#126376=CARTESIAN_POINT('Ctrl Pts',(-6.43768917687825,-78.1193716314746,
57.2055448111296));
#126377=CARTESIAN_POINT('Ctrl Pts',(-6.46127749702327,-78.5607009250776,
57.2372938612818));
#126378=CARTESIAN_POINT('Ctrl Pts',(-6.50284708023062,-79.220321178602,
57.2950452555082));
#126379=CARTESIAN_POINT('Ctrl Pts',(-6.52517453823015,-79.5495378836441,
57.3264553750152));
#126380=CARTESIAN_POINT('Ctrl Pts',(-6.55374130281479,-79.9325855515165,
57.3676563681427));
#126381=CARTESIAN_POINT('Ctrl Pts',(-6.56650133766688,-80.0965263046025,
57.3863044363751));
#126382=CARTESIAN_POINT('Ctrl Pts',(-6.5751203655941,-80.2057706881831,
57.3989582017931));
#126383=CARTESIAN_POINT('Ctrl Pts',(-6.57964866975663,-80.2623756631579,
57.4056368678187));
#126384=CARTESIAN_POINT('Ctrl Pts',(-6.72015992204332,-81.9970282825598,
57.6138171149191));
#126385=CARTESIAN_POINT('Ctrl Pts',(-6.90771485277002,-83.6167188709601,
57.9152192285855));
#126386=CARTESIAN_POINT('Ctrl Pts',(-7.08824189517591,-85.17401265925,58.3404161122));
#126387=CARTESIAN_POINT('',(-7.08815755158619,25.,58.3404518909995));
#126388=CARTESIAN_POINT('Origin',(27.4324635166691,25.,72.98888938658));
#126389=CARTESIAN_POINT('',(-8.15021171484832,-89.0000000007984,61.1515796381337));
#126390=CARTESIAN_POINT('Ctrl Pts',(-7.08815755570517,-85.17401265925,58.3404519007063));
#126391=CARTESIAN_POINT('Ctrl Pts',(-7.17009088674586,-85.5332934006639,
58.5335366223212));
#126392=CARTESIAN_POINT('Ctrl Pts',(-7.25466994278313,-85.8832477134225,
58.7373493420429));
#126393=CARTESIAN_POINT('Ctrl Pts',(-7.34134732186451,-86.2238755975257,
58.9520777911399));
#126394=CARTESIAN_POINT('Ctrl Pts',(-7.38468601140521,-86.3941895395773,
59.0594420156884));
#126395=CARTESIAN_POINT('Ctrl Pts',(-7.42854839638355,-86.5621718744651,
59.1695353419165));
#126396=CARTESIAN_POINT('Ctrl Pts',(-7.47286045458535,-86.727822602189,
59.2823814993839));
#126397=CARTESIAN_POINT('Ctrl Pts',(-7.49501648368625,-86.8106479660509,
59.3388045781176));
#126398=CARTESIAN_POINT('Ctrl Pts',(-7.51728487970092,-86.8928904281219,
59.395915884714));
#126399=CARTESIAN_POINT('Ctrl Pts',(-7.53965601887953,-86.974549988402,
59.4537183425445));
#126400=CARTESIAN_POINT('Ctrl Pts',(-7.56202715805814,-87.056209548682,
59.5115208003749));
#126401=CARTESIAN_POINT('Ctrl Pts',(-7.58475892257956,-87.1382060307662,
59.5706907776505));
#126402=CARTESIAN_POINT('Ctrl Pts',(-7.6070678306237,-87.2177799638692,
59.6292021536361));
#126403=CARTESIAN_POINT('Ctrl Pts',(-7.69754835975279,-87.5405161353482,
59.8665127494201));
#126404=CARTESIAN_POINT('Ctrl Pts',(-7.78908991439444,-87.8523241301438,
60.1138381553492));
#126405=CARTESIAN_POINT('Ctrl Pts',(-7.88109427946115,-88.1532039481646,
60.371336700763));
#126406=CARTESIAN_POINT('Ctrl Pts',(-7.97056691853573,-88.4458043192783,
60.6217495414943));
#126407=CARTESIAN_POINT('Ctrl Pts',(-8.06047707269029,-88.7280696699181,
60.8817836000023));
#126408=CARTESIAN_POINT('Ctrl Pts',(-8.15022843089587,-89.,61.15157407589));
#126409=CARTESIAN_POINT('Origin',(27.4324635166691,-89.,72.98888938658));
#126410=CARTESIAN_POINT('Origin',(27.4324635166691,-89.,72.98888938658));
#126411=CARTESIAN_POINT('',(-9.69875398068591,-89.98547710816,72.9888884257558));
#126412=CARTESIAN_POINT('Ctrl Pts',(-8.15021171484831,-89.0000000007984,
61.1515796381337));
#126413=CARTESIAN_POINT('Ctrl Pts',(-8.18209401555367,-89.016084121901,
61.247394756252));
#126414=CARTESIAN_POINT('Ctrl Pts',(-8.21351914995864,-89.0320746553665,
61.3439406457586));
#126415=CARTESIAN_POINT('Ctrl Pts',(-8.24446559888565,-89.0479569881628,
61.441196198803));
#126416=CARTESIAN_POINT('Ctrl Pts',(-8.29197525924787,-89.0723398903396,
61.5905050356386));
#126417=CARTESIAN_POINT('Ctrl Pts',(-8.33835843912484,-89.0964700937086,
61.7414879393347));
#126418=CARTESIAN_POINT('Ctrl Pts',(-8.38362243092968,-89.1203436093358,
61.8941276178605));
#126419=CARTESIAN_POINT('Ctrl Pts',(-8.42888642273451,-89.1442171249629,
62.0467672963862));
#126420=CARTESIAN_POINT('Ctrl Pts',(-8.47303075616557,-89.1678336747818,
62.2010637343623));
#126421=CARTESIAN_POINT('Ctrl Pts',(-8.51603088739236,-89.1911430500894,
62.3569811977979));
#126422=CARTESIAN_POINT('Ctrl Pts',(-8.54388046912763,-89.2062396633859,
62.4579631254809));
#126423=CARTESIAN_POINT('Ctrl Pts',(-8.57124991958204,-89.2212197737176,
62.55963207447));
#126424=CARTESIAN_POINT('Ctrl Pts',(-8.59812340744795,-89.2360643190087,
62.6619701173454));
#126425=CARTESIAN_POINT('Ctrl Pts',(-8.62625664141202,-89.2516047307279,
62.7691054515457));
#126426=CARTESIAN_POINT('Ctrl Pts',(-8.65384642235063,-89.2669966465503,
62.8769743529093));
#126427=CARTESIAN_POINT('Ctrl Pts',(-8.68089332036743,-89.282247619279,
62.9855784771597));
#126428=CARTESIAN_POINT('Ctrl Pts',(-8.70733466723629,-89.2971571390234,
63.0917510711077));
#126429=CARTESIAN_POINT('Ctrl Pts',(-8.73325657894745,-89.3119259141199,
63.1986202964528));
#126430=CARTESIAN_POINT('Ctrl Pts',(-8.7586549986539,-89.3265499257272,
63.3061769093053));
#126431=CARTESIAN_POINT('Ctrl Pts',(-8.77135420850712,-89.3338619315309,
63.3599552157315));
#126432=CARTESIAN_POINT('Ctrl Pts',(-8.7839224900317,-89.3411377408504,
63.4139053859424));
#126433=CARTESIAN_POINT('Ctrl Pts',(-8.79635897506002,-89.3483768140945,
63.4680263665213));
#126434=CARTESIAN_POINT('Ctrl Pts',(-8.80504617371202,-89.353433489448,
63.5058312373075));
#126435=CARTESIAN_POINT('Ctrl Pts',(-8.8135248704471,-89.3583844131764,
63.5430801157702));
#126436=CARTESIAN_POINT('Ctrl Pts',(-8.82209708340818,-89.3634146593055,
63.5811113108075));
#126437=CARTESIAN_POINT('Ctrl Pts',(-8.82579674339726,-89.365585650673,
63.5975250993187));
#126438=CARTESIAN_POINT('Ctrl Pts',(-8.82951373013669,-89.3677709458225,
63.6140850461936));
#126439=CARTESIAN_POINT('Ctrl Pts',(-8.83327191475055,-89.369983233208,
63.6309007518484));
#126440=CARTESIAN_POINT('Ctrl Pts',(-8.8572936644153,-89.3841238407679,
63.7383842081388));
#126441=CARTESIAN_POINT('Ctrl Pts',(-8.88059574867455,-89.3979965883317,
63.8456211319469));
#126442=CARTESIAN_POINT('Ctrl Pts',(-8.9031979127015,-89.41159584742,63.9525808563939));
#126443=CARTESIAN_POINT('Ctrl Pts',(-8.93881407811077,-89.4330253645474,
64.1211264537753));
#126444=CARTESIAN_POINT('Ctrl Pts',(-8.97269344987008,-89.4537784137391,
64.2889863577911));
#126445=CARTESIAN_POINT('Ctrl Pts',(-9.00495691259786,-89.4738783490184,
64.456129214163));
#126446=CARTESIAN_POINT('Ctrl Pts',(-9.03722037532564,-89.4939782842977,
64.623272070535));
#126447=CARTESIAN_POINT('Ctrl Pts',(-9.067867221227,-89.5134242699625,64.7896971699235));
#126448=CARTESIAN_POINT('Ctrl Pts',(-9.09700654351357,-89.5321971028266,
64.9553440727831));
#126449=CARTESIAN_POINT('Ctrl Pts',(-9.11569946399035,-89.544239904248,
65.0616068180841));
#126450=CARTESIAN_POINT('Ctrl Pts',(-9.1337712008358,-89.5560112179457,
65.1675566042376));
#126451=CARTESIAN_POINT('Ctrl Pts',(-9.15124299591421,-89.5675125901354,
65.2731732755662));
#126452=CARTESIAN_POINT('Ctrl Pts',(-9.16964894930865,-89.5796289021427,
65.3844369162756));
#126453=CARTESIAN_POINT('Ctrl Pts',(-9.18738923923466,-89.5914456250726,
65.4953311385514));
#126454=CARTESIAN_POINT('Ctrl Pts',(-9.20449991765006,-89.6029672745584,
65.6058534556344));
#126455=CARTESIAN_POINT('Ctrl Pts',(-9.22117638648685,-89.6141965446045,
65.7135711002455));
#126456=CARTESIAN_POINT('Ctrl Pts',(-9.23725367603251,-89.6251457653554,
65.8209307443482));
#126457=CARTESIAN_POINT('Ctrl Pts',(-9.25276003570989,-89.6358193485331,
65.9279223147034));
#126458=CARTESIAN_POINT('Ctrl Pts',(-9.26051321554857,-89.6411561401219,
65.981418099881));
#126459=CARTESIAN_POINT('Ctrl Pts',(-9.26812362181095,-89.6464240048523,
66.0348218752061));
#126460=CARTESIAN_POINT('Ctrl Pts',(-9.27559453031638,-89.6516234702577,
66.0881325230372));
#126461=CARTESIAN_POINT('Ctrl Pts',(-9.27932998456911,-89.6542232029604,
66.1147878469527));
#126462=CARTESIAN_POINT('Ctrl Pts',(-9.28303056205811,-89.6568058346514,
66.1414198894198));
#126463=CARTESIAN_POINT('Ctrl Pts',(-9.28669665832162,-89.6593714261074,
66.1680285154141));
#126464=CARTESIAN_POINT('Ctrl Pts',(-9.28852970645337,-89.6606542218354,
66.1813328284112));
#126465=CARTESIAN_POINT('Ctrl Pts',(-9.29035413414395,-89.6619327574292,
66.1946312873125));
#126466=CARTESIAN_POINT('Ctrl Pts',(-9.2921699899623,-89.6632070403074,
66.2079238756842));
#126467=CARTESIAN_POINT('Ctrl Pts',(-9.29307791787148,-89.6638441817465,
66.2145701698701));
#126468=CARTESIAN_POINT('Ctrl Pts',(-9.29398370280446,-89.6644802600019,
66.2212149964247));
#126469=CARTESIAN_POINT('Ctrl Pts',(-9.29488735077875,-89.66511527599,66.2278583533219));
#126470=CARTESIAN_POINT('Ctrl Pts',(-9.29579099875305,-89.6657502919782,
66.2345017102192));
#126471=CARTESIAN_POINT('Ctrl Pts',(-9.29651740248539,-89.6662610229698,
66.239850723387));
#126472=CARTESIAN_POINT('Ctrl Pts',(-9.29759188980969,-89.6670171380553,
66.2477840130256));
#126473=CARTESIAN_POINT('Ctrl Pts',(-9.31182399920604,-89.6770322516533,
66.3528643089539));
#126474=CARTESIAN_POINT('Ctrl Pts',(-9.32551671844582,-89.6867588740448,
66.457480530125));
#126475=CARTESIAN_POINT('Ctrl Pts',(-9.33868951779708,-89.6962118077819,
66.5616189265927));
#126476=CARTESIAN_POINT('Ctrl Pts',(-9.36621604052355,-89.7159651182519,
66.7792315889151));
#126477=CARTESIAN_POINT('Ctrl Pts',(-9.3914768363582,-89.7345241980598,
66.994757794308));
#126478=CARTESIAN_POINT('Ctrl Pts',(-9.41474181762129,-89.7519385865142,
67.2081436914698));
#126479=CARTESIAN_POINT('Ctrl Pts',(-9.434138334951,-89.7664573382649,67.3860481224001));
#126480=CARTESIAN_POINT('Ctrl Pts',(-9.45214578494019,-89.7801797718888,
67.5624644758447));
#126481=CARTESIAN_POINT('Ctrl Pts',(-9.46889638665283,-89.7931234924939,
67.7373665660249));
#126482=CARTESIAN_POINT('Ctrl Pts',(-9.47600631428016,-89.7986175588151,
67.8116051649949));
#126483=CARTESIAN_POINT('Ctrl Pts',(-9.48289068462014,-89.8039692324113,
67.8855695517355));
#126484=CARTESIAN_POINT('Ctrl Pts',(-9.48955517202189,-89.8091856646797,
67.9592604516609));
#126485=CARTESIAN_POINT('Ctrl Pts',(-9.50466375404086,-89.8210114646285,
68.1263198124878));
#126486=CARTESIAN_POINT('Ctrl Pts',(-9.5186447410226,-89.8321414282993,
68.2919706567794));
#126487=CARTESIAN_POINT('Ctrl Pts',(-9.53162797150561,-89.8425937213016,
68.4561895503427));
#126488=CARTESIAN_POINT('Ctrl Pts',(-9.54098307770475,-89.8501251528039,
68.5745179733959));
#126489=CARTESIAN_POINT('Ctrl Pts',(-9.54981726512395,-89.8573080437861,
68.6921043252551));
#126490=CARTESIAN_POINT('Ctrl Pts',(-9.55816846897785,-89.8641521140158,
68.8089439460119));
#126491=CARTESIAN_POINT('Ctrl Pts',(-9.5623440709048,-89.8675741491307,
68.8673637563902));
#126492=CARTESIAN_POINT('Ctrl Pts',(-9.56639886080588,-89.870911431891,
68.9255968914723));
#126493=CARTESIAN_POINT('Ctrl Pts',(-9.57033720511539,-89.8741650071343,
68.9836429109746));
#126494=CARTESIAN_POINT('Ctrl Pts',(-9.57230637727014,-89.8757917947559,
69.0126659207258));
#126495=CARTESIAN_POINT('Ctrl Pts',(-9.57424643505923,-89.8773976532099,
69.0416421518496));
#126496=CARTESIAN_POINT('Ctrl Pts',(-9.57615790736035,-89.8789827019431,
69.0705715529551));
#126497=CARTESIAN_POINT('Ctrl Pts',(-9.57711364351091,-89.8797752263098,
69.0850362535078));
#126498=CARTESIAN_POINT('Ctrl Pts',(-9.5780622331368,-89.8805625481215,
69.0994892465667));
#126499=CARTESIAN_POINT('Ctrl Pts',(-9.57900374133827,-89.8813446818348,
69.1139305261119));
#126500=CARTESIAN_POINT('Ctrl Pts',(-9.57970987248937,-89.8819312821198,
69.1247614857708));
#126501=CARTESIAN_POINT('Ctrl Pts',(-9.58041202032738,-89.8825149640896,
69.1355858565792));
#126502=CARTESIAN_POINT('Ctrl Pts',(-9.5811102120887,-89.8830957337268,
69.1464036360814));
#126503=CARTESIAN_POINT('Ctrl Pts',(-9.58134294267581,-89.8832893236059,
69.1500095625822));
#126504=CARTESIAN_POINT('Ctrl Pts',(-9.5814788872496,-89.8834024123336,
69.1521169202122));
#126505=CARTESIAN_POINT('Ctrl Pts',(-9.58180708615587,-89.8836755328058,
69.1572192183974));
#126506=CARTESIAN_POINT('Ctrl Pts',(-9.59057123577426,-89.890968880334,
69.2934698390995));
#126507=CARTESIAN_POINT('Ctrl Pts',(-9.59875323496047,-89.8978406637106,
69.429383537476));
#126508=CARTESIAN_POINT('Ctrl Pts',(-9.60637084586831,-89.9043168788772,
69.5650066938047));
#126509=CARTESIAN_POINT('Ctrl Pts',(-9.6151037548574,-89.9117412798249,
69.7204865017603));
#126510=CARTESIAN_POINT('Ctrl Pts',(-9.62309536810506,-89.9186454307002,
69.8755816217704));
#126511=CARTESIAN_POINT('Ctrl Pts',(-9.63040876584963,-89.925030666439,
70.0302322420457));
#126512=CARTESIAN_POINT('Ctrl Pts',(-9.63791116337966,-89.9315809155174,
70.1888794908479));
#126513=CARTESIAN_POINT('Ctrl Pts',(-9.64469942220319,-89.9375852668526,
70.3470593513853));
#126514=CARTESIAN_POINT('Ctrl Pts',(-9.65083230009781,-89.9430469783969,
70.5047651994685));
#126515=CARTESIAN_POINT('Ctrl Pts',(-9.65730123938662,-89.9488079736425,
70.6711128056447));
#126516=CARTESIAN_POINT('Ctrl Pts',(-9.66304052990155,-89.9539654654836,
70.836933200003));
#126517=CARTESIAN_POINT('Ctrl Pts',(-9.66811581934112,-89.9585219861143,
71.0022782405352));
#126518=CARTESIAN_POINT('Ctrl Pts',(-9.67230014378107,-89.962278611399,
71.1385970263627));
#126519=CARTESIAN_POINT('Ctrl Pts',(-9.67603295014039,-89.9656267811013,
71.2745939771198));
#126520=CARTESIAN_POINT('Ctrl Pts',(-9.67935298844021,-89.9685655423977,
71.4103244434226));
#126521=CARTESIAN_POINT('Ctrl Pts',(-9.6832714542365,-89.9720340070909,
71.5705199416948));
#126522=CARTESIAN_POINT('Ctrl Pts',(-9.68661369895617,-89.9749328318067,
71.7303422457988));
#126523=CARTESIAN_POINT('Ctrl Pts',(-9.68935269073222,-89.9772973600029,
71.8897156366769));
#126524=CARTESIAN_POINT('Ctrl Pts',(-9.69223792563923,-89.9797881375766,
72.0575984593386));
#126525=CARTESIAN_POINT('Ctrl Pts',(-9.69445346644508,-89.981686222432,
72.2249840222755));
#126526=CARTESIAN_POINT('Ctrl Pts',(-9.69599245988841,-89.9830179188359,
72.3918357271171));
#126527=CARTESIAN_POINT('Ctrl Pts',(-9.69764057859723,-89.9844440417134,
72.5705183703347));
#126528=CARTESIAN_POINT('Ctrl Pts',(-9.69851227080421,-89.9852209484255,
72.7485899466107));
#126529=CARTESIAN_POINT('Ctrl Pts',(-9.69863352861823,-89.9853599569616,
72.926047324153));
#126530=CARTESIAN_POINT('Ctrl Pts',(-9.69864784763287,-89.9853763721121,
72.9470027966594));
#126531=CARTESIAN_POINT('Ctrl Pts',(-9.69865174465511,-89.9853838658523,
72.9679497363086));
#126532=CARTESIAN_POINT('Ctrl Pts',(-9.69864529703997,-89.9853824355062,
72.9888881602058));
#126533=CARTESIAN_POINT('',(-8.1502284310481,-88.9999999997697,84.8262046968124));
#126534=CARTESIAN_POINT('Ctrl Pts',(-9.69875398068591,-89.98547710816,72.9888884257558));
#126535=CARTESIAN_POINT('Ctrl Pts',(-9.69890573883026,-89.9848877911751,
73.9716069035248));
#126536=CARTESIAN_POINT('Ctrl Pts',(-9.67912136001599,-89.9640632821437,
74.9856759988131));
#126537=CARTESIAN_POINT('Ctrl Pts',(-9.60195490217224,-89.8977852775027,
76.5544514555789));
#126538=CARTESIAN_POINT('Ctrl Pts',(-9.56819216649599,-89.8697589747,77.0852934680504));
#126539=CARTESIAN_POINT('Ctrl Pts',(-9.50208752038253,-89.8176498462862,
77.8929954127754));
#126540=CARTESIAN_POINT('Ctrl Pts',(-9.47746662247536,-89.7985988344223,
78.1641308573158));
#126541=CARTESIAN_POINT('Ctrl Pts',(-9.43614470342231,-89.7673400574451,
78.5735759435839));
#126542=CARTESIAN_POINT('Ctrl Pts',(-9.41438517235184,-89.7510400643076,
78.7789833001031));
#126543=CARTESIAN_POINT('Ctrl Pts',(-9.38695474897263,-89.730815278714,
79.0197918353817));
#126544=CARTESIAN_POINT('Ctrl Pts',(-9.37271249123869,-89.7203966553879,
79.1404831516953));
#126545=CARTESIAN_POINT('Ctrl Pts',(-9.36545758383888,-89.715110269035,
79.2008999758989));
#126546=CARTESIAN_POINT('Ctrl Pts',(-9.36231945271429,-89.71282810399,79.2268080846274));
#126547=CARTESIAN_POINT('Ctrl Pts',(-9.36022092200985,-89.7113029721415,
79.2440835239248));
#126548=CARTESIAN_POINT('Ctrl Pts',(-9.35901417344777,-89.710426596697,
79.2539855590541));
#126549=CARTESIAN_POINT('Ctrl Pts',(-9.24272592603309,-89.6260229082353,
80.2058056935545));
#126550=CARTESIAN_POINT('Ctrl Pts',(-9.09014305109249,-89.5253628372099,
81.1460397672208));
#126551=CARTESIAN_POINT('Ctrl Pts',(-8.69368888297694,-89.2881476313874,
83.006160518697));
#126552=CARTESIAN_POINT('Ctrl Pts',(-8.4496752067201,-89.1513839217613,
83.9260746582551));
#126553=CARTESIAN_POINT('Ctrl Pts',(-8.15022843089591,-89.,84.82620469727));
#126554=CARTESIAN_POINT('Origin',(27.4324635166691,-89.,72.98888938658));
#126555=CARTESIAN_POINT('Origin',(27.4324635166691,25.,72.98888938658));
#126556=CARTESIAN_POINT('Ctrl Pts',(-8.15022843089586,-89.,84.82620469727));
#126557=CARTESIAN_POINT('Ctrl Pts',(-8.0592727893093,-88.7244220625868,
85.0996152207309));
#126558=CARTESIAN_POINT('Ctrl Pts',(-7.96815107952594,-88.4382163304836,
85.3630149775318));
#126559=CARTESIAN_POINT('Ctrl Pts',(-7.87748303577277,-88.1413827738554,
85.6165445316851));
#126560=CARTESIAN_POINT('Ctrl Pts',(-7.83214901389618,-87.9929659955412,
85.7433093087617));
#126561=CARTESIAN_POINT('Ctrl Pts',(-7.7869276544551,-87.8418922610958,
85.8676067479479));
#126562=CARTESIAN_POINT('Ctrl Pts',(-7.7418919204437,-87.6881615705191,
85.989455512086));
#126563=CARTESIAN_POINT('Ctrl Pts',(-7.719374053438,-87.6112962252308,86.050379894155));
#126564=CARTESIAN_POINT('Ctrl Pts',(-7.69690255497006,-87.5337666409097,
86.1106920933842));
#126565=CARTESIAN_POINT('Ctrl Pts',(-7.67448625331229,-87.4555728175557,
86.1703945300757));
#126566=CARTESIAN_POINT('Ctrl Pts',(-7.65206995165452,-87.3773789942017,
86.2300969667672));
#126567=CARTESIAN_POINT('Ctrl Pts',(-7.62999301043884,-87.2995343704679,
86.2884442841026));
#126568=CARTESIAN_POINT('Ctrl Pts',(-7.60741161314129,-87.2189986303954,
86.3476749184798));
#126569=CARTESIAN_POINT('Ctrl Pts',(-7.51708602403756,-86.8968556704137,
86.5845974557616));
#126570=CARTESIAN_POINT('Ctrl Pts',(-7.42825142502899,-86.5653686931437,
86.8104033987204));
#126571=CARTESIAN_POINT('Ctrl Pts',(-7.34151639358491,-86.2245376985853,
87.0252821283513));
#126572=CARTESIAN_POINT('Ctrl Pts',(-7.25478136214084,-85.8837067040269,
87.2401608579821));
#126573=CARTESIAN_POINT('Ctrl Pts',(-7.17014580984083,-85.5335316921802,
87.4441127186809));
#126574=CARTESIAN_POINT('Ctrl Pts',(-7.08815755482003,-85.1740126630452,
87.6373268745396));
#126575=CARTESIAN_POINT('Ctrl Pts',(-7.03188518854192,-85.51135559513,87.78728732497));
#126576=CARTESIAN_POINT('Ctrl Pts',(-6.88609751019091,-84.8164336540901,
88.13174534986));
#126577=CARTESIAN_POINT('Ctrl Pts',(-6.48107502706592,-82.93977280408,88.90591654473));
#126578=CARTESIAN_POINT('Ctrl Pts',(-5.85681573002491,-79.41119109238,89.73590455514));
#126579=CARTESIAN_POINT('Ctrl Pts',(-5.56514360048591,-74.999772686,90.0489960419));
#126580=CARTESIAN_POINT('Ctrl Pts',(-5.85684197555091,-70.58850343071,89.73588726852));
#126581=CARTESIAN_POINT('Ctrl Pts',(-6.48119721132191,-67.05962993044,88.90572058463));
#126582=CARTESIAN_POINT('Ctrl Pts',(-6.88619857614591,-65.18309553123,88.13154378191));
#126583=CARTESIAN_POINT('Ctrl Pts',(-7.03199309806391,-64.48813202086,87.78703389719));
#126584=CARTESIAN_POINT('Ctrl Pts',(-7.61748505797291,-84.28363064449,86.1725311745699));
#126585=CARTESIAN_POINT('Ctrl Pts',(-7.51829975074291,-83.66265636758,86.47777956431));
#126586=CARTESIAN_POINT('Ctrl Pts',(-7.23957840814891,-81.99276209823,87.16157935315));
#126587=CARTESIAN_POINT('Ctrl Pts',(-6.79943451186591,-78.87943948555,87.89696709168));
#126588=CARTESIAN_POINT('Ctrl Pts',(-6.59060359545691,-74.99979991999,88.17713587471));
#126589=CARTESIAN_POINT('Ctrl Pts',(-6.79945368327691,-71.12029257632,87.8969512836301));
#126590=CARTESIAN_POINT('Ctrl Pts',(-7.23966353825691,-68.0067086013501,
87.16140622182));
#126591=CARTESIAN_POINT('Ctrl Pts',(-7.51836905611891,-66.33692462081,86.47760140457));
#126592=CARTESIAN_POINT('Ctrl Pts',(-7.61755845601991,-65.7159117191401,
86.1723066272));
#126593=CARTESIAN_POINT('Ctrl Pts',(-8.94180725924391,-83.1405774216701,
84.9904520841));
#126594=CARTESIAN_POINT('Ctrl Pts',(-8.87784551922691,-82.57791839499,85.27891283488));
#126595=CARTESIAN_POINT('Ctrl Pts',(-8.69724304976191,-81.08162805277,85.91955509897));
#126596=CARTESIAN_POINT('Ctrl Pts',(-8.40920175141591,-78.35538419096,86.60152333573));
#126597=CARTESIAN_POINT('Ctrl Pts',(-8.27170075666791,-74.99982653108,86.86227405379));
#126598=CARTESIAN_POINT('Ctrl Pts',(-8.40921447291491,-71.64438573464,86.60150867591));
#126599=CARTESIAN_POINT('Ctrl Pts',(-8.69729849347391,-68.91790285567,85.9193939094799));
#126600=CARTESIAN_POINT('Ctrl Pts',(-8.87789036104291,-67.42170567277,85.27874554859));
#126601=CARTESIAN_POINT('Ctrl Pts',(-8.94185458683591,-66.85900818197,84.99023987675));
#126602=CARTESIAN_POINT('Ctrl Pts',(-10.7849815469809,-82.27197103756,84.43730442383));
#126603=CARTESIAN_POINT('Ctrl Pts',(-10.7390165867829,-81.74231307311,84.73418669521));
#126604=CARTESIAN_POINT('Ctrl Pts',(-10.6120605629239,-80.3576414581,85.38605053251));
#126605=CARTESIAN_POINT('Ctrl Pts',(-10.4188562658489,-77.92603135117,86.06464899639));
#126606=CARTESIAN_POINT('Ctrl Pts',(-10.3293313697989,-74.99984810118,86.32271016737));
#126607=CARTESIAN_POINT('Ctrl Pts',(-10.4188642324849,-72.07377047682,86.06463496379));
#126608=CARTESIAN_POINT('Ctrl Pts',(-10.6120986166669,-69.64193190681,85.38588841531));
#126609=CARTESIAN_POINT('Ctrl Pts',(-10.7390483236119,-68.25733819811,84.73401594236));
#126610=CARTESIAN_POINT('Ctrl Pts',(-10.7850155734819,-67.72763911956,84.43708596738));
#126611=CARTESIAN_POINT('',(-10.5124641215422,-67.7275765921281,84.5902475699691));
#126612=CARTESIAN_POINT('Origin',(-13.9923868665804,-64.8259016968275,90.5664476682519));
#126613=CARTESIAN_POINT('',(-10.5124533883332,-82.2723820629486,84.5902806024135));
#126614=CARTESIAN_POINT('Ctrl Pts',(-7.08822305920791,-85.17401266098,87.6373546719));
#126615=CARTESIAN_POINT('Ctrl Pts',(-7.69414323235493,-84.0874541957658,
86.2096035275483));
#126616=CARTESIAN_POINT('Ctrl Pts',(-8.88948386358317,-83.0746694882491,
85.1457926978883));
#126617=CARTESIAN_POINT('Ctrl Pts',(-10.5124533883332,-82.2723820629485,
84.5902806024135));
#126618=CARTESIAN_POINT('',(-9.07682641225685,-75.0000006726261,86.7031084130407));
#126619=CARTESIAN_POINT('Ctrl Pts',(-9.07682655323991,-75.00000067265,86.70310871249));
#126620=CARTESIAN_POINT('Ctrl Pts',(-9.07712527162583,-75.7710653833458,
86.703079548411));
#126621=CARTESIAN_POINT('Ctrl Pts',(-9.14270874172081,-76.5105174064079,
86.6375317298765));
#126622=CARTESIAN_POINT('Ctrl Pts',(-9.35334858385702,-77.8974408785069,
86.4100699179464));
#126623=CARTESIAN_POINT('Ctrl Pts',(-9.49860676910191,-78.5448431892613,
86.2490985948516));
#126624=CARTESIAN_POINT('Ctrl Pts',(-9.80522934488242,-79.7518959795621,
85.8621453182158));
#126625=CARTESIAN_POINT('Ctrl Pts',(-9.96585902065113,-80.3121962983374,
85.6360301024058));
#126626=CARTESIAN_POINT('Ctrl Pts',(-10.2616504213497,-81.3517147132588,
85.1408733798662));
#126627=CARTESIAN_POINT('Ctrl Pts',(-10.3972012330611,-81.831526988694,
84.8713589226467));
#126628=CARTESIAN_POINT('Ctrl Pts',(-10.5124534169749,-82.27238204879,84.59028059261));
#126629=CARTESIAN_POINT('Ctrl Pts',(-10.5124650377649,-67.72757582813,84.59024914348));
#126630=CARTESIAN_POINT('Ctrl Pts',(-10.4327423171429,-68.0325174777516,
84.7846763698828));
#126631=CARTESIAN_POINT('Ctrl Pts',(-10.3563334338288,-68.3071255764948,
84.9428892616601));
#126632=CARTESIAN_POINT('Ctrl Pts',(-10.2548365651166,-68.6670586204727,
85.1382149877773));
#126633=CARTESIAN_POINT('Ctrl Pts',(-10.223125993645,-68.7784239097236,
85.1962985864462));
#126634=CARTESIAN_POINT('Ctrl Pts',(-10.1646839277008,-68.9833111354606,
85.3001142621517));
#126635=CARTESIAN_POINT('Ctrl Pts',(-10.137524099967,-69.0783222991939,
85.3465564639887));
#126636=CARTESIAN_POINT('Ctrl Pts',(-10.0666768665712,-69.3268944073992,
85.4651755558802));
#126637=CARTESIAN_POINT('Ctrl Pts',(-10.0065160646104,-69.5382359356507,
85.5619916181195));
#126638=CARTESIAN_POINT('Ctrl Pts',(-9.8977910040944,-69.927385302646,85.7233076444201));
#126639=CARTESIAN_POINT('Ctrl Pts',(-9.85850403230828,-70.0691379356638,
85.7797140223083));
#126640=CARTESIAN_POINT('Ctrl Pts',(-9.79563566630381,-70.3003928382042,
85.8665387091036));
#126641=CARTESIAN_POINT('Ctrl Pts',(-9.77402788007526,-70.3805828396457,
85.8958465728976));
#126642=CARTESIAN_POINT('Ctrl Pts',(-9.74076713746608,-70.5056027949893,
85.940114802761));
#126643=CARTESIAN_POINT('Ctrl Pts',(-9.7239250814145,-70.5692965693181,
85.962325255793));
#126644=CARTESIAN_POINT('Ctrl Pts',(-9.70394026882669,-70.645695140865,
85.9883150254738));
#126645=CARTESIAN_POINT('Ctrl Pts',(-9.69386879831417,-70.6844189512115,
86.0013220886582));
#126646=CARTESIAN_POINT('Ctrl Pts',(-9.68953604802536,-70.7011275081655,
86.0068983758215));
#126647=CARTESIAN_POINT('Ctrl Pts',(-9.68664396323484,-70.7122916036429,
86.0106162205642));
#126648=CARTESIAN_POINT('Ctrl Pts',(-9.68488025991898,-70.7191079772815,
86.0128804243338));
#126649=CARTESIAN_POINT('Ctrl Pts',(-9.53862940322314,-71.2848144523634,
86.2004563984907));
#126650=CARTESIAN_POINT('Ctrl Pts',(-9.38875606960968,-71.9186428381076,
86.3702386471311));
#126651=CARTESIAN_POINT('Ctrl Pts',(-9.1579878314319,-73.3455803154869,
86.621969533406));
#126652=CARTESIAN_POINT('Ctrl Pts',(-9.07716137299026,-74.1401369689079,
86.7030186524931));
#126653=CARTESIAN_POINT('Ctrl Pts',(-9.07682655323991,-75.00000067265,86.70310871249));
#126654=CARTESIAN_POINT('Ctrl Pts',(-6.92065457530891,-65.0085199552,88.04213796552));
#126655=CARTESIAN_POINT('Ctrl Pts',(-7.12075460565991,-64.0617034611701,
87.58903703014));
#126656=CARTESIAN_POINT('Ctrl Pts',(-7.57373925880491,-62.21199765049,86.51254138381));
#126657=CARTESIAN_POINT('Ctrl Pts',(-8.29170030411691,-59.88527159252,84.5296397505));
#126658=CARTESIAN_POINT('Ctrl Pts',(-8.94052593337591,-58.09298635035,82.330744365395));
#126659=CARTESIAN_POINT('Ctrl Pts',(-9.43809466145892,-56.85575438086,80.175556126363));
#126660=CARTESIAN_POINT('Ctrl Pts',(-9.78504368857292,-56.04942203172,78.151265483228));
#126661=CARTESIAN_POINT('Ctrl Pts',(-10.0084080082939,-55.55161389672,76.24295421649));
#126662=CARTESIAN_POINT('Ctrl Pts',(-10.1306719411089,-55.28587008401,74.370377310615));
#126663=CARTESIAN_POINT('Ctrl Pts',(-10.1545766833119,-55.23449747153,72.4633569248084));
#126664=CARTESIAN_POINT('Ctrl Pts',(-10.0742919226589,-55.40774496076,70.54498904177));
#126665=CARTESIAN_POINT('Ctrl Pts',(-9.89754394190891,-55.79679141717,68.694837416293));
#126666=CARTESIAN_POINT('Ctrl Pts',(-9.63436051758492,-56.39594592554,66.889026863432));
#126667=CARTESIAN_POINT('Ctrl Pts',(-9.27716813710291,-57.24836476724,65.062303256644));
#126668=CARTESIAN_POINT('Ctrl Pts',(-8.80090929958791,-58.46683609555,63.14889932481));
#126669=CARTESIAN_POINT('Ctrl Pts',(-8.20270682605691,-60.16216466129,61.19431102613));
#126670=CARTESIAN_POINT('Ctrl Pts',(-7.53829930230291,-62.35228602585,59.3803617293));
#126671=CARTESIAN_POINT('Ctrl Pts',(-7.11363397064091,-64.09507808025,58.37279234099));
#126672=CARTESIAN_POINT('Ctrl Pts',(-6.92079475816891,-65.00772646722,57.93600906651));
#126673=CARTESIAN_POINT('Ctrl Pts',(-7.63686846205491,-66.3621040647101,
86.13865710204));
#126674=CARTESIAN_POINT('Ctrl Pts',(-7.76950703063191,-65.54018993106,85.74905955785));
#126675=CARTESIAN_POINT('Ctrl Pts',(-8.07016186809891,-63.92982350139,84.82480089674));
#126676=CARTESIAN_POINT('Ctrl Pts',(-8.54916445708991,-61.88218169553,83.12176196493));
#126677=CARTESIAN_POINT('Ctrl Pts',(-8.98476748958292,-60.28053161396,81.222506221777));
#126678=CARTESIAN_POINT('Ctrl Pts',(-9.32101949477791,-59.15720375094,79.345376616387));
#126679=CARTESIAN_POINT('Ctrl Pts',(-9.5568109059989,-58.41509188199,77.567583873189));
#126680=CARTESIAN_POINT('Ctrl Pts',(-9.70924409102191,-57.95233484547,75.880638307014));
#126681=CARTESIAN_POINT('Ctrl Pts',(-9.79291036296791,-57.70366775115,74.217967928337));
#126682=CARTESIAN_POINT('Ctrl Pts',(-9.80928988049891,-57.65544493246,72.5212298562295));
#126683=CARTESIAN_POINT('Ctrl Pts',(-9.75430501765591,-57.81788267456,70.815731431435));
#126684=CARTESIAN_POINT('Ctrl Pts',(-9.63352487119791,-58.18069632678,69.176762924934));
#126685=CARTESIAN_POINT('Ctrl Pts',(-9.45430378327291,-58.73477501893,67.585691843247));
#126686=CARTESIAN_POINT('Ctrl Pts',(-9.21211183497991,-59.51491229764,65.986727637278));
#126687=CARTESIAN_POINT('Ctrl Pts',(-8.89088286577791,-60.61594879951,64.324292302119));
#126688=CARTESIAN_POINT('Ctrl Pts',(-8.48972710545391,-62.12654662001,62.63793056294));
#126689=CARTESIAN_POINT('Ctrl Pts',(-8.04663367869591,-64.05203475839,61.08013396196));
#126690=CARTESIAN_POINT('Ctrl Pts',(-7.76477879250591,-65.56916470704,60.21501006199));
#126691=CARTESIAN_POINT('Ctrl Pts',(-7.63695856837891,-66.36141690504,59.8394398311601));
#126692=CARTESIAN_POINT('Ctrl Pts',(-9.30568646040191,-67.5925100747501,
84.84655826695));
#126693=CARTESIAN_POINT('Ctrl Pts',(-9.38430344193091,-66.8864512848699,
84.49764454981));
#126694=CARTESIAN_POINT('Ctrl Pts',(-9.56256965368191,-65.50055373805,83.67212409033));
#126695=CARTESIAN_POINT('Ctrl Pts',(-9.84698595988291,-63.72418521299,82.154388156787));
#126696=CARTESIAN_POINT('Ctrl Pts',(-10.1060740212189,-62.31869562594,80.456822147596));
#126697=CARTESIAN_POINT('Ctrl Pts',(-10.3064235701329,-61.32140256381,78.769328788008));
#126698=CARTESIAN_POINT('Ctrl Pts',(-10.4471274598089,-60.65609648668,77.161368332835));
#126699=CARTESIAN_POINT('Ctrl Pts',(-10.5381893031789,-60.23829278713,75.6280051070961));
#126700=CARTESIAN_POINT('Ctrl Pts',(-10.5882066814419,-60.01274187767,74.111586341137));
#126701=CARTESIAN_POINT('Ctrl Pts',(-10.5980020454079,-59.96890586323,72.561632978805));
#126702=CARTESIAN_POINT('Ctrl Pts',(-10.5651238429639,-60.11644815221,71.0046224172161));
#126703=CARTESIAN_POINT('Ctrl Pts',(-10.4929458682419,-60.44475452627,69.512475580624));
#126704=CARTESIAN_POINT('Ctrl Pts',(-10.3859423486419,-60.94317745813,68.069876677003));
#126705=CARTESIAN_POINT('Ctrl Pts',(-10.2415081737819,-61.6397769585701,
66.627215680196));
#126706=CARTESIAN_POINT('Ctrl Pts',(-10.0502091869879,-62.61390026386,65.135327797585));
#126707=CARTESIAN_POINT('Ctrl Pts',(-9.81168369918191,-63.93662258829,63.629051184382));
#126708=CARTESIAN_POINT('Ctrl Pts',(-9.54861819276191,-65.60577043727,62.24063178495));
#126709=CARTESIAN_POINT('Ctrl Pts',(-9.38149959755591,-66.91134741848,61.4678544918301));
#126710=CARTESIAN_POINT('Ctrl Pts',(-9.30573940932591,-67.59192210557,61.1315047603));
#126711=CARTESIAN_POINT('Ctrl Pts',(-11.5646178953289,-68.43247654302,84.4465034494));
#126712=CARTESIAN_POINT('Ctrl Pts',(-11.6143874109131,-67.80806067473,84.10661689733));
#126713=CARTESIAN_POINT('Ctrl Pts',(-11.7267907129605,-66.583003723,83.30488853365));
#126714=CARTESIAN_POINT('Ctrl Pts',(-11.9032597796691,-65.01117314613,81.837645484982));
#126715=CARTESIAN_POINT('Ctrl Pts',(-12.0608820228823,-63.7647605769001,
80.200009462762));
#126716=CARTESIAN_POINT('Ctrl Pts',(-12.1802633017076,-62.87825648365,78.57253830883));
#126717=CARTESIAN_POINT('Ctrl Pts',(-12.2626041075034,-62.2856582147501,
77.02085457485));
#126718=CARTESIAN_POINT('Ctrl Pts',(-12.3151851184271,-61.91294559539,75.539930091032));
#126719=CARTESIAN_POINT('Ctrl Pts',(-12.3438113818399,-61.71152917766,74.074340121796));
#126720=CARTESIAN_POINT('Ctrl Pts',(-12.3493938338451,-61.67236410253,72.5757901676427));
#126721=CARTESIAN_POINT('Ctrl Pts',(-12.3306271776957,-61.80416073374,71.070632227735));
#126722=CARTESIAN_POINT('Ctrl Pts',(-12.2891286387917,-62.09718082047,69.629053886055));
#126723=CARTESIAN_POINT('Ctrl Pts',(-12.2269112507223,-62.54145725969,68.23640962794));
#126724=CARTESIAN_POINT('Ctrl Pts',(-12.1417578310604,-63.16140834367,66.844644399399));
#126725=CARTESIAN_POINT('Ctrl Pts',(-12.0270663262746,-64.02670740855,65.4058375265251));
#126726=CARTESIAN_POINT('Ctrl Pts',(-11.8814290941622,-65.19921867886,63.9523875906491));
#126727=CARTESIAN_POINT('Ctrl Pts',(-11.7180007421678,-66.67599988134,62.60977879472));
#126728=CARTESIAN_POINT('Ctrl Pts',(-11.6126219518349,-67.83008530504,61.85919024876));
#126729=CARTESIAN_POINT('Ctrl Pts',(-11.5646546770989,-68.43195908097,61.53154922964));
#126730=CARTESIAN_POINT('',(-10.5124610812362,-67.7276344807769,61.3874942276418));
#126731=CARTESIAN_POINT('Ctrl Pts',(-7.08825603872491,-64.825987319,58.34041012264));
#126732=CARTESIAN_POINT('Ctrl Pts',(-7.69416695291821,-65.9125766751487,
59.7681366846271));
#126733=CARTESIAN_POINT('Ctrl Pts',(-8.88950139818992,-66.9253426838604,
60.8319665772906));
#126734=CARTESIAN_POINT('Ctrl Pts',(-10.5124619777589,-67.72763373312,61.38749268805));
#126735=CARTESIAN_POINT('Ctrl Pts',(-10.5124561093177,-67.7276386264893,
61.3875027668017));
#126736=CARTESIAN_POINT('Ctrl Pts',(-10.5438023417544,-67.6076229168416,
61.4640236233382));
#126737=CARTESIAN_POINT('Ctrl Pts',(-10.576340043582,-67.4844449032088,
61.5453107016493));
#126738=CARTESIAN_POINT('Ctrl Pts',(-10.6098920208526,-67.3584444482681,
61.6317332225431));
#126739=CARTESIAN_POINT('Ctrl Pts',(-10.6430841483886,-67.2337953661514,
61.7172288495922));
#126740=CARTESIAN_POINT('Ctrl Pts',(-10.6772689260462,-67.1063838842474,
61.8077504324841));
#126741=CARTESIAN_POINT('Ctrl Pts',(-10.7122657704729,-66.9765786831478,
61.9036851495562));
#126742=CARTESIAN_POINT('Ctrl Pts',(-10.7465708814531,-66.849339159057,
61.9977236598827));
#126743=CARTESIAN_POINT('Ctrl Pts',(-10.7816562679877,-66.7197994639639,
62.0969635646312));
#126744=CARTESIAN_POINT('Ctrl Pts',(-10.8173430910532,-66.5883473939177,
62.2017966028244));
#126745=CARTESIAN_POINT('Ctrl Pts',(-10.8465046193832,-66.4809311843642,
62.2874610400198));
#126746=CARTESIAN_POINT('Ctrl Pts',(-10.8760675936279,-66.3722386719903,
62.3768607253668));
#126747=CARTESIAN_POINT('Ctrl Pts',(-10.905929980847,-66.2625034493625,
62.4702223439506));
#126748=CARTESIAN_POINT('Ctrl Pts',(-10.9314965512758,-66.1685540515048,
62.5501535423291));
#126749=CARTESIAN_POINT('Ctrl Pts',(-10.9572825668611,-66.0738408708389,
62.6329889654811));
#126750=CARTESIAN_POINT('Ctrl Pts',(-10.9832185102277,-65.9785092162543,
62.7188774816556));
#126751=CARTESIAN_POINT('Ctrl Pts',(-11.026670215868,-65.8187956120613,
62.8627705519772));
#126752=CARTESIAN_POINT('Ctrl Pts',(-11.0705064137141,-65.6573614979089,
63.0151950488345));
#126753=CARTESIAN_POINT('Ctrl Pts',(-11.1143817956528,-65.4951382027885,
63.1767142242415));
#126754=CARTESIAN_POINT('Ctrl Pts',(-11.1560082078672,-65.3412301692834,
63.3299542298881));
#126755=CARTESIAN_POINT('Ctrl Pts',(-11.1976696927773,-65.1866119558448,
63.4913808424263));
#126756=CARTESIAN_POINT('Ctrl Pts',(-11.2390529797762,-65.032118176574,
63.6614748088734));
#126757=CARTESIAN_POINT('Ctrl Pts',(-11.2609077837574,-64.9505289286642,
63.751302624996));
#126758=CARTESIAN_POINT('Ctrl Pts',(-11.282686080715,-64.868981940792,63.8435429374389));
#126759=CARTESIAN_POINT('Ctrl Pts',(-11.3043495221077,-64.7876164372335,
63.9382629119894));
#126760=CARTESIAN_POINT('Ctrl Pts',(-11.3248151405692,-64.7107498248809,
64.0277455950355));
#126761=CARTESIAN_POINT('Ctrl Pts',(-11.3451782345556,-64.6340451386831,
64.1194414174417));
#126762=CARTESIAN_POINT('Ctrl Pts',(-11.3654052810579,-64.5576276447232,
64.2133953716165));
#126763=CARTESIAN_POINT('Ctrl Pts',(-11.3862242573906,-64.478973848284,
64.3100988200467));
#126764=CARTESIAN_POINT('Ctrl Pts',(-11.406899835192,-64.4006233060692,
64.4091961323424));
#126765=CARTESIAN_POINT('Ctrl Pts',(-11.4273972521796,-64.3227181963433,
64.5107349606021));
#126766=CARTESIAN_POINT('Ctrl Pts',(-11.4376459606734,-64.2837656414803,
64.5615043747319));
#126767=CARTESIAN_POINT('Ctrl Pts',(-11.4478501704006,-64.2449246102199,
64.612884080549));
#126768=CARTESIAN_POINT('Ctrl Pts',(-11.4580056783908,-64.2062137707468,
64.6648794653407));
#126769=CARTESIAN_POINT('Ctrl Pts',(-11.4630834323859,-64.1868583510102,
64.6908771577365));
#126770=CARTESIAN_POINT('Ctrl Pts',(-11.468149010096,-64.1675354801149,
64.7170287702674));
#126771=CARTESIAN_POINT('Ctrl Pts',(-11.4732018890547,-64.1482475470137,
64.7433349320655));
#126772=CARTESIAN_POINT('Ctrl Pts',(-11.4757283285341,-64.1386035804631,
64.7564880129645));
#126773=CARTESIAN_POINT('Ctrl Pts',(-11.4782515932834,-64.1289683484049,
64.7696797312012));
#126774=CARTESIAN_POINT('Ctrl Pts',(-11.4807716179499,-64.1193421511978,
64.7829101641624));
#126775=CARTESIAN_POINT('Ctrl Pts',(-11.482976639533,-64.1109192286416,
64.7944867930035));
#126776=CARTESIAN_POINT('Ctrl Pts',(-11.4851791804248,-64.1025032233963,
64.8060930628069));
#126777=CARTESIAN_POINT('Ctrl Pts',(-11.487379196887,-64.094094337761,64.8177290245631));
#126778=CARTESIAN_POINT('Ctrl Pts',(-11.487693484953,-64.0928930683846,
64.819391304814));
#126779=CARTESIAN_POINT('Ctrl Pts',(-11.4877849049776,-64.0925436650061,
64.8198744603236));
#126780=CARTESIAN_POINT('Ctrl Pts',(-11.4883219064042,-64.0904909661437,
64.822717683314));
#126781=CARTESIAN_POINT('Ctrl Pts',(-11.5258190563035,-63.9471573488824,
65.0212511571591));
#126782=CARTESIAN_POINT('Ctrl Pts',(-11.5609964063703,-63.8111425419701,
65.2209281352053));
#126783=CARTESIAN_POINT('Ctrl Pts',(-11.594015105858,-63.6821643659619,
65.4211892538843));
#126784=CARTESIAN_POINT('Ctrl Pts',(-11.6274131721106,-63.5517043013831,
65.6237512630868));
#126785=CARTESIAN_POINT('Ctrl Pts',(-11.6586031518168,-63.4284436783251,
65.8269094954421));
#126786=CARTESIAN_POINT('Ctrl Pts',(-11.6877753102132,-63.312096759407,
66.0300444814576));
#126787=CARTESIAN_POINT('Ctrl Pts',(-11.7174950675559,-63.1935658591276,
66.2369925725164));
#126788=CARTESIAN_POINT('Ctrl Pts',(-11.7451206692197,-63.0822108218853,
66.4439166065601));
#126789=CARTESIAN_POINT('Ctrl Pts',(-11.7708581256066,-62.9777293233036,
66.6502154332417));
#126790=CARTESIAN_POINT('Ctrl Pts',(-11.7801202228301,-62.9401297336867,
66.7244558617095));
#126791=CARTESIAN_POINT('Ctrl Pts',(-11.7891378310711,-62.9034202902373,
66.7986158159301));
#126792=CARTESIAN_POINT('Ctrl Pts',(-11.7979206601765,-62.8675868429193,
66.8726689124244));
#126793=CARTESIAN_POINT('Ctrl Pts',(-11.8039223096278,-62.8431004517058,
66.9232722795869));
#126794=CARTESIAN_POINT('Ctrl Pts',(-11.8098143307674,-62.8190231075782,
66.973825761044));
#126795=CARTESIAN_POINT('Ctrl Pts',(-11.8156000723212,-62.7953502204353,
67.0243199683128));
#126796=CARTESIAN_POINT('Ctrl Pts',(-11.8366325561611,-62.7092939022176,
67.2078778732972));
#126797=CARTESIAN_POINT('Ctrl Pts',(-11.856262485958,-62.6285637495704,
67.3906826664573));
#126798=CARTESIAN_POINT('Ctrl Pts',(-11.8745953081227,-62.5528590078558,
67.5723776005199));
#126799=CARTESIAN_POINT('Ctrl Pts',(-11.8934193020411,-62.4751259897296,
67.7589404931876));
#126800=CARTESIAN_POINT('Ctrl Pts',(-11.9108757973575,-62.4026912023522,
67.9443333953572));
#126801=CARTESIAN_POINT('Ctrl Pts',(-11.9270787481793,-62.3352376974856,
68.128224202014));
#126802=CARTESIAN_POINT('Ctrl Pts',(-11.9310492584917,-62.3187083109794,
68.1732863855755));
#126803=CARTESIAN_POINT('Ctrl Pts',(-11.9349444923878,-62.3024780870216,
68.2182586128735));
#126804=CARTESIAN_POINT('Ctrl Pts',(-11.9387661208648,-62.2865424453986,
68.2631364596983));
#126805=CARTESIAN_POINT('Ctrl Pts',(-11.9542469369982,-62.2219896665453,
68.4449295616027));
#126806=CARTESIAN_POINT('Ctrl Pts',(-11.9685202013225,-62.1622697499585,
68.6251697788815));
#126807=CARTESIAN_POINT('Ctrl Pts',(-11.9817054877579,-62.1070691003341,
68.8035570717619));
#126808=CARTESIAN_POINT('Ctrl Pts',(-11.9905306773405,-62.070122144316,
68.9229554395179));
#126809=CARTESIAN_POINT('Ctrl Pts',(-11.9988683951492,-62.0352000449545,
69.0415248418523));
#126810=CARTESIAN_POINT('Ctrl Pts',(-12.0067537158868,-62.0022120194877,
69.1591878279127));
#126811=CARTESIAN_POINT('Ctrl Pts',(-12.0165282381559,-61.9613205706461,
69.3050410551654));
#126812=CARTESIAN_POINT('Ctrl Pts',(-12.0256045901432,-61.9233962069462,
69.4495053598849));
#126813=CARTESIAN_POINT('Ctrl Pts',(-12.0340260667932,-61.8882498965005,
69.5924495455297));
#126814=CARTESIAN_POINT('Ctrl Pts',(-12.0443085686483,-61.845336756991,
69.7669823400919));
#126815=CARTESIAN_POINT('Ctrl Pts',(-12.053615002802,-61.8065643760454,
69.9392473392475));
#126816=CARTESIAN_POINT('Ctrl Pts',(-12.0620297563089,-61.7715807855154,
70.1090179180091));
#126817=CARTESIAN_POINT('Ctrl Pts',(-12.0707293734922,-61.7354128995448,
70.2845357205214));
#126818=CARTESIAN_POINT('Ctrl Pts',(-12.0784759221661,-61.7032945687419,
70.457387502534));
#126819=CARTESIAN_POINT('Ctrl Pts',(-12.0853584309557,-61.6748564071382,
70.6273760230889));
#126820=CARTESIAN_POINT('Ctrl Pts',(-12.0912109139692,-61.650674257459,
70.7719243207282));
#126821=CARTESIAN_POINT('Ctrl Pts',(-12.096438548449,-61.6291535020079,
70.9144032875922));
#126822=CARTESIAN_POINT('Ctrl Pts',(-12.1010937813383,-61.6100782623838,
71.0547188720989));
#126823=CARTESIAN_POINT('Ctrl Pts',(-12.101742421823,-61.607420399078,71.07426985288));
#126824=CARTESIAN_POINT('Ctrl Pts',(-12.1023799462569,-61.604810030352,
71.0937788696004));
#126825=CARTESIAN_POINT('Ctrl Pts',(-12.1030065055343,-61.6022465427781,
71.1132456782365));
#126826=CARTESIAN_POINT('Ctrl Pts',(-12.1084457844721,-61.5799924249766,
71.2822407055606));
#126827=CARTESIAN_POINT('Ctrl Pts',(-12.1130528169592,-61.5612642377236,
71.4480414148776));
#126828=CARTESIAN_POINT('Ctrl Pts',(-12.116911318386,-61.5456656243764,
71.6104912946339));
#126829=CARTESIAN_POINT('Ctrl Pts',(-12.1200457784369,-61.5329940648827,
71.7424577246135));
#126830=CARTESIAN_POINT('Ctrl Pts',(-12.1226861568724,-61.5223882620892,
71.87221393459));
#126831=CARTESIAN_POINT('Ctrl Pts',(-12.1248747923724,-61.513648042856,
71.9996978758656));
#126832=CARTESIAN_POINT('Ctrl Pts',(-12.1273162086756,-61.5038983546462,
72.1419058280955));
#126833=CARTESIAN_POINT('Ctrl Pts',(-12.1291916676191,-61.4964661468903,
72.2812835408876));
#126834=CARTESIAN_POINT('Ctrl Pts',(-12.1305459358192,-61.4910776631597,
72.4177568917541));
#126835=CARTESIAN_POINT('Ctrl Pts',(-12.1311089653444,-61.488837430807,
72.474494933694));
#126836=CARTESIAN_POINT('Ctrl Pts',(-12.1315818513851,-61.4869505975996,
72.5307311892445));
#126837=CARTESIAN_POINT('Ctrl Pts',(-12.1319676597541,-61.4853982272355,
72.5864611708658));
#126838=CARTESIAN_POINT('Ctrl Pts',(-12.1320458483712,-61.4850836210691,
72.5977555090442));
#126839=CARTESIAN_POINT('Ctrl Pts',(-12.1321204603002,-61.4847827532277,
72.6090290559099));
#126840=CARTESIAN_POINT('Ctrl Pts',(-12.1321915229297,-61.484495458529,
72.6202817765625));
#126841=CARTESIAN_POINT('Ctrl Pts',(-12.1324023774452,-61.4836430078827,
72.6536704504152));
#126842=CARTESIAN_POINT('Ctrl Pts',(-12.1325820021325,-61.482910069771,
72.6868757439766));
#126843=CARTESIAN_POINT('Ctrl Pts',(-12.1327311936757,-61.4822924708232,
72.7198968084425));
#126844=CARTESIAN_POINT('Ctrl Pts',(-12.1328457263696,-61.481818346957,
72.7452467135941));
#126845=CARTESIAN_POINT('Ctrl Pts',(-12.1329392063142,-61.4814268389799,
72.7695145227435));
#126846=CARTESIAN_POINT('Ctrl Pts',(-12.1330192927011,-61.4810814594443,
72.7949419211735));
#126847=CARTESIAN_POINT('Ctrl Pts',(-12.1330435277201,-61.480976943809,
72.8026365308037));
#126848=CARTESIAN_POINT('Ctrl Pts',(-12.1330664824746,-61.4808770019494,
72.8104373358324));
#126849=CARTESIAN_POINT('Ctrl Pts',(-12.1330882249236,-61.4807815611221,
72.8184064724661));
#126850=CARTESIAN_POINT('Ctrl Pts',(-12.1335198815254,-61.4788867578659,
72.9766191208087));
#126851=CARTESIAN_POINT('Ctrl Pts',(-12.1332896604181,-61.4795152831409,
73.1386795008977));
#126852=CARTESIAN_POINT('Ctrl Pts',(-12.1323239957528,-61.4830694277461,
73.3045108131254));
#126853=CARTESIAN_POINT('Ctrl Pts',(-12.1313891342929,-61.4865102006496,
73.4650523636382));
#126854=CARTESIAN_POINT('Ctrl Pts',(-12.1297650083798,-61.4926929857708,
73.6291282763541));
#126855=CARTESIAN_POINT('Ctrl Pts',(-12.1273794940025,-61.5020097389348,
73.7966288939179));
#126856=CARTESIAN_POINT('Ctrl Pts',(-12.1259968230349,-61.5074098338727,
73.8937141360713));
#126857=CARTESIAN_POINT('Ctrl Pts',(-12.1243582631598,-61.5138632821912,
73.9919491456346));
#126858=CARTESIAN_POINT('Ctrl Pts',(-12.1224488799031,-61.5214506542386,
74.0913057436497));
#126859=CARTESIAN_POINT('Ctrl Pts',(-12.1192505880294,-61.5341598001248,
74.2577319437944));
#126860=CARTESIAN_POINT('Ctrl Pts',(-12.1152925857901,-61.5500496941281,
74.4273073862083));
#126861=CARTESIAN_POINT('Ctrl Pts',(-12.1105082832172,-61.5694865436168,
74.5998752133286));
#126862=CARTESIAN_POINT('Ctrl Pts',(-12.1058412023223,-61.5884471648407,
74.7682149027085));
#126863=CARTESIAN_POINT('Ctrl Pts',(-12.1003894003114,-61.6107843636321,
74.9394029220836));
#126864=CARTESIAN_POINT('Ctrl Pts',(-12.094069497973,-61.6368433161217,
75.1132814589855));
#126865=CARTESIAN_POINT('Ctrl Pts',(-12.0890393747711,-61.6575841020577,
75.2516744935554));
#126866=CARTESIAN_POINT('Ctrl Pts',(-12.0834592429624,-61.680682966408,
75.3917711999041));
#126867=CARTESIAN_POINT('Ctrl Pts',(-12.0772848465946,-61.7063238630825,
75.5334705951441));
#126868=CARTESIAN_POINT('Ctrl Pts',(-12.0695748590907,-61.7383417286644,
75.7104110605041));
#126869=CARTESIAN_POINT('Ctrl Pts',(-12.0609382481766,-61.7743231686574,
75.8898518990448));
#126870=CARTESIAN_POINT('Ctrl Pts',(-12.0512938757378,-61.8146144057835,
76.0715772112131));
#126871=CARTESIAN_POINT('Ctrl Pts',(-12.0416495032989,-61.8549056429096,
76.2533025233813));
#126872=CARTESIAN_POINT('Ctrl Pts',(-12.0309973732903,-61.8995066938939,
76.4373127173123));
#126873=CARTESIAN_POINT('Ctrl Pts',(-12.0192532062723,-61.9487789363498,
76.6233402471264));
#126874=CARTESIAN_POINT('Ctrl Pts',(-12.0119610900703,-61.9793727551339,
76.7388473207304));
#126875=CARTESIAN_POINT('Ctrl Pts',(-12.0042493416637,-62.0117709110583,
76.8551362886535));
#126876=CARTESIAN_POINT('Ctrl Pts',(-11.9960865951416,-62.04605383537,76.9721351064428));
#126877=CARTESIAN_POINT('Ctrl Pts',(-11.983203031392,-62.1001638386265,
77.1567986536362));
#126878=CARTESIAN_POINT('Ctrl Pts',(-11.9691959878891,-62.158968700625,
77.3432328300292));
#126879=CARTESIAN_POINT('Ctrl Pts',(-11.953950818084,-62.2227705709226,
77.5311535277543));
#126880=CARTESIAN_POINT('Ctrl Pts',(-11.9391675825026,-62.2846392212027,
77.7133801595713));
#126881=CARTESIAN_POINT('Ctrl Pts',(-11.9232200992943,-62.3512067118891,
77.8970046933264));
#126882=CARTESIAN_POINT('Ctrl Pts',(-11.9060019391879,-62.4227585422542,
78.0817208074706));
#126883=CARTESIAN_POINT('Ctrl Pts',(-11.8924848796091,-62.47893006976,78.2267315812477));
#126884=CARTESIAN_POINT('Ctrl Pts',(-11.8781846626541,-62.5381736325303,
78.3724142381549));
#126885=CARTESIAN_POINT('Ctrl Pts',(-11.8630490617186,-62.6006315321448,
78.518598370791));
#126886=CARTESIAN_POINT('Ctrl Pts',(-11.8527079585239,-62.6433046699995,
78.6184758191628));
#126887=CARTESIAN_POINT('Ctrl Pts',(-11.8419768601538,-62.6874783657934,
78.7185868613273));
#126888=CARTESIAN_POINT('Ctrl Pts',(-11.8308411848522,-62.7331971715572,
78.8188816475872));
#126889=CARTESIAN_POINT('Ctrl Pts',(-11.8088680429328,-62.8234104527664,
79.0167853680701));
#126890=CARTESIAN_POINT('Ctrl Pts',(-11.7853100432508,-62.9196242385598,
79.2153970823566));
#126891=CARTESIAN_POINT('Ctrl Pts',(-11.7600015537594,-63.0221098479846,
79.4142611496952));
#126892=CARTESIAN_POINT('Ctrl Pts',(-11.7374125321294,-63.1135830925194,
79.5917567177362));
#126893=CARTESIAN_POINT('Ctrl Pts',(-11.7134289650972,-63.2100527378074,
79.7694528166375));
#126894=CARTESIAN_POINT('Ctrl Pts',(-11.6879340427069,-63.3117149837188,
79.946990504635));
#126895=CARTESIAN_POINT('Ctrl Pts',(-11.6776109810424,-63.3528786953563,
80.0188766815338));
#126896=CARTESIAN_POINT('Ctrl Pts',(-11.6670390543325,-63.3948936216669,
80.0907377515338));
#126897=CARTESIAN_POINT('Ctrl Pts',(-11.6562097610406,-63.4377703728835,
80.162545776049));
#126898=CARTESIAN_POINT('Ctrl Pts',(-11.6386839781394,-63.507160739649,
80.2787575928594));
#126899=CARTESIAN_POINT('Ctrl Pts',(-11.6204840638948,-63.5788083395828,
80.3948305815524));
#126900=CARTESIAN_POINT('Ctrl Pts',(-11.6015778893442,-63.6527581555802,
80.510661085996));
#126901=CARTESIAN_POINT('Ctrl Pts',(-11.5862836790107,-63.712580095601,
80.6043625428008));
#126902=CARTESIAN_POINT('Ctrl Pts',(-11.5705275262936,-63.7739076751408,
80.6979037327157));
#126903=CARTESIAN_POINT('Ctrl Pts',(-11.5542930734213,-63.8367611427316,
80.7912243017232));
#126904=CARTESIAN_POINT('Ctrl Pts',(-11.5461758469852,-63.868187876527,
80.837884586227));
#126905=CARTESIAN_POINT('Ctrl Pts',(-11.5379390457412,-63.8999960821772,
80.8844897138579));
#126906=CARTESIAN_POINT('Ctrl Pts',(-11.5295806409392,-63.9321880788289,
80.9310318791045));
#126907=CARTESIAN_POINT('Ctrl Pts',(-11.5254014385383,-63.9482840771547,
80.9543029617278));
#126908=CARTESIAN_POINT('Ctrl Pts',(-11.5211918353313,-63.9644760231451,
80.9775583038081));
#126909=CARTESIAN_POINT('Ctrl Pts',(-11.5169515785101,-63.9807642000307,
81.0007969225799));
#126910=CARTESIAN_POINT('Ctrl Pts',(-11.5148314500995,-63.9889082884735,
81.0124162319659));
#126911=CARTESIAN_POINT('Ctrl Pts',(-11.5127036582898,-63.9970764346354,
81.0240313605289));
#126912=CARTESIAN_POINT('Ctrl Pts',(-11.5105681715546,-64.0052686731633,
81.0356421845783));
#126913=CARTESIAN_POINT('Ctrl Pts',(-11.5089665565033,-64.0114128520592,
81.0443503026154));
#126914=CARTESIAN_POINT('Ctrl Pts',(-11.5073606130567,-64.0175705829106,
81.053055999364));
#126915=CARTESIAN_POINT('Ctrl Pts',(-11.5057503279326,-64.0237418801664,
81.0617592224612));
#126916=CARTESIAN_POINT('Ctrl Pts',(-11.5052135662245,-64.0257989792517,
81.0646602968269));
#126917=CARTESIAN_POINT('Ctrl Pts',(-11.5044589032026,-64.0286905507612,
81.0687338632904));
#126918=CARTESIAN_POINT('Ctrl Pts',(-11.5041385950919,-64.0299177000775,
81.0704616190519));
#126919=CARTESIAN_POINT('Ctrl Pts',(-11.4693282359868,-64.1632815049607,
81.2582301971615));
#126920=CARTESIAN_POINT('Ctrl Pts',(-11.4338224094827,-64.2984486344061,
81.4383197181533));
#126921=CARTESIAN_POINT('Ctrl Pts',(-11.3978475310335,-64.4346583969914,
81.6109610394162));
#126922=CARTESIAN_POINT('Ctrl Pts',(-11.3818221835758,-64.4953343149279,
81.687865737307));
#126923=CARTESIAN_POINT('Ctrl Pts',(-11.365703592804,-64.5562176505651,
81.7632928978732));
#126924=CARTESIAN_POINT('Ctrl Pts',(-11.3495109701921,-64.6172436488808,
81.8372649522619));
#126925=CARTESIAN_POINT('Ctrl Pts',(-11.3088630152425,-64.7704357592468,
82.0229552389044));
#126926=CARTESIAN_POINT('Ctrl Pts',(-11.2677500849922,-64.9245238729807,
82.1994752984627));
#126927=CARTESIAN_POINT('Ctrl Pts',(-11.2264661430999,-65.0785573569255,
82.3672898262114));
#126928=CARTESIAN_POINT('Ctrl Pts',(-11.1844002383752,-65.2355084028539,
82.5382829439258));
#126929=CARTESIAN_POINT('Ctrl Pts',(-11.1421568545417,-65.3924027172242,
82.7002380132411));
#126930=CARTESIAN_POINT('Ctrl Pts',(-11.1000240148836,-65.548281736956,
82.8536621198914));
#126931=CARTESIAN_POINT('Ctrl Pts',(-11.0627471787476,-65.6861949828407,
82.9894033927163));
#126932=CARTESIAN_POINT('Ctrl Pts',(-11.0255565497497,-65.8233142083913,
83.1184672839319));
#126933=CARTESIAN_POINT('Ctrl Pts',(-10.9886364195613,-65.9590053830707,
83.2412108269353));
#126934=CARTESIAN_POINT('Ctrl Pts',(-10.966306089561,-66.0410752103776,
83.3154495635453));
#126935=CARTESIAN_POINT('Ctrl Pts',(-10.9440995863303,-66.1226383441794,
83.3873692256676));
#126936=CARTESIAN_POINT('Ctrl Pts',(-10.9220620077695,-66.2035972621863,
83.4570689492617));
#126937=CARTESIAN_POINT('Ctrl Pts',(-10.8850013345343,-66.3397461588291,
83.5742832191318));
#126938=CARTESIAN_POINT('Ctrl Pts',(-10.8484188681295,-66.4741832051189,
83.6852208513242));
#126939=CARTESIAN_POINT('Ctrl Pts',(-10.8125103570658,-66.6064494670023,
83.790334502538));
#126940=CARTESIAN_POINT('Ctrl Pts',(-10.7771834166723,-66.7365735576764,
83.8937457435215));
#126941=CARTESIAN_POINT('Ctrl Pts',(-10.7425087210743,-66.8645970764474,
83.9915201052581));
#126942=CARTESIAN_POINT('Ctrl Pts',(-10.7086632572777,-66.9901294897027,
84.0840601625485));
#126943=CARTESIAN_POINT('Ctrl Pts',(-10.6739820207459,-67.1187617738597,
84.1788853844699));
#126944=CARTESIAN_POINT('Ctrl Pts',(-10.6401714806484,-67.2447785203136,
84.2682147686759));
#126945=CARTESIAN_POINT('Ctrl Pts',(-10.6074124011771,-67.3678047457111,
84.3524499440023));
#126946=CARTESIAN_POINT('Ctrl Pts',(-10.5746533217058,-67.4908309711085,
84.4366851193286));
#126947=CARTESIAN_POINT('Ctrl Pts',(-10.5429456614745,-67.6108669255703,
84.5158261086302));
#126948=CARTESIAN_POINT('Ctrl Pts',(-10.5124609685256,-67.727579221203,
84.5902421548952));
#126949=CARTESIAN_POINT('Ctrl Pts',(-7.03190132271491,-64.48874263761,58.19041163036));
#126950=CARTESIAN_POINT('Ctrl Pts',(-6.87538499698691,-65.23521415548,57.82043934767));
#126951=CARTESIAN_POINT('Ctrl Pts',(-6.44219525657191,-67.23717591574,57.00605633762));
#126952=CARTESIAN_POINT('Ctrl Pts',(-5.81802729745091,-70.88052909333,56.2001657272));
#126953=CARTESIAN_POINT('Ctrl Pts',(-5.65466277349091,-73.83365375479,56.02303478332));
#126954=CARTESIAN_POINT('Ctrl Pts',(-5.66377280622291,-75.2425631386,56.03448007742));
#126955=CARTESIAN_POINT('Ctrl Pts',(-7.61748996822491,-65.7164492576301,
59.80517843096));
#126956=CARTESIAN_POINT('Ctrl Pts',(-7.51101325256191,-66.3834691039,59.4773126071101));
#126957=CARTESIAN_POINT('Ctrl Pts',(-7.21262838267092,-68.16429015863,58.75816291855));
#126958=CARTESIAN_POINT('Ctrl Pts',(-6.77170455789591,-71.37723474796,58.04355709918));
#126959=CARTESIAN_POINT('Ctrl Pts',(-6.65471882509291,-73.97423010814,57.88507987323));
#126960=CARTESIAN_POINT('Ctrl Pts',(-6.66121085611991,-75.21333331973,57.8952394617801));
#126961=CARTESIAN_POINT('Ctrl Pts',(-8.94180688412191,-66.85948039078,60.9872761331401));
#126962=CARTESIAN_POINT('Ctrl Pts',(-8.87314531440391,-67.46383081509,60.6774497334101));
#126963=CARTESIAN_POINT('Ctrl Pts',(-8.67972634156291,-69.0582366384701,
60.0041732311799));
#126964=CARTESIAN_POINT('Ctrl Pts',(-8.39095292952791,-71.86723579451,59.34163138087));
#126965=CARTESIAN_POINT('Ctrl Pts',(-8.31392057053391,-74.11277277759,59.19423894577));
#126966=CARTESIAN_POINT('Ctrl Pts',(-8.31818721880991,-75.18451754242,59.20357135831));
#126967=CARTESIAN_POINT('Ctrl Pts',(-10.7849809204589,-67.72806305548,61.54044568591));
#126968=CARTESIAN_POINT('Ctrl Pts',(-10.7356317320139,-68.29693106613,61.22159666065));
#126969=CARTESIAN_POINT('Ctrl Pts',(-10.5999126060329,-69.77059692297,60.53721706415));
#126970=CARTESIAN_POINT('Ctrl Pts',(-10.4069349481069,-72.2691792786301,
59.87887438407));
#126971=CARTESIAN_POINT('Ctrl Pts',(-10.3567972434249,-74.22628006642,59.73315744833));
#126972=CARTESIAN_POINT('Ctrl Pts',(-10.3596005994849,-75.1608999773,59.74225854723));
#126973=CARTESIAN_POINT('',(-9.07718749353492,-75.0000704107034,59.2746757745282));
#126974=CARTESIAN_POINT('Origin',(-12.2732112378679,-75.0025912594184,52.4899004903005));
#126975=CARTESIAN_POINT('Ctrl Pts',(-9.07715892555361,-75.0000703914058,
59.2747363757385));
#126976=CARTESIAN_POINT('Ctrl Pts',(-9.0773127009558,-74.832857148716,59.2747599930608));
#126977=CARTESIAN_POINT('Ctrl Pts',(-9.08051151357833,-74.6670415245432,
59.2778801351493));
#126978=CARTESIAN_POINT('Ctrl Pts',(-9.08649648450185,-74.50288770246,59.2839023726706));
#126979=CARTESIAN_POINT('Ctrl Pts',(-9.0925301261762,-74.3373989549659,
59.2899735840006));
#126980=CARTESIAN_POINT('Ctrl Pts',(-9.10139524577937,-74.1735991368877,
59.2989940519194));
#126981=CARTESIAN_POINT('Ctrl Pts',(-9.11282574947299,-74.011705812419,
59.3107672755481));
#126982=CARTESIAN_POINT('Ctrl Pts',(-9.12433239231336,-73.8487341085611,
59.3226189211978));
#126983=CARTESIAN_POINT('Ctrl Pts',(-9.13843855877331,-73.6876942906821,
59.3372598927645));
#126984=CARTESIAN_POINT('Ctrl Pts',(-9.15487444279722,-73.5287554860593,
59.3544959235967));
#126985=CARTESIAN_POINT('Ctrl Pts',(-9.17153044121632,-73.3676881242626,
59.3719627846353));
#126986=CARTESIAN_POINT('Ctrl Pts',(-9.19057884342498,-73.2087783349392,
59.3920944476079));
#126987=CARTESIAN_POINT('Ctrl Pts',(-9.21174268813516,-73.052149383601,
59.4146985404614));
#126988=CARTESIAN_POINT('Ctrl Pts',(-9.22410816607753,-72.9606352060292,
59.4279055175213));
#126989=CARTESIAN_POINT('Ctrl Pts',(-9.23719588777561,-72.8698986706841,
59.4419567242433));
#126990=CARTESIAN_POINT('Ctrl Pts',(-9.25095145667989,-72.7799564487297,
59.4568157702803));
#126991=CARTESIAN_POINT('Ctrl Pts',(-9.2740752764921,-72.6287589411269,
59.4817945919875));
#126992=CARTESIAN_POINT('Ctrl Pts',(-9.29905722820936,-72.4796871923342,
59.5090536971147));
#126993=CARTESIAN_POINT('Ctrl Pts',(-9.32558888018677,-72.3328475236606,
59.5384048910294));
#126994=CARTESIAN_POINT('Ctrl Pts',(-9.3361553352476,-72.2743673822239,
59.5500942525417));
#126995=CARTESIAN_POINT('Ctrl Pts',(-9.34696763875273,-72.2162406966429,
59.5621155468557));
#126996=CARTESIAN_POINT('Ctrl Pts',(-9.35800653552035,-72.1584719535309,
59.574457351823));
#126997=CARTESIAN_POINT('Ctrl Pts',(-9.38679592664713,-72.0078113417539,
59.6066447214392));
#126998=CARTESIAN_POINT('Ctrl Pts',(-9.41712538814356,-71.8595886590536,
59.6410108307925));
#126999=CARTESIAN_POINT('Ctrl Pts',(-9.44860522972388,-71.7137833374362,
59.6773583586395));
#127000=CARTESIAN_POINT('Ctrl Pts',(-9.48147079396201,-71.5615597580496,
59.715305881606));
#127001=CARTESIAN_POINT('Ctrl Pts',(-9.51559001782784,-71.4119710067821,
59.7554127840311));
#127002=CARTESIAN_POINT('Ctrl Pts',(-9.55053752099497,-71.2649410788004,
59.7974761241889));
#127003=CARTESIAN_POINT('Ctrl Pts',(-9.58548502416211,-71.1179111508188,
59.8395394643468));
#127004=CARTESIAN_POINT('Ctrl Pts',(-9.62126076092705,-70.9734395747625,
59.8835591509684));
#127005=CARTESIAN_POINT('Ctrl Pts',(-9.65745893337754,-70.8314033385646,
59.9293563090885));
#127006=CARTESIAN_POINT('Ctrl Pts',(-9.69745063613198,-70.6744818545821,
59.9799529610892));
#127007=CARTESIAN_POINT('Ctrl Pts',(-9.73787512708575,-70.5205510584211,
60.0326779352948));
#127008=CARTESIAN_POINT('Ctrl Pts',(-9.77836794971244,-70.3696212117005,
60.0873359005608));
#127009=CARTESIAN_POINT('Ctrl Pts',(-9.81980468036516,-70.2151731144741,
60.1432679704398));
#127010=CARTESIAN_POINT('Ctrl Pts',(-9.86131281739014,-70.0638671796215,
60.201224220966));
#127011=CARTESIAN_POINT('Ctrl Pts',(-9.90252777852388,-69.9156655216722,
60.2610014311872));
#127012=CARTESIAN_POINT('Ctrl Pts',(-9.94565783802503,-69.7605775111613,
60.3235562550359));
#127013=CARTESIAN_POINT('Ctrl Pts',(-9.9884666611632,-69.6088886519274,
60.3881052946684));
#127014=CARTESIAN_POINT('Ctrl Pts',(-10.0305673179908,-69.4605073347355,
60.4544214019772));
#127015=CARTESIAN_POINT('Ctrl Pts',(-10.0464816427542,-69.4044182223903,
60.4794893260496));
#127016=CARTESIAN_POINT('Ctrl Pts',(-10.0622950959451,-69.348801273108,
60.5048097923068));
#127017=CARTESIAN_POINT('Ctrl Pts',(-10.0779879145727,-69.2936500306986,
60.5303706686463));
#127018=CARTESIAN_POINT('Ctrl Pts',(-10.0913798922194,-69.2465849225712,
60.5521838745904));
#127019=CARTESIAN_POINT('Ctrl Pts',(-10.1046840277155,-69.1998589447846,
60.5741721611837));
#127020=CARTESIAN_POINT('Ctrl Pts',(-10.1178881125732,-69.1534664352015,
60.5963277239018));
#127021=CARTESIAN_POINT('Ctrl Pts',(-10.1645098311032,-68.9896611774352,
60.6745558192263));
#127022=CARTESIAN_POINT('Ctrl Pts',(-10.20985514067,-68.830019727719,60.7548568087025));
#127023=CARTESIAN_POINT('Ctrl Pts',(-10.2536478639727,-68.674514504205,
60.8369131460621));
#127024=CARTESIAN_POINT('Ctrl Pts',(-10.2976229428249,-68.5183617475314,
60.9193111709755));
#127025=CARTESIAN_POINT('Ctrl Pts',(-10.3400326286217,-68.3663793370692,
61.0034794657588));
#127026=CARTESIAN_POINT('Ctrl Pts',(-10.3806348632554,-68.2185240971467,
61.0890630067659));
#127027=CARTESIAN_POINT('Ctrl Pts',(-10.421394210819,-68.0700967219673,
61.1749777187295));
#127028=CARTESIAN_POINT('Ctrl Pts',(-10.4603322871068,-67.9258281880866,
61.2623188942037));
#127029=CARTESIAN_POINT('Ctrl Pts',(-10.4972393820192,-67.7856650022798,
61.3506897699846));
#127030=CARTESIAN_POINT('Ctrl Pts',(-10.5023538913183,-67.7662414762911,
61.3629360241811));
#127031=CARTESIAN_POINT('Ctrl Pts',(-10.507429450164,-67.7468967778124,
61.37520199055));
#127032=CARTESIAN_POINT('Ctrl Pts',(-10.5124655500624,-67.7276307548579,
61.387486552728));
#127033=CARTESIAN_POINT('Ctrl Pts',(-5.66390799836291,-74.75737804457,56.03434061462));
#127034=CARTESIAN_POINT('Ctrl Pts',(-5.65535142628591,-76.10467861883,56.0232167771601));
#127035=CARTESIAN_POINT('Ctrl Pts',(-5.80770735786591,-79.026938051,56.19025778671));
#127036=CARTESIAN_POINT('Ctrl Pts',(-6.42570231203591,-82.68817021729,56.97863787517));
#127037=CARTESIAN_POINT('Ctrl Pts',(-6.87092180434491,-84.74323712603,57.80972126602));
#127038=CARTESIAN_POINT('Ctrl Pts',(-7.03202708148491,-85.51176293719,58.190648673));
#127039=CARTESIAN_POINT('Ctrl Pts',(-6.66130762481391,-74.78661230242,57.89514017999));
#127040=CARTESIAN_POINT('Ctrl Pts',(-6.65520895153991,-75.97153049077,57.88529641475));
#127041=CARTESIAN_POINT('Ctrl Pts',(-6.76428650217192,-78.54142323843,58.0346527913201));
#127042=CARTESIAN_POINT('Ctrl Pts',(-7.20118434740491,-81.76946793919,58.7339909933601));
#127043=CARTESIAN_POINT('Ctrl Pts',(-7.50797960521091,-83.59728170036,59.46781607306));
#127044=CARTESIAN_POINT('Ctrl Pts',(-7.61757460804891,-84.28400193635,59.8053942113101));
#127045=CARTESIAN_POINT('Ctrl Pts',(-8.31825718332691,-74.8154343473,59.20351517363));
#127046=CARTESIAN_POINT('Ctrl Pts',(-8.31424878828192,-75.84030625732,59.19451804723));
#127047=CARTESIAN_POINT('Ctrl Pts',(-8.38606722527991,-78.06244770262,59.33332269739));
#127048=CARTESIAN_POINT('Ctrl Pts',(-8.67229125102691,-80.88281314368,59.98168293644));
#127049=CARTESIAN_POINT('Ctrl Pts',(-8.87119507621291,-82.5187403495901,
60.66848706106));
#127050=CARTESIAN_POINT('Ctrl Pts',(-8.94186638725491,-83.14093103373,60.98748931569));
#127051=CARTESIAN_POINT('Ctrl Pts',(-10.3596572459539,-74.8390589230501,
59.74223918064));
#127052=CARTESIAN_POINT('Ctrl Pts',(-10.3570244645989,-75.73279276851,59.73351469424));
#127053=CARTESIAN_POINT('Ctrl Pts',(-10.4037890980549,-77.6695346223,59.8706524028));
#127054=CARTESIAN_POINT('Ctrl Pts',(-10.5947786127089,-80.17541503562,60.51456235328));
#127055=CARTESIAN_POINT('Ctrl Pts',(-10.7342367672979,-81.68668075087,61.21238965717));
#127056=CARTESIAN_POINT('Ctrl Pts',(-10.7850333778129,-82.27233159581,61.54067352347));
#127057=CARTESIAN_POINT('',(-10.5124842662009,-82.2724282582398,61.3875276985405));
#127058=CARTESIAN_POINT('Origin',(-13.992064676801,-85.1738977789521,55.4111095407736));
#127059=CARTESIAN_POINT('Ctrl Pts',(-10.5124867527329,-82.2724303312993,
61.3875234280722));
#127060=CARTESIAN_POINT('Ctrl Pts',(-10.4762711011264,-82.1338625944223,
61.2991699968375));
#127061=CARTESIAN_POINT('Ctrl Pts',(-10.438002373032,-81.9912324976581,
61.2117810269455));
#127062=CARTESIAN_POINT('Ctrl Pts',(-10.3978910917222,-81.8444856272407,
61.1257577565632));
#127063=CARTESIAN_POINT('Ctrl Pts',(-10.3579096744694,-81.698213863659,
61.0400129946334));
#127064=CARTESIAN_POINT('Ctrl Pts',(-10.3160974143833,-81.5478516042782,
60.9556248663313));
#127065=CARTESIAN_POINT('Ctrl Pts',(-10.2726971972061,-81.3933546676573,
60.8729533678949));
#127066=CARTESIAN_POINT('Ctrl Pts',(-10.2295936236166,-81.2399137286455,
60.7908469350617));
#127067=CARTESIAN_POINT('Ctrl Pts',(-10.1849235906381,-81.0823940478829,
60.7104334616942));
#127068=CARTESIAN_POINT('Ctrl Pts',(-10.1389615230731,-80.9207673678253,
60.6320326508068));
#127069=CARTESIAN_POINT('Ctrl Pts',(-10.1319059530302,-80.8959562915974,
60.6199974565272));
#127070=CARTESIAN_POINT('Ctrl Pts',(-10.1248200088764,-80.8710484703209,
60.6080096315989));
#127071=CARTESIAN_POINT('Ctrl Pts',(-10.1177047628883,-80.8460438430459,
60.5960702697948));
#127072=CARTESIAN_POINT('Ctrl Pts',(-10.0996785737433,-80.7826956269042,
60.5658223775208));
#127073=CARTESIAN_POINT('Ctrl Pts',(-10.0814646789748,-80.7187301616859,
60.5358871188695));
#127074=CARTESIAN_POINT('Ctrl Pts',(-10.0630950294152,-80.654132126471,
60.5062841964149));
#127075=CARTESIAN_POINT('Ctrl Pts',(-10.0218969588841,-80.5092565041948,
60.4398929850177));
#127076=CARTESIAN_POINT('Ctrl Pts',(-9.97991351415051,-80.3611963072566,
60.3751730647508));
#127077=CARTESIAN_POINT('Ctrl Pts',(-9.93751558889771,-80.2098428202604,
60.3123409636049));
#127078=CARTESIAN_POINT('Ctrl Pts',(-9.89646762773618,-80.0633084788077,
60.2515094575311));
#127079=CARTESIAN_POINT('Ctrl Pts',(-9.85503123342581,-79.9136868150178,
60.1924473470377));
#127080=CARTESIAN_POINT('Ctrl Pts',(-9.81356958142742,-79.7609190158336,
60.1353567984347));
#127081=CARTESIAN_POINT('Ctrl Pts',(-9.77350619410377,-79.613303201839,
60.0801915879097));
#127082=CARTESIAN_POINT('Ctrl Pts',(-9.73341937574205,-79.4627496238593,
60.0268671777777));
#127083=CARTESIAN_POINT('Ctrl Pts',(-9.69366035730599,-79.3092477597733,
59.975572340852));
#127084=CARTESIAN_POINT('Ctrl Pts',(-9.68152659738807,-79.2624016644964,
59.9599180500579));
#127085=CARTESIAN_POINT('Ctrl Pts',(-9.66942352908825,-79.2152812982283,
59.944452833371));
#127086=CARTESIAN_POINT('Ctrl Pts',(-9.65736155610982,-79.1678872397631,
59.9291821806378));
#127087=CARTESIAN_POINT('Ctrl Pts',(-9.62201461612017,-79.0290015911687,
59.8844323833426));
#127088=CARTESIAN_POINT('Ctrl Pts',(-9.58703968796021,-78.8878078118406,
59.8413703728143));
#127089=CARTESIAN_POINT('Ctrl Pts',(-9.55282750996213,-78.7441854699933,
59.800166502298));
#127090=CARTESIAN_POINT('Ctrl Pts',(-9.5191756918907,-78.6029155128712,
59.7596375083668));
#127091=CARTESIAN_POINT('Ctrl Pts',(-9.48626192830372,-78.4592955945563,
59.7209064168299));
#127092=CARTESIAN_POINT('Ctrl Pts',(-9.45447515147843,-78.3132529060324,
59.6841568027735));
#127093=CARTESIAN_POINT('Ctrl Pts',(-9.42327095192074,-78.1698868383845,
59.6480807231828));
#127094=CARTESIAN_POINT('Ctrl Pts',(-9.39315293618557,-78.0241857785365,
59.6139143499317));
#127095=CARTESIAN_POINT('Ctrl Pts',(-9.36450404991878,-77.8761252320951,
59.5818497633476));
#127096=CARTESIAN_POINT('Ctrl Pts',(-9.35417346630618,-77.8227356573488,
59.5702875026152));
#127097=CARTESIAN_POINT('Ctrl Pts',(-9.34403404331903,-77.7690397248902,
59.558998692747));
#127098=CARTESIAN_POINT('Ctrl Pts',(-9.33410417244265,-77.7150378179831,
59.547992859992));
#127099=CARTESIAN_POINT('Ctrl Pts',(-9.30747413422574,-77.5702149031008,
59.5184772952358));
#127100=CARTESIAN_POINT('Ctrl Pts',(-9.28235096974286,-77.4231876848988,
59.4909962251838));
#127101=CARTESIAN_POINT('Ctrl Pts',(-9.25904243547962,-77.2740527153528,
59.4657370725323));
#127102=CARTESIAN_POINT('Ctrl Pts',(-9.25620601913232,-77.2559044757081,
59.4626632853653));
#127103=CARTESIAN_POINT('Ctrl Pts',(-9.25339647976746,-77.2377250856647,
59.459622413244));
#127104=CARTESIAN_POINT('Ctrl Pts',(-9.25061437593473,-77.2195147713465,
59.4566148033186));
#127105=CARTESIAN_POINT('Ctrl Pts',(-9.22695626991347,-77.0646601818987,
59.4310390668385));
#127106=CARTESIAN_POINT('Ctrl Pts',(-9.20528666567254,-76.9074701121915,
59.407860857459));
#127107=CARTESIAN_POINT('Ctrl Pts',(-9.18587873902337,-76.7480308556771,
59.3872658982294));
#127108=CARTESIAN_POINT('Ctrl Pts',(-9.16679394018577,-76.5912461463984,
59.3670138300373));
#127109=CARTESIAN_POINT('Ctrl Pts',(-9.14989624892856,-76.4322864143346,
59.3492599343375));
#127110=CARTESIAN_POINT('Ctrl Pts',(-9.13545003206928,-76.2712822983254,
59.334193112631));
#127111=CARTESIAN_POINT('Ctrl Pts',(-9.12111676305156,-76.1115369940565,
59.3192440909692));
#127112=CARTESIAN_POINT('Ctrl Pts',(-9.10919691016474,-75.9497790199847,
59.3069405025098));
#127113=CARTESIAN_POINT('Ctrl Pts',(-9.09995150671631,-75.7861860647748,
59.2974758526382));
#127114=CARTESIAN_POINT('Ctrl Pts',(-9.09078434628428,-75.6239775820057,
59.2880913012457));
#127115=CARTESIAN_POINT('Ctrl Pts',(-9.08424670897293,-75.4599649789326,
59.2814980596483));
#127116=CARTESIAN_POINT('Ctrl Pts',(-9.0805937999134,-75.2943723586259,
59.2778904338773));
#127117=CARTESIAN_POINT('Ctrl Pts',(-9.07844141775526,-75.1968011911922,
59.2757647337254));
#127118=CARTESIAN_POINT('Ctrl Pts',(-9.07729057504939,-75.0986824358921,
59.2746756866574));
#127119=CARTESIAN_POINT('Ctrl Pts',(-9.07719325348405,-75.0000704146066,
59.2746634980018));
#127120=CARTESIAN_POINT('Ctrl Pts',(-6.95501045707591,-85.1529137311,58.01387408059));
#127121=CARTESIAN_POINT('Ctrl Pts',(-7.05774004267591,-85.63125128373,58.24814136492));
#127122=CARTESIAN_POINT('Ctrl Pts',(-7.30909908298691,-86.71753851572,58.83656145538));
#127123=CARTESIAN_POINT('Ctrl Pts',(-7.70408428485791,-88.18560403961,59.83257430806));
#127124=CARTESIAN_POINT('Ctrl Pts',(-7.99155039204292,-89.1287412301401,
60.6313043667));
#127125=CARTESIAN_POINT('Ctrl Pts',(-8.11817253279791,-89.52581262105,61.00177960564));
#127126=CARTESIAN_POINT('Ctrl Pts',(-7.61082803413691,-83.8733505902,59.77519556645));
#127127=CARTESIAN_POINT('Ctrl Pts',(-7.68132640632891,-84.29308008815,59.97887993217));
#127128=CARTESIAN_POINT('Ctrl Pts',(-7.85394933178791,-85.24759038451,60.490155777));
#127129=CARTESIAN_POINT('Ctrl Pts',(-8.12583286142491,-86.5433442491299,
61.3549613678501));
#127130=CARTESIAN_POINT('Ctrl Pts',(-8.32426658251891,-87.38107274318,62.04914416167));
#127131=CARTESIAN_POINT('Ctrl Pts',(-8.41178668367091,-87.73491510949,62.37149197426));
#127132=CARTESIAN_POINT('Ctrl Pts',(-9.10619475060691,-82.69410558745,61.0173249886));
#127133=CARTESIAN_POINT('Ctrl Pts',(-9.15027307656091,-83.0587530577401,
61.20050989027));
#127134=CARTESIAN_POINT('Ctrl Pts',(-9.25823067031591,-83.88877557576,61.65978326684));
#127135=CARTESIAN_POINT('Ctrl Pts',(-9.42839777627291,-85.01925517755,62.43508999421));
#127136=CARTESIAN_POINT('Ctrl Pts',(-9.55271238964991,-85.7537033340401,
63.057206833302));
#127137=CARTESIAN_POINT('Ctrl Pts',(-9.60756611401691,-86.06469941247,63.346234090372));
#127138=CARTESIAN_POINT('Ctrl Pts',(-11.1563436524369,-81.83974571622,61.5037200941));
#127139=CARTESIAN_POINT('Ctrl Pts',(-11.1848443441729,-82.16332661371,61.68039275776));
#127140=CARTESIAN_POINT('Ctrl Pts',(-11.2545217931519,-82.89985707379,62.12270842198));
#127141=CARTESIAN_POINT('Ctrl Pts',(-11.3637278730099,-83.90357345901,62.86726820837));
#127142=CARTESIAN_POINT('Ctrl Pts',(-11.4429513703819,-84.55653760648,63.463524128386));
#127143=CARTESIAN_POINT('Ctrl Pts',(-11.4777951321979,-84.83322947472,63.740383029282));
#127144=CARTESIAN_POINT('',(-11.2183622024927,-84.8936594351933,63.5797742587981));
#127145=CARTESIAN_POINT('Origin',(-15.266749813004,-89.0000231752399,58.784173264979));
#127146=CARTESIAN_POINT('Ctrl Pts',(-11.2183618829509,-84.89365911108,63.579774637322));
#127147=CARTESIAN_POINT('Ctrl Pts',(-11.1916862812499,-84.79459105882,63.472429641703));
#127148=CARTESIAN_POINT('Ctrl Pts',(-11.1374145693669,-84.59364149351,63.261778406171));
#127149=CARTESIAN_POINT('Ctrl Pts',(-11.0534807578479,-84.28415018161,62.95789841798));
#127150=CARTESIAN_POINT('Ctrl Pts',(-10.9672526777759,-83.96690341805,62.66606616824));
#127151=CARTESIAN_POINT('Ctrl Pts',(-10.8789867581169,-83.64220144843,62.38623331845));
#127152=CARTESIAN_POINT('Ctrl Pts',(-10.7889753777679,-83.31030668945,62.11833551683));
#127153=CARTESIAN_POINT('Ctrl Pts',(-10.6976076698479,-82.97144101564,61.86230947727));
#127154=CARTESIAN_POINT('Ctrl Pts',(-10.6052835128899,-82.62579823329,61.61807691418));
#127155=CARTESIAN_POINT('Ctrl Pts',(-10.5434296705349,-82.39092106547,61.46307272833));
#127156=CARTESIAN_POINT('Ctrl Pts',(-10.5124834373569,-82.27242756722,61.38752912203));
#127157=CARTESIAN_POINT('Ctrl Pts',(-8.06612779774991,-89.12550208689,60.88625533387));
#127158=CARTESIAN_POINT('Ctrl Pts',(-8.09637982822591,-89.23409807329,60.9678095002));
#127159=CARTESIAN_POINT('Ctrl Pts',(-8.20385936829092,-89.63416343301,61.28679075656));
#127160=CARTESIAN_POINT('Ctrl Pts',(-8.35457669863391,-90.30389549261,61.94147242306));
#127161=CARTESIAN_POINT('Ctrl Pts',(-8.4646874159229,-91.0756228145,62.9334803921));
#127162=CARTESIAN_POINT('Ctrl Pts',(-8.49068670939391,-91.7484865399,64.060395809805));
#127163=CARTESIAN_POINT('Ctrl Pts',(-8.4424810519869,-92.33192150942,65.328224889624));
#127164=CARTESIAN_POINT('Ctrl Pts',(-8.32876960322491,-92.84821811054,66.807276461651));
#127165=CARTESIAN_POINT('Ctrl Pts',(-8.15823859365691,-93.3022201360699,
68.644737618775));
#127166=CARTESIAN_POINT('Ctrl Pts',(-7.99043840954591,-93.61899006591,70.8474005016));
#127167=CARTESIAN_POINT('Ctrl Pts',(-7.95242679364891,-93.68276184645,72.4799516511365));
#127168=CARTESIAN_POINT('Ctrl Pts',(-7.95741734812491,-93.6732941703,73.2720763218484));
#127169=CARTESIAN_POINT('Ctrl Pts',(-8.43949877683291,-87.3537747401099,
62.27006488597));
#127170=CARTESIAN_POINT('Ctrl Pts',(-8.45731359140492,-87.4535563417601,
62.34368555564));
#127171=CARTESIAN_POINT('Ctrl Pts',(-8.52131292219791,-87.82106654726,62.63149311457));
#127172=CARTESIAN_POINT('Ctrl Pts',(-8.61411039860292,-88.43540728025,63.222074263414));
#127173=CARTESIAN_POINT('Ctrl Pts',(-8.68403744008991,-89.13943833049,64.117405994067));
#127174=CARTESIAN_POINT('Ctrl Pts',(-8.70113772340991,-89.7471218280801,
65.132620071883));
#127175=CARTESIAN_POINT('Ctrl Pts',(-8.66952211163591,-90.26679126728,66.269050071176));
#127176=CARTESIAN_POINT('Ctrl Pts',(-8.59296528164791,-90.71932698016,67.5848917653981));
#127177=CARTESIAN_POINT('Ctrl Pts',(-8.47524822121891,-91.1106638471899,
69.204437583702));
#127178=CARTESIAN_POINT('Ctrl Pts',(-8.35657014317891,-91.37998713432,71.128070825606));
#127179=CARTESIAN_POINT('Ctrl Pts',(-8.32937461695891,-91.43389890748,72.5465372663564));
#127180=CARTESIAN_POINT('Ctrl Pts',(-8.33290939283891,-91.42587213809,73.2350085774806));
#127181=CARTESIAN_POINT('Ctrl Pts',(-9.70290977013891,-85.71563863313,63.225929504496));
#127182=CARTESIAN_POINT('Ctrl Pts',(-9.71347226780991,-85.81258521909,63.3042697667619));
#127183=CARTESIAN_POINT('Ctrl Pts',(-9.75155217659191,-86.16920472985,63.607119168682));
#127184=CARTESIAN_POINT('Ctrl Pts',(-9.80734092195292,-86.76321296501,64.208958863088));
#127185=CARTESIAN_POINT('Ctrl Pts',(-9.84976775888791,-87.44130407606,65.092689108936));
#127186=CARTESIAN_POINT('Ctrl Pts',(-9.86024687222591,-88.02252314883,66.068935008635));
#127187=CARTESIAN_POINT('Ctrl Pts',(-9.84088807922991,-88.51301036784,67.134160433264));
#127188=CARTESIAN_POINT('Ctrl Pts',(-9.79367311983191,-88.93113286615,68.3343103616489));
#127189=CARTESIAN_POINT('Ctrl Pts',(-9.72059012292691,-89.2817921413201,
69.767187011365));
#127190=CARTESIAN_POINT('Ctrl Pts',(-9.64644890999391,-89.51483550078,71.418566814176));
#127191=CARTESIAN_POINT('Ctrl Pts',(-9.62940986650091,-89.56052949701,72.6152524275675));
#127192=CARTESIAN_POINT('Ctrl Pts',(-9.63161894838992,-89.55368004058,73.1967232445338));
#127193=CARTESIAN_POINT('Ctrl Pts',(-11.6147520896694,-84.5243630961,63.571054202212));
#127194=CARTESIAN_POINT('Ctrl Pts',(-11.6246340679083,-84.6249961903,63.66586459399));
#127195=CARTESIAN_POINT('Ctrl Pts',(-11.6593120484911,-84.99447215027,64.027094849045));
#127196=CARTESIAN_POINT('Ctrl Pts',(-11.7060805587835,-85.60709500622,64.713399121719));
#127197=CARTESIAN_POINT('Ctrl Pts',(-11.7389496702744,-86.30596314069,65.6728212489209));
#127198=CARTESIAN_POINT('Ctrl Pts',(-11.7463516547408,-86.90449452193,66.690284220663));
#127199=CARTESIAN_POINT('Ctrl Pts',(-11.7325725181496,-87.40596349938,67.7581163994829));
#127200=CARTESIAN_POINT('Ctrl Pts',(-11.7012754818754,-87.82560147568,68.912217015091));
#127201=CARTESIAN_POINT('Ctrl Pts',(-11.6561110576122,-88.16534971416,70.225368387264));
#127202=CARTESIAN_POINT('Ctrl Pts',(-11.6134044513163,-88.3802178611799,
71.663335401016));
#127203=CARTESIAN_POINT('Ctrl Pts',(-11.6039200063252,-88.42090783937,72.6729563753231));
#127204=CARTESIAN_POINT('Ctrl Pts',(-11.6051869982177,-88.4147469583799,
73.1645418273416));
#127205=CARTESIAN_POINT('',(-11.2241290292204,-88.6512992632751,72.9889531634726));
#127206=CARTESIAN_POINT('Origin',(-15.3537166934403,-94.9097718533471,73.0060860461187));
#127207=CARTESIAN_POINT('Ctrl Pts',(-11.2240197558157,-88.6511336051499,
72.9889531154357));
#127208=CARTESIAN_POINT('Ctrl Pts',(-11.2242745255353,-88.6509671919425,
72.9761856442956));
#127209=CARTESIAN_POINT('Ctrl Pts',(-11.2245118171374,-88.6508027974082,
72.9569880187906));
#127210=CARTESIAN_POINT('Ctrl Pts',(-11.2247672217957,-88.6505537102174,
72.9313531986707));
#127211=CARTESIAN_POINT('Ctrl Pts',(-11.2250224784259,-88.6503047673933,
72.905733236053));
#127212=CARTESIAN_POINT('Ctrl Pts',(-11.2252958726478,-88.6499712088215,
72.8736832010589));
#127213=CARTESIAN_POINT('Ctrl Pts',(-11.2256349948435,-88.6494160359053,
72.8352002030464));
#127214=CARTESIAN_POINT('Ctrl Pts',(-11.2259720748059,-88.6488642063049,
72.7969489541183));
#127215=CARTESIAN_POINT('Ctrl Pts',(-11.2263741723918,-88.6480933420174,
72.7523415227726));
#127216=CARTESIAN_POINT('Ctrl Pts',(-11.2268989971422,-88.6469198945246,
72.7013851606149));
#127217=CARTESIAN_POINT('Ctrl Pts',(-11.2272369925059,-88.6461641759504,
72.6685684648564));
#127218=CARTESIAN_POINT('Ctrl Pts',(-11.2276261104829,-88.6452404949846,
72.6331187210802));
#127219=CARTESIAN_POINT('Ctrl Pts',(-11.2280839387327,-88.6440892094085,
72.5950416458244));
#127220=CARTESIAN_POINT('Ctrl Pts',(-11.2287632555083,-88.6423809539531,
72.5385436119001));
#127221=CARTESIAN_POINT('Ctrl Pts',(-11.2295979323301,-88.640170573144,
72.4762570353377));
#127222=CARTESIAN_POINT('Ctrl Pts',(-11.2306657390954,-88.637218963774,
72.4081865053001));
#127223=CARTESIAN_POINT('Ctrl Pts',(-11.2316410246325,-88.634523099669,
72.3460140171672));
#127224=CARTESIAN_POINT('Ctrl Pts',(-11.2328109383719,-88.6312084061529,
72.2790163014364));
#127225=CARTESIAN_POINT('Ctrl Pts',(-11.2342393575461,-88.6270626171519,
72.2072196998836));
#127226=CARTESIAN_POINT('Ctrl Pts',(-11.2357355307736,-88.6227201813865,
72.1320175778403));
#127227=CARTESIAN_POINT('Ctrl Pts',(-11.2375167516463,-88.6174653044088,
72.051546660498));
#127228=CARTESIAN_POINT('Ctrl Pts',(-11.2396643553321,-88.6110151748712,
71.9658383006492));
#127229=CARTESIAN_POINT('Ctrl Pts',(-11.240738157175,-88.6077901101024,
71.9229841207248));
#127230=CARTESIAN_POINT('Ctrl Pts',(-11.2419034100726,-88.6042657527526,
71.8788202239335));
#127231=CARTESIAN_POINT('Ctrl Pts',(-11.2431696669609,-88.6004035007701,
71.8333495265937));
#127232=CARTESIAN_POINT('Ctrl Pts',(-11.243802795405,-88.5984723747788,
71.8106141779239));
#127233=CARTESIAN_POINT('Ctrl Pts',(-11.244461156607,-88.5964567476816,
71.7875521308478));
#127234=CARTESIAN_POINT('Ctrl Pts',(-11.2451459415228,-88.5943515507392,
71.7641637757324));
#127235=CARTESIAN_POINT('Ctrl Pts',(-11.2454883339806,-88.593298952268,
71.7524695981747));
#127236=CARTESIAN_POINT('Ctrl Pts',(-11.2458373311496,-88.5922239595018,
71.7406938437182));
#127237=CARTESIAN_POINT('Ctrl Pts',(-11.2461930770222,-88.5911259259485,
71.7288365623583));
#127238=CARTESIAN_POINT('Ctrl Pts',(-11.2463709499585,-88.5905769091719,
71.7229079216783));
#127239=CARTESIAN_POINT('Ctrl Pts',(-11.2465505099919,-88.5900221320799,
71.7169588992809));
#127240=CARTESIAN_POINT('Ctrl Pts',(-11.2467317749972,-88.5894615129103,
71.7109895015165));
#127241=CARTESIAN_POINT('Ctrl Pts',(-11.2468224074999,-88.5891812033255,
71.7080048026343));
#127242=CARTESIAN_POINT('Ctrl Pts',(-11.2469134662406,-88.5888994332138,
71.7050150099109));
#127243=CARTESIAN_POINT('Ctrl Pts',(-11.2470049534458,-88.5886161922945,
71.7020201241467));
#127244=CARTESIAN_POINT('Ctrl Pts',(-11.2470964406511,-88.5883329513752,
71.6990252383824));
#127245=CARTESIAN_POINT('Ctrl Pts',(-11.2472508047561,-88.5878547041565,
71.6939931057192));
#127246=CARTESIAN_POINT('Ctrl Pts',(-11.2472807026685,-88.5877620467987,
71.6930201885352));
#127247=CARTESIAN_POINT('Ctrl Pts',(-11.2477188332067,-88.5864042256359,
71.6787628475912));
#127248=CARTESIAN_POINT('Ctrl Pts',(-11.2481906728962,-88.5849616586075,
71.6639168877229));
#127249=CARTESIAN_POINT('Ctrl Pts',(-11.2486979846655,-88.5834283333534,
71.6484822011923));
#127250=CARTESIAN_POINT('Ctrl Pts',(-11.2503106722699,-88.5785540631702,
71.5994170520069));
#127251=CARTESIAN_POINT('Ctrl Pts',(-11.2522817326128,-88.5727659906201,
71.5444007021859));
#127252=CARTESIAN_POINT('Ctrl Pts',(-11.2546673042124,-88.5658423347889,
71.4834425465419));
#127253=CARTESIAN_POINT('Ctrl Pts',(-11.2570204709904,-88.5590127276259,
71.4233124264758));
#127254=CARTESIAN_POINT('Ctrl Pts',(-11.2597772685108,-88.5510780541774,
71.3574005696904));
#127255=CARTESIAN_POINT('Ctrl Pts',(-11.2629906638128,-88.5417831055776,
71.2857435995938));
#127256=CARTESIAN_POINT('Ctrl Pts',(-11.2644459367637,-88.5375736367738,
71.2532918031204));
#127257=CARTESIAN_POINT('Ctrl Pts',(-11.2659948166465,-88.5330846099312,
71.2196620993046));
#127258=CARTESIAN_POINT('Ctrl Pts',(-11.2676418836711,-88.5282895140319,
71.1848600200692));
#127259=CARTESIAN_POINT('Ctrl Pts',(-11.2711519048001,-88.5180708115325,
71.1106942261965));
#127260=CARTESIAN_POINT('Ctrl Pts',(-11.2751087946652,-88.5064636760206,
71.0311953045052));
#127261=CARTESIAN_POINT('Ctrl Pts',(-11.2795473902357,-88.4931829448063,
70.9464067805103));
#127262=CARTESIAN_POINT('Ctrl Pts',(-11.2815142287214,-88.4872979632045,
70.9088351366222));
#127263=CARTESIAN_POINT('Ctrl Pts',(-11.2835755289603,-88.4810838644701,
70.8702252769905));
#127264=CARTESIAN_POINT('Ctrl Pts',(-11.2857335898617,-88.4745134816927,
70.8305831879646));
#127265=CARTESIAN_POINT('Ctrl Pts',(-11.2892476854252,-88.4638145468512,
70.7660316782822));
#127266=CARTESIAN_POINT('Ctrl Pts',(-11.293018420646,-88.4521714371299,
70.6987413507889));
#127267=CARTESIAN_POINT('Ctrl Pts',(-11.2970505565863,-88.4394586051646,
70.628738799706));
#127268=CARTESIAN_POINT('Ctrl Pts',(-11.2990666245565,-88.4331021891819,
70.5937375241646));
#127269=CARTESIAN_POINT('Ctrl Pts',(-11.3011479344878,-88.4264781837837,
70.5580582142501));
#127270=CARTESIAN_POINT('Ctrl Pts',(-11.3032946151084,-88.4195697734577,
70.5217045156815));
#127271=CARTESIAN_POINT('Ctrl Pts',(-11.3043679554187,-88.4161155682947,
70.5035276663972));
#127272=CARTESIAN_POINT('Ctrl Pts',(-11.3054576310313,-88.4125902510797,
70.4851822214201));
#127273=CARTESIAN_POINT('Ctrl Pts',(-11.3065636138707,-88.4089916532588,
70.466668651342));
#127274=CARTESIAN_POINT('Ctrl Pts',(-11.3071166052905,-88.4071923543484,
70.4574118663029));
#127275=CARTESIAN_POINT('Ctrl Pts',(-11.3076736730322,-88.405374734581,
70.4481130500982));
#127276=CARTESIAN_POINT('Ctrl Pts',(-11.3082348106141,-88.4035385188914,
70.4387722639503));
#127277=CARTESIAN_POINT('Ctrl Pts',(-11.3087959481959,-88.4017023032017,
70.4294314778024));
#127278=CARTESIAN_POINT('Ctrl Pts',(-11.309459193718,-88.3995248099728,
70.4184256286073));
#127279=CARTESIAN_POINT('Ctrl Pts',(-11.3099304244086,-88.3979738061611,
70.4106240577841));
#127280=CARTESIAN_POINT('Ctrl Pts',(-11.3161893151632,-88.3773733579903,
70.3070035159241));
#127281=CARTESIAN_POINT('Ctrl Pts',(-11.3224767080662,-88.3558955118018,
70.2052254946104));
#127282=CARTESIAN_POINT('Ctrl Pts',(-11.3287287672198,-88.3336575856445,
70.1053181242262));
#127283=CARTESIAN_POINT('Ctrl Pts',(-11.3396427516581,-88.2948376746266,
69.9309135866394));
#127284=CARTESIAN_POINT('Ctrl Pts',(-11.3504467258724,-88.253701523487,
69.7622090979111));
#127285=CARTESIAN_POINT('Ctrl Pts',(-11.3608858503052,-88.2108286042613,
69.5991748821252));
#127286=CARTESIAN_POINT('Ctrl Pts',(-11.3716123989377,-88.166775249399,
69.431651786138));
#127287=CARTESIAN_POINT('Ctrl Pts',(-11.3819537487847,-88.1208883263476,
69.2701150314172));
#127288=CARTESIAN_POINT('Ctrl Pts',(-11.3916854425355,-88.0737898026253,
69.1145168693028));
#127289=CARTESIAN_POINT('Ctrl Pts',(-11.3931999939023,-88.0664598212977,
69.0903010015266));
#127290=CARTESIAN_POINT('Ctrl Pts',(-11.3946998778907,-88.0591004783046,
69.0662289505687));
#127291=CARTESIAN_POINT('Ctrl Pts',(-11.3961843563362,-88.0517141003437,
69.0423005151616));
#127292=CARTESIAN_POINT('Ctrl Pts',(-11.4015341233223,-88.0250950537155,
68.956067162196));
#127293=CARTESIAN_POINT('Ctrl Pts',(-11.4066887884465,-87.9981222265563,
68.8717032079022));
#127294=CARTESIAN_POINT('Ctrl Pts',(-11.4116279620168,-87.9708955175075,
68.7891981885541));
#127295=CARTESIAN_POINT('Ctrl Pts',(-11.4185172356412,-87.9329190735016,
68.6741182777992));
#127296=CARTESIAN_POINT('Ctrl Pts',(-11.4249872025774,-87.8944486596017,
68.562654875211));
#127297=CARTESIAN_POINT('Ctrl Pts',(-11.4310142678285,-87.855743445013,
68.4547791264471));
#127298=CARTESIAN_POINT('Ctrl Pts',(-11.4361883127967,-87.822516241981,
68.3621712067002));
#127299=CARTESIAN_POINT('Ctrl Pts',(-11.4410356293391,-87.7891159936686,
68.2722057637127));
#127300=CARTESIAN_POINT('Ctrl Pts',(-11.4455514956465,-87.7556979118045,
68.1848566034732));
#127301=CARTESIAN_POINT('Ctrl Pts',(-11.4478094288002,-87.7389888708724,
68.1411820233534));
#127302=CARTESIAN_POINT('Ctrl Pts',(-11.4499845038457,-87.7222753760469,
68.0981615098983));
#127303=CARTESIAN_POINT('Ctrl Pts',(-11.4520774016122,-87.7055757548429,
68.0557915330754));
#127304=CARTESIAN_POINT('Ctrl Pts',(-11.4534623527881,-87.6945249713823,
68.0277536851878));
#127305=CARTESIAN_POINT('Ctrl Pts',(-11.4547703837296,-87.683821685813,
68.0008571179604));
#127306=CARTESIAN_POINT('Ctrl Pts',(-11.4560833007314,-87.6727952916227,
67.9733995645209));
#127307=CARTESIAN_POINT('Ctrl Pts',(-11.4567544255561,-87.667158920962,
67.9593640651589));
#127308=CARTESIAN_POINT('Ctrl Pts',(-11.4574267125168,-87.6614374289534,
67.9451823919486));
#127309=CARTESIAN_POINT('Ctrl Pts',(-11.4581103184323,-87.6555367675149,
67.9306298265414));
#127310=CARTESIAN_POINT('Ctrl Pts',(-11.4623071180713,-87.619311373272,
67.8412885849503));
#127311=CARTESIAN_POINT('Ctrl Pts',(-11.4662235340514,-87.5818180497456,
67.7513816670787));
#127312=CARTESIAN_POINT('Ctrl Pts',(-11.4698027840946,-87.5430029926291,
67.6609294029669));
#127313=CARTESIAN_POINT('Ctrl Pts',(-11.475785945847,-87.4781187955625,
67.5097271900694));
#127314=CARTESIAN_POINT('Ctrl Pts',(-11.4808278170763,-87.4095416663116,
67.3569981853293));
#127315=CARTESIAN_POINT('Ctrl Pts',(-11.4846831264988,-87.337022253606,
67.2029120936388));
#127316=CARTESIAN_POINT('Ctrl Pts',(-11.4883729157958,-87.2676163192169,
67.0554413851604));
#127317=CARTESIAN_POINT('Ctrl Pts',(-11.4909758971826,-87.1945991804734,
66.9067274080467));
#127318=CARTESIAN_POINT('Ctrl Pts',(-11.4922587536103,-87.1177441567912,
66.7569628191743));
#127319=CARTESIAN_POINT('Ctrl Pts',(-11.4926072969111,-87.096863173498,
66.7162728066242));
#127320=CARTESIAN_POINT('Ctrl Pts',(-11.4928582814169,-87.0756988479199,
66.6755055098484));
#127321=CARTESIAN_POINT('Ctrl Pts',(-11.4930067714473,-87.0542465467405,
66.6346654152655));
#127322=CARTESIAN_POINT('Ctrl Pts',(-11.493518944891,-86.9802530339186,
66.4937993125153));
#127323=CARTESIAN_POINT('Ctrl Pts',(-11.4928126466536,-86.9028330702812,
66.3520630396957));
#127324=CARTESIAN_POINT('Ctrl Pts',(-11.4907005478281,-86.8218389933892,
66.2097182555379));
#127325=CARTESIAN_POINT('Ctrl Pts',(-11.4885884490026,-86.7408449164971,
66.0673734713802));
#127326=CARTESIAN_POINT('Ctrl Pts',(-11.4850706336615,-86.6562766227845,
65.9244197258589));
#127327=CARTESIAN_POINT('Ctrl Pts',(-11.4799467033179,-86.5679916716801,
65.781175173196));
#127328=CARTESIAN_POINT('Ctrl Pts',(-11.4778444076629,-86.5317692688256,
65.7224034139284));
#127329=CARTESIAN_POINT('Ctrl Pts',(-11.4754702275825,-86.4949212922084,
65.663581338532));
#127330=CARTESIAN_POINT('Ctrl Pts',(-11.4727992458932,-86.457434097807,
65.604715206676));
#127331=CARTESIAN_POINT('Ctrl Pts',(-11.4676289803903,-86.3848694865291,
65.4907670160001));
#127332=CARTESIAN_POINT('Ctrl Pts',(-11.4613470631302,-86.3099097321324,
65.3766505663401));
#127333=CARTESIAN_POINT('Ctrl Pts',(-11.4537794840977,-86.2324876677326,
65.262464666662));
#127334=CARTESIAN_POINT('Ctrl Pts',(-11.4465361633332,-86.1583830109739,
65.1531714442723));
#127335=CARTESIAN_POINT('Ctrl Pts',(-11.4381149629705,-86.0820223655018,
65.0438144674924));
#127336=CARTESIAN_POINT('Ctrl Pts',(-11.4283559618822,-86.0033458151717,
64.9345266511644));
#127337=CARTESIAN_POINT('Ctrl Pts',(-11.4205914636241,-85.9407488411113,
64.8475746104977));
#127338=CARTESIAN_POINT('Ctrl Pts',(-11.411979975111,-85.876685805877,64.7606671320666));
#127339=CARTESIAN_POINT('Ctrl Pts',(-11.4024376136905,-85.811127109965,
64.6738946118772));
#127340=CARTESIAN_POINT('Ctrl Pts',(-11.4010476440789,-85.8015776293827,
64.6612550606308));
#127341=CARTESIAN_POINT('Ctrl Pts',(-11.399638690759,-85.7919965920506,
64.6486194534414));
#127342=CARTESIAN_POINT('Ctrl Pts',(-11.3982101770104,-85.7823838748884,
64.635987712293));
#127343=CARTESIAN_POINT('Ctrl Pts',(-11.3880774781259,-85.7141991839361,
64.5463885540258));
#127344=CARTESIAN_POINT('Ctrl Pts',(-11.3769610614966,-85.6444206348788,
64.4569799346877));
#127345=CARTESIAN_POINT('Ctrl Pts',(-11.3646619607724,-85.5730292249959,
64.3677650832233));
#127346=CARTESIAN_POINT('Ctrl Pts',(-11.352722443728,-85.5037250559967,
64.2811585691726));
#127347=CARTESIAN_POINT('Ctrl Pts',(-11.3396683115244,-85.4329006832326,
64.1947343917873));
#127348=CARTESIAN_POINT('Ctrl Pts',(-11.3253131918183,-85.3605404164633,
64.1085436510511));
#127349=CARTESIAN_POINT('Ctrl Pts',(-11.3115545684955,-85.2911869262528,
64.0259343827223));
#127350=CARTESIAN_POINT('Ctrl Pts',(-11.2966007409571,-85.2204222912503,
63.9435394171877));
#127351=CARTESIAN_POINT('Ctrl Pts',(-11.2802847637017,-85.1482379428458,
63.8614513511311));
#127352=CARTESIAN_POINT('Ctrl Pts',(-11.2744827839982,-85.1225691080715,
63.8322607433176));
#127353=CARTESIAN_POINT('Ctrl Pts',(-11.2685085368507,-85.0967208144483,
63.8031094064044));
#127354=CARTESIAN_POINT('Ctrl Pts',(-11.262354457998,-85.0706929373549,
63.7740031019365));
#127355=CARTESIAN_POINT('Ctrl Pts',(-11.2486127761017,-85.0125742788164,
63.7090105032463));
#127356=CARTESIAN_POINT('Ctrl Pts',(-11.2339742973963,-84.9535597088113,
63.6442408305321));
#127357=CARTESIAN_POINT('Ctrl Pts',(-11.2183631611147,-84.8936604075354,
63.579773123225));
#127358=CARTESIAN_POINT('Ctrl Pts',(-7.95814792783791,-93.67295473434,72.7059852969892));
#127359=CARTESIAN_POINT('Ctrl Pts',(-7.95271346435991,-93.6874724926401,
73.9073476595992));
#127360=CARTESIAN_POINT('Ctrl Pts',(-8.06439460568691,-93.50423865288,76.59995736407));
#127361=CARTESIAN_POINT('Ctrl Pts',(-8.42970521090091,-92.66068586414,80.031694782438));
#127362=CARTESIAN_POINT('Ctrl Pts',(-8.53434685477391,-91.35085311195,82.802279089842));
#127363=CARTESIAN_POINT('Ctrl Pts',(-8.31596425941191,-90.05403658787,84.34463821187));
#127364=CARTESIAN_POINT('Ctrl Pts',(-8.1057478610679,-89.26927616764,84.98339808023));
#127365=CARTESIAN_POINT('Ctrl Pts',(-8.06516310420291,-89.12509080528,85.09190979212));
#127366=CARTESIAN_POINT('Ctrl Pts',(-8.33354804813591,-91.42591365382,72.7430411923306));
#127367=CARTESIAN_POINT('Ctrl Pts',(-8.32981191803891,-91.43826407759,73.7872734245095));
#127368=CARTESIAN_POINT('Ctrl Pts',(-8.40995296574992,-91.28362370523,76.126620078171));
#127369=CARTESIAN_POINT('Ctrl Pts',(-8.66300469726491,-90.56112912654,79.150030229971));
#127370=CARTESIAN_POINT('Ctrl Pts',(-8.72873058528991,-89.39410231427,81.640904005726));
#127371=CARTESIAN_POINT('Ctrl Pts',(-8.58890642680991,-88.20699181858,83.0342999759601));
#127372=CARTESIAN_POINT('Ctrl Pts',(-8.46279625181091,-87.48612778525,83.61026163649));
#127373=CARTESIAN_POINT('Ctrl Pts',(-8.43880080502891,-87.3536321469,83.70816700881));
#127374=CARTESIAN_POINT('Ctrl Pts',(-9.63185731428291,-89.5539832136501,
72.781364998818));
#127375=CARTESIAN_POINT('Ctrl Pts',(-9.62954009343191,-89.56450050364,73.6635123434199));
#127376=CARTESIAN_POINT('Ctrl Pts',(-9.67979255886791,-89.43456846233,75.636780916767));
#127377=CARTESIAN_POINT('Ctrl Pts',(-9.83705040271291,-88.79415684226,78.3069686379569));
#127378=CARTESIAN_POINT('Ctrl Pts',(-9.87680294572491,-87.68882950106,80.657534553207));
#127379=CARTESIAN_POINT('Ctrl Pts',(-9.79176044324591,-86.54376161791,82.044574788622));
#127380=CARTESIAN_POINT('Ctrl Pts',(-9.71654265497591,-85.8444122705301,
82.648215408587));
#127381=CARTESIAN_POINT('Ctrl Pts',(-9.70229630805891,-85.7156408435,82.752331765737));
#127382=CARTESIAN_POINT('Ctrl Pts',(-11.6048653665117,-88.41503849039,72.8136299831037));
#127383=CARTESIAN_POINT('Ctrl Pts',(-11.603416364145,-88.42440730528,73.5597250211369));
#127384=CARTESIAN_POINT('Ctrl Pts',(-11.6311458484653,-88.31057472766,75.224087177656));
#127385=CARTESIAN_POINT('Ctrl Pts',(-11.7273886361771,-87.6975782204,77.663686258094));
#127386=CARTESIAN_POINT('Ctrl Pts',(-11.7590758209942,-86.56104819585,80.0401709969071));
#127387=CARTESIAN_POINT('Ctrl Pts',(-11.6945650537626,-85.38232181583,81.564678001863));
#127388=CARTESIAN_POINT('Ctrl Pts',(-11.6272962250143,-84.6579922825401,
82.281183093728));
#127389=CARTESIAN_POINT('Ctrl Pts',(-11.6140949378786,-84.52426756057,82.407140345955));
#127390=CARTESIAN_POINT('',(-11.2182878249493,-84.8936697055269,82.3980269273797));
#127391=CARTESIAN_POINT('Origin',(-15.2669619786145,-88.9999686914874,87.1938529810033));
#127392=CARTESIAN_POINT('Ctrl Pts',(-11.2182787039429,-84.89366045326,82.398016121838));
#127393=CARTESIAN_POINT('Ctrl Pts',(-11.3430626531798,-85.3496693368457,
81.9024669884646));
#127394=CARTESIAN_POINT('Ctrl Pts',(-11.4164398924616,-85.7961369782742,
81.3484093064796));
#127395=CARTESIAN_POINT('Ctrl Pts',(-11.4782992679321,-86.4220082696662,
80.4300644193753));
#127396=CARTESIAN_POINT('Ctrl Pts',(-11.4902933546158,-86.6235627591728,
80.1091043375985));
#127397=CARTESIAN_POINT('Ctrl Pts',(-11.4960118930784,-86.9113210240422,
79.6062440989535));
#127398=CARTESIAN_POINT('Ctrl Pts',(-11.4959454832308,-87.0047852362595,
79.4351079792639));
#127399=CARTESIAN_POINT('Ctrl Pts',(-11.4931937770432,-87.1408527017736,
79.1732045109814));
#127400=CARTESIAN_POINT('Ctrl Pts',(-11.4911535852368,-87.207857804048,
79.0409473814055));
#127401=CARTESIAN_POINT('Ctrl Pts',(-11.4876778074931,-87.2841422644907,
78.8843632165692));
#127402=CARTESIAN_POINT('Ctrl Pts',(-11.4856711248064,-87.3218005338773,
78.8055014690377));
#127403=CARTESIAN_POINT('Ctrl Pts',(-11.4845249525581,-87.3418433962271,
78.7631016647935));
#127404=CARTESIAN_POINT('Ctrl Pts',(-11.4839708080131,-87.351160796497,
78.7432736154725));
#127405=CARTESIAN_POINT('Ctrl Pts',(-11.4836494562678,-87.3564761847352,
78.7319331490591));
#127406=CARTESIAN_POINT('Ctrl Pts',(-11.4835239494247,-87.3585369885875,
78.7275313025709));
#127407=CARTESIAN_POINT('Ctrl Pts',(-11.4788357164147,-87.4352505833193,
78.5635820136977));
#127408=CARTESIAN_POINT('Ctrl Pts',(-11.4691050177157,-87.5706949678135,
78.2721609350838));
#127409=CARTESIAN_POINT('Ctrl Pts',(-11.436532125925,-87.8206224854711,
77.6267037058662));
#127410=CARTESIAN_POINT('Ctrl Pts',(-11.422499106422,-87.9113251064847,
77.3766987634165));
#127411=CARTESIAN_POINT('Ctrl Pts',(-11.3963228623726,-88.0493517436767,
76.9476848439182));
#127412=CARTESIAN_POINT('Ctrl Pts',(-11.3867564782335,-88.0956584606176,
76.7956922087132));
#127413=CARTESIAN_POINT('Ctrl Pts',(-11.3713368768106,-88.1642089966755,
76.5540216285056));
#127414=CARTESIAN_POINT('Ctrl Pts',(-11.3633625248204,-88.1982545023846,
76.4297665144432));
#127415=CARTESIAN_POINT('Ctrl Pts',(-11.3536733662997,-88.2372497858451,
76.2787824303504));
#127416=CARTESIAN_POINT('Ctrl Pts',(-11.3487450162542,-88.2565240599301,
76.2017818743169));
#127417=CARTESIAN_POINT('Ctrl Pts',(-11.3466164315199,-88.2647320395063,
76.1684580009983));
#127418=CARTESIAN_POINT('Ctrl Pts',(-11.3451939196021,-88.2701918684418,
76.1461701194819));
#127419=CARTESIAN_POINT('Ctrl Pts',(-11.3443530684592,-88.273401943246,
76.1329833439319));
#127420=CARTESIAN_POINT('Ctrl Pts',(-11.3062141912186,-88.4184339482895,
75.5343934562496));
#127421=CARTESIAN_POINT('Ctrl Pts',(-11.2748698034577,-88.5118391686237,
74.9752281112511));
#127422=CARTESIAN_POINT('Ctrl Pts',(-11.2346789802457,-88.6282672494248,
73.9272753026554));
#127423=CARTESIAN_POINT('Ctrl Pts',(-11.2248258049113,-88.6512540350557,
73.4383979205486));
#127424=CARTESIAN_POINT('Ctrl Pts',(-11.2240831851649,-88.65122976349,72.9889532029839));
#127425=CARTESIAN_POINT('Ctrl Pts',(-8.11808175007291,-89.52553005688,84.97626614071));
#127426=CARTESIAN_POINT('Ctrl Pts',(-7.99010363327091,-89.1241947504099,
85.35070169572));
#127427=CARTESIAN_POINT('Ctrl Pts',(-7.69938772208291,-88.16991851438,86.15798661873));
#127428=CARTESIAN_POINT('Ctrl Pts',(-7.30474282753991,-86.6999882338099,
87.1516158381));
#127429=CARTESIAN_POINT('Ctrl Pts',(-7.05497526331491,-85.61835734781,87.73595158981));
#127430=CARTESIAN_POINT('Ctrl Pts',(-6.95502900065691,-85.15297983312,87.96387367036));
#127431=CARTESIAN_POINT('Ctrl Pts',(-8.41172030319291,-87.7346806391301,
83.6065321030901));
#127432=CARTESIAN_POINT('Ctrl Pts',(-8.32326273657991,-87.3770388479801,
83.93232607158));
#127433=CARTESIAN_POINT('Ctrl Pts',(-8.12258789573591,-86.52944513715,84.63393589531));
#127434=CARTESIAN_POINT('Ctrl Pts',(-7.85094891605191,-85.2321620574,85.49666769891));
#127435=CARTESIAN_POINT('Ctrl Pts',(-7.67942255015891,-84.28177895711,86.00440541648));
#127436=CARTESIAN_POINT('Ctrl Pts',(-7.61083400787491,-83.8734210634099,
86.202573254));
#127437=CARTESIAN_POINT('Ctrl Pts',(-9.60750379728591,-86.06450877549,82.631770479613));
#127438=CARTESIAN_POINT('Ctrl Pts',(-9.55206217138891,-85.75017345838,82.9238877548731));
#127439=CARTESIAN_POINT('Ctrl Pts',(-9.42634334149491,-85.00709560531,83.5526574662701));
#127440=CARTESIAN_POINT('Ctrl Pts',(-9.25633058814091,-83.87535919677,84.32611853891));
#127441=CARTESIAN_POINT('Ctrl Pts',(-9.14905898422491,-83.04894649912,84.7822283658801));
#127442=CARTESIAN_POINT('Ctrl Pts',(-9.10617448690291,-82.6941779,84.96045202937));
#127443=CARTESIAN_POINT('Ctrl Pts',(-11.4777197527979,-84.8330644961,82.237604660585));
#127444=CARTESIAN_POINT('Ctrl Pts',(-11.4425022483259,-84.5534017806,82.517423172522));
#127445=CARTESIAN_POINT('Ctrl Pts',(-11.3623805326309,-83.89277021298,83.12005866634));
#127446=CARTESIAN_POINT('Ctrl Pts',(-11.2532616833429,-82.88795497252,83.86287547546));
#127447=CARTESIAN_POINT('Ctrl Pts',(-11.1840224014209,-82.15462766988,84.30215902993));
#127448=CARTESIAN_POINT('Ctrl Pts',(-11.1562934646479,-81.83981305517,84.47404654791));
#127449=CARTESIAN_POINT('Ctrl Pts',(-10.5124540782072,-82.2723839409002,
84.5902798667472));
#127450=CARTESIAN_POINT('Ctrl Pts',(-10.5589860307587,-82.4505577062519,
84.4766884517136));
#127451=CARTESIAN_POINT('Ctrl Pts',(-10.6048707416816,-82.6240058202091,
84.3601665283034));
#127452=CARTESIAN_POINT('Ctrl Pts',(-10.6498634719091,-82.7927321454252,
84.241090889674));
#127453=CARTESIAN_POINT('Ctrl Pts',(-10.6647639335523,-82.8486100644659,
84.2016560303743));
#127454=CARTESIAN_POINT('Ctrl Pts',(-10.6795667719249,-82.9039704873559,
84.1619410628824));
#127455=CARTESIAN_POINT('Ctrl Pts',(-10.6942637014701,-82.9588146439936,
84.1219596015313));
#127456=CARTESIAN_POINT('Ctrl Pts',(-10.7011862115472,-82.9846471980538,
84.1031276361028));
#127457=CARTESIAN_POINT('Ctrl Pts',(-10.7080853830463,-83.0103652957587,
84.0842364087212));
#127458=CARTESIAN_POINT('Ctrl Pts',(-10.7149605779035,-83.0359688607419,
84.0652873462258));
#127459=CARTESIAN_POINT('Ctrl Pts',(-10.7374211071262,-83.1196129801387,
84.0033827775899));
#127460=CARTESIAN_POINT('Ctrl Pts',(-10.7596256252642,-83.2020345828744,
83.9408609130829));
#127461=CARTESIAN_POINT('Ctrl Pts',(-10.7815513942294,-83.2832401218694,
83.8777695031336));
#127462=CARTESIAN_POINT('Ctrl Pts',(-10.7958700307634,-83.3362714476698,
83.8365676201386));
#127463=CARTESIAN_POINT('Ctrl Pts',(-10.8100698415077,-83.3887839747292,
83.7951229639608));
#127464=CARTESIAN_POINT('Ctrl Pts',(-10.8241461578732,-83.4407780456636,
83.7534493364609));
#127465=CARTESIAN_POINT('Ctrl Pts',(-10.8311843160559,-83.4667750811308,
83.732612522711));
#127466=CARTESIAN_POINT('Ctrl Pts',(-10.8381916040485,-83.4926425056323,
83.7117184715802));
#127467=CARTESIAN_POINT('Ctrl Pts',(-10.8451674543059,-83.5183804254234,
83.6907689146438));
#127468=CARTESIAN_POINT('Ctrl Pts',(-10.8507162070296,-83.5388529624296,
83.6741051522605));
#127469=CARTESIAN_POINT('Ctrl Pts',(-10.8564229129647,-83.5599006965701,
83.6568664032067));
#127470=CARTESIAN_POINT('Ctrl Pts',(-10.8618629080467,-83.5799551092879,
83.640341318734));
#127471=CARTESIAN_POINT('Ctrl Pts',(-10.8632620339316,-83.5851129536458,
83.6360911910982));
#127472=CARTESIAN_POINT('Ctrl Pts',(-10.8646435212819,-83.5902052797057,
83.6318884682935));
#127473=CARTESIAN_POINT('Ctrl Pts',(-10.8660001538151,-83.5952057823778,
83.6277554717686));
#127474=CARTESIAN_POINT('Ctrl Pts',(-10.8932821168994,-83.6957661964699,
83.5446406592721));
#127475=CARTESIAN_POINT('Ctrl Pts',(-10.9215231939352,-83.7996244495179,
83.4562915788775));
#127476=CARTESIAN_POINT('Ctrl Pts',(-10.9505677005548,-83.9063897436635,
83.3623391081002));
#127477=CARTESIAN_POINT('Ctrl Pts',(-10.9741423207597,-83.9930481707976,
83.2860804942117));
#127478=CARTESIAN_POINT('Ctrl Pts',(-10.9982461043705,-84.0816211316533,
83.2061296345882));
#127479=CARTESIAN_POINT('Ctrl Pts',(-11.0227911613409,-84.1718808298857,
83.1222729447451));
#127480=CARTESIAN_POINT('Ctrl Pts',(-11.0523588430011,-84.2806102586782,
83.0212567640396));
#127481=CARTESIAN_POINT('Ctrl Pts',(-11.0825673448688,-84.391789165629,
82.9145725157852));
#127482=CARTESIAN_POINT('Ctrl Pts',(-11.1132477111449,-84.5049638728565,
82.8018482205845));
#127483=CARTESIAN_POINT('Ctrl Pts',(-11.1434088030221,-84.6162230642284,
82.6910318178809));
#127484=CARTESIAN_POINT('Ctrl Pts',(-11.1740259596734,-84.729411220195,
82.5743778595687));
#127485=CARTESIAN_POINT('Ctrl Pts',(-11.2049266350637,-84.8440507040571,
82.4515174287385));
#127486=CARTESIAN_POINT('Ctrl Pts',(-11.2093777150624,-84.8605639196173,
82.4338200289442));
#127487=CARTESIAN_POINT('Ctrl Pts',(-11.2138346564853,-84.8771071660355,
82.4159938285928));
#127488=CARTESIAN_POINT('Ctrl Pts',(-11.2182969218548,-84.8936789311703,
82.398037702481));
#127489=CARTESIAN_POINT('Ctrl Pts',(-8.78823419897191,-74.82614074722,86.78284890078));
#127490=CARTESIAN_POINT('Ctrl Pts',(-8.7830641547019,-75.27337593527,86.78841383868));
#127491=CARTESIAN_POINT('Ctrl Pts',(-8.81909035363991,-76.30222111183,86.7513931298999));
#127492=CARTESIAN_POINT('Ctrl Pts',(-9.02657683691191,-77.8128025443,86.5260662143401));
#127493=CARTESIAN_POINT('Ctrl Pts',(-9.35664843786591,-79.26654580558,86.1326423177499));
#127494=CARTESIAN_POINT('Ctrl Pts',(-9.6889294635519,-80.5040342907,85.6588740936));
#127495=CARTESIAN_POINT('Ctrl Pts',(-9.98045484240391,-81.56707970974,85.1378870544099));
#127496=CARTESIAN_POINT('Ctrl Pts',(-10.1467265870689,-82.21888736454,84.7499607329399));
#127497=CARTESIAN_POINT('Ctrl Pts',(-10.2190780893279,-82.52447496234,84.5512375554));
#127498=CARTESIAN_POINT('Ctrl Pts',(-10.2208467462859,-82.53195984062,84.54635981205));
#127499=CARTESIAN_POINT('Ctrl Pts',(-9.36200580719791,-74.83444576085,86.7229059112));
#127500=CARTESIAN_POINT('Ctrl Pts',(-9.35704322394791,-75.26072541529,86.72795887141));
#127501=CARTESIAN_POINT('Ctrl Pts',(-9.39143229143391,-76.2407078089901,
86.69443228383));
#127502=CARTESIAN_POINT('Ctrl Pts',(-9.59050034074491,-77.69241237804,86.4878381930401));
#127503=CARTESIAN_POINT('Ctrl Pts',(-9.91209801158591,-79.1100671474,86.11982387127));
#127504=CARTESIAN_POINT('Ctrl Pts',(-10.2428814792609,-80.34262221862,85.66384781911));
#127505=CARTESIAN_POINT('Ctrl Pts',(-10.5367862747679,-81.4145391991,85.1527501983101));
#127506=CARTESIAN_POINT('Ctrl Pts',(-10.7064485902869,-82.07950817142,84.76549076934));
#127507=CARTESIAN_POINT('Ctrl Pts',(-10.7804334814949,-82.39193104589,84.56605530898));
#127508=CARTESIAN_POINT('Ctrl Pts',(-10.7822421679279,-82.39958375107,84.56115953279));
#127509=CARTESIAN_POINT('Ctrl Pts',(-9.69871563901291,-74.8448186684699,
86.25448988185));
#127510=CARTESIAN_POINT('Ctrl Pts',(-9.69387480135591,-75.24465675332,86.25906511337));
#127511=CARTESIAN_POINT('Ctrl Pts',(-9.72730314117991,-76.16342344133,86.22876881924));
#127512=CARTESIAN_POINT('Ctrl Pts',(-9.92143095043291,-77.53286478316,86.04033581316));
#127513=CARTESIAN_POINT('Ctrl Pts',(-10.2380558140759,-78.88352999808,85.69971076668));
#127514=CARTESIAN_POINT('Ctrl Pts',(-10.5679604608069,-80.07432532315,85.2691364616501));
#127515=CARTESIAN_POINT('Ctrl Pts',(-10.8632615836509,-81.11812953757,84.78024447856));
#127516=CARTESIAN_POINT('Ctrl Pts',(-11.0349136081859,-81.77043206243,84.4055551387));
#127517=CARTESIAN_POINT('Ctrl Pts',(-11.1098570308209,-82.07731007429,84.21193509085));
#127518=CARTESIAN_POINT('Ctrl Pts',(-11.1116892079909,-82.0848272083201,
84.20718173107));
#127519=CARTESIAN_POINT('Ctrl Pts',(-9.5727563378399,-74.8503092594,85.69145592527));
#127520=CARTESIAN_POINT('Ctrl Pts',(-9.56786995654791,-75.23593651453,85.69590777201));
#127521=CARTESIAN_POINT('Ctrl Pts',(-9.6016576936139,-76.12215123656,85.6664135340699));
#127522=CARTESIAN_POINT('Ctrl Pts',(-9.79763359022991,-77.44106222501,85.48340131111));
#127523=CARTESIAN_POINT('Ctrl Pts',(-10.1161187242309,-78.73872216599,85.1537934685601));
#127524=CARTESIAN_POINT('Ctrl Pts',(-10.4463521278369,-79.87891190224,84.73921042734));
#127525=CARTESIAN_POINT('Ctrl Pts',(-10.7411309005779,-80.876455559,84.26996174785));
#127526=CARTESIAN_POINT('Ctrl Pts',(-10.9120385977019,-81.49875083394,83.9113232946299));
#127527=CARTESIAN_POINT('Ctrl Pts',(-10.9866234446819,-81.79141909568,83.7261498249799));
#127528=CARTESIAN_POINT('Ctrl Pts',(-10.9884468342349,-81.79858809794,83.72160390688));
#127529=CARTESIAN_POINT('Ctrl Pts',(-9.44679703666692,-74.85579985033,85.12842196869));
#127530=CARTESIAN_POINT('Ctrl Pts',(-9.44186511173891,-75.2272162757499,
85.13275043066));
#127531=CARTESIAN_POINT('Ctrl Pts',(-9.47601224604791,-76.0808790318,85.10405824889));
#127532=CARTESIAN_POINT('Ctrl Pts',(-9.67383623002691,-77.34925966686,84.92646680905));
#127533=CARTESIAN_POINT('Ctrl Pts',(-9.99418163438691,-78.5939143339,84.60787617043));
#127534=CARTESIAN_POINT('Ctrl Pts',(-10.3247437948669,-79.68349848133,84.20928439302));
#127535=CARTESIAN_POINT('Ctrl Pts',(-10.6190002175039,-80.63478158042,83.75967901714));
#127536=CARTESIAN_POINT('Ctrl Pts',(-10.7891635872179,-81.22706960545,83.41709145055));
#127537=CARTESIAN_POINT('Ctrl Pts',(-10.8633898585419,-81.50552811708,83.2403645591));
#127538=CARTESIAN_POINT('Ctrl Pts',(-10.8652044604789,-81.51234898755,83.23602608269));
#127539=CARTESIAN_POINT('Ctrl Pts',(-8.94256573703792,-74.85272923674,84.84802251592));
#127540=CARTESIAN_POINT('Ctrl Pts',(-8.93745149507291,-75.23168732494,84.85266460914));
#127541=CARTESIAN_POINT('Ctrl Pts',(-8.97303734281391,-76.1032728097299,
84.82180884061));
#127542=CARTESIAN_POINT('Ctrl Pts',(-9.17825945844692,-77.38671306824,84.63326576812));
#127543=CARTESIAN_POINT('Ctrl Pts',(-9.50605176455791,-78.6278621281099,
84.30193835036));
#127544=CARTESIAN_POINT('Ctrl Pts',(-9.83792998113391,-79.6919023574,83.89921264773));
#127545=CARTESIAN_POINT('Ctrl Pts',(-10.1300953690529,-80.60977329784,83.45352654133));
#127546=CARTESIAN_POINT('Ctrl Pts',(-10.2972791003129,-81.17481917682,83.1197160038201));
#127547=CARTESIAN_POINT('Ctrl Pts',(-10.3700699471209,-81.4399240801001,
82.9484073536091));
#127548=CARTESIAN_POINT('Ctrl Pts',(-10.3718493710999,-81.44641751861,82.94420235099));
#127549=CARTESIAN_POINT('Ctrl Pts',(-8.3979150344609,-74.84315483705,85.03813500131));
#127550=CARTESIAN_POINT('Ctrl Pts',(-8.3926038608449,-75.24635390287,85.0433175979099));
#127551=CARTESIAN_POINT('Ctrl Pts',(-8.42974374991891,-76.17432795641,85.0087822784299));
#127552=CARTESIAN_POINT('Ctrl Pts',(-8.6429570346969,-77.52832734109,84.8002531342));
#127553=CARTESIAN_POINT('Ctrl Pts',(-8.9787931894819,-78.8178193399,84.4409690414599));
#127554=CARTESIAN_POINT('Ctrl Pts',(-9.31209295778892,-79.89849263975,84.01675409896));
#127555=CARTESIAN_POINT('Ctrl Pts',(-9.6019996927279,-80.81818713473,83.5566371803699));
#127556=CARTESIAN_POINT('Ctrl Pts',(-9.76596493640291,-81.37700916158,83.21844889811));
#127557=CARTESIAN_POINT('Ctrl Pts',(-9.83720529443491,-81.63856398261,83.04589974118));
#127558=CARTESIAN_POINT('Ctrl Pts',(-9.83894672057291,-81.64497007984,83.04166481234));
#127559=CARTESIAN_POINT('Origin',(-10.0948648922209,-81.92420577264,83.87306935796));
#127560=CARTESIAN_POINT('Ctrl Pts',(-9.07682613029074,-75.0000006725783,
86.7031078141421));
#127561=CARTESIAN_POINT('Ctrl Pts',(-9.10399999504518,-74.9999907514271,
86.6903141483888));
#127562=CARTESIAN_POINT('Ctrl Pts',(-9.13088724151304,-74.9999811036892,
86.6759898162106));
#127563=CARTESIAN_POINT('Ctrl Pts',(-9.1572412637087,-74.999971777649,86.6601431358597));
#127564=CARTESIAN_POINT('Ctrl Pts',(-9.18329122530418,-74.9999625592083,
86.6444792872262));
#127565=CARTESIAN_POINT('Ctrl Pts',(-9.20881934010855,-74.9999536552907,
86.6273278788702));
#127566=CARTESIAN_POINT('Ctrl Pts',(-9.23358406665683,-74.9999451130034,
86.6087473498612));
#127567=CARTESIAN_POINT('Ctrl Pts',(-9.25813552876659,-74.9999366442791,
86.5903268293255));
#127568=CARTESIAN_POINT('Ctrl Pts',(-9.28193582084024,-74.9999285311918,
86.5705018011061));
#127569=CARTESIAN_POINT('Ctrl Pts',(-9.30475915361208,-74.9999208170244,
86.5493793145265));
#127570=CARTESIAN_POINT('Ctrl Pts',(-9.32745319920907,-74.9999131465553,
86.5283764803502));
#127571=CARTESIAN_POINT('Ctrl Pts',(-9.34918050304556,-74.9999058706931,
86.506091191989));
#127572=CARTESIAN_POINT('Ctrl Pts',(-9.3697412764515,-74.9998990263766,
86.4826751026726));
#127573=CARTESIAN_POINT('Ctrl Pts',(-9.39024645363464,-74.9998922005671,
86.4593223303381));
#127574=CARTESIAN_POINT('Ctrl Pts',(-9.40959070386907,-74.9998858041356,
86.434845429367));
#127575=CARTESIAN_POINT('Ctrl Pts',(-9.4276093994838,-74.9998798654377,
86.4094343007998));
#127576=CARTESIAN_POINT('Ctrl Pts',(-9.44563283269752,-74.9998739251784,
86.3840164909646));
#127577=CARTESIAN_POINT('Ctrl Pts',(-9.46232950020998,-74.9998684430116,
86.3576647027707));
#127578=CARTESIAN_POINT('Ctrl Pts',(-9.47757741530284,-74.9998634368882,
86.330598712092));
#127579=CARTESIAN_POINT('Ctrl Pts',(-9.49293759605705,-74.9998583939063,
86.3033334429334));
#127580=CARTESIAN_POINT('Ctrl Pts',(-9.50682728712112,-74.9998538340757,
86.2753442715325));
#127581=CARTESIAN_POINT('Ctrl Pts',(-9.51917165228492,-74.9998497636995,
86.2468739512399));
#127582=CARTESIAN_POINT('Ctrl Pts',(-9.53159872212772,-74.9998456660525,
86.218212885723));
#127583=CARTESIAN_POINT('Ctrl Pts',(-9.54245964807191,-74.9998420644443,
86.189065122376));
#127584=CARTESIAN_POINT('Ctrl Pts',(-9.55173123092076,-74.9998389525596,
86.1596830567581));
#127585=CARTESIAN_POINT('Ctrl Pts',(-9.56108916788417,-74.9998358116912,
86.1300273310433));
#127586=CARTESIAN_POINT('Ctrl Pts',(-9.56882823591605,-74.9998331696532,
86.1001338087774));
#127587=CARTESIAN_POINT('Ctrl Pts',(-9.57497724561255,-74.9998310074135,
86.0702529880118));
#127588=CARTESIAN_POINT('Ctrl Pts',(-9.58119948158175,-74.9998288194246,
86.0400163276497));
#127589=CARTESIAN_POINT('Ctrl Pts',(-9.58579401693701,-74.9998271226158,
86.0097934597263));
#127590=CARTESIAN_POINT('Ctrl Pts',(-9.58883927510594,-74.9998258857931,
85.9798218969432));
#127591=CARTESIAN_POINT('Ctrl Pts',(-9.59195555286494,-74.9998246201261,
85.9491513562788));
#127592=CARTESIAN_POINT('Ctrl Pts',(-9.59345005338149,-74.9998238360011,
85.9187446672511));
#127593=CARTESIAN_POINT('Ctrl Pts',(-9.5934493444679,-74.9998234900437,
85.8888219184142));
#127594=CARTESIAN_POINT('Ctrl Pts',(-9.59344862496583,-74.999823138919,
85.8584522370923));
#127595=CARTESIAN_POINT('Ctrl Pts',(-9.59190851333374,-74.9998232389509,
85.8285814699716));
#127596=CARTESIAN_POINT('Ctrl Pts',(-9.58899358054596,-74.9998237373645,
85.7993962358241));
#127597=CARTESIAN_POINT('Ctrl Pts',(-9.58600511871662,-74.9998242483505,
85.7694748055271));
#127598=CARTESIAN_POINT('Ctrl Pts',(-9.58157246621915,-74.9998251778617,
85.7402741621824));
#127599=CARTESIAN_POINT('Ctrl Pts',(-9.5758936539825,-74.9998264644108,
85.7119449365536));
#127600=CARTESIAN_POINT('Ctrl Pts',(-9.57457467685541,-74.9998267632284,
85.705365109809));
#127601=CARTESIAN_POINT('Ctrl Pts',(-9.57318852871841,-74.9998270812952,
85.6988320763153));
#127602=CARTESIAN_POINT('Ctrl Pts',(-9.57173776914569,-74.9998274178246,
85.6923473348233));
#127603=CARTESIAN_POINT('Ctrl Pts',(-9.56551370279836,-74.9998288616072,
85.6645264180766));
#127604=CARTESIAN_POINT('Ctrl Pts',(-9.55783270403854,-74.9998306249665,
85.6364049762161));
#127605=CARTESIAN_POINT('Ctrl Pts',(-9.54857347396069,-74.9998327271977,
85.6081918997131));
#127606=CARTESIAN_POINT('Ctrl Pts',(-9.53951690601265,-74.9998347834162,
85.5805963391509));
#127607=CARTESIAN_POINT('Ctrl Pts',(-9.52894976120909,-74.9998371640152,
85.5529135806603));
#127608=CARTESIAN_POINT('Ctrl Pts',(-9.51679285414336,-74.9998398786314,
85.525374443191));
#127609=CARTESIAN_POINT('Ctrl Pts',(-9.50486790627308,-74.9998425414514,
85.4983607647169));
#127610=CARTESIAN_POINT('Ctrl Pts',(-9.49141274535437,-74.9998455258108,
85.4714859248127));
#127611=CARTESIAN_POINT('Ctrl Pts',(-9.47639499415803,-74.9998488301971,
85.444993978127));
#127612=CARTESIAN_POINT('Ctrl Pts',(-9.46162100402897,-74.9998520809482,
85.4189320362478));
#127613=CARTESIAN_POINT('Ctrl Pts',(-9.44533438718281,-74.9998556415217,
85.3932414401984));
#127614=CARTESIAN_POINT('Ctrl Pts',(-9.42755231432449,-74.9998594982772,
85.3681696172929));
#127615=CARTESIAN_POINT('Ctrl Pts',(-9.41000756113224,-74.9998633035605,
85.3434324031075));
#127616=CARTESIAN_POINT('Ctrl Pts',(-9.39100687524507,-74.9998673972163,
85.3192984171782));
#127617=CARTESIAN_POINT('Ctrl Pts',(-9.37061743520078,-74.999871753094,
85.2960079213209));
#127618=CARTESIAN_POINT('Ctrl Pts',(-9.34984201493274,-74.9998761914302,
85.2722765270973));
#127619=CARTESIAN_POINT('Ctrl Pts',(-9.32762462572471,-74.9998809020583,
85.2494218850682));
#127620=CARTESIAN_POINT('Ctrl Pts',(-9.30409180453394,-74.9998858428542,
85.2276865690306));
#127621=CARTESIAN_POINT('Ctrl Pts',(-9.28144013241718,-74.9998905986497,
85.2067650973445));
#127622=CARTESIAN_POINT('Ctrl Pts',(-9.25757030985327,-74.9998955675488,
85.186881423829));
#127623=CARTESIAN_POINT('Ctrl Pts',(-9.23264164306874,-74.9999006997037,
85.1682285148043));
#127624=CARTESIAN_POINT('Ctrl Pts',(-9.20779321329438,-74.9999058153399,
85.1496356432322));
#127625=CARTESIAN_POINT('Ctrl Pts',(-9.18189331394207,-74.9999110930441,
85.1322663161802));
#127626=CARTESIAN_POINT('Ctrl Pts',(-9.15513836009451,-74.9999164730492,
85.1162773047068));
#127627=CARTESIAN_POINT('Ctrl Pts',(-9.12839924598703,-74.9999218498692,
85.1002977592108));
#127628=CARTESIAN_POINT('Ctrl Pts',(-9.10080683593486,-74.9999273286825,
85.0856974009578));
#127629=CARTESIAN_POINT('Ctrl Pts',(-9.07258596059659,-74.9999328418655,
85.0725893291592));
#127630=CARTESIAN_POINT('Ctrl Pts',(-9.04430746240289,-74.9999383663057,
85.0594544926158));
#127631=CARTESIAN_POINT('Ctrl Pts',(-9.01539879073536,-74.9999439250373,
85.0478183180839));
#127632=CARTESIAN_POINT('Ctrl Pts',(-8.9861029073353,-74.9999494450838,
85.0377450762627));
#127633=CARTESIAN_POINT('Ctrl Pts',(-8.95654791083695,-74.9999550139534,
85.0275827397088));
#127634=CARTESIAN_POINT('Ctrl Pts',(-8.92659973489103,-74.9999605432158,
85.0190111633963));
#127635=CARTESIAN_POINT('Ctrl Pts',(-8.89651140595007,-74.999965956364,
85.0120433514983));
#127636=CARTESIAN_POINT('Ctrl Pts',(-8.86622517470663,-74.9999714051166,
85.0050297096699));
#127637=CARTESIAN_POINT('Ctrl Pts',(-8.83579781987997,-74.9999767359927,
84.9996407568067));
#127638=CARTESIAN_POINT('Ctrl Pts',(-8.80547732474302,-74.9999818729188,
84.995837732317));
#127639=CARTESIAN_POINT('Ctrl Pts',(-8.77474583349687,-74.9999870794761,
84.9919831576049));
#127640=CARTESIAN_POINT('Ctrl Pts',(-8.74412491066357,-74.9999920865798,
84.9897573534694));
#127641=CARTESIAN_POINT('Ctrl Pts',(-8.71384962962935,-74.9999968203932,
84.9890718459364));
#127642=CARTESIAN_POINT('Ctrl Pts',(-8.70698518555899,-74.999997893711,
84.988916417879));
#127643=CARTESIAN_POINT('Ctrl Pts',(-8.70013839104334,-74.9999989530079,
84.9888399980106));
#127644=CARTESIAN_POINT('Ctrl Pts',(-8.69331176399212,-74.9999999974771,
84.9888412596817));
#127645=CARTESIAN_POINT('Ctrl Pts',(-10.2209979427679,-67.46798896641,84.5463096825499));
#127646=CARTESIAN_POINT('Ctrl Pts',(-10.2196132646019,-67.4738480541,84.5501279961));
#127647=CARTESIAN_POINT('Ctrl Pts',(-10.1480245164719,-67.77630330004,84.7469081971199));
#127648=CARTESIAN_POINT('Ctrl Pts',(-9.98388527989691,-68.42046765222,85.1308217788001));
#127649=CARTESIAN_POINT('Ctrl Pts',(-9.69703741833592,-69.46700133775,85.64545920484));
#127650=CARTESIAN_POINT('Ctrl Pts',(-9.37340189687591,-70.6706622866,86.1104956752401));
#127651=CARTESIAN_POINT('Ctrl Pts',(-9.05098927287391,-72.06834247106,86.4981844835201));
#127652=CARTESIAN_POINT('Ctrl Pts',(-8.82755044173492,-73.59330681594,86.7431130017399));
#127653=CARTESIAN_POINT('Ctrl Pts',(-8.7822484149829,-74.66230448112,86.7892411673399));
#127654=CARTESIAN_POINT('Ctrl Pts',(-8.78824703444391,-75.1740212775,86.7828639942899));
#127655=CARTESIAN_POINT('Ctrl Pts',(-10.7823181781539,-67.6003915011101,
84.56103425336));
#127656=CARTESIAN_POINT('Ctrl Pts',(-10.7809021555679,-67.60638197925,84.56486670678));
#127657=CARTESIAN_POINT('Ctrl Pts',(-10.7076960644999,-67.91560684941,84.76235822432));
#127658=CARTESIAN_POINT('Ctrl Pts',(-10.5401996588409,-68.57280682492,85.14564918501));
#127659=CARTESIAN_POINT('Ctrl Pts',(-10.2509568505849,-69.62827488174,85.65066970524));
#127660=CARTESIAN_POINT('Ctrl Pts',(-9.92861982731791,-70.82766304517,86.09858814927));
#127661=CARTESIAN_POINT('Ctrl Pts',(-9.61403567119891,-72.1924890331,86.46193063502));
#127662=CARTESIAN_POINT('Ctrl Pts',(-9.39940208312791,-73.65946242481,86.68685818601));
#127663=CARTESIAN_POINT('Ctrl Pts',(-9.35621111589692,-74.67798882017,86.72863385846));
#127664=CARTESIAN_POINT('Ctrl Pts',(-9.36195895040191,-75.16571991393,86.72284269434));
#127665=CARTESIAN_POINT('Ctrl Pts',(-11.1116938129149,-67.91511854175,84.2070762476901));
#127666=CARTESIAN_POINT('Ctrl Pts',(-11.1102593978189,-67.921002933,84.21079725143));
#127667=CARTESIAN_POINT('Ctrl Pts',(-11.0361042703119,-68.22474376388,84.40253481458));
#127668=CARTESIAN_POINT('Ctrl Pts',(-10.8666379201759,-68.8694457640601,
84.77340996466));
#127669=CARTESIAN_POINT('Ctrl Pts',(-10.5759897874039,-69.89736182966,85.25658866886));
#127670=CARTESIAN_POINT('Ctrl Pts',(-10.2544147065009,-71.05644978244,85.67978174226));
#127671=CARTESIAN_POINT('Ctrl Pts',(-9.94442419660191,-72.3579693818601,
86.01654748832));
#127672=CARTESIAN_POINT('Ctrl Pts',(-9.73495741411192,-73.74276331425,86.22195023037));
#127673=CARTESIAN_POINT('Ctrl Pts',(-9.69300518998291,-74.69786958715,86.25970207886));
#127674=CARTESIAN_POINT('Ctrl Pts',(-9.69860586703891,-75.15534537984,86.25445790011));
#127675=CARTESIAN_POINT('Ctrl Pts',(-10.9884700791849,-68.20132868183,83.72155861371));
#127676=CARTESIAN_POINT('Ctrl Pts',(-10.9870425449669,-68.20694057842,83.7251172404199));
#127677=CARTESIAN_POINT('Ctrl Pts',(-10.9132424644069,-68.49661756483,83.9084902576501));
#127678=CARTESIAN_POINT('Ctrl Pts',(-10.7445130962709,-69.1116606135,84.26347398636));
#127679=CARTESIAN_POINT('Ctrl Pts',(-10.4543907137839,-70.09399590872,84.7272181967299));
#127680=CARTESIAN_POINT('Ctrl Pts',(-10.1325305802749,-71.20375407453,85.13464253368));
#127681=CARTESIAN_POINT('Ctrl Pts',(-9.82082152723193,-72.45392520214,85.4604053674));
#127682=CARTESIAN_POINT('Ctrl Pts',(-9.60942177518391,-73.78740469336,85.6598394857501));
#127683=CARTESIAN_POINT('Ctrl Pts',(-9.56700612105591,-74.7086282923,85.69659181281));
#127684=CARTESIAN_POINT('Ctrl Pts',(-9.5726618516389,-75.14984776556,85.6914891603501));
#127685=CARTESIAN_POINT('Ctrl Pts',(-10.8652463454549,-68.48753882192,83.23604097973));
#127686=CARTESIAN_POINT('Ctrl Pts',(-10.8638256921159,-68.49287822383,83.2394372294));
#127687=CARTESIAN_POINT('Ctrl Pts',(-10.7903806585019,-68.7684913657901,
83.41444570072));
#127688=CARTESIAN_POINT('Ctrl Pts',(-10.6223882723649,-69.35387546295,83.7535380080601));
#127689=CARTESIAN_POINT('Ctrl Pts',(-10.3327916401629,-70.29062998778,84.1978477246001));
#127690=CARTESIAN_POINT('Ctrl Pts',(-10.0106464540489,-71.3510583666101,
84.5895033251));
#127691=CARTESIAN_POINT('Ctrl Pts',(-9.69721885786292,-72.54988102242,84.90426324647));
#127692=CARTESIAN_POINT('Ctrl Pts',(-9.48388613625691,-73.83204607248,85.09772874113));
#127693=CARTESIAN_POINT('Ctrl Pts',(-9.44100705212892,-74.71938699745,85.13348154676));
#127694=CARTESIAN_POINT('Ctrl Pts',(-9.44671783623892,-75.14435015128,85.12852042059));
#127695=CARTESIAN_POINT('Ctrl Pts',(-10.3719730784129,-68.55349464875,82.94422086921));
#127696=CARTESIAN_POINT('Ctrl Pts',(-10.3705799697159,-68.55857769736,82.947512593833));
#127697=CARTESIAN_POINT('Ctrl Pts',(-10.2985562139839,-68.82096881656,83.11714949015));
#127698=CARTESIAN_POINT('Ctrl Pts',(-10.1335140185879,-69.37940206064,83.44752071946));
#127699=CARTESIAN_POINT('Ctrl Pts',(-9.84602200173092,-70.28308242848,83.8878227876));
#127700=CARTESIAN_POINT('Ctrl Pts',(-9.52273573000191,-71.31819837143,84.2832300510801));
#127701=CARTESIAN_POINT('Ctrl Pts',(-9.20242868482291,-72.51202975347,84.60993193985));
#127702=CARTESIAN_POINT('Ctrl Pts',(-8.98135815021491,-73.80812186411,84.81498348635));
#127703=CARTESIAN_POINT('Ctrl Pts',(-8.93662392322791,-74.71381618721,84.8534306707901));
#127704=CARTESIAN_POINT('Ctrl Pts',(-8.9425550904749,-75.14741240926,84.84811080078));
#127705=CARTESIAN_POINT('Ctrl Pts',(-9.83910307039591,-68.35501114641,83.04159391677));
#127706=CARTESIAN_POINT('Ctrl Pts',(-9.83773971744291,-68.36002571887,83.04490899157));
#127707=CARTESIAN_POINT('Ctrl Pts',(-9.76725133045291,-68.61889431212,83.21576580024));
#127708=CARTESIAN_POINT('Ctrl Pts',(-9.60539614775291,-69.17113967145,83.5504287047001));
#127709=CARTESIAN_POINT('Ctrl Pts',(-9.3201776909509,-70.07640947898,84.0048347668901));
#127710=CARTESIAN_POINT('Ctrl Pts',(-8.99565873474091,-71.1271876013501,
84.4210007850601));
#127711=CARTESIAN_POINT('Ctrl Pts',(-8.66792000354691,-72.36572865333,84.77458937839));
#127712=CARTESIAN_POINT('Ctrl Pts',(-8.43849051508591,-73.73165933346,85.0010199440401));
#127713=CARTESIAN_POINT('Ctrl Pts',(-8.39175222654391,-74.69564784935,85.0440503938199));
#127714=CARTESIAN_POINT('Ctrl Pts',(-8.39792146783991,-75.15698307681,85.0381118389));
#127715=CARTESIAN_POINT('Origin',(-10.0948615431041,-68.0757444516113,83.873039637936));
#127716=CARTESIAN_POINT('Ctrl Pts',(-10.1785854175429,-67.85588330056,61.19532449647));
#127717=CARTESIAN_POINT('Ctrl Pts',(-10.1850298753019,-67.82902615816,61.21159366354));
#127718=CARTESIAN_POINT('Ctrl Pts',(-10.2405662560859,-67.59793547837,61.35266188607));
#127719=CARTESIAN_POINT('Ctrl Pts',(-10.3533091174039,-67.13450494732,61.65463623851));
#127720=CARTESIAN_POINT('Ctrl Pts',(-10.5195786451669,-66.45531759647,62.15428395171));
#127721=CARTESIAN_POINT('Ctrl Pts',(-10.6976369657359,-65.72051916043,62.77307815338));
#127722=CARTESIAN_POINT('Ctrl Pts',(-10.8773515530769,-64.95635886287,63.519467755676));
#127723=CARTESIAN_POINT('Ctrl Pts',(-11.0500634386659,-64.18718474885,64.403598938773));
#127724=CARTESIAN_POINT('Ctrl Pts',(-11.2102175450769,-63.4329994378,65.4436382220611));
#127725=CARTESIAN_POINT('Ctrl Pts',(-11.3532874167409,-62.71533896826,66.6679533293209));
#127726=CARTESIAN_POINT('Ctrl Pts',(-11.4749421508609,-62.0659368475,68.113631709785));
#127727=CARTESIAN_POINT('Ctrl Pts',(-11.5688811502722,-61.5357441304,69.820891505791));
#127728=CARTESIAN_POINT('Ctrl Pts',(-11.6237522292211,-61.21258620971,71.773832111478));
#127729=CARTESIAN_POINT('Ctrl Pts',(-11.6284201506308,-61.1848010717,73.857068402466));
#127730=CARTESIAN_POINT('Ctrl Pts',(-11.5808138773938,-61.46645898683,75.861242610505));
#127731=CARTESIAN_POINT('Ctrl Pts',(-11.4904794662569,-61.98015285862,77.637523541923));
#127732=CARTESIAN_POINT('Ctrl Pts',(-11.3699894781989,-62.62857578264,79.142058916883));
#127733=CARTESIAN_POINT('Ctrl Pts',(-11.2268663935649,-63.35208396897,80.410836525289));
#127734=CARTESIAN_POINT('Ctrl Pts',(-11.0656654745509,-64.11575643041,81.484871784862));
#127735=CARTESIAN_POINT('Ctrl Pts',(-10.8912137555179,-64.89642330348,82.395342195428));
#127736=CARTESIAN_POINT('Ctrl Pts',(-10.7089402192919,-65.67337171062,83.1624171289));
#127737=CARTESIAN_POINT('Ctrl Pts',(-10.5277886673999,-66.42174040101,83.7974836243801));
#127738=CARTESIAN_POINT('Ctrl Pts',(-10.3581235993269,-67.1148137986,84.3098671031399));
#127739=CARTESIAN_POINT('Ctrl Pts',(-10.2425760647809,-67.5895814439499,
84.6199517927501));
#127740=CARTESIAN_POINT('Ctrl Pts',(-10.1854502907699,-67.82725682396,84.7651133990399));
#127741=CARTESIAN_POINT('Ctrl Pts',(-10.1785764846769,-67.85590275553,84.7824661081499));
#127742=CARTESIAN_POINT('Ctrl Pts',(-10.7233079330559,-68.00453699972,61.20971563528));
#127743=CARTESIAN_POINT('Ctrl Pts',(-10.7297606902689,-67.9776801853,61.22566612772));
#127744=CARTESIAN_POINT('Ctrl Pts',(-10.7853820779999,-67.74653156878,61.36401929391));
#127745=CARTESIAN_POINT('Ctrl Pts',(-10.8985266262999,-67.28195020988,61.66103214993));
#127746=CARTESIAN_POINT('Ctrl Pts',(-11.0658987462389,-66.59877623104,62.15484889246));
#127747=CARTESIAN_POINT('Ctrl Pts',(-11.2455867209609,-65.85758537412,62.76912806206));
#127748=CARTESIAN_POINT('Ctrl Pts',(-11.4272960177459,-65.08510007019,63.512959516944));
#127749=CARTESIAN_POINT('Ctrl Pts',(-11.6019946953778,-64.30706109192,64.396071768386));
#127750=CARTESIAN_POINT('Ctrl Pts',(-11.7639748214603,-63.54414794216,65.436512178071));
#127751=CARTESIAN_POINT('Ctrl Pts',(-11.9085537069501,-62.81872865971,66.6619954797));
#127752=CARTESIAN_POINT('Ctrl Pts',(-12.0313720955718,-62.1629201997,68.10924847471));
#127753=CARTESIAN_POINT('Ctrl Pts',(-12.1261231817684,-61.6279818110999,
69.8182781818619));
#127754=CARTESIAN_POINT('Ctrl Pts',(-12.1814253595411,-61.30218855351,71.772869650253));
#127755=CARTESIAN_POINT('Ctrl Pts',(-12.1861300800116,-61.27417565406,73.8577126819013));
#127756=CARTESIAN_POINT('Ctrl Pts',(-12.1381497767974,-61.55812922566,75.863657594818));
#127757=CARTESIAN_POINT('Ctrl Pts',(-12.0470505708238,-62.07633100854,77.64164293623));
#127758=CARTESIAN_POINT('Ctrl Pts',(-11.9254239898882,-62.73106818597,79.147840288293));
#127759=CARTESIAN_POINT('Ctrl Pts',(-11.7808009392146,-63.46234925653,80.417907163538));
#127760=CARTESIAN_POINT('Ctrl Pts',(-11.6177839675048,-64.2347707502,81.4923857304049));
#127761=CARTESIAN_POINT('Ctrl Pts',(-11.4413148751619,-65.0244906302599,
82.401998788017));
#127762=CARTESIAN_POINT('Ctrl Pts',(-11.2570027672979,-65.80998285409,83.16660599563));
#127763=CARTESIAN_POINT('Ctrl Pts',(-11.0741741737809,-66.56495328861,83.79717032534));
#127764=CARTESIAN_POINT('Ctrl Pts',(-10.9033624485049,-67.2621908432,84.30367256423));
#127765=CARTESIAN_POINT('Ctrl Pts',(-10.7873948695429,-67.73817520654,84.6086930769));
#127766=CARTESIAN_POINT('Ctrl Pts',(-10.7301812558329,-67.97591244501,84.75106289439));
#127767=CARTESIAN_POINT('Ctrl Pts',(-10.7232986708699,-68.00455776379,84.76807553907));
#127768=CARTESIAN_POINT('Ctrl Pts',(-11.0265915836499,-68.30671850109,61.57813520514));
#127769=CARTESIAN_POINT('Ctrl Pts',(-11.0330489617269,-68.28068236006,61.59340875318));
#127770=CARTESIAN_POINT('Ctrl Pts',(-11.0887176785409,-68.05656087501,61.72591938424));
#127771=CARTESIAN_POINT('Ctrl Pts',(-11.2020858729929,-67.60548761868,62.01090569511));
#127772=CARTESIAN_POINT('Ctrl Pts',(-11.3700718801319,-66.94081207514,62.48616605829));
#127773=CARTESIAN_POINT('Ctrl Pts',(-11.5506671928959,-66.2184602959799,
63.078991875129));
#127774=CARTESIAN_POINT('Ctrl Pts',(-11.7334870785492,-65.46461996317,63.798576759107));
#127775=CARTESIAN_POINT('Ctrl Pts',(-11.9092919369002,-64.70507433139,64.6541034439819));
#127776=CARTESIAN_POINT('Ctrl Pts',(-12.0722887309123,-63.9602739817501,
65.6629970275841));
#127777=CARTESIAN_POINT('Ctrl Pts',(-12.2177077858624,-63.25239876227,66.851736936753));
#127778=CARTESIAN_POINT('Ctrl Pts',(-12.3411740591877,-62.61281265647,68.255713330532));
#127779=CARTESIAN_POINT('Ctrl Pts',(-12.4363772887007,-62.09139235649,69.913585361883));
#127780=CARTESIAN_POINT('Ctrl Pts',(-12.4919194881749,-61.77398372438,71.809446369507));
#127781=CARTESIAN_POINT('Ctrl Pts',(-12.4966446971569,-61.74669107217,73.8315534842725));
#127782=CARTESIAN_POINT('Ctrl Pts',(-12.4484561463053,-62.02333606787,75.777270406522));
#127783=CARTESIAN_POINT('Ctrl Pts',(-12.3569311276225,-62.5283895667699,
77.501952488849));
#127784=CARTESIAN_POINT('Ctrl Pts',(-12.2346717290096,-63.166882314,78.963124476845));
#127785=CARTESIAN_POINT('Ctrl Pts',(-12.0892135463862,-63.88044861778,80.195157982113));
#127786=CARTESIAN_POINT('Ctrl Pts',(-11.9251854560324,-64.63447944362,81.23707495747));
#127787=CARTESIAN_POINT('Ctrl Pts',(-11.7475931563231,-65.4054610954199,
82.118389008027));
#127788=CARTESIAN_POINT('Ctrl Pts',(-11.5621460385589,-66.17204120784,82.858168756855));
#127789=CARTESIAN_POINT('Ctrl Pts',(-11.3783837232079,-66.90787617342,83.46678987785));
#127790=CARTESIAN_POINT('Ctrl Pts',(-11.2069335767679,-67.5862913034,83.95431827718));
#127791=CARTESIAN_POINT('Ctrl Pts',(-11.0907321308349,-68.04845841504,84.24700650097));
#127792=CARTESIAN_POINT('Ctrl Pts',(-11.0334696108579,-68.27896957299,84.38336540787));
#127793=CARTESIAN_POINT('Ctrl Pts',(-11.0265821381089,-68.30673940993,84.39965592943));
#127794=CARTESIAN_POINT('Ctrl Pts',(-10.8914619965499,-68.56616924746,62.0613048488));
#127795=CARTESIAN_POINT('Ctrl Pts',(-10.8979173157779,-68.54124112046,62.07598283942));
#127796=CARTESIAN_POINT('Ctrl Pts',(-10.9535649448759,-68.32666790684,62.20331802211));
#127797=CARTESIAN_POINT('Ctrl Pts',(-11.0668334926369,-67.89498854316,62.47702364874));
#127798=CARTESIAN_POINT('Ctrl Pts',(-11.2345459791829,-67.2592822743,62.93305408088));
#127799=CARTESIAN_POINT('Ctrl Pts',(-11.4147370228249,-66.56876560972,63.5014215856259));
#127800=CARTESIAN_POINT('Ctrl Pts',(-11.5970620799083,-65.84843083062,64.190818954792));
#127801=CARTESIAN_POINT('Ctrl Pts',(-11.7723740737627,-65.1227258372001,
65.010109503435));
#127802=CARTESIAN_POINT('Ctrl Pts',(-11.9349178861608,-64.411115162,65.975997102607));
#127803=CARTESIAN_POINT('Ctrl Pts',(-12.0799625992957,-63.73469249597,67.113945853266));
#127804=CARTESIAN_POINT('Ctrl Pts',(-12.2031402042661,-63.12342146587,68.457901389867));
#127805=CARTESIAN_POINT('Ctrl Pts',(-12.2981419790039,-62.6250033886,70.04491365903));
#127806=CARTESIAN_POINT('Ctrl Pts',(-12.3535772355771,-62.3215537612,71.859806698113));
#127807=CARTESIAN_POINT('Ctrl Pts',(-12.3582933157977,-62.29546158414,73.7955804875104));
#127808=CARTESIAN_POINT('Ctrl Pts',(-12.3101975507498,-62.55994049022,75.658187143643));
#127809=CARTESIAN_POINT('Ctrl Pts',(-12.2188622551049,-63.0427289581601,
77.309177295583));
#127810=CARTESIAN_POINT('Ctrl Pts',(-12.0968848116561,-63.6529689013,78.707879311435));
#127811=CARTESIAN_POINT('Ctrl Pts',(-11.9517987263592,-64.33483804012,79.887258435538));
#127812=CARTESIAN_POINT('Ctrl Pts',(-11.7882211451067,-65.05528272997,80.884756776892));
#127813=CARTESIAN_POINT('Ctrl Pts',(-11.6111292962042,-65.79190488112,81.728709591473));
#127814=CARTESIAN_POINT('Ctrl Pts',(-11.4261878879259,-66.52439984917,82.437426898831));
#127815=CARTESIAN_POINT('Ctrl Pts',(-11.2428415971309,-67.22779009247,83.02091527749));
#127816=CARTESIAN_POINT('Ctrl Pts',(-11.0716759025169,-67.87662086228,83.48870022348));
#127817=CARTESIAN_POINT('Ctrl Pts',(-10.9555786572129,-68.3189106767101,
83.76979752821));
#127818=CARTESIAN_POINT('Ctrl Pts',(-10.8983379276749,-68.53960095533,83.9008303234899));
#127819=CARTESIAN_POINT('Ctrl Pts',(-10.8914526327039,-68.56618904268,83.9164856622999));
#127820=CARTESIAN_POINT('Ctrl Pts',(-10.7563324094499,-68.82561999382,62.54447449247));
#127821=CARTESIAN_POINT('Ctrl Pts',(-10.7627856698279,-68.80179988086,62.5585569256599));
#127822=CARTESIAN_POINT('Ctrl Pts',(-10.8184122112099,-68.59677493867,62.68071665998));
#127823=CARTESIAN_POINT('Ctrl Pts',(-10.9315811122809,-68.1844894676501,
62.94314160236));
#127824=CARTESIAN_POINT('Ctrl Pts',(-11.0990200782339,-67.57775247346,63.379942103459));
#127825=CARTESIAN_POINT('Ctrl Pts',(-11.2788068527549,-66.91907092346,63.923851296123));
#127826=CARTESIAN_POINT('Ctrl Pts',(-11.4606370812679,-66.23224169808,64.583061150478));
#127827=CARTESIAN_POINT('Ctrl Pts',(-11.6354562106252,-65.540377343,65.366115562889));
#127828=CARTESIAN_POINT('Ctrl Pts',(-11.7975470414093,-64.86195634224,66.288997177629));
#127829=CARTESIAN_POINT('Ctrl Pts',(-11.942217412729,-64.21698622967,67.37615476978));
#127830=CARTESIAN_POINT('Ctrl Pts',(-12.0651063493446,-63.63403027526,68.660089449201));
#127831=CARTESIAN_POINT('Ctrl Pts',(-12.1599066693072,-63.15861442072,70.176241956177));
#127832=CARTESIAN_POINT('Ctrl Pts',(-12.2152349829793,-62.86912379802,71.910167026718));
#127833=CARTESIAN_POINT('Ctrl Pts',(-12.2199419344384,-62.84423209612,73.7596074907483));
#127834=CARTESIAN_POINT('Ctrl Pts',(-12.1719389551942,-63.09654491258,75.539103880765));
#127835=CARTESIAN_POINT('Ctrl Pts',(-12.0807933825874,-63.5570683495501,
77.116402102318));
#127836=CARTESIAN_POINT('Ctrl Pts',(-11.9590978943026,-64.13905548859,78.452634146025));
#127837=CARTESIAN_POINT('Ctrl Pts',(-11.8143839063321,-64.78922746246,79.579358888962));
#127838=CARTESIAN_POINT('Ctrl Pts',(-11.6512568341809,-65.47608601633,80.532438596313));
#127839=CARTESIAN_POINT('Ctrl Pts',(-11.4746654360849,-66.17834866682,81.339030174918));
#127840=CARTESIAN_POINT('Ctrl Pts',(-11.2902297372939,-66.87675849051,82.0166850408071));
#127841=CARTESIAN_POINT('Ctrl Pts',(-11.1072994710539,-67.54770401151,82.57504067714));
#127842=CARTESIAN_POINT('Ctrl Pts',(-10.9364182282669,-68.16695042115,83.02308216978));
#127843=CARTESIAN_POINT('Ctrl Pts',(-10.8204251835919,-68.58936293838,83.2925885554499));
#127844=CARTESIAN_POINT('Ctrl Pts',(-10.7632062444909,-68.80023233767,83.4182952391));
#127845=CARTESIAN_POINT('Ctrl Pts',(-10.7563231272989,-68.82563867543,83.43331539516));
#127846=CARTESIAN_POINT('Ctrl Pts',(-10.2705525273999,-68.8738338756999,
62.8285888422));
#127847=CARTESIAN_POINT('Ctrl Pts',(-10.2769983863809,-68.85068949284,62.84254390307));
#127848=CARTESIAN_POINT('Ctrl Pts',(-10.3325491191389,-68.6515326229,62.96355658686));
#127849=CARTESIAN_POINT('Ctrl Pts',(-10.4453597984549,-68.2519310358,63.222773199426));
#127850=CARTESIAN_POINT('Ctrl Pts',(-10.6118154801089,-67.66581941013,63.652159528043));
#127851=CARTESIAN_POINT('Ctrl Pts',(-10.7901489399979,-67.03129298199,64.184490448952));
#127852=CARTESIAN_POINT('Ctrl Pts',(-10.9702003000219,-66.37106895915,64.82717780351));
#127853=CARTESIAN_POINT('Ctrl Pts',(-11.1432476215749,-65.7064139723,65.5888798818629));
#127854=CARTESIAN_POINT('Ctrl Pts',(-11.3037100202759,-65.05470374144,66.4852275554991));
#127855=CARTESIAN_POINT('Ctrl Pts',(-11.4470346631969,-64.43466710615,67.540533680774));
#127856=CARTESIAN_POINT('Ctrl Pts',(-11.5688858605402,-63.87372908761,68.786685139671));
#127857=CARTESIAN_POINT('Ctrl Pts',(-11.6629619669604,-63.41586028015,70.25829726077));
#127858=CARTESIAN_POINT('Ctrl Pts',(-11.7179058295959,-63.13683705251,71.941603319142));
#127859=CARTESIAN_POINT('Ctrl Pts',(-11.7225799638996,-63.1128463781799,
73.737184164859));
#127860=CARTESIAN_POINT('Ctrl Pts',(-11.6749105420778,-63.3560371312,75.464665840692));
#127861=CARTESIAN_POINT('Ctrl Pts',(-11.5844470083718,-63.79963931423,76.995744338442));
#127862=CARTESIAN_POINT('Ctrl Pts',(-11.4637651259839,-64.35971469293,78.2926343272081));
#127863=CARTESIAN_POINT('Ctrl Pts',(-11.3203887976569,-64.98479353874,79.386281247239));
#127864=CARTESIAN_POINT('Ctrl Pts',(-11.1588812691069,-65.64468375819,80.311933956733));
#127865=CARTESIAN_POINT('Ctrl Pts',(-10.9840889509839,-66.31928118437,81.096367163558));
#127866=CARTESIAN_POINT('Ctrl Pts',(-10.8014712366919,-66.99057019265,81.756898804972));
#127867=CARTESIAN_POINT('Ctrl Pts',(-10.6200365449139,-67.63683369098,82.303255188861));
#127868=CARTESIAN_POINT('Ctrl Pts',(-10.4501778833209,-68.2349480315001,
82.743606443185));
#127869=CARTESIAN_POINT('Ctrl Pts',(-10.3345594314369,-68.64433296274,83.00979126212));
#127870=CARTESIAN_POINT('Ctrl Pts',(-10.2774188271899,-68.84916507436,83.13431579583));
#127871=CARTESIAN_POINT('Ctrl Pts',(-10.2705435389349,-68.87385090858,83.14920024321));
#127872=CARTESIAN_POINT('Ctrl Pts',(-9.74962299603692,-68.67949730555,62.72912345785));
#127873=CARTESIAN_POINT('Ctrl Pts',(-9.75606091807592,-68.65615750078,62.74350205631));
#127874=CARTESIAN_POINT('Ctrl Pts',(-9.8115303569129,-68.4553773527,62.86814106512));
#127875=CARTESIAN_POINT('Ctrl Pts',(-9.92395689456892,-68.05351180776,63.134305424098));
#127876=CARTESIAN_POINT('Ctrl Pts',(-10.0893581442709,-67.46628603603,63.572908639484));
#127877=CARTESIAN_POINT('Ctrl Pts',(-10.2661331318189,-66.83254665104,64.114061097385));
#127878=CARTESIAN_POINT('Ctrl Pts',(-10.4442769094929,-66.17474813376,64.76462187543));
#127879=CARTESIAN_POINT('Ctrl Pts',(-10.6154242202729,-65.51299951022,65.533723174415));
#127880=CARTESIAN_POINT('Ctrl Pts',(-10.7741403581809,-64.8641732358,66.437242013761));
#127881=CARTESIAN_POINT('Ctrl Pts',(-10.9160218996279,-64.24635739527,67.500323013726));
#127882=CARTESIAN_POINT('Ctrl Pts',(-11.0367602698399,-63.68684013021,68.755468049206));
#127883=CARTESIAN_POINT('Ctrl Pts',(-11.1300597606879,-63.22966687071,70.237786913862));
#127884=CARTESIAN_POINT('Ctrl Pts',(-11.1845913545039,-62.95082114388,71.933698569817));
#127885=CARTESIAN_POINT('Ctrl Pts',(-11.1892302970969,-62.92684685694,73.7428738420364));
#127886=CARTESIAN_POINT('Ctrl Pts',(-11.1419185679629,-63.16988410153,75.483218478992));
#127887=CARTESIAN_POINT('Ctrl Pts',(-11.0521864235499,-63.61289869572,77.02556789635));
#127888=CARTESIAN_POINT('Ctrl Pts',(-10.9325914886959,-64.17163444229,78.331795327822));
#127889=CARTESIAN_POINT('Ctrl Pts',(-10.7906496092569,-64.79452149207,79.433424117582));
#127890=CARTESIAN_POINT('Ctrl Pts',(-10.6308788098719,-65.4515763686501,
80.366454544603));
#127891=CARTESIAN_POINT('Ctrl Pts',(-10.4580157480269,-66.12317064763,81.158323495647));
#127892=CARTESIAN_POINT('Ctrl Pts',(-10.2773475624179,-66.79191739163,81.826792191972));
#127893=CARTESIAN_POINT('Ctrl Pts',(-10.0975166606109,-67.43729186041,82.382075997074));
#127894=CARTESIAN_POINT('Ctrl Pts',(-9.9287545712769,-68.03645111936,82.83178482597));
#127895=CARTESIAN_POINT('Ctrl Pts',(-9.8135378166519,-68.44811923391,83.10507469653));
#127896=CARTESIAN_POINT('Ctrl Pts',(-9.75648121534591,-68.65461870147,83.23332881579));
#127897=CARTESIAN_POINT('Ctrl Pts',(-9.74961432250691,-68.6795132254,83.24866516762));
#127898=CARTESIAN_POINT('Origin',(-10.0948830014566,-68.0758056986579,62.1047072263252));
#127899=CARTESIAN_POINT('Ctrl Pts',(-8.78850469721091,-75.17359603956,59.19490760027));
#127900=CARTESIAN_POINT('Ctrl Pts',(-8.78188852477292,-74.58082390223,59.18747495126));
#127901=CARTESIAN_POINT('Ctrl Pts',(-8.83939730088191,-73.4519410195699,
59.24647973494));
#127902=CARTESIAN_POINT('Ctrl Pts',(-9.0876090788949,-71.8919076279,59.52130962477));
#127903=CARTESIAN_POINT('Ctrl Pts',(-9.40574366428991,-70.55021010581,59.90923180519));
#127904=CARTESIAN_POINT('Ctrl Pts',(-9.7179242559119,-69.39113414181,60.36713913229));
#127905=CARTESIAN_POINT('Ctrl Pts',(-9.99356323184191,-68.38469862843,60.8676797454));
#127906=CARTESIAN_POINT('Ctrl Pts',(-10.1509562713109,-67.76495549583,61.2382841953));
#127907=CARTESIAN_POINT('Ctrl Pts',(-10.2198399627489,-67.47399185811,61.42758621355));
#127908=CARTESIAN_POINT('Ctrl Pts',(-10.2212119301449,-67.46818801423,61.43136843613));
#127909=CARTESIAN_POINT('Ctrl Pts',(-9.36212373097791,-75.16592254393,59.25507590282));
#127910=CARTESIAN_POINT('Ctrl Pts',(-9.35580368697291,-74.60107228412,59.24829590499));
#127911=CARTESIAN_POINT('Ctrl Pts',(-9.41070341504091,-73.52317121109,59.30190722471));
#127912=CARTESIAN_POINT('Ctrl Pts',(-9.64914079436791,-72.0227183761,59.5544042459601));
#127913=CARTESIAN_POINT('Ctrl Pts',(-9.9606708405339,-70.70775665002,59.91952962685));
#127914=CARTESIAN_POINT('Ctrl Pts',(-10.2718202607639,-69.55215247787,60.36120446053));
#127915=CARTESIAN_POINT('Ctrl Pts',(-10.5499421585049,-68.53642237687,60.85287618635));
#127916=CARTESIAN_POINT('Ctrl Pts',(-10.7105856685029,-67.90404690096,61.22299765997));
#127917=CARTESIAN_POINT('Ctrl Pts',(-10.7810225640879,-67.6065779882001,
61.4129801104));
#127918=CARTESIAN_POINT('Ctrl Pts',(-10.7824255217669,-67.60064414927,61.41677625211));
#127919=CARTESIAN_POINT('Ctrl Pts',(-9.69865424996091,-75.15593500828,59.72344078075));
#127920=CARTESIAN_POINT('Ctrl Pts',(-9.69250793843191,-74.62620644493,59.71728021902));
#127921=CARTESIAN_POINT('Ctrl Pts',(-9.74587699154091,-73.61389373368,59.76584842473));
#127922=CARTESIAN_POINT('Ctrl Pts',(-9.97857993168691,-72.1976445875,59.9965061873401));
#127923=CARTESIAN_POINT('Ctrl Pts',(-10.2862352301819,-70.9405985037,60.33596972223));
#127924=CARTESIAN_POINT('Ctrl Pts',(-10.5967796833119,-69.82341248365,60.75367197684));
#127925=CARTESIAN_POINT('Ctrl Pts',(-10.8763582603419,-68.83375635653,61.22439153824));
#127926=CARTESIAN_POINT('Ctrl Pts',(-11.0389087547129,-68.21334787189,61.5826002728));
#127927=CARTESIAN_POINT('Ctrl Pts',(-11.1102568833069,-67.92115734446,61.76704648123));
#127928=CARTESIAN_POINT('Ctrl Pts',(-11.1116780223479,-67.91532865455,61.77073220163));
#127929=CARTESIAN_POINT('Ctrl Pts',(-9.57270218655892,-75.15032266631,60.28631102627));
#127930=CARTESIAN_POINT('Ctrl Pts',(-9.56649085280391,-74.63939257487,60.28032181318));
#127931=CARTESIAN_POINT('Ctrl Pts',(-9.62043278610791,-73.6633464358201,
60.32757492167));
#127932=CARTESIAN_POINT('Ctrl Pts',(-9.8552819341209,-72.29952800127,60.55151405768));
#127933=CARTESIAN_POINT('Ctrl Pts',(-10.1643874204499,-71.09278793092,60.87963793134));
#127934=CARTESIAN_POINT('Ctrl Pts',(-10.4751582924339,-70.02323555163,61.28168335214));
#127935=CARTESIAN_POINT('Ctrl Pts',(-10.7541916833609,-69.07755870261,61.73340035548));
#127936=CARTESIAN_POINT('Ctrl Pts',(-10.9160284575699,-68.48570155355,62.07624524263));
#127937=CARTESIAN_POINT('Ctrl Pts',(-10.9870355422719,-68.20703783005,62.25264647826));
#127938=CARTESIAN_POINT('Ctrl Pts',(-10.9884498766409,-68.20147900883,62.25617139248));
#127939=CARTESIAN_POINT('Ctrl Pts',(-9.44675012315791,-75.14471032433,60.84918127178));
#127940=CARTESIAN_POINT('Ctrl Pts',(-9.4404737671749,-74.65257870482,60.84336340734));
#127941=CARTESIAN_POINT('Ctrl Pts',(-9.49498858067491,-73.71279913797,60.88930141861));
#127942=CARTESIAN_POINT('Ctrl Pts',(-9.73198393655491,-72.4014114150499,
61.10652192802));
#127943=CARTESIAN_POINT('Ctrl Pts',(-10.0425396107169,-71.24497735813,61.42330614046));
#127944=CARTESIAN_POINT('Ctrl Pts',(-10.3535369015559,-70.22305861962,61.80969472745));
#127945=CARTESIAN_POINT('Ctrl Pts',(-10.6320251063809,-69.3213610486901,
62.24240917272));
#127946=CARTESIAN_POINT('Ctrl Pts',(-10.7931481604269,-68.7580552352099,
62.56989021246));
#127947=CARTESIAN_POINT('Ctrl Pts',(-10.8638142012379,-68.49291831565,62.7382464752801));
#127948=CARTESIAN_POINT('Ctrl Pts',(-10.8652217309329,-68.48762936311,62.74161058333));
#127949=CARTESIAN_POINT('Ctrl Pts',(-8.94267290200891,-75.1472320879701,
61.12956993419));
#127950=CARTESIAN_POINT('Ctrl Pts',(-8.93613631826291,-74.64498528552,61.12336056877));
#127951=CARTESIAN_POINT('Ctrl Pts',(-8.99294387591691,-73.68786066791,61.17259229674));
#127952=CARTESIAN_POINT('Ctrl Pts',(-9.23852864643891,-72.3620147815,61.4027146666999));
#127953=CARTESIAN_POINT('Ctrl Pts',(-9.55488816877592,-71.21458424523,61.73007623356));
#127954=CARTESIAN_POINT('Ctrl Pts',(-9.86679161854391,-70.2176116156401,
62.11961002449));
#127955=CARTESIAN_POINT('Ctrl Pts',(-10.1430979147259,-69.34834314582,62.54799863675));
#127956=CARTESIAN_POINT('Ctrl Pts',(-10.3013645639899,-68.8110505217,62.8669547831799));
#127957=CARTESIAN_POINT('Ctrl Pts',(-10.3706657009459,-68.55862913711,63.030145528726));
#127958=CARTESIAN_POINT('Ctrl Pts',(-10.3720459974179,-68.55359402616,63.033406146974));
#127959=CARTESIAN_POINT('Ctrl Pts',(-8.39808036486592,-75.1561989854,60.93968441351));
#127960=CARTESIAN_POINT('Ctrl Pts',(-8.39126263749392,-74.62169807166,60.93278290848));
#127961=CARTESIAN_POINT('Ctrl Pts',(-8.45054721911191,-73.60523376996,60.98771117336));
#127962=CARTESIAN_POINT('Ctrl Pts',(-8.7054117803419,-72.20772431819,61.24171476441));
#127963=CARTESIAN_POINT('Ctrl Pts',(-9.02804163640791,-71.02196462817,61.59448643168));
#127964=CARTESIAN_POINT('Ctrl Pts',(-9.34092407782691,-70.01054271518,62.00386093826));
#127965=CARTESIAN_POINT('Ctrl Pts',(-9.6148730939859,-69.14043351377,62.44549770458));
#127966=CARTESIAN_POINT('Ctrl Pts',(-9.7700537543129,-68.60919338644,62.76847752884));
#127967=CARTESIAN_POINT('Ctrl Pts',(-9.83788028297091,-68.36015993432,62.93284186008));
#127968=CARTESIAN_POINT('Ctrl Pts',(-9.83923115734292,-68.35519262538,62.93612561805));
#127969=CARTESIAN_POINT('Ctrl Pts',(-9.07717754188891,-75.00007042599,59.27469685199));
#127970=CARTESIAN_POINT('Ctrl Pts',(-9.16720240148093,-75.0001184241262,
59.3170480141474));
#127971=CARTESIAN_POINT('Ctrl Pts',(-9.25404279049002,-75.0000081264142,
59.3767114129865));
#127972=CARTESIAN_POINT('Ctrl Pts',(-9.40351821239825,-74.9998108011234,
59.5255401835551));
#127973=CARTESIAN_POINT('Ctrl Pts',(-9.46580962876273,-74.9997241032735,
59.6145335066925));
#127974=CARTESIAN_POINT('Ctrl Pts',(-9.5544246386508,-74.9995852537322,
59.8054548367005));
#127975=CARTESIAN_POINT('Ctrl Pts',(-9.58072200049293,-74.9995331268317,
59.9070017703381));
#127976=CARTESIAN_POINT('Ctrl Pts',(-9.5990568491044,-74.999461759626,60.1039339215817));
#127977=CARTESIAN_POINT('Ctrl Pts',(-9.59135343873692,-74.9994422704594,
60.1991266817374));
#127978=CARTESIAN_POINT('Ctrl Pts',(-9.55275050059125,-74.9994255438882,
60.3716696675316));
#127979=CARTESIAN_POINT('Ctrl Pts',(-9.51915258821981,-74.9994305591295,
60.461075888367));
#127980=CARTESIAN_POINT('Ctrl Pts',(-9.41864283736518,-74.9994712546601,
60.6314235011437));
#127981=CARTESIAN_POINT('Ctrl Pts',(-9.35157790424355,-74.9995070680353,
60.7120836753056));
#127982=CARTESIAN_POINT('Ctrl Pts',(-9.19005028283362,-74.9996032866802,
60.8470403630072));
#127983=CARTESIAN_POINT('Ctrl Pts',(-9.09577378900014,-74.999663508245,
60.9010033430434));
#127984=CARTESIAN_POINT('Ctrl Pts',(-8.89712916494651,-74.9997921275302,
60.971943546326));
#127985=CARTESIAN_POINT('Ctrl Pts',(-8.79314519935482,-74.9998601681799,
60.9889116321022));
#127986=CARTESIAN_POINT('Ctrl Pts',(-8.69365830054091,-75.00000003516,60.98889557741));
#127987=CARTESIAN_POINT('Ctrl Pts',(-10.2211081281489,-82.53194766886,61.43143972309));
#127988=CARTESIAN_POINT('Ctrl Pts',(-10.2201357177169,-82.52783508187,61.42875952001));
#127989=CARTESIAN_POINT('Ctrl Pts',(-10.1636466673389,-82.28917485816,61.27340440246));
#127990=CARTESIAN_POINT('Ctrl Pts',(-10.0368070869879,-81.78301134763,60.9658648185301));
#127991=CARTESIAN_POINT('Ctrl Pts',(-9.81630097459091,-80.9666590177,60.53842194595));
#127992=CARTESIAN_POINT('Ctrl Pts',(-9.56244033240291,-80.03767866059,60.13185887577));
#127993=CARTESIAN_POINT('Ctrl Pts',(-9.28898299286992,-78.9779691788,59.7621739654));
#127994=CARTESIAN_POINT('Ctrl Pts',(-9.02433492858491,-77.76063725352,59.45104885705));
#127995=CARTESIAN_POINT('Ctrl Pts',(-8.82681152382191,-76.3599906814101,
59.23360212967));
#127996=CARTESIAN_POINT('Ctrl Pts',(-8.7826942367269,-75.35421730322,59.18826906547));
#127997=CARTESIAN_POINT('Ctrl Pts',(-8.78852660746291,-74.82645883891,59.19489180675));
#127998=CARTESIAN_POINT('Ctrl Pts',(-10.7823639233799,-82.39954255881,61.4167769709));
#127999=CARTESIAN_POINT('Ctrl Pts',(-10.7813694075629,-82.39533735498,61.41408657358));
#128000=CARTESIAN_POINT('Ctrl Pts',(-10.7235982190879,-82.15131047794,61.25815097326));
#128001=CARTESIAN_POINT('Ctrl Pts',(-10.5941274800899,-81.6347455455,60.95074942728));
#128002=CARTESIAN_POINT('Ctrl Pts',(-10.3707861071929,-80.80778684534,60.52861636853));
#128003=CARTESIAN_POINT('Ctrl Pts',(-10.1166516515639,-79.87750579632,60.13360638867));
#128004=CARTESIAN_POINT('Ctrl Pts',(-9.8458315642529,-78.82770723874,59.78020710747));
#128005=CARTESIAN_POINT('Ctrl Pts',(-9.58828415333991,-77.64224093098,59.48963830546));
#128006=CARTESIAN_POINT('Ctrl Pts',(-9.39873529568491,-76.29731610985,59.29012441741));
#128007=CARTESIAN_POINT('Ctrl Pts',(-9.35661561995691,-75.3371255297,59.24892709446));
#128008=CARTESIAN_POINT('Ctrl Pts',(-9.3621874047499,-74.83402387572,59.25497557751));
#128009=CARTESIAN_POINT('Ctrl Pts',(-11.1116909558609,-82.08485676008,61.77071305075));
#128010=CARTESIAN_POINT('Ctrl Pts',(-11.1106834693079,-82.08072576851,61.76810071081));
#128011=CARTESIAN_POINT('Ctrl Pts',(-11.0521599630159,-81.84101032029,61.6166957882701));
#128012=CARTESIAN_POINT('Ctrl Pts',(-10.9211453438879,-81.33416964011,61.31902500224));
#128013=CARTESIAN_POINT('Ctrl Pts',(-10.6961403303939,-80.5265460574199,
60.91344585688));
#128014=CARTESIAN_POINT('Ctrl Pts',(-10.4418452097559,-79.62464188561,60.5380300981801));
#128015=CARTESIAN_POINT('Ctrl Pts',(-10.1725725780889,-78.61395801647,60.20586918788));
#128016=CARTESIAN_POINT('Ctrl Pts',(-9.91919160451791,-77.48554684164,59.93722926782));
#128017=CARTESIAN_POINT('Ctrl Pts',(-9.73432195722691,-76.2175491581999,
59.75515226542));
#128018=CARTESIAN_POINT('Ctrl Pts',(-9.69337441625392,-75.31589529607,59.71782522343));
#128019=CARTESIAN_POINT('Ctrl Pts',(-9.69879329751091,-74.84394649489,59.72332601301));
#128020=CARTESIAN_POINT('Ctrl Pts',(-10.9885024775799,-81.7986701666301,
62.25617781303));
#128021=CARTESIAN_POINT('Ctrl Pts',(-10.9874998428759,-81.7947305082801,
62.25367949842));
#128022=CARTESIAN_POINT('Ctrl Pts',(-10.9292577495199,-81.56611673017,62.10888171807));
#128023=CARTESIAN_POINT('Ctrl Pts',(-10.7988206361079,-81.08261256883,61.8240166475));
#128024=CARTESIAN_POINT('Ctrl Pts',(-10.5744379260799,-80.31131472407,61.43514752791));
#128025=CARTESIAN_POINT('Ctrl Pts',(-10.3202029039939,-79.4484578645,61.07424270354));
#128026=CARTESIAN_POINT('Ctrl Pts',(-10.0503514291499,-78.47989301382,60.7540472192201));
#128027=CARTESIAN_POINT('Ctrl Pts',(-9.79541195285791,-77.39551035263,60.49402055841));
#128028=CARTESIAN_POINT('Ctrl Pts',(-9.60879199433392,-76.17411857882,60.31720507657));
#128029=CARTESIAN_POINT('Ctrl Pts',(-9.56740600318091,-75.30474683854,60.28089049991));
#128030=CARTESIAN_POINT('Ctrl Pts',(-9.57288207972391,-74.84958042058,60.28623701171));
#128031=CARTESIAN_POINT('Ctrl Pts',(-10.8653139992979,-81.51248357318,62.7416425753));
#128032=CARTESIAN_POINT('Ctrl Pts',(-10.8643162164439,-81.50873524805,62.73925828603));
#128033=CARTESIAN_POINT('Ctrl Pts',(-10.8063555360239,-81.2912231400401,
62.60106764788));
#128034=CARTESIAN_POINT('Ctrl Pts',(-10.6764959283279,-80.83105549755,62.32900829277));
#128035=CARTESIAN_POINT('Ctrl Pts',(-10.4527355217649,-80.09608339071,61.95684919894));
#128036=CARTESIAN_POINT('Ctrl Pts',(-10.1985605982329,-79.2722738434,61.6104553089));
#128037=CARTESIAN_POINT('Ctrl Pts',(-9.9281302802099,-78.34582801118,61.30222525055));
#128038=CARTESIAN_POINT('Ctrl Pts',(-9.67163230119791,-77.30547386363,61.050811849));
#128039=CARTESIAN_POINT('Ctrl Pts',(-9.48326203144091,-76.13068799945,60.8792578877099));
#128040=CARTESIAN_POINT('Ctrl Pts',(-9.44143759010691,-75.29359838101,60.8439557764));
#128041=CARTESIAN_POINT('Ctrl Pts',(-9.44697086193691,-74.85521434627,60.84914801041));
#128042=CARTESIAN_POINT('Ctrl Pts',(-10.3721229628409,-81.44648700826,63.033466560404));
#128043=CARTESIAN_POINT('Ctrl Pts',(-10.3711446046019,-81.44291898027,63.031155889041));
#128044=CARTESIAN_POINT('Ctrl Pts',(-10.3143105744929,-81.23586276699,62.8972233234));
#128045=CARTESIAN_POINT('Ctrl Pts',(-10.1867630388899,-80.79701286147,62.63246723488));
#128046=CARTESIAN_POINT('Ctrl Pts',(-9.9654940543779,-80.0910257475,62.26598172626));
#128047=CARTESIAN_POINT('Ctrl Pts',(-9.71155973831091,-79.29077964255,61.9192959056199));
#128048=CARTESIAN_POINT('Ctrl Pts',(-9.4388119936039,-78.3812453924001,
61.60574375877));
#128049=CARTESIAN_POINT('Ctrl Pts',(-9.17607447350191,-77.34240237262,61.34385874115));
#128050=CARTESIAN_POINT('Ctrl Pts',(-8.98069674798891,-76.1526840562,61.16186671292));
#128051=CARTESIAN_POINT('Ctrl Pts',(-8.93711695013291,-75.29999905499,61.12404109126));
#128052=CARTESIAN_POINT('Ctrl Pts',(-8.9428792060599,-74.85278591516,61.12957580007));
#128053=CARTESIAN_POINT('Ctrl Pts',(-9.83927396841091,-81.64488567277,62.93618296021));
#128054=CARTESIAN_POINT('Ctrl Pts',(-9.8383165967389,-81.64136614092,62.93385618928));
#128055=CARTESIAN_POINT('Ctrl Pts',(-9.78269981195991,-81.4371165775,62.79898052422));
#128056=CARTESIAN_POINT('Ctrl Pts',(-9.65765026435391,-81.00328678021,62.53113344782));
#128057=CARTESIAN_POINT('Ctrl Pts',(-9.43907303949791,-80.29952945763,62.15548485613));
#128058=CARTESIAN_POINT('Ctrl Pts',(-9.18539867836992,-79.49157988093,61.79389977818));
#128059=CARTESIAN_POINT('Ctrl Pts',(-8.91014716050591,-78.56242221897,61.4613028198301));
#128060=CARTESIAN_POINT('Ctrl Pts',(-8.64066837191091,-77.48156077165,61.1768753106));
#128061=CARTESIAN_POINT('Ctrl Pts',(-8.4377197144919,-76.22537355638,60.97573715615));
#128062=CARTESIAN_POINT('Ctrl Pts',(-8.39224341023391,-75.3196616209701,
60.93354232254));
#128063=CARTESIAN_POINT('Ctrl Pts',(-8.3982530630859,-74.84392171622,60.93968686546));
#128064=CARTESIAN_POINT('Origin',(-10.0948738970799,-81.9242545390876,62.1047355865488));
#128065=CARTESIAN_POINT('Ctrl Pts',(-10.9000979577359,-85.14899987206,63.654865562155));
#128066=CARTESIAN_POINT('Ctrl Pts',(-10.9000477186829,-85.1487800261801,
63.654626518916));
#128067=CARTESIAN_POINT('Ctrl Pts',(-10.8750123876449,-85.03922772795,63.535516356367));
#128068=CARTESIAN_POINT('Ctrl Pts',(-10.8237192351409,-84.81696300348,63.302245679743));
#128069=CARTESIAN_POINT('Ctrl Pts',(-10.7430009632029,-84.4733922665001,
62.9660343526));
#128070=CARTESIAN_POINT('Ctrl Pts',(-10.6588871180149,-84.1207589005599,
62.64415049315));
#128071=CARTESIAN_POINT('Ctrl Pts',(-10.5716358795289,-83.75942733737,62.33649495227));
#128072=CARTESIAN_POINT('Ctrl Pts',(-10.4815738635699,-83.38968061365,62.04294556664));
#128073=CARTESIAN_POINT('Ctrl Pts',(-10.3891615445639,-83.01173552994,61.76338234176));
#128074=CARTESIAN_POINT('Ctrl Pts',(-10.2950592384889,-82.62625937344,61.49804807824));
#128075=CARTESIAN_POINT('Ctrl Pts',(-10.2315020580689,-82.36404669929,61.33035293551));
#128076=CARTESIAN_POINT('Ctrl Pts',(-10.1997022332309,-82.23195048545,61.24897957104));
#128077=CARTESIAN_POINT('Ctrl Pts',(-11.4503057701359,-85.02149435186,63.648348588485));
#128078=CARTESIAN_POINT('Ctrl Pts',(-11.4502549602019,-85.02127201958,63.648109994586));
#128079=CARTESIAN_POINT('Ctrl Pts',(-11.4249351524119,-84.91048075584,63.529223852626));
#128080=CARTESIAN_POINT('Ctrl Pts',(-11.3730662784169,-84.68574220319,63.296515421712));
#128081=CARTESIAN_POINT('Ctrl Pts',(-11.2914781830179,-84.33853514106,62.96153745929));
#128082=CARTESIAN_POINT('Ctrl Pts',(-11.2065129108719,-83.9824407764401,
62.6413211441));
#128083=CARTESIAN_POINT('Ctrl Pts',(-11.1184473571699,-83.61789787307,62.33578331032));
#128084=CARTESIAN_POINT('Ctrl Pts',(-11.0276490263389,-83.24534740716,62.04487515227));
#128085=CARTESIAN_POINT('Ctrl Pts',(-10.9346294336719,-82.86520152909,61.76854759814));
#128086=CARTESIAN_POINT('Ctrl Pts',(-10.8400644177689,-82.4781916511,61.50699095751));
#128087=CARTESIAN_POINT('Ctrl Pts',(-10.7763175869489,-82.2154961895,61.34218060436));
#128088=CARTESIAN_POINT('Ctrl Pts',(-10.7444583451179,-82.0833195767701,
61.26233610244));
#128089=CARTESIAN_POINT('Ctrl Pts',(-11.7566449436726,-84.63945239913,63.929825092945));
#128090=CARTESIAN_POINT('Ctrl Pts',(-11.7565938158894,-84.63923537938,63.929594055548));
#128091=CARTESIAN_POINT('Ctrl Pts',(-11.7311156199935,-84.53109144801,63.814473228003));
#128092=CARTESIAN_POINT('Ctrl Pts',(-11.678926201576,-84.31174641896,63.589208692137));
#128093=CARTESIAN_POINT('Ctrl Pts',(-11.5968538146156,-83.97298246405,63.265198385424));
#128094=CARTESIAN_POINT('Ctrl Pts',(-11.5114144935289,-83.62570705904,62.95575715306));
#128095=CARTESIAN_POINT('Ctrl Pts',(-11.4228955535879,-83.27038980136,62.66081388226));
#128096=CARTESIAN_POINT('Ctrl Pts',(-11.3316872647659,-82.90755219152,62.3803649164701));
#128097=CARTESIAN_POINT('Ctrl Pts',(-11.2383295603769,-82.53771004922,62.11440489199));
#128098=CARTESIAN_POINT('Ctrl Pts',(-11.1435069215479,-82.16161060535,61.8630870648701));
#128099=CARTESIAN_POINT('Ctrl Pts',(-11.0796544990849,-81.90665320588,61.70502854942));
#128100=CARTESIAN_POINT('Ctrl Pts',(-11.0477621756589,-81.77846676124,61.6285331978));
#128101=CARTESIAN_POINT('Ctrl Pts',(-11.6201560889415,-84.2510004051699,
64.316483348219));
#128102=CARTESIAN_POINT('Ctrl Pts',(-11.6201051027755,-84.2507930465299,
64.316262066733));
#128103=CARTESIAN_POINT('Ctrl Pts',(-11.5946974764085,-84.1474633713399,
64.206002372866));
#128104=CARTESIAN_POINT('Ctrl Pts',(-11.5426508759679,-83.93787626324,63.990228763609));
#128105=CARTESIAN_POINT('Ctrl Pts',(-11.4607942642209,-83.61415126761,63.679797194182));
#128106=CARTESIAN_POINT('Ctrl Pts',(-11.3755661547679,-83.28224709377,63.383240444918));
#128107=CARTESIAN_POINT('Ctrl Pts',(-11.2872492202299,-82.94260064881,63.100487697675));
#128108=CARTESIAN_POINT('Ctrl Pts',(-11.1962235874359,-82.59568424389,62.83152291331));
#128109=CARTESIAN_POINT('Ctrl Pts',(-11.1030165281019,-82.24195835696,62.57632883436));
#128110=CARTESIAN_POINT('Ctrl Pts',(-11.0083086726939,-81.88212745736,62.33506116619));
#128111=CARTESIAN_POINT('Ctrl Pts',(-10.9445032963929,-81.6381032979,62.18323639217));
#128112=CARTESIAN_POINT('Ctrl Pts',(-10.9126257124109,-81.51538607709,62.10973529188));
#128113=CARTESIAN_POINT('Ctrl Pts',(-11.4836672342099,-83.8625484112,64.703141603492));
#128114=CARTESIAN_POINT('Ctrl Pts',(-11.4836163896619,-83.86235071367,64.702930077918));
#128115=CARTESIAN_POINT('Ctrl Pts',(-11.4582793328239,-83.76383529467,64.5975315177281));
#128116=CARTESIAN_POINT('Ctrl Pts',(-11.4063755503609,-83.56400610752,64.391248835081));
#128117=CARTESIAN_POINT('Ctrl Pts',(-11.3247347138269,-83.25532007118,64.09439600294));
#128118=CARTESIAN_POINT('Ctrl Pts',(-11.2397178160059,-82.9387871285,63.810723736779));
#128119=CARTESIAN_POINT('Ctrl Pts',(-11.1516028868719,-82.61481149627,63.540161513093));
#128120=CARTESIAN_POINT('Ctrl Pts',(-11.0607599101069,-82.28381629625,63.282680910147));
#128121=CARTESIAN_POINT('Ctrl Pts',(-10.9677034958279,-81.94620666469,63.038252776739));
#128122=CARTESIAN_POINT('Ctrl Pts',(-10.8731104238399,-81.60264430937,62.8070352675));
#128123=CARTESIAN_POINT('Ctrl Pts',(-10.8093520937009,-81.36955338991,62.66144423492));
#128124=CARTESIAN_POINT('Ctrl Pts',(-10.7774892491629,-81.2523053929401,
62.59093738595));
#128125=CARTESIAN_POINT('Ctrl Pts',(-10.9929963408319,-83.7199759237,64.943857048887));
#128126=CARTESIAN_POINT('Ctrl Pts',(-10.9929460053909,-83.71978596121,64.94365114242));
#128127=CARTESIAN_POINT('Ctrl Pts',(-10.9678626426279,-83.62512498703,64.841052354269));
#128128=CARTESIAN_POINT('Ctrl Pts',(-10.9164722839509,-83.43308060028,64.640143517834));
#128129=CARTESIAN_POINT('Ctrl Pts',(-10.8356071489709,-83.13626195926,64.350661465033));
#128130=CARTESIAN_POINT('Ctrl Pts',(-10.7513495468499,-82.83166930126,64.073614942909));
#128131=CARTESIAN_POINT('Ctrl Pts',(-10.6639608174649,-82.51963186023,63.80892177283));
#128132=CARTESIAN_POINT('Ctrl Pts',(-10.5737744803679,-82.20042580216,63.5564916609381));
#128133=CARTESIAN_POINT('Ctrl Pts',(-10.4812596278459,-81.87427785351,63.316235685092));
#128134=CARTESIAN_POINT('Ctrl Pts',(-10.3870791967539,-81.54177615285,63.088352361282));
#128135=CARTESIAN_POINT('Ctrl Pts',(-10.3234899953139,-81.31571279398,62.94442831965));
#128136=CARTESIAN_POINT('Ctrl Pts',(-10.2916801383709,-81.20186095682,62.87461613406));
#128137=CARTESIAN_POINT('Ctrl Pts',(-10.4668214943349,-83.9158800948,64.88229121328));
#128138=CARTESIAN_POINT('Ctrl Pts',(-10.4667717048379,-83.91569091757,64.882083139652));
#128139=CARTESIAN_POINT('Ctrl Pts',(-10.4419603929409,-83.82142121439,64.778404382196));
#128140=CARTESIAN_POINT('Ctrl Pts',(-10.3911206083559,-83.6301324804899,
64.575262137112));
#128141=CARTESIAN_POINT('Ctrl Pts',(-10.3110873031249,-83.33430210374,64.282155774695));
#128142=CARTESIAN_POINT('Ctrl Pts',(-10.2276439378039,-83.0304638771,64.00117300774));
#128143=CARTESIAN_POINT('Ctrl Pts',(-10.1410339545129,-82.7188784586,63.732215622428));
#128144=CARTESIAN_POINT('Ctrl Pts',(-10.0515517702039,-82.39967273597,63.475122147589));
#128145=CARTESIAN_POINT('Ctrl Pts',(-9.95961766575091,-82.0728878304499,
63.22973483264));
#128146=CARTESIAN_POINT('Ctrl Pts',(-9.86587973341591,-81.73905528501,62.996304253343));
#128147=CARTESIAN_POINT('Ctrl Pts',(-9.80247189848491,-81.51154958802,62.84839778456));
#128148=CARTESIAN_POINT('Ctrl Pts',(-9.7707188632119,-81.39681512848,62.77652950846));
#128149=CARTESIAN_POINT('Origin',(-10.7325612699948,-84.4008983433199,64.1552576107488));
#128150=CARTESIAN_POINT('Ctrl Pts',(-10.9457112853099,-88.7723095427,73.1633008345938));
#128151=CARTESIAN_POINT('Ctrl Pts',(-10.9450018737129,-88.7745370054799,
72.987400423028));
#128152=CARTESIAN_POINT('Ctrl Pts',(-10.9460260077449,-88.77205014386,72.6044578842011));
#128153=CARTESIAN_POINT('Ctrl Pts',(-10.9558737619719,-88.74262773799,71.9944222624584));
#128154=CARTESIAN_POINT('Ctrl Pts',(-10.9769412377749,-88.6771448963399,
71.310998753955));
#128155=CARTESIAN_POINT('Ctrl Pts',(-11.0102164392899,-88.56545006486,70.560459108714));
#128156=CARTESIAN_POINT('Ctrl Pts',(-11.0530137011699,-88.3969466046301,
69.752251524636));
#128157=CARTESIAN_POINT('Ctrl Pts',(-11.0991047356729,-88.1686714004199,
68.920979936926));
#128158=CARTESIAN_POINT('Ctrl Pts',(-11.1393227521459,-87.888632837,68.107252447975));
#128159=CARTESIAN_POINT('Ctrl Pts',(-11.1675251720229,-87.5709448254,67.341066879205));
#128160=CARTESIAN_POINT('Ctrl Pts',(-11.1808972887479,-87.22746712569,66.633570170775));
#128161=CARTESIAN_POINT('Ctrl Pts',(-11.1788763078239,-86.87105465404,65.992404193633));
#128162=CARTESIAN_POINT('Ctrl Pts',(-11.1627503627999,-86.51320748952,65.419759920927));
#128163=CARTESIAN_POINT('Ctrl Pts',(-11.1340216992209,-86.1624575053199,
64.91289537508));
#128164=CARTESIAN_POINT('Ctrl Pts',(-11.0945767098009,-85.8242611711499,
64.466136015972));
#128165=CARTESIAN_POINT('Ctrl Pts',(-11.0458305932859,-85.50274962242,64.073903342735));
#128166=CARTESIAN_POINT('Ctrl Pts',(-10.9894638587469,-85.2010373165,63.730974057673));
#128167=CARTESIAN_POINT('Ctrl Pts',(-10.9440465981759,-84.99834908578,63.514663353308));
#128168=CARTESIAN_POINT('Ctrl Pts',(-10.9192732707999,-84.89780249114,63.41068261844));
#128169=CARTESIAN_POINT('Ctrl Pts',(-10.9177140490529,-84.89150973702,63.404187754761));
#128170=CARTESIAN_POINT('Ctrl Pts',(-11.4761904670739,-88.6404673409601,
73.1593416733101));
#128171=CARTESIAN_POINT('Ctrl Pts',(-11.4754919605259,-88.64261186187,72.9876546744834));
#128172=CARTESIAN_POINT('Ctrl Pts',(-11.4764990546509,-88.64023131728,72.6137103493763));
#128173=CARTESIAN_POINT('Ctrl Pts',(-11.4862124533569,-88.6118783058,72.0173035258748));
#128174=CARTESIAN_POINT('Ctrl Pts',(-11.5069967010369,-88.54872844628,71.348776611085));
#128175=CARTESIAN_POINT('Ctrl Pts',(-11.5399844616029,-88.44039024958,70.61107031933));
#128176=CARTESIAN_POINT('Ctrl Pts',(-11.582615894791,-88.27588931312,69.813090462725));
#128177=CARTESIAN_POINT('Ctrl Pts',(-11.6287959324594,-88.05129587406,68.987787659599));
#128178=CARTESIAN_POINT('Ctrl Pts',(-11.669305562902,-87.77371776389,68.175949983838));
#128179=CARTESIAN_POINT('Ctrl Pts',(-11.6978313787621,-87.45685828132,67.408646414581));
#128180=CARTESIAN_POINT('Ctrl Pts',(-11.7114009845464,-87.11262810213,66.698289589759));
#128181=CARTESIAN_POINT('Ctrl Pts',(-11.7093587965017,-86.75393399862,66.053125508229));
#128182=CARTESIAN_POINT('Ctrl Pts',(-11.6929225816759,-86.39232720817,65.475670662799));
#128183=CARTESIAN_POINT('Ctrl Pts',(-11.6635630956701,-86.0365935910501,
64.963608459124));
#128184=CARTESIAN_POINT('Ctrl Pts',(-11.6230843718873,-85.69193147085,64.510908749976));
#128185=CARTESIAN_POINT('Ctrl Pts',(-11.5728539359695,-85.36268242413,64.112285611781));
#128186=CARTESIAN_POINT('Ctrl Pts',(-11.5144463383459,-85.05180029684,63.76229349374));
#128187=CARTESIAN_POINT('Ctrl Pts',(-11.4670572666889,-84.84139611019,63.540339695315));
#128188=CARTESIAN_POINT('Ctrl Pts',(-11.4410866627279,-84.73653930447,63.43329389282));
#128189=CARTESIAN_POINT('Ctrl Pts',(-11.4394516418749,-84.72997489958,63.426606166869));
#128190=CARTESIAN_POINT('Ctrl Pts',(-11.7472020744045,-88.1658022693401,
73.1521332719869));
#128191=CARTESIAN_POINT('Ctrl Pts',(-11.746509139036,-88.1678377977,72.9878314959629));
#128192=CARTESIAN_POINT('Ctrl Pts',(-11.7475075277997,-88.16558611108,72.6298738240873));
#128193=CARTESIAN_POINT('Ctrl Pts',(-11.7571522868552,-88.1386590847199,
72.058565121298));
#128194=CARTESIAN_POINT('Ctrl Pts',(-11.7777918387362,-88.07865829698,71.417961246875));
#128195=CARTESIAN_POINT('Ctrl Pts',(-11.8106327512531,-87.97536584284,70.709076227008));
#128196=CARTESIAN_POINT('Ctrl Pts',(-11.8531794657527,-87.8179219397101,
69.940253903915));
#128197=CARTESIAN_POINT('Ctrl Pts',(-11.8994049734258,-87.6019786177801,
69.1425609119151));
#128198=CARTESIAN_POINT('Ctrl Pts',(-11.9400635838349,-87.33393685455,68.355683161392));
#128199=CARTESIAN_POINT('Ctrl Pts',(-11.9687546164803,-87.02686944062,67.610366073095));
#128200=CARTESIAN_POINT('Ctrl Pts',(-11.9824251156254,-86.6923642999,66.919355788869));
#128201=CARTESIAN_POINT('Ctrl Pts',(-11.9803720932708,-86.3429766281501,
66.29098910701));
#128202=CARTESIAN_POINT('Ctrl Pts',(-11.9637773675727,-85.98994563365,65.7278882031509));
#128203=CARTESIAN_POINT('Ctrl Pts',(-11.9340956065262,-85.6419386551799,
65.228039708533));
#128204=CARTESIAN_POINT('Ctrl Pts',(-11.8930887677471,-85.3038582790601,
64.78539468191));
#128205=CARTESIAN_POINT('Ctrl Pts',(-11.8421000216054,-84.98003443023,64.394984537295));
#128206=CARTESIAN_POINT('Ctrl Pts',(-11.7826497862989,-84.67324521565,64.051401372673));
#128207=CARTESIAN_POINT('Ctrl Pts',(-11.7342533542964,-84.46477706569,63.832868896649));
#128208=CARTESIAN_POINT('Ctrl Pts',(-11.7076710847639,-84.3606282937899,
63.727283428551));
#128209=CARTESIAN_POINT('Ctrl Pts',(-11.705997339607,-84.35410721095,63.7206861801679));
#128210=CARTESIAN_POINT('Ctrl Pts',(-11.5910801936143,-87.6419739009899,
73.1461352299971));
#128211=CARTESIAN_POINT('Ctrl Pts',(-11.5903840488516,-87.6439418162,72.9878214938683));
#128212=CARTESIAN_POINT('Ctrl Pts',(-11.5913874525196,-87.6417618083599,
72.6429485013794));
#128213=CARTESIAN_POINT('Ctrl Pts',(-11.6010717528755,-87.6157351480201,
72.0926798649851));
#128214=CARTESIAN_POINT('Ctrl Pts',(-11.6217946597851,-87.5577512951999,
71.475750416479));
#128215=CARTESIAN_POINT('Ctrl Pts',(-11.6547201671793,-87.4580720574301,
70.793843819682));
#128216=CARTESIAN_POINT('Ctrl Pts',(-11.6973156856438,-87.30637374418,70.0550700349761));
#128217=CARTESIAN_POINT('Ctrl Pts',(-11.7435149993737,-87.0986973501601,
69.28954660411));
#128218=CARTESIAN_POINT('Ctrl Pts',(-11.7840877867703,-86.8413680052499,
68.535257011051));
#128219=CARTESIAN_POINT('Ctrl Pts',(-11.8126836428455,-86.5469981707199,
67.821428576924));
#128220=CARTESIAN_POINT('Ctrl Pts',(-11.8262960202688,-86.2266790269099,
67.160002425791));
#128221=CARTESIAN_POINT('Ctrl Pts',(-11.8242492392441,-85.89242826919,66.558836652314));
#128222=CARTESIAN_POINT('Ctrl Pts',(-11.8077458270353,-85.5550029313299,
66.02037389564));
#128223=CARTESIAN_POINT('Ctrl Pts',(-11.778249719238,-85.2226526474,65.542594259322));
#128224=CARTESIAN_POINT('Ctrl Pts',(-11.7375471121017,-84.9001296381899,
65.119778448422));
#128225=CARTESIAN_POINT('Ctrl Pts',(-11.6869952063578,-84.5915372927401,
64.747103648563));
#128226=CARTESIAN_POINT('Ctrl Pts',(-11.6281456042038,-84.29957157528,64.419436216352));
#128227=CARTESIAN_POINT('Ctrl Pts',(-11.5803294831087,-84.10149369279,64.21127282023));
#128228=CARTESIAN_POINT('Ctrl Pts',(-11.5540995762679,-84.00263316253,64.110769627984));
#128229=CARTESIAN_POINT('Ctrl Pts',(-11.5524481390529,-83.99644357262,64.104490221532));
#128230=CARTESIAN_POINT('Ctrl Pts',(-11.4349583128239,-87.11814553264,73.1401371880075));
#128231=CARTESIAN_POINT('Ctrl Pts',(-11.4342589586669,-87.1200458347101,
72.9878114917734));
#128232=CARTESIAN_POINT('Ctrl Pts',(-11.4352673772399,-87.11793750563,72.6560231786716));
#128233=CARTESIAN_POINT('Ctrl Pts',(-11.4449912188959,-87.09281121132,72.1267946086722));
#128234=CARTESIAN_POINT('Ctrl Pts',(-11.4657974808339,-87.03684429341,71.533539586084));
#128235=CARTESIAN_POINT('Ctrl Pts',(-11.4988075831059,-86.94077827202,70.878611412355));
#128236=CARTESIAN_POINT('Ctrl Pts',(-11.5414519055349,-86.79482554866,70.169886166037));
#128237=CARTESIAN_POINT('Ctrl Pts',(-11.5876250253216,-86.59541608253,69.436532296305));
#128238=CARTESIAN_POINT('Ctrl Pts',(-11.6281119897057,-86.34879915595,68.714830860709));
#128239=CARTESIAN_POINT('Ctrl Pts',(-11.6566126692108,-86.06712690083,68.032491080753));
#128240=CARTESIAN_POINT('Ctrl Pts',(-11.6701669249123,-85.76099375391,67.400649062714));
#128241=CARTESIAN_POINT('Ctrl Pts',(-11.6681263852174,-85.4418799102201,
66.826684197617));
#128242=CARTESIAN_POINT('Ctrl Pts',(-11.6517142864979,-85.120060229,66.31285958813));
#128243=CARTESIAN_POINT('Ctrl Pts',(-11.6224038319499,-84.8033666396201,
65.8571488101121));
#128244=CARTESIAN_POINT('Ctrl Pts',(-11.5820054564562,-84.49640099733,65.454162214934));
#128245=CARTESIAN_POINT('Ctrl Pts',(-11.5318903911099,-84.20304015525,65.099222759832));
#128246=CARTESIAN_POINT('Ctrl Pts',(-11.4736414221089,-83.9258979349,64.78747106003));
#128247=CARTESIAN_POINT('Ctrl Pts',(-11.4264056119209,-83.73821031989,64.589676743811));
#128248=CARTESIAN_POINT('Ctrl Pts',(-11.4005280677719,-83.6446380312701,
64.494255827417));
#128249=CARTESIAN_POINT('Ctrl Pts',(-11.3988989384989,-83.63877993428,64.488294262896));
#128250=CARTESIAN_POINT('Ctrl Pts',(-10.9482903854889,-86.86922914558,73.139060295455));
#128251=CARTESIAN_POINT('Ctrl Pts',(-10.9475810269089,-86.87114504394,72.9876208540694));
#128252=CARTESIAN_POINT('Ctrl Pts',(-10.9486050780959,-86.86900686913,72.657920188345));
#128253=CARTESIAN_POINT('Ctrl Pts',(-10.9584521791089,-86.84369829509,72.1326568375601));
#128254=CARTESIAN_POINT('Ctrl Pts',(-10.9795182779059,-86.78736836434,71.544181042512));
#128255=CARTESIAN_POINT('Ctrl Pts',(-11.0127920819299,-86.69124765573,70.897697785394));
#128256=CARTESIAN_POINT('Ctrl Pts',(-11.0555885375789,-86.54617447248,70.201322045947));
#128257=CARTESIAN_POINT('Ctrl Pts',(-11.1016800048009,-86.3495342702701,
69.484795244371));
#128258=CARTESIAN_POINT('Ctrl Pts',(-11.1418994390519,-86.10817841465,68.783148983785));
#128259=CARTESIAN_POINT('Ctrl Pts',(-11.1701034312259,-85.83425367749,68.1223190428309));
#128260=CARTESIAN_POINT('Ctrl Pts',(-11.1834765081089,-85.5379910790401,
67.511996026178));
#128261=CARTESIAN_POINT('Ctrl Pts',(-11.1814554240789,-85.23047992381,66.958807276233));
#128262=CARTESIAN_POINT('Ctrl Pts',(-11.1653279705759,-84.92164105655,66.4646622131589));
#128263=CARTESIAN_POINT('Ctrl Pts',(-11.1365962400459,-84.61884793878,66.0272221703121));
#128264=CARTESIAN_POINT('Ctrl Pts',(-11.0971462247829,-84.32679045813,65.641571644434));
#128265=CARTESIAN_POINT('Ctrl Pts',(-11.0483928917579,-84.04904419777,65.302917614327));
#128266=CARTESIAN_POINT('Ctrl Pts',(-10.9920162348879,-83.7882852518,65.006741888935));
#128267=CARTESIAN_POINT('Ctrl Pts',(-10.9465893877049,-83.61301402036,64.819849403497));
#128268=CARTESIAN_POINT('Ctrl Pts',(-10.9218102393719,-83.52603852108,64.729988468514));
#128269=CARTESIAN_POINT('Ctrl Pts',(-10.9202506491019,-83.5205950042099,
64.724375472001));
#128270=CARTESIAN_POINT('Ctrl Pts',(-10.4321617544179,-87.04922107186,73.1435707901278));
#128271=CARTESIAN_POINT('Ctrl Pts',(-10.4314417857939,-87.0512261270099,
72.9873675219955));
#128272=CARTESIAN_POINT('Ctrl Pts',(-10.4324824159229,-87.0489750465499,
72.6474659132869));
#128273=CARTESIAN_POINT('Ctrl Pts',(-10.4424602378649,-87.0225143174599,
72.1066397846169));
#128274=CARTESIAN_POINT('Ctrl Pts',(-10.4638019028829,-86.96366601015,71.501091268797));
#128275=CARTESIAN_POINT('Ctrl Pts',(-10.4973553719879,-86.8638565438999,
70.839294831367));
#128276=CARTESIAN_POINT('Ctrl Pts',(-10.5403131703229,-86.71425270862,70.1299293360159));
#128277=CARTESIAN_POINT('Ctrl Pts',(-10.5863180420969,-86.5131708543901,
69.40447675936));
#128278=CARTESIAN_POINT('Ctrl Pts',(-10.6262537511339,-86.2683698718599,
68.697945218175));
#128279=CARTESIAN_POINT('Ctrl Pts',(-10.6541430958509,-85.99244945822,68.035338875427));
#128280=CARTESIAN_POINT('Ctrl Pts',(-10.6673240261589,-85.69563537809,67.425156634356));
#128281=CARTESIAN_POINT('Ctrl Pts',(-10.6653235755539,-85.3890144863201,
66.873465711372));
#128282=CARTESIAN_POINT('Ctrl Pts',(-10.6494979984179,-85.0825007902901,
66.381866509769));
#128283=CARTESIAN_POINT('Ctrl Pts',(-10.6213800252729,-84.78325215938,65.947595579691));
#128284=CARTESIAN_POINT('Ctrl Pts',(-10.5829357797369,-84.49623044878,65.566062724265));
#128285=CARTESIAN_POINT('Ctrl Pts',(-10.5356266122269,-84.22482162347,65.232168945831));
#128286=CARTESIAN_POINT('Ctrl Pts',(-10.4812356089069,-83.97186993939,64.94159309689));
#128287=CARTESIAN_POINT('Ctrl Pts',(-10.4377272312729,-83.80335960198,64.759390591149));
#128288=CARTESIAN_POINT('Ctrl Pts',(-10.4141129707359,-83.72020822447,64.672127566615));
#128289=CARTESIAN_POINT('Ctrl Pts',(-10.4126271290499,-83.71500588789,64.666678216697));
#128290=CARTESIAN_POINT('Ctrl Pts',(-11.2240831851649,-88.65122976349,72.9889532029839));
#128291=CARTESIAN_POINT('Ctrl Pts',(-11.3032351536548,-88.5991560625599,
72.9890176977034));
#128292=CARTESIAN_POINT('Ctrl Pts',(-11.3769892253945,-88.5321181182094,
72.9888757744761));
#128293=CARTESIAN_POINT('Ctrl Pts',(-11.4995563634225,-88.374992788323,
72.9886266426874));
#128294=CARTESIAN_POINT('Ctrl Pts',(-11.5481347520047,-88.2850759639086,
72.9885197770362));
#128295=CARTESIAN_POINT('Ctrl Pts',(-11.6123569941101,-88.0972289441662,
72.9883528279406));
#128296=CARTESIAN_POINT('Ctrl Pts',(-11.6280120210786,-87.9995855317363,
72.9882927405526));
#128297=CARTESIAN_POINT('Ctrl Pts',(-11.6292320149507,-87.8121305336596,
72.9882159438058));
#128298=CARTESIAN_POINT('Ctrl Pts',(-11.6150356049613,-87.7225667916036,
72.9881989050114));
#128299=CARTESIAN_POINT('Ctrl Pts',(-11.5663507330197,-87.5602645510202,
72.9881945590678));
#128300=CARTESIAN_POINT('Ctrl Pts',(-11.5288061045921,-87.4774628379731,
72.9882110757354));
#128301=CARTESIAN_POINT('Ctrl Pts',(-11.4244552027482,-87.3215153774326,
72.9882855525215));
#128302=CARTESIAN_POINT('Ctrl Pts',(-11.3575532357774,-87.2485944781033,
72.9883436484516));
#128303=CARTESIAN_POINT('Ctrl Pts',(-11.2004148129803,-87.1271549781129,
72.9884929133032));
#128304=CARTESIAN_POINT('Ctrl Pts',(-11.1103290403818,-87.0788809918115,
72.9885838692378));
#128305=CARTESIAN_POINT('Ctrl Pts',(-10.9215320523432,-87.0152878970258,
72.9887780410119));
#128306=CARTESIAN_POINT('Ctrl Pts',(-10.823110509523,-86.9999796268137,
72.9888808467404));
#128307=CARTESIAN_POINT('Ctrl Pts',(-10.7284497219739,-86.99999983559,72.9890778951927));
#128308=CARTESIAN_POINT('Ctrl Pts',(-10.9175000005819,-84.8914604129799,
82.573632476901));
#128309=CARTESIAN_POINT('Ctrl Pts',(-10.9187148702499,-84.8963481517099,
82.568587786684));
#128310=CARTESIAN_POINT('Ctrl Pts',(-10.9496313599749,-85.0212737335599,
82.439453037357));
#128311=CARTESIAN_POINT('Ctrl Pts',(-11.0058431886349,-85.27706754662,82.164507487811));
#128312=CARTESIAN_POINT('Ctrl Pts',(-11.0708521503739,-85.6539729890001,
81.725209488295));
#128313=CARTESIAN_POINT('Ctrl Pts',(-11.1207286557869,-86.03545424853,81.23869304884));
#128314=CARTESIAN_POINT('Ctrl Pts',(-11.1549334002079,-86.40251457695,80.723477204648));
#128315=CARTESIAN_POINT('Ctrl Pts',(-11.1745731186709,-86.7447659739099,
80.192953837545));
#128316=CARTESIAN_POINT('Ctrl Pts',(-11.1807648168209,-87.06062102531,79.650614129966));
#128317=CARTESIAN_POINT('Ctrl Pts',(-11.1760880469139,-87.35492773232,79.088005209122));
#128318=CARTESIAN_POINT('Ctrl Pts',(-11.1616928465779,-87.63400684917,78.48818413759));
#128319=CARTESIAN_POINT('Ctrl Pts',(-11.1372368107129,-87.902076581,77.828950659358));
#128320=CARTESIAN_POINT('Ctrl Pts',(-11.1008128139689,-88.1581700157699,
77.087248046884));
#128321=CARTESIAN_POINT('Ctrl Pts',(-11.0546164356989,-88.3902796938699,
76.256928159294));
#128322=CARTESIAN_POINT('Ctrl Pts',(-11.0064698093009,-88.57829407792,75.361422431816));
#128323=CARTESIAN_POINT('Ctrl Pts',(-10.9692740524649,-88.7055150063399,
74.45212684179));
#128324=CARTESIAN_POINT('Ctrl Pts',(-10.9486889645929,-88.7677494397999,
73.6016671236896));
#128325=CARTESIAN_POINT('Ctrl Pts',(-10.9451851927139,-88.7754227146399,
73.0611701552288));
#128326=CARTESIAN_POINT('Ctrl Pts',(-10.9459672912859,-88.77230539163,72.8146988191757));
#128327=CARTESIAN_POINT('Ctrl Pts',(-11.4392120691599,-84.72970045485,82.5514119589451));
#128328=CARTESIAN_POINT('Ctrl Pts',(-11.4404857879209,-84.73479847883,82.546218425558));
#128329=CARTESIAN_POINT('Ctrl Pts',(-11.4728940472009,-84.86507337982,82.41329139738));
#128330=CARTESIAN_POINT('Ctrl Pts',(-11.5315139643969,-85.1304815547,82.131221295799));
#128331=CARTESIAN_POINT('Ctrl Pts',(-11.598755706812,-85.51811794423,81.683330398921));
#128332=CARTESIAN_POINT('Ctrl Pts',(-11.6499756528862,-85.9073743459,81.190085371289));
#128333=CARTESIAN_POINT('Ctrl Pts',(-11.6849611287431,-86.28001943032,80.66938665616));
#128334=CARTESIAN_POINT('Ctrl Pts',(-11.7050077077243,-86.62644648557,80.133835806426));
#128335=CARTESIAN_POINT('Ctrl Pts',(-11.7113084987726,-86.94510548552,79.587146028598));
#128336=CARTESIAN_POINT('Ctrl Pts',(-11.7065522361436,-87.24050734235,79.021973767765));
#128337=CARTESIAN_POINT('Ctrl Pts',(-11.6919769255882,-87.51959465724,78.4207110295121));
#128338=CARTESIAN_POINT('Ctrl Pts',(-11.667258928563,-87.78680743792,77.760882962257));
#128339=CARTESIAN_POINT('Ctrl Pts',(-11.6305324924398,-88.04095857353,77.020117236076));
#128340=CARTESIAN_POINT('Ctrl Pts',(-11.5842251848039,-88.2694212430601,
76.195453975661));
#128341=CARTESIAN_POINT('Ctrl Pts',(-11.5362920311509,-88.45285201793,75.311618240522));
#128342=CARTESIAN_POINT('Ctrl Pts',(-11.4994922869709,-88.5760310449,74.4195924580851));
#128343=CARTESIAN_POINT('Ctrl Pts',(-11.4791528728089,-88.63611386146,73.5865621709933));
#128344=CARTESIAN_POINT('Ctrl Pts',(-11.4757076647519,-88.6434404726801,
73.058635682904));
#128345=CARTESIAN_POINT('Ctrl Pts',(-11.4764772673159,-88.64043162139,72.8181652199194));
#128346=CARTESIAN_POINT('Ctrl Pts',(-11.7057132270397,-84.35369441765,82.257404991939));
#128347=CARTESIAN_POINT('Ctrl Pts',(-11.7070170071163,-84.35875839185,82.252282259352));
#128348=CARTESIAN_POINT('Ctrl Pts',(-11.7401872926896,-84.48814975745,82.121176924537));
#128349=CARTESIAN_POINT('Ctrl Pts',(-11.8000373105898,-84.75104883033,81.84348205208));
#128350=CARTESIAN_POINT('Ctrl Pts',(-11.868419602882,-85.13319173531,81.404040811101));
#128351=CARTESIAN_POINT('Ctrl Pts',(-11.9203258058273,-85.51527430505,80.921611413094));
#128352=CARTESIAN_POINT('Ctrl Pts',(-11.9557100952138,-85.88002512022,80.413225238712));
#128353=CARTESIAN_POINT('Ctrl Pts',(-11.9759645068405,-86.2185520436701,
79.890676037857));
#128354=CARTESIAN_POINT('Ctrl Pts',(-11.9823210247644,-86.52937136749,79.357690250987));
#128355=CARTESIAN_POINT('Ctrl Pts',(-11.9775241556327,-86.81667491343,78.807753404929));
#128356=CARTESIAN_POINT('Ctrl Pts',(-11.9628568411064,-87.08754421069,78.22340893719));
#128357=CARTESIAN_POINT('Ctrl Pts',(-11.9380050289816,-87.34641096537,77.582692485394));
#128358=CARTESIAN_POINT('Ctrl Pts',(-11.9011241006592,-87.59200141635,76.864268881454));
#128359=CARTESIAN_POINT('Ctrl Pts',(-11.8547601280426,-87.81171865749,76.067026470817));
#128360=CARTESIAN_POINT('Ctrl Pts',(-11.8069360206181,-87.98721342102,75.215676380909));
#128361=CARTESIAN_POINT('Ctrl Pts',(-11.7703385677752,-88.10453079837,74.359470559734));
#128362=CARTESIAN_POINT('Ctrl Pts',(-11.7501246487507,-88.16165500829,73.5606102595776));
#128363=CARTESIAN_POINT('Ctrl Pts',(-11.7467093562876,-88.1685742837001,
73.0551809007065));
#128364=CARTESIAN_POINT('Ctrl Pts',(-11.7474725756366,-88.1657139936001,
72.8251097834962));
#128365=CARTESIAN_POINT('Ctrl Pts',(-11.5521126194759,-83.99608653211,81.873520954723));
#128366=CARTESIAN_POINT('Ctrl Pts',(-11.5533990734129,-84.00089318895,81.868644860704));
#128367=CARTESIAN_POINT('Ctrl Pts',(-11.5861301575113,-84.1237148298,81.743848064745));
#128368=CARTESIAN_POINT('Ctrl Pts',(-11.6452711945686,-84.37353378032,81.47932114015));
#128369=CARTESIAN_POINT('Ctrl Pts',(-11.7129961195329,-84.73735772374,81.060144097334));
#128370=CARTESIAN_POINT('Ctrl Pts',(-11.7645067914674,-85.10175611464,80.599382649326));
#128371=CARTESIAN_POINT('Ctrl Pts',(-11.7996612206877,-85.4500180148699,
80.113486354029));
#128372=CARTESIAN_POINT('Ctrl Pts',(-11.8197958458907,-85.7734570232501,
79.613923491977));
#128373=CARTESIAN_POINT('Ctrl Pts',(-11.8261202450725,-86.0706436476901,
79.104216759278));
#128374=CARTESIAN_POINT('Ctrl Pts',(-11.8213467799047,-86.3456660471901,
78.577887554994));
#128375=CARTESIAN_POINT('Ctrl Pts',(-11.8067324927872,-86.6051758018201,
78.018353542789));
#128376=CARTESIAN_POINT('Ctrl Pts',(-11.7819578063333,-86.85337134828,77.404630081976));
#128377=CARTESIAN_POINT('Ctrl Pts',(-11.7451659211349,-87.0890794363699,
76.716130212862));
#128378=CARTESIAN_POINT('Ctrl Pts',(-11.6988346079466,-87.3003638420499,
75.951106916957));
#128379=CARTESIAN_POINT('Ctrl Pts',(-11.6509476506377,-87.4694803984999,
75.132958453367));
#128380=CARTESIAN_POINT('Ctrl Pts',(-11.61423360516,-87.5827431255899,74.308960051561));
#128381=CARTESIAN_POINT('Ctrl Pts',(-11.5939473557576,-87.6379323021899,
73.539868478611));
#128382=CARTESIAN_POINT('Ctrl Pts',(-11.5905148211427,-87.64463559833,73.0529433677899));
#128383=CARTESIAN_POINT('Ctrl Pts',(-11.5912817195219,-87.64187204039,72.8312357367396));
#128384=CARTESIAN_POINT('Ctrl Pts',(-11.3985120119129,-83.63847864657,81.489636917508));
#128385=CARTESIAN_POINT('Ctrl Pts',(-11.3997811397099,-83.64302798605,81.485007462056));
#128386=CARTESIAN_POINT('Ctrl Pts',(-11.4320730223329,-83.75927990215,81.366519204953));
#128387=CARTESIAN_POINT('Ctrl Pts',(-11.4905050785479,-83.9960187303,81.11516022822));
#128388=CARTESIAN_POINT('Ctrl Pts',(-11.5575726361839,-84.34152371217,80.716247383567));
#128389=CARTESIAN_POINT('Ctrl Pts',(-11.6086877771075,-84.6882379242201,
80.277153885558));
#128390=CARTESIAN_POINT('Ctrl Pts',(-11.6436123461616,-85.02001090952,79.813747469345));
#128391=CARTESIAN_POINT('Ctrl Pts',(-11.6636271849409,-85.32836200283,79.3371709460971));
#128392=CARTESIAN_POINT('Ctrl Pts',(-11.6699194653806,-85.6119159279,78.85074326757));
#128393=CARTESIAN_POINT('Ctrl Pts',(-11.6651694041767,-85.87465718095,78.3480217050591));
#128394=CARTESIAN_POINT('Ctrl Pts',(-11.650608144468,-86.12280739294,77.813298148387));
#128395=CARTESIAN_POINT('Ctrl Pts',(-11.6259105836849,-86.36033173119,77.226567678558));
#128396=CARTESIAN_POINT('Ctrl Pts',(-11.5892077416107,-86.58615745639,76.567991544269));
#128397=CARTESIAN_POINT('Ctrl Pts',(-11.5429090878509,-86.7890090266,75.835187363097));
#128398=CARTESIAN_POINT('Ctrl Pts',(-11.4949592806569,-86.95174737597,75.050240525825));
#128399=CARTESIAN_POINT('Ctrl Pts',(-11.4581286425449,-87.0609554528,74.258449543389));
#128400=CARTESIAN_POINT('Ctrl Pts',(-11.4377700627649,-87.11420959609,73.5191266976445));
#128401=CARTESIAN_POINT('Ctrl Pts',(-11.4343202859979,-87.12069691296,73.0507058348735));
#128402=CARTESIAN_POINT('Ctrl Pts',(-11.4350908634069,-87.11803008719,72.8373616899829));
#128403=CARTESIAN_POINT('Ctrl Pts',(-10.9198461320759,-83.52052975215,81.253394354178));
#128404=CARTESIAN_POINT('Ctrl Pts',(-10.9210612663879,-83.52475771529,81.2490347736811));
#128405=CARTESIAN_POINT('Ctrl Pts',(-10.9519844645779,-83.63281856841,81.13743865198));
#128406=CARTESIAN_POINT('Ctrl Pts',(-11.0082071223769,-83.8539992488999,
80.89989300697));
#128407=CARTESIAN_POINT('Ctrl Pts',(-11.0732261248979,-84.1796941866,80.520520942376));
#128408=CARTESIAN_POINT('Ctrl Pts',(-11.1231086717439,-84.50915551152,80.100541218406));
#128409=CARTESIAN_POINT('Ctrl Pts',(-11.1573169271029,-84.8260470355,79.655886975436));
#128410=CARTESIAN_POINT('Ctrl Pts',(-11.1769584752109,-85.12145769654,79.198059264838));
#128411=CARTESIAN_POINT('Ctrl Pts',(-11.1831506639509,-85.39402078712,78.730082377384));
#128412=CARTESIAN_POINT('Ctrl Pts',(-11.1784735365659,-85.64789670709,78.244734052057));
#128413=CARTESIAN_POINT('Ctrl Pts',(-11.1640775262769,-85.88857428129,77.727362293743));
#128414=CARTESIAN_POINT('Ctrl Pts',(-11.1396203123759,-86.11970476943,77.1588049595881));
#128415=CARTESIAN_POINT('Ctrl Pts',(-11.1031949555669,-86.34044091572,76.519219618205));
#128416=CARTESIAN_POINT('Ctrl Pts',(-11.0569980784489,-86.54038984716,75.803498053924));
#128417=CARTESIAN_POINT('Ctrl Pts',(-11.0088524120349,-86.70225414811,75.0319261570531));
#128418=CARTESIAN_POINT('Ctrl Pts',(-10.9716584360619,-86.81172328639,74.248802525509));
#128419=CARTESIAN_POINT('Ctrl Pts',(-10.9510744529809,-86.8652632226401,
73.5164284997833));
#128420=CARTESIAN_POINT('Ctrl Pts',(-10.9475709444619,-86.8718595485001,
73.0510699681692));
#128421=CARTESIAN_POINT('Ctrl Pts',(-10.9483529868409,-86.86917777529,72.8388787541773));
#128422=CARTESIAN_POINT('Ctrl Pts',(-10.4122773932589,-83.71521774574,81.310962378986));
#128423=CARTESIAN_POINT('Ctrl Pts',(-10.4134352738449,-83.71925911704,81.306728931525));
#128424=CARTESIAN_POINT('Ctrl Pts',(-10.4429071435399,-83.82257558211,81.198344207213));
#128425=CARTESIAN_POINT('Ctrl Pts',(-10.4967869947709,-84.03534630022,80.966710627961));
#128426=CARTESIAN_POINT('Ctrl Pts',(-10.5596337460819,-84.35199707519,80.594065561619));
#128427=CARTESIAN_POINT('Ctrl Pts',(-10.6082092722099,-84.6753115925,80.178819271204));
#128428=CARTESIAN_POINT('Ctrl Pts',(-10.6416579613369,-84.98813663679,79.737577062465));
#128429=CARTESIAN_POINT('Ctrl Pts',(-10.6609036786939,-85.2807609136999,
79.282660284474));
#128430=CARTESIAN_POINT('Ctrl Pts',(-10.6669897319839,-85.5517753356901,
78.81688996442));
#128431=CARTESIAN_POINT('Ctrl Pts',(-10.6623899423179,-85.80568693668,78.331931220347));
#128432=CARTESIAN_POINT('Ctrl Pts',(-10.6481691595579,-86.0474022836899,
77.813716616604));
#128433=CARTESIAN_POINT('Ctrl Pts',(-10.6239668051929,-86.2803723129499,
77.243268394502));
#128434=CARTESIAN_POINT('Ctrl Pts',(-10.5878356887969,-86.50396071259,76.59999083105));
#128435=CARTESIAN_POINT('Ctrl Pts',(-10.5417467338089,-86.70833313634,75.875645948436));
#128436=CARTESIAN_POINT('Ctrl Pts',(-10.4933933817809,-86.87536834288,75.089346899771));
#128437=CARTESIAN_POINT('Ctrl Pts',(-10.4558141288379,-86.9892527291599,
74.285987846374));
#128438=CARTESIAN_POINT('Ctrl Pts',(-10.4349911321279,-87.04512245748,73.5334433267483));
#128439=CARTESIAN_POINT('Ctrl Pts',(-10.4314306474199,-87.05208533402,73.0538104694048));
#128440=CARTESIAN_POINT('Ctrl Pts',(-10.4322248470459,-87.04928618213,72.834848284201));
#128441=CARTESIAN_POINT('Ctrl Pts',(-11.2182969702623,-84.8936789842178,
82.3980377633591));
#128442=CARTESIAN_POINT('Ctrl Pts',(-11.2433855557306,-84.8786414224159,
82.3897381760834));
#128443=CARTESIAN_POINT('Ctrl Pts',(-11.2679068003975,-84.8626035236921,
82.3803586826996));
#128444=CARTESIAN_POINT('Ctrl Pts',(-11.2916243250072,-84.8456399233827,
82.3699174155352));
#128445=CARTESIAN_POINT('Ctrl Pts',(-11.3151598443708,-84.8288064995694,
82.3595562733177));
#128446=CARTESIAN_POINT('Ctrl Pts',(-11.3379030705374,-84.8110617165967,
82.3481495705518));
#128447=CARTESIAN_POINT('Ctrl Pts',(-11.3596341093316,-84.7925135973983,
82.3357505614535));
#128448=CARTESIAN_POINT('Ctrl Pts',(-11.3812224972171,-84.7740872351986,
82.3234329442267));
#128449=CARTESIAN_POINT('Ctrl Pts',(-11.4018111484351,-84.7548684162775,
82.3101361680513));
#128450=CARTESIAN_POINT('Ctrl Pts',(-11.4212078536227,-84.7349936564423,
82.2959465950604));
#128451=CARTESIAN_POINT('Ctrl Pts',(-11.424977064801,-84.7311315486146,
82.2931892454686));
#128452=CARTESIAN_POINT('Ctrl Pts',(-11.4287013583715,-84.7272447543509,
82.290398281619));
#128453=CARTESIAN_POINT('Ctrl Pts',(-11.4323794650856,-84.7233343896316,
82.2875744770987));
#128454=CARTESIAN_POINT('Ctrl Pts',(-11.4512354021245,-84.7032877741644,
82.2730981488187));
#128455=CARTESIAN_POINT('Ctrl Pts',(-11.4688740430804,-84.6826203892961,
82.2577567169767));
#128456=CARTESIAN_POINT('Ctrl Pts',(-11.485147615708,-84.6614963607626,
82.2416701986431));
#128457=CARTESIAN_POINT('Ctrl Pts',(-11.5019402316215,-84.6396985843413,
82.2250706030935));
#128458=CARTESIAN_POINT('Ctrl Pts',(-11.5172785757103,-84.6174151865612,
82.2076780423576));
#128459=CARTESIAN_POINT('Ctrl Pts',(-11.53104990243,-84.5948418128098,82.1896502597164));
#128460=CARTESIAN_POINT('Ctrl Pts',(-11.544511691304,-84.5727758203458,
82.1720276871987));
#128461=CARTESIAN_POINT('Ctrl Pts',(-11.5564761293108,-84.5504334643273,
82.1537988106687));
#128462=CARTESIAN_POINT('Ctrl Pts',(-11.5668892660002,-84.5280015911096,
82.1351267153699));
#128463=CARTESIAN_POINT('Ctrl Pts',(-11.5773770291814,-84.5054089582615,
82.1163208051593));
#128464=CARTESIAN_POINT('Ctrl Pts',(-11.5862912234104,-84.4827261841208,
82.0970659351269));
#128465=CARTESIAN_POINT('Ctrl Pts',(-11.5936293209293,-84.4601379692456,
82.0775350777285));
#128466=CARTESIAN_POINT('Ctrl Pts',(-11.6010391730179,-84.4373288786418,
82.0578132405478));
#128467=CARTESIAN_POINT('Ctrl Pts',(-11.6068422524605,-84.4146167999226,
82.037810619652));
#128468=CARTESIAN_POINT('Ctrl Pts',(-11.6110867946357,-84.392176000142,
82.0177021343215));
#128469=CARTESIAN_POINT('Ctrl Pts',(-11.6154255116511,-84.369237300082,
81.9971474964223));
#128470=CARTESIAN_POINT('Ctrl Pts',(-11.6181362269336,-84.3465825828635,
81.9764828516226));
#128471=CARTESIAN_POINT('Ctrl Pts',(-11.6193176321618,-84.3243726751204,
81.9558821694911));
#128472=CARTESIAN_POINT('Ctrl Pts',(-11.6205146597371,-84.3018690740015,
81.9350090736266));
#128473=CARTESIAN_POINT('Ctrl Pts',(-11.6201423946605,-84.2798224502727,
81.9142021189062));
#128474=CARTESIAN_POINT('Ctrl Pts',(-11.6183421066293,-84.2583678331536,
81.8936208899891));
#128475=CARTESIAN_POINT('Ctrl Pts',(-11.616492258386,-84.2363225908918,
81.8724730794731));
#128476=CARTESIAN_POINT('Ctrl Pts',(-11.6131354923086,-84.214902618432,
81.8515639882498));
#128477=CARTESIAN_POINT('Ctrl Pts',(-11.6084537419359,-84.1942161957235,
81.8310374785355));
#128478=CARTESIAN_POINT('Ctrl Pts',(-11.6042944389499,-84.1758382189213,
81.8128015696655));
#128479=CARTESIAN_POINT('Ctrl Pts',(-11.5990901824507,-84.1580385852257,
81.7948672220324));
#128480=CARTESIAN_POINT('Ctrl Pts',(-11.5929787721051,-84.1408680578277,
81.7773140347692));
#128481=CARTESIAN_POINT('Ctrl Pts',(-11.5860445120705,-84.1213856642106,
81.7573974593739));
#128482=CARTESIAN_POINT('Ctrl Pts',(-11.5776480727554,-84.1018875939657,
81.7371276918464));
#128483=CARTESIAN_POINT('Ctrl Pts',(-11.5676769120622,-84.0825449312996,
81.7166394401541));
#128484=CARTESIAN_POINT('Ctrl Pts',(-11.5574726006912,-84.0627499887989,
81.6956721218904));
#128485=CARTESIAN_POINT('Ctrl Pts',(-11.5456179778182,-84.0431181587144,
81.6744760618832));
#128486=CARTESIAN_POINT('Ctrl Pts',(-11.5320349835769,-84.0238570172672,
81.6532282396095));
#128487=CARTESIAN_POINT('Ctrl Pts',(-11.5194075887975,-84.0059509479106,
81.6334752576613));
#128488=CARTESIAN_POINT('Ctrl Pts',(-11.5052863423841,-83.9883659472882,
81.6136781742483));
#128489=CARTESIAN_POINT('Ctrl Pts',(-11.4896522818661,-83.9712811933441,
81.5940009641816));
#128490=CARTESIAN_POINT('Ctrl Pts',(-11.4742397728455,-83.9544385487876,
81.5746026014014));
#128491=CARTESIAN_POINT('Ctrl Pts',(-11.4573567200337,-83.9380826848318,
81.5553212432214));
#128492=CARTESIAN_POINT('Ctrl Pts',(-11.4390326898169,-83.9223884465296,
81.5363280263991));
#128493=CARTESIAN_POINT('Ctrl Pts',(-11.4209217467494,-83.9068767139568,
81.5175556785877));
#128494=CARTESIAN_POINT('Ctrl Pts',(-11.4014030677723,-83.8920119462866,
81.4990653908471));
#128495=CARTESIAN_POINT('Ctrl Pts',(-11.3805550175105,-83.8779567998221,
81.4810281424953));
#128496=CARTESIAN_POINT('Ctrl Pts',(-11.3598956981088,-83.8640288901903,
81.4631541796955));
#128497=CARTESIAN_POINT('Ctrl Pts',(-11.3379311319091,-83.8508966205834,
81.4457257031722));
#128498=CARTESIAN_POINT('Ctrl Pts',(-11.3147861625713,-83.8387028673069,
81.4289058648591));
#128499=CARTESIAN_POINT('Ctrl Pts',(-11.291811934848,-83.8265990679678,
81.4122101073478));
#128500=CARTESIAN_POINT('Ctrl Pts',(-11.267675062256,-83.8154205147056,
81.3961146293196));
#128501=CARTESIAN_POINT('Ctrl Pts',(-11.2425414819819,-83.8052831936582,
81.3807668276438));
#128502=CARTESIAN_POINT('Ctrl Pts',(-11.2174805704165,-83.7951751826425,
81.3654634010599));
#128503=CARTESIAN_POINT('Ctrl Pts',(-11.1914293085413,-83.7861027995091,
81.3509038563171));
#128504=CARTESIAN_POINT('Ctrl Pts',(-11.1645884150797,-83.7781502842866,
81.3372138112605));
#128505=CARTESIAN_POINT('Ctrl Pts',(-11.137715324457,-83.770188229575,81.3235073442249));
#128506=CARTESIAN_POINT('Ctrl Pts',(-11.1100514689375,-83.7633489876007,
81.3106728816397));
#128507=CARTESIAN_POINT('Ctrl Pts',(-11.0818243842738,-83.7576811857671,
81.2988087855567));
#128508=CARTESIAN_POINT('Ctrl Pts',(-11.0601958237095,-83.7533383215754,
81.2897181081549));
#128509=CARTESIAN_POINT('Ctrl Pts',(-11.0382372286131,-83.7496824821535,
81.2811965966304));
#128510=CARTESIAN_POINT('Ctrl Pts',(-11.0160567890457,-83.7467203804265,
81.2732756023359));
#128511=CARTESIAN_POINT('Ctrl Pts',(-10.9868578190103,-83.7428209843256,
81.2628481771106));
#128512=CARTESIAN_POINT('Ctrl Pts',(-10.9572749163021,-83.7401251164008,
81.2534627663865));
#128513=CARTESIAN_POINT('Ctrl Pts',(-10.9275572528519,-83.7386131255171,
81.2451598069053));
#128514=CARTESIAN_POINT('Ctrl Pts',(-10.8976502687018,-83.7370915022755,
81.2368039522123));
#128515=CARTESIAN_POINT('Ctrl Pts',(-10.8676076690518,-83.7367686166817,
81.2295443295768));
#128516=CARTESIAN_POINT('Ctrl Pts',(-10.837673769809,-83.7375876583117,
81.2233853462825));
#128517=CARTESIAN_POINT('Ctrl Pts',(-10.8073511595244,-83.7384173357271,
81.2171463846068));
#128518=CARTESIAN_POINT('Ctrl Pts',(-10.777140872443,-83.7404183794199,
81.2120366270806));
#128519=CARTESIAN_POINT('Ctrl Pts',(-10.7472743538497,-83.7434992703846,
81.2080249338404));
#128520=CARTESIAN_POINT('Ctrl Pts',(-10.7423430476946,-83.7440079609616,
81.2073625570887));
#128521=CARTESIAN_POINT('Ctrl Pts',(-10.737421049655,-83.7445460278415,
81.2067300423042));
#128522=CARTESIAN_POINT('Ctrl Pts',(-10.7325093222788,-83.7451129887462,
81.2061271649026));
#128523=CARTESIAN_POINT('Ctrl Pts',(-10.1996868022679,-82.23194843945,84.7288031621899));
#128524=CARTESIAN_POINT('Ctrl Pts',(-10.2310549729399,-82.36225217191,84.64853404355));
#128525=CARTESIAN_POINT('Ctrl Pts',(-10.2941852691639,-82.62272957896,84.4820327658399));
#128526=CARTESIAN_POINT('Ctrl Pts',(-10.3878876652799,-83.00658824629,84.21807111946));
#128527=CARTESIAN_POINT('Ctrl Pts',(-10.4803333774059,-83.38465446058,83.93868646342));
#128528=CARTESIAN_POINT('Ctrl Pts',(-10.5704313181939,-83.75452094002,83.64531909529));
#128529=CARTESIAN_POINT('Ctrl Pts',(-10.6577223613839,-84.11597215343,83.33784927704));
#128530=CARTESIAN_POINT('Ctrl Pts',(-10.7418800834869,-84.46872560982,83.01615568715));
#128531=CARTESIAN_POINT('Ctrl Pts',(-10.8226451344339,-84.81241750864,82.680139979899));
#128532=CARTESIAN_POINT('Ctrl Pts',(-10.8743243729249,-85.0362970369799,
82.445396126594));
#128533=CARTESIAN_POINT('Ctrl Pts',(-10.8997098703319,-85.14736683005,82.3246922926509));
#128534=CARTESIAN_POINT('Ctrl Pts',(-10.9001033512449,-85.1490887083899,
82.32282002129));
#128535=CARTESIAN_POINT('Ctrl Pts',(-10.7444620454609,-82.0833175450401,
84.7154537425701));
#128536=CARTESIAN_POINT('Ctrl Pts',(-10.7758888964799,-82.21370092662,84.6366925769601));
#128537=CARTESIAN_POINT('Ctrl Pts',(-10.8392066322589,-82.47465378675,84.47305894541));
#128538=CARTESIAN_POINT('Ctrl Pts',(-10.9333668192599,-82.86002706205,84.21286727656));
#128539=CARTESIAN_POINT('Ctrl Pts',(-11.0264183851959,-83.24028739056,83.93672505408));
#128540=CARTESIAN_POINT('Ctrl Pts',(-11.1172518052149,-83.61295320576,83.64600480045));
#128541=CARTESIAN_POINT('Ctrl Pts',(-11.2053563091919,-83.97761128967,83.34065945251));
#128542=CARTESIAN_POINT('Ctrl Pts',(-11.2903648245519,-84.33382210991,83.0206402545));
#128543=CARTESIAN_POINT('Ctrl Pts',(-11.3719996179599,-84.68114887489,82.685863360081));
#128544=CARTESIAN_POINT('Ctrl Pts',(-11.4242587012799,-84.90751917291,82.4516886974891));
#128545=CARTESIAN_POINT('Ctrl Pts',(-11.4499326462989,-85.01984506826,82.3312125004971));
#128546=CARTESIAN_POINT('Ctrl Pts',(-11.4503305990829,-85.0215864245201,
82.3293437447811));
#128547=CARTESIAN_POINT('Ctrl Pts',(-11.0477735235679,-81.77845486342,84.34924299992));
#128548=CARTESIAN_POINT('Ctrl Pts',(-11.0792330457179,-81.9049022180901,
84.27378555556));
#128549=CARTESIAN_POINT('Ctrl Pts',(-11.1426551411729,-82.15816549389,84.1168578421401));
#128550=CARTESIAN_POINT('Ctrl Pts',(-11.2370702098559,-82.53266637268,83.8668591095801));
#128551=CARTESIAN_POINT('Ctrl Pts',(-11.3304590936439,-82.90261491216,83.601083179));
#128552=CARTESIAN_POINT('Ctrl Pts',(-11.4217020023379,-83.26556115233,83.32082030468));
#128553=CARTESIAN_POINT('Ctrl Pts',(-11.5102594123469,-83.62098684921,83.02606811274));
#128554=CARTESIAN_POINT('Ctrl Pts',(-11.5957416191302,-83.96837243791,82.716822523456));
#128555=CARTESIAN_POINT('Ctrl Pts',(-11.6778606542034,-84.30725103196,82.393010881238));
#128556=CARTESIAN_POINT('Ctrl Pts',(-11.7304425745,-84.52818768737,82.166329389436));
#128557=CARTESIAN_POINT('Ctrl Pts',(-11.7562771168898,-84.63782939136,82.049669415333));
#128558=CARTESIAN_POINT('Ctrl Pts',(-11.7566775594532,-84.63952913831,82.0478598454959));
#128559=CARTESIAN_POINT('Ctrl Pts',(-10.9126188732579,-81.5153702725701,
83.86802669304));
#128560=CARTESIAN_POINT('Ctrl Pts',(-10.9440638372539,-81.636422394,83.7955229542399));
#128561=CARTESIAN_POINT('Ctrl Pts',(-11.0074394303619,-81.87882547258,83.64478390263));
#128562=CARTESIAN_POINT('Ctrl Pts',(-11.1017409245619,-82.23712862778,83.40478070061));
#128563=CARTESIAN_POINT('Ctrl Pts',(-11.1949795005649,-82.59095703495,83.14976196043));
#128564=CARTESIAN_POINT('Ctrl Pts',(-11.2860399423799,-82.93797770321,82.880974608658));
#128565=CARTESIAN_POINT('Ctrl Pts',(-11.3743955388709,-83.27772823833,82.598403949157));
#128566=CARTESIAN_POINT('Ctrl Pts',(-11.4596666702309,-83.60973803331,82.302033671229));
#128567=CARTESIAN_POINT('Ctrl Pts',(-11.5415699287259,-83.9335725497799,
81.991791732945));
#128568=CARTESIAN_POINT('Ctrl Pts',(-11.594007993871,-84.14468032908,81.774660539086));
#128569=CARTESIAN_POINT('Ctrl Pts',(-11.6197709745725,-84.2494409441699,
81.662926717437));
#128570=CARTESIAN_POINT('Ctrl Pts',(-11.6201703076981,-84.25106502002,81.661193562179));
#128571=CARTESIAN_POINT('Ctrl Pts',(-10.7774642229489,-81.25228568173,83.38681038616));
#128572=CARTESIAN_POINT('Ctrl Pts',(-10.8088946287909,-81.36794256992,83.31726035291));
#128573=CARTESIAN_POINT('Ctrl Pts',(-10.8722237195519,-81.5994854512799,
83.17270996312));
#128574=CARTESIAN_POINT('Ctrl Pts',(-10.9664116392669,-81.94159088287,82.942702291641));
#128575=CARTESIAN_POINT('Ctrl Pts',(-11.0594999074859,-82.27929915774,82.698440741869));
#128576=CARTESIAN_POINT('Ctrl Pts',(-11.1503778824219,-82.61039425409,82.441128912633));
#128577=CARTESIAN_POINT('Ctrl Pts',(-11.2385316653959,-82.93446962745,82.170739785574));
#128578=CARTESIAN_POINT('Ctrl Pts',(-11.3235917213319,-83.25110362872,81.887244819002));
#128579=CARTESIAN_POINT('Ctrl Pts',(-11.4052792032479,-83.55989406761,81.590572584651));
#128580=CARTESIAN_POINT('Ctrl Pts',(-11.4575734132419,-83.76117297079,81.382991688735));
#128581=CARTESIAN_POINT('Ctrl Pts',(-11.4832648322549,-83.86105249698,81.27618401954));
#128582=CARTESIAN_POINT('Ctrl Pts',(-11.4836630559429,-83.86260090173,81.274527278862));
#128583=CARTESIAN_POINT('Ctrl Pts',(-10.2916270839719,-81.20185397504,83.10314097868));
#128584=CARTESIAN_POINT('Ctrl Pts',(-10.3230051579719,-81.31416065537,83.03427618836));
#128585=CARTESIAN_POINT('Ctrl Pts',(-10.3861670878749,-81.5387264805201,
82.891377636428));
#128586=CARTESIAN_POINT('Ctrl Pts',(-10.4799467441519,-81.86982936611,82.664675941307));
#128587=CARTESIAN_POINT('Ctrl Pts',(-10.5724947046279,-82.19607927414,82.424575630003));
#128588=CARTESIAN_POINT('Ctrl Pts',(-10.6627167703069,-82.51538654248,82.172304055685));
#128589=CARTESIAN_POINT('Ctrl Pts',(-10.7501450991309,-82.82752507745,81.907772869607));
#128590=CARTESIAN_POINT('Ctrl Pts',(-10.8344464073679,-83.13221937986,81.630892336144));
#128591=CARTESIAN_POINT('Ctrl Pts',(-10.9153582424579,-83.42914104018,81.341580665038));
#128592=CARTESIAN_POINT('Ctrl Pts',(-10.9671353398329,-83.62257973927,81.139404226637));
#128593=CARTESIAN_POINT('Ctrl Pts',(-10.9925695177819,-83.7185515713301,
81.035433078134));
#128594=CARTESIAN_POINT('Ctrl Pts',(-10.9929637534009,-83.72003939198,81.033820349075));
#128595=CARTESIAN_POINT('Ctrl Pts',(-9.77066117414391,-81.3968308051,83.20126320814));
#128596=CARTESIAN_POINT('Ctrl Pts',(-9.80198313241291,-81.51000828017,83.13037012931));
#128597=CARTESIAN_POINT('Ctrl Pts',(-9.86496581478391,-81.73601182397,82.983513714113));
#128598=CARTESIAN_POINT('Ctrl Pts',(-9.95830768786792,-82.0684535513199,
82.751281192542));
#128599=CARTESIAN_POINT('Ctrl Pts',(-10.0502762732979,-82.39534912611,82.506043422008));
#128600=CARTESIAN_POINT('Ctrl Pts',(-10.1397950037739,-82.71466256519,82.249103163521));
#128601=CARTESIAN_POINT('Ctrl Pts',(-10.2264454240119,-83.02635562299,81.980301564201));
#128602=CARTESIAN_POINT('Ctrl Pts',(-10.3099331228039,-83.33030121714,81.699478477315));
#128603=CARTESIAN_POINT('Ctrl Pts',(-10.3900132274179,-83.62623823057,81.40653750512));
#128604=CARTESIAN_POINT('Ctrl Pts',(-10.4412358220089,-83.8189176504501,
81.202109460885));
#128605=CARTESIAN_POINT('Ctrl Pts',(-10.4663941589129,-83.91449325055,81.09704286655));
#128606=CARTESIAN_POINT('Ctrl Pts',(-10.4667841181019,-83.9159749237701,
81.095413160376));
#128607=CARTESIAN_POINT('Origin',(-8.56753648333091,1.4210854715202E-14,
72.98888938658));
#128608=CARTESIAN_POINT('',(-8.56795784296129,-66.4424972638774,69.9758907965238));
#128609=CARTESIAN_POINT('Ctrl Pts',(-8.56753648333091,-72.6784966214787,
81.061721731149));
#128610=CARTESIAN_POINT('Ctrl Pts',(-8.56753648333091,-72.0736574609292,
80.9189296982678));
#128611=CARTESIAN_POINT('Ctrl Pts',(-8.56753648333125,-71.4844480422102,
80.7093614983211));
#128612=CARTESIAN_POINT('Ctrl Pts',(-8.56753648333125,-70.3508022556626,
80.1607120918089));
#128613=CARTESIAN_POINT('Ctrl Pts',(-8.56753648333122,-69.8135934358944,
79.8216225166484));
#128614=CARTESIAN_POINT('Ctrl Pts',(-8.56753648333122,-68.4473368829776,
78.7233837561792));
#128615=CARTESIAN_POINT('Ctrl Pts',(-8.56753648333092,-67.7165424986972,
77.8572780272833));
#128616=CARTESIAN_POINT('Ctrl Pts',(-8.56753648333092,-66.4689218847558,
75.6285559895337));
#128617=CARTESIAN_POINT('Ctrl Pts',(-8.56753648333069,-66.2230924334251,
74.4581989464032));
#128618=CARTESIAN_POINT('Ctrl Pts',(-8.56753648333069,-66.0482530107463,
73.0618974695663));
#128619=CARTESIAN_POINT('Ctrl Pts',(-8.56753648333066,-66.0347923157517,
72.4374342122791));
#128620=CARTESIAN_POINT('Ctrl Pts',(-8.56753648333066,-66.1408479418231,
71.1931468548539));
#128621=CARTESIAN_POINT('Ctrl Pts',(-8.56753648333091,-66.2606244843831,
70.5750930481944));
#128622=CARTESIAN_POINT('Ctrl Pts',(-8.56753648333091,-66.4418053341428,
69.9756606261135));
#128623=CARTESIAN_POINT('',(-8.56568834200734,-73.334592210701,64.0777114412437));
#128624=CARTESIAN_POINT('Ctrl Pts',(-8.56753648333091,-66.4431946200656,
69.976105782015));
#128625=CARTESIAN_POINT('Ctrl Pts',(-8.56753648333091,-66.7099427616035,
69.2296629521477));
#128626=CARTESIAN_POINT('Ctrl Pts',(-8.56753648333093,-67.0759536435953,
68.5186782220475));
#128627=CARTESIAN_POINT('Ctrl Pts',(-8.56753648333093,-67.9733465906314,
67.2115334810726));
#128628=CARTESIAN_POINT('Ctrl Pts',(-8.56753648333091,-68.5055791540009,
66.6142037248065));
#128629=CARTESIAN_POINT('Ctrl Pts',(-8.56753648333091,-69.8717500230355,
65.4338849316529));
#128630=CARTESIAN_POINT('Ctrl Pts',(-8.56753648333092,-70.5858970496848,
65.0401447415795));
#128631=CARTESIAN_POINT('Ctrl Pts',(-8.56753648333092,-71.797320001775,
64.4667419598192));
#128632=CARTESIAN_POINT('Ctrl Pts',(-8.56753648333091,-72.5576048061066,
64.2249906466459));
#128633=CARTESIAN_POINT('Ctrl Pts',(-8.56753648333091,-73.3353239041699,
64.0818175558208));
#128634=CARTESIAN_POINT('Ctrl Pts',(-8.56753648333091,-73.3334510577524,
64.0699842298794));
#128635=CARTESIAN_POINT('Ctrl Pts',(-8.56753648333091,-73.9396539367879,
63.9867207515655));
#128636=CARTESIAN_POINT('Ctrl Pts',(-8.56753648333073,-74.5544091401536,
63.965415257747));
#128637=CARTESIAN_POINT('Ctrl Pts',(-8.56753648333073,-75.7715247557608,
64.0447290124391));
#128638=CARTESIAN_POINT('Ctrl Pts',(-8.56753648333076,-76.3744099119309,
64.144574635375));
#128639=CARTESIAN_POINT('Ctrl Pts',(-8.56753648333076,-78.0901283056316,
64.611417005806));
#128640=CARTESIAN_POINT('Ctrl Pts',(-8.5675364833309,-79.1248322783208,
65.1310007962587));
#128641=CARTESIAN_POINT('Ctrl Pts',(-8.5675364833309,-80.9371209889916,
66.5524367891479));
#128642=CARTESIAN_POINT('Ctrl Pts',(-8.567536483331,-81.6981213556041,67.42795058762));
#128643=CARTESIAN_POINT('Ctrl Pts',(-8.567536483331,-82.5704038623667,68.9625486543065));
#128644=CARTESIAN_POINT('Ctrl Pts',(-8.56753648333101,-82.814707297137,
69.5342669600823));
#128645=CARTESIAN_POINT('Ctrl Pts',(-8.56753648333101,-83.1721280645855,
70.7266324610845));
#128646=CARTESIAN_POINT('Ctrl Pts',(-8.56753648333091,-83.2844104837004,
71.3379527534998));
#128647=CARTESIAN_POINT('Ctrl Pts',(-8.56753648333091,-83.3301907683851,
71.9538361593952));
#128648=CARTESIAN_POINT('Ctrl Pts',(-9.33949250599091,-68.28843467669,68.385749441946));
#128649=CARTESIAN_POINT('Ctrl Pts',(-9.28372478921891,-67.21314456544,69.953566173561));
#128650=CARTESIAN_POINT('Ctrl Pts',(-9.17218935567391,-66.21224057553,73.8663634510705));
#128651=CARTESIAN_POINT('Ctrl Pts',(-9.00488620535791,-68.84902572167,79.327681027565));
#128652=CARTESIAN_POINT('Ctrl Pts',(-8.83758305504191,-74.3860768082,81.799718607153));
#128653=CARTESIAN_POINT('Ctrl Pts',(-8.67027990472591,-80.21224973459,80.119224478064));
#128654=CARTESIAN_POINT('Ctrl Pts',(-8.50297675440891,-83.58160767004,75.077818068246));
#128655=CARTESIAN_POINT('Ctrl Pts',(-8.33567360409291,-82.90653225676,69.051693466476));
#128656=CARTESIAN_POINT('Ctrl Pts',(-8.16837045377691,-78.50298784705,64.8818706633));
#128657=CARTESIAN_POINT('Ctrl Pts',(-8.05683502023291,-74.47097197897,64.648120002453));
#128658=CARTESIAN_POINT('Ctrl Pts',(-8.00106730345991,-72.65076867909,65.196898714115));
#128659=CARTESIAN_POINT('Ctrl Pts',(-9.57007551786691,-67.95907438126,68.159857051868));
#128660=CARTESIAN_POINT('Ctrl Pts',(-9.51430780109491,-66.83101597355,69.804612106664));
#128661=CARTESIAN_POINT('Ctrl Pts',(-9.40277236755091,-65.78099407777,73.9094242130813));
#128662=CARTESIAN_POINT('Ctrl Pts',(-9.23546921723391,-68.54717561549,79.638747997329));
#128663=CARTESIAN_POINT('Ctrl Pts',(-9.06816606691691,-74.3559494215,82.232097221564));
#128664=CARTESIAN_POINT('Ctrl Pts',(-8.90086291659891,-80.46803330067,80.469135290092));
#128665=CARTESIAN_POINT('Ctrl Pts',(-8.73355976628091,-84.00273757062,75.180329201596));
#128666=CARTESIAN_POINT('Ctrl Pts',(-8.56625661596291,-83.29453381444,68.858481309736));
#128667=CARTESIAN_POINT('Ctrl Pts',(-8.39895346564491,-78.67489187492,64.484030524229));
#128668=CARTESIAN_POINT('Ctrl Pts',(-8.28741803209991,-74.4450106992,64.238808890051));
#128669=CARTESIAN_POINT('Ctrl Pts',(-8.23165031532691,-72.5354835728,64.814518117892));
#128670=CARTESIAN_POINT('Ctrl Pts',(-9.80065852974291,-67.62971408584,67.93396466179));
#128671=CARTESIAN_POINT('Ctrl Pts',(-9.74489081297091,-66.44888738166,69.655658039767));
#128672=CARTESIAN_POINT('Ctrl Pts',(-9.63335537942691,-65.34974758001,73.9524849750929));
#128673=CARTESIAN_POINT('Ctrl Pts',(-9.46605222911091,-68.24532550932,79.949814967102));
#128674=CARTESIAN_POINT('Ctrl Pts',(-9.29874907879591,-74.32582203482,82.66447583598));
#128675=CARTESIAN_POINT('Ctrl Pts',(-9.13144592848091,-80.72381686678,80.8190461021));
#128676=CARTESIAN_POINT('Ctrl Pts',(-8.96414277816591,-84.42386747123,75.282840334888));
#128677=CARTESIAN_POINT('Ctrl Pts',(-8.79683962785091,-83.68253537209,68.665269152917));
#128678=CARTESIAN_POINT('Ctrl Pts',(-8.62953647753691,-78.84679590269,64.086190385108));
#128679=CARTESIAN_POINT('Ctrl Pts',(-8.51800104399391,-74.41904941931,63.829497777655));
#128680=CARTESIAN_POINT('Ctrl Pts',(-8.46223332722191,-72.4201984664,64.432137521706));
#128681=CARTESIAN_POINT('Ctrl Pts',(-10.0312415416199,-67.30035379041,67.708072271712));
#128682=CARTESIAN_POINT('Ctrl Pts',(-9.97547382484791,-66.06675878978,69.50670397287));
#128683=CARTESIAN_POINT('Ctrl Pts',(-9.86393839130291,-64.91850108225,73.995545737104));
#128684=CARTESIAN_POINT('Ctrl Pts',(-9.69663524098691,-67.94347540314,80.260881936865));
#128685=CARTESIAN_POINT('Ctrl Pts',(-9.52933209067091,-74.29569464812,83.09685445039));
#128686=CARTESIAN_POINT('Ctrl Pts',(-9.36202894035391,-80.97960043285,81.168956914129));
#128687=CARTESIAN_POINT('Ctrl Pts',(-9.19472579003791,-84.84499737182,75.38535146824));
#128688=CARTESIAN_POINT('Ctrl Pts',(-9.02742263972191,-84.07053692978,68.47205699618));
#128689=CARTESIAN_POINT('Ctrl Pts',(-8.86011948940491,-79.01869993056,63.68835024604));
#128690=CARTESIAN_POINT('Ctrl Pts',(-8.74858405586091,-74.39308813955,63.420186665253));
#128691=CARTESIAN_POINT('Ctrl Pts',(-8.69281633908891,-72.30491336013,64.049756925482));
#128692=CARTESIAN_POINT('',(-9.85448345426765,-67.0071858774639,68.6911520794415));
#128693=CARTESIAN_POINT('Ctrl Pts',(-9.85448345426765,-67.0071858774639,
68.6911520794415));
#128694=CARTESIAN_POINT('Ctrl Pts',(-9.79971249899291,-66.0535515884723,
70.4917741499841));
#128695=CARTESIAN_POINT('Ctrl Pts',(-9.74592499989422,-65.7106640987246,
72.62028225223));
#128696=CARTESIAN_POINT('Ctrl Pts',(-9.63834989066502,-66.4347938378737,
76.617555712199));
#128697=CARTESIAN_POINT('Ctrl Pts',(-9.58456228053448,-67.5188766918498,
78.4829403854034));
#128698=CARTESIAN_POINT('Ctrl Pts',(-9.51732776787134,-69.4294746814203,
80.1653430250265));
#128699=CARTESIAN_POINT('Ctrl Pts',(-9.5038808653387,-69.8393117287546,
80.4693684884601));
#128700=CARTESIAN_POINT('Ctrl Pts',(-9.47698706027345,-70.705657587077,
81.0004575955979));
#128701=CARTESIAN_POINT('Ctrl Pts',(-9.46354015774083,-71.1625234758073,
81.2268973342743));
#128702=CARTESIAN_POINT('Ctrl Pts',(-9.3963056450777,-73.5294734721993,
82.1577931504897));
#128703=CARTESIAN_POINT('Ctrl Pts',(-9.34251803494718,-75.6862304181982,
82.2604177652121));
#128704=CARTESIAN_POINT('Ctrl Pts',(-9.26183661975145,-78.6050687686331,
81.3802459755177));
#128705=CARTESIAN_POINT('Ctrl Pts',(-9.2349428146862,-79.5243766321848,
80.911716381337));
#128706=CARTESIAN_POINT('Ctrl Pts',(-9.16770830202308,-81.577804542804,
79.4008185283445));
#128707=CARTESIAN_POINT('Ctrl Pts',(-9.12736759442522,-82.5896606086484,
78.1891376421487));
#128708=CARTESIAN_POINT('Ctrl Pts',(-9.07357998429472,-83.4468232021015,
76.3465169977388));
#128709=CARTESIAN_POINT('Ctrl Pts',(-9.0601330817621,-83.6196372087911,
75.8667299911412));
#128710=CARTESIAN_POINT('Ctrl Pts',(-8.99289856909898,-84.2755040487159,
73.4089183747913));
#128711=CARTESIAN_POINT('Ctrl Pts',(-8.93911095896847,-84.1348835562278,
71.2546776032613));
#128712=CARTESIAN_POINT('Ctrl Pts',(-8.83153573870747,-82.5254092780411,
67.5221796143094));
#128713=CARTESIAN_POINT('Ctrl Pts',(-8.77774812857696,-81.0499897572754,
65.9468497653013));
#128714=CARTESIAN_POINT('Ctrl Pts',(-8.71051361591392,-78.8096606761766,
64.7397816608276));
#128715=CARTESIAN_POINT('Ctrl Pts',(-8.69706671338133,-78.3418002183133,
64.5364691422482));
#128716=CARTESIAN_POINT('Ctrl Pts',(-8.67017290831613,-77.3775596950603,
64.2160019939825));
#128717=CARTESIAN_POINT('Ctrl Pts',(-8.65672600578354,-76.8811017434786,
64.0990887496991));
#128718=CARTESIAN_POINT('Ctrl Pts',(-8.61640526799513,-75.3716441191094,
63.8760691192961));
#128719=CARTESIAN_POINT('Ctrl Pts',(-8.58953143273933,-74.3378692213475,
63.8972735937159));
#128720=CARTESIAN_POINT('Ctrl Pts',(-8.56568834200734,-73.334592210701,
64.0777114412437));
#128721=CARTESIAN_POINT('',(-9.46541110279056,-67.6020149116865,69.0109979579471));
#128722=CARTESIAN_POINT('Ctrl Pts',(-9.99199816632791,-67.59428425961,67.303209521688));
#128723=CARTESIAN_POINT('Ctrl Pts',(-9.95025389358791,-66.60009764549,68.598158170228));
#128724=CARTESIAN_POINT('Ctrl Pts',(-9.86676534810891,-65.30823381695,71.71969580549));
#128725=CARTESIAN_POINT('Ctrl Pts',(-9.74153252989091,-65.975649193,76.744817636531));
#128726=CARTESIAN_POINT('Ctrl Pts',(-9.61629971167191,-69.0702482942,80.759474381881));
#128727=CARTESIAN_POINT('Ctrl Pts',(-9.49106689345391,-73.75942478415,82.684532165368));
#128728=CARTESIAN_POINT('Ctrl Pts',(-9.36583407523591,-78.78224537899,82.00215805984));
#128729=CARTESIAN_POINT('Ctrl Pts',(-9.24060125701691,-82.78791878897,78.895896207008));
#128730=CARTESIAN_POINT('Ctrl Pts',(-9.11536843879891,-84.6992258503,74.201089045578));
#128731=CARTESIAN_POINT('Ctrl Pts',(-8.99013562057991,-84.00216577159,69.180291345096));
#128732=CARTESIAN_POINT('Ctrl Pts',(-8.86490280236191,-80.88419637879,65.183721669986));
#128733=CARTESIAN_POINT('Ctrl Pts',(-8.73966998414291,-76.18381732287,63.28615857581));
#128734=CARTESIAN_POINT('Ctrl Pts',(-8.61443716592491,-71.16508250412,63.997905008714));
#128735=CARTESIAN_POINT('Ctrl Pts',(-8.48920434770591,-67.17764413613,67.127552977624));
#128736=CARTESIAN_POINT('Ctrl Pts',(-8.36397152948791,-65.29387078721,71.833466448308));
#128737=CARTESIAN_POINT('Ctrl Pts',(-8.23873871126891,-66.02018597587,76.850086687758));
#128738=CARTESIAN_POINT('Ctrl Pts',(-8.11350589305091,-69.16190222137,80.828391821067));
#128739=CARTESIAN_POINT('Ctrl Pts',(-8.03001734757191,-72.30180432462,82.07495675794));
#128740=CARTESIAN_POINT('Ctrl Pts',(-7.98827307483191,-73.92349052215,82.263193053033));
#128741=CARTESIAN_POINT('Ctrl Pts',(-10.2225811782039,-67.91107137654,67.546420332812));
#128742=CARTESIAN_POINT('Ctrl Pts',(-10.1808369054639,-66.95941211861,68.78597621942));
#128743=CARTESIAN_POINT('Ctrl Pts',(-10.0973483599859,-65.72280909565,71.77398686789));
#128744=CARTESIAN_POINT('Ctrl Pts',(-9.97211554176791,-66.36167509171,76.584153937925));
#128745=CARTESIAN_POINT('Ctrl Pts',(-9.84688272354991,-69.32389952966,80.42707960685));
#128746=CARTESIAN_POINT('Ctrl Pts',(-9.72164990533191,-73.81249166652,82.269791061293));
#128747=CARTESIAN_POINT('Ctrl Pts',(-9.59641708711391,-78.6204559381,81.616606210807));
#128748=CARTESIAN_POINT('Ctrl Pts',(-9.47118426889691,-82.45478254308,78.643217907434));
#128749=CARTESIAN_POINT('Ctrl Pts',(-9.34595145067991,-84.28433147665,74.149235956863));
#128750=CARTESIAN_POINT('Ctrl Pts',(-9.22071863246191,-83.61708886061,69.343208048246));
#128751=CARTESIAN_POINT('Ctrl Pts',(-9.09548581424491,-80.63249381933,65.517595756513));
#128752=CARTESIAN_POINT('Ctrl Pts',(-8.97025299602791,-76.13317831779,63.701202877746));
#128753=CARTESIAN_POINT('Ctrl Pts',(-8.84502017781091,-71.32912504901,64.382503624079));
#128754=CARTESIAN_POINT('Ctrl Pts',(-8.71978735959391,-67.51225346334,67.37827767835));
#128755=CARTESIAN_POINT('Ctrl Pts',(-8.59455454137691,-65.70906045929,71.88289085437));
#128756=CARTESIAN_POINT('Ctrl Pts',(-8.46932172315991,-66.40430676786,76.684919997149));
#128757=CARTESIAN_POINT('Ctrl Pts',(-8.34408890494191,-69.41163286577,80.493049031651));
#128758=CARTESIAN_POINT('Ctrl Pts',(-8.26060035946391,-72.41722242321,81.686290869658));
#128759=CARTESIAN_POINT('Ctrl Pts',(-8.21885608672491,-73.96953932369,81.866475163376));
#128760=CARTESIAN_POINT('Ctrl Pts',(-10.4531641900799,-68.22785849346,67.789631143935));
#128761=CARTESIAN_POINT('Ctrl Pts',(-10.4114199173409,-67.31872659173,68.973794268612));
#128762=CARTESIAN_POINT('Ctrl Pts',(-10.3279313718619,-66.13738437435,71.82827793029));
#128763=CARTESIAN_POINT('Ctrl Pts',(-10.2026985536429,-66.74770099042,76.423490239315));
#128764=CARTESIAN_POINT('Ctrl Pts',(-10.0774657354239,-69.57755076511,80.09468483181));
#128765=CARTESIAN_POINT('Ctrl Pts',(-9.95223291720491,-73.86555854886,81.855049957214));
#128766=CARTESIAN_POINT('Ctrl Pts',(-9.82700009898591,-78.45866649718,81.231054361786));
#128767=CARTESIAN_POINT('Ctrl Pts',(-9.70176728076691,-82.12164629715,78.390539607897));
#128768=CARTESIAN_POINT('Ctrl Pts',(-9.57653446254691,-83.86943710299,74.097382868212));
#128769=CARTESIAN_POINT('Ctrl Pts',(-9.45130164432791,-83.23201194965,69.506124751474));
#128770=CARTESIAN_POINT('Ctrl Pts',(-9.32606882610791,-80.38079125995,65.851469843104));
#128771=CARTESIAN_POINT('Ctrl Pts',(-9.20083600788791,-76.08253931283,64.116247179702));
#128772=CARTESIAN_POINT('Ctrl Pts',(-9.07560318966791,-71.49316759404,64.76710223939));
#128773=CARTESIAN_POINT('Ctrl Pts',(-8.95037037144891,-67.84686279065,67.629002378947));
#128774=CARTESIAN_POINT('Ctrl Pts',(-8.82513755322891,-66.1242501314,71.932315260248));
#128775=CARTESIAN_POINT('Ctrl Pts',(-8.69990473500891,-66.78842755977,76.519753306352));
#128776=CARTESIAN_POINT('Ctrl Pts',(-8.57467191678891,-69.66136350999,80.1577062421));
#128777=CARTESIAN_POINT('Ctrl Pts',(-8.49118337130991,-72.53264052159,81.29762498131));
#128778=CARTESIAN_POINT('Ctrl Pts',(-8.44943909856991,-74.01558812501,81.469757273692));
#128779=CARTESIAN_POINT('Ctrl Pts',(-10.6837472019569,-68.54464561039,68.032841955058));
#128780=CARTESIAN_POINT('Ctrl Pts',(-10.6420029292169,-67.67804106486,69.161612317803));
#128781=CARTESIAN_POINT('Ctrl Pts',(-10.5585143837379,-66.55195965305,71.882568992689));
#128782=CARTESIAN_POINT('Ctrl Pts',(-10.4332815655199,-67.13372688913,76.262826540709));
#128783=CARTESIAN_POINT('Ctrl Pts',(-10.3080487473019,-69.83120200056,79.762290056778));
#128784=CARTESIAN_POINT('Ctrl Pts',(-10.1828159290829,-73.91862543122,81.440308853139));
#128785=CARTESIAN_POINT('Ctrl Pts',(-10.0575831108649,-78.29687705629,80.845502512754));
#128786=CARTESIAN_POINT('Ctrl Pts',(-9.93235029264591,-81.78851005125,78.137861308325));
#128787=CARTESIAN_POINT('Ctrl Pts',(-9.80711747442791,-83.45454272935,74.0455297795));
#128788=CARTESIAN_POINT('Ctrl Pts',(-9.68188465620991,-82.84693503866,69.669041454627));
#128789=CARTESIAN_POINT('Ctrl Pts',(-9.55665183799091,-80.1290887005,66.185343929634));
#128790=CARTESIAN_POINT('Ctrl Pts',(-9.43141901977291,-76.03190030776,64.531291481639));
#128791=CARTESIAN_POINT('Ctrl Pts',(-9.30618620155491,-71.65721013894,65.151700854752));
#128792=CARTESIAN_POINT('Ctrl Pts',(-9.18095338333591,-68.18147211787,67.879727079667));
#128793=CARTESIAN_POINT('Ctrl Pts',(-9.05572056511791,-66.53943980348,71.981739666301));
#128794=CARTESIAN_POINT('Ctrl Pts',(-8.93048774689891,-67.17254835176,76.354586615735));
#128795=CARTESIAN_POINT('Ctrl Pts',(-8.80525492868091,-69.91109415439,79.822363452678));
#128796=CARTESIAN_POINT('Ctrl Pts',(-8.72176638320191,-72.64805862017,80.908959093025));
#128797=CARTESIAN_POINT('Ctrl Pts',(-8.68002211046191,-74.06163692655,81.073039384033));
#128798=CARTESIAN_POINT('',(-10.0985254848049,-67.01215254309,68.6936268804507));
#128799=CARTESIAN_POINT('',(-10.0976119119436,-67.0107639369115,68.6928899475042));
#128800=CARTESIAN_POINT('Ctrl Pts',(-10.1056201537506,-67.0100609947306,
68.6927734040079));
#128801=CARTESIAN_POINT('Ctrl Pts',(-10.0858288974105,-66.6260431282916,
69.4150543477338));
#128802=CARTESIAN_POINT('Ctrl Pts',(-10.0673827948632,-66.3411294788075,
70.1900495876074));
#128803=CARTESIAN_POINT('Ctrl Pts',(-10.0353495239254,-66.0633179308166,
71.4200744687751));
#128804=CARTESIAN_POINT('Ctrl Pts',(-10.0232792679854,-65.9963533493792,
71.8592112503599));
#128805=CARTESIAN_POINT('Ctrl Pts',(-10.0020449919732,-65.9382221349775,
72.5860608468921));
#128806=CARTESIAN_POINT('Ctrl Pts',(-9.99345424936893,-65.9286151577416,
72.8724489958298));
#128807=CARTESIAN_POINT('Ctrl Pts',(-9.96978124698292,-65.9394232775651,
73.6637855017629));
#128808=CARTESIAN_POINT('Ctrl Pts',(-9.95478264023665,-65.9884311928924,
74.1682378197038));
#128809=CARTESIAN_POINT('Ctrl Pts',(-9.93276979943483,-66.1405570108522,
74.9827935804844));
#128810=CARTESIAN_POINT('Ctrl Pts',(-9.9250031085192,-66.2175611627718,
75.2952032094914));
#128811=CARTESIAN_POINT('Ctrl Pts',(-9.90660496999056,-66.4505874392876,
76.0577540452807));
#128812=CARTESIAN_POINT('Ctrl Pts',(-9.89614883297556,-66.626578834097,
76.5013880191161));
#128813=CARTESIAN_POINT('Ctrl Pts',(-9.87648446127022,-66.9900401148003,
77.2443161242015));
#128814=CARTESIAN_POINT('Ctrl Pts',(-9.86781300305152,-67.1624496274915,
77.5510235654546));
#128815=CARTESIAN_POINT('Ctrl Pts',(-9.83445661031167,-67.864285454012,
78.6503572119695));
#128816=CARTESIAN_POINT('Ctrl Pts',(-9.80762292083788,-68.500619259633,
79.3771609760621));
#128817=CARTESIAN_POINT('Ctrl Pts',(-9.76803229526134,-69.538252857365,
80.2425287011678));
#128818=CARTESIAN_POINT('Ctrl Pts',(-9.75603894613835,-69.8608619067118,
80.4773256996633));
#128819=CARTESIAN_POINT('Ctrl Pts',(-9.7354525920193,-70.4740212840394,
80.8618096607943));
#128820=CARTESIAN_POINT('Ctrl Pts',(-9.72688917025221,-70.757447065395,
81.0176909946875));
#128821=CARTESIAN_POINT('Ctrl Pts',(-9.70180950486301,-71.6712457260181,
81.4557429774271));
#128822=CARTESIAN_POINT('Ctrl Pts',(-9.68700819128544,-72.3277386010445,
81.6799951258321));
#128823=CARTESIAN_POINT('Ctrl Pts',(-9.66320386310093,-73.3220371140291,
81.9007688530295));
#128824=CARTESIAN_POINT('Ctrl Pts',(-9.65519700831005,-73.6473197544878,
81.9550842937002));
#128825=CARTESIAN_POINT('Ctrl Pts',(-9.62768684262128,-74.6887798708784,
82.0731851906225));
#128826=CARTESIAN_POINT('Ctrl Pts',(-9.60600749490843,-75.4131320814911,
82.0722511733354));
#128827=CARTESIAN_POINT('Ctrl Pts',(-9.5728056010411,-76.5283475754138,
81.938809530694));
#128828=CARTESIAN_POINT('Ctrl Pts',(-9.56099613423051,-76.9266813718286,
81.8640002443785));
#128829=CARTESIAN_POINT('Ctrl Pts',(-9.53752942078241,-77.7541854435951,
81.6481365797571));
#128830=CARTESIAN_POINT('Ctrl Pts',(-9.52652650667813,-78.1764052469984,
81.5016462968993));
#128831=CARTESIAN_POINT('Ctrl Pts',(-9.49549132094949,-79.3626611652649,
80.9849160430836));
#128832=CARTESIAN_POINT('Ctrl Pts',(-9.47577017339058,-80.0888067054271,
80.5359409488921));
#128833=CARTESIAN_POINT('Ctrl Pts',(-9.43839760642428,-81.2371199228423,
79.5921011886046));
#128834=CARTESIAN_POINT('Ctrl Pts',(-9.42135872104697,-81.6912316979897,
79.1337121374095));
#128835=CARTESIAN_POINT('Ctrl Pts',(-9.39220782815627,-82.3240882281726,
78.3463877463461));
#128836=CARTESIAN_POINT('Ctrl Pts',(-9.38097818917659,-82.5379930731196,
78.0449993103856));
#128837=CARTESIAN_POINT('Ctrl Pts',(-9.35775260825943,-82.945334146773,
77.3886404803726));
#128838=CARTESIAN_POINT('Ctrl Pts',(-9.34582770326582,-83.1348815306979,
77.0313987126338));
#128839=CARTESIAN_POINT('Ctrl Pts',(-9.32494003038193,-83.4535024982193,
76.3117296668395));
#128840=CARTESIAN_POINT('Ctrl Pts',(-9.31587772144192,-83.5849139954119,
75.9509159743823));
#128841=CARTESIAN_POINT('Ctrl Pts',(-9.28861783421259,-83.9216282439495,
74.8011690336164));
#128842=CARTESIAN_POINT('Ctrl Pts',(-9.27067335198321,-84.0435701905272,
73.9876456980361));
#128843=CARTESIAN_POINT('Ctrl Pts',(-9.23559857568525,-84.0692658482991,
72.6688868688745));
#128844=CARTESIAN_POINT('Ctrl Pts',(-9.22129912397754,-84.0385238649345,
72.1639069572095));
#128845=CARTESIAN_POINT('Ctrl Pts',(-9.17806499529417,-83.8261976625481,
70.6799500060793));
#128846=CARTESIAN_POINT('Ctrl Pts',(-9.14973443391088,-83.5394059276481,
69.759533298521));
#128847=CARTESIAN_POINT('Ctrl Pts',(-9.11259821608478,-82.8754352936373,
68.457692926074));
#128848=CARTESIAN_POINT('Ctrl Pts',(-9.10120006670172,-82.6205555564293,
68.0464749363187));
#128849=CARTESIAN_POINT('Ctrl Pts',(-9.07117941927312,-81.8617738677188,
67.0142743202317));
#128850=CARTESIAN_POINT('Ctrl Pts',(-9.0526252660902,-81.3037983603748,
66.4320817378967));
#128851=CARTESIAN_POINT('Ctrl Pts',(-9.02101932872785,-80.3960614529603,
65.6984913538591));
#128852=CARTESIAN_POINT('Ctrl Pts',(-9.01027898281615,-80.095877405622,
65.4838148866877));
#128853=CARTESIAN_POINT('Ctrl Pts',(-8.97854614193354,-79.1982942694184,
64.919936575508));
#128854=CARTESIAN_POINT('Ctrl Pts',(-8.95702945793924,-78.5711451652899,
64.6180035181383));
#128855=CARTESIAN_POINT('Ctrl Pts',(-8.93208463483441,-77.6737217783435,
64.3127662936522));
#128856=CARTESIAN_POINT('Ctrl Pts',(-8.92586970758882,-77.4284089827495,
64.2415585305407));
#128857=CARTESIAN_POINT('Ctrl Pts',(-8.90731371882341,-76.656624899155,
64.0536446207396));
#128858=CARTESIAN_POINT('Ctrl Pts',(-8.89561309755475,-76.1209216390034,
63.9745840947576));
#128859=CARTESIAN_POINT('Ctrl Pts',(-8.86487641062158,-74.8360842494938,
63.8986189294642));
#128860=CARTESIAN_POINT('Ctrl Pts',(-8.8454456967949,-74.0835849981138,
63.9451390777231));
#128861=CARTESIAN_POINT('Ctrl Pts',(-8.80150233458386,-72.5160619401253,
64.2314456703135));
#128862=CARTESIAN_POINT('Ctrl Pts',(-8.77624830234048,-71.7038290454958,
64.4962199491525));
#128863=CARTESIAN_POINT('Ctrl Pts',(-8.74167392707594,-70.6373754027766,
65.0238411724459));
#128864=CARTESIAN_POINT('Ctrl Pts',(-8.7322116805582,-70.3402399112782,
65.1935581209927));
#128865=CARTESIAN_POINT('Ctrl Pts',(-8.71444262084913,-69.7582083441322,
65.5740566021455));
#128866=CARTESIAN_POINT('Ctrl Pts',(-8.70610048266984,-69.4763651028232,
65.7836686004065));
#128867=CARTESIAN_POINT('Ctrl Pts',(-8.6828861938593,-68.7101137563505,
66.4260840139121));
#128868=CARTESIAN_POINT('Ctrl Pts',(-8.66847293392533,-68.2575214534165,
66.8969486960608));
#128869=CARTESIAN_POINT('Ctrl Pts',(-8.63968961238916,-67.5604294912633,
67.7914454924441));
#128870=CARTESIAN_POINT('Ctrl Pts',(-8.62604720722989,-67.2920488707874,
68.1971115278178));
#128871=CARTESIAN_POINT('Ctrl Pts',(-8.59751203614483,-66.8162040163527,
69.0551559022318));
#128872=CARTESIAN_POINT('Ctrl Pts',(-8.58263360341257,-66.6102415503235,
69.5086547539668));
#128873=CARTESIAN_POINT('Ctrl Pts',(-8.56837920259168,-66.4431891936119,
69.976120966934));
#128874=CARTESIAN_POINT('Ctrl Pts',(-9.88022273965691,-67.62520219141,67.700413019766));
#128875=CARTESIAN_POINT('Ctrl Pts',(-9.81362168955091,-66.1498345501,69.757818081886));
#128876=CARTESIAN_POINT('Ctrl Pts',(-9.68041958933991,-65.03881684527,75.159924360853));
#128877=CARTESIAN_POINT('Ctrl Pts',(-9.48061643902391,-69.94095953137,81.84418107373));
#128878=CARTESIAN_POINT('Ctrl Pts',(-9.28081328870791,-78.18756436805,82.675374708005));
#128879=CARTESIAN_POINT('Ctrl Pts',(-9.08101013839191,-84.3279816375,77.109502645436));
#128880=CARTESIAN_POINT('Ctrl Pts',(-8.88120698807591,-84.30727308569,68.821968198106));
#128881=CARTESIAN_POINT('Ctrl Pts',(-8.68140383775991,-78.13920519194,63.285515123434));
#128882=CARTESIAN_POINT('Ctrl Pts',(-8.48160068744491,-69.89662703841,64.163123294247));
#128883=CARTESIAN_POINT('Ctrl Pts',(-8.34839858723391,-66.65138462743,68.622440986855));
#128884=CARTESIAN_POINT('Ctrl Pts',(-8.28179753712891,-66.12404568677,71.098635427588));
#128885=CARTESIAN_POINT('Ctrl Pts',(-9.96688940632291,-67.62520219141,67.700413019766));
#128886=CARTESIAN_POINT('Ctrl Pts',(-9.90028835621791,-66.1498345501,69.757818081886));
#128887=CARTESIAN_POINT('Ctrl Pts',(-9.76708625600691,-65.03881684527,75.159924360853));
#128888=CARTESIAN_POINT('Ctrl Pts',(-9.56728310569091,-69.94095953137,81.84418107373));
#128889=CARTESIAN_POINT('Ctrl Pts',(-9.36747995537491,-78.18756436805,82.675374708005));
#128890=CARTESIAN_POINT('Ctrl Pts',(-9.16767680505891,-84.3279816375,77.109502645436));
#128891=CARTESIAN_POINT('Ctrl Pts',(-8.96787365474291,-84.30727308569,68.821968198106));
#128892=CARTESIAN_POINT('Ctrl Pts',(-8.76807050442691,-78.13920519194,63.285515123434));
#128893=CARTESIAN_POINT('Ctrl Pts',(-8.56826735411091,-69.89662703841,64.163123294247));
#128894=CARTESIAN_POINT('Ctrl Pts',(-8.43506525390091,-66.65138462743,68.622440986855));
#128895=CARTESIAN_POINT('Ctrl Pts',(-8.36846420379491,-66.12404568677,71.098635427588));
#128896=CARTESIAN_POINT('Ctrl Pts',(-10.0535560729899,-67.62520219141,67.700413019766));
#128897=CARTESIAN_POINT('Ctrl Pts',(-9.98695502288491,-66.1498345501,69.757818081886));
#128898=CARTESIAN_POINT('Ctrl Pts',(-9.85375292267391,-65.03881684527,75.159924360853));
#128899=CARTESIAN_POINT('Ctrl Pts',(-9.65394977235791,-69.94095953137,81.84418107373));
#128900=CARTESIAN_POINT('Ctrl Pts',(-9.45414662204191,-78.18756436805,82.675374708005));
#128901=CARTESIAN_POINT('Ctrl Pts',(-9.25434347172591,-84.3279816375,77.109502645436));
#128902=CARTESIAN_POINT('Ctrl Pts',(-9.05454032140991,-84.30727308569,68.821968198106));
#128903=CARTESIAN_POINT('Ctrl Pts',(-8.85473717109391,-78.13920519194,63.285515123434));
#128904=CARTESIAN_POINT('Ctrl Pts',(-8.65493402077791,-69.89662703841,64.163123294247));
#128905=CARTESIAN_POINT('Ctrl Pts',(-8.52173192056691,-66.65138462743,68.622440986855));
#128906=CARTESIAN_POINT('Ctrl Pts',(-8.45513087046191,-66.12404568677,71.098635427588));
#128907=CARTESIAN_POINT('Ctrl Pts',(-10.1402227396569,-67.62520219141,67.700413019766));
#128908=CARTESIAN_POINT('Ctrl Pts',(-10.0736216895509,-66.1498345501,69.757818081886));
#128909=CARTESIAN_POINT('Ctrl Pts',(-9.94041958933991,-65.03881684527,75.159924360853));
#128910=CARTESIAN_POINT('Ctrl Pts',(-9.74061643902391,-69.94095953137,81.84418107373));
#128911=CARTESIAN_POINT('Ctrl Pts',(-9.54081328870791,-78.18756436805,82.675374708005));
#128912=CARTESIAN_POINT('Ctrl Pts',(-9.34101013839191,-84.3279816375,77.109502645436));
#128913=CARTESIAN_POINT('Ctrl Pts',(-9.14120698807591,-84.30727308569,68.821968198106));
#128914=CARTESIAN_POINT('Ctrl Pts',(-8.94140383775991,-78.13920519194,63.285515123434));
#128915=CARTESIAN_POINT('Ctrl Pts',(-8.74160068744491,-69.89662703841,64.163123294247));
#128916=CARTESIAN_POINT('Ctrl Pts',(-8.60839858723391,-66.65138462743,68.622440986855));
#128917=CARTESIAN_POINT('Ctrl Pts',(-8.54179753712891,-66.12404568677,71.098635427588));
#128918=CARTESIAN_POINT('Ctrl Pts',(-10.1421465283748,-67.62520219141,67.700413019766));
#128919=CARTESIAN_POINT('Ctrl Pts',(-10.0755454782688,-66.1498345501,69.757818081886));
#128920=CARTESIAN_POINT('Ctrl Pts',(-9.94234337805777,-65.03881684527,75.159924360853));
#128921=CARTESIAN_POINT('Ctrl Pts',(-9.74254022774178,-69.94095953137,81.84418107373));
#128922=CARTESIAN_POINT('Ctrl Pts',(-9.54273707742577,-78.18756436805,82.675374708005));
#128923=CARTESIAN_POINT('Ctrl Pts',(-9.34293392710978,-84.3279816375,77.109502645436));
#128924=CARTESIAN_POINT('Ctrl Pts',(-9.14313077679378,-84.30727308569,68.821968198106));
#128925=CARTESIAN_POINT('Ctrl Pts',(-8.94332762647777,-78.13920519194,63.285515123434));
#128926=CARTESIAN_POINT('Ctrl Pts',(-8.7435244761628,-69.89662703841,64.163123294247));
#128927=CARTESIAN_POINT('Ctrl Pts',(-8.6103223759518,-66.65138462743,68.622440986855));
#128928=CARTESIAN_POINT('Ctrl Pts',(-8.5437213258468,-66.12404568677,71.098635427588));
#128929=CARTESIAN_POINT('Ctrl Pts',(-10.1440703170927,-67.62520219141,67.700413019766));
#128930=CARTESIAN_POINT('Ctrl Pts',(-10.0774692669866,-66.1498345501,69.757818081886));
#128931=CARTESIAN_POINT('Ctrl Pts',(-9.94426716677564,-65.03881684527,75.159924360853));
#128932=CARTESIAN_POINT('Ctrl Pts',(-9.74446401645964,-69.94095953137,81.84418107373));
#128933=CARTESIAN_POINT('Ctrl Pts',(-9.54466086614364,-78.18756436805,82.675374708005));
#128934=CARTESIAN_POINT('Ctrl Pts',(-9.34485771582764,-84.3279816375,77.109502645436));
#128935=CARTESIAN_POINT('Ctrl Pts',(-9.14505456551164,-84.30727308569,68.821968198106));
#128936=CARTESIAN_POINT('Ctrl Pts',(-8.94525141519564,-78.13920519194,63.285515123434));
#128937=CARTESIAN_POINT('Ctrl Pts',(-8.74544826488068,-69.89662703841,64.163123294247));
#128938=CARTESIAN_POINT('Ctrl Pts',(-8.61224616466968,-66.65138462743,68.622440986855));
#128939=CARTESIAN_POINT('Ctrl Pts',(-8.54564511456468,-66.12404568677,71.098635427588));
#128940=CARTESIAN_POINT('Ctrl Pts',(-10.1459941058106,-67.62520219141,67.700413019766));
#128941=CARTESIAN_POINT('Ctrl Pts',(-10.0793930557045,-66.1498345501,69.757818081886));
#128942=CARTESIAN_POINT('Ctrl Pts',(-9.9461909554935,-65.03881684527,75.159924360853));
#128943=CARTESIAN_POINT('Ctrl Pts',(-9.7463878051775,-69.94095953137,81.84418107373));
#128944=CARTESIAN_POINT('Ctrl Pts',(-9.5465846548615,-78.18756436805,82.675374708005));
#128945=CARTESIAN_POINT('Ctrl Pts',(-9.3467815045455,-84.3279816375,77.109502645436));
#128946=CARTESIAN_POINT('Ctrl Pts',(-9.1469783542295,-84.30727308569,68.821968198106));
#128947=CARTESIAN_POINT('Ctrl Pts',(-8.9471752039135,-78.13920519194,63.285515123434));
#128948=CARTESIAN_POINT('Ctrl Pts',(-8.74737205359857,-69.89662703841,64.163123294247));
#128949=CARTESIAN_POINT('Ctrl Pts',(-8.61416995338757,-66.65138462743,68.622440986855));
#128950=CARTESIAN_POINT('Ctrl Pts',(-8.54756890328257,-66.12404568677,71.098635427588));
#128951=CARTESIAN_POINT('',(-9.85448379345391,-67.0101053268475,68.6926900228996));
#128952=CARTESIAN_POINT('Ctrl Pts',(-13.1454639400434,-80.45858984268,79.025262748814));
#128953=CARTESIAN_POINT('Ctrl Pts',(-13.1047676696649,-81.48759917444,78.094747098225));
#128954=CARTESIAN_POINT('Ctrl Pts',(-13.023375128908,-83.05789139581,75.697173136178));
#128955=CARTESIAN_POINT('Ctrl Pts',(-12.9012863177725,-83.35252030674,71.406833513058));
#128956=CARTESIAN_POINT('Ctrl Pts',(-12.779197506637,-81.50958548889,67.521577101676));
#128957=CARTESIAN_POINT('Ctrl Pts',(-12.6571086955016,-78.00102966728,65.03524813757));
#128958=CARTESIAN_POINT('Ctrl Pts',(-12.535019884366,-73.72453794147,64.584146732116));
#128959=CARTESIAN_POINT('Ctrl Pts',(-12.4129310732305,-69.77442198226,66.283678758148));
#128960=CARTESIAN_POINT('Ctrl Pts',(-12.2908422620949,-67.16144589233,69.698967665193));
#128961=CARTESIAN_POINT('Ctrl Pts',(-12.1687534509593,-66.5542301033,73.9560942582189));
#128962=CARTESIAN_POINT('Ctrl Pts',(-12.0466646398237,-68.10815086311,77.965728779761));
#128963=CARTESIAN_POINT('Ctrl Pts',(-11.9245758286881,-71.42558498136,80.70187013362));
#128964=CARTESIAN_POINT('Ctrl Pts',(-11.8024870175525,-75.65765439615,81.464383794463));
#128965=CARTESIAN_POINT('Ctrl Pts',(-11.6803982064169,-79.72144063224,80.058154773716));
#128966=CARTESIAN_POINT('Ctrl Pts',(-11.5583093952809,-82.57708616044,76.843014459137));
#128967=CARTESIAN_POINT('Ctrl Pts',(-11.4362205841459,-83.49387722752,72.6416655369234));
#128968=CARTESIAN_POINT('Ctrl Pts',(-11.3141317730099,-82.23722174699,68.52916561233));
#128969=CARTESIAN_POINT('Ctrl Pts',(-11.1920429618739,-79.12867764146,65.557837261156));
#128970=CARTESIAN_POINT('Ctrl Pts',(-11.0699541507389,-74.96367134257,64.48799561084));
#128971=CARTESIAN_POINT('Ctrl Pts',(-10.9478653396029,-70.80796096272,65.593395929895));
#128972=CARTESIAN_POINT('Ctrl Pts',(-10.8257765284669,-67.72492593816,68.59118405853));
#128973=CARTESIAN_POINT('Ctrl Pts',(-10.7036877173319,-66.50346533712,72.714274237664));
#128974=CARTESIAN_POINT('Ctrl Pts',(-10.5815989061959,-67.45613127848,76.907634016596));
#128975=CARTESIAN_POINT('Ctrl Pts',(-10.4595100950609,-70.33915187332,80.09825008004));
#128976=CARTESIAN_POINT('Ctrl Pts',(-10.3374212839249,-74.4148085262,81.46969511541));
#128977=CARTESIAN_POINT('Ctrl Pts',(-10.2153324727889,-78.64020627051,80.671038351543));
#128978=CARTESIAN_POINT('Ctrl Pts',(-10.0932436616539,-81.93413376206,77.906643386292));
#128979=CARTESIAN_POINT('Ctrl Pts',(-9.97115485051791,-83.45372806371,73.8838737528785));
#128980=CARTESIAN_POINT('Ctrl Pts',(-9.84906603938191,-82.81014898713,69.632093987784));
#128981=CARTESIAN_POINT('Ctrl Pts',(-9.72697722824691,-80.16807974905,66.239256812192));
#128982=CARTESIAN_POINT('Ctrl Pts',(-9.60488841711091,-76.20357708221,64.573569483865));
#128983=CARTESIAN_POINT('Ctrl Pts',(-9.48279960597591,-71.93111689791,65.061124710008));
#128984=CARTESIAN_POINT('Ctrl Pts',(-9.36071079483991,-68.44386550154,67.577649690078));
#128985=CARTESIAN_POINT('Ctrl Pts',(-9.27931825408291,-67.23760922485,70.177481292106));
#128986=CARTESIAN_POINT('Ctrl Pts',(-9.23862198370491,-66.9910877936,71.542745649207));
#128987=CARTESIAN_POINT('Ctrl Pts',(-13.3760469519197,-80.72646219088,79.321488981906));
#128988=CARTESIAN_POINT('Ctrl Pts',(-13.3353506815413,-81.80596865723,78.345309630701));
#128989=CARTESIAN_POINT('Ctrl Pts',(-13.2539581407843,-83.45332068284,75.830078217611));
#128990=CARTESIAN_POINT('Ctrl Pts',(-13.1318693296489,-83.76240807855,71.329196424715));
#128991=CARTESIAN_POINT('Ctrl Pts',(-13.0097805185134,-81.82903391805,67.253276712327));
#128992=CARTESIAN_POINT('Ctrl Pts',(-12.8876917073779,-78.14830082834,64.644934774694));
#128993=CARTESIAN_POINT('Ctrl Pts',(-12.7656028962424,-73.66194649816,64.171696224628));
#128994=CARTESIAN_POINT('Ctrl Pts',(-12.6435140851068,-69.51798435008,65.954630310129));
#128995=CARTESIAN_POINT('Ctrl Pts',(-12.5214252739713,-66.77678026333,69.537519547238));
#128996=CARTESIAN_POINT('Ctrl Pts',(-12.3993364628357,-66.13976624364,74.003558428952));
#128997=CARTESIAN_POINT('Ctrl Pts',(-12.2772476517001,-67.76994340206,78.209959926145));
#128998=CARTESIAN_POINT('Ctrl Pts',(-12.1551588405645,-71.2501757691,81.080373432798));
#128999=CARTESIAN_POINT('Ctrl Pts',(-12.0330700294289,-75.68992782805,81.880306341227));
#129000=CARTESIAN_POINT('Ctrl Pts',(-11.9109812182932,-79.95313845632,80.405068678906));
#129001=CARTESIAN_POINT('Ctrl Pts',(-11.7888924071576,-82.94892063066,77.032150034994));
#129002=CARTESIAN_POINT('Ctrl Pts',(-11.666803596022,-83.91070188439,72.6246260320682));
#129003=CARTESIAN_POINT('Ctrl Pts',(-11.5447147848859,-82.59237786598,68.310311161955));
#129004=CARTESIAN_POINT('Ctrl Pts',(-11.4226259737509,-79.33128648485,65.193169198556));
#129005=CARTESIAN_POINT('Ctrl Pts',(-11.3005371626149,-74.96188856657,64.070826627081));
#129006=CARTESIAN_POINT('Ctrl Pts',(-11.1784483514789,-70.60224275103,65.23047285722));
#129007=CARTESIAN_POINT('Ctrl Pts',(-11.0563595403439,-67.36791227191,68.375373073155));
#129008=CARTESIAN_POINT('Ctrl Pts',(-10.9342707292079,-66.08651027048,72.7007978991383));
#129009=CARTESIAN_POINT('Ctrl Pts',(-10.8121819180719,-67.08592690573,77.0999407032));
#129010=CARTESIAN_POINT('Ctrl Pts',(-10.6900931069369,-70.11042753827,80.447131604038));
#129011=CARTESIAN_POINT('Ctrl Pts',(-10.5680042958009,-74.38609110676,81.885878307519));
#129012=CARTESIAN_POINT('Ctrl Pts',(-10.4459154846659,-78.8188440927,81.048028625887));
#129013=CARTESIAN_POINT('Ctrl Pts',(-10.3238266735299,-82.27441627954,78.147975002984));
#129014=CARTESIAN_POINT('Ctrl Pts',(-10.2017378623939,-83.86858245883,73.9277938074276));
#129015=CARTESIAN_POINT('Ctrl Pts',(-10.0796490512589,-83.19342067618,69.46736414145));
#129016=CARTESIAN_POINT('Ctrl Pts',(-9.95756024012291,-80.4216957374,65.908028421839));
#129017=CARTESIAN_POINT('Ctrl Pts',(-9.83547142898791,-76.26264087496,64.160599913318));
#129018=CARTESIAN_POINT('Ctrl Pts',(-9.71338261785191,-71.78051592832,64.672081202253));
#129019=CARTESIAN_POINT('Ctrl Pts',(-9.59129380671691,-68.12213274751,67.312100981366));
#129020=CARTESIAN_POINT('Ctrl Pts',(-9.50990126595991,-66.8566812005,70.039515533604));
#129021=CARTESIAN_POINT('Ctrl Pts',(-9.46920499558091,-66.59806208898,71.471778251044));
#129022=CARTESIAN_POINT('Ctrl Pts',(-13.6066299637959,-80.99433453906,79.617715215002));
#129023=CARTESIAN_POINT('Ctrl Pts',(-13.5659336934176,-82.12433814002,78.595872163185));
#129024=CARTESIAN_POINT('Ctrl Pts',(-13.4845411526607,-83.84874996986,75.962983299056));
#129025=CARTESIAN_POINT('Ctrl Pts',(-13.3624523415252,-84.17229585037,71.251559336391));
#129026=CARTESIAN_POINT('Ctrl Pts',(-13.2403635303897,-82.14848234721,66.984976322999));
#129027=CARTESIAN_POINT('Ctrl Pts',(-13.1182747192542,-78.29557198944,64.254621411829));
#129028=CARTESIAN_POINT('Ctrl Pts',(-12.9961859081187,-73.59935505488,63.759245717135));
#129029=CARTESIAN_POINT('Ctrl Pts',(-12.8740970969832,-69.26154671793,65.625581862084));
#129030=CARTESIAN_POINT('Ctrl Pts',(-12.7520082858476,-66.39211463435,69.376071429236));
#129031=CARTESIAN_POINT('Ctrl Pts',(-12.629919474712,-65.72530238397,74.051022599625));
#129032=CARTESIAN_POINT('Ctrl Pts',(-12.5078306635764,-67.43173594097,78.454191072474));
#129033=CARTESIAN_POINT('Ctrl Pts',(-12.3857418524408,-71.07476655678,81.458876731945));
#129034=CARTESIAN_POINT('Ctrl Pts',(-12.2636530413052,-75.72220125986,82.296228887996));
#129035=CARTESIAN_POINT('Ctrl Pts',(-12.1415642301696,-80.18483628034,80.751982584142));
#129036=CARTESIAN_POINT('Ctrl Pts',(-12.0194754190339,-83.32075510084,77.221285610932));
#129037=CARTESIAN_POINT('Ctrl Pts',(-11.8973866078983,-84.32752654126,72.6075865273095));
#129038=CARTESIAN_POINT('Ctrl Pts',(-11.7752977967627,-82.94753398501,68.091456711666));
#129039=CARTESIAN_POINT('Ctrl Pts',(-11.653208985627,-79.53389532833,64.828501136008));
#129040=CARTESIAN_POINT('Ctrl Pts',(-11.5311201744909,-74.96010579067,63.653657643322));
#129041=CARTESIAN_POINT('Ctrl Pts',(-11.4090313633559,-70.39652453943,64.867549784492));
#129042=CARTESIAN_POINT('Ctrl Pts',(-11.2869425522199,-67.01089860571,68.159562087686));
#129043=CARTESIAN_POINT('Ctrl Pts',(-11.1648537410839,-65.66955520384,72.6873215605024));
#129044=CARTESIAN_POINT('Ctrl Pts',(-11.0427649299489,-66.71572253294,77.292247389707));
#129045=CARTESIAN_POINT('Ctrl Pts',(-10.9206761188129,-69.88170320312,80.796013127978));
#129046=CARTESIAN_POINT('Ctrl Pts',(-10.7985873076779,-74.35737368722,82.302061499622));
#129047=CARTESIAN_POINT('Ctrl Pts',(-10.6764984965419,-78.99748191481,81.425018900273));
#129048=CARTESIAN_POINT('Ctrl Pts',(-10.5544096854059,-82.61469879698,78.389306619751));
#129049=CARTESIAN_POINT('Ctrl Pts',(-10.4323208742709,-84.28343685395,73.9717138620569));
#129050=CARTESIAN_POINT('Ctrl Pts',(-10.3102320631349,-83.57669236526,69.30263429518));
#129051=CARTESIAN_POINT('Ctrl Pts',(-10.1881432519999,-80.67531172579,65.57680003152));
#129052=CARTESIAN_POINT('Ctrl Pts',(-10.0660544408639,-76.32170466775,63.747630342775));
#129053=CARTESIAN_POINT('Ctrl Pts',(-9.94396562972891,-71.62991495875,64.283037694485));
#129054=CARTESIAN_POINT('Ctrl Pts',(-9.82187681859291,-67.80039999349,67.046552272646));
#129055=CARTESIAN_POINT('Ctrl Pts',(-9.74048427783591,-66.47575317615,69.901549775107));
#129056=CARTESIAN_POINT('Ctrl Pts',(-9.69978800745791,-66.20503638435,71.400810852893));
#129057=CARTESIAN_POINT('Ctrl Pts',(-13.8372129756729,-81.26220688726,79.913941448094));
#129058=CARTESIAN_POINT('Ctrl Pts',(-13.7965167052939,-82.44270762281,78.846434695661));
#129059=CARTESIAN_POINT('Ctrl Pts',(-13.7151241645369,-84.24417925689,76.095888380488));
#129060=CARTESIAN_POINT('Ctrl Pts',(-13.5930353534019,-84.58218362219,71.173922248048));
#129061=CARTESIAN_POINT('Ctrl Pts',(-13.4709465422661,-82.46793077636,66.716675933649));
#129062=CARTESIAN_POINT('Ctrl Pts',(-13.3488577311306,-78.4428431505,63.864308048952));
#129063=CARTESIAN_POINT('Ctrl Pts',(-13.2267689199951,-73.53676361156,63.346795209648));
#129064=CARTESIAN_POINT('Ctrl Pts',(-13.1046801088595,-69.00510908574,65.296533414067));
#129065=CARTESIAN_POINT('Ctrl Pts',(-12.982591297724,-66.00744900535,69.214623311284));
#129066=CARTESIAN_POINT('Ctrl Pts',(-12.8605024865884,-65.31083852431,74.098486770361));
#129067=CARTESIAN_POINT('Ctrl Pts',(-12.7384136754528,-67.09352847992,78.698422218861));
#129068=CARTESIAN_POINT('Ctrl Pts',(-12.6163248643172,-70.89935734453,81.837380031125));
#129069=CARTESIAN_POINT('Ctrl Pts',(-12.4942360531816,-75.75447469176,82.71215143476));
#129070=CARTESIAN_POINT('Ctrl Pts',(-12.3721472420459,-80.41653410443,81.098896489329));
#129071=CARTESIAN_POINT('Ctrl Pts',(-12.2500584309103,-83.69258957107,77.410421186785));
#129072=CARTESIAN_POINT('Ctrl Pts',(-12.1279696197746,-84.74435119813,72.5905470224496));
#129073=CARTESIAN_POINT('Ctrl Pts',(-12.005880808639,-83.302690104,67.872602261286));
#129074=CARTESIAN_POINT('Ctrl Pts',(-11.8837919975033,-79.73650417172,64.463833073406));
#129075=CARTESIAN_POINT('Ctrl Pts',(-11.7617031863677,-74.95832301467,63.236488659563));
#129076=CARTESIAN_POINT('Ctrl Pts',(-11.639614375232,-70.19080632774,64.50462671182));
#129077=CARTESIAN_POINT('Ctrl Pts',(-11.5175255640959,-66.65388493945,67.943751102315));
#129078=CARTESIAN_POINT('Ctrl Pts',(-11.3954367529609,-65.25260013719,72.673845221982));
#129079=CARTESIAN_POINT('Ctrl Pts',(-11.2733479418249,-66.34551816019,77.484554076315));
#129080=CARTESIAN_POINT('Ctrl Pts',(-11.1512591306899,-69.65297886807,81.144894651979));
#129081=CARTESIAN_POINT('Ctrl Pts',(-11.0291703195539,-74.32865626779,82.718244691732));
#129082=CARTESIAN_POINT('Ctrl Pts',(-10.9070815084179,-79.176119737,81.802009174614));
#129083=CARTESIAN_POINT('Ctrl Pts',(-10.7849926972829,-82.95498131447,78.63063823644));
#129084=CARTESIAN_POINT('Ctrl Pts',(-10.6629038861469,-84.69829124907,74.015633916602));
#129085=CARTESIAN_POINT('Ctrl Pts',(-10.5408150750119,-83.95996405431,69.137904448843));
#129086=CARTESIAN_POINT('Ctrl Pts',(-10.4187262638759,-80.92892771414,65.245571641166));
#129087=CARTESIAN_POINT('Ctrl Pts',(-10.2966374527399,-76.3807684605,63.334660772228));
#129088=CARTESIAN_POINT('Ctrl Pts',(-10.1745486416049,-71.47931398915,63.89399418673));
#129089=CARTESIAN_POINT('Ctrl Pts',(-10.0524598304689,-67.47866723947,66.781003563935));
#129090=CARTESIAN_POINT('Ctrl Pts',(-9.97106728971191,-66.0948251518,69.763584016604));
#129091=CARTESIAN_POINT('Ctrl Pts',(-9.93037101933391,-65.81201067972,71.32984345473));
#129092=CARTESIAN_POINT('',(-13.5671411686305,-83.5589497503404,76.0033450387178));
#129093=CARTESIAN_POINT('Ctrl Pts',(-13.5667458539302,-83.5583092465054,
76.0031044421984));
#129094=CARTESIAN_POINT('Ctrl Pts',(-13.5640800181624,-83.5922872145127,
75.9068207927514));
#129095=CARTESIAN_POINT('Ctrl Pts',(-13.5614447593399,-83.6246546966739,
75.8099696689204));
#129096=CARTESIAN_POINT('Ctrl Pts',(-13.5530672454983,-83.7233362399437,
75.4973489808209));
#129097=CARTESIAN_POINT('Ctrl Pts',(-13.5474177830113,-83.7833032435454,
75.2795745744807));
#129098=CARTESIAN_POINT('Ctrl Pts',(-13.5350766693028,-83.8962038299702,
74.8001260870673));
#129099=CARTESIAN_POINT('Ctrl Pts',(-13.5283798935997,-83.9458836624366,
74.5376098343622));
#129100=CARTESIAN_POINT('Ctrl Pts',(-13.5177668235028,-84.0038523401724,
74.1318657443427));
#129101=CARTESIAN_POINT('Ctrl Pts',(-13.5140091710748,-84.0206428553733,
73.9899873829069));
#129102=CARTESIAN_POINT('Ctrl Pts',(-13.5002165626111,-84.069262514367,
73.4739678360416));
#129103=CARTESIAN_POINT('Ctrl Pts',(-13.4899251488299,-84.0810377628333,
73.0979524172502));
#129104=CARTESIAN_POINT('Ctrl Pts',(-13.4703039519722,-84.0594037634423,
72.3811619891736));
#129105=CARTESIAN_POINT('Ctrl Pts',(-13.4609717905523,-84.0299673204892,
72.0402094984997));
#129106=CARTESIAN_POINT('Ctrl Pts',(-13.448222877598,-83.9620661056739,
71.5649788215202));
#129107=CARTESIAN_POINT('Ctrl Pts',(-13.4445894694965,-83.9393892802237,
71.4284087441626));
#129108=CARTESIAN_POINT('Ctrl Pts',(-13.4339896337949,-83.8630274060158,
71.0253456742784));
#129109=CARTESIAN_POINT('Ctrl Pts',(-13.4271842518906,-83.8005219868351,
70.7605125131827));
#129110=CARTESIAN_POINT('Ctrl Pts',(-13.4140566946332,-83.6572722714153,
70.2563978903051));
#129111=CARTESIAN_POINT('Ctrl Pts',(-13.4077344473922,-83.578171160243,
70.0166636317799));
#129112=CARTESIAN_POINT('Ctrl Pts',(-13.3975075655731,-83.4380202727791,
69.6457919580006));
#129113=CARTESIAN_POINT('Ctrl Pts',(-13.3937272172911,-83.3837478006566,
69.5121191198762));
#129114=CARTESIAN_POINT('Ctrl Pts',(-13.3812477757693,-83.1962513613288,
69.0804671876166));
#129115=CARTESIAN_POINT('Ctrl Pts',(-13.3723658901788,-83.0498920388042,
68.7882126092547));
#129116=CARTESIAN_POINT('Ctrl Pts',(-13.3558977290774,-82.7512917519671,
68.2640874293851));
#129117=CARTESIAN_POINT('Ctrl Pts',(-13.3483197841579,-82.6033049797775,
68.0297661795723));
#129118=CARTESIAN_POINT('Ctrl Pts',(-13.3356439017166,-82.3348534023005,
67.6444514316513));
#129119=CARTESIAN_POINT('Ctrl Pts',(-13.3304913444046,-82.2196693095211,
67.4897495021949));
#129120=CARTESIAN_POINT('Ctrl Pts',(-13.3216308651203,-82.0096748178785,
67.2255380783767));
#129121=CARTESIAN_POINT('Ctrl Pts',(-13.3178882932308,-81.916940108937,
67.1143726804648));
#129122=CARTESIAN_POINT('Ctrl Pts',(-13.3064348773527,-81.6210698998257,
66.7763831217991));
#129123=CARTESIAN_POINT('Ctrl Pts',(-13.2988745494577,-81.4090562151365,
66.5573305579049));
#129124=CARTESIAN_POINT('Ctrl Pts',(-13.287872999267,-81.0900536116174,
66.2596318506067));
#129125=CARTESIAN_POINT('Ctrl Pts',(-13.2845263606801,-80.9916661173901,
66.171791176635));
#129126=CARTESIAN_POINT('Ctrl Pts',(-13.2773780454483,-80.7804502592599,
65.9915038295038));
#129127=CARTESIAN_POINT('Ctrl Pts',(-13.2735652493214,-80.667249665329,
65.8996055717503));
#129128=CARTESIAN_POINT('Ctrl Pts',(-13.2569637833204,-80.1708073118262,
65.5162542685411));
#129129=CARTESIAN_POINT('Ctrl Pts',(-13.2437214187867,-79.7660220760457,
65.2526560754908));
#129130=CARTESIAN_POINT('Ctrl Pts',(-13.2249963764698,-79.1622973306626,
64.9239326290828));
#129131=CARTESIAN_POINT('Ctrl Pts',(-13.2194107577164,-78.9781280276051,
64.8315536077034));
#129132=CARTESIAN_POINT('Ctrl Pts',(-13.2094511159405,-78.6401712057606,
64.6760356169752));
#129133=CARTESIAN_POINT('Ctrl Pts',(-13.2050514003971,-78.4873851110901,
64.6106925387327));
#129134=CARTESIAN_POINT('Ctrl Pts',(-13.1960707382152,-78.1668763190988,
64.4838235016176));
#129135=CARTESIAN_POINT('Ctrl Pts',(-13.1915142562595,-77.9988949418862,
64.4229538109884));
#129136=CARTESIAN_POINT('Ctrl Pts',(-13.180415362693,-77.5813063138297,
64.2854135325013));
#129137=CARTESIAN_POINT('Ctrl Pts',(-13.1739176940635,-77.3298340995017,
64.2144287922523));
#129138=CARTESIAN_POINT('Ctrl Pts',(-13.163063039009,-76.9126045445894,
64.1161350615823));
#129139=CARTESIAN_POINT('Ctrl Pts',(-13.158772440825,-76.7486833212321,
64.0823561069267));
#129140=CARTESIAN_POINT('Ctrl Pts',(-13.1496316182324,-76.4040563125874,
64.0214430337194));
#129141=CARTESIAN_POINT('Ctrl Pts',(-13.1447908325575,-76.2236333412628,
63.9952203562065));
#129142=CARTESIAN_POINT('Ctrl Pts',(-13.1283856998445,-75.6163755370945,
63.9256352625226));
#129143=CARTESIAN_POINT('Ctrl Pts',(-13.1165911008828,-75.1866770975472,
63.9071418211856));
#129144=CARTESIAN_POINT('Ctrl Pts',(-13.0998492934382,-74.5700735368246,
63.9237963404925));
#129145=CARTESIAN_POINT('Ctrl Pts',(-13.0947798985282,-74.3824540529019,
63.9346345962008));
#129146=CARTESIAN_POINT('Ctrl Pts',(-13.0855265611452,-74.0365003082374,
63.9653006109643));
#129147=CARTESIAN_POINT('Ctrl Pts',(-13.0813243282303,-73.8780146894078,
63.9835242403866));
#129148=CARTESIAN_POINT('Ctrl Pts',(-13.0709193471626,-73.4806638935296,
64.0397825970281));
#129149=CARTESIAN_POINT('Ctrl Pts',(-13.0648252092706,-73.2425600506697,
64.0831879404041));
#129150=CARTESIAN_POINT('Ctrl Pts',(-13.0520354529743,-72.7455612383279,
64.1945445275424));
#129151=CARTESIAN_POINT('Ctrl Pts',(-13.0453376145367,-72.4870360765741,
64.264634065654));
#129152=CARTESIAN_POINT('Ctrl Pts',(-13.034385538917,-72.0824983766059,
64.3942244165957));
#129153=CARTESIAN_POINT('Ctrl Pts',(-13.030271002386,-71.9342234575551,
64.446095201498));
#129154=CARTESIAN_POINT('Ctrl Pts',(-13.0136565124453,-71.3481710882388,
64.6685101182148));
#129155=CARTESIAN_POINT('Ctrl Pts',(-13.0007741957329,-70.9220142912128,
64.8696380442875));
#129156=CARTESIAN_POINT('Ctrl Pts',(-12.982152422141,-70.3268398396603,
65.2085630953448));
#129157=CARTESIAN_POINT('Ctrl Pts',(-12.976326844472,-70.1436463124613,
65.3215949165373));
#129158=CARTESIAN_POINT('Ctrl Pts',(-12.9659322363181,-69.8200770099199,
65.5373007093749));
#129159=CARTESIAN_POINT('Ctrl Pts',(-12.9613367010879,-69.6782317161318,
65.6377940024871));
#129160=CARTESIAN_POINT('Ctrl Pts',(-12.9474668712654,-69.2521331205604,
65.958296317252));
#129161=CARTESIAN_POINT('Ctrl Pts',(-12.9385186395591,-68.9776493854189,
66.1912805204721));
#129162=CARTESIAN_POINT('Ctrl Pts',(-12.9259108354926,-68.6162479933985,
66.5373953347773));
#129163=CARTESIAN_POINT('Ctrl Pts',(-12.9223398605986,-68.5167177393356,
66.6373160508213));
#129164=CARTESIAN_POINT('Ctrl Pts',(-12.9146492875739,-68.3105958471069,
66.8543448854849));
#129165=CARTESIAN_POINT('Ctrl Pts',(-12.9105158741154,-68.2046724252965,
66.9720243878612));
#129166=CARTESIAN_POINT('Ctrl Pts',(-12.8939773679671,-67.7983988832239,
67.4480995965967));
#129167=CARTESIAN_POINT('Ctrl Pts',(-12.8811892322323,-67.5226375585457,
67.8274973976122));
#129168=CARTESIAN_POINT('Ctrl Pts',(-12.8622215343773,-67.1566058114058,
68.4216312289478));
#129169=CARTESIAN_POINT('Ctrl Pts',(-12.8559830998545,-67.0432252457875,
68.6222022127429));
#129170=CARTESIAN_POINT('Ctrl Pts',(-12.8449495602273,-66.8538563952299,
68.9887312750473));
#129171=CARTESIAN_POINT('Ctrl Pts',(-12.8401238962256,-66.7749905455055,
69.1532203824882));
#129172=CARTESIAN_POINT('Ctrl Pts',(-12.8260882362863,-66.5565002368576,
69.6462360142252));
#129173=CARTESIAN_POINT('Ctrl Pts',(-12.8171900872545,-66.4310078991802,
69.9810141155976));
#129174=CARTESIAN_POINT('Ctrl Pts',(-12.8046090173476,-66.2840149886737,
70.4578371198973));
#129175=CARTESIAN_POINT('Ctrl Pts',(-12.8010077046728,-66.2453827957356,
70.5946070810551));
#129176=CARTESIAN_POINT('Ctrl Pts',(-12.7931083760621,-66.1690244194849,
70.8920803051291));
#129177=CARTESIAN_POINT('Ctrl Pts',(-12.7887950627577,-66.1324577536049,
71.0530276441246));
#129178=CARTESIAN_POINT('Ctrl Pts',(-12.7726402520091,-66.0135761571878,
71.6521427829917));
#129179=CARTESIAN_POINT('Ctrl Pts',(-12.7604785726686,-65.9593325993155,
72.0958671031451));
#129180=CARTESIAN_POINT('Ctrl Pts',(-12.7417813500953,-65.9257357403144,
72.7834136930754));
#129181=CARTESIAN_POINT('Ctrl Pts',(-12.7352087298558,-65.9235134175458,
73.0261761341576));
#129182=CARTESIAN_POINT('Ctrl Pts',(-12.7236478526681,-65.9366908056587,
73.4582749982496));
#129183=CARTESIAN_POINT('Ctrl Pts',(-12.7186260357509,-65.948357594045,
73.6477433913853));
#129184=CARTESIAN_POINT('Ctrl Pts',(-12.7049061682116,-65.9971259901677,
74.172634625439));
#129185=CARTESIAN_POINT('Ctrl Pts',(-12.6964671708652,-66.0469555065457,
74.5068642205268));
#129186=CARTESIAN_POINT('Ctrl Pts',(-12.6842565636745,-66.1452288670634,
74.9811030723674));
#129187=CARTESIAN_POINT('Ctrl Pts',(-12.6805358559911,-66.1785740163575,
75.1242414019398));
#129188=CARTESIAN_POINT('Ctrl Pts',(-12.6723915520485,-66.2581222352044,
75.4310215752946));
#129189=CARTESIAN_POINT('Ctrl Pts',(-12.6679518101771,-66.3055053509249,
75.5943144175234));
#129190=CARTESIAN_POINT('Ctrl Pts',(-12.6516212436858,-66.4944563271868,
76.1826445936466));
#129191=CARTESIAN_POINT('Ctrl Pts',(-12.6394187259343,-66.6633011130804,
76.5989086290332));
#129192=CARTESIAN_POINT('Ctrl Pts',(-12.6204973832283,-66.9719492483717,
77.2242291686741));
#129193=CARTESIAN_POINT('Ctrl Pts',(-12.6137457233882,-67.0914616914067,
77.4433682809365));
#129194=CARTESIAN_POINT('Ctrl Pts',(-12.6018724518322,-67.3199298894286,
77.8244732523635));
#129195=CARTESIAN_POINT('Ctrl Pts',(-12.5967164002634,-67.4255026661867,
77.9884898912608));
#129196=CARTESIAN_POINT('Ctrl Pts',(-12.5853460546946,-67.673796987118,
78.3483727903719));
#129197=CARTESIAN_POINT('Ctrl Pts',(-12.5792117016916,-67.8193138805894,
78.5423053192264));
#129198=CARTESIAN_POINT('Ctrl Pts',(-12.5683096863466,-68.0927037691992,
78.8776387789366));
#129199=CARTESIAN_POINT('Ctrl Pts',(-12.5635236220845,-68.217674991041,
79.0213866934708));
#129200=CARTESIAN_POINT('Ctrl Pts',(-12.5542317363497,-68.4651435564829,
79.2882454482999));
#129201=CARTESIAN_POINT('Ctrl Pts',(-12.5497357559432,-68.5866986269073,
79.4118384285661));
#129202=CARTESIAN_POINT('Ctrl Pts',(-12.5381251345081,-68.9054205928239,
79.7176821663174));
#129203=CARTESIAN_POINT('Ctrl Pts',(-12.5309312787889,-69.1075075161986,
79.8949000650061));
#129204=CARTESIAN_POINT('Ctrl Pts',(-12.5133411163695,-69.6159873837846,
80.302521491647));
#129205=CARTESIAN_POINT('Ctrl Pts',(-12.5028886133086,-69.9301047940802,
80.5233495686275));
#129206=CARTESIAN_POINT('Ctrl Pts',(-12.4860285719784,-70.464264540149,
80.8509991125645));
#129207=CARTESIAN_POINT('Ctrl Pts',(-12.4795352140262,-70.6768760668288,
80.970048415271));
#129208=CARTESIAN_POINT('Ctrl Pts',(-12.4684239451364,-71.0552045178678,
81.1624621476388));
#129209=CARTESIAN_POINT('Ctrl Pts',(-12.4637616215854,-71.2189555267709,
81.2397121151644));
#129210=CARTESIAN_POINT('Ctrl Pts',(-12.4512555091035,-71.6702335519829,
81.4363149037997));
#129211=CARTESIAN_POINT('Ctrl Pts',(-12.4434969476487,-71.9619996094954,
81.5459414268526));
#129212=CARTESIAN_POINT('Ctrl Pts',(-12.4308368744386,-72.432246629013,
81.6949422127961));
#129213=CARTESIAN_POINT('Ctrl Pts',(-12.4260886116885,-72.6074084118894,
81.7445741053388));
#129214=CARTESIAN_POINT('Ctrl Pts',(-12.4106932123179,-73.1730791994157,
81.8864772631894));
#129215=CARTESIAN_POINT('Ctrl Pts',(-12.3998302925292,-73.5687624449072,
81.9580731462943));
#129216=CARTESIAN_POINT('Ctrl Pts',(-12.3783768815432,-74.35582030368,82.0477162622559));
#129217=CARTESIAN_POINT('Ctrl Pts',(-12.3677869869934,-74.7471274668323,
82.0670978702825));
#129218=CARTESIAN_POINT('Ctrl Pts',(-12.3526344492061,-75.3200793364769,
82.0588030438593));
#129219=CARTESIAN_POINT('Ctrl Pts',(-12.347873911003,-75.5020586445725,
82.0507357538656));
#129220=CARTESIAN_POINT('Ctrl Pts',(-12.3356308365092,-75.9767837340445,
82.0153873268272));
#129221=CARTESIAN_POINT('Ctrl Pts',(-12.328282306456,-76.2688704651353,
81.9793459652047));
#129222=CARTESIAN_POINT('Ctrl Pts',(-12.3157260852563,-76.7563694762715,
81.8946079983548));
#129223=CARTESIAN_POINT('Ctrl Pts',(-12.3105740210083,-76.9524881347204,
81.8536303360942));
#129224=CARTESIAN_POINT('Ctrl Pts',(-12.2983032564264,-77.4081668153727,
81.7423142094984));
#129225=CARTESIAN_POINT('Ctrl Pts',(-12.2911459512972,-77.6661252285936,
81.6668766432329));
#129226=CARTESIAN_POINT('Ctrl Pts',(-12.2726493307792,-78.3173925485451,
81.4447294518154));
#129227=CARTESIAN_POINT('Ctrl Pts',(-12.2612227927062,-78.7052121629505,
81.2817875539456));
#129228=CARTESIAN_POINT('Ctrl Pts',(-12.2429374821052,-79.3132607670729,
80.9758038124274));
#129229=CARTESIAN_POINT('Ctrl Pts',(-12.2359833432898,-79.5414862948691,
80.8484830999955));
#129230=CARTESIAN_POINT('Ctrl Pts',(-12.2195299249525,-80.0775160531477,
80.5185476562888));
#129231=CARTESIAN_POINT('Ctrl Pts',(-12.2102794690912,-80.3794929708895,
80.3064921890982));
#129232=CARTESIAN_POINT('Ctrl Pts',(-12.1954914979162,-80.8350893803178,
79.9426080988649));
#129233=CARTESIAN_POINT('Ctrl Pts',(-12.1899920400428,-80.9974964776671,
79.802975437941));
#129234=CARTESIAN_POINT('Ctrl Pts',(-12.1770600988137,-81.3606739236908,
79.4672802425608));
#129235=CARTESIAN_POINT('Ctrl Pts',(-12.1695974691883,-81.5574135001567,
79.2675554631078));
#129236=CARTESIAN_POINT('Ctrl Pts',(-12.1507377520941,-82.0265282874472,
78.7452319839698));
#129237=CARTESIAN_POINT('Ctrl Pts',(-12.1392631758226,-82.2867251066204,
78.4116296283477));
#129238=CARTESIAN_POINT('Ctrl Pts',(-12.1208039387541,-82.6715879988969,
77.8412003225792));
#129239=CARTESIAN_POINT('Ctrl Pts',(-12.113725939776,-82.8108352065244,
77.6141165479128));
#129240=CARTESIAN_POINT('Ctrl Pts',(-12.0989816577469,-83.0847324128818,
77.1201990817444));
#129241=CARTESIAN_POINT('Ctrl Pts',(-12.0914137425593,-83.2167364123384,
76.8519027478229));
#129242=CARTESIAN_POINT('Ctrl Pts',(-12.0793375090851,-83.4057016154436,
76.4139386474057));
#129243=CARTESIAN_POINT('Ctrl Pts',(-12.0748081726496,-83.4714716736889,
76.2480793804726));
#129244=CARTESIAN_POINT('Ctrl Pts',(-12.0644662388748,-83.607794733024,
75.8714583153122));
#129245=CARTESIAN_POINT('Ctrl Pts',(-12.0586414508195,-83.6754985219537,
75.6600669295798));
#129246=CARTESIAN_POINT('Ctrl Pts',(-12.0390058468372,-83.8751177082579,
74.9476081985485));
#129247=CARTESIAN_POINT('Ctrl Pts',(-12.0249158600219,-83.9720370010646,
74.4366951858765));
#129248=CARTESIAN_POINT('Ctrl Pts',(-12.0026358185394,-84.0572776247063,
73.6122150928465));
#129249=CARTESIAN_POINT('Ctrl Pts',(-11.9943402672332,-84.0735397666877,
73.3014068899227));
#129250=CARTESIAN_POINT('Ctrl Pts',(-11.9773923867064,-84.0743154600487,
72.6534647140689));
#129251=CARTESIAN_POINT('Ctrl Pts',(-11.9688614612502,-84.0560248499278,
72.3163295312918));
#129252=CARTESIAN_POINT('Ctrl Pts',(-11.9541753138052,-83.9921224259184,
71.741263674071));
#129253=CARTESIAN_POINT('Ctrl Pts',(-11.9479953932471,-83.9558164733411,
71.503227393253));
#129254=CARTESIAN_POINT('Ctrl Pts',(-11.9254148566645,-83.7913493443104,
70.6560033933371));
#129255=CARTESIAN_POINT('Ctrl Pts',(-11.9085159411425,-83.6093857480237,
70.0578490970235));
#129256=CARTESIAN_POINT('Ctrl Pts',(-11.8826144802468,-83.2371879173642,
69.1690316337926));
#129257=CARTESIAN_POINT('Ctrl Pts',(-11.8734848276452,-83.0875724163114,
68.8611572423334));
#129258=CARTESIAN_POINT('Ctrl Pts',(-11.8566199967557,-82.7736413442767,
68.2979857932564));
#129259=CARTESIAN_POINT('Ctrl Pts',(-11.8489074740658,-82.6129107786165,
68.0406797197332));
#129260=CARTESIAN_POINT('Ctrl Pts',(-11.8361106588257,-82.324560748579,
67.6272750175843));
#129261=CARTESIAN_POINT('Ctrl Pts',(-11.8309916451167,-82.2042288866748,
67.4665816910673));
#129262=CARTESIAN_POINT('Ctrl Pts',(-11.818678293496,-81.9070784219599,
67.0966178448928));
#129263=CARTESIAN_POINT('Ctrl Pts',(-11.8114601160653,-81.7261893091633,
66.8914253334011));
#129264=CARTESIAN_POINT('Ctrl Pts',(-11.7908919240504,-81.190462082797,
66.3362918257294));
#129265=CARTESIAN_POINT('Ctrl Pts',(-11.777383867518,-80.8149659368627,
66.0061964107906));
#129266=CARTESIAN_POINT('Ctrl Pts',(-11.7577317786491,-80.225805379811,
65.567651078504));
#129267=CARTESIAN_POINT('Ctrl Pts',(-11.751449727912,-80.0308352533544,
65.4339001907069));
#129268=CARTESIAN_POINT('Ctrl Pts',(-11.739122124479,-79.6335188690206,
65.1834506279975));
#129269=CARTESIAN_POINT('Ctrl Pts',(-11.7330872672043,-79.4312820732563,
65.0665614617833));
#129270=CARTESIAN_POINT('Ctrl Pts',(-11.7218695882869,-79.0420503425554,
64.8613229085897));
#129271=CARTESIAN_POINT('Ctrl Pts',(-11.7166449615531,-78.8559849360608,
64.7712442010359));
#129272=CARTESIAN_POINT('Ctrl Pts',(-11.7051066279327,-78.4447421435435,
64.5895791838651));
#129273=CARTESIAN_POINT('Ctrl Pts',(-11.6987634650751,-78.2184774724938,
64.5005323416728));
#129274=CARTESIAN_POINT('Ctrl Pts',(-11.684810169018,-77.71919504776,64.3269414567394));
#129275=CARTESIAN_POINT('Ctrl Pts',(-11.6771735870387,-77.4449562289354,
64.24593787506));
#129276=CARTESIAN_POINT('Ctrl Pts',(-11.6529074994395,-76.5667248405637,
64.0306387496498));
#129277=CARTESIAN_POINT('Ctrl Pts',(-11.6361711939247,-75.9507792794544,
63.9442463551502));
#129278=CARTESIAN_POINT('Ctrl Pts',(-11.6138739515497,-75.0975870679637,
63.912031360932));
#129279=CARTESIAN_POINT('Ctrl Pts',(-11.6078398531792,-74.8622347970138,
63.9122696229956));
#129280=CARTESIAN_POINT('Ctrl Pts',(-11.5935419814758,-74.3013077601243,
63.9348828004118));
#129281=CARTESIAN_POINT('Ctrl Pts',(-11.5852325020868,-73.9777636940373,
63.9657446322328));
#129282=CARTESIAN_POINT('Ctrl Pts',(-11.5646853634814,-73.2027886852206,
64.0825572666288));
#129283=CARTESIAN_POINT('Ctrl Pts',(-11.5524082523738,-72.7552675906697,
64.1853590880314));
#129284=CARTESIAN_POINT('Ctrl Pts',(-11.5268837316571,-71.8468711198061,
64.4669025930135));
#129285=CARTESIAN_POINT('Ctrl Pts',(-11.5136349918919,-71.3874765934729,
64.650941098511));
#129286=CARTESIAN_POINT('Ctrl Pts',(-11.4937069948878,-70.7067134752823,
64.989997602512));
#129287=CARTESIAN_POINT('Ctrl Pts',(-11.4868272513075,-70.4726686597408,
65.1197169811987));
#129288=CARTESIAN_POINT('Ctrl Pts',(-11.4716339850267,-69.9651612665699,
65.4314252057549));
#129289=CARTESIAN_POINT('Ctrl Pts',(-11.4632440124045,-69.6963165277426,
65.617753987906));
#129290=CARTESIAN_POINT('Ctrl Pts',(-11.4470462594358,-69.2089929719968,
65.9965466507828));
#129291=CARTESIAN_POINT('Ctrl Pts',(-11.439347003723,-68.988918485167,66.1853004906013));
#129292=CARTESIAN_POINT('Ctrl Pts',(-11.4120393622787,-68.245668214213,
66.8867172062944));
#129293=CARTESIAN_POINT('Ctrl Pts',(-11.3922182362063,-67.7732597186835,
67.4536250804195));
#129294=CARTESIAN_POINT('Ctrl Pts',(-11.366936788712,-67.2452516347224,
68.2698493731437));
#129295=CARTESIAN_POINT('Ctrl Pts',(-11.3608163913894,-67.1230253326142,
68.4762992188587));
#129296=CARTESIAN_POINT('Ctrl Pts',(-11.3475668900671,-66.8772108415422,
68.932436411952));
#129297=CARTESIAN_POINT('Ctrl Pts',(-11.3403831528437,-66.7570892772954,
69.1829057883462));
#129298=CARTESIAN_POINT('Ctrl Pts',(-11.3248512505511,-66.5261303460856,
69.7276262003982));
#129299=CARTESIAN_POINT('Ctrl Pts',(-11.3164971605737,-66.4186286059857,
70.0232446326753));
#129300=CARTESIAN_POINT('Ctrl Pts',(-11.2896150174832,-66.1237919521111,
70.9855319451296));
#129301=CARTESIAN_POINT('Ctrl Pts',(-11.2709446351782,-65.9960640135589,
71.6707490856593));
#129302=CARTESIAN_POINT('Ctrl Pts',(-11.2460031258948,-65.9288496133152,
72.6251134699327));
#129303=CARTESIAN_POINT('Ctrl Pts',(-11.239241899148,-65.9218086926354,
72.8896632608712));
#129304=CARTESIAN_POINT('Ctrl Pts',(-11.2248477107533,-65.9318359002663,
73.4511502989318));
#129305=CARTESIAN_POINT('Ctrl Pts',(-11.2171422305074,-65.9520534110402,
73.7471976633819));
#129306=CARTESIAN_POINT('Ctrl Pts',(-11.1998417502573,-66.0289896609921,
74.4001777604379));
#129307=CARTESIAN_POINT('Ctrl Pts',(-11.1902105720864,-66.0928032406218,
74.75650596556));
#129308=CARTESIAN_POINT('Ctrl Pts',(-11.1637323086314,-66.3248103640701,
75.7200972951544));
#129309=CARTESIAN_POINT('Ctrl Pts',(-11.1468388232568,-66.5353946698986,
76.3173862305834));
#129310=CARTESIAN_POINT('Ctrl Pts',(-11.1230378117483,-66.9267660286225,
77.1425850466735));
#129311=CARTESIAN_POINT('Ctrl Pts',(-11.1158001611499,-67.0602709151533,
77.393018191316));
#129312=CARTESIAN_POINT('Ctrl Pts',(-11.0991110754866,-67.3922405884766,
77.9498465268579));
#129313=CARTESIAN_POINT('Ctrl Pts',(-11.0895530133271,-67.5982301647372,
78.2514307931786));
#129314=CARTESIAN_POINT('Ctrl Pts',(-11.0665262427273,-68.1312114054166,
78.939176623819));
#129315=CARTESIAN_POINT('Ctrl Pts',(-11.0529699195005,-68.4743874713834,
79.3130933754959));
#129316=CARTESIAN_POINT('Ctrl Pts',(-11.0282535705372,-69.1560840092167,
79.9427746266769));
#129317=CARTESIAN_POINT('Ctrl Pts',(-11.0170659596609,-69.4861319311373,
80.2079374301951));
#129318=CARTESIAN_POINT('Ctrl Pts',(-10.9983567631792,-70.07719144732,80.6182380424736));
#129319=CARTESIAN_POINT('Ctrl Pts',(-10.9907753226796,-70.3298606857768,
80.7757836916518));
#129320=CARTESIAN_POINT('Ctrl Pts',(-10.9694617859358,-71.0487938222381,
81.1751307786503));
#129321=CARTESIAN_POINT('Ctrl Pts',(-10.9555724402751,-71.5294163569786,
81.3892160763062));
#129322=CARTESIAN_POINT('Ctrl Pts',(-10.9218765541441,-72.7253853419579,
81.8034386875353));
#129323=CARTESIAN_POINT('Ctrl Pts',(-10.9020080574071,-73.4557989655504,
81.961124441332));
#129324=CARTESIAN_POINT('Ctrl Pts',(-10.8750202645403,-74.4901964527539,
82.0543517725009));
#129325=CARTESIAN_POINT('Ctrl Pts',(-10.8674301257071,-74.7871980771689,
82.0663737775191));
#129326=CARTESIAN_POINT('Ctrl Pts',(-10.843232576932,-75.7176036781963,
82.0571381219942));
#129327=CARTESIAN_POINT('Ctrl Pts',(-10.8264023611081,-76.3492646983437,
81.983744053942));
#129328=CARTESIAN_POINT('Ctrl Pts',(-10.7939437530567,-77.5398607522838,
81.719188310539));
#129329=CARTESIAN_POINT('Ctrl Pts',(-10.7783170880428,-78.1010200303309,
81.5367601632063));
#129330=CARTESIAN_POINT('Ctrl Pts',(-10.7542234072266,-78.9481683680525,
81.1669141646729));
#129331=CARTESIAN_POINT('Ctrl Pts',(-10.7455985843692,-79.2490240312718,
81.0149469874758));
#129332=CARTESIAN_POINT('Ctrl Pts',(-10.7252961957682,-79.9229130642142,
80.6247931408589));
#129333=CARTESIAN_POINT('Ctrl Pts',(-10.7136535989653,-80.2878531273247,
80.3759504681903));
#129334=CARTESIAN_POINT('Ctrl Pts',(-10.6866596950859,-81.0849277124096,
79.7438003105246));
#129335=CARTESIAN_POINT('Ctrl Pts',(-10.6712728449618,-81.5030910693985,
79.3425840826091));
#129336=CARTESIAN_POINT('Ctrl Pts',(-10.640264473015,-82.2714169121863,
78.4511433781504));
#129337=CARTESIAN_POINT('Ctrl Pts',(-10.6249089475234,-82.6170020718191,
77.9593174230282));
#129338=CARTESIAN_POINT('Ctrl Pts',(-10.5943269453012,-83.1875127282136,
76.9413325641774));
#129339=CARTESIAN_POINT('Ctrl Pts',(-10.5793594704117,-83.4169537126725,
76.42375256271));
#129340=CARTESIAN_POINT('Ctrl Pts',(-10.5486920919653,-83.7864617386823,
75.32866985789));
#129341=CARTESIAN_POINT('Ctrl Pts',(-10.5329917514054,-83.9215192221644,
74.7492098724526));
#129342=CARTESIAN_POINT('Ctrl Pts',(-10.5064524109376,-84.0539207745023,
73.7405954091737));
#129343=CARTESIAN_POINT('Ctrl Pts',(-10.4955303508667,-84.078894120976,
73.3178579165979));
#129344=CARTESIAN_POINT('Ctrl Pts',(-10.4655678147656,-84.0657291154148,
72.1769734891154));
#129345=CARTESIAN_POINT('Ctrl Pts',(-10.4464935053981,-83.9721818897685,
71.4609994507493));
#129346=CARTESIAN_POINT('Ctrl Pts',(-10.3959152218326,-83.5050413124618,
69.6067577364375));
#129347=CARTESIAN_POINT('Ctrl Pts',(-10.3655684986034,-82.9909991768275,
68.5274137916928));
#129348=CARTESIAN_POINT('Ctrl Pts',(-10.3184357299047,-81.9259658131339,
67.0981133706526));
#129349=CARTESIAN_POINT('Ctrl Pts',(-10.3027988491642,-81.5278160566466,
66.6590415619498));
#129350=CARTESIAN_POINT('Ctrl Pts',(-10.2630955556355,-80.4101039975176,
65.644636052641));
#129351=CARTESIAN_POINT('Ctrl Pts',(-10.2394869280064,-79.6434187528559,
65.1397751598418));
#129352=CARTESIAN_POINT('Ctrl Pts',(-10.1997971790316,-78.2789760985098,
64.5083161720554));
#129353=CARTESIAN_POINT('Ctrl Pts',(-10.1841445272966,-77.7180805394768,
64.3118157166981));
#129354=CARTESIAN_POINT('Ctrl Pts',(-10.1531620117269,-76.5749408104176,
64.0325708395138));
#129355=CARTESIAN_POINT('Ctrl Pts',(-10.1380002434501,-75.9966210051096,
63.9495786207854));
#129356=CARTESIAN_POINT('Ctrl Pts',(-10.0920399907937,-74.2484621824054,
63.8722749150175));
#129357=CARTESIAN_POINT('Ctrl Pts',(-10.061200132307,-73.0759366879517,
64.0451649366301));
#129358=CARTESIAN_POINT('Ctrl Pts',(-10.0230977550266,-71.7072452821346,
64.5273486670839));
#129359=CARTESIAN_POINT('Ctrl Pts',(-10.0155852308537,-71.4413011270864,
64.6358162931003));
#129360=CARTESIAN_POINT('Ctrl Pts',(-9.98249427654821,-70.2985321732764,
65.1673203799454));
#129361=CARTESIAN_POINT('Ctrl Pts',(-9.95683561054873,-69.482851806251,
65.7207502006352));
#129362=CARTESIAN_POINT('Ctrl Pts',(-9.90543200422985,-68.0615733940599,
67.0581188366673));
#129363=CARTESIAN_POINT('Ctrl Pts',(-9.88009613193941,-67.4686921055001,
67.8345464024768));
#129364=CARTESIAN_POINT('Ctrl Pts',(-9.85451228705275,-67.0084263223619,
68.6918085046015));
#129365=CARTESIAN_POINT('Ctrl Pts',(-13.5675364833309,-82.8095169451273,
77.459392053019));
#129366=CARTESIAN_POINT('Ctrl Pts',(-13.5675364833309,-82.9556776154695,
77.2295778420848));
#129367=CARTESIAN_POINT('Ctrl Pts',(-13.5675364833312,-83.0914974938587,
76.9931764216597));
#129368=CARTESIAN_POINT('Ctrl Pts',(-13.5675364833312,-83.3420981768321,
76.5073540267254));
#129369=CARTESIAN_POINT('Ctrl Pts',(-13.5675364833309,-83.456720060448,
76.2578575306141));
#129370=CARTESIAN_POINT('Ctrl Pts',(-13.5675364833309,-83.5595902541753,
76.0035856352372));
#129371=CARTESIAN_POINT('Ctrl Pts',(-13.4857787351652,-83.53086080835,69.194683933252));
#129372=CARTESIAN_POINT('Ctrl Pts',(-13.4107459268847,-82.33835458422,66.513462598172));
#129373=CARTESIAN_POINT('Ctrl Pts',(-13.2981967144638,-78.53320802489,63.458709829566));
#129374=CARTESIAN_POINT('Ctrl Pts',(-13.1481310979025,-72.48811911993,63.63322643035));
#129375=CARTESIAN_POINT('Ctrl Pts',(-13.0355818854816,-68.51429278678,65.790797832361));
#129376=CARTESIAN_POINT('Ctrl Pts',(-12.9230326730606,-65.95227475056,69.522686716285));
#129377=CARTESIAN_POINT('Ctrl Pts',(-12.8104834606397,-65.36509547432,74.009771845382));
#129378=CARTESIAN_POINT('Ctrl Pts',(-12.6979342482187,-66.87977327092,78.274405364341));
#129379=CARTESIAN_POINT('Ctrl Pts',(-12.5853850357977,-70.16613638824,81.385801227635));
#129380=CARTESIAN_POINT('Ctrl Pts',(-12.4728358233767,-74.50710712086,82.665227893767));
#129381=CARTESIAN_POINT('Ctrl Pts',(-12.3602866109556,-78.95561877133,81.83352216413));
#129382=CARTESIAN_POINT('Ctrl Pts',(-12.2477373985346,-82.54111542822,79.072147533527));
#129383=CARTESIAN_POINT('Ctrl Pts',(-12.1351881861136,-84.48133587032,74.983562774911));
#129384=CARTESIAN_POINT('Ctrl Pts',(-12.0226389736926,-84.35297372718,70.459791926131));
#129385=CARTESIAN_POINT('Ctrl Pts',(-11.9100897612715,-82.18403440969,66.487804766612));
#129386=CARTESIAN_POINT('Ctrl Pts',(-11.7975405488505,-78.44772440513,63.934186298037));
#129387=CARTESIAN_POINT('Ctrl Pts',(-11.6849913364294,-73.95921002211,63.356070078148));
#129388=CARTESIAN_POINT('Ctrl Pts',(-11.5724421240084,-69.69776911955,64.879586131319));
#129389=CARTESIAN_POINT('Ctrl Pts',(-11.4598929115869,-66.59313798963,68.172342617968));
#129390=CARTESIAN_POINT('Ctrl Pts',(-11.3473436991659,-65.32266693424,72.5159451614496));
#129391=CARTESIAN_POINT('Ctrl Pts',(-11.2347944867449,-66.16353987442,76.962731892397));
#129392=CARTESIAN_POINT('Ctrl Pts',(-11.1222452743239,-68.93230019525,80.542528950631));
#129393=CARTESIAN_POINT('Ctrl Pts',(-11.0096960619029,-73.02487543835,82.474316725385));
#129394=CARTESIAN_POINT('Ctrl Pts',(-10.8971468494819,-77.5483732915,82.336630496769));
#129395=CARTESIAN_POINT('Ctrl Pts',(-10.7845976370609,-81.5158764696,80.159504403197));
#129396=CARTESIAN_POINT('Ctrl Pts',(-10.6720484246399,-84.06180417873,76.417951402524));
#129397=CARTESIAN_POINT('Ctrl Pts',(-10.5594992122189,-84.63060417684,71.928205926366));
#129398=CARTESIAN_POINT('Ctrl Pts',(-10.4469499997979,-83.09853951678,67.670097151854));
#129399=CARTESIAN_POINT('Ctrl Pts',(-10.3344007873769,-79.79852165914,64.571579248221));
#129400=CARTESIAN_POINT('Ctrl Pts',(-10.2218515749559,-75.45555056223,63.312606598678));
#129401=CARTESIAN_POINT('Ctrl Pts',(-10.0717859583949,-69.51269706816,64.433342187813));
#129402=CARTESIAN_POINT('Ctrl Pts',(-9.95923674597391,-66.44785978885,68.230370929682));
#129403=CARTESIAN_POINT('Ctrl Pts',(-9.88420393769391,-65.8555809379,71.104431594487));
#129404=CARTESIAN_POINT('Ctrl Pts',(-13.7163617470419,-83.16594445251,69.356984978657));
#129405=CARTESIAN_POINT('Ctrl Pts',(-13.6413289387609,-82.02444891012,66.790455647208));
#129406=CARTESIAN_POINT('Ctrl Pts',(-13.5287797263401,-78.38207141327,63.866373073948));
#129407=CARTESIAN_POINT('Ctrl Pts',(-13.3787141097789,-72.59556741124,64.033424547414));
#129408=CARTESIAN_POINT('Ctrl Pts',(-13.2661648973579,-68.79172559158,66.09870361091));
#129409=CARTESIAN_POINT('Ctrl Pts',(-13.153615684937,-66.33930051512,69.670957104856));
#129410=CARTESIAN_POINT('Ctrl Pts',(-13.041066472516,-65.77723843707,73.9661025469177));
#129411=CARTESIAN_POINT('Ctrl Pts',(-12.928517260095,-67.22712433115,78.048311975543));
#129412=CARTESIAN_POINT('Ctrl Pts',(-12.815968047674,-70.37290988194,81.026614676792));
#129413=CARTESIAN_POINT('Ctrl Pts',(-12.703418835253,-74.5281911213,82.251312549785));
#129414=CARTESIAN_POINT('Ctrl Pts',(-12.590869622832,-78.78641310501,81.455183889208));
#129415=CARTESIAN_POINT('Ctrl Pts',(-12.478320410411,-82.2185364502,78.811929902003));
#129416=CARTESIAN_POINT('Ctrl Pts',(-12.3657711979899,-84.07576196493,74.898238566719));
#129417=CARTESIAN_POINT('Ctrl Pts',(-12.2532219855689,-83.95289064466,70.567976674408));
#129418=CARTESIAN_POINT('Ctrl Pts',(-12.1406727731479,-81.87672993999,66.765895355835));
#129419=CARTESIAN_POINT('Ctrl Pts',(-12.0281235607268,-78.3002444434,64.321510546861));
#129420=CARTESIAN_POINT('Ctrl Pts',(-11.9155743483058,-74.00373088522,63.768123843582));
#129421=CARTESIAN_POINT('Ctrl Pts',(-11.8030251358847,-69.92457750553,65.2264699287));
#129422=CARTESIAN_POINT('Ctrl Pts',(-11.6904759234637,-66.95275016922,68.378375365861));
#129423=CARTESIAN_POINT('Ctrl Pts',(-11.5779267110427,-65.73662482149,72.5361758376591));
#129424=CARTESIAN_POINT('Ctrl Pts',(-11.4653774986219,-66.54152855574,76.792746687058));
#129425=CARTESIAN_POINT('Ctrl Pts',(-11.3528282862009,-69.19185230266,80.219414239796));
#129426=CARTESIAN_POINT('Ctrl Pts',(-11.2402790737799,-73.10936342534,82.068567803219));
#129427=CARTESIAN_POINT('Ctrl Pts',(-11.1277298613589,-77.4393639997,81.936771244834));
#129428=CARTESIAN_POINT('Ctrl Pts',(-11.0151806489379,-81.23715314378,79.852773961851));
#129429=CARTESIAN_POINT('Ctrl Pts',(-10.9026314365169,-83.67417617347,76.271269743701));
#129430=CARTESIAN_POINT('Ctrl Pts',(-10.7900822240959,-84.21864516594,71.973577753657));
#129431=CARTESIAN_POINT('Ctrl Pts',(-10.6775330116749,-82.75211614938,67.89761396681));
#129432=CARTESIAN_POINT('Ctrl Pts',(-10.5649837992539,-79.59325995385,64.931638357232));
#129433=CARTESIAN_POINT('Ctrl Pts',(-10.4524345868329,-75.43606391784,63.726519559207));
#129434=CARTESIAN_POINT('Ctrl Pts',(-10.3023689702719,-69.7474221017,64.799314529419));
#129435=CARTESIAN_POINT('Ctrl Pts',(-10.1898197578509,-66.81368639306,68.433921456821));
#129436=CARTESIAN_POINT('Ctrl Pts',(-10.1147869495699,-66.24674287986,71.185041217093));
#129437=CARTESIAN_POINT('Ctrl Pts',(-13.9469447589179,-82.80102809666,69.519286024043));
#129438=CARTESIAN_POINT('Ctrl Pts',(-13.8719119506369,-81.710543236,67.067448696223));
#129439=CARTESIAN_POINT('Ctrl Pts',(-13.7593627382169,-78.23093480162,64.274036318316));
#129440=CARTESIAN_POINT('Ctrl Pts',(-13.6092971216549,-72.7030157025,64.433622664488));
#129441=CARTESIAN_POINT('Ctrl Pts',(-13.4967479092343,-69.06915839634,66.406609389489));
#129442=CARTESIAN_POINT('Ctrl Pts',(-13.3841986968133,-66.72632627966,69.819227493478));
#129443=CARTESIAN_POINT('Ctrl Pts',(-13.2716494843923,-66.18938139983,73.9224332485153));
#129444=CARTESIAN_POINT('Ctrl Pts',(-13.1591002719714,-67.57447539142,77.822218586803));
#129445=CARTESIAN_POINT('Ctrl Pts',(-13.0465510595504,-70.57968337571,80.667428125987));
#129446=CARTESIAN_POINT('Ctrl Pts',(-12.9340018471294,-74.54927512182,81.837397205809));
#129447=CARTESIAN_POINT('Ctrl Pts',(-12.8214526347083,-78.61720743877,81.076845614251));
#129448=CARTESIAN_POINT('Ctrl Pts',(-12.7089034222873,-81.89595747223,78.551712270408));
#129449=CARTESIAN_POINT('Ctrl Pts',(-12.5963542098663,-83.67018805956,74.81291435843));
#129450=CARTESIAN_POINT('Ctrl Pts',(-12.4838049974453,-83.55280756212,70.676161422585));
#129451=CARTESIAN_POINT('Ctrl Pts',(-12.3712557850242,-81.56942547021,67.043985944979));
#129452=CARTESIAN_POINT('Ctrl Pts',(-12.2587065726032,-78.15276448156,64.708834795646));
#129453=CARTESIAN_POINT('Ctrl Pts',(-12.1461573601821,-74.04825174822,64.180177609028));
#129454=CARTESIAN_POINT('Ctrl Pts',(-12.0336081477611,-70.15138589142,65.573353726144));
#129455=CARTESIAN_POINT('Ctrl Pts',(-11.92105893534,-67.31236234875,68.584408113854));
#129456=CARTESIAN_POINT('Ctrl Pts',(-11.808509722919,-66.15058270873,72.5564065139834));
#129457=CARTESIAN_POINT('Ctrl Pts',(-11.695960510498,-66.9195172371,76.622761481822));
#129458=CARTESIAN_POINT('Ctrl Pts',(-11.5834112980769,-69.45140441015,79.89629952903));
#129459=CARTESIAN_POINT('Ctrl Pts',(-11.4708620856559,-73.19385141245,81.662818881074));
#129460=CARTESIAN_POINT('Ctrl Pts',(-11.3583128732349,-77.330354708,81.53691199287));
#129461=CARTESIAN_POINT('Ctrl Pts',(-11.2457636608139,-80.95842981803,79.54604352044));
#129462=CARTESIAN_POINT('Ctrl Pts',(-11.1332144483929,-83.28654816823,76.124588084794));
#129463=CARTESIAN_POINT('Ctrl Pts',(-11.0206652359719,-83.80668615503,72.0189495808697));
#129464=CARTESIAN_POINT('Ctrl Pts',(-10.9081160235509,-82.40569278195,68.125130781709));
#129465=CARTESIAN_POINT('Ctrl Pts',(-10.7955668111299,-79.38799824851,65.291697466218));
#129466=CARTESIAN_POINT('Ctrl Pts',(-10.6830175987089,-75.4165772734,64.140432519737));
#129467=CARTESIAN_POINT('Ctrl Pts',(-10.5329519821479,-69.98214713522,65.165286871043));
#129468=CARTESIAN_POINT('Ctrl Pts',(-10.4204027697269,-67.17951299727,68.637471983962));
#129469=CARTESIAN_POINT('Ctrl Pts',(-10.3453699614459,-66.63790482183,71.265650839687));
#129470=CARTESIAN_POINT('Ctrl Pts',(-14.1775277707939,-82.43611174083,69.681587069447));
#129471=CARTESIAN_POINT('Ctrl Pts',(-14.1024949625139,-81.3966375619,67.344441745258));
#129472=CARTESIAN_POINT('Ctrl Pts',(-13.9899457500929,-78.07979819,64.681699562697));
#129473=CARTESIAN_POINT('Ctrl Pts',(-13.8398801335319,-72.8104639938,64.833820781552));
#129474=CARTESIAN_POINT('Ctrl Pts',(-13.7273309211109,-69.34659120114,66.714515168039));
#129475=CARTESIAN_POINT('Ctrl Pts',(-13.6147817086899,-67.11335204423,69.967497882051));
#129476=CARTESIAN_POINT('Ctrl Pts',(-13.5022324962687,-66.60152436258,73.878763950054));
#129477=CARTESIAN_POINT('Ctrl Pts',(-13.3896832838477,-67.92182645165,77.596125198008));
#129478=CARTESIAN_POINT('Ctrl Pts',(-13.2771340714267,-70.78645686942,80.308241575145));
#129479=CARTESIAN_POINT('Ctrl Pts',(-13.1645848590057,-74.57035912226,81.423481861828));
#129480=CARTESIAN_POINT('Ctrl Pts',(-13.0520356465847,-78.44800177245,80.698507339327));
#129481=CARTESIAN_POINT('Ctrl Pts',(-12.9394864341637,-81.57337849421,78.29149463888));
#129482=CARTESIAN_POINT('Ctrl Pts',(-12.8269372217426,-83.26461415418,74.727590150234));
#129483=CARTESIAN_POINT('Ctrl Pts',(-12.7143880093216,-83.1527244796,70.784346170858));
#129484=CARTESIAN_POINT('Ctrl Pts',(-12.6018387969006,-81.26212100051,67.322076534199));
#129485=CARTESIAN_POINT('Ctrl Pts',(-12.4892895844795,-78.00528451983,65.096159044468));
#129486=CARTESIAN_POINT('Ctrl Pts',(-12.3767403720585,-74.09277261133,64.592231374463));
#129487=CARTESIAN_POINT('Ctrl Pts',(-12.2641911596374,-70.37819427741,65.920237523529));
#129488=CARTESIAN_POINT('Ctrl Pts',(-12.1516419472164,-67.67197452834,68.790440861752));
#129489=CARTESIAN_POINT('Ctrl Pts',(-12.0390927347954,-66.56454059598,72.5766371901983));
#129490=CARTESIAN_POINT('Ctrl Pts',(-11.9265435223743,-67.29750591841,76.452776276488));
#129491=CARTESIAN_POINT('Ctrl Pts',(-11.8139943099533,-69.71095651757,79.573184818198));
#129492=CARTESIAN_POINT('Ctrl Pts',(-11.7014450975323,-73.27833939945,81.257069958908));
#129493=CARTESIAN_POINT('Ctrl Pts',(-11.5888958851112,-77.22134541621,81.137052740933));
#129494=CARTESIAN_POINT('Ctrl Pts',(-11.4763466726899,-80.67970649221,79.239313079091));
#129495=CARTESIAN_POINT('Ctrl Pts',(-11.3637974602689,-82.89892016296,75.977906425967));
#129496=CARTESIAN_POINT('Ctrl Pts',(-11.2512482478479,-83.39472714413,72.0643214081572));
#129497=CARTESIAN_POINT('Ctrl Pts',(-11.1386990354269,-82.05926941456,68.352647596662));
#129498=CARTESIAN_POINT('Ctrl Pts',(-11.0261498230059,-79.18273654321,65.651756575228));
#129499=CARTESIAN_POINT('Ctrl Pts',(-10.9136006105849,-75.39709062901,64.554345480267));
#129500=CARTESIAN_POINT('Ctrl Pts',(-10.7635349940239,-70.21687216876,65.53125921265));
#129501=CARTESIAN_POINT('Ctrl Pts',(-10.6509857816029,-67.54533960148,68.841022511101));
#129502=CARTESIAN_POINT('Ctrl Pts',(-10.5759529733229,-67.02906676379,71.346260462292));
#129503=CARTESIAN_POINT('',(-13.563311219297,-81.8872991846617,67.092553089091));
#129504=CARTESIAN_POINT('Ctrl Pts',(-13.559085955263,-81.8925473588303,
67.087485454259));
#129505=CARTESIAN_POINT('Ctrl Pts',(-13.5557378489868,-81.8226484187543,
67.0056955122904));
#129506=CARTESIAN_POINT('Ctrl Pts',(-13.5524040041999,-81.7513035648403,
66.9251397154799));
#129507=CARTESIAN_POINT('Ctrl Pts',(-13.5407945360191,-81.4958535332512,
66.6468193919849));
#129508=CARTESIAN_POINT('Ctrl Pts',(-13.5326654402662,-81.3042813848844,
66.4559020117066));
#129509=CARTESIAN_POINT('Ctrl Pts',(-13.5216044230679,-81.0190668043286,
66.1963000811713));
#129510=CARTESIAN_POINT('Ctrl Pts',(-13.5183611378651,-80.932138867054,
66.1202002131299));
#129511=CARTESIAN_POINT('Ctrl Pts',(-13.5133368922477,-80.7915755236166,
66.0019193088781));
#129512=CARTESIAN_POINT('Ctrl Pts',(-13.5115026272737,-80.7389583800737,
65.9586663606433));
#129513=CARTESIAN_POINT('Ctrl Pts',(-13.5079429779001,-80.634394306066,
65.8746963206787));
#129514=CARTESIAN_POINT('Ctrl Pts',(-13.5062160018049,-80.5824778523595,
65.8339426977273));
#129515=CARTESIAN_POINT('Ctrl Pts',(-13.5021175780405,-80.4565479340235,
65.7373147660614));
#129516=CARTESIAN_POINT('Ctrl Pts',(-13.4997684762369,-80.3821031546346,
65.6820031944673));
#129517=CARTESIAN_POINT('Ctrl Pts',(-13.4917599280967,-80.1210357304505,
65.4942033786579));
#129518=CARTESIAN_POINT('Ctrl Pts',(-13.4863033905747,-79.9301647455721,
65.3676160031791));
#129519=CARTESIAN_POINT('Ctrl Pts',(-13.4630988413414,-79.0746195119488,
64.8454007412283));
#129520=CARTESIAN_POINT('Ctrl Pts',(-13.446939288299,-78.3629248291164,
64.5261308523007));
#129521=CARTESIAN_POINT('Ctrl Pts',(-13.4209340605883,-77.2639858617722,
64.1930428150856));
#129522=CARTESIAN_POINT('Ctrl Pts',(-13.4120849370132,-76.8984839701938,
64.1065784692331));
#129523=CARTESIAN_POINT('Ctrl Pts',(-13.3969918678252,-76.2964750450373,
64.0041304265887));
#129524=CARTESIAN_POINT('Ctrl Pts',(-13.3910705329244,-76.0640729471427,
63.9739159071207));
#129525=CARTESIAN_POINT('Ctrl Pts',(-13.3785301259652,-75.5780202632669,
63.9297652567008));
#129526=CARTESIAN_POINT('Ctrl Pts',(-13.3718943919218,-75.3242247504548,
63.9174109355893));
#129527=CARTESIAN_POINT('Ctrl Pts',(-13.3434831198087,-74.2489047375888,
63.9097876203767));
#129528=CARTESIAN_POINT('Ctrl Pts',(-13.3210969350338,-73.4262833985882,
64.0144787652504));
#129529=CARTESIAN_POINT('Ctrl Pts',(-13.2926222433935,-72.4136094699141,
64.2872776090376));
#129530=CARTESIAN_POINT('Ctrl Pts',(-13.2864879360885,-72.196911524819,
64.3546050530603));
#129531=CARTESIAN_POINT('Ctrl Pts',(-13.2630150838093,-71.3647346241283,
64.6485723429744));
#129532=CARTESIAN_POINT('Ctrl Pts',(-13.2462305930131,-70.7711117695441,
64.9345765112858));
#129533=CARTESIAN_POINT('Ctrl Pts',(-13.2210144551986,-69.9428478544483,
65.4487924270168));
#129534=CARTESIAN_POINT('Ctrl Pts',(-13.2127031844204,-69.6798945229241,
65.6317243516277));
#129535=CARTESIAN_POINT('Ctrl Pts',(-13.1966424718445,-69.1982179606711,
66.0058185752753));
#129536=CARTESIAN_POINT('Ctrl Pts',(-13.1888955316257,-68.9776420069283,
66.1946330030121));
#129537=CARTESIAN_POINT('Ctrl Pts',(-13.1773764931447,-68.6676876440164,
66.4870709710263));
#129538=CARTESIAN_POINT('Ctrl Pts',(-13.1736883415841,-68.5708050822243,
66.5827289685801));
#129539=CARTESIAN_POINT('Ctrl Pts',(-13.1634531773245,-68.3063476211814,
66.8561035446628));
#129540=CARTESIAN_POINT('Ctrl Pts',(-13.1569968246614,-68.1440755051959,
67.0383552906632));
#129541=CARTESIAN_POINT('Ctrl Pts',(-13.1366314630471,-67.6506569957674,
67.6398730643821));
#129542=CARTESIAN_POINT('Ctrl Pts',(-13.1229846344129,-67.3484668753696,
68.0831733061487));
#129543=CARTESIAN_POINT('Ctrl Pts',(-13.1026671090003,-66.9635998900805,
68.7692394324011));
#129544=CARTESIAN_POINT('Ctrl Pts',(-13.0961153737121,-66.8492400866051,
68.9943566288763));
#129545=CARTESIAN_POINT('Ctrl Pts',(-13.083431494371,-66.6488881705089,
69.4327296147196));
#129546=CARTESIAN_POINT('Ctrl Pts',(-13.0773086994625,-66.5612676714018,
69.6452604753881));
#129547=CARTESIAN_POINT('Ctrl Pts',(-13.0645429528433,-66.3982345792593,
70.0877189116747));
#129548=CARTESIAN_POINT('Ctrl Pts',(-13.0579148759919,-66.3237102061575,
70.3179694825108));
#129549=CARTESIAN_POINT('Ctrl Pts',(-13.0463406873125,-66.2085000486793,
70.7304437977745));
#129550=CARTESIAN_POINT('Ctrl Pts',(-13.0413850099358,-66.1641151190626,
70.9111354100525));
#129551=CARTESIAN_POINT('Ctrl Pts',(-13.0288741208045,-66.0650095113933,
71.3767387413974));
#129552=CARTESIAN_POINT('Ctrl Pts',(-13.0214032712663,-66.0184056734035,
71.6632455841991));
#129553=CARTESIAN_POINT('Ctrl Pts',(-13.0051273905784,-65.9464198857517,
72.2944176611577));
#129554=CARTESIAN_POINT('Ctrl Pts',(-12.9963384395356,-65.9267882999154,
72.6397606252193));
#129555=CARTESIAN_POINT('Ctrl Pts',(-12.9813320943859,-65.9265458581992,
73.2211658979305));
#129556=CARTESIAN_POINT('Ctrl Pts',(-12.9751799741108,-65.9355563574263,
73.4572664963566));
#129557=CARTESIAN_POINT('Ctrl Pts',(-12.9597906409308,-65.9800744166607,
74.0355245727726));
#129558=CARTESIAN_POINT('Ctrl Pts',(-12.9503423706044,-66.0258024785281,
74.376894732432));
#129559=CARTESIAN_POINT('Ctrl Pts',(-12.936706483897,-66.1201634042575,
74.8664653571157));
#129560=CARTESIAN_POINT('Ctrl Pts',(-12.9324897465908,-66.1533623899488,
75.017630596075));
#129561=CARTESIAN_POINT('Ctrl Pts',(-12.9242274807111,-66.2270688729963,
75.3158989494287));
#129562=CARTESIAN_POINT('Ctrl Pts',(-12.9201940123229,-66.2674172210885,
75.4627941290223));
#129563=CARTESIAN_POINT('Ctrl Pts',(-12.9056351533373,-66.4284273094106,
75.9954678935174));
#129564=CARTESIAN_POINT('Ctrl Pts',(-12.8953959509123,-66.5715638217598,
76.3744766954144));
#129565=CARTESIAN_POINT('Ctrl Pts',(-12.8791747875566,-66.8360786683099,
76.9553847514503));
#129566=CARTESIAN_POINT('Ctrl Pts',(-12.8732144367455,-66.9412535465598,
77.164683710942));
#129567=CARTESIAN_POINT('Ctrl Pts',(-12.862496332028,-67.1416748123932,
77.5281895284742));
#129568=CARTESIAN_POINT('Ctrl Pts',(-12.8577716964445,-67.2337792288395,
77.6841463237772));
#129569=CARTESIAN_POINT('Ctrl Pts',(-12.8426574301479,-67.5377368105897,
78.1656496446993));
#129570=CARTESIAN_POINT('Ctrl Pts',(-12.8319026905027,-67.7659395902239,
78.480884158594));
#129571=CARTESIAN_POINT('Ctrl Pts',(-12.8172087319959,-68.1082589586898,
78.8946606387161));
#129572=CARTESIAN_POINT('Ctrl Pts',(-12.813161188698,-68.2058592810763,
79.0068609964641));
#129573=CARTESIAN_POINT('Ctrl Pts',(-12.8054836864172,-68.3987426811209,
79.2177078607287));
#129574=CARTESIAN_POINT('Ctrl Pts',(-12.8018591577577,-68.4934297980403,
79.3165212196181));
#129575=CARTESIAN_POINT('Ctrl Pts',(-12.7924877187558,-68.7473583304201,
79.5695965652197));
#129576=CARTESIAN_POINT('Ctrl Pts',(-12.7868132265313,-68.9100914481405,
79.7201525763961));
#129577=CARTESIAN_POINT('Ctrl Pts',(-12.7731297896651,-69.3184822447202,
80.0711096023261));
#129578=CARTESIAN_POINT('Ctrl Pts',(-12.7651667228754,-69.569679986819,
80.2650684300452));
#129579=CARTESIAN_POINT('Ctrl Pts',(-12.7519826161154,-69.9944066093667,
80.5592161990268));
#129580=CARTESIAN_POINT('Ctrl Pts',(-12.7468362248654,-70.1623146785122,
80.6675635282834));
#129581=CARTESIAN_POINT('Ctrl Pts',(-12.7377107898938,-70.4601528412897,
80.8462648526309));
#129582=CARTESIAN_POINT('Ctrl Pts',(-12.7337704010071,-70.5885659943192,
80.9191581331012));
#129583=CARTESIAN_POINT('Ctrl Pts',(-12.7205899472585,-71.0185155206958,
81.1496543168899));
#129584=CARTESIAN_POINT('Ctrl Pts',(-12.7111645111972,-71.3273400643339,
81.2936959039509));
#129585=CARTESIAN_POINT('Ctrl Pts',(-12.6978913807998,-71.778492875624,
81.473837303909));
#129586=CARTESIAN_POINT('Ctrl Pts',(-12.6939377820586,-71.9149891906426,
81.5245438986882));
#129587=CARTESIAN_POINT('Ctrl Pts',(-12.6865509171379,-72.1755740522596,
81.6141597880879));
#129588=CARTESIAN_POINT('Ctrl Pts',(-12.6831168399744,-72.2992233922656,
81.6536808195843));
#129589=CARTESIAN_POINT('Ctrl Pts',(-12.6686769484691,-72.8300938688756,
81.8106190406682));
#129590=CARTESIAN_POINT('Ctrl Pts',(-12.6581004599294,-73.2447671539909,
81.9017477773994));
#129591=CARTESIAN_POINT('Ctrl Pts',(-12.6429841521371,-73.8365551857166,
81.9893019522603));
#129592=CARTESIAN_POINT('Ctrl Pts',(-12.6385485030208,-74.0100931116062,
82.009911378161));
#129593=CARTESIAN_POINT('Ctrl Pts',(-12.6303897858426,-74.3256428695035,
82.0382757901307));
#129594=CARTESIAN_POINT('Ctrl Pts',(-12.6266868331992,-74.4675083578769,
82.047710511139));
#129595=CARTESIAN_POINT('Ctrl Pts',(-12.617520560906,-74.8133822434634,
82.0626548227512));
#129596=CARTESIAN_POINT('Ctrl Pts',(-12.6120030923282,-75.0175466471059,
82.0646645233081));
#129597=CARTESIAN_POINT('Ctrl Pts',(-12.5981418281175,-75.5257306599595,
82.052666705461));
#129598=CARTESIAN_POINT('Ctrl Pts',(-12.5897407616311,-75.8295717809301,
82.0303066237215));
#129599=CARTESIAN_POINT('Ctrl Pts',(-12.5776346915689,-76.271213910937,
81.9752554899712));
#129600=CARTESIAN_POINT('Ctrl Pts',(-12.5738318146591,-76.4105098580751,
81.9545707858028));
#129601=CARTESIAN_POINT('Ctrl Pts',(-12.5666397528045,-76.6762659673904,
81.9086642122392));
#129602=CARTESIAN_POINT('Ctrl Pts',(-12.5632489873379,-76.8026940836846,
81.8839939833719));
#129603=CARTESIAN_POINT('Ctrl Pts',(-12.5543979821308,-77.1359613642734,
81.8113936413141));
#129604=CARTESIAN_POINT('Ctrl Pts',(-12.5490142640923,-77.3415385101451,
81.758863685658));
#129605=CARTESIAN_POINT('Ctrl Pts',(-12.5371414791353,-77.7931385035952,
81.6263902756365));
#129606=CARTESIAN_POINT('Ctrl Pts',(-12.5306687199678,-78.0381323963354,
81.5429642811284));
#129607=CARTESIAN_POINT('Ctrl Pts',(-12.5198097905863,-78.4360483812377,
81.3883567270092));
#129608=CARTESIAN_POINT('Ctrl Pts',(-12.5154832156024,-78.5912660416973,
81.3230622102699));
#129609=CARTESIAN_POINT('Ctrl Pts',(-12.5067780224793,-78.8938256450294,
81.1858722808496));
#129610=CARTESIAN_POINT('Ctrl Pts',(-12.5024086538887,-79.0412709331833,
81.1141948716209));
#129611=CARTESIAN_POINT('Ctrl Pts',(-12.4876512850363,-79.527378984235,
80.8615686936808));
#129612=CARTESIAN_POINT('Ctrl Pts',(-12.47705886029,-79.8569878952453,80.6631100560213));
#129613=CARTESIAN_POINT('Ctrl Pts',(-12.4605950155113,-80.354581441332,
80.3186909925396));
#129614=CARTESIAN_POINT('Ctrl Pts',(-12.4546255940102,-80.5318605086843,
80.1861291658312));
#129615=CARTESIAN_POINT('Ctrl Pts',(-12.4451535059546,-80.810645255994,
79.9610489072495));
#129616=CARTESIAN_POINT('Ctrl Pts',(-12.441587635747,-80.9151227787878,
79.8726402084329));
#129617=CARTESIAN_POINT('Ctrl Pts',(-12.4297682171708,-81.2591813213333,
79.5675826799819));
#129618=CARTESIAN_POINT('Ctrl Pts',(-12.4217150343873,-81.4890080079709,
79.3404125362031));
#129619=CARTESIAN_POINT('Ctrl Pts',(-12.4097902796803,-81.8067228412527,
78.9911061652808));
#129620=CARTESIAN_POINT('Ctrl Pts',(-12.4059944973883,-81.9045785673756,
78.8780468884581));
#129621=CARTESIAN_POINT('Ctrl Pts',(-12.3983150778161,-82.0941562183193,
78.6478522649579));
#129622=CARTESIAN_POINT('Ctrl Pts',(-12.3944253424699,-82.1859075482073,
78.5307387402166));
#129623=CARTESIAN_POINT('Ctrl Pts',(-12.3792466122153,-82.5284005675861,
78.0709765756556));
#129624=CARTESIAN_POINT('Ctrl Pts',(-12.3676265905513,-82.7584450752342,
77.7128311661701));
#129625=CARTESIAN_POINT('Ctrl Pts',(-12.3501789095285,-83.0665612399772,
77.1504303401466));
#129626=CARTESIAN_POINT('Ctrl Pts',(-12.3443007404031,-83.1639025978138,
76.9566677648474));
#129627=CARTESIAN_POINT('Ctrl Pts',(-12.3338989010385,-83.3256751822307,
76.603449511283));
#129628=CARTESIAN_POINT('Ctrl Pts',(-12.3293470789259,-83.3927442843099,
76.4452086806175));
#129629=CARTESIAN_POINT('Ctrl Pts',(-12.3188128681221,-83.5396698100925,
76.0685689243611));
#129630=CARTESIAN_POINT('Ctrl Pts',(-12.3129233796486,-83.6155003438947,
75.8490333280528));
#129631=CARTESIAN_POINT('Ctrl Pts',(-12.3017494698807,-83.7437471914812,
75.4254880926722));
#129632=CARTESIAN_POINT('Ctrl Pts',(-12.2964530014789,-83.7977143608655,
75.2217730391077));
#129633=CARTESIAN_POINT('Ctrl Pts',(-12.2866451140008,-83.8831460865559,
74.847307777468));
#129634=CARTESIAN_POINT('Ctrl Pts',(-12.2821484921725,-83.9169005397076,
74.6770802211227));
#129635=CARTESIAN_POINT('Ctrl Pts',(-12.2699862396666,-83.993978017679,
74.2208274413097));
#129636=CARTESIAN_POINT('Ctrl Pts',(-12.2622222761676,-84.0286547814944,
73.9333196481195));
#129637=CARTESIAN_POINT('Ctrl Pts',(-12.2450150622112,-84.07496636679,73.2979981206966));
#129638=CARTESIAN_POINT('Ctrl Pts',(-12.2355493233976,-84.0805245330233,
72.9496900656169));
#129639=CARTESIAN_POINT('Ctrl Pts',(-12.219973209062,-84.0564487416857,
72.370212445068));
#129640=CARTESIAN_POINT('Ctrl Pts',(-12.2137929796483,-84.0378942134671,
72.1385725370326));
#129641=CARTESIAN_POINT('Ctrl Pts',(-12.2014267933846,-83.9817597033124,
71.6687664535025));
#129642=CARTESIAN_POINT('Ctrl Pts',(-12.1953024392983,-83.9435552079869,
71.4314753887407));
#129643=CARTESIAN_POINT('Ctrl Pts',(-12.1824024959074,-83.8426072573388,
70.9328443161101));
#129644=CARTESIAN_POINT('Ctrl Pts',(-12.175606987108,-83.7775697389122,
70.6721752894815));
#129645=CARTESIAN_POINT('Ctrl Pts',(-12.1618712395346,-83.6269495897832,
70.164906507135));
#129646=CARTESIAN_POINT('Ctrl Pts',(-12.1549798667685,-83.5420053403461,
69.9181172023374));
#129647=CARTESIAN_POINT('Ctrl Pts',(-12.1353898234166,-83.2735999437275,
69.2344195535132));
#129648=CARTESIAN_POINT('Ctrl Pts',(-12.1225434617862,-83.0662956243893,
68.8067637860057));
#129649=CARTESIAN_POINT('Ctrl Pts',(-12.1037492686791,-82.7116612292542,
68.2006434754007));
#129650=CARTESIAN_POINT('Ctrl Pts',(-12.0976726041932,-82.5888330849021,
68.0077748431867));
#129651=CARTESIAN_POINT('Ctrl Pts',(-12.0856429660484,-82.3280912483103,
67.6309355267796));
#129652=CARTESIAN_POINT('Ctrl Pts',(-12.0797266482992,-82.1904393974301,
67.4475114577697));
#129653=CARTESIAN_POINT('Ctrl Pts',(-12.0671749847703,-81.8806577161547,
67.0664029530817));
#129654=CARTESIAN_POINT('Ctrl Pts',(-12.0605190336008,-81.7070720184151,
66.8709785133379));
#129655=CARTESIAN_POINT('Ctrl Pts',(-12.035267722196,-81.0308357003993,
66.1726915170404));
#129656=CARTESIAN_POINT('Ctrl Pts',(-12.0161276153687,-80.4762119092328,
65.7198702614967));
#129657=CARTESIAN_POINT('Ctrl Pts',(-11.9885354599265,-79.6047850254594,
65.1632441845259));
#129658=CARTESIAN_POINT('Ctrl Pts',(-11.9799480428361,-79.3232196806061,
65.0037564975032));
#129659=CARTESIAN_POINT('Ctrl Pts',(-11.9555460584312,-78.4902178801228,
64.5896125196323));
#129660=CARTESIAN_POINT('Ctrl Pts',(-11.9401654023462,-77.9226318585693,
64.3769185663475));
#129661=CARTESIAN_POINT('Ctrl Pts',(-11.9095711822706,-76.7974166915148,
64.077714367338));
#129662=CARTESIAN_POINT('Ctrl Pts',(-11.8946383898076,-76.2413160159509,
63.983441562345));
#129663=CARTESIAN_POINT('Ctrl Pts',(-11.8651054933457,-75.1313007927164,
63.8988593087306));
#129664=CARTESIAN_POINT('Ctrl Pts',(-11.8505012040217,-74.5763507546515,
63.9066755440276));
#129665=CARTESIAN_POINT('Ctrl Pts',(-11.8056121264091,-72.8668116532728,
64.0920100148967));
#129666=CARTESIAN_POINT('Ctrl Pts',(-11.7749787653385,-71.7329701178857,
64.4446450603372));
#129667=CARTESIAN_POINT('Ctrl Pts',(-11.7288034797534,-70.1937132121955,
65.2692902920736));
#129668=CARTESIAN_POINT('Ctrl Pts',(-11.7134866021105,-69.7120312900423,
65.5907288589313));
#129669=CARTESIAN_POINT('Ctrl Pts',(-11.6715688233447,-68.4736430122908,
66.6038228064739));
#129670=CARTESIAN_POINT('Ctrl Pts',(-11.6452414234691,-67.7939667727339,
67.3819253526641));
#129671=CARTESIAN_POINT('Ctrl Pts',(-11.6118309935208,-67.1379883663413,
68.4505909544893));
#129672=CARTESIAN_POINT('Ctrl Pts',(-11.6054799560098,-67.0225405329474,
68.6563132895332));
#129673=CARTESIAN_POINT('Ctrl Pts',(-11.5886254045895,-66.7359352067647,
69.2183212618494));
#129674=CARTESIAN_POINT('Ctrl Pts',(-11.5782817421966,-66.5799982454277,
69.5821855594921));
#129675=CARTESIAN_POINT('Ctrl Pts',(-11.5514878718896,-66.236295204117,
70.5541418509554));
#129676=CARTESIAN_POINT('Ctrl Pts',(-11.535146718226,-66.0870511625888,
71.1761051919815));
#129677=CARTESIAN_POINT('Ctrl Pts',(-11.5094703351698,-65.9590926721202,
72.1432071313965));
#129678=CARTESIAN_POINT('Ctrl Pts',(-11.5003872011654,-65.9333107407222,
72.4823240137874));
#129679=CARTESIAN_POINT('Ctrl Pts',(-11.4829997777813,-65.9209453621675,
73.124259887423));
#129680=CARTESIAN_POINT('Ctrl Pts',(-11.4748714117761,-65.9304147698513,
73.4257664585309));
#129681=CARTESIAN_POINT('Ctrl Pts',(-11.4556877679753,-65.9902539903833,
74.1516658337673));
#129682=CARTESIAN_POINT('Ctrl Pts',(-11.4447447212086,-66.0554078580195,
74.5733722865264));
#129683=CARTESIAN_POINT('Ctrl Pts',(-11.4224735425153,-66.2469448313981,
75.4183849888865));
#129684=CARTESIAN_POINT('Ctrl Pts',(-11.41113960832,-66.3754432388486,75.8413030543231));
#129685=CARTESIAN_POINT('Ctrl Pts',(-11.3935752632689,-66.6144863276698,
76.4629018788126));
#129686=CARTESIAN_POINT('Ctrl Pts',(-11.3875512045202,-66.703078855393,
76.670103989202));
#129687=CARTESIAN_POINT('Ctrl Pts',(-11.3735078648652,-66.9240711877018,
77.137935896527));
#129688=CARTESIAN_POINT('Ctrl Pts',(-11.3654708854703,-67.0616573327916,
77.3961033942245));
#129689=CARTESIAN_POINT('Ctrl Pts',(-11.3527699139652,-67.3046267288358,
77.8023906857588));
#129690=CARTESIAN_POINT('Ctrl Pts',(-11.3479887887623,-67.4023484089624,
77.9549881033649));
#129691=CARTESIAN_POINT('Ctrl Pts',(-11.3377039099922,-67.6247424021602,
78.2802199958459));
#129692=CARTESIAN_POINT('Ctrl Pts',(-11.3322193338531,-67.7511630632259,
78.4517057192843));
#129693=CARTESIAN_POINT('Ctrl Pts',(-11.3124185053928,-68.2312664237496,
79.0572791980971));
#129694=CARTESIAN_POINT('Ctrl Pts',(-11.2982657719826,-68.6196423799201,
79.4639972476825));
#129695=CARTESIAN_POINT('Ctrl Pts',(-11.2787715814941,-69.1771042720877,
79.9500337849055));
#129696=CARTESIAN_POINT('Ctrl Pts',(-11.2739662512911,-69.3160426787427,
80.0641532312963));
#129697=CARTESIAN_POINT('Ctrl Pts',(-11.262817305294,-69.6412828963894,
80.3155537500748));
#129698=CARTESIAN_POINT('Ctrl Pts',(-11.2564498950354,-69.8297243550707,
80.4500687474039));
#129699=CARTESIAN_POINT('Ctrl Pts',(-11.2447256892503,-70.1883215496775,
80.6857100721471));
#129700=CARTESIAN_POINT('Ctrl Pts',(-11.2393556625268,-70.3572539516981,
80.7889130438971));
#129701=CARTESIAN_POINT('Ctrl Pts',(-11.2294950337287,-70.6803179939104,
80.971690160875));
#129702=CARTESIAN_POINT('Ctrl Pts',(-11.2249757098433,-70.8333852967702,
81.052492076728));
#129703=CARTESIAN_POINT('Ctrl Pts',(-11.2147842416095,-71.1873142054762,
81.2264846822883));
#129704=CARTESIAN_POINT('Ctrl Pts',(-11.2091430517,-71.3895698597399,81.3168235808343));
#129705=CARTESIAN_POINT('Ctrl Pts',(-11.1928228284033,-71.985184406746,
81.5572487943015));
#129706=CARTESIAN_POINT('Ctrl Pts',(-11.1821830457734,-72.3864812781739,
81.6877900173541));
#129707=CARTESIAN_POINT('Ctrl Pts',(-11.1672197941371,-72.94151884285,81.8270353181207));
#129708=CARTESIAN_POINT('Ctrl Pts',(-11.1632145090628,-73.0891861999772,
81.8602227975301));
#129709=CARTESIAN_POINT('Ctrl Pts',(-11.155076789241,-73.3861335316759,
81.9192649628482));
#129710=CARTESIAN_POINT('Ctrl Pts',(-11.1509507638806,-73.5354179741734,
81.9451126153875));
#129711=CARTESIAN_POINT('Ctrl Pts',(-11.136345270979,-74.0632482480024,
82.0229871572942));
#129712=CARTESIAN_POINT('Ctrl Pts',(-11.1257607190002,-74.4447532345393,
82.0549445472154));
#129713=CARTESIAN_POINT('Ctrl Pts',(-11.1117147504199,-74.9733152347867,
82.0650328851075));
#129714=CARTESIAN_POINT('Ctrl Pts',(-11.1078845385412,-75.1198987599237,
82.064201547195));
#129715=CARTESIAN_POINT('Ctrl Pts',(-11.0994677740146,-75.4453943606477,
82.0543833055328));
#129716=CARTESIAN_POINT('Ctrl Pts',(-11.0949024066108,-75.6242461350268,
82.0436262524113));
#129717=CARTESIAN_POINT('Ctrl Pts',(-11.0787649462341,-76.258124511933,
81.9866335788158));
#129718=CARTESIAN_POINT('Ctrl Pts',(-11.0673216940971,-76.7105666564122,
81.9112406965473));
#129719=CARTESIAN_POINT('Ctrl Pts',(-11.0517603340098,-77.2894569777918,
81.7697555753342));
#129720=CARTESIAN_POINT('Ctrl Pts',(-11.0480914431371,-77.4233479071564,
81.7337998165184));
#129721=CARTESIAN_POINT('Ctrl Pts',(-11.0402828875073,-77.7025558157715,
81.6519880196989));
#129722=CARTESIAN_POINT('Ctrl Pts',(-11.0361393291105,-77.8476910893183,
81.6055027991634));
#129723=CARTESIAN_POINT('Ctrl Pts',(-11.0226028032279,-78.3151379631504,
81.4427744268616));
#129724=CARTESIAN_POINT('Ctrl Pts',(-11.013117398753,-78.632367274265,81.3119098409886));
#129725=CARTESIAN_POINT('Ctrl Pts',(-11.0001390418047,-79.0660376683573,
81.1031778333896));
#129726=CARTESIAN_POINT('Ctrl Pts',(-10.996440079161,-79.1896286560287,
81.0401168218329));
#129727=CARTESIAN_POINT('Ctrl Pts',(-10.9881276344862,-79.4684405309305,
80.8894971637464));
#129728=CARTESIAN_POINT('Ctrl Pts',(-10.9835493630003,-79.6224993875693,
80.8002005014945));
#129729=CARTESIAN_POINT('Ctrl Pts',(-10.9719173868032,-80.0107888351821,
80.559498709591));
#129730=CARTESIAN_POINT('Ctrl Pts',(-10.9649310590942,-80.2409714860484,
80.4015796609635));
#129731=CARTESIAN_POINT('Ctrl Pts',(-10.9520909189305,-80.6463227010311,
80.0953038614243));
#129732=CARTESIAN_POINT('Ctrl Pts',(-10.9462563662033,-80.823996584897,
79.9502453449538));
#129733=CARTESIAN_POINT('Ctrl Pts',(-10.9367398462232,-81.0981567056813,
79.7087565036097));
#129734=CARTESIAN_POINT('Ctrl Pts',(-10.9331400685857,-81.1983222258153,
79.6164897843008));
#129735=CARTESIAN_POINT('Ctrl Pts',(-10.9253018669614,-81.4092241844754,
79.4133595792018));
#129736=CARTESIAN_POINT('Ctrl Pts',(-10.9210528015737,-81.5192815238177,
79.3017862909333));
#129737=CARTESIAN_POINT('Ctrl Pts',(-10.9068397495232,-81.875487434268,
78.921620380461));
#129738=CARTESIAN_POINT('Ctrl Pts',(-10.8967655389423,-82.1087030403898,
78.6408843880499));
#129739=CARTESIAN_POINT('Ctrl Pts',(-10.8828483312068,-82.413679900872,
78.2247447023));
#129740=CARTESIAN_POINT('Ctrl Pts',(-10.8788010458399,-82.500209868164,
78.1001817229147));
#129741=CARTESIAN_POINT('Ctrl Pts',(-10.8706266961558,-82.671333260355,
77.8398668968101));
#129742=CARTESIAN_POINT('Ctrl Pts',(-10.8665121345898,-82.7555152168254,
77.7039405008203));
#129743=CARTESIAN_POINT('Ctrl Pts',(-10.856353382447,-82.9563723238259,
77.3594219109496));
#129744=CARTESIAN_POINT('Ctrl Pts',(-10.8503610923287,-83.068510749718,
77.1481308616468));
#129745=CARTESIAN_POINT('Ctrl Pts',(-10.8381288231242,-83.2790978353818,
76.710575011933));
#129746=CARTESIAN_POINT('Ctrl Pts',(-10.831886352734,-83.3770033625072,
76.4840451405209));
#129747=CARTESIAN_POINT('Ctrl Pts',(-10.8217668907393,-83.5169687353684,
76.1206408386014));
#129748=CARTESIAN_POINT('Ctrl Pts',(-10.8179950385984,-83.5651983130977,
75.9861295767924));
#129749=CARTESIAN_POINT('Ctrl Pts',(-10.8096809863021,-83.6634147315317,
75.690676263741));
#129750=CARTESIAN_POINT('Ctrl Pts',(-10.8051227658235,-83.7121656758757,
75.5293153899842));
#129751=CARTESIAN_POINT('Ctrl Pts',(-10.7899774491732,-83.8583919350915,
74.9922351118796));
#129752=CARTESIAN_POINT('Ctrl Pts',(-10.779276771381,-83.9365571395873,
74.6112262864475));
#129753=CARTESIAN_POINT('Ctrl Pts',(-10.764446174225,-84.0122615806992,
74.0652142323235));
#129754=CARTESIAN_POINT('Ctrl Pts',(-10.7601036036432,-84.0302707333152,
73.903055698679));
#129755=CARTESIAN_POINT('Ctrl Pts',(-10.7514349197537,-84.0577630941967,
73.5730469775939));
#129756=CARTESIAN_POINT('Ctrl Pts',(-10.7471287260413,-84.0669374929368,
73.405428682919));
#129757=CARTESIAN_POINT('Ctrl Pts',(-10.7358619095138,-84.0787625241277,
72.9619473847261));
#129758=CARTESIAN_POINT('Ctrl Pts',(-10.7289707149286,-84.0733941778988,
72.685805038355));
#129759=CARTESIAN_POINT('Ctrl Pts',(-10.7172883315525,-84.0435205228047,
72.225632846293));
#129760=CARTESIAN_POINT('Ctrl Pts',(-10.7125468286424,-84.0258848894152,
72.0411589170452));
#129761=CARTESIAN_POINT('Ctrl Pts',(-10.7028091161632,-83.9791780091691,
71.6713067829865));
#129762=CARTESIAN_POINT('Ctrl Pts',(-10.6978240824464,-83.9499652833923,
71.4859437134095));
#129763=CARTESIAN_POINT('Ctrl Pts',(-10.6859519616658,-83.8677668236538,
71.0514043390162));
#129764=CARTESIAN_POINT('Ctrl Pts',(-10.6790221537907,-83.8100096489346,
70.8031104204124));
#129765=CARTESIAN_POINT('Ctrl Pts',(-10.6625254816767,-83.6480677969372,
70.2187496496713));
#129766=CARTESIAN_POINT('Ctrl Pts',(-10.6529601698758,-83.5345692708946,
69.8852398590506));
#129767=CARTESIAN_POINT('Ctrl Pts',(-10.6395386792417,-83.3435586958817,
69.416262784576));
#129768=CARTESIAN_POINT('Ctrl Pts',(-10.635484714546,-83.2814771857297,
69.2744458777196));
#129769=CARTESIAN_POINT('Ctrl Pts',(-10.6276706720216,-83.1526957541936,
69.0000729422436));
#129770=CARTESIAN_POINT('Ctrl Pts',(-10.6239043064502,-83.0863940754931,
68.8675296775701));
#129771=CARTESIAN_POINT('Ctrl Pts',(-10.6111042815369,-82.8490086757923,
68.420914084305));
#129772=CARTESIAN_POINT('Ctrl Pts',(-10.6021268483587,-82.6623278250407,
68.1151571826957));
#129773=CARTESIAN_POINT('Ctrl Pts',(-10.5867381875179,-82.326115834269,
67.630735462257));
#129774=CARTESIAN_POINT('Ctrl Pts',(-10.5805715462487,-82.1865607801452,
67.4451454461591));
#129775=CARTESIAN_POINT('Ctrl Pts',(-10.5650350745576,-81.8210906315581,
66.9956415649896));
#129776=CARTESIAN_POINT('Ctrl Pts',(-10.5555949762819,-81.5866782437081,
66.7385774415894));
#129777=CARTESIAN_POINT('Ctrl Pts',(-10.5385582191953,-81.1355374615621,
66.2972824871332));
#129778=CARTESIAN_POINT('Ctrl Pts',(-10.5309401020441,-80.9234004412554,
66.1083149121387));
#129779=CARTESIAN_POINT('Ctrl Pts',(-10.5185784955525,-80.558712438817,
65.8132329292415));
#129780=CARTESIAN_POINT('Ctrl Pts',(-10.5137593129423,-80.4110295335681,
65.7011238923676));
#129781=CARTESIAN_POINT('Ctrl Pts',(-10.5032278352579,-80.075827983657,
65.4628829634833));
#129782=CARTESIAN_POINT('Ctrl Pts',(-10.4975397088479,-79.8870655411617,
65.3392252239502));
#129783=CARTESIAN_POINT('Ctrl Pts',(-10.4863052237275,-79.5093908763208,
65.1115097278787));
#129784=CARTESIAN_POINT('Ctrl Pts',(-10.4807413503383,-79.3208662242744,
65.006831185423));
#129785=CARTESIAN_POINT('Ctrl Pts',(-10.4659000199624,-78.8168341624272,
64.7498478759028));
#129786=CARTESIAN_POINT('Ctrl Pts',(-10.4565068000018,-78.495612857664,
64.6086814206857));
#129787=CARTESIAN_POINT('Ctrl Pts',(-10.4328689875357,-77.6742738991775,
64.3024572344422));
#129788=CARTESIAN_POINT('Ctrl Pts',(-10.4185567360137,-77.1652267829833,
64.1609942365449));
#129789=CARTESIAN_POINT('Ctrl Pts',(-10.3998132013467,-76.4650161673287,
64.0310789897881));
#129790=CARTESIAN_POINT('Ctrl Pts',(-10.3949774604576,-76.2811265669053,
64.0028226988203));
#129791=CARTESIAN_POINT('Ctrl Pts',(-10.3854233122192,-75.9102533351739,
63.9577407002902));
#129792=CARTESIAN_POINT('Ctrl Pts',(-10.3807025242223,-75.7234889632973,
63.9410072019634));
#129793=CARTESIAN_POINT('Ctrl Pts',(-10.3598136559066,-74.8969357704687,
63.8928675879046));
#129794=CARTESIAN_POINT('Ctrl Pts',(-10.3434208244558,-74.2534668802988,
63.9237836430573));
#129795=CARTESIAN_POINT('Ctrl Pts',(-10.3163511471999,-73.2248189217987,
64.0816982601024));
#129796=CARTESIAN_POINT('Ctrl Pts',(-10.3058317022822,-72.833207037268,
64.1683093390963));
#129797=CARTESIAN_POINT('Ctrl Pts',(-10.2868973273492,-72.1534178330174,
64.3666454477573));
#129798=CARTESIAN_POINT('Ctrl Pts',(-10.2785506208785,-71.8619117144815,
64.4680682443189));
#129799=CARTESIAN_POINT('Ctrl Pts',(-10.2634506828038,-71.3557661531558,
64.6744071121457));
#129800=CARTESIAN_POINT('Ctrl Pts',(-10.2567170220152,-71.1391476857274,
64.7730143965423));
#129801=CARTESIAN_POINT('Ctrl Pts',(-10.2405995625591,-70.6479643524153,
65.0204229195374));
#129802=CARTESIAN_POINT('Ctrl Pts',(-10.2311102067042,-70.376468234342,
65.1752660712453));
#129803=CARTESIAN_POINT('Ctrl Pts',(-10.2011100154883,-69.5562051963923,
65.7003104258447));
#129804=CARTESIAN_POINT('Ctrl Pts',(-10.1801506924231,-69.0372672770758,
66.1176270367454));
#129805=CARTESIAN_POINT('Ctrl Pts',(-10.1564941020868,-68.4598867081246,
66.6961827051763));
#129806=CARTESIAN_POINT('Ctrl Pts',(-10.152091703178,-68.3528454317604,
66.8091134944626));
#129807=CARTESIAN_POINT('Ctrl Pts',(-10.1457737775871,-68.1990347021608,
66.9800801024668));
#129808=CARTESIAN_POINT('Ctrl Pts',(-10.1437587930829,-68.1499490975946,
67.036025392201));
#129809=CARTESIAN_POINT('Ctrl Pts',(-10.1402109642241,-68.0633659894135,
67.1372354834832));
#129810=CARTESIAN_POINT('Ctrl Pts',(-10.1386658575816,-68.0256028272131,
67.18227159919));
#129811=CARTESIAN_POINT('Ctrl Pts',(-10.1352649287799,-67.9422968840066,
67.2836493022914));
#129812=CARTESIAN_POINT('Ctrl Pts',(-10.1334204988097,-67.8969890987286,
67.3401823061191));
#129813=CARTESIAN_POINT('Ctrl Pts',(-10.1274698000766,-67.7506851965573,
67.5273566676092));
#129814=CARTESIAN_POINT('Ctrl Pts',(-10.123488960456,-67.6526051050933,
67.660273810607));
#129815=CARTESIAN_POINT('Ctrl Pts',(-10.1114123720327,-67.3579075215302,
68.0834662666085));
#129816=CARTESIAN_POINT('Ctrl Pts',(-10.1037158808832,-67.1743297727036,
68.3828182585121));
#129817=CARTESIAN_POINT('Ctrl Pts',(-10.0961244884418,-67.0084911154305,
68.6916878272719));
#129818=CARTESIAN_POINT('Ctrl Pts',(-13.5675364833309,-81.8820510104931,
67.097620723923));
#129819=CARTESIAN_POINT('Ctrl Pts',(-13.5675364833309,-81.6920778341857,
66.8981047934654));
#129820=CARTESIAN_POINT('Ctrl Pts',(-13.5675364833309,-81.4931660627479,
66.7070837578721));
#129821=CARTESIAN_POINT('Ctrl Pts',(-13.5675364833309,-81.0810140826979,
66.3448797285691));
#129822=CARTESIAN_POINT('Ctrl Pts',(-13.5675364833309,-80.8678695555096,
66.1735119454469));
#129823=CARTESIAN_POINT('Ctrl Pts',(-13.5675364833309,-80.6476829122575,
66.0117865989301));
#129824=CARTESIAN_POINT('Ctrl Pts',(-13.6367975371279,-82.22637258748,78.478439844214));
#129825=CARTESIAN_POINT('Ctrl Pts',(-13.5965727996549,-83.15132333764,77.260846746689));
#129826=CARTESIAN_POINT('Ctrl Pts',(-13.5161233247074,-84.37134578258,74.349656820311));
#129827=CARTESIAN_POINT('Ctrl Pts',(-13.3954491122865,-83.85839097116,69.641309155131));
#129828=CARTESIAN_POINT('Ctrl Pts',(-13.2747748998656,-81.12957508313,65.770566029046));
#129829=CARTESIAN_POINT('Ctrl Pts',(-13.1541006874447,-76.867728622,63.705144460549));
#129830=CARTESIAN_POINT('Ctrl Pts',(-13.0334264750238,-72.13871802361,63.961747337343));
#129831=CARTESIAN_POINT('Ctrl Pts',(-12.9127522626029,-68.12536086466,66.476164874831));
#129832=CARTESIAN_POINT('Ctrl Pts',(-12.7920780501819,-65.83145073401,70.619512225841));
#129833=CARTESIAN_POINT('Ctrl Pts',(-12.6714038377609,-65.83072989138,75.355475184308));
#129834=CARTESIAN_POINT('Ctrl Pts',(-12.5507296253399,-68.12337819702,79.499520367103));
#129835=CARTESIAN_POINT('Ctrl Pts',(-12.4300554129189,-72.13597072448,82.015161004986));
#129836=CARTESIAN_POINT('Ctrl Pts',(-12.3093812004979,-76.86489906758,82.273198436157));
#129837=CARTESIAN_POINT('Ctrl Pts',(-12.1887069880768,-81.12738874216,80.209093695038));
#129838=CARTESIAN_POINT('Ctrl Pts',(-12.0680327756558,-83.857328421,76.339109722068));
#129839=CARTESIAN_POINT('Ctrl Pts',(-11.9473585632348,-84.37192006169,71.631186395751));
#129840=CARTESIAN_POINT('Ctrl Pts',(-11.8266843508137,-82.5424567304,67.262844545329));
#129841=CARTESIAN_POINT('Ctrl Pts',(-11.7060101383926,-78.82651409889,64.326670680903));
#129842=CARTESIAN_POINT('Ctrl Pts',(-11.5853359259716,-74.15350404259,63.557045046897));
#129843=CARTESIAN_POINT('Ctrl Pts',(-11.4646617135509,-69.69221506849,65.146462327629));
#129844=CARTESIAN_POINT('Ctrl Pts',(-11.3439875011299,-66.55848112866,68.697385897282));
#129845=CARTESIAN_POINT('Ctrl Pts',(-11.2233132887089,-65.53609514649,73.3216775732695));
#129846=CARTESIAN_POINT('Ctrl Pts',(-11.1026390762869,-66.88077088472,77.862734032643));
#129847=CARTESIAN_POINT('Ctrl Pts',(-10.9819648638659,-70.25618517554,81.184770299059));
#129848=CARTESIAN_POINT('Ctrl Pts',(-10.8612906514449,-74.81809728471,82.456896282854));
#129849=CARTESIAN_POINT('Ctrl Pts',(-10.7406164390239,-79.42550594423,81.360934525046));
#129850=CARTESIAN_POINT('Ctrl Pts',(-10.6199422266029,-82.92603048601,78.171001360235));
#129851=CARTESIAN_POINT('Ctrl Pts',(-10.4992680141819,-84.44413839523,73.6849452599873));
#129852=CARTESIAN_POINT('Ctrl Pts',(-10.3785938017609,-83.60012808368,69.02479742627));
#129853=CARTESIAN_POINT('Ctrl Pts',(-10.2579195893399,-80.60510074462,65.356119528941));
#129854=CARTESIAN_POINT('Ctrl Pts',(-10.1372453769189,-76.20814999546,63.596538435828));
#129855=CARTESIAN_POINT('Ctrl Pts',(-10.0165711644989,-71.50904302936,64.186014661069));
#129856=CARTESIAN_POINT('Ctrl Pts',(-9.89589695207791,-67.68300161261,66.977621268753));
#129857=CARTESIAN_POINT('Ctrl Pts',(-9.81544747712991,-66.35255094703,69.840029796558));
#129858=CARTESIAN_POINT('Ctrl Pts',(-9.77522273965691,-66.0753597154,71.343769089941));
#129859=CARTESIAN_POINT('Ctrl Pts',(-13.7234642037949,-82.22637258748,78.478439844214));
#129860=CARTESIAN_POINT('Ctrl Pts',(-13.6832394663209,-83.15132333764,77.260846746689));
#129861=CARTESIAN_POINT('Ctrl Pts',(-13.6027899913739,-84.37134578258,74.349656820311));
#129862=CARTESIAN_POINT('Ctrl Pts',(-13.4821157789532,-83.85839097116,69.641309155131));
#129863=CARTESIAN_POINT('Ctrl Pts',(-13.3614415665323,-81.12957508313,65.770566029046));
#129864=CARTESIAN_POINT('Ctrl Pts',(-13.2407673541114,-76.867728622,63.705144460549));
#129865=CARTESIAN_POINT('Ctrl Pts',(-13.1200931416905,-72.13871802361,63.961747337343));
#129866=CARTESIAN_POINT('Ctrl Pts',(-12.9994189292695,-68.12536086466,66.476164874831));
#129867=CARTESIAN_POINT('Ctrl Pts',(-12.8787447168486,-65.83145073401,70.619512225841));
#129868=CARTESIAN_POINT('Ctrl Pts',(-12.7580705044276,-65.83072989138,75.355475184308));
#129869=CARTESIAN_POINT('Ctrl Pts',(-12.6373962920066,-68.12337819702,79.499520367103));
#129870=CARTESIAN_POINT('Ctrl Pts',(-12.5167220795856,-72.13597072448,82.015161004986));
#129871=CARTESIAN_POINT('Ctrl Pts',(-12.3960478671645,-76.86489906758,82.273198436157));
#129872=CARTESIAN_POINT('Ctrl Pts',(-12.2753736547435,-81.12738874216,80.209093695038));
#129873=CARTESIAN_POINT('Ctrl Pts',(-12.1546994423225,-83.857328421,76.339109722068));
#129874=CARTESIAN_POINT('Ctrl Pts',(-12.0340252299014,-84.37192006169,71.631186395751));
#129875=CARTESIAN_POINT('Ctrl Pts',(-11.9133510174804,-82.5424567304,67.262844545329));
#129876=CARTESIAN_POINT('Ctrl Pts',(-11.7926768050593,-78.82651409889,64.326670680903));
#129877=CARTESIAN_POINT('Ctrl Pts',(-11.6720025926383,-74.15350404259,63.557045046897));
#129878=CARTESIAN_POINT('Ctrl Pts',(-11.5513283802169,-69.69221506849,65.146462327629));
#129879=CARTESIAN_POINT('Ctrl Pts',(-11.4306541677959,-66.55848112866,68.697385897282));
#129880=CARTESIAN_POINT('Ctrl Pts',(-11.3099799553749,-65.53609514649,73.3216775732695));
#129881=CARTESIAN_POINT('Ctrl Pts',(-11.1893057429539,-66.88077088472,77.862734032643));
#129882=CARTESIAN_POINT('Ctrl Pts',(-11.0686315305329,-70.25618517554,81.184770299059));
#129883=CARTESIAN_POINT('Ctrl Pts',(-10.9479573181119,-74.81809728471,82.456896282854));
#129884=CARTESIAN_POINT('Ctrl Pts',(-10.8272831056909,-79.42550594423,81.360934525046));
#129885=CARTESIAN_POINT('Ctrl Pts',(-10.7066088932699,-82.92603048601,78.171001360235));
#129886=CARTESIAN_POINT('Ctrl Pts',(-10.5859346808489,-84.44413839523,73.6849452599873));
#129887=CARTESIAN_POINT('Ctrl Pts',(-10.4652604684279,-83.60012808368,69.02479742627));
#129888=CARTESIAN_POINT('Ctrl Pts',(-10.3445862560069,-80.60510074462,65.356119528941));
#129889=CARTESIAN_POINT('Ctrl Pts',(-10.2239120435859,-76.20814999546,63.596538435828));
#129890=CARTESIAN_POINT('Ctrl Pts',(-10.1032378311649,-71.50904302936,64.186014661069));
#129891=CARTESIAN_POINT('Ctrl Pts',(-9.98256361874391,-67.68300161261,66.977621268753));
#129892=CARTESIAN_POINT('Ctrl Pts',(-9.90211414379691,-66.35255094703,69.840029796558));
#129893=CARTESIAN_POINT('Ctrl Pts',(-9.86188940632291,-66.0753597154,71.343769089941));
#129894=CARTESIAN_POINT('Ctrl Pts',(-13.8101308704619,-82.22637258748,78.478439844214));
#129895=CARTESIAN_POINT('Ctrl Pts',(-13.7699061329879,-83.15132333764,77.260846746689));
#129896=CARTESIAN_POINT('Ctrl Pts',(-13.6894566580409,-84.37134578258,74.349656820311));
#129897=CARTESIAN_POINT('Ctrl Pts',(-13.5687824456199,-83.85839097116,69.641309155131));
#129898=CARTESIAN_POINT('Ctrl Pts',(-13.448108233199,-81.12957508313,65.770566029046));
#129899=CARTESIAN_POINT('Ctrl Pts',(-13.3274340207781,-76.867728622,63.705144460549));
#129900=CARTESIAN_POINT('Ctrl Pts',(-13.2067598083571,-72.13871802361,63.961747337343));
#129901=CARTESIAN_POINT('Ctrl Pts',(-13.0860855959362,-68.12536086466,66.476164874831));
#129902=CARTESIAN_POINT('Ctrl Pts',(-12.9654113835152,-65.83145073401,70.619512225841));
#129903=CARTESIAN_POINT('Ctrl Pts',(-12.8447371710942,-65.83072989138,75.355475184308));
#129904=CARTESIAN_POINT('Ctrl Pts',(-12.7240629586732,-68.12337819702,79.499520367103));
#129905=CARTESIAN_POINT('Ctrl Pts',(-12.6033887462522,-72.13597072448,82.015161004986));
#129906=CARTESIAN_POINT('Ctrl Pts',(-12.4827145338312,-76.86489906758,82.273198436157));
#129907=CARTESIAN_POINT('Ctrl Pts',(-12.3620403214102,-81.12738874216,80.209093695038));
#129908=CARTESIAN_POINT('Ctrl Pts',(-12.2413661089891,-83.857328421,76.339109722068));
#129909=CARTESIAN_POINT('Ctrl Pts',(-12.1206918965681,-84.37192006169,71.631186395751));
#129910=CARTESIAN_POINT('Ctrl Pts',(-12.000017684147,-82.5424567304,67.262844545329));
#129911=CARTESIAN_POINT('Ctrl Pts',(-11.879343471726,-78.82651409889,64.326670680903));
#129912=CARTESIAN_POINT('Ctrl Pts',(-11.7586692593049,-74.15350404259,63.557045046897));
#129913=CARTESIAN_POINT('Ctrl Pts',(-11.6379950468839,-69.69221506849,65.146462327629));
#129914=CARTESIAN_POINT('Ctrl Pts',(-11.5173208344629,-66.55848112866,68.697385897282));
#129915=CARTESIAN_POINT('Ctrl Pts',(-11.3966466220419,-65.53609514649,73.3216775732695));
#129916=CARTESIAN_POINT('Ctrl Pts',(-11.2759724096209,-66.88077088472,77.862734032643));
#129917=CARTESIAN_POINT('Ctrl Pts',(-11.1552981971999,-70.25618517554,81.184770299059));
#129918=CARTESIAN_POINT('Ctrl Pts',(-11.0346239847789,-74.81809728471,82.456896282854));
#129919=CARTESIAN_POINT('Ctrl Pts',(-10.9139497723579,-79.42550594423,81.360934525046));
#129920=CARTESIAN_POINT('Ctrl Pts',(-10.7932755599369,-82.92603048601,78.171001360235));
#129921=CARTESIAN_POINT('Ctrl Pts',(-10.6726013475159,-84.44413839523,73.6849452599872));
#129922=CARTESIAN_POINT('Ctrl Pts',(-10.5519271350949,-83.60012808368,69.02479742627));
#129923=CARTESIAN_POINT('Ctrl Pts',(-10.4312529226739,-80.60510074462,65.356119528941));
#129924=CARTESIAN_POINT('Ctrl Pts',(-10.3105787102529,-76.20814999546,63.596538435828));
#129925=CARTESIAN_POINT('Ctrl Pts',(-10.1899044978319,-71.50904302936,64.186014661069));
#129926=CARTESIAN_POINT('Ctrl Pts',(-10.0692302854109,-67.68300161261,66.977621268753));
#129927=CARTESIAN_POINT('Ctrl Pts',(-9.98878081046391,-66.35255094703,69.840029796558));
#129928=CARTESIAN_POINT('Ctrl Pts',(-9.94855607298991,-66.0753597154,71.343769089941));
#129929=CARTESIAN_POINT('Ctrl Pts',(-13.8967975371279,-82.22637258748,78.478439844214));
#129930=CARTESIAN_POINT('Ctrl Pts',(-13.8565727996549,-83.15132333764,77.260846746689));
#129931=CARTESIAN_POINT('Ctrl Pts',(-13.7761233247079,-84.37134578258,74.349656820311));
#129932=CARTESIAN_POINT('Ctrl Pts',(-13.6554491122869,-83.85839097116,69.641309155131));
#129933=CARTESIAN_POINT('Ctrl Pts',(-13.5347748998657,-81.12957508313,65.770566029046));
#129934=CARTESIAN_POINT('Ctrl Pts',(-13.4141006874447,-76.867728622,63.705144460549));
#129935=CARTESIAN_POINT('Ctrl Pts',(-13.2934264750238,-72.13871802361,63.961747337343));
#129936=CARTESIAN_POINT('Ctrl Pts',(-13.1727522626029,-68.12536086466,66.476164874831));
#129937=CARTESIAN_POINT('Ctrl Pts',(-13.0520780501819,-65.83145073401,70.619512225841));
#129938=CARTESIAN_POINT('Ctrl Pts',(-12.9314038377609,-65.83072989138,75.355475184308));
#129939=CARTESIAN_POINT('Ctrl Pts',(-12.8107296253399,-68.12337819702,79.499520367103));
#129940=CARTESIAN_POINT('Ctrl Pts',(-12.6900554129189,-72.13597072448,82.015161004986));
#129941=CARTESIAN_POINT('Ctrl Pts',(-12.5693812004979,-76.86489906758,82.273198436157));
#129942=CARTESIAN_POINT('Ctrl Pts',(-12.4487069880768,-81.12738874216,80.209093695038));
#129943=CARTESIAN_POINT('Ctrl Pts',(-12.3280327756558,-83.857328421,76.339109722068));
#129944=CARTESIAN_POINT('Ctrl Pts',(-12.2073585632348,-84.37192006169,71.631186395751));
#129945=CARTESIAN_POINT('Ctrl Pts',(-12.0866843508137,-82.5424567304,67.262844545329));
#129946=CARTESIAN_POINT('Ctrl Pts',(-11.9660101383927,-78.82651409889,64.326670680903));
#129947=CARTESIAN_POINT('Ctrl Pts',(-11.8453359259716,-74.15350404259,63.557045046897));
#129948=CARTESIAN_POINT('Ctrl Pts',(-11.7246617135505,-69.69221506849,65.146462327629));
#129949=CARTESIAN_POINT('Ctrl Pts',(-11.6039875011295,-66.55848112866,68.697385897282));
#129950=CARTESIAN_POINT('Ctrl Pts',(-11.4833132887089,-65.53609514649,73.3216775732695));
#129951=CARTESIAN_POINT('Ctrl Pts',(-11.3626390762869,-66.88077088472,77.862734032643));
#129952=CARTESIAN_POINT('Ctrl Pts',(-11.2419648638659,-70.25618517554,81.184770299059));
#129953=CARTESIAN_POINT('Ctrl Pts',(-11.1212906514449,-74.81809728471,82.456896282854));
#129954=CARTESIAN_POINT('Ctrl Pts',(-11.0006164390239,-79.42550594423,81.360934525046));
#129955=CARTESIAN_POINT('Ctrl Pts',(-10.8799422266029,-82.92603048601,78.171001360235));
#129956=CARTESIAN_POINT('Ctrl Pts',(-10.7592680141819,-84.44413839523,73.6849452599872));
#129957=CARTESIAN_POINT('Ctrl Pts',(-10.6385938017609,-83.60012808368,69.02479742627));
#129958=CARTESIAN_POINT('Ctrl Pts',(-10.5179195893399,-80.60510074462,65.356119528941));
#129959=CARTESIAN_POINT('Ctrl Pts',(-10.3972453769189,-76.20814999546,63.596538435828));
#129960=CARTESIAN_POINT('Ctrl Pts',(-10.2765711644989,-71.50904302936,64.186014661069));
#129961=CARTESIAN_POINT('Ctrl Pts',(-10.1558969520779,-67.68300161261,66.977621268753));
#129962=CARTESIAN_POINT('Ctrl Pts',(-10.0754474771299,-66.35255094703,69.840029796558));
#129963=CARTESIAN_POINT('Ctrl Pts',(-10.0352227396569,-66.0753597154,71.343769089941));
#129964=CARTESIAN_POINT('Ctrl Pts',(-13.5675364833309,-83.5583138245559,
76.0030914693076));
#129965=CARTESIAN_POINT('Ctrl Pts',(-13.5675364833309,-83.8209811139739,
75.2587654320264));
#129966=CARTESIAN_POINT('Ctrl Pts',(-13.5675364833309,-83.9873332505196,
74.480716603791));
#129967=CARTESIAN_POINT('Ctrl Pts',(-13.5675364833309,-84.1078633043029,
72.8969024422775));
#129968=CARTESIAN_POINT('Ctrl Pts',(-13.5675364833309,-84.0638930649032,
72.0991602388659));
#129969=CARTESIAN_POINT('Ctrl Pts',(-13.5675364833309,-83.7739991701906,
70.5423334575277));
#129970=CARTESIAN_POINT('Ctrl Pts',(-13.5675364833309,-83.5285763798928,
69.785555327736));
#129971=CARTESIAN_POINT('Ctrl Pts',(-13.5675364833309,-82.8410434730265,
68.3550103187433));
#129972=CARTESIAN_POINT('Ctrl Pts',(-13.5675364833309,-82.4057128334609,
67.6879975203469));
#129973=CARTESIAN_POINT('Ctrl Pts',(-13.5675364833309,-81.8927835901898,
67.0877618837426));
#129974=CARTESIAN_POINT('Origin',(-13.5675364833309,-75.,72.98888938658));
#129975=CARTESIAN_POINT('Ctrl Pts',(20.4053531221886,-17.1864037180436,
115.724508184767));
#129976=CARTESIAN_POINT('Ctrl Pts',(22.6252113906833,-17.1864037180436,
115.358472943979));
#129977=CARTESIAN_POINT('Ctrl Pts',(27.063989861239,-16.2914328094368,114.626567868827));
#129978=CARTESIAN_POINT('Ctrl Pts',(32.7110101862275,-12.4690426124586,
113.707002820814));
#129979=CARTESIAN_POINT('Ctrl Pts',(36.4883533005745,-6.74813242015872,
113.117112310253));
#129980=CARTESIAN_POINT('Ctrl Pts',(37.8234383481741,1.42212630560579E-14,
112.957857790712));
#129981=CARTESIAN_POINT('Ctrl Pts',(36.5144005272245,6.74813242015874,113.264833473205));
#129982=CARTESIAN_POINT('Ctrl Pts',(32.7631046395276,12.4690426124586,114.002445146718));
#129983=CARTESIAN_POINT('Ctrl Pts',(27.1421315411891,16.2914328094368,115.069731357682));
#129984=CARTESIAN_POINT('Ctrl Pts',(20.5095420287887,17.633889172347,116.315392836574));
#129985=CARTESIAN_POINT('Ctrl Pts',(13.8769525163883,16.2914328094368,117.561054315465));
#129986=CARTESIAN_POINT('Ctrl Pts',(8.25597941804984,12.4690426124586,118.62834052643));
#129987=CARTESIAN_POINT('Ctrl Pts',(4.50468353035287,6.74813242015876,119.365952199943));
#129988=CARTESIAN_POINT('Ctrl Pts',(3.19564570940331,1.55535306856081E-14,
119.672927882436));
#129989=CARTESIAN_POINT('Ctrl Pts',(4.5307307570029,-6.74813242015873,119.513673362895));
#129990=CARTESIAN_POINT('Ctrl Pts',(8.30807387134991,-12.4690426124586,
118.923782852334));
#129991=CARTESIAN_POINT('Ctrl Pts',(13.9550941963384,-16.2914328094368,
118.004217804321));
#129992=CARTESIAN_POINT('Ctrl Pts',(20.6137309353888,-17.633889172347,116.906277488381));
#129993=CARTESIAN_POINT('Ctrl Pts',(27.2723676744393,-16.2914328094368,
115.808337172442));
#129994=CARTESIAN_POINT('Ctrl Pts',(32.9193879994278,-12.4690426124586,
114.888772124429));
#129995=CARTESIAN_POINT('Ctrl Pts',(36.6967311137748,-6.74813242015874,
114.298881613867));
#129996=CARTESIAN_POINT('Ctrl Pts',(38.0318161613744,7.55992490830693E-15,
114.139627094327));
#129997=CARTESIAN_POINT('Ctrl Pts',(36.7227783404248,6.74813242015876,114.446602776819));
#129998=CARTESIAN_POINT('Ctrl Pts',(32.9714824527279,12.4690426124586,115.184214450332));
#129999=CARTESIAN_POINT('Ctrl Pts',(27.3505093543894,16.2914328094368,116.251500661297));
#130000=CARTESIAN_POINT('Ctrl Pts',(20.717919841989,17.633889172347,117.497162140189));
#130001=CARTESIAN_POINT('Ctrl Pts',(14.0853303295886,16.2914328094368,118.74282361908));
#130002=CARTESIAN_POINT('Ctrl Pts',(8.46435723125011,12.4690426124586,119.810109830045));
#130003=CARTESIAN_POINT('Ctrl Pts',(4.71306134355316,6.74813242015877,120.547721503558));
#130004=CARTESIAN_POINT('Ctrl Pts',(3.4040235226036,2.04385119939587E-14,
120.85469718605));
#130005=CARTESIAN_POINT('Ctrl Pts',(4.73910857020318,-6.74813242015873,
120.69544266651));
#130006=CARTESIAN_POINT('Ctrl Pts',(8.51645168455017,-12.4690426124586,
120.105552155948));
#130007=CARTESIAN_POINT('Ctrl Pts',(14.1634720095387,-16.2914328094368,
119.185987107935));
#130008=CARTESIAN_POINT('Ctrl Pts',(20.8221087485891,-17.633889172347,118.088046791996));
#130009=CARTESIAN_POINT('Ctrl Pts',(27.4807454876395,-16.2914328094368,
116.990106476056));
#130010=CARTESIAN_POINT('Ctrl Pts',(33.1277658126281,-12.4690426124586,
116.070541428043));
#130011=CARTESIAN_POINT('Ctrl Pts',(36.905108926975,-6.74813242015875,115.480650917482));
#130012=CARTESIAN_POINT('Ctrl Pts',(38.2401939745746,4.89538964920655E-15,
115.321396397941));
#130013=CARTESIAN_POINT('Ctrl Pts',(36.9311561536251,6.74813242015876,115.628372080434));
#130014=CARTESIAN_POINT('Ctrl Pts',(33.1798602659281,12.4690426124586,116.365983753947));
#130015=CARTESIAN_POINT('Ctrl Pts',(27.5588871675897,16.2914328094368,117.433269964912));
#130016=CARTESIAN_POINT('Ctrl Pts',(20.9262976551893,17.633889172347,118.678931443803));
#130017=CARTESIAN_POINT('Ctrl Pts',(14.293708142789,16.2914328094368,119.924592922695));
#130018=CARTESIAN_POINT('Ctrl Pts',(8.67273504445038,12.4690426124586,120.991879133659));
#130019=CARTESIAN_POINT('Ctrl Pts',(4.92143915675344,6.74813242015876,121.729490807172));
#130020=CARTESIAN_POINT('Ctrl Pts',(3.61240133580388,7.9058287694167E-14,
122.036466489665));
#130021=CARTESIAN_POINT('Ctrl Pts',(4.94748638340347,-6.74813242015874,
121.877211970124));
#130022=CARTESIAN_POINT('Ctrl Pts',(8.72482949775044,-12.4690426124586,
121.287321459563));
#130023=CARTESIAN_POINT('Ctrl Pts',(14.371849822739,-16.2914328094368,120.36775641155));
#130024=CARTESIAN_POINT('Ctrl Pts',(21.0304865617894,-17.633889172347,119.26981609561));
#130025=CARTESIAN_POINT('Ctrl Pts',(27.6891233008398,-16.2914328094368,
118.171875779671));
#130026=CARTESIAN_POINT('Ctrl Pts',(33.3361436258284,-12.4690426124586,
117.252310731658));
#130027=CARTESIAN_POINT('Ctrl Pts',(37.1134867401753,-6.74813242015876,
116.662420221097));
#130028=CARTESIAN_POINT('Ctrl Pts',(38.4485717877749,5.33011135228634E-14,
116.503165701556));
#130029=CARTESIAN_POINT('Ctrl Pts',(37.1395339668254,6.74813242015874,116.810141384049));
#130030=CARTESIAN_POINT('Ctrl Pts',(33.3882380791284,12.4690426124586,117.547753057562));
#130031=CARTESIAN_POINT('Ctrl Pts',(27.7672649807899,16.2914328094368,118.615039268526));
#130032=CARTESIAN_POINT('Ctrl Pts',(21.1346754683896,17.633889172347,119.860700747418));
#130033=CARTESIAN_POINT('Ctrl Pts',(14.5020859559892,16.2914328094368,121.106362226309));
#130034=CARTESIAN_POINT('Ctrl Pts',(8.88111285765067,12.4690426124586,122.173648437274));
#130035=CARTESIAN_POINT('Ctrl Pts',(5.12981696995372,6.74813242015876,122.911260110787));
#130036=CARTESIAN_POINT('Ctrl Pts',(3.82077914900416,8.30550905828176E-14,
123.21823579328));
#130037=CARTESIAN_POINT('Ctrl Pts',(5.15586419660375,-6.74813242015874,
123.058981273739));
#130038=CARTESIAN_POINT('Ctrl Pts',(8.93320731095072,-12.4690426124585,
122.469090763178));
#130039=CARTESIAN_POINT('Ctrl Pts',(14.5802276359393,-16.2914328094368,
121.549525715165));
#130040=CARTESIAN_POINT('Ctrl Pts',(21.2388643749897,-17.633889172347,120.451585399225));
#130041=CARTESIAN_POINT('Ctrl Pts',(27.89750111404,-16.2914328094368,119.353645083286));
#130042=CARTESIAN_POINT('Ctrl Pts',(33.5445214390286,-12.4690426124586,
118.434080035273));
#130043=CARTESIAN_POINT('Ctrl Pts',(37.3218645533756,-6.74813242015877,
117.844189524711));
#130044=CARTESIAN_POINT('Ctrl Pts',(38.6569496009752,4.93043106342128E-14,
117.684935005171));
#130045=CARTESIAN_POINT('Ctrl Pts',(37.3479117800257,6.74813242015873,117.991910687663));
#130046=CARTESIAN_POINT('Ctrl Pts',(33.5966158923287,12.4690426124586,118.729522361176));
#130047=CARTESIAN_POINT('Ctrl Pts',(27.9756427939902,16.2914328094368,119.796808572141));
#130048=CARTESIAN_POINT('Ctrl Pts',(21.3430532815898,17.633889172347,121.042470051032));
#130049=CARTESIAN_POINT('Ctrl Pts',(14.7104637691895,16.2914328094368,122.288131529924));
#130050=CARTESIAN_POINT('Ctrl Pts',(9.08949067085095,12.4690426124586,123.355417740889));
#130051=CARTESIAN_POINT('Ctrl Pts',(5.33819478315401,6.74813242015877,124.093029414402));
#130052=CARTESIAN_POINT('Ctrl Pts',(4.02915696220445,8.70518934714681E-14,
124.400005096894));
#130053=CARTESIAN_POINT('Ctrl Pts',(5.36424200980403,-6.74813242015873,
124.240750577354));
#130054=CARTESIAN_POINT('Ctrl Pts',(9.141585124151,-12.4690426124585,123.650860066792));
#130055=CARTESIAN_POINT('Ctrl Pts',(14.7886054491396,-16.2914328094368,
122.731295018779));
#130056=CARTESIAN_POINT('Ctrl Pts',(21.4472421881899,-17.633889172347,121.63335470284));
#130057=CARTESIAN_POINT('Ctrl Pts',(26.7715870880817,-16.5604411124356,
120.755425308182));
#130058=CARTESIAN_POINT('Ctrl Pts',(29.5464702774019,-15.1257033979806,
120.301649134085));
#130059=CARTESIAN_POINT('Ctrl Pts',(30.3017625288241,-14.6570228943777,
120.178595667035));
#130060=CARTESIAN_POINT('Ctrl Pts',(20.311092103448,-16.2461987828381,115.189927382884));
#130061=CARTESIAN_POINT('Ctrl Pts',(22.4097475821195,-16.2461987828381,
114.84526346408));
#130062=CARTESIAN_POINT('Ctrl Pts',(26.6061717911932,-15.4001884409061,
114.156091984117));
#130063=CARTESIAN_POINT('Ctrl Pts',(31.9449768781284,-11.7869071527165,
113.290873598438));
#130064=CARTESIAN_POINT('Ctrl Pts',(35.5163879178765,-6.37896691532468,
112.737294468822));
#130065=CARTESIAN_POINT('Ctrl Pts',(36.7791478469962,1.33330846363577E-14,
112.590792819052));
#130066=CARTESIAN_POINT('Ctrl Pts',(35.5424351445265,6.3789669153247,112.885015631774));
#130067=CARTESIAN_POINT('Ctrl Pts',(31.9970713314284,11.7869071527165,113.586315924342));
#130068=CARTESIAN_POINT('Ctrl Pts',(26.6843134711433,15.4001884409061,114.599255472972));
#130069=CARTESIAN_POINT('Ctrl Pts',(20.4152810100481,16.6692039538042,115.780812034692));
#130070=CARTESIAN_POINT('Ctrl Pts',(14.146248548953,15.4001884409061,116.962368596411));
#130071=CARTESIAN_POINT('Ctrl Pts',(8.83349068866784,11.7869071527165,117.975308145042));
#130072=CARTESIAN_POINT('Ctrl Pts',(5.28812687556977,6.37896691532472,118.67660843761));
#130073=CARTESIAN_POINT('Ctrl Pts',(4.05141417310005,1.59976198954581E-14,
118.970831250331));
#130074=CARTESIAN_POINT('Ctrl Pts',(5.31417410221981,-6.37896691532469,
118.824329600562));
#130075=CARTESIAN_POINT('Ctrl Pts',(8.88558514196791,-11.7869071527165,
118.270750470945));
#130076=CARTESIAN_POINT('Ctrl Pts',(14.2243902289031,-15.4001884409061,
117.405532085267));
#130077=CARTESIAN_POINT('Ctrl Pts',(20.5194699166483,-16.6692039538041,
116.371696686499));
#130078=CARTESIAN_POINT('Ctrl Pts',(26.8145496043935,-15.4001884409061,
115.337861287731));
#130079=CARTESIAN_POINT('Ctrl Pts',(32.1533546913286,-11.7869071527165,
114.472642902053));
#130080=CARTESIAN_POINT('Ctrl Pts',(35.7247657310767,-6.3789669153247,113.919063772437));
#130081=CARTESIAN_POINT('Ctrl Pts',(36.9875256601965,7.55992490830693E-15,
113.772562122667));
#130082=CARTESIAN_POINT('Ctrl Pts',(35.7508129577268,6.37896691532472,114.066784935388));
#130083=CARTESIAN_POINT('Ctrl Pts',(32.2054491446287,11.7869071527165,114.768085227956));
#130084=CARTESIAN_POINT('Ctrl Pts',(26.8926912843436,15.4001884409061,115.781024776587));
#130085=CARTESIAN_POINT('Ctrl Pts',(20.6236588232484,16.6692039538042,116.962581338306));
#130086=CARTESIAN_POINT('Ctrl Pts',(14.3546263621533,15.4001884409061,118.144137900026));
#130087=CARTESIAN_POINT('Ctrl Pts',(9.04186850186811,11.7869071527165,119.157077448656));
#130088=CARTESIAN_POINT('Ctrl Pts',(5.49650468877006,6.37896691532473,119.858377741224));
#130089=CARTESIAN_POINT('Ctrl Pts',(4.25979198630033,2.04385119939587E-14,
120.152600553946));
#130090=CARTESIAN_POINT('Ctrl Pts',(5.52255191542009,-6.37896691532469,
120.006098904176));
#130091=CARTESIAN_POINT('Ctrl Pts',(9.09396295516817,-11.7869071527165,
119.45251977456));
#130092=CARTESIAN_POINT('Ctrl Pts',(14.4327680421034,-15.4001884409061,
118.587301388881));
#130093=CARTESIAN_POINT('Ctrl Pts',(20.7278477298486,-16.6692039538041,
117.553465990114));
#130094=CARTESIAN_POINT('Ctrl Pts',(27.0229274175937,-15.4001884409061,
116.519630591346));
#130095=CARTESIAN_POINT('Ctrl Pts',(32.3617325045289,-11.7869071527165,
115.654412205667));
#130096=CARTESIAN_POINT('Ctrl Pts',(35.933143544277,-6.3789669153247,115.100833076051));
#130097=CARTESIAN_POINT('Ctrl Pts',(37.1959034733968,5.33947885905661E-15,
114.954331426281));
#130098=CARTESIAN_POINT('Ctrl Pts',(35.9591907709271,6.37896691532471,115.248554239003));
#130099=CARTESIAN_POINT('Ctrl Pts',(32.413826957829,11.7869071527165,115.949854531571));
#130100=CARTESIAN_POINT('Ctrl Pts',(27.1010690975439,15.4001884409061,116.962794080202));
#130101=CARTESIAN_POINT('Ctrl Pts',(20.8320366364487,16.6692039538041,118.144350641921));
#130102=CARTESIAN_POINT('Ctrl Pts',(14.5630041753536,15.4001884409062,119.325907203641));
#130103=CARTESIAN_POINT('Ctrl Pts',(9.25024631506838,11.7869071527165,120.338846752271));
#130104=CARTESIAN_POINT('Ctrl Pts',(5.70488250197034,6.37896691532472,121.040147044839));
#130105=CARTESIAN_POINT('Ctrl Pts',(4.46816979950061,7.50614848055164E-14,
121.334369857561));
#130106=CARTESIAN_POINT('Ctrl Pts',(5.73092972862037,-6.3789669153247,121.187868207791));
#130107=CARTESIAN_POINT('Ctrl Pts',(9.30234076836844,-11.7869071527165,
120.634289078175));
#130108=CARTESIAN_POINT('Ctrl Pts',(14.6411458553037,-15.4001884409061,
119.769070692496));
#130109=CARTESIAN_POINT('Ctrl Pts',(20.9362255430488,-16.6692039538041,
118.735235293728));
#130110=CARTESIAN_POINT('Ctrl Pts',(27.231305230794,-15.4001884409061,117.701399894961));
#130111=CARTESIAN_POINT('Ctrl Pts',(32.5701103177292,-11.7869071527165,
116.836181509282));
#130112=CARTESIAN_POINT('Ctrl Pts',(36.1415213574773,-6.37896691532472,
116.282602379666));
#130113=CARTESIAN_POINT('Ctrl Pts',(37.4042812865971,5.15247566834631E-14,
116.136100729896));
#130114=CARTESIAN_POINT('Ctrl Pts',(36.1675685841274,6.3789669153247,116.430323542618));
#130115=CARTESIAN_POINT('Ctrl Pts',(32.6222047710293,11.7869071527165,117.131623835186));
#130116=CARTESIAN_POINT('Ctrl Pts',(27.3094469107441,15.4001884409062,118.144563383816));
#130117=CARTESIAN_POINT('Ctrl Pts',(21.040414449649,16.6692039538041,119.326119945536));
#130118=CARTESIAN_POINT('Ctrl Pts',(14.7713819885539,15.4001884409062,120.507676507255));
#130119=CARTESIAN_POINT('Ctrl Pts',(9.45862412826867,11.7869071527165,121.520616055886));
#130120=CARTESIAN_POINT('Ctrl Pts',(5.91326031517062,6.37896691532472,122.221916348454));
#130121=CARTESIAN_POINT('Ctrl Pts',(4.6765476127009,7.9058287694167E-14,
122.516139161175));
#130122=CARTESIAN_POINT('Ctrl Pts',(5.93930754182065,-6.37896691532469,
122.369637511406));
#130123=CARTESIAN_POINT('Ctrl Pts',(9.51071858156872,-11.7869071527165,
121.816058381789));
#130124=CARTESIAN_POINT('Ctrl Pts',(14.849523668504,-15.4001884409061,120.950839996111));
#130125=CARTESIAN_POINT('Ctrl Pts',(21.1446033562491,-16.6692039538041,
119.917004597343));
#130126=CARTESIAN_POINT('Ctrl Pts',(27.4396830439942,-15.4001884409061,
118.883169198575));
#130127=CARTESIAN_POINT('Ctrl Pts',(32.7784881309295,-11.7869071527165,
118.017950812897));
#130128=CARTESIAN_POINT('Ctrl Pts',(36.3498991706776,-6.37896691532472,
117.464371683281));
#130129=CARTESIAN_POINT('Ctrl Pts',(37.6126590997973,4.70838645849625E-14,
117.317870033511));
#130130=CARTESIAN_POINT('Ctrl Pts',(36.3759463973276,6.37896691532469,117.612092846232));
#130131=CARTESIAN_POINT('Ctrl Pts',(32.8305825842296,11.7869071527165,118.3133931388));
#130132=CARTESIAN_POINT('Ctrl Pts',(27.5178247239444,15.4001884409062,119.326332687431));
#130133=CARTESIAN_POINT('Ctrl Pts',(21.2487922628493,16.6692039538041,120.50788924915));
#130134=CARTESIAN_POINT('Ctrl Pts',(14.9797598017542,15.4001884409062,121.68944581087));
#130135=CARTESIAN_POINT('Ctrl Pts',(9.66700194146895,11.7869071527165,122.7023853595));
#130136=CARTESIAN_POINT('Ctrl Pts',(6.12163812837091,6.37896691532473,123.403685652068));
#130137=CARTESIAN_POINT('Ctrl Pts',(4.88492542590118,8.26110013729675E-14,
123.69790846479));
#130138=CARTESIAN_POINT('Ctrl Pts',(6.14768535502093,-6.37896691532469,
123.55140681502));
#130139=CARTESIAN_POINT('Ctrl Pts',(9.719096394769,-11.7869071527165,122.997827685404));
#130140=CARTESIAN_POINT('Ctrl Pts',(15.0579014817043,-15.4001884409061,
122.132609299725));
#130141=CARTESIAN_POINT('Ctrl Pts',(21.3529811694494,-16.6692039538041,
121.098773900958));
#130142=CARTESIAN_POINT('Ctrl Pts',(26.3866204477858,-15.6544802890701,
120.272103750824));
#130143=CARTESIAN_POINT('Ctrl Pts',(29.0100321973966,-14.2982317979562,
119.845036078354));
#130144=CARTESIAN_POINT('Ctrl Pts',(29.7240999098662,-13.8551910808817,
119.729251609789));
#130145=CARTESIAN_POINT('',(29.803853834021,-13.9658945114651,119.791289468368));
#130146=CARTESIAN_POINT('Ctrl Pts',(20.5130133806899,-16.2461987828381,
116.335079851501));
#130147=CARTESIAN_POINT('Ctrl Pts',(22.6116688593615,-16.2461987828381,
115.990415932697));
#130148=CARTESIAN_POINT('Ctrl Pts',(26.8080930684351,-15.4001884409061,
115.301244452733));
#130149=CARTESIAN_POINT('Ctrl Pts',(32.1468981553703,-11.7869071527165,
114.436026067055));
#130150=CARTESIAN_POINT('Ctrl Pts',(35.7183091951184,-6.37896691532468,
113.882446937438));
#130151=CARTESIAN_POINT('Ctrl Pts',(36.9810691242382,1.33330846363577E-14,
113.735945287669));
#130152=CARTESIAN_POINT('Ctrl Pts',(35.7443564217685,6.3789669153247,114.03016810039));
#130153=CARTESIAN_POINT('Ctrl Pts',(32.1989926086704,11.7869071527165,114.731468392958));
#130154=CARTESIAN_POINT('Ctrl Pts',(26.8862347483852,15.4001884409061,115.744407941589));
#130155=CARTESIAN_POINT('Ctrl Pts',(20.6172022872901,16.6692039538042,116.925964503308));
#130156=CARTESIAN_POINT('Ctrl Pts',(14.348169826195,15.4001884409061,118.107521065028));
#130157=CARTESIAN_POINT('Ctrl Pts',(9.03541196590979,11.7869071527165,119.120460613658));
#130158=CARTESIAN_POINT('Ctrl Pts',(5.49004815281173,6.37896691532472,119.821760906226));
#130159=CARTESIAN_POINT('Ctrl Pts',(4.253335450342,1.59976198954581E-14,
120.115983718948));
#130160=CARTESIAN_POINT('Ctrl Pts',(5.51609537946176,-6.37896691532469,
119.969482069178));
#130161=CARTESIAN_POINT('Ctrl Pts',(9.08750641920986,-11.7869071527165,
119.415902939562));
#130162=CARTESIAN_POINT('Ctrl Pts',(14.426311506145,-15.4001884409061,118.550684553883));
#130163=CARTESIAN_POINT('Ctrl Pts',(20.7213911938902,-16.6692039538041,
117.516849155116));
#130164=CARTESIAN_POINT('Ctrl Pts',(27.0164708816354,-15.4001884409061,
116.483013756348));
#130165=CARTESIAN_POINT('Ctrl Pts',(32.3552759685706,-11.7869071527165,
115.617795370669));
#130166=CARTESIAN_POINT('Ctrl Pts',(35.9266870083187,-6.3789669153247,115.064216241053));
#130167=CARTESIAN_POINT('Ctrl Pts',(37.1894469374384,7.55992490830693E-15,
114.917714591283));
#130168=CARTESIAN_POINT('Ctrl Pts',(35.9527342349687,6.37896691532472,115.211937404005));
#130169=CARTESIAN_POINT('Ctrl Pts',(32.4073704218707,11.7869071527165,115.913237696573));
#130170=CARTESIAN_POINT('Ctrl Pts',(27.0946125615855,15.4001884409061,116.926177245203));
#130171=CARTESIAN_POINT('Ctrl Pts',(20.8255801004904,16.6692039538042,118.107733806923));
#130172=CARTESIAN_POINT('Ctrl Pts',(14.5565476393952,15.4001884409061,119.289290368642));
#130173=CARTESIAN_POINT('Ctrl Pts',(9.24378977911006,11.7869071527165,120.302229917273));
#130174=CARTESIAN_POINT('Ctrl Pts',(5.69842596601202,6.37896691532473,121.003530209841));
#130175=CARTESIAN_POINT('Ctrl Pts',(4.46171326354229,2.04385119939587E-14,
121.297753022563));
#130176=CARTESIAN_POINT('Ctrl Pts',(5.72447319266205,-6.37896691532469,
121.151251372793));
#130177=CARTESIAN_POINT('Ctrl Pts',(9.29588423241012,-11.7869071527165,
120.597672243177));
#130178=CARTESIAN_POINT('Ctrl Pts',(14.6346893193453,-15.4001884409061,
119.732453857498));
#130179=CARTESIAN_POINT('Ctrl Pts',(20.9297690070905,-16.6692039538041,
118.69861845873));
#130180=CARTESIAN_POINT('Ctrl Pts',(27.2248486948357,-15.4001884409061,
117.664783059963));
#130181=CARTESIAN_POINT('Ctrl Pts',(32.5636537817709,-11.7869071527165,
116.799564674284));
#130182=CARTESIAN_POINT('Ctrl Pts',(36.135064821519,-6.3789669153247,116.245985544668));
#130183=CARTESIAN_POINT('Ctrl Pts',(37.3978247506387,5.33947885905661E-15,
116.099483894898));
#130184=CARTESIAN_POINT('Ctrl Pts',(36.161112048169,6.37896691532471,116.39370670762));
#130185=CARTESIAN_POINT('Ctrl Pts',(32.615748235071,11.7869071527165,117.095007000188));
#130186=CARTESIAN_POINT('Ctrl Pts',(27.3029903747858,15.4001884409061,118.107946548818));
#130187=CARTESIAN_POINT('Ctrl Pts',(21.0339579136907,16.6692039538041,119.289503110538));
#130188=CARTESIAN_POINT('Ctrl Pts',(14.7649254525956,15.4001884409062,120.471059672257));
#130189=CARTESIAN_POINT('Ctrl Pts',(9.45216759231034,11.7869071527165,121.483999220888));
#130190=CARTESIAN_POINT('Ctrl Pts',(5.9068037792123,6.37896691532472,122.185299513456));
#130191=CARTESIAN_POINT('Ctrl Pts',(4.67009107674257,7.50614848055164E-14,
122.479522326177));
#130192=CARTESIAN_POINT('Ctrl Pts',(5.93285100586233,-6.3789669153247,122.333020676407));
#130193=CARTESIAN_POINT('Ctrl Pts',(9.50426204561039,-11.7869071527165,
121.779441546791));
#130194=CARTESIAN_POINT('Ctrl Pts',(14.8430671325457,-15.4001884409061,
120.914223161113));
#130195=CARTESIAN_POINT('Ctrl Pts',(21.1381468202908,-16.6692039538041,
119.880387762345));
#130196=CARTESIAN_POINT('Ctrl Pts',(27.4332265080359,-15.4001884409061,
118.846552363577));
#130197=CARTESIAN_POINT('Ctrl Pts',(32.7720315949712,-11.7869071527165,
117.981333977899));
#130198=CARTESIAN_POINT('Ctrl Pts',(36.3434426347193,-6.37896691532472,
117.427754848282));
#130199=CARTESIAN_POINT('Ctrl Pts',(37.606202563839,5.15247566834631E-14,
117.281253198513));
#130200=CARTESIAN_POINT('Ctrl Pts',(36.3694898613693,6.3789669153247,117.575476011234));
#130201=CARTESIAN_POINT('Ctrl Pts',(32.8241260482713,11.7869071527165,118.276776303802));
#130202=CARTESIAN_POINT('Ctrl Pts',(27.511368187986,15.4001884409062,119.289715852433));
#130203=CARTESIAN_POINT('Ctrl Pts',(21.242335726891,16.6692039538041,120.471272414152));
#130204=CARTESIAN_POINT('Ctrl Pts',(14.9733032657959,15.4001884409062,121.652828975872));
#130205=CARTESIAN_POINT('Ctrl Pts',(9.66054540551062,11.7869071527165,122.665768524502));
#130206=CARTESIAN_POINT('Ctrl Pts',(6.11518159241258,6.37896691532472,123.36706881707));
#130207=CARTESIAN_POINT('Ctrl Pts',(4.87846888994285,7.9058287694167E-14,
123.661291629792));
#130208=CARTESIAN_POINT('Ctrl Pts',(6.14122881906261,-6.37896691532469,
123.514789980022));
#130209=CARTESIAN_POINT('Ctrl Pts',(9.71263985881067,-11.7869071527165,
122.961210850406));
#130210=CARTESIAN_POINT('Ctrl Pts',(15.0514449457459,-15.4001884409061,
122.095992464727));
#130211=CARTESIAN_POINT('Ctrl Pts',(21.3465246334911,-16.6692039538041,
121.06215706596));
#130212=CARTESIAN_POINT('Ctrl Pts',(27.6416043212362,-15.4001884409061,
120.028321667192));
#130213=CARTESIAN_POINT('Ctrl Pts',(32.9804094081715,-11.7869071527165,
119.163103281513));
#130214=CARTESIAN_POINT('Ctrl Pts',(36.5518204479195,-6.37896691532472,
118.609524151897));
#130215=CARTESIAN_POINT('Ctrl Pts',(37.8145803770393,4.70838645849625E-14,
118.463022502127));
#130216=CARTESIAN_POINT('Ctrl Pts',(36.5778676745696,6.37896691532469,118.757245314849));
#130217=CARTESIAN_POINT('Ctrl Pts',(33.0325038614716,11.7869071527165,119.458545607417));
#130218=CARTESIAN_POINT('Ctrl Pts',(27.7197460011863,15.4001884409062,120.471485156047));
#130219=CARTESIAN_POINT('Ctrl Pts',(21.4507135400912,16.6692039538041,121.653041717767));
#130220=CARTESIAN_POINT('Ctrl Pts',(15.1816810789961,15.4001884409062,122.834598279486));
#130221=CARTESIAN_POINT('Ctrl Pts',(9.86892321871091,11.7869071527165,123.847537828117));
#130222=CARTESIAN_POINT('Ctrl Pts',(6.32355940561287,6.37896691532473,124.548838120685));
#130223=CARTESIAN_POINT('Ctrl Pts',(5.08684670314314,8.26110013729675E-14,
124.843060933407));
#130224=CARTESIAN_POINT('Ctrl Pts',(6.34960663226289,-6.37896691532469,
124.696559283637));
#130225=CARTESIAN_POINT('Ctrl Pts',(9.92101767201095,-11.7869071527165,
124.142980154021));
#130226=CARTESIAN_POINT('Ctrl Pts',(15.2598227589462,-15.4001884409061,
123.277761768342));
#130227=CARTESIAN_POINT('Ctrl Pts',(21.5549024466913,-16.6692039538041,
122.243926369574));
#130228=CARTESIAN_POINT('Ctrl Pts',(26.5885417250278,-15.6544802890701,
121.417256219441));
#130229=CARTESIAN_POINT('Ctrl Pts',(29.2119534746386,-14.2982317979562,
120.99018854697));
#130230=CARTESIAN_POINT('Ctrl Pts',(29.9260211871081,-13.8551910808817,
120.874404078406));
#130231=CARTESIAN_POINT('Ctrl Pts',(20.4187523619494,-17.1864037180436,
115.800499049619));
#130232=CARTESIAN_POINT('Ctrl Pts',(22.6386106304441,-17.1864037180436,
115.434463808832));
#130233=CARTESIAN_POINT('Ctrl Pts',(27.0773891009998,-16.2914328094368,
114.702558733679));
#130234=CARTESIAN_POINT('Ctrl Pts',(32.7244094259883,-12.4690426124586,
113.782993685666));
#130235=CARTESIAN_POINT('Ctrl Pts',(36.5017525403353,-6.74813242015872,
113.193103175105));
#130236=CARTESIAN_POINT('Ctrl Pts',(37.8368375879349,1.42212630560579E-14,
113.033848655564));
#130237=CARTESIAN_POINT('Ctrl Pts',(36.5277997669854,6.74813242015874,113.340824338057));
#130238=CARTESIAN_POINT('Ctrl Pts',(32.7765038792884,12.4690426124586,114.07843601157));
#130239=CARTESIAN_POINT('Ctrl Pts',(27.1555307809499,16.2914328094368,115.145722222535));
#130240=CARTESIAN_POINT('Ctrl Pts',(20.5229412685495,17.633889172347,116.391383701426));
#130241=CARTESIAN_POINT('Ctrl Pts',(13.8903517561492,16.2914328094368,117.637045180318));
#130242=CARTESIAN_POINT('Ctrl Pts',(8.26937865781067,12.4690426124586,118.704331391282));
#130243=CARTESIAN_POINT('Ctrl Pts',(4.5180827701137,6.74813242015876,119.441943064795));
#130244=CARTESIAN_POINT('Ctrl Pts',(3.20904494916414,1.55535306856081E-14,
119.748918747288));
#130245=CARTESIAN_POINT('Ctrl Pts',(4.54412999676373,-6.74813242015873,
119.589664227747));
#130246=CARTESIAN_POINT('Ctrl Pts',(8.32147311111074,-12.4690426124586,
118.999773717186));
#130247=CARTESIAN_POINT('Ctrl Pts',(13.9684934360992,-16.2914328094368,
118.080208669173));
#130248=CARTESIAN_POINT('Ctrl Pts',(20.6271301751497,-17.633889172347,116.982268353233));
#130249=CARTESIAN_POINT('Ctrl Pts',(27.2857669142001,-16.2914328094368,
115.884328037294));
#130250=CARTESIAN_POINT('Ctrl Pts',(32.9327872391886,-12.4690426124586,
114.964762989281));
#130251=CARTESIAN_POINT('Ctrl Pts',(36.7101303535356,-6.74813242015874,
114.37487247872));
#130252=CARTESIAN_POINT('Ctrl Pts',(38.0452154011352,7.55992490830693E-15,
114.215617959179));
#130253=CARTESIAN_POINT('Ctrl Pts',(36.7361775801856,6.74813242015876,114.522593641672));
#130254=CARTESIAN_POINT('Ctrl Pts',(32.9848816924887,12.4690426124586,115.260205315185));
#130255=CARTESIAN_POINT('Ctrl Pts',(27.3639085941502,16.2914328094368,116.327491526149));
#130256=CARTESIAN_POINT('Ctrl Pts',(20.7313190817498,17.633889172347,117.573153005041));
#130257=CARTESIAN_POINT('Ctrl Pts',(14.0987295693494,16.2914328094368,118.818814483932));
#130258=CARTESIAN_POINT('Ctrl Pts',(8.47775647101094,12.4690426124586,119.886100694897));
#130259=CARTESIAN_POINT('Ctrl Pts',(4.72646058331399,6.74813242015877,120.62371236841));
#130260=CARTESIAN_POINT('Ctrl Pts',(3.41742276236443,2.04385119939587E-14,
120.930688050903));
#130261=CARTESIAN_POINT('Ctrl Pts',(4.75250780996401,-6.74813242015873,
120.771433531362));
#130262=CARTESIAN_POINT('Ctrl Pts',(8.529850924311,-12.4690426124586,120.181543020801));
#130263=CARTESIAN_POINT('Ctrl Pts',(14.1768712492995,-16.2914328094368,
119.261977972788));
#130264=CARTESIAN_POINT('Ctrl Pts',(20.8355079883499,-17.633889172347,118.164037656848));
#130265=CARTESIAN_POINT('Ctrl Pts',(27.4941447274004,-16.2914328094368,
117.066097340909));
#130266=CARTESIAN_POINT('Ctrl Pts',(33.1411650523889,-12.4690426124586,
116.146532292896));
#130267=CARTESIAN_POINT('Ctrl Pts',(36.9185081667359,-6.74813242015875,
115.556641782334));
#130268=CARTESIAN_POINT('Ctrl Pts',(38.2535932143355,4.89538964920655E-15,
115.397387262794));
#130269=CARTESIAN_POINT('Ctrl Pts',(36.9445553933859,6.74813242015876,115.704362945286));
#130270=CARTESIAN_POINT('Ctrl Pts',(33.193259505689,12.4690426124586,116.441974618799));
#130271=CARTESIAN_POINT('Ctrl Pts',(27.5722864073505,16.2914328094368,117.509260829764));
#130272=CARTESIAN_POINT('Ctrl Pts',(20.9396968949501,17.633889172347,118.754922308655));
#130273=CARTESIAN_POINT('Ctrl Pts',(14.3071073825498,16.2914328094368,120.000583787547));
#130274=CARTESIAN_POINT('Ctrl Pts',(8.68613428421121,12.4690426124586,121.067869998512));
#130275=CARTESIAN_POINT('Ctrl Pts',(4.93483839651427,6.74813242015876,121.805481672025));
#130276=CARTESIAN_POINT('Ctrl Pts',(3.62580057556471,7.9058287694167E-14,
122.112457354517));
#130277=CARTESIAN_POINT('Ctrl Pts',(4.9608856231643,-6.74813242015874,121.953202834977));
#130278=CARTESIAN_POINT('Ctrl Pts',(8.73822873751127,-12.4690426124586,
121.363312324415));
#130279=CARTESIAN_POINT('Ctrl Pts',(14.3852490624999,-16.2914328094368,
120.443747276402));
#130280=CARTESIAN_POINT('Ctrl Pts',(21.0438858015502,-17.633889172347,119.345806960463));
#130281=CARTESIAN_POINT('Ctrl Pts',(27.7025225406006,-16.2914328094368,
118.247866644523));
#130282=CARTESIAN_POINT('Ctrl Pts',(33.3495428655892,-12.4690426124586,
117.32830159651));
#130283=CARTESIAN_POINT('Ctrl Pts',(37.1268859799362,-6.74813242015876,
116.738411085949));
#130284=CARTESIAN_POINT('Ctrl Pts',(38.4619710275358,5.33011135228634E-14,
116.579156566408));
#130285=CARTESIAN_POINT('Ctrl Pts',(37.1529332065862,6.74813242015874,116.886132248901));
#130286=CARTESIAN_POINT('Ctrl Pts',(33.4016373188893,12.4690426124586,117.623743922414));
#130287=CARTESIAN_POINT('Ctrl Pts',(27.7806642205507,16.2914328094368,118.691030133379));
#130288=CARTESIAN_POINT('Ctrl Pts',(21.1480747081504,17.633889172347,119.93669161227));
#130289=CARTESIAN_POINT('Ctrl Pts',(14.5154851957501,16.2914328094368,121.182353091162));
#130290=CARTESIAN_POINT('Ctrl Pts',(8.8945120974115,12.4690426124586,122.249639302126));
#130291=CARTESIAN_POINT('Ctrl Pts',(5.14321620971455,6.74813242015876,122.987250975639));
#130292=CARTESIAN_POINT('Ctrl Pts',(3.83417838876499,8.30550905828176E-14,
123.294226658132));
#130293=CARTESIAN_POINT('Ctrl Pts',(5.16926343636458,-6.74813242015874,
123.134972138591));
#130294=CARTESIAN_POINT('Ctrl Pts',(8.94660655071155,-12.4690426124585,
122.54508162803));
#130295=CARTESIAN_POINT('Ctrl Pts',(14.5936268757001,-16.2914328094368,
121.625516580017));
#130296=CARTESIAN_POINT('Ctrl Pts',(21.2522636147505,-17.633889172347,120.527576264077));
#130297=CARTESIAN_POINT('Ctrl Pts',(27.9109003538009,-16.2914328094368,
119.429635948138));
#130298=CARTESIAN_POINT('Ctrl Pts',(33.5579206787895,-12.4690426124586,
118.510070900125));
#130299=CARTESIAN_POINT('Ctrl Pts',(37.3352637931364,-6.74813242015877,
117.920180389564));
#130300=CARTESIAN_POINT('Ctrl Pts',(38.670348840736,4.93043106342128E-14,
117.760925870023));
#130301=CARTESIAN_POINT('Ctrl Pts',(37.3613110197865,6.74813242015873,118.067901552516));
#130302=CARTESIAN_POINT('Ctrl Pts',(33.6100151320896,12.4690426124586,118.805513226029));
#130303=CARTESIAN_POINT('Ctrl Pts',(27.989042033751,16.2914328094368,119.872799436993));
#130304=CARTESIAN_POINT('Ctrl Pts',(21.3564525213507,17.633889172347,121.118460915885));
#130305=CARTESIAN_POINT('Ctrl Pts',(14.7238630089504,16.2914328094368,122.364122394776));
#130306=CARTESIAN_POINT('Ctrl Pts',(9.10288991061178,12.4690426124586,123.431408605741));
#130307=CARTESIAN_POINT('Ctrl Pts',(5.35159402291484,6.74813242015877,124.169020279254));
#130308=CARTESIAN_POINT('Ctrl Pts',(4.04255620196528,8.70518934714681E-14,
124.475995961747));
#130309=CARTESIAN_POINT('Ctrl Pts',(5.37764124956486,-6.74813242015873,
124.316741442206));
#130310=CARTESIAN_POINT('Ctrl Pts',(9.15498436391183,-12.4690426124585,
123.726850931645));
#130311=CARTESIAN_POINT('Ctrl Pts',(14.8020046889004,-16.2914328094368,
122.807285883632));
#130312=CARTESIAN_POINT('Ctrl Pts',(21.4606414279508,-17.633889172347,121.709345567692));
#130313=CARTESIAN_POINT('Ctrl Pts',(26.7849863278426,-16.5604411124356,
120.831416173035));
#130314=CARTESIAN_POINT('Ctrl Pts',(29.5598695171627,-15.1257033979806,
120.377639998937));
#130315=CARTESIAN_POINT('Ctrl Pts',(30.315161768585,-14.6570228943777,120.254586531888));
#130316=CARTESIAN_POINT('',(30.2384437550856,-14.4989439202996,120.376781885352));
#130317=CARTESIAN_POINT('Origin',(29.8250605484872,-13.8551910808817,120.301827844097));
#130318=CARTESIAN_POINT('Origin',(22.6000197806719,1.4210854715202E-14,
128.171081305147));
#130319=CARTESIAN_POINT('Origin',(20.5162416486691,1.4210854715202E-14,
116.353388269));
#130320=CARTESIAN_POINT('Origin',(13.6416661832291,-6.,84.56419651818));
#130321=CARTESIAN_POINT('',(-5.0395856121756,-6.,84.304212101522));
#130322=CARTESIAN_POINT('',(-6.7204718626933,-5.99999999998125,84.6005928870242));
#130323=CARTESIAN_POINT('',(-0.312555071850913,-6.,83.47070907863));
#130324=CARTESIAN_POINT('',(-7.47066009951181,-6.,70.5169035593534));
#130325=CARTESIAN_POINT('',(-7.47066009951181,-6.,70.5169035593534));
#130326=CARTESIAN_POINT('',(22.1743288589254,-6.0000000159505,65.2896921631773));
#130327=CARTESIAN_POINT('',(10.6028230740595,-6.,67.3300608404729));
#130328=CARTESIAN_POINT('',(21.4524700019691,-6.,61.19591303503));
#130329=CARTESIAN_POINT('',(22.8689360308591,-6.00000009375099,69.228922547753));
#130330=CARTESIAN_POINT('',(21.7837557160991,-6.00001782727999,59.21971079975));
#130331=CARTESIAN_POINT('Origin',(24.4068932609991,-6.,60.67496850203));
#130332=CARTESIAN_POINT('',(-2.24980788089431,-5.99999999999387,55.9944999784261));
#130333=CARTESIAN_POINT('Origin',(1.07038457110909,-5.99999999998499,122.41156512159));
#130334=CARTESIAN_POINT('',(-6.16760615831108,-5.99999999999855,58.7310775215164));
#130335=CARTESIAN_POINT('Origin',(-2.02513312664091,-5.99999999999799,60.48888938658));
#130336=CARTESIAN_POINT('',(-7.28284231406048,-5.99999999998002,84.26262682962));
#130337=CARTESIAN_POINT('Origin',(27.4324635166691,-5.99999999999899,72.98888938658));
#130338=CARTESIAN_POINT('Origin',(-6.80729512863291,-5.99999999995499,84.10819367738));
#130339=CARTESIAN_POINT('Origin',(-9.10739291134991,6.,88.57546942229));
#130340=CARTESIAN_POINT('',(-7.47066009951181,6.,70.5169035593534));
#130341=CARTESIAN_POINT('',(22.1746244425332,5.99999996177058,65.2896400438122));
#130342=CARTESIAN_POINT('',(-12.1462360205204,6.,71.3413337445779));
#130343=CARTESIAN_POINT('',(-5.03958561217587,6.,84.3042121015204));
#130344=CARTESIAN_POINT('',(-7.47066009951181,6.,70.5169035593534));
#130345=CARTESIAN_POINT('',(-6.72047186372468,5.99999999998125,84.6005928811747));
#130346=CARTESIAN_POINT('',(-6.72047103979891,6.,84.60059755389));
#130347=CARTESIAN_POINT('',(-7.28284229737108,5.99999999998,84.2626268242002));
#130348=CARTESIAN_POINT('Origin',(-6.80729512863291,5.99999999995501,84.10819367738));
#130349=CARTESIAN_POINT('',(-6.16760614884715,5.99999999999856,58.7310775255325));
#130350=CARTESIAN_POINT('Origin',(27.4324635166691,5.99999999999901,72.98888938658));
#130351=CARTESIAN_POINT('',(-2.249807880305,5.99999999999389,55.9944999902141));
#130352=CARTESIAN_POINT('Origin',(-2.02513312664091,5.99999999999801,60.48888938658));
#130353=CARTESIAN_POINT('',(21.7835206002327,6.00000000005992,59.219661206118));
#130354=CARTESIAN_POINT('Origin',(1.07038457110909,5.99999999998501,122.41156512159));
#130355=CARTESIAN_POINT('',(21.4524700019691,6.,61.19591303503));
#130356=CARTESIAN_POINT('Origin',(24.4068932609991,6.,60.67496850203));
#130357=CARTESIAN_POINT('',(21.4524700019491,6.,61.1959130349));
#130358=CARTESIAN_POINT('Origin',(-8.75366715310791,111.0724296188,85.97453149762));
#130359=CARTESIAN_POINT('',(33.8591356989091,-12.92363696959,78.460761865691));
#130360=CARTESIAN_POINT('',(29.8285484048191,-12.92381593441,79.171454261306));
#130361=CARTESIAN_POINT('',(33.6423057253991,-11.63783768946,78.49897240947));
#130362=CARTESIAN_POINT('',(33.6423057253991,-11.63783768946,78.49897240947));
#130363=CARTESIAN_POINT('Origin',(36.7188322241242,-11.4176049647123,77.9561983041534));
#130364=CARTESIAN_POINT('Origin',(-8.75366715310791,111.0724296188,85.97453149762));
#130365=CARTESIAN_POINT('',(33.6423056644279,11.63783769022,78.498972064024));
#130366=CARTESIAN_POINT('',(33.6423057253991,-11.63783768946,78.49897240947));
#130367=CARTESIAN_POINT('',(33.8592119939158,12.9236986194734,78.4607301343571));
#130368=CARTESIAN_POINT('',(33.8592136711991,12.92369861938,78.460739645228));
#130369=CARTESIAN_POINT('Origin',(36.7134944496243,11.4180028254251,77.9569478528599));
#130370=CARTESIAN_POINT('Origin',(27.2132013147391,-12.92381190166,78.109462257321));
#130371=CARTESIAN_POINT('',(33.818257678174,-13.7317225406618,78.228144902818));
#130372=CARTESIAN_POINT('Origin',(33.5977564035364,-12.9238122378902,76.9836935245755));
#130373=CARTESIAN_POINT('',(33.6728408920201,-14.3619759694431,77.403275003416));
#130374=CARTESIAN_POINT('Origin',(33.5986100047126,-12.9238119282868,76.9835424355099));
#130375=CARTESIAN_POINT('',(29.6420890790991,-14.36196613703,78.113990728651));
#130376=CARTESIAN_POINT('',(29.6420897207604,-14.3619786049901,78.1139943676928));
#130377=CARTESIAN_POINT('Origin',(29.5680176896579,-12.9236693686975,77.6941105696628));
#130378=CARTESIAN_POINT('Ctrl Pts',(27.5244159794491,-12.80681735949,79.549155074551));
#130379=CARTESIAN_POINT('Ctrl Pts',(27.5827558822291,-12.79405706744,79.538099789147));
#130380=CARTESIAN_POINT('Ctrl Pts',(28.3905563838491,-12.62204439971,79.384761922452));
#130381=CARTESIAN_POINT('Ctrl Pts',(29.2129925125091,-12.51120733417,79.224589989218));
#130382=CARTESIAN_POINT('Ctrl Pts',(29.9816324828591,-12.46457130983,79.071054735497));
#130383=CARTESIAN_POINT('Ctrl Pts',(27.7070605433691,-13.81411105762,79.72010021776));
#130384=CARTESIAN_POINT('Ctrl Pts',(27.7619085286391,-13.80141862852,79.71237284821));
#130385=CARTESIAN_POINT('Ctrl Pts',(28.5216090046891,-13.62979474475,79.605264089276));
#130386=CARTESIAN_POINT('Ctrl Pts',(29.2985927528191,-13.51173676089,79.494180558665));
#130387=CARTESIAN_POINT('Ctrl Pts',(30.0268234514991,-13.45237632462,79.38633904926));
#130388=CARTESIAN_POINT('Ctrl Pts',(27.7062881845591,-14.59938920963,79.041460544841));
#130389=CARTESIAN_POINT('Ctrl Pts',(27.7587276207091,-14.58888856718,79.036271398538));
#130390=CARTESIAN_POINT('Ctrl Pts',(28.4849791691991,-14.44741116539,78.964587688416));
#130391=CARTESIAN_POINT('Ctrl Pts',(29.2264592716991,-14.35719351328,78.893669194586));
#130392=CARTESIAN_POINT('Ctrl Pts',(29.9188937984091,-14.31933226887,78.8260112440331));
#130393=CARTESIAN_POINT('Ctrl Pts',(27.5226758911191,-14.5760123706,78.020211577781));
#130394=CARTESIAN_POINT('Ctrl Pts',(27.5755894451791,-14.56819007155,78.014874790841));
#130395=CARTESIAN_POINT('Ctrl Pts',(28.3080310747691,-14.46409602014,77.941347905091));
#130396=CARTESIAN_POINT('Ctrl Pts',(29.0504791474991,-14.41598192215,77.871665924383));
#130397=CARTESIAN_POINT('Ctrl Pts',(29.7384720137891,-14.41778257326,77.808662352547));
#130398=CARTESIAN_POINT('Ctrl Pts',(28.583810069542,-14.4235289944163,78.2160017822117));
#130399=CARTESIAN_POINT('Ctrl Pts',(28.9401679712898,-14.3897216672816,
78.1843085059736));
#130400=CARTESIAN_POINT('Ctrl Pts',(29.2930910333242,-14.3696365833235,
78.1493275324345));
#130401=CARTESIAN_POINT('Ctrl Pts',(29.6420890790991,-14.36196613703,78.113990728651));
#130402=CARTESIAN_POINT('Origin',(26.6903689106391,-17.,82.263358164095));
#130403=CARTESIAN_POINT('',(23.6515258014693,-10.9473150473928,65.0292224863868));
#130404=CARTESIAN_POINT('',(23.6515258014716,-7.5,65.0292224863863));
#130405=CARTESIAN_POINT('',(23.6515258014693,-17.,65.0292224863868));
#130406=CARTESIAN_POINT('',(22.9355719200891,-10.33193324195,60.96884625134));
#130407=CARTESIAN_POINT('Ctrl Pts',(23.651525801475,-10.9473150473928,65.0292224863858));
#130408=CARTESIAN_POINT('Ctrl Pts',(23.649538794891,-10.9444282998633,65.0179536120707));
#130409=CARTESIAN_POINT('Ctrl Pts',(23.6475480201257,-10.9415421742228,
65.0066633673373));
#130410=CARTESIAN_POINT('Ctrl Pts',(23.645553440154,-10.9386567173531,64.9953515422064));
#130411=CARTESIAN_POINT('Ctrl Pts',(23.6193912182559,-10.9008091685076,
64.8469782087948));
#130412=CARTESIAN_POINT('Ctrl Pts',(23.5925742504193,-10.8631053140448,
64.6948916264451));
#130413=CARTESIAN_POINT('Ctrl Pts',(23.5650981559036,-10.8259116051253,
64.5390669507413));
#130414=CARTESIAN_POINT('Ctrl Pts',(23.5502223202996,-10.8057745547496,
64.4547018945107));
#130415=CARTESIAN_POINT('Ctrl Pts',(23.5351532379843,-10.7857878904675,
64.3692408817632));
#130416=CARTESIAN_POINT('Ctrl Pts',(23.5198899259623,-10.7660159568398,
64.2826783379113));
#130417=CARTESIAN_POINT('Ctrl Pts',(23.5026409053267,-10.7436717571888,
64.1848542809157));
#130418=CARTESIAN_POINT('Ctrl Pts',(23.4851438221287,-10.7216013585723,
64.0856233918126));
#130419=CARTESIAN_POINT('Ctrl Pts',(23.4673981473186,-10.6999293150683,
63.984982668886));
#130420=CARTESIAN_POINT('Ctrl Pts',(23.4445642071311,-10.6720431878624,
63.8554849590316));
#130421=CARTESIAN_POINT('Ctrl Pts',(23.4213212328658,-10.6447569234707,
63.7236675037941));
#130422=CARTESIAN_POINT('Ctrl Pts',(23.3978341137514,-10.61857549495,63.5904654234402));
#130423=CARTESIAN_POINT('Ctrl Pts',(23.3766359460333,-10.5949455933781,
63.4702446323763));
#130424=CARTESIAN_POINT('Ctrl Pts',(23.3552389149002,-10.5722162410661,
63.3488960207313));
#130425=CARTESIAN_POINT('Ctrl Pts',(23.3337672030354,-10.5507173831927,
63.2271238921102));
#130426=CARTESIAN_POINT('Ctrl Pts',(23.3314487146874,-10.5483959636529,
63.2139750913488));
#130427=CARTESIAN_POINT('Ctrl Pts',(23.3291293586053,-10.5460888432694,
63.2008213696401));
#130428=CARTESIAN_POINT('Ctrl Pts',(23.3268092933577,-10.5437964012374,
63.1876636262863));
#130429=CARTESIAN_POINT('Ctrl Pts',(23.309310409464,-10.5265058629688,63.0884225280079));
#130430=CARTESIAN_POINT('Ctrl Pts',(23.2917710596858,-10.5100526735849,
62.9889519597633));
#130431=CARTESIAN_POINT('Ctrl Pts',(23.2742619690445,-10.4946060514652,
62.8896529723304));
#130432=CARTESIAN_POINT('Ctrl Pts',(23.2578463446928,-10.4801240916984,
62.7965553403862));
#130433=CARTESIAN_POINT('Ctrl Pts',(23.2414572804221,-10.4664710978206,
62.7036083027852));
#130434=CARTESIAN_POINT('Ctrl Pts',(23.2252065308699,-10.4537748697727,
62.6114456888268));
#130435=CARTESIAN_POINT('Ctrl Pts',(23.2094400821371,-10.4414570115733,
62.5220296822983));
#130436=CARTESIAN_POINT('Ctrl Pts',(23.1938038426215,-10.430039913861,62.4333521317278));
#130437=CARTESIAN_POINT('Ctrl Pts',(23.1784012188369,-10.4195924205753,
62.3459995053294));
#130438=CARTESIAN_POINT('Ctrl Pts',(23.1629985950523,-10.4091449272895,
62.2586468789311));
#130439=CARTESIAN_POINT('Ctrl Pts',(23.1478295974388,-10.3996672586441,
62.1726192371723));
#130440=CARTESIAN_POINT('Ctrl Pts',(23.1329988176234,-10.3911763876647,
62.0885097389733));
#130441=CARTESIAN_POINT('Ctrl Pts',(23.1186007850307,-10.3829332717514,
62.0068544712464));
#130442=CARTESIAN_POINT('Ctrl Pts',(23.1045215897217,-10.375620358595,61.9270074349582));
#130443=CARTESIAN_POINT('Ctrl Pts',(23.0908595573615,-10.3692172844012,
61.8495262080312));
#130444=CARTESIAN_POINT('Ctrl Pts',(23.0896052918578,-10.368629439572,61.8424129156926));
#130445=CARTESIAN_POINT('Ctrl Pts',(23.0883545424879,-10.3680492269807,
61.8353195639691));
#130446=CARTESIAN_POINT('Ctrl Pts',(23.087107385374,-10.3674766089124,61.8282465845024));
#130447=CARTESIAN_POINT('Ctrl Pts',(23.0666311162332,-10.3580751617747,
61.7121198915922));
#130448=CARTESIAN_POINT('Ctrl Pts',(23.0471148480774,-10.3508869369945,
61.6014375750419));
#130449=CARTESIAN_POINT('Ctrl Pts',(23.0284541449167,-10.3455073057329,
61.4956074781716));
#130450=CARTESIAN_POINT('Ctrl Pts',(23.0103685575805,-10.3402934726752,
61.3930390249216));
#130451=CARTESIAN_POINT('Ctrl Pts',(22.993086486547,-10.3367775742029,61.2950275620653));
#130452=CARTESIAN_POINT('Ctrl Pts',(22.976507171293,-10.3346276973853,61.2010015992793));
#130453=CARTESIAN_POINT('Ctrl Pts',(22.9734133232253,-10.3342265112002,
61.1834555161736));
#130454=CARTESIAN_POINT('Ctrl Pts',(22.9703439336347,-10.3338730176223,
61.1660481433642));
#130455=CARTESIAN_POINT('Ctrl Pts',(22.9672983299519,-10.3335652372066,
61.1487756666496));
#130456=CARTESIAN_POINT('Ctrl Pts',(22.9564298118544,-10.3324668943601,
61.087137237848));
#130457=CARTESIAN_POINT('Ctrl Pts',(22.9458642968996,-10.3319499802198,
61.0272172190325));
#130458=CARTESIAN_POINT('Ctrl Pts',(22.9355719203965,-10.33193324195,60.9688462512858));
#130459=CARTESIAN_POINT('',(22.9355719200891,-10.33193324195,60.96884625134));
#130460=CARTESIAN_POINT('',(22.9296816314691,-7.5,60.93544076845));
#130461=CARTESIAN_POINT('',(22.9296817835391,-10.33198955295,60.93544163085));
#130462=CARTESIAN_POINT('',(24.8670630451391,-7.5,71.922876757467));
#130463=CARTESIAN_POINT('Ctrl Pts',(16.7315271092291,25.77957474242,75.8056538642681));
#130464=CARTESIAN_POINT('Ctrl Pts',(16.8902739491491,25.78276104928,76.726755143248));
#130465=CARTESIAN_POINT('Ctrl Pts',(17.4170423638691,25.68741378017,79.011155596728));
#130466=CARTESIAN_POINT('Ctrl Pts',(18.6971928491291,25.1486541372,82.327981456666));
#130467=CARTESIAN_POINT('Ctrl Pts',(20.3541926191191,24.21296098443,85.29757061493));
#130468=CARTESIAN_POINT('Ctrl Pts',(21.9876235905991,23.12636897321,87.62326197554));
#130469=CARTESIAN_POINT('Ctrl Pts',(23.5303110581191,21.96974605327,89.49482082956));
#130470=CARTESIAN_POINT('Ctrl Pts',(25.0147293345491,20.73535636643,91.08394632963));
#130471=CARTESIAN_POINT('Ctrl Pts',(26.4477039632491,19.42122041898,92.4661164628101));
#130472=CARTESIAN_POINT('Ctrl Pts',(27.8040593501691,18.0525443245,93.66246634875));
#130473=CARTESIAN_POINT('Ctrl Pts',(29.0976297887891,16.61722673478,94.7173081814599));
#130474=CARTESIAN_POINT('Ctrl Pts',(30.3859883571291,15.03805899871,95.692928827));
#130475=CARTESIAN_POINT('Ctrl Pts',(31.6846191544191,13.2490375268,96.6017522016999));
#130476=CARTESIAN_POINT('Ctrl Pts',(32.9283641549091,11.27078505501,97.39922069443));
#130477=CARTESIAN_POINT('Ctrl Pts',(34.0024905191591,9.24026551673301,98.0256740975701));
#130478=CARTESIAN_POINT('Ctrl Pts',(34.8835248980591,7.19980133487202,98.4916705583199));
#130479=CARTESIAN_POINT('Ctrl Pts',(35.5865206621291,5.09129120886101,98.8275149094299));
#130480=CARTESIAN_POINT('Ctrl Pts',(36.0644764908891,2.94897602587201,99.0360923986901));
#130481=CARTESIAN_POINT('Ctrl Pts',(36.2175390832591,1.50759720120401,99.1082321058299));
#130482=CARTESIAN_POINT('Ctrl Pts',(36.2511547877691,0.817200229439614,
99.1309346670101));
#130483=CARTESIAN_POINT('Ctrl Pts',(16.5657307648391,19.34436604072,75.8499470296021));
#130484=CARTESIAN_POINT('Ctrl Pts',(16.7027032210391,19.34727467235,76.647687526976));
#130485=CARTESIAN_POINT('Ctrl Pts',(17.1758927443291,19.26031994756,78.623309386718));
#130486=CARTESIAN_POINT('Ctrl Pts',(18.3744374416091,18.77127275203,81.451029832546));
#130487=CARTESIAN_POINT('Ctrl Pts',(19.9464727370091,17.9342387447,83.90371085737));
#130488=CARTESIAN_POINT('Ctrl Pts',(21.5011129654591,16.97934371574,85.75395997948));
#130489=CARTESIAN_POINT('Ctrl Pts',(22.9701058542891,15.98027083986,87.18714704112));
#130490=CARTESIAN_POINT('Ctrl Pts',(24.3829496628191,14.93205005415,88.35697360021));
#130491=CARTESIAN_POINT('Ctrl Pts',(25.7455828440791,13.83506997747,89.33304121868));
#130492=CARTESIAN_POINT('Ctrl Pts',(27.0338235509591,12.71200151814,90.14134599812));
#130493=CARTESIAN_POINT('Ctrl Pts',(28.2606989614091,11.55431815225,90.82076231519));
#130494=CARTESIAN_POINT('Ctrl Pts',(29.4805515038791,10.30341122855,91.41513380966));
#130495=CARTESIAN_POINT('Ctrl Pts',(30.7073346580191,8.91606547149402,91.92891446662));
#130496=CARTESIAN_POINT('Ctrl Pts',(31.8785519228191,7.42186252822301,92.33283454608));
#130497=CARTESIAN_POINT('Ctrl Pts',(32.8858034194691,5.93611159812901,92.60136415471));
#130498=CARTESIAN_POINT('Ctrl Pts',(33.7077479385191,4.49637949617201,92.75525280737));
#130499=CARTESIAN_POINT('Ctrl Pts',(34.3594477230791,3.06936714330901,92.82352537927));
#130500=CARTESIAN_POINT('Ctrl Pts',(34.7987841186091,1.68933111557601,92.83289655037));
#130501=CARTESIAN_POINT('Ctrl Pts',(34.9379185776691,0.799874261541514,
92.83329103801));
#130502=CARTESIAN_POINT('Ctrl Pts',(34.9680789093591,0.377412282680914,
92.8379453280101));
#130503=CARTESIAN_POINT('Ctrl Pts',(21.0648245475691,14.80356751578,75.088574197736));
#130504=CARTESIAN_POINT('Ctrl Pts',(21.1562893009191,14.80542149402,75.624814594272));
#130505=CARTESIAN_POINT('Ctrl Pts',(21.4915191590391,14.74994267437,76.949273101324));
#130506=CARTESIAN_POINT('Ctrl Pts',(22.4029329257891,14.43645292234,78.850401178621));
#130507=CARTESIAN_POINT('Ctrl Pts',(23.6728411634791,13.89196197301,80.525093828825));
#130508=CARTESIAN_POINT('Ctrl Pts',(24.9938756020691,13.25961078348,81.813737319686));
#130509=CARTESIAN_POINT('Ctrl Pts',(26.2936708744891,12.5864534242,82.832583999374));
#130510=CARTESIAN_POINT('Ctrl Pts',(27.5870975206191,11.86798256843,83.68225710374));
#130511=CARTESIAN_POINT('Ctrl Pts',(28.8717832775691,11.10303997034,84.4077907698501));
#130512=CARTESIAN_POINT('Ctrl Pts',(30.1179515221891,10.306293006,85.0241310085501));
#130513=CARTESIAN_POINT('Ctrl Pts',(31.3323143284891,9.47069299188402,85.55730149859));
#130514=CARTESIAN_POINT('Ctrl Pts',(32.5667384548491,8.55128051724301,86.04034306038));
#130515=CARTESIAN_POINT('Ctrl Pts',(33.8387497469191,7.50960072681501,86.47900335892));
#130516=CARTESIAN_POINT('Ctrl Pts',(35.0880429676691,6.35762147075602,86.85127259704));
#130517=CARTESIAN_POINT('Ctrl Pts',(36.1977391360291,5.17506491544101,87.13119140558));
#130518=CARTESIAN_POINT('Ctrl Pts',(37.1355508905091,3.98655984369701,87.32815521361));
#130519=CARTESIAN_POINT('Ctrl Pts',(37.9083300473991,2.75824145710901,87.46012871543));
#130520=CARTESIAN_POINT('Ctrl Pts',(38.4524854874891,1.51002426311401,87.5351100622101));
#130521=CARTESIAN_POINT('Ctrl Pts',(38.6303209632591,0.670091817760814,
87.56162468684));
#130522=CARTESIAN_POINT('Ctrl Pts',(38.6686985395891,0.267767345835414,
87.57156379687));
#130523=CARTESIAN_POINT('Ctrl Pts',(27.4060955579191,15.00605745049,73.9992175459301));
#130524=CARTESIAN_POINT('Ctrl Pts',(27.4568706345291,15.00674148237,74.299882608077));
#130525=CARTESIAN_POINT('Ctrl Pts',(27.6563153791591,14.98607407549,75.03933020766));
#130526=CARTESIAN_POINT('Ctrl Pts',(28.2552178354491,14.86384274642,76.157719195735));
#130527=CARTESIAN_POINT('Ctrl Pts',(29.1953897033191,14.62223845856,77.28144993045));
#130528=CARTESIAN_POINT('Ctrl Pts',(30.2745666151391,14.3009152899,78.274673456111));
#130529=CARTESIAN_POINT('Ctrl Pts',(31.4158151207291,13.9175608677,79.163166612491));
#130530=CARTESIAN_POINT('Ctrl Pts',(32.6169037455491,13.46553722345,79.992694706598));
#130531=CARTESIAN_POINT('Ctrl Pts',(33.8649399941491,12.93919476597,80.780446952018));
#130532=CARTESIAN_POINT('Ctrl Pts',(35.1214740837291,12.3447503952,81.5213409775531));
#130533=CARTESIAN_POINT('Ctrl Pts',(36.3853570661891,11.67360909312,82.229199358404));
#130534=CARTESIAN_POINT('Ctrl Pts',(37.7082882345091,10.88094645291,82.940678146904));
#130535=CARTESIAN_POINT('Ctrl Pts',(39.1142274982291,9.91205347783502,83.67127064968));
#130536=CARTESIAN_POINT('Ctrl Pts',(40.5432158335391,8.74576233655301,84.3936442258099));
#130537=CARTESIAN_POINT('Ctrl Pts',(41.8604028480391,7.43460302127903,85.0471196915701));
#130538=CARTESIAN_POINT('Ctrl Pts',(43.0163443071791,5.99020112655302,85.6153164434601));
#130539=CARTESIAN_POINT('Ctrl Pts',(44.0066134889891,4.35311312370201,86.1022978834));
#130540=CARTESIAN_POINT('Ctrl Pts',(44.7332634147991,2.52355184883601,86.4665423458501));
#130541=CARTESIAN_POINT('Ctrl Pts',(44.9781481988991,1.19967484028401,86.60065479763));
#130542=CARTESIAN_POINT('Ctrl Pts',(45.0312601718991,0.557056200456914,
86.6358961446099));
#130543=CARTESIAN_POINT('',(29.6421154185267,14.3619794304194,78.1139870084275));
#130544=CARTESIAN_POINT('Ctrl Pts',(29.6421046546614,14.3619829782172,78.1140023840685));
#130545=CARTESIAN_POINT('Ctrl Pts',(29.5145956406364,14.3649991419673,78.1261564978929));
#130546=CARTESIAN_POINT('Ctrl Pts',(29.3820227690687,14.369719041399,78.1388270540191));
#130547=CARTESIAN_POINT('Ctrl Pts',(29.2447491213195,14.3765172160041,78.1520061984839));
#130548=CARTESIAN_POINT('Ctrl Pts',(29.2357685362962,14.3769619596679,78.1528683918425));
#130549=CARTESIAN_POINT('Ctrl Pts',(29.2267678363257,14.3774156051513,78.1537327452661));
#130550=CARTESIAN_POINT('Ctrl Pts',(29.2177471248349,14.3778782601166,78.1545992495703));
#130551=CARTESIAN_POINT('Ctrl Pts',(29.1231957583653,14.3827276180877,78.1636815892615));
#130552=CARTESIAN_POINT('Ctrl Pts',(29.0264438263049,14.3885640451357,78.172998206678));
#130553=CARTESIAN_POINT('Ctrl Pts',(28.9271250708793,14.3955514440818,78.1826054494819));
#130554=CARTESIAN_POINT('Ctrl Pts',(28.872119986792,14.3994212314643,78.1879261685748));
#130555=CARTESIAN_POINT('Ctrl Pts',(28.8163274509837,14.4036448482421,78.1933357668402));
#130556=CARTESIAN_POINT('Ctrl Pts',(28.7596841741806,14.4082565912696,78.1988414060183));
#130557=CARTESIAN_POINT('Ctrl Pts',(28.701932031196,14.4129586151948,78.2044548252797));
#130558=CARTESIAN_POINT('Ctrl Pts',(28.6432962519838,14.4180637104245,78.2101696022246));
#130559=CARTESIAN_POINT('Ctrl Pts',(28.5837302065717,14.4236103462183,78.2159942181859));
#130560=CARTESIAN_POINT('Ctrl Pts',(27.6070995425304,14.9199507410733,75.6071390537838));
#130561=CARTESIAN_POINT('Ctrl Pts',(27.7192629013877,14.8959306840627,75.8250406547776));
#130562=CARTESIAN_POINT('Ctrl Pts',(27.8457646196489,14.8667398375127,76.0382447729958));
#130563=CARTESIAN_POINT('Ctrl Pts',(27.9845985217786,14.8326654832504,76.2466690142022));
#130564=CARTESIAN_POINT('Ctrl Pts',(28.1242452289094,14.7983916402096,76.4563134780127));
#130565=CARTESIAN_POINT('Ctrl Pts',(28.2763688932358,14.7591771556667,76.661121665329));
#130566=CARTESIAN_POINT('Ctrl Pts',(28.4389329606639,14.7153582057326,76.861038443836));
#130567=CARTESIAN_POINT('Ctrl Pts',(28.4556902247096,14.7108413052523,76.8816460620976));
#130568=CARTESIAN_POINT('Ctrl Pts',(28.4725584300046,14.7062755155822,76.9022017328212));
#130569=CARTESIAN_POINT('Ctrl Pts',(28.4895353492335,14.7016612297159,76.9227054145368));
#130570=CARTESIAN_POINT('Ctrl Pts',(28.6751623758138,14.6512082497849,77.1468943512624));
#130571=CARTESIAN_POINT('Ctrl Pts',(28.8735586889575,14.5949456973791,77.3649852820764));
#130572=CARTESIAN_POINT('Ctrl Pts',(29.0821746934216,14.533243265586,77.5774426839974));
#130573=CARTESIAN_POINT('Ctrl Pts',(29.261787491736,14.480119122663,77.7603628227453));
#130574=CARTESIAN_POINT('Ctrl Pts',(29.4489760014774,14.4229617454712,77.9391075942936));
#130575=CARTESIAN_POINT('Ctrl Pts',(29.6421154185267,14.3619794304194,78.1139870084275));
#130576=CARTESIAN_POINT('Origin',(58.0152958556891,-0.499074165591486,68.638644839116));
#130577=CARTESIAN_POINT('',(63.7242586906601,14.99856960786,67.8461534157091));
#130578=CARTESIAN_POINT('Ctrl Pts',(63.7242533230191,14.99854021533,67.846155382807));
#130579=CARTESIAN_POINT('Ctrl Pts',(51.5782329133125,14.9978694358453,69.9878171256976));
#130580=CARTESIAN_POINT('Ctrl Pts',(39.4322140887331,14.9978694371101,72.1294878582915));
#130581=CARTESIAN_POINT('Ctrl Pts',(27.2861971798628,14.9986801148638,74.2711694554112));
#130582=CARTESIAN_POINT('',(63.7044144696626,14.9224864514636,69.2168818788526));
#130583=CARTESIAN_POINT('Ctrl Pts',(63.7044145289691,14.92248985567,69.216882216528));
#130584=CARTESIAN_POINT('Ctrl Pts',(63.6851849469295,14.9336666490122,69.1078885713561));
#130585=CARTESIAN_POINT('Ctrl Pts',(63.6707295798855,14.9437626665518,68.9967717088079));
#130586=CARTESIAN_POINT('Ctrl Pts',(63.6613828168746,14.9526646152637,68.8841400361723));
#130587=CARTESIAN_POINT('Ctrl Pts',(63.6522220369491,14.961389431862,68.7737495229593));
#130588=CARTESIAN_POINT('Ctrl Pts',(63.6479686149546,14.9689673053526,68.6619040795053));
#130589=CARTESIAN_POINT('Ctrl Pts',(63.6489383237461,14.9753434652124,68.5491819025216));
#130590=CARTESIAN_POINT('Ctrl Pts',(63.6499375632273,14.9819137992407,68.4330269798916));
#130591=CARTESIAN_POINT('Ctrl Pts',(63.6564829323108,14.9872078381345,68.3159413010022));
#130592=CARTESIAN_POINT('Ctrl Pts',(63.6689204526746,14.991223439365,68.1985604179833));
#130593=CARTESIAN_POINT('Ctrl Pts',(63.6813579730383,14.9952390405955,68.0811795349645));
#130594=CARTESIAN_POINT('Ctrl Pts',(63.6996876813661,14.9979763340792,67.9635036558599));
#130595=CARTESIAN_POINT('Ctrl Pts',(63.7242555654557,14.9994907873196,67.8461681406557));
#130596=CARTESIAN_POINT('',(66.1162021797537,0.79020098334245,82.8948096732265));
#130597=CARTESIAN_POINT('Origin',(63.4339821949991,-0.499074165591486,67.683184237498));
#130598=CARTESIAN_POINT('',(44.6819013833791,0.790370888696714,86.67422941916));
#130599=CARTESIAN_POINT('',(44.6819028561657,0.790371596722371,86.6742377717481));
#130600=CARTESIAN_POINT('',(37.5050940990142,10.7061722565098,83.1298152725198));
#130601=CARTESIAN_POINT('Ctrl Pts',(37.5051003753486,10.7061762392465,83.1298227805085));
#130602=CARTESIAN_POINT('Ctrl Pts',(38.3763978528178,10.1348334115302,83.5832077696022));
#130603=CARTESIAN_POINT('Ctrl Pts',(39.2226440888349,9.50364223937353,84.0079460340611));
#130604=CARTESIAN_POINT('Ctrl Pts',(40.8102490283764,8.10943081545489,84.7907499725118));
#130605=CARTESIAN_POINT('Ctrl Pts',(41.5520655694067,7.34592818639295,85.1489322811934));
#130606=CARTESIAN_POINT('Ctrl Pts',(42.8580113501118,5.68093119810927,85.776362545284));
#130607=CARTESIAN_POINT('Ctrl Pts',(43.4218825811718,4.77838638362871,86.0454790494045));
#130608=CARTESIAN_POINT('Ctrl Pts',(44.0639229648733,3.33561826274428,86.3569296909199));
#130609=CARTESIAN_POINT('Ctrl Pts',(44.2439337207264,2.84043576288029,86.4453260797462));
#130610=CARTESIAN_POINT('Ctrl Pts',(44.5242936554535,1.82822955706199,86.586853260865));
#130611=CARTESIAN_POINT('Ctrl Pts',(44.6247440186015,1.31135464491908,86.6400205490487));
#130612=CARTESIAN_POINT('Ctrl Pts',(44.6819013833791,0.790370888696714,
86.67422941916));
#130613=CARTESIAN_POINT('',(36.7493876194873,13.6349921310859,78.8488579760133));
#130614=CARTESIAN_POINT('Origin',(35.6454492392491,-0.499074165591586,72.5830523519042));
#130615=CARTESIAN_POINT('',(33.6728394647692,14.3619762585541,77.4032747789144));
#130616=CARTESIAN_POINT('Ctrl Pts',(36.7499023085083,13.6386605077094,78.850394493121));
#130617=CARTESIAN_POINT('Ctrl Pts',(36.7483039859788,13.6431409106807,78.8404660979912));
#130618=CARTESIAN_POINT('Ctrl Pts',(36.7466776914937,13.6470698094342,78.831711908129));
#130619=CARTESIAN_POINT('Ctrl Pts',(36.7450249995319,13.6504651160832,78.8241397777305));
#130620=CARTESIAN_POINT('Ctrl Pts',(36.7441982906584,13.6521635149378,78.8203520498683));
#130621=CARTESIAN_POINT('Ctrl Pts',(36.7433649733905,13.6537282955424,78.8168600514848));
#130622=CARTESIAN_POINT('Ctrl Pts',(36.742525153558,13.6551610905843,78.8136644833911));
#130623=CARTESIAN_POINT('Ctrl Pts',(36.7421052436417,13.6558774881053,78.8120666993442));
#130624=CARTESIAN_POINT('Ctrl Pts',(36.7416837081268,13.6565608828926,78.8105430198817));
#130625=CARTESIAN_POINT('Ctrl Pts',(36.741260559816,13.6572114408692,78.8090935149832));
#130626=CARTESIAN_POINT('Ctrl Pts',(36.7410489856607,13.6575367198576,78.808368762534));
#130627=CARTESIAN_POINT('Ctrl Pts',(36.7408370083007,13.6578537892448,78.8076625535445));
#130628=CARTESIAN_POINT('Ctrl Pts',(36.7406246292619,13.6581626673822,78.8069748956749));
#130629=CARTESIAN_POINT('Ctrl Pts',(36.7405184397425,13.6583171064509,78.8066310667402));
#130630=CARTESIAN_POINT('Ctrl Pts',(36.7405071118863,13.6583391525674,78.8065816613395));
#130631=CARTESIAN_POINT('Ctrl Pts',(36.740448204214,13.6584243401768,78.8063920073941));
#130632=CARTESIAN_POINT('Ctrl Pts',(36.7403892965417,13.6585095277861,78.8062023534488));
#130633=CARTESIAN_POINT('Ctrl Pts',(36.7402828111207,13.6586578767028,78.8058724585813));
#130634=CARTESIAN_POINT('Ctrl Pts',(36.7399862885877,13.6590647448003,78.8049675823703));
#130635=CARTESIAN_POINT('Ctrl Pts',(36.7352419280597,13.6655746343596,78.7904895629937));
#130636=CARTESIAN_POINT('Ctrl Pts',(36.7282234174915,13.6735556178127,78.7727678395045));
#130637=CARTESIAN_POINT('Ctrl Pts',(36.7189266889496,13.6830013954498,78.7518015064668));
#130638=CARTESIAN_POINT('Ctrl Pts',(36.7142783246787,13.6877242842683,78.7413183399479));
#130639=CARTESIAN_POINT('Ctrl Pts',(36.7090604132126,13.6928133730756,78.7300240140316));
#130640=CARTESIAN_POINT('Ctrl Pts',(36.70327253979,13.698267885164,78.7179183561814));
#130641=CARTESIAN_POINT('Ctrl Pts',(36.7003786030787,13.7009951412082,78.7118655272564));
#130642=CARTESIAN_POINT('Ctrl Pts',(36.6973421775542,13.7038137533595,78.7056098641795));
#130643=CARTESIAN_POINT('Ctrl Pts',(36.6941632209318,13.7067236250423,78.6991513408688));
#130644=CARTESIAN_POINT('Ctrl Pts',(36.6911649311007,13.709468122597,78.6930598690224));
#130645=CARTESIAN_POINT('Ctrl Pts',(36.6885450749576,13.7118426094089,78.687789320445));
#130646=CARTESIAN_POINT('Ctrl Pts',(36.6848741180589,13.7151236456254,78.6805062934297));
#130647=CARTESIAN_POINT('Ctrl Pts',(36.6846529186282,13.7153213497562,78.6800674428864));
#130648=CARTESIAN_POINT('Ctrl Pts',(36.6844278930973,13.7155223487087,78.6796212730289));
#130649=CARTESIAN_POINT('Ctrl Pts',(36.6841987246351,13.7157269231489,78.6791671587984));
#130650=CARTESIAN_POINT('Ctrl Pts',(36.6680692169269,13.7301254358376,78.6472053482076));
#130651=CARTESIAN_POINT('Ctrl Pts',(36.6503646181003,13.7445537303848,78.6152586270666));
#130652=CARTESIAN_POINT('Ctrl Pts',(36.6310925009288,13.7590546689286,78.5833421826575));
#130653=CARTESIAN_POINT('Ctrl Pts',(36.6180877346395,13.7688398583326,78.5618050626497));
#130654=CARTESIAN_POINT('Ctrl Pts',(36.6040633494866,13.7788041463262,78.5399779777372));
#130655=CARTESIAN_POINT('Ctrl Pts',(36.589949449959,13.788501639847,78.5188095793515));
#130656=CARTESIAN_POINT('Ctrl Pts',(36.5831475775772,13.7931751259535,78.508607951937));
#130657=CARTESIAN_POINT('Ctrl Pts',(36.5763246574787,13.7977863511604,78.4985596617409));
#130658=CARTESIAN_POINT('Ctrl Pts',(36.5695809276106,13.8022700534891,78.4888012993751));
#130659=CARTESIAN_POINT('Ctrl Pts',(36.559212435832,13.8091637505443,78.4737978069545));
#130660=CARTESIAN_POINT('Ctrl Pts',(36.548971858619,13.8158029081853,78.4593755010848));
#130661=CARTESIAN_POINT('Ctrl Pts',(36.5388588882553,13.8221821595769,78.4455321849782));
#130662=CARTESIAN_POINT('Ctrl Pts',(36.5334905180153,13.8255685220493,78.4381835976159));
#130663=CARTESIAN_POINT('Ctrl Pts',(36.5283454585794,13.8287795761135,78.431215627966));
#130664=CARTESIAN_POINT('Ctrl Pts',(36.5229768883168,13.8320566518634,78.4241131015378));
#130665=CARTESIAN_POINT('Ctrl Pts',(36.5182321114119,13.8349529524748,78.4178358430286));
#130666=CARTESIAN_POINT('Ctrl Pts',(36.5133127821366,13.8379011442613,78.4114528236521));
#130667=CARTESIAN_POINT('Ctrl Pts',(36.5079093897136,13.8410531095132,78.4046389204707));
#130668=CARTESIAN_POINT('Ctrl Pts',(36.5015447951238,13.8447657735989,78.3966129012723));
#130669=CARTESIAN_POINT('Ctrl Pts',(36.4945829395513,13.8487260779931,78.388062192188));
#130670=CARTESIAN_POINT('Ctrl Pts',(36.4870259347947,13.8529298786463,78.3789766395846));
#130671=CARTESIAN_POINT('Ctrl Pts',(36.4844101699437,13.8543849728726,78.375831786575));
#130672=CARTESIAN_POINT('Ctrl Pts',(36.4817230461861,13.8558690534932,78.3726232353304));
#130673=CARTESIAN_POINT('Ctrl Pts',(36.4789644617547,13.8573812806233,78.3693519287813));
#130674=CARTESIAN_POINT('Ctrl Pts',(36.4752711027011,13.8594059414236,78.3649721064627));
#130675=CARTESIAN_POINT('Ctrl Pts',(36.4714496611526,13.8614809894887,78.3604799314432));
#130676=CARTESIAN_POINT('Ctrl Pts',(36.4674996366288,13.8636072933881,78.3558716882688));
#130677=CARTESIAN_POINT('Ctrl Pts',(36.4597877537408,13.8677586110717,78.3468747234483));
#130678=CARTESIAN_POINT('Ctrl Pts',(36.4515871632937,13.8721025800674,78.3374418240048));
#130679=CARTESIAN_POINT('Ctrl Pts',(36.4428975930266,13.8766350377088,78.3275713885573));
#130680=CARTESIAN_POINT('Ctrl Pts',(36.438552807893,13.8789012665295,78.3226361708335));
#130681=CARTESIAN_POINT('Ctrl Pts',(36.4340857780505,13.8812146199161,78.3175915703031));
#130682=CARTESIAN_POINT('Ctrl Pts',(36.4294964723451,13.8835746144666,78.3124374042033));
#130683=CARTESIAN_POINT('Ctrl Pts',(36.4267289688733,13.8849977694122,78.309329271189));
#130684=CARTESIAN_POINT('Ctrl Pts',(36.4243686482471,13.8862050042778,78.3066910306504));
#130685=CARTESIAN_POINT('Ctrl Pts',(36.421598860639,13.8876189102116,78.3035976453758));
#130686=CARTESIAN_POINT('Ctrl Pts',(36.4197755547958,13.8885496613433,78.3015613204858));
#130687=CARTESIAN_POINT('Ctrl Pts',(36.4177747384656,13.8895696444297,78.2993284362583));
#130688=CARTESIAN_POINT('Ctrl Pts',(36.4153616994248,13.8907940838674,78.2966460457519));
#130689=CARTESIAN_POINT('Ctrl Pts',(36.4019716470465,13.8975885484107,78.2817613510696));
#130690=CARTESIAN_POINT('Ctrl Pts',(36.3890010975978,13.9040184390785,78.2676211351411));
#130691=CARTESIAN_POINT('Ctrl Pts',(36.3764337310713,13.910136612886,78.2541341879297));
#130692=CARTESIAN_POINT('Ctrl Pts',(36.3672900523479,13.9145880320081,78.2443214469707));
#130693=CARTESIAN_POINT('Ctrl Pts',(36.3583600601549,13.9188739784771,78.2348555092975));
#130694=CARTESIAN_POINT('Ctrl Pts',(36.3496410325615,13.9230076695007,78.2257166146442));
#130695=CARTESIAN_POINT('Ctrl Pts',(36.3268217375824,13.9338262973593,78.2017984505322));
#130696=CARTESIAN_POINT('Ctrl Pts',(36.3054447977087,13.943598679941,78.1801266659689));
#130697=CARTESIAN_POINT('Ctrl Pts',(36.2855839501909,13.9521935012056,78.1611288208426));
#130698=CARTESIAN_POINT('Ctrl Pts',(36.2808490071319,13.9542425572318,78.1565996226381));
#130699=CARTESIAN_POINT('Ctrl Pts',(36.2761982177636,13.9562293358506,78.1522106338178));
#130700=CARTESIAN_POINT('Ctrl Pts',(36.2716316100593,13.9581542476587,78.1479620137005));
#130701=CARTESIAN_POINT('Ctrl Pts',(36.2686426206986,13.9594141633964,78.1451811572858));
#130702=CARTESIAN_POINT('Ctrl Pts',(36.2640769281232,13.9613255588747,78.1409638939666));
#130703=CARTESIAN_POINT('Ctrl Pts',(36.2592938494356,13.9633073451264,78.1365905752382));
#130704=CARTESIAN_POINT('Ctrl Pts',(36.2567692928829,13.9643533516412,78.1342822940716));
#130705=CARTESIAN_POINT('Ctrl Pts',(36.2541844203468,13.965419258694,78.1319299371098));
#130706=CARTESIAN_POINT('Ctrl Pts',(36.2517412373075,13.9664222308341,78.1297163483021));
#130707=CARTESIAN_POINT('Ctrl Pts',(36.2375970578421,13.9722286799298,78.1169013455558));
#130708=CARTESIAN_POINT('Ctrl Pts',(36.2230046602156,13.9780685655748,78.1040081587856));
#130709=CARTESIAN_POINT('Ctrl Pts',(36.2079638463695,13.9839387279526,78.0910356788575));
#130710=CARTESIAN_POINT('Ctrl Pts',(36.207192383829,13.9842398160737,78.0903703038037));
#130711=CARTESIAN_POINT('Ctrl Pts',(36.2064197402877,13.9845409860667,78.0897047141239));
#130712=CARTESIAN_POINT('Ctrl Pts',(36.2056459158412,13.9848422362319,78.0890389129253));
#130713=CARTESIAN_POINT('Ctrl Pts',(36.1778639481647,13.9956577673124,78.0651352129796));
#130714=CARTESIAN_POINT('Ctrl Pts',(36.148561323177,14.0065748413203,78.0409623999071));
#130715=CARTESIAN_POINT('Ctrl Pts',(36.1177379487843,14.0175855767315,78.0165187379705));
#130716=CARTESIAN_POINT('Ctrl Pts',(36.1159428936046,14.0182268069025,78.0150952169305));
#130717=CARTESIAN_POINT('Ctrl Pts',(36.114142675661,14.0188683610647,78.0136707648243));
#130718=CARTESIAN_POINT('Ctrl Pts',(36.112337293027,14.0195102400722,78.0122453765528));
#130719=CARTESIAN_POINT('Ctrl Pts',(36.0931864763242,14.026319050009,77.9971253964415));
#130720=CARTESIAN_POINT('Ctrl Pts',(36.0730170337921,14.0333203443543,77.9815520871684));
#130721=CARTESIAN_POINT('Ctrl Pts',(36.0520653827686,14.0403913058479,77.9658078664028));
#130722=CARTESIAN_POINT('Ctrl Pts',(36.050604035552,14.0408844951381,77.9647097298804));
#130723=CARTESIAN_POINT('Ctrl Pts',(36.0491388901179,14.041378032158,77.9636107440935));
#130724=CARTESIAN_POINT('Ctrl Pts',(36.0476700299407,14.04187187919,77.9625109968557));
#130725=CARTESIAN_POINT('Ctrl Pts',(36.0257420075874,14.0492443227505,77.9460933130025));
#130726=CARTESIAN_POINT('Ctrl Pts',(36.0029842929834,14.0566841655443,77.9295094191599));
#130727=CARTESIAN_POINT('Ctrl Pts',(35.9796840785309,14.0640627858329,77.9130581508823));
#130728=CARTESIAN_POINT('Ctrl Pts',(35.9564015056663,14.0714358194528,77.8966193385627));
#130729=CARTESIAN_POINT('Ctrl Pts',(35.9325772396664,14.0787477537516,77.8803130083138));
#130730=CARTESIAN_POINT('Ctrl Pts',(35.9085200506683,14.0858906018936,77.8643943068697));
#130731=CARTESIAN_POINT('Ctrl Pts',(35.9000853007769,14.0883949733559,77.8588130120107));
#130732=CARTESIAN_POINT('Ctrl Pts',(35.8916221174696,14.0908787388124,77.8532789794143));
#130733=CARTESIAN_POINT('Ctrl Pts',(35.8831444455004,14.0933378118669,77.8478019599974));
#130734=CARTESIAN_POINT('Ctrl Pts',(35.8818762623415,14.0937056669863,77.8469826473593));
#130735=CARTESIAN_POINT('Ctrl Pts',(35.8806072317308,14.0940731498235,77.8461641921004));
#130736=CARTESIAN_POINT('Ctrl Pts',(35.8793373537139,14.0944402608808,77.8453465942344));
#130737=CARTESIAN_POINT('Ctrl Pts',(35.8396948890402,14.105900564095,77.8198232021532));
#130738=CARTESIAN_POINT('Ctrl Pts',(35.7992265591956,14.1169982935614,77.7951356522314));
#130739=CARTESIAN_POINT('Ctrl Pts',(35.7579333334925,14.1277470638494,77.7712893746665));
#130740=CARTESIAN_POINT('Ctrl Pts',(35.7392147843485,14.1326195673035,77.7604796665146));
#130741=CARTESIAN_POINT('Ctrl Pts',(35.7203267314783,14.1374203733427,77.7498428800502));
#130742=CARTESIAN_POINT('Ctrl Pts',(35.7012692658199,14.1421509171572,77.7393794462338));
#130743=CARTESIAN_POINT('Ctrl Pts',(35.6986329392312,14.1428053199335,77.7379319804861));
#130744=CARTESIAN_POINT('Ctrl Pts',(35.6959933706936,14.1434583783386,77.7364878319158));
#130745=CARTESIAN_POINT('Ctrl Pts',(35.693350560544,14.1441100928129,77.7350470088184));
#130746=CARTESIAN_POINT('Ctrl Pts',(35.6824769884722,14.1467915053646,77.7291188895419));
#130747=CARTESIAN_POINT('Ctrl Pts',(35.6715485390952,14.1494501996738,77.7232469700815));
#130748=CARTESIAN_POINT('Ctrl Pts',(35.6605652265203,14.152086379761,77.7174313304439));
#130749=CARTESIAN_POINT('Ctrl Pts',(35.6523277420891,14.1540635148264,77.7130696007158));
#130750=CARTESIAN_POINT('Ctrl Pts',(35.6440593971144,14.1560279857181,77.7087395284178));
#130751=CARTESIAN_POINT('Ctrl Pts',(35.6357601976009,14.1579798800796,77.7044411476049));
#130752=CARTESIAN_POINT('Ctrl Pts',(35.632993797763,14.1586305115335,77.7030083540006));
#130753=CARTESIAN_POINT('Ctrl Pts',(35.6312566437295,14.159038510211,77.7021099864139));
#130754=CARTESIAN_POINT('Ctrl Pts',(35.6274507134639,14.159927585583,77.700153331884));
#130755=CARTESIAN_POINT('Ctrl Pts',(35.5902453846576,14.1686188487543,77.6810258203259));
#130756=CARTESIAN_POINT('Ctrl Pts',(35.5527081000862,14.1769924264008,77.6626793895717));
#130757=CARTESIAN_POINT('Ctrl Pts',(35.5148349612072,14.1850634367579,77.6451066981544));
#130758=CARTESIAN_POINT('Ctrl Pts',(35.4512220903169,14.1986197501503,77.6155910735347));
#130759=CARTESIAN_POINT('Ctrl Pts',(35.3866613241379,14.2113228793747,77.5882569010224));
#130760=CARTESIAN_POINT('Ctrl Pts',(35.3211605362392,14.2232164189763,77.5631320161429));
#130761=CARTESIAN_POINT('Ctrl Pts',(35.2980032775437,14.2274212809664,77.5542493220942));
#130762=CARTESIAN_POINT('Ctrl Pts',(35.2747285838988,14.2315248799444,77.5456430074866));
#130763=CARTESIAN_POINT('Ctrl Pts',(35.2513373519199,14.2355283160288,77.5373160290319));
#130764=CARTESIAN_POINT('Ctrl Pts',(35.2083795937033,14.2428805854393,77.5220236182921));
#130765=CARTESIAN_POINT('Ctrl Pts',(35.1650259012283,14.2498975030737,77.5076661870025));
#130766=CARTESIAN_POINT('Ctrl Pts',(35.1212771035081,14.2565914142495,77.4942454624149));
#130767=CARTESIAN_POINT('Ctrl Pts',(35.0993661923743,14.2599439565034,77.4875238993295));
#130768=CARTESIAN_POINT('Ctrl Pts',(35.077356146224,14.2632154521057,77.4810373778554));
#130769=CARTESIAN_POINT('Ctrl Pts',(35.0552470419858,14.2664069878756,77.4747869789205));
#130770=CARTESIAN_POINT('Ctrl Pts',(35.0221202281705,14.2711889731651,77.4654217961634));
#130771=CARTESIAN_POINT('Ctrl Pts',(34.988771045946,14.2757917356906,77.4565857932991));
#130772=CARTESIAN_POINT('Ctrl Pts',(34.9551997454641,14.280219626959,77.4482803889722));
#130773=CARTESIAN_POINT('Ctrl Pts',(34.9422709177221,14.2819248764622,77.4450818491382));
#130774=CARTESIAN_POINT('Ctrl Pts',(34.9293091485656,14.2836041887418,77.4419620088157));
#130775=CARTESIAN_POINT('Ctrl Pts',(34.9163144477114,14.2852578167427,77.4389209376207));
#130776=CARTESIAN_POINT('Ctrl Pts',(34.9124379744826,14.2857511135679,77.438013750052));
#130777=CARTESIAN_POINT('Ctrl Pts',(34.9085585705191,14.2862421246787,77.4371135724129));
#130778=CARTESIAN_POINT('Ctrl Pts',(34.9046762371865,14.2867308552347,77.4362204079851));
#130779=CARTESIAN_POINT('Ctrl Pts',(34.8962278979827,14.2877943809966,77.4342767943372));
#130780=CARTESIAN_POINT('Ctrl Pts',(34.8877656839372,14.2888471091787,77.4323663859133));
#130781=CARTESIAN_POINT('Ctrl Pts',(34.8792895983832,14.2898890981529,77.4304892016174));
#130782=CARTESIAN_POINT('Ctrl Pts',(34.8750515556062,14.2904100926399,77.4295506094695));
#130783=CARTESIAN_POINT('Ctrl Pts',(34.8708100449522,14.290928402325,77.4286203233538));
#130784=CARTESIAN_POINT('Ctrl Pts',(34.8665650668364,14.2914440345086,77.4276983456258));
#130785=CARTESIAN_POINT('Ctrl Pts',(34.8630614993612,14.2918696084689,77.426937396784));
#130786=CARTESIAN_POINT('Ctrl Pts',(34.8608359622675,14.292139014898,77.4264567387017));
#130787=CARTESIAN_POINT('Ctrl Pts',(34.8567182529457,14.2926345630268,77.4255759377945));
#130788=CARTESIAN_POINT('Ctrl Pts',(34.8558468801156,14.292739428898,77.4253895463037));
#130789=CARTESIAN_POINT('Ctrl Pts',(34.8548907417037,14.29285437067,77.425185390079));
#130790=CARTESIAN_POINT('Ctrl Pts',(34.8538197305188,14.2929829058584,77.4249573399584));
#130791=CARTESIAN_POINT('Ctrl Pts',(34.8050235101287,14.2988390831483,77.4145671740102));
#130792=CARTESIAN_POINT('Ctrl Pts',(34.7562088083104,14.30427527912,77.405416163315));
#130793=CARTESIAN_POINT('Ctrl Pts',(34.7073784381505,14.3093168215444,77.3974681360169));
#130794=CARTESIAN_POINT('Ctrl Pts',(34.6367845691646,14.3166053590719,77.3859777050425));
#130795=CARTESIAN_POINT('Ctrl Pts',(34.5661586592343,14.3230696569618,77.3769996824145));
#130796=CARTESIAN_POINT('Ctrl Pts',(34.4955002238291,14.3287650076083,77.370466012057));
#130797=CARTESIAN_POINT('Ctrl Pts',(34.4242963422592,14.3345043233829,77.3638819051815));
#130798=CARTESIAN_POINT('Ctrl Pts',(34.3530589739449,14.339462739832,77.3597798029414));
#130799=CARTESIAN_POINT('Ctrl Pts',(34.2817762337855,14.3436823305113,77.3581082693766));
#130800=CARTESIAN_POINT('Ctrl Pts',(34.2103212232019,14.3479121187599,77.3564326961832));
#130801=CARTESIAN_POINT('Ctrl Pts',(34.1388201014431,14.3513994978328,77.3571992693894));
#130802=CARTESIAN_POINT('Ctrl Pts',(34.0672795372947,14.3541443651951,77.360469723857));
#130803=CARTESIAN_POINT('Ctrl Pts',(33.995928686004,14.3568819536571,77.3637315056608));
#130804=CARTESIAN_POINT('Ctrl Pts',(33.924538247131,14.358880723838,77.3694846102313));
#130805=CARTESIAN_POINT('Ctrl Pts',(33.853048606998,14.3602097289537,77.3775449630649));
#130806=CARTESIAN_POINT('Ctrl Pts',(33.7930046121601,14.3613259574891,77.3843148360567));
#130807=CARTESIAN_POINT('Ctrl Pts',(33.7328896972954,14.3619703585475,77.3927103145005));
#130808=CARTESIAN_POINT('Ctrl Pts',(33.6728395094596,14.361977126785,77.4032750323744));
#130809=CARTESIAN_POINT('',(33.6728394518991,14.36197600861,77.403274705915));
#130810=CARTESIAN_POINT('Origin',(57.8121127436691,0.499074165591614,68.674471503788));
#130811=CARTESIAN_POINT('Ctrl Pts',(29.6420897207618,-14.3619786049856,
78.1139943677011));
#130812=CARTESIAN_POINT('Ctrl Pts',(29.4150088098653,-14.4336850553689,
77.9083573314674));
#130813=CARTESIAN_POINT('Ctrl Pts',(29.1961090381446,-14.5001071219915,
77.6973723716935));
#130814=CARTESIAN_POINT('Ctrl Pts',(28.988087795971,-14.5608976041789,77.4805442029342));
#130815=CARTESIAN_POINT('Ctrl Pts',(28.8137425456767,-14.6118468809053,
77.2988177553936));
#130816=CARTESIAN_POINT('Ctrl Pts',(28.6470387676822,-14.6588395856372,
77.1129870427136));
#130817=CARTESIAN_POINT('Ctrl Pts',(28.489566865647,-14.7016466499152,76.9227741006316));
#130818=CARTESIAN_POINT('Ctrl Pts',(28.328472849534,-14.7454383474399,76.7281859464236));
#130819=CARTESIAN_POINT('Ctrl Pts',(28.1771332810037,-14.784864646458,76.5288895083911));
#130820=CARTESIAN_POINT('Ctrl Pts',(28.037477697831,-14.8195994014424,76.3249565636834));
#130821=CARTESIAN_POINT('Ctrl Pts',(27.8986632578008,-14.8541249496032,
76.1222519035461));
#130822=CARTESIAN_POINT('Ctrl Pts',(27.7713925293067,-14.8840150929903,
75.9149666874586));
#130823=CARTESIAN_POINT('Ctrl Pts',(27.6575651521258,-14.9089932661783,
75.7031983825737));
#130824=CARTESIAN_POINT('Ctrl Pts',(27.6404658644236,-14.9127455178791,
75.6713862890237));
#130825=CARTESIAN_POINT('Ctrl Pts',(27.6236699529832,-14.916387008058,75.639473073654));
#130826=CARTESIAN_POINT('Ctrl Pts',(27.60718386578,-14.9199168893285,75.6074591138482));
#130827=CARTESIAN_POINT('',(36.6019507223326,-13.7800919958273,78.5369560490225));
#130828=CARTESIAN_POINT('Ctrl Pts',(33.6728409414565,-14.3619769299805,
77.4032752837662));
#130829=CARTESIAN_POINT('Ctrl Pts',(33.7272025377404,-14.361970498807,77.3937110128019));
#130830=CARTESIAN_POINT('Ctrl Pts',(33.7815742626743,-14.3615351034956,
77.3856122868006));
#130831=CARTESIAN_POINT('Ctrl Pts',(33.8359564067913,-14.3606723999005,
77.3789753427906));
#130832=CARTESIAN_POINT('Ctrl Pts',(33.9066462029422,-14.3595509961334,
77.3703481688026));
#130833=CARTESIAN_POINT('Ctrl Pts',(33.9773542073291,-14.3577080326573,
77.3641892993487));
#130834=CARTESIAN_POINT('Ctrl Pts',(34.04807857051,-14.355129255808,77.3605032924183));
#130835=CARTESIAN_POINT('Ctrl Pts',(34.0992590960304,-14.3532630933088,
77.3578358697187));
#130836=CARTESIAN_POINT('Ctrl Pts',(34.1504484442645,-14.3510120544897,
77.3564618530038));
#130837=CARTESIAN_POINT('Ctrl Pts',(34.2016464248871,-14.34837174654,77.3563790209224));
#130838=CARTESIAN_POINT('Ctrl Pts',(34.2130363325421,-14.3477843627534,
77.3563605934425));
#130839=CARTESIAN_POINT('Ctrl Pts',(34.2244266638507,-14.3471776973984,
77.3564061216377));
#130840=CARTESIAN_POINT('Ctrl Pts',(34.2358174143738,-14.3465516544306,
77.3565155763719));
#130841=CARTESIAN_POINT('Ctrl Pts',(34.2671136743056,-14.3448315918756,
77.3568163049152));
#130842=CARTESIAN_POINT('Ctrl Pts',(34.2984131089727,-14.3429653097249,
77.3575994149109));
#130843=CARTESIAN_POINT('Ctrl Pts',(34.3297156117792,-14.340950787442,77.3588643018472));
#130844=CARTESIAN_POINT('Ctrl Pts',(34.3453668631825,-14.3399435263006,
77.3594967453153));
#130845=CARTESIAN_POINT('Ctrl Pts',(34.3610188815834,-14.3388992044659,
77.3602496328084));
#130846=CARTESIAN_POINT('Ctrl Pts',(34.3766716533494,-14.3378175653105,
77.3611228870165));
#130847=CARTESIAN_POINT('Ctrl Pts',(34.3844980392324,-14.3372767457328,
77.3615595141205));
#130848=CARTESIAN_POINT('Ctrl Pts',(34.3923246134542,-14.3367265967795,
77.3620262328891));
#130849=CARTESIAN_POINT('Ctrl Pts',(34.4001513742904,-14.3361670861053,
77.3625230335429));
#130850=CARTESIAN_POINT('Ctrl Pts',(34.4066761933168,-14.3357006471825,
77.3629371939378));
#130851=CARTESIAN_POINT('Ctrl Pts',(34.4140182080303,-14.3351679045298,
77.3634285831324));
#130852=CARTESIAN_POINT('Ctrl Pts',(34.4201339208968,-14.3347182637942,
77.3638567490773));
#130853=CARTESIAN_POINT('Ctrl Pts',(34.4213542309539,-14.3346285438999,
77.3639421839596));
#130854=CARTESIAN_POINT('Ctrl Pts',(34.4225257326911,-14.3345421830295,
77.3640249374553));
#130855=CARTESIAN_POINT('Ctrl Pts',(34.4236322149063,-14.334460436391,77.3641036713141));
#130856=CARTESIAN_POINT('Ctrl Pts',(34.4597437123129,-14.3317925276942,
77.3666732539962));
#130857=CARTESIAN_POINT('Ctrl Pts',(34.4957326686996,-14.3289393393633,
77.3698560515037));
#130858=CARTESIAN_POINT('Ctrl Pts',(34.5315995951639,-14.3258983524844,
77.3736496133823));
#130859=CARTESIAN_POINT('Ctrl Pts',(34.6014396266313,-14.3199769468819,
77.3810364320224));
#130860=CARTESIAN_POINT('Ctrl Pts',(34.6708180602052,-14.313344326686,77.3907363531963));
#130861=CARTESIAN_POINT('Ctrl Pts',(34.7397301308635,-14.3059682544703,
77.4027474724843));
#130862=CARTESIAN_POINT('Ctrl Pts',(34.7687691767077,-14.3028600312349,
77.4078088708767));
#130863=CARTESIAN_POINT('Ctrl Pts',(34.7977255652342,-14.2996199103586,
77.4132802005972));
#130864=CARTESIAN_POINT('Ctrl Pts',(34.8265993196458,-14.2962456152313,
77.4191605433792));
#130865=CARTESIAN_POINT('Ctrl Pts',(34.8495799359604,-14.293560014303,77.4238407072175));
#130866=CARTESIAN_POINT('Ctrl Pts',(34.8725082027622,-14.2907894109111,
77.4287799916888));
#130867=CARTESIAN_POINT('Ctrl Pts',(34.8953839390617,-14.2879323808891,
77.4339780314365));
#130868=CARTESIAN_POINT('Ctrl Pts',(34.9211927967197,-14.2847090231709,
77.4398425625797));
#130869=CARTESIAN_POINT('Ctrl Pts',(34.9469348594218,-14.2813756705961,
77.4460363981471));
#130870=CARTESIAN_POINT('Ctrl Pts',(34.9726100094389,-14.2779302667008,
77.4525588704641));
#130871=CARTESIAN_POINT('Ctrl Pts',(34.9854475844475,-14.2762075647531,
77.4558201066226));
#130872=CARTESIAN_POINT('Ctrl Pts',(34.9982684312438,-14.2744568492298,
77.459163501736));
#130873=CARTESIAN_POINT('Ctrl Pts',(35.0110725347527,-14.2726778586205,
77.4625889703087));
#130874=CARTESIAN_POINT('Ctrl Pts',(35.0174745865072,-14.2717883633158,
77.4643017045951));
#130875=CARTESIAN_POINT('Ctrl Pts',(35.023872452437,-14.27089179919,77.4660349572307));
#130876=CARTESIAN_POINT('Ctrl Pts',(35.0302661306316,-14.2699881332691,
77.4677887173792));
#130877=CARTESIAN_POINT('Ctrl Pts',(35.0356931412296,-14.2692210936433,
77.4692773245037));
#130878=CARTESIAN_POINT('Ctrl Pts',(35.0420294242761,-14.2683183798507,
77.4710354852173));
#130879=CARTESIAN_POINT('Ctrl Pts',(35.0469517917309,-14.2676123183688,
77.4724147355838));
#130880=CARTESIAN_POINT('Ctrl Pts',(35.0478285715033,-14.2674865535958,
77.4726604098114));
#130881=CARTESIAN_POINT('Ctrl Pts',(35.0486605342653,-14.2673670708111,
77.4728939369763));
#130882=CARTESIAN_POINT('Ctrl Pts',(35.0494346000841,-14.2672557969472,
77.4731115094452));
#130883=CARTESIAN_POINT('Ctrl Pts',(35.0623241236228,-14.2654028962588,
77.4767344642254));
#130884=CARTESIAN_POINT('Ctrl Pts',(35.0753465740663,-14.2634907558366,
77.4805104914103));
#130885=CARTESIAN_POINT('Ctrl Pts',(35.0885017828721,-14.261518982626,77.484438676299));
#130886=CARTESIAN_POINT('Ctrl Pts',(35.1345547101024,-14.254616323039,77.4981902187866));
#130887=CARTESIAN_POINT('Ctrl Pts',(35.1822339451496,-14.2469843083068,
77.5138031645961));
#130888=CARTESIAN_POINT('Ctrl Pts',(35.2315364670706,-14.2385942411379,
77.5312608583579));
#130889=CARTESIAN_POINT('Ctrl Pts',(35.2576548507792,-14.2341495396273,
77.5405092036062));
#130890=CARTESIAN_POINT('Ctrl Pts',(35.2842289482715,-14.2294917892299,
77.550275976932));
#130891=CARTESIAN_POINT('Ctrl Pts',(35.3112593298257,-14.2246143399155,
77.5605641669722));
#130892=CARTESIAN_POINT('Ctrl Pts',(35.3140793555763,-14.2241054853647,
77.5616375133022));
#130893=CARTESIAN_POINT('Ctrl Pts',(35.3169043406836,-14.2235942515125,
77.562716497919));
#130894=CARTESIAN_POINT('Ctrl Pts',(35.3197342849219,-14.223080632316,77.5638011189002));
#130895=CARTESIAN_POINT('Ctrl Pts',(35.3285237742618,-14.2214853887098,
77.5671698299947));
#130896=CARTESIAN_POINT('Ctrl Pts',(35.3373611008867,-14.2198671364423,
77.5705929090628));
#130897=CARTESIAN_POINT('Ctrl Pts',(35.3462462540574,-14.2182256868004,
77.5740702954494));
#130898=CARTESIAN_POINT('Ctrl Pts',(35.3540296323547,-14.2167877798478,
77.5771164797089));
#130899=CARTESIAN_POINT('Ctrl Pts',(35.3599572575574,-14.2156825647817,
77.579461915545));
#130900=CARTESIAN_POINT('Ctrl Pts',(35.3656786235503,-14.2146112070245,
77.5817371358453));
#130901=CARTESIAN_POINT('Ctrl Pts',(35.3685913724629,-14.2140657785121,
77.5828954510909));
#130902=CARTESIAN_POINT('Ctrl Pts',(35.3714502843064,-14.2135288364717,
77.584036354385));
#130903=CARTESIAN_POINT('Ctrl Pts',(35.3744709742961,-14.2129594153419,
77.5852472046803));
#130904=CARTESIAN_POINT('Ctrl Pts',(35.3923791327044,-14.2095836025881,
77.5924257297757));
#130905=CARTESIAN_POINT('Ctrl Pts',(35.4099953379316,-14.2061959516237,
77.5996561073567));
#130906=CARTESIAN_POINT('Ctrl Pts',(35.4273195837607,-14.2027964278702,
77.6069383021139));
#130907=CARTESIAN_POINT('Ctrl Pts',(35.4607114505945,-14.1962439669093,
77.6209744731535));
#130908=CARTESIAN_POINT('Ctrl Pts',(35.4930186015498,-14.1896473791923,
77.6352031769755));
#130909=CARTESIAN_POINT('Ctrl Pts',(35.5242411510413,-14.183006578874,77.6496241184234));
#130910=CARTESIAN_POINT('Ctrl Pts',(35.5254161386802,-14.1827566678829,
77.6501668168327));
#130911=CARTESIAN_POINT('Ctrl Pts',(35.5265895893368,-14.1825066941666,
77.6507097880553));
#130912=CARTESIAN_POINT('Ctrl Pts',(35.527761502806,-14.1822566576985,77.6512530321797));
#130913=CARTESIAN_POINT('Ctrl Pts',(35.5600742768922,-14.1753624866553,
77.6662317188553));
#130914=CARTESIAN_POINT('Ctrl Pts',(35.5901199709455,-14.1686382498632,
77.6809571423816));
#130915=CARTESIAN_POINT('Ctrl Pts',(35.6178208546784,-14.1622409278501,
77.6950090128537));
#130916=CARTESIAN_POINT('Ctrl Pts',(35.6455217384113,-14.155843605837,77.7090608833258));
#130917=CARTESIAN_POINT('Ctrl Pts',(35.672869329356,-14.1493103821472,77.7234596228866));
#130918=CARTESIAN_POINT('Ctrl Pts',(35.6998633988907,-14.1426379035811,
77.7382039349708));
#130919=CARTESIAN_POINT('Ctrl Pts',(35.7012774602112,-14.1422883714796,
77.73897630319));
#130920=CARTESIAN_POINT('Ctrl Pts',(35.7026905508738,-14.1419384571469,
77.7397496200118));
#130921=CARTESIAN_POINT('Ctrl Pts',(35.7041026711878,-14.1415881600775,
77.7405238852301));
#130922=CARTESIAN_POINT('Ctrl Pts',(35.7296475670897,-14.1352513755382,
77.7545301453251));
#130923=CARTESIAN_POINT('Ctrl Pts',(35.7548750275898,-14.1287893912822,
77.7688466343453));
#130924=CARTESIAN_POINT('Ctrl Pts',(35.7797848051706,-14.1221992814675,
77.7834722384713));
#130925=CARTESIAN_POINT('Ctrl Pts',(35.7929281994666,-14.1187220761225,
77.7911892917939));
#130926=CARTESIAN_POINT('Ctrl Pts',(35.8059831537425,-14.1152091991775,
77.7989923998503));
#130927=CARTESIAN_POINT('Ctrl Pts',(35.8189496368222,-14.1116602102718,
77.8068813858294));
#130928=CARTESIAN_POINT('Ctrl Pts',(35.8276686349742,-14.1092737784598,
77.8121861437774));
#130929=CARTESIAN_POINT('Ctrl Pts',(35.8368584600997,-14.1067289489184,
77.8178457671225));
#130930=CARTESIAN_POINT('Ctrl Pts',(35.8454873274808,-14.1043115113263,
77.8232242220107));
#130931=CARTESIAN_POINT('Ctrl Pts',(35.8496909049451,-14.1031338496779,
77.8258443517175));
#130932=CARTESIAN_POINT('Ctrl Pts',(35.8537618658522,-14.1019866869613,
77.8283971315277));
#130933=CARTESIAN_POINT('Ctrl Pts',(35.8575836406485,-14.10090445785,77.8308057970622));
#130934=CARTESIAN_POINT('Ctrl Pts',(35.859161032695,-14.1004577806689,77.8317999450849));
#130935=CARTESIAN_POINT('Ctrl Pts',(35.8607397270648,-14.1000095030216,
77.8327979050927));
#130936=CARTESIAN_POINT('Ctrl Pts',(35.862319725231,-14.0995596222712,77.8337996742316));
#130937=CARTESIAN_POINT('Ctrl Pts',(35.8989675468846,-14.0891247054091,
77.8570355598966));
#130938=CARTESIAN_POINT('Ctrl Pts',(35.9363187501883,-14.0778289565087,
77.8823174887484));
#130939=CARTESIAN_POINT('Ctrl Pts',(35.9743728723604,-14.065631652356,77.9096255199391));
#130940=CARTESIAN_POINT('Ctrl Pts',(35.9831256240291,-14.0628261750994,
77.9159065849573));
#130941=CARTESIAN_POINT('Ctrl Pts',(35.9919154615997,-14.0599729189671,
77.9222950088109));
#130942=CARTESIAN_POINT('Ctrl Pts',(36.0007421893682,-14.0570712344685,
77.9287908690435));
#130943=CARTESIAN_POINT('Ctrl Pts',(36.0008339072921,-14.0570410832635,
77.9288583670824));
#130944=CARTESIAN_POINT('Ctrl Pts',(36.0009256291984,-14.0570109268291,
77.9289258767226));
#130945=CARTESIAN_POINT('Ctrl Pts',(36.0010173550866,-14.0569807651646,
77.928993397964));
#130946=CARTESIAN_POINT('Ctrl Pts',(36.0254938233812,-14.0489323173462,
77.9470110106164));
#130947=CARTESIAN_POINT('Ctrl Pts',(36.0502552108871,-14.0405123339591,
77.9658522623971));
#130948=CARTESIAN_POINT('Ctrl Pts',(36.0753006900738,-14.0317086757779,
77.9855124604623));
#130949=CARTESIAN_POINT('Ctrl Pts',(36.0878234296672,-14.0273068466874,
77.9953425594949));
#130950=CARTESIAN_POINT('Ctrl Pts',(36.1004171912915,-14.0228090849255,
78.0053773900386));
#130951=CARTESIAN_POINT('Ctrl Pts',(36.1130818628475,-14.0182137803284,
78.0156163166988));
#130952=CARTESIAN_POINT('Ctrl Pts',(36.1159381083572,-14.0171774077653,
78.0179254873842));
#130953=CARTESIAN_POINT('Ctrl Pts',(36.1187979572607,-14.0161360746697,
78.0202450365019));
#130954=CARTESIAN_POINT('Ctrl Pts',(36.1216614144598,-14.0150897599198,
78.0225749611393));
#130955=CARTESIAN_POINT('Ctrl Pts',(36.1251462814536,-14.0138163804056,
78.0254105116304));
#130956=CARTESIAN_POINT('Ctrl Pts',(36.1286364928932,-14.0125356224787,
78.028261429478));
#130957=CARTESIAN_POINT('Ctrl Pts',(36.1321320379128,-14.0112474556699,
78.0311276953339));
#130958=CARTESIAN_POINT('Ctrl Pts',(36.1369172510304,-14.0094840245952,
78.0350514591232));
#130959=CARTESIAN_POINT('Ctrl Pts',(36.1423402142178,-14.0074737274822,
78.0395217443241));
#130960=CARTESIAN_POINT('Ctrl Pts',(36.1469848824806,-14.0057413974127,
78.0433719312452));
#130961=CARTESIAN_POINT('Ctrl Pts',(36.1485209646206,-14.0051684821624,
78.0446452629516));
#130962=CARTESIAN_POINT('Ctrl Pts',(36.1499722687784,-14.00462610118,78.0458504981156));
#130963=CARTESIAN_POINT('Ctrl Pts',(36.1512884913628,-14.0041335817444,
78.0469447278));
#130964=CARTESIAN_POINT('Ctrl Pts',(36.1782330656311,-13.9940511483721,
78.0693448547607));
#130965=CARTESIAN_POINT('Ctrl Pts',(36.2037212320875,-13.9842162837019,
78.0911091994145));
#130966=CARTESIAN_POINT('Ctrl Pts',(36.2277600458757,-13.9746408618653,
78.1122449979267));
#130967=CARTESIAN_POINT('Ctrl Pts',(36.2415208838529,-13.9691594837233,
78.1243440266646));
#130968=CARTESIAN_POINT('Ctrl Pts',(36.2548065124784,-13.9637630862073,
78.1362371448907));
#130969=CARTESIAN_POINT('Ctrl Pts',(36.2676148158524,-13.9584547731634,
78.147923948464));
#130970=CARTESIAN_POINT('Ctrl Pts',(36.2852063828794,-13.9511640694703,
78.1639751913482));
#130971=CARTESIAN_POINT('Ctrl Pts',(36.3019001339735,-13.9440388550898,
78.1796385997256));
#130972=CARTESIAN_POINT('Ctrl Pts',(36.3176964474293,-13.9370850777245,
78.1949163196451));
#130973=CARTESIAN_POINT('Ctrl Pts',(36.3185529732293,-13.9367080220439,
78.1957447256724));
#130974=CARTESIAN_POINT('Ctrl Pts',(36.3194068612149,-13.9363314697869,
78.1965719988951));
#130975=CARTESIAN_POINT('Ctrl Pts',(36.3202581102729,-13.9359554225258,
78.1973981381346));
#130976=CARTESIAN_POINT('Ctrl Pts',(36.3272563602897,-13.9328638798961,
78.2041899564549));
#130977=CARTESIAN_POINT('Ctrl Pts',(36.3340762696947,-13.9298064677979,
78.2109051346778));
#130978=CARTESIAN_POINT('Ctrl Pts',(36.3407178844198,-13.9267836947292,
78.2175438886205));
#130979=CARTESIAN_POINT('Ctrl Pts',(36.3457493310117,-13.9244937514121,
78.2225731679873));
#130980=CARTESIAN_POINT('Ctrl Pts',(36.3511819022624,-13.9219895669129,
78.2280732250152));
#130981=CARTESIAN_POINT('Ctrl Pts',(36.3559936534691,-13.9197452641846,
78.2330022598293));
#130982=CARTESIAN_POINT('Ctrl Pts',(36.358306108191,-13.9186666862991,78.2353710792759));
#130983=CARTESIAN_POINT('Ctrl Pts',(36.3604759564432,-13.9176483357899,
78.2376076286151));
#130984=CARTESIAN_POINT('Ctrl Pts',(36.3623934414974,-13.9167437885408,
78.2395944935088));
#130985=CARTESIAN_POINT('Ctrl Pts',(36.3749919734724,-13.9108006040469,
78.2526488747348));
#130986=CARTESIAN_POINT('Ctrl Pts',(36.3873118234454,-13.9048459166144,
78.2657120018899));
#130987=CARTESIAN_POINT('Ctrl Pts',(36.3993672617985,-13.898875701994,78.2787923249773));
#130988=CARTESIAN_POINT('Ctrl Pts',(36.4229875655499,-13.8871782191928,
78.3044206924779));
#130989=CARTESIAN_POINT('Ctrl Pts',(36.4455937762913,-13.8754216409494,
78.330114080275));
#130990=CARTESIAN_POINT('Ctrl Pts',(36.4672289647874,-13.8635913786357,
78.3559045591743));
#130991=CARTESIAN_POINT('Ctrl Pts',(36.487490605428,-13.8525121812565,78.3800576843251));
#130992=CARTESIAN_POINT('Ctrl Pts',(36.5069006425037,-13.8413682226984,
78.4042962747751));
#130993=CARTESIAN_POINT('Ctrl Pts',(36.5254653006551,-13.8301512702905,
78.4286404423582));
#130994=CARTESIAN_POINT('Ctrl Pts',(36.5427401219216,-13.8197136502481,
78.4512932238126));
#130995=CARTESIAN_POINT('Ctrl Pts',(36.5592829741807,-13.809212717274,78.4740376470478));
#130996=CARTESIAN_POINT('Ctrl Pts',(36.5750485509559,-13.7986683824196,
78.4968346922204));
#130997=CARTESIAN_POINT('Ctrl Pts',(36.5842881569723,-13.7924887480714,
78.5101951749186));
#130998=CARTESIAN_POINT('Ctrl Pts',(36.5932605244772,-13.7862941512809,
78.5235738259073));
#130999=CARTESIAN_POINT('Ctrl Pts',(36.6019498638648,-13.7800926665008,
78.5369546240003));
#131000=CARTESIAN_POINT('',(36.732951463716,-13.66231606687,78.7896965370107));
#131001=CARTESIAN_POINT('Ctrl Pts',(36.6019526015505,-13.7800906846102,
78.5369587979563));
#131002=CARTESIAN_POINT('Ctrl Pts',(36.6186687600556,-13.7682869278469,
78.5623962793156));
#131003=CARTESIAN_POINT('Ctrl Pts',(36.6410689345548,-13.751533992336,78.598384532446));
#131004=CARTESIAN_POINT('Ctrl Pts',(36.6597206152858,-13.7363178480004,
78.6309989125395));
#131005=CARTESIAN_POINT('Ctrl Pts',(36.6713225306487,-13.7265215745043,
78.6519946927202));
#131006=CARTESIAN_POINT('Ctrl Pts',(36.6772545910443,-13.7212964464913,
78.6631933561585));
#131007=CARTESIAN_POINT('Ctrl Pts',(36.6993608981787,-13.701065109125,78.706581709443));
#131008=CARTESIAN_POINT('Ctrl Pts',(36.7163702000577,-13.6827870327493,
78.745902507885));
#131009=CARTESIAN_POINT('Ctrl Pts',(36.7329514516655,-13.6623159070804,
78.7896964668812));
#131010=CARTESIAN_POINT('',(36.7432202460569,-13.6362301419005,78.8470059772675));
#131011=CARTESIAN_POINT('Ctrl Pts',(36.732951638443,-13.6623156764858,78.7896969601932));
#131012=CARTESIAN_POINT('Ctrl Pts',(36.7358943168784,-13.6534550679484,
78.8093974025206));
#131013=CARTESIAN_POINT('Ctrl Pts',(36.7390843317269,-13.6445697336436,
78.8289974475113));
#131014=CARTESIAN_POINT('Ctrl Pts',(36.7385844993717,-13.6362413718505,
78.8476679968162));
#131015=CARTESIAN_POINT('',(37.505104684855,-10.7061845463452,83.1298573144579));
#131016=CARTESIAN_POINT('Origin',(35.6454492392491,0.499074165591614,72.5830523519042));
#131017=CARTESIAN_POINT('',(44.6819372453691,-0.790063546693886,86.67424130138));
#131018=CARTESIAN_POINT('Ctrl Pts',(44.6819372453691,-0.790063546693886,
86.67424130138));
#131019=CARTESIAN_POINT('Ctrl Pts',(44.6247705097188,-1.31120277256221,
86.6400071574514));
#131020=CARTESIAN_POINT('Ctrl Pts',(44.5244235625226,-1.8281974408512,86.5868803494066));
#131021=CARTESIAN_POINT('Ctrl Pts',(44.2439884476587,-2.84029710432558,
86.4453289128632));
#131022=CARTESIAN_POINT('Ctrl Pts',(44.0639901013491,-3.33552362347414,
86.3569370305293));
#131023=CARTESIAN_POINT('Ctrl Pts',(43.421984756127,-4.77832198714366,86.045504650961));
#131024=CARTESIAN_POINT('Ctrl Pts',(42.8581121434222,-5.68082820437495,
85.7763936738176));
#131025=CARTESIAN_POINT('Ctrl Pts',(41.5521349176424,-7.34586556449325,
85.1489543034165));
#131026=CARTESIAN_POINT('Ctrl Pts',(40.8103108900288,-8.10938402555221,
84.7907746159092));
#131027=CARTESIAN_POINT('Ctrl Pts',(39.2226854324597,-9.50361172924995,
84.0079690139411));
#131028=CARTESIAN_POINT('Ctrl Pts',(38.3764113480733,-10.134813445805,83.5832161340583));
#131029=CARTESIAN_POINT('Ctrl Pts',(37.5051065718069,-10.7061611690822,
83.129837958246));
#131030=CARTESIAN_POINT('',(66.1162021796967,-0.790200987013387,82.8948096729252));
#131031=CARTESIAN_POINT('',(44.6819400502385,-0.790064894780452,86.6742572085851));
#131032=CARTESIAN_POINT('',(63.7044145293691,-14.9224898553757,69.2168822194142));
#131033=CARTESIAN_POINT('Origin',(63.4339821949991,0.499074165591614,67.683184237498));
#131034=CARTESIAN_POINT('',(63.7242525775431,-14.9985986835124,67.8461529431334));
#131035=CARTESIAN_POINT('Ctrl Pts',(63.7242555858646,-14.9994907861995,
67.8461682206232));
#131036=CARTESIAN_POINT('Ctrl Pts',(63.6999435022481,-14.9979924635271,
67.9622549775836));
#131037=CARTESIAN_POINT('Ctrl Pts',(63.681735399389,-14.9952970619206,68.0786951824008));
#131038=CARTESIAN_POINT('Ctrl Pts',(63.6693017595057,-14.99134917377,68.1948747105009));
#131039=CARTESIAN_POINT('Ctrl Pts',(63.6570882649006,-14.9874711854189,
68.3089972082561));
#131040=CARTESIAN_POINT('Ctrl Pts',(63.6504465299545,-14.9823847045197,
68.4228679931466));
#131041=CARTESIAN_POINT('Ctrl Pts',(63.6490641819511,-14.9760888534598,
68.5359047043168));
#131042=CARTESIAN_POINT('Ctrl Pts',(63.6476444592164,-14.9696227806171,
68.6519976044444));
#131043=CARTESIAN_POINT('Ctrl Pts',(63.6517723278146,-14.9618807905353,
68.7672105049499));
#131044=CARTESIAN_POINT('Ctrl Pts',(63.6611098706025,-14.9529192231808,
68.8809152638675));
#131045=CARTESIAN_POINT('Ctrl Pts',(63.6704474133904,-14.9439576558262,
68.9946200227852));
#131046=CARTESIAN_POINT('Ctrl Pts',(63.6849945952704,-14.933776612024,69.1068164410672));
#131047=CARTESIAN_POINT('Ctrl Pts',(63.7044145293206,-14.9224898553757,
69.2168822194228));
#131048=CARTESIAN_POINT('Ctrl Pts',(27.2861973898773,-14.9986800996563,
74.271170552334));
#131049=CARTESIAN_POINT('Ctrl Pts',(39.4322141020864,-14.9978694362286,
72.1294879217807));
#131050=CARTESIAN_POINT('Ctrl Pts',(51.5782329298002,-14.9978694348211,
69.9878171992915));
#131051=CARTESIAN_POINT('Ctrl Pts',(63.7242533594791,-14.99854733863,67.846155561997));
#131052=CARTESIAN_POINT('Origin',(58.0356083261291,-9.5,68.77323523472));
#131053=CARTESIAN_POINT('',(65.9990597672842,-14.4574398737317,64.9541505386072));
#131054=CARTESIAN_POINT('Ctrl Pts',(65.9990597672842,-14.4574398737317,
64.9541505386072));
#131055=CARTESIAN_POINT('Ctrl Pts',(65.9270095132669,-14.457429104092,64.9668321465929));
#131056=CARTESIAN_POINT('Ctrl Pts',(65.8553939405631,-14.4591199027381,
64.9830287465842));
#131057=CARTESIAN_POINT('Ctrl Pts',(65.784532717612,-14.4625090986378,65.0027367719546));
#131058=CARTESIAN_POINT('Ctrl Pts',(65.7329671490077,-14.4649754096384,
65.0170782621515));
#131059=CARTESIAN_POINT('Ctrl Pts',(65.6818011220681,-14.4683401652805,
65.03327966161));
#131060=CARTESIAN_POINT('Ctrl Pts',(65.6311590992478,-14.4725863916555,
65.0513468480837));
#131061=CARTESIAN_POINT('Ctrl Pts',(65.5710420430455,-14.4776270795155,
65.0727943733634));
#131062=CARTESIAN_POINT('Ctrl Pts',(65.5116611670506,-14.4839081718085,
65.0968661895181));
#131063=CARTESIAN_POINT('Ctrl Pts',(65.4532016956852,-14.49136284998,65.123557551863));
#131064=CARTESIAN_POINT('Ctrl Pts',(65.4239719600025,-14.4950901890658,
65.1369032330354));
#131065=CARTESIAN_POINT('Ctrl Pts',(65.3949702682945,-14.4991102138833,
65.1509037399944));
#131066=CARTESIAN_POINT('Ctrl Pts',(65.3662323314153,-14.5034123711069,
65.1655579908485));
#131067=CARTESIAN_POINT('Ctrl Pts',(65.3518633629756,-14.5055634497187,
65.1728851162755));
#131068=CARTESIAN_POINT('Ctrl Pts',(65.3375603353684,-14.5077850356995,
65.1803756897286));
#131069=CARTESIAN_POINT('Ctrl Pts',(65.3233279147348,-14.5100756367114,
65.1880295723925));
#131070=CARTESIAN_POINT('Ctrl Pts',(65.3162117044181,-14.5112209372173,
65.1918565137245));
#131071=CARTESIAN_POINT('Ctrl Pts',(65.3091131459849,-14.5123834898947,
65.1957242831542));
#131072=CARTESIAN_POINT('Ctrl Pts',(65.3020327945485,-14.5135630957985,
65.199632866648));
#131073=CARTESIAN_POINT('Ctrl Pts',(65.294952443112,-14.5147427017023,65.2035414501419));
#131074=CARTESIAN_POINT('Ctrl Pts',(65.2861174085656,-14.5162448133906,
65.2084952227636));
#131075=CARTESIAN_POINT('Ctrl Pts',(65.2808469250696,-14.5171528679838,
65.2114810471074));
#131076=CARTESIAN_POINT('Ctrl Pts',(65.2471863459398,-14.5229522682689,
65.2305503747447));
#131077=CARTESIAN_POINT('Ctrl Pts',(65.2102793351576,-14.529835281351,65.2527723345158));
#131078=CARTESIAN_POINT('Ctrl Pts',(65.170514597363,-14.5379387602517,65.2786049054499));
#131079=CARTESIAN_POINT('Ctrl Pts',(65.1341288410832,-14.5453536515511,
65.3022423712606));
#131080=CARTESIAN_POINT('Ctrl Pts',(65.0953503875563,-14.5537906843503,
65.3289028868235));
#131081=CARTESIAN_POINT('Ctrl Pts',(65.0544797357755,-14.5633146115661,
65.3589526481561));
#131082=CARTESIAN_POINT('Ctrl Pts',(65.0281172728456,-14.5694577526034,
65.3783354004408));
#131083=CARTESIAN_POINT('Ctrl Pts',(65.0008843990089,-14.5760522986969,
65.3991285700309));
#131084=CARTESIAN_POINT('Ctrl Pts',(64.9728624378503,-14.5831045879113,
65.4214342907374));
#131085=CARTESIAN_POINT('Ctrl Pts',(64.934797171896,-14.5926844764499,65.4517345679446));
#131086=CARTESIAN_POINT('Ctrl Pts',(64.8952962752854,-14.6031201309233,
65.4848433642836));
#131087=CARTESIAN_POINT('Ctrl Pts',(64.854649312531,-14.6144275372323,65.5211013146095));
#131088=CARTESIAN_POINT('Ctrl Pts',(64.8317911295075,-14.6207863582958,
65.5414912972415));
#131089=CARTESIAN_POINT('Ctrl Pts',(64.8085705507282,-14.6274200722944,
65.5628774467885));
#131090=CARTESIAN_POINT('Ctrl Pts',(64.7850394363295,-14.634324440184,65.5853223999462));
#131091=CARTESIAN_POINT('Ctrl Pts',(64.7523520864935,-14.6439153794305,
65.6165009503322));
#131092=CARTESIAN_POINT('Ctrl Pts',(64.7190722998677,-14.6540298778063,
65.6497217557215));
#131093=CARTESIAN_POINT('Ctrl Pts',(64.6853904030749,-14.6646369600161,
65.6851483623767));
#131094=CARTESIAN_POINT('Ctrl Pts',(64.6685494546785,-14.6699405011211,
65.7028616657043));
#131095=CARTESIAN_POINT('Ctrl Pts',(64.6516084134835,-14.6753668640736,
65.7211265619829));
#131096=CARTESIAN_POINT('Ctrl Pts',(64.6345938415512,-14.6809100308888,
65.7399643525514));
#131097=CARTESIAN_POINT('Ctrl Pts',(64.626086555585,-14.6836816142964,65.7493832478357));
#131098=CARTESIAN_POINT('Ctrl Pts',(64.6175608885395,-14.686482372973,65.7589453757946));
#131099=CARTESIAN_POINT('Ctrl Pts',(64.6090203879065,-14.6893114063194,
65.7686534527022));
#131100=CARTESIAN_POINT('Ctrl Pts',(64.6011479460988,-14.6919191457656,
65.7776021401157));
#131101=CARTESIAN_POINT('Ctrl Pts',(64.5921868900647,-14.6949139227446,
65.7879309235735));
#131102=CARTESIAN_POINT('Ctrl Pts',(64.5851155508268,-14.6972910105629,
65.7961684881991));
#131103=CARTESIAN_POINT('Ctrl Pts',(64.5845154739129,-14.6974927312659,
65.7968675315051));
#131104=CARTESIAN_POINT('Ctrl Pts',(64.5839290036382,-14.6976900332066,
65.7975515053185));
#131105=CARTESIAN_POINT('Ctrl Pts',(64.5833579591697,-14.6978823175386,
65.7982182831661));
#131106=CARTESIAN_POINT('Ctrl Pts',(64.5249558489375,-14.717547705039,65.8664112795133));
#131107=CARTESIAN_POINT('Ctrl Pts',(64.4695712568179,-14.7373782766372,
65.9376452711858));
#131108=CARTESIAN_POINT('Ctrl Pts',(64.4175227606522,-14.7569885426821,
66.011790428281));
#131109=CARTESIAN_POINT('Ctrl Pts',(64.3914985125693,-14.7667936757046,
66.0488630068287));
#131110=CARTESIAN_POINT('Ctrl Pts',(64.3663083025939,-14.7765435299738,
66.0866634568049));
#131111=CARTESIAN_POINT('Ctrl Pts',(64.3419912851458,-14.7861886364692,
66.1251755013527));
#131112=CARTESIAN_POINT('Ctrl Pts',(64.3298327764217,-14.7910111897169,
66.1444315236266));
#131113=CARTESIAN_POINT('Ctrl Pts',(64.3178925663944,-14.7958075451137,
66.163865447748));
#131114=CARTESIAN_POINT('Ctrl Pts',(64.3061755059024,-14.8005714396201,
66.1834752027238));
#131115=CARTESIAN_POINT('Ctrl Pts',(64.3003169756564,-14.8029533868733,
66.1932800802117));
#131116=CARTESIAN_POINT('Ctrl Pts',(64.2945142328176,-14.8053272182757,
66.2031289155464));
#131117=CARTESIAN_POINT('Ctrl Pts',(64.2887678799285,-14.8076921461525,
66.2130214471302));
#131118=CARTESIAN_POINT('Ctrl Pts',(64.2830215270394,-14.8100570740294,
66.2229139787141));
#131119=CARTESIAN_POINT('Ctrl Pts',(64.2767774131408,-14.8126439219698,
66.2338319698607));
#131120=CARTESIAN_POINT('Ctrl Pts',(64.2716985922896,-14.8147594287093,
66.242829868022));
#131121=CARTESIAN_POINT('Ctrl Pts',(64.2455179843022,-14.8256645687533,
66.2892127689693));
#131122=CARTESIAN_POINT('Ctrl Pts',(64.2186897195521,-14.8367435952576,
66.3383173283336));
#131123=CARTESIAN_POINT('Ctrl Pts',(64.1915599660569,-14.8478672945918,
66.3903785105779));
#131124=CARTESIAN_POINT('Ctrl Pts',(64.1765861418789,-14.8540068386931,
66.4191128295079));
#131125=CARTESIAN_POINT('Ctrl Pts',(64.1615204845469,-14.860159138803,66.4487478811398));
#131126=CARTESIAN_POINT('Ctrl Pts',(64.146421231491,-14.8662955758726,66.479323365031));
#131127=CARTESIAN_POINT('Ctrl Pts',(64.1251931014459,-14.874922829396,66.5223096204327));
#131128=CARTESIAN_POINT('Ctrl Pts',(64.1039048702332,-14.8835197451949,
66.5671536303125));
#131129=CARTESIAN_POINT('Ctrl Pts',(64.0827596108614,-14.8919890457415,
66.6139619949472));
#131130=CARTESIAN_POINT('Ctrl Pts',(64.0721869811755,-14.8962236960148,
66.6373661772646));
#131131=CARTESIAN_POINT('Ctrl Pts',(64.0616505576379,-14.9004261006137,
66.6612614116885));
#131132=CARTESIAN_POINT('Ctrl Pts',(64.0511786752497,-14.9045819186505,
66.6856607382273));
#131133=CARTESIAN_POINT('Ctrl Pts',(64.0459427340556,-14.9066598276688,
66.6978604014967));
#131134=CARTESIAN_POINT('Ctrl Pts',(64.0407229289312,-14.9087260667076,
66.7101860922319));
#131135=CARTESIAN_POINT('Ctrl Pts',(64.0355230345318,-14.9107786956948,
66.7226394085536));
#131136=CARTESIAN_POINT('Ctrl Pts',(64.0329230873321,-14.9118050101884,
66.7288660667144));
#131137=CARTESIAN_POINT('Ctrl Pts',(64.0303281178679,-14.9128279206411,
66.7351246315797));
#131138=CARTESIAN_POINT('Ctrl Pts',(64.0277386058808,-14.9138471750793,
66.7414153025324));
#131139=CARTESIAN_POINT('Ctrl Pts',(64.0251490938937,-14.9148664295174,
66.7477059734851));
#131140=CARTESIAN_POINT('Ctrl Pts',(64.0219496993838,-14.9161234947288,
66.7555455694723));
#131141=CARTESIAN_POINT('Ctrl Pts',(64.0199869263796,-14.9168937119836,
66.7603838331213));
#131142=CARTESIAN_POINT('Ctrl Pts',(63.9930424016886,-14.9274670884227,
66.8268024735216));
#131143=CARTESIAN_POINT('Ctrl Pts',(63.9667351901692,-14.9373914127289,
66.8954367155941));
#131144=CARTESIAN_POINT('Ctrl Pts',(63.9414487228419,-14.9464636582685,
66.9664575673575));
#131145=CARTESIAN_POINT('Ctrl Pts',(63.9170190071715,-14.9552285195738,
67.0350721030613));
#131146=CARTESIAN_POINT('Ctrl Pts',(63.893542086014,-14.9631981366324,67.1059145343941));
#131147=CARTESIAN_POINT('Ctrl Pts',(63.8713619612557,-14.9701418134995,
67.1791290840267));
#131148=CARTESIAN_POINT('Ctrl Pts',(63.8629841166152,-14.9727645690818,
67.20678357781));
#131149=CARTESIAN_POINT('Ctrl Pts',(63.8547912654684,-14.9752404488901,
67.2347763792355));
#131150=CARTESIAN_POINT('Ctrl Pts',(63.8468018538309,-14.9775551290378,
67.2631147380346));
#131151=CARTESIAN_POINT('Ctrl Pts',(63.8212844927312,-14.9849479799559,
67.3536245486764));
#131152=CARTESIAN_POINT('Ctrl Pts',(63.7978340122759,-14.9906976585156,
67.4476669344656));
#131153=CARTESIAN_POINT('Ctrl Pts',(63.7771704812227,-14.994266115557,67.5449460559198));
#131154=CARTESIAN_POINT('Ctrl Pts',(63.7565069501695,-14.9978345725983,
67.642225177374));
#131155=CARTESIAN_POINT('Ctrl Pts',(63.7386304626905,-14.9992212736701,
67.7427415685702));
#131156=CARTESIAN_POINT('Ctrl Pts',(63.7242517575141,-14.9978694334135,
67.8461464768021));
#131157=CARTESIAN_POINT('',(82.7407915597954,-14.4574398738313,62.0021315200116));
#131158=CARTESIAN_POINT('',(83.2822162694133,-14.4574398738744,61.9066637357724));
#131159=CARTESIAN_POINT('',(82.3362806376591,-12.34366528766,59.70878371338));
#131160=CARTESIAN_POINT('Origin',(83.1537660643691,-9.5,64.344226319777));
#131161=CARTESIAN_POINT('',(62.6710204155491,-11.87440155793,62.91980324276));
#131162=CARTESIAN_POINT('Ctrl Pts',(82.3362806376591,-12.34366528766,59.70878371338));
#131163=CARTESIAN_POINT('Ctrl Pts',(81.5289715591157,-12.5189817352091,
59.9597488743679));
#131164=CARTESIAN_POINT('Ctrl Pts',(80.7191589758644,-12.6646044612898,
60.205268368155));
#131165=CARTESIAN_POINT('Ctrl Pts',(79.0922716340717,-12.9033042732495,
60.6726263401023));
#131166=CARTESIAN_POINT('Ctrl Pts',(78.2740835955906,-12.9965399890585,
60.8947778340494));
#131167=CARTESIAN_POINT('Ctrl Pts',(76.6333619159099,-13.1367557266633,
61.3054335510454));
#131168=CARTESIAN_POINT('Ctrl Pts',(75.8144583018363,-13.1835019769691,
61.4930702647479));
#131169=CARTESIAN_POINT('Ctrl Pts',(74.5876982409067,-13.2215047114112,
61.7446398483009));
#131170=CARTESIAN_POINT('Ctrl Pts',(74.1790500717552,-13.2287938444501,
61.8235492499852));
#131171=CARTESIAN_POINT('Ctrl Pts',(73.5664630342142,-13.2317789353712,
61.9343647160185));
#131172=CARTESIAN_POINT('Ctrl Pts',(73.3623319014373,-13.2314474053304,
61.9700470478659));
#131173=CARTESIAN_POINT('Ctrl Pts',(72.9541990694171,-13.2281294125987,
62.0389013302574));
#131174=CARTESIAN_POINT('Ctrl Pts',(72.7513086447414,-13.2251664982903,
62.0718993111952));
#131175=CARTESIAN_POINT('Ctrl Pts',(71.7260750308394,-13.2034383942672,
62.2323964648994));
#131176=CARTESIAN_POINT('Ctrl Pts',(70.901717929154,-13.1646760772142,62.3414667200486));
#131177=CARTESIAN_POINT('Ctrl Pts',(69.6594184975944,-13.0719790447237,
62.4788685448483));
#131178=CARTESIAN_POINT('Ctrl Pts',(69.2443638049454,-13.0352930516122,
62.5203344903412));
#131179=CARTESIAN_POINT('Ctrl Pts',(68.6204663969968,-12.9710473833339,
62.5766946947534));
#131180=CARTESIAN_POINT('Ctrl Pts',(68.3081894608378,-12.9366182519558,
62.6034185783192));
#131181=CARTESIAN_POINT('Ctrl Pts',(67.9433242738696,-12.8922774289481,
62.6322313077126));
#131182=CARTESIAN_POINT('Ctrl Pts',(67.7607607235711,-12.869045168763,62.646072288788));
#131183=CARTESIAN_POINT('Ctrl Pts',(67.6824916428283,-12.8588589471043,
62.6518858367753));
#131184=CARTESIAN_POINT('Ctrl Pts',(67.6303061887625,-12.8520168987905,
62.6557355716152));
#131185=CARTESIAN_POINT('Ctrl Pts',(67.605471099205,-12.848737986768,62.6575557243891));
#131186=CARTESIAN_POINT('Ctrl Pts',(65.8271077618809,-12.6121314762894,
62.7869577419132));
#131187=CARTESIAN_POINT('Ctrl Pts',(64.188516413027,-12.295603114885,62.8572957814988));
#131188=CARTESIAN_POINT('Ctrl Pts',(62.6710204155491,-11.87440155793,62.91980324276));
#131189=CARTESIAN_POINT('',(36.1590071618821,-11.8741528675302,67.5951619717139));
#131190=CARTESIAN_POINT('',(36.1589535195822,-11.8742995089298,67.5948528813764));
#131191=CARTESIAN_POINT('',(35.3959116334435,-12.2791716992138,67.9475259026238));
#131192=CARTESIAN_POINT('Ctrl Pts',(35.3959116334435,-12.2791716992137,
67.9475259026238));
#131193=CARTESIAN_POINT('Ctrl Pts',(35.500819870766,-12.228986514838,67.8990761283221));
#131194=CARTESIAN_POINT('Ctrl Pts',(35.5993587298791,-12.1799558327146,
67.8535278096658));
#131195=CARTESIAN_POINT('Ctrl Pts',(35.6918786734976,-12.1322701611091,
67.8107381519324));
#131196=CARTESIAN_POINT('Ctrl Pts',(35.786399164668,-12.0835533879935,67.7670232586047));
#131197=CARTESIAN_POINT('Ctrl Pts',(35.8746375695955,-12.0362405275576,
67.7261873566712));
#131198=CARTESIAN_POINT('Ctrl Pts',(35.9569194368958,-11.9905098620958,
67.6880679527576));
#131199=CARTESIAN_POINT('Ctrl Pts',(36.0287090291249,-11.9506105995537,
67.6548093922416));
#131200=CARTESIAN_POINT('Ctrl Pts',(36.0959635043088,-11.9119153534715,
67.6236184209543));
#131201=CARTESIAN_POINT('Ctrl Pts',(36.158870968792,-11.874526930468,67.5943834483743));
#131202=CARTESIAN_POINT('Ctrl Pts',(27.2015513459991,-14.9604546753208,
73.5554952088459));
#131203=CARTESIAN_POINT('Ctrl Pts',(27.2537025903662,-14.9462882647007,
73.4244569905557));
#131204=CARTESIAN_POINT('Ctrl Pts',(27.3252684746861,-14.9283662985821,
73.2922068281088));
#131205=CARTESIAN_POINT('Ctrl Pts',(27.412747118424,-14.9070793296614,73.1596515499058));
#131206=CARTESIAN_POINT('Ctrl Pts',(27.4999391612395,-14.8858621019332,
73.0275305544418));
#131207=CARTESIAN_POINT('Ctrl Pts',(27.6029398617996,-14.8613023293257,
72.8951064138094));
#131208=CARTESIAN_POINT('Ctrl Pts',(27.7182733036733,-14.8338054582636,
72.7632297613986));
#131209=CARTESIAN_POINT('Ctrl Pts',(27.8272278175409,-14.8078293998821,
72.6386470183496));
#131210=CARTESIAN_POINT('Ctrl Pts',(27.9470866107628,-14.7792198528575,
72.5144976463921));
#131211=CARTESIAN_POINT('Ctrl Pts',(28.0757305316629,-14.7482215091595,
72.3910614055773));
#131212=CARTESIAN_POINT('Ctrl Pts',(28.2074333096326,-14.7164860960213,
72.2646901343684));
#131213=CARTESIAN_POINT('Ctrl Pts',(28.3483438822667,-14.6822469401442,
72.1390658554838));
#131214=CARTESIAN_POINT('Ctrl Pts',(28.4961857531228,-14.6457145038354,
72.0144742663498));
#131215=CARTESIAN_POINT('Ctrl Pts',(28.5101650783585,-14.642260145433,72.002693393069));
#131216=CARTESIAN_POINT('Ctrl Pts',(28.5242063737892,-14.6387852456508,
71.9909217454062));
#131217=CARTESIAN_POINT('Ctrl Pts',(28.5383077140983,-14.6352899590774,
71.9791595606471));
#131218=CARTESIAN_POINT('Ctrl Pts',(28.6847794480744,-14.5989841417632,
71.8569848198595));
#131219=CARTESIAN_POINT('Ctrl Pts',(28.8377290347631,-14.5604732260721,
71.7358048516294));
#131220=CARTESIAN_POINT('Ctrl Pts',(28.9958806914247,-14.5198822842996,
71.6156910439134));
#131221=CARTESIAN_POINT('Ctrl Pts',(29.1567521931228,-14.4785932716132,
71.4935115547457));
#131222=CARTESIAN_POINT('Ctrl Pts',(29.3230061490674,-14.4351519447313,
71.3724347497099));
#131223=CARTESIAN_POINT('Ctrl Pts',(29.4933006217649,-14.3896366301522,
71.2525403307251));
#131224=CARTESIAN_POINT('Ctrl Pts',(29.5086621111986,-14.3855309007477,
71.2417252007844));
#131225=CARTESIAN_POINT('Ctrl Pts',(29.5240564794304,-14.381408260802,71.2309196977313));
#131226=CARTESIAN_POINT('Ctrl Pts',(29.5394827421391,-14.3772687475314,
71.2201238838441));
#131227=CARTESIAN_POINT('Ctrl Pts',(29.7221144459034,-14.3282610017378,
71.0923121175746));
#131228=CARTESIAN_POINT('Ctrl Pts',(29.9091906174023,-14.2768899174541,
70.9658567538731));
#131229=CARTESIAN_POINT('Ctrl Pts',(30.099730401364,-14.2232101873667,70.840797820168));
#131230=CARTESIAN_POINT('Ctrl Pts',(30.2791033513307,-14.1726764282798,
70.7230681293288));
#131231=CARTESIAN_POINT('Ctrl Pts',(30.4615457919628,-14.1200960307155,
70.6065757634804));
#131232=CARTESIAN_POINT('Ctrl Pts',(30.6462418466383,-14.0654748228539,
70.4913679270501));
#131233=CARTESIAN_POINT('Ctrl Pts',(30.860779879735,-14.0020282780938,70.3575455632291));
#131234=CARTESIAN_POINT('Ctrl Pts',(31.0782473012234,-13.9358160337048,
70.225457787358));
#131235=CARTESIAN_POINT('Ctrl Pts',(31.2978702818636,-13.8668363361836,
70.0951844910434));
#131236=CARTESIAN_POINT('Ctrl Pts',(31.517347052676,-13.7979025605858,69.9649979217014));
#131237=CARTESIAN_POINT('Ctrl Pts',(31.7389764286382,-13.7262046325469,
69.8366229352475));
#131238=CARTESIAN_POINT('Ctrl Pts',(31.9619915002813,-13.6516990359388,
69.710169748752));
#131239=CARTESIAN_POINT('Ctrl Pts',(32.1834412073867,-13.5777164013796,
69.584604149505));
#131240=CARTESIAN_POINT('Ctrl Pts',(32.4062571525262,-13.5009649386618,
69.4609330508715));
#131241=CARTESIAN_POINT('Ctrl Pts',(32.6296949326618,-13.4213670101209,
69.3393010612166));
#131242=CARTESIAN_POINT('Ctrl Pts',(32.7555951577233,-13.3765160582735,
69.2707652260371));
#131243=CARTESIAN_POINT('Ctrl Pts',(32.8816929368142,-13.330760762943,69.2028775008318));
#131244=CARTESIAN_POINT('Ctrl Pts',(33.0078561433856,-13.2840830912989,
69.1356696935853));
#131245=CARTESIAN_POINT('Ctrl Pts',(33.2327786922416,-13.2008665881188,
69.0158522624996));
#131246=CARTESIAN_POINT('Ctrl Pts',(33.4579869112649,-13.1147366014515,
68.8981960536854));
#131247=CARTESIAN_POINT('Ctrl Pts',(33.6828933077903,-13.0255928904122,
68.7829022808979));
#131248=CARTESIAN_POINT('Ctrl Pts',(33.904633708151,-12.9377040509621,68.6692314928191));
#131249=CARTESIAN_POINT('Ctrl Pts',(34.1260806762181,-12.8468852456101,
68.5578568279212));
#131250=CARTESIAN_POINT('Ctrl Pts',(34.3466794893567,-12.7530259357027,
68.4490182347965));
#131251=CARTESIAN_POINT('Ctrl Pts',(34.5618976776729,-12.6614559478706,
68.3428343233877));
#131252=CARTESIAN_POINT('Ctrl Pts',(34.7763085573311,-12.5669914708446,
68.239064142722));
#131253=CARTESIAN_POINT('Ctrl Pts',(34.9894054742867,-12.4695232535759,
68.1379784867459));
#131254=CARTESIAN_POINT('Ctrl Pts',(35.1254955837338,-12.4072771143768,
68.0734221422344));
#131255=CARTESIAN_POINT('Ctrl Pts',(35.2610499665858,-12.3438057886536,
68.0099616468521));
#131256=CARTESIAN_POINT('Ctrl Pts',(35.3959386020984,-12.2790808122887,
67.9476785607999));
#131257=CARTESIAN_POINT('Origin',(58.0359414686091,9.5,68.773176492713));
#131258=CARTESIAN_POINT('',(35.3959428302217,12.2790662096383,67.9477033388501));
#131259=CARTESIAN_POINT('Ctrl Pts',(35.3959384678484,12.2790809112017,67.9476786433073));
#131260=CARTESIAN_POINT('Ctrl Pts',(35.1846027686219,12.38049236243,68.0452626205346));
#131261=CARTESIAN_POINT('Ctrl Pts',(34.971630142807,12.4788242303402,68.1457335657174));
#131262=CARTESIAN_POINT('Ctrl Pts',(34.7575222122605,12.5741879244869,68.2487880787564));
#131263=CARTESIAN_POINT('Ctrl Pts',(34.5399879310559,12.6710777155668,68.3534917642369));
#131264=CARTESIAN_POINT('Ctrl Pts',(34.3212817528117,12.7649041083006,68.4608625658059));
#131265=CARTESIAN_POINT('Ctrl Pts',(34.1019392637244,12.8557816179673,68.5706361300887));
#131266=CARTESIAN_POINT('Ctrl Pts',(33.8777656711369,12.9486607400751,68.6828274997536));
#131267=CARTESIAN_POINT('Ctrl Pts',(33.6529274636052,13.0384601940759,68.7975288373825));
#131268=CARTESIAN_POINT('Ctrl Pts',(33.4280057224191,13.1252915128353,68.9145107933281));
#131269=CARTESIAN_POINT('Ctrl Pts',(33.2879527170998,13.1793591502455,68.9873524599982));
#131270=CARTESIAN_POINT('Ctrl Pts',(33.1478675064981,13.2322757250493,69.061079411678));
#131271=CARTESIAN_POINT('Ctrl Pts',(33.0078920406793,13.2840647581322,69.1356457047561));
#131272=CARTESIAN_POINT('Ctrl Pts',(32.7838505729871,13.3669570772566,69.2549947752798));
#131273=CARTESIAN_POINT('Ctrl Pts',(32.5600163098531,13.4469415289604,69.3764846407735));
#131274=CARTESIAN_POINT('Ctrl Pts',(32.3371306874339,13.5241132751291,69.4999469835736));
#131275=CARTESIAN_POINT('Ctrl Pts',(32.1131440080578,13.6016662504102,69.6240192314451));
#131276=CARTESIAN_POINT('Ctrl Pts',(31.8901154401888,13.6763791066002,69.7500839185269));
#131277=CARTESIAN_POINT('Ctrl Pts',(31.6688047376244,13.7483162091762,69.8780114798589));
#131278=CARTESIAN_POINT('Ctrl Pts',(31.4471601729343,13.8203618337246,70.0061320285479));
#131279=CARTESIAN_POINT('Ctrl Pts',(31.2272387427077,13.8896237244916,70.136121542552));
#131280=CARTESIAN_POINT('Ctrl Pts',(31.0098097350917,13.9561279803308,70.267884411958));
#131281=CARTESIAN_POINT('Ctrl Pts',(30.8877961052469,13.9934478657685,70.3418251715248));
#131282=CARTESIAN_POINT('Ctrl Pts',(30.7665674583,14.0298986263602,70.4163249544217));
#131283=CARTESIAN_POINT('Ctrl Pts',(30.6462604266937,14.0654788649446,70.4913707665092));
#131284=CARTESIAN_POINT('Ctrl Pts',(30.4507151912467,14.1233104483389,70.6133490980999));
#131285=CARTESIAN_POINT('Ctrl Pts',(30.2576886721935,14.1788533664209,70.7367664634594));
#131286=CARTESIAN_POINT('Ctrl Pts',(30.0681599843068,14.2321011530085,70.861568004652));
#131287=CARTESIAN_POINT('Ctrl Pts',(29.8885216001801,14.2825702743198,70.9798569425765));
#131288=CARTESIAN_POINT('Ctrl Pts',(29.7120256014514,14.3309774346097,71.0993898650131));
#131289=CARTESIAN_POINT('Ctrl Pts',(29.5395081699614,14.3772763216838,71.2201341766509));
#131290=CARTESIAN_POINT('Ctrl Pts',(29.3622416148093,14.4248497416456,71.3442023823584));
#131291=CARTESIAN_POINT('Ctrl Pts',(29.1891821649001,14.470197093175,71.4695456224595));
#131292=CARTESIAN_POINT('Ctrl Pts',(29.0218222185181,14.5132384215319,71.5960808254033));
#131293=CARTESIAN_POINT('Ctrl Pts',(28.8640265888147,14.5538200162215,71.7153847715375));
#131294=CARTESIAN_POINT('Ctrl Pts',(28.7112977339314,14.5923513952753,71.8357488452308));
#131295=CARTESIAN_POINT('Ctrl Pts',(28.5648874571433,14.6287141046279,71.9571086643009));
#131296=CARTESIAN_POINT('Ctrl Pts',(28.5560132300508,14.630918123004,71.9644645317848));
#131297=CARTESIAN_POINT('Ctrl Pts',(28.547162216342,14.6331141581006,71.9718240578045));
#131298=CARTESIAN_POINT('Ctrl Pts',(28.5383346947726,14.635302177299,71.9791872280613));
#131299=CARTESIAN_POINT('Ctrl Pts',(28.3838674613872,14.6735889455064,72.1080307012333));
#131300=CARTESIAN_POINT('Ctrl Pts',(28.2366363763939,14.7094295606917,72.2379913483665));
#131301=CARTESIAN_POINT('Ctrl Pts',(28.0991271518032,14.7426018475479,72.3687793402463));
#131302=CARTESIAN_POINT('Ctrl Pts',(27.9715295101533,14.7733830957412,72.4901402116327));
#131303=CARTESIAN_POINT('Ctrl Pts',(27.8523028105917,14.8018663841165,72.6122138209336));
#131304=CARTESIAN_POINT('Ctrl Pts',(27.743431052339,14.827824076867,72.7347571512724));
#131305=CARTESIAN_POINT('Ctrl Pts',(27.7349740663958,14.8298404293741,72.7442761233066));
#131306=CARTESIAN_POINT('Ctrl Pts',(27.7265795601537,14.8318415175968,72.753797921904));
#131307=CARTESIAN_POINT('Ctrl Pts',(27.7182484627975,14.833827222121,72.7633224290272));
#131308=CARTESIAN_POINT('Ctrl Pts',(27.6026668404061,14.8613759279739,72.8954608423381));
#131309=CARTESIAN_POINT('Ctrl Pts',(27.499559649583,14.8859752343313,73.0281296908167));
#131310=CARTESIAN_POINT('Ctrl Pts',(27.4123172044704,14.9072171780113,73.1604861524754));
#131311=CARTESIAN_POINT('Ctrl Pts',(27.3250747593577,14.9284591216913,73.2928426141342));
#131312=CARTESIAN_POINT('Ctrl Pts',(27.2536970570319,14.946343257526,73.4248866723926));
#131313=CARTESIAN_POINT('Ctrl Pts',(27.2015660065188,14.9604820182035,73.5557278374816));
#131314=CARTESIAN_POINT('',(36.1590567380064,11.8740010057512,67.5954592543057));
#131315=CARTESIAN_POINT('Ctrl Pts',(36.1588385012177,11.8746149117224,67.5942070353847));
#131316=CARTESIAN_POINT('Ctrl Pts',(36.0248459115227,11.9546473040868,67.6567966276318));
#131317=CARTESIAN_POINT('Ctrl Pts',(35.8850483327633,12.0328525721753,67.7221131308698));
#131318=CARTESIAN_POINT('Ctrl Pts',(35.7391385019241,12.1090378043059,67.7897526024016));
#131319=CARTESIAN_POINT('Ctrl Pts',(35.6283105785524,12.1669053997931,67.8411291417665));
#131320=CARTESIAN_POINT('Ctrl Pts',(35.5139562241468,12.2236075905504,67.8938446914323));
#131321=CARTESIAN_POINT('Ctrl Pts',(35.3959428302217,12.2790662096383,67.9477033388501));
#131322=CARTESIAN_POINT('',(62.6710208743191,11.87440113975,62.91980295862));
#131323=CARTESIAN_POINT('',(36.1589529072075,11.874300349392,67.5948533979391));
#131324=CARTESIAN_POINT('',(82.3364382228178,12.3433341995235,59.7089279795811));
#131325=CARTESIAN_POINT('Ctrl Pts',(62.6710208743191,11.87440113975,62.91980295862));
#131326=CARTESIAN_POINT('Ctrl Pts',(63.4281166754305,12.0846306344014,62.8888133082932));
#131327=CARTESIAN_POINT('Ctrl Pts',(64.2163274555045,12.2690616559132,62.8560593750203));
#131328=CARTESIAN_POINT('Ctrl Pts',(65.4435012996331,12.5103870064531,62.7939898400575));
#131329=CARTESIAN_POINT('Ctrl Pts',(65.8600410701228,12.584956407583,62.7711749943272));
#131330=CARTESIAN_POINT('Ctrl Pts',(66.4958864972862,12.6885240050038,62.7327049090558));
#131331=CARTESIAN_POINT('Ctrl Pts',(66.8165686353613,12.7382365709795,62.7124106437459));
#131332=CARTESIAN_POINT('Ctrl Pts',(67.195490824901,12.7927258737427,62.6866763968924));
#131333=CARTESIAN_POINT('Ctrl Pts',(67.3861460351238,12.8191077763637,62.6732713839456));
#131334=CARTESIAN_POINT('Ctrl Pts',(67.4681108568743,12.8302309673599,62.6674086440074));
#131335=CARTESIAN_POINT('Ctrl Pts',(67.5228107896359,12.8376058562909,62.6634737181123));
#131336=CARTESIAN_POINT('Ctrl Pts',(67.5514629683228,12.8414425243988,62.6614003567288));
#131337=CARTESIAN_POINT('Ctrl Pts',(68.4138456274695,12.9561983158044,62.5986558946661));
#131338=CARTESIAN_POINT('Ctrl Pts',(69.2465420140072,13.0411633210121,62.5245233792394));
#131339=CARTESIAN_POINT('Ctrl Pts',(70.4891530095295,13.1339297429258,62.3871328855657));
#131340=CARTESIAN_POINT('Ctrl Pts',(70.902291431658,13.1590527041346,62.337010585665));
#131341=CARTESIAN_POINT('Ctrl Pts',(71.726331983732,13.1982235913239,62.227514992348));
#131342=CARTESIAN_POINT('Ctrl Pts',(72.1385502864971,13.2122999760018,62.1679361496933));
#131343=CARTESIAN_POINT('Ctrl Pts',(74.1807440478251,13.2554807810021,61.8481459426687));
#131344=CARTESIAN_POINT('Ctrl Pts',(75.8173705513391,13.206865618323,61.5099893968683));
#131345=CARTESIAN_POINT('Ctrl Pts',(79.0977809214279,12.9263175231934,60.6887657913152));
#131346=CARTESIAN_POINT('Ctrl Pts',(80.7213342216137,12.694823500819,60.2100114146928));
#131347=CARTESIAN_POINT('Ctrl Pts',(82.3365243969791,12.34303336447,59.70941850923));
#131348=CARTESIAN_POINT('',(82.7407915597713,14.4574398737622,62.0021315198703));
#131349=CARTESIAN_POINT('Origin',(83.1537660643691,9.5,64.344226319776));
#131350=CARTESIAN_POINT('',(65.9990597676261,14.4574398737488,64.9541505385815));
#131351=CARTESIAN_POINT('',(65.617923889253,14.4574398737354,65.021355077224));
#131352=CARTESIAN_POINT('Ctrl Pts',(63.7242517378918,14.9978694345806,67.8461463931036));
#131353=CARTESIAN_POINT('Ctrl Pts',(63.7337825611654,14.998764850968,67.7776529607607));
#131354=CARTESIAN_POINT('Ctrl Pts',(63.7449416159549,14.9985039978351,67.7066972644362));
#131355=CARTESIAN_POINT('Ctrl Pts',(63.7581983113509,14.9968754692981,67.6336509130626));
#131356=CARTESIAN_POINT('Ctrl Pts',(63.771015396592,14.9953009449952,67.5630268786308));
#131357=CARTESIAN_POINT('Ctrl Pts',(63.7857933628015,14.9924477215874,67.4904488594246));
#131358=CARTESIAN_POINT('Ctrl Pts',(63.802958556956,14.9881719476635,67.4162646465039));
#131359=CARTESIAN_POINT('Ctrl Pts',(63.8117053466523,14.9859931610466,67.378462935474));
#131360=CARTESIAN_POINT('Ctrl Pts',(63.8210720260374,14.9834457896389,67.340244331803));
#131361=CARTESIAN_POINT('Ctrl Pts',(63.8311151525638,14.9805159890665,67.301655683593));
#131362=CARTESIAN_POINT('Ctrl Pts',(63.8436495338607,14.9768594347652,67.2534949012788));
#131363=CARTESIAN_POINT('Ctrl Pts',(63.8572423152196,14.9726097528716,67.2047923803538));
#131364=CARTESIAN_POINT('Ctrl Pts',(63.8719889212853,14.9677502820913,67.1556379765422));
#131365=CARTESIAN_POINT('Ctrl Pts',(63.8756755728017,14.9665354143963,67.1433493755893));
#131366=CARTESIAN_POINT('Ctrl Pts',(63.8794342263518,14.9652824508048,67.1310322852469));
#131367=CARTESIAN_POINT('Ctrl Pts',(63.8832662473991,14.9639911935129,67.1186879620414));
#131368=CARTESIAN_POINT('Ctrl Pts',(63.8851822579228,14.963345564867,67.1125158004387));
#131369=CARTESIAN_POINT('Ctrl Pts',(63.8871190274097,14.9626890327076,67.1063445400929));
#131370=CARTESIAN_POINT('Ctrl Pts',(63.8881246655709,14.9623466418033,67.1031452704268));
#131371=CARTESIAN_POINT('Ctrl Pts',(63.889130303732,14.962004250899,67.0999460007607));
#131372=CARTESIAN_POINT('Ctrl Pts',(63.8901472151135,14.9616562478876,67.0967169599364));
#131373=CARTESIAN_POINT('Ctrl Pts',(63.8911756672465,14.9613025150278,67.0934582802534));
#131374=CARTESIAN_POINT('Ctrl Pts',(63.8952894757787,14.9598875835887,67.0804235615214));
#131375=CARTESIAN_POINT('Ctrl Pts',(63.8995879358875,14.9583809988961,67.0669146185049));
#131376=CARTESIAN_POINT('Ctrl Pts',(63.9040893584918,14.9567751639957,67.0529409938371));
#131377=CARTESIAN_POINT('Ctrl Pts',(63.9220950489092,14.950351824394,66.9970464951659));
#131378=CARTESIAN_POINT('Ctrl Pts',(63.9433324465097,14.9423392673845,66.9336940725849));
#131379=CARTESIAN_POINT('Ctrl Pts',(63.9691124192012,14.9322462007947,66.8636663834272));
#131380=CARTESIAN_POINT('Ctrl Pts',(63.9892714061719,14.9243537953096,66.8089073155952));
#131381=CARTESIAN_POINT('Ctrl Pts',(64.0122117937822,14.9151735758559,66.7499932158726));
#131382=CARTESIAN_POINT('Ctrl Pts',(64.0386276242206,14.9045267344321,66.6875743978673));
#131383=CARTESIAN_POINT('Ctrl Pts',(64.0626328772686,14.8948514708384,66.6308516109511));
#131384=CARTESIAN_POINT('Ctrl Pts',(64.0895082802585,14.8839646264364,66.5712349562864));
#131385=CARTESIAN_POINT('Ctrl Pts',(64.1197755996161,14.8717745154457,66.5092176688769));
#131386=CARTESIAN_POINT('Ctrl Pts',(64.1413890174507,14.86306974846,66.4649320970391));
#131387=CARTESIAN_POINT('Ctrl Pts',(64.1647320513516,14.8537012799868,66.4194225295541));
#131388=CARTESIAN_POINT('Ctrl Pts',(64.1899947219018,14.8436522220047,66.3728687534608));
#131389=CARTESIAN_POINT('Ctrl Pts',(64.2208107999915,14.8313941135482,66.3160812180094));
#131390=CARTESIAN_POINT('Ctrl Pts',(64.2544746774233,14.8181382068145,66.2578139673371));
#131391=CARTESIAN_POINT('Ctrl Pts',(64.2913278249673,14.8039250787308,66.1984992639139));
#131392=CARTESIAN_POINT('Ctrl Pts',(64.3140132909143,14.7951759906709,66.1619872758115));
#131393=CARTESIAN_POINT('Ctrl Pts',(64.3379072085807,14.7860651649021,66.12507825814));
#131394=CARTESIAN_POINT('Ctrl Pts',(64.3630889037512,14.7766117776763,66.0878712102795));
#131395=CARTESIAN_POINT('Ctrl Pts',(64.3961339207526,14.764206443584,66.0390457630331));
#131396=CARTESIAN_POINT('Ctrl Pts',(64.4313982390898,14.7512094777188,65.989704540002));
#131397=CARTESIAN_POINT('Ctrl Pts',(64.4690558065301,14.7376915386291,65.9400894217365));
#131398=CARTESIAN_POINT('Ctrl Pts',(64.4878845902503,14.7309325690842,65.9152818626037));
#131399=CARTESIAN_POINT('Ctrl Pts',(64.5073115484353,14.7240438671898,65.8904061716917));
#131400=CARTESIAN_POINT('Ctrl Pts',(64.5273575133116,14.7170375583601,65.8654948206653));
#131401=CARTESIAN_POINT('Ctrl Pts',(64.5373804957498,14.7135344039452,65.8530391451521));
#131402=CARTESIAN_POINT('Ctrl Pts',(64.5475582283756,14.7100018734831,65.840574546187));
#131403=CARTESIAN_POINT('Ctrl Pts',(64.5578932426902,14.7064417183732,65.8281052748378));
#131404=CARTESIAN_POINT('Ctrl Pts',(64.5630607498474,14.7046616408183,65.8218706391632));
#131405=CARTESIAN_POINT('Ctrl Pts',(64.5682675773319,14.7028746588143,65.8156348348536));
#131406=CARTESIAN_POINT('Ctrl Pts',(64.5735140388626,14.701081004319,65.8093983984261));
#131407=CARTESIAN_POINT('Ctrl Pts',(64.5787605003933,14.6992873498238,65.8031619619987));
#131408=CARTESIAN_POINT('Ctrl Pts',(64.5850099785308,14.6971602131997,65.7957967052526));
#131409=CARTESIAN_POINT('Ctrl Pts',(64.5893726377915,14.695680263695,65.790687731514));
#131410=CARTESIAN_POINT('Ctrl Pts',(64.6293285984423,14.6821259609999,65.7438965563464));
#131411=CARTESIAN_POINT('Ctrl Pts',(64.6689335996178,14.6691901554928,65.7004189411246));
#131412=CARTESIAN_POINT('Ctrl Pts',(64.7079063914946,14.6569598950792,65.6599692986373));
#131413=CARTESIAN_POINT('Ctrl Pts',(64.7483012578738,14.6442833658546,65.6180436929858));
#131414=CARTESIAN_POINT('Ctrl Pts',(64.7880169175196,14.6323643974131,65.5793709618982));
#131415=CARTESIAN_POINT('Ctrl Pts',(64.826742420664,14.621243752578,65.5436457176895));
#131416=CARTESIAN_POINT('Ctrl Pts',(64.8678098352823,14.6094505905741,65.5057600016334));
#131417=CARTESIAN_POINT('Ctrl Pts',(64.9077636973584,14.5985549248645,65.4711889571079));
#131418=CARTESIAN_POINT('Ctrl Pts',(64.9462359138267,14.5885487374807,65.43958397432));
#131419=CARTESIAN_POINT('Ctrl Pts',(64.9587773526386,14.585286851415,65.4292811637681));
#131420=CARTESIAN_POINT('Ctrl Pts',(64.9711613623282,14.5821190820351,65.4192936715562));
#131421=CARTESIAN_POINT('Ctrl Pts',(64.983375252308,14.5790440470746,65.4096097661362));
#131422=CARTESIAN_POINT('Ctrl Pts',(65.0252691727882,14.5684966072071,65.3763937502495));
#131423=CARTESIAN_POINT('Ctrl Pts',(65.0652298005112,14.5590473736055,65.3467438621354));
#131424=CARTESIAN_POINT('Ctrl Pts',(65.1029270992231,14.5506453301593,65.3202694661502));
#131425=CARTESIAN_POINT('Ctrl Pts',(65.1188141328085,14.54710439882,65.3091121781603));
#131426=CARTESIAN_POINT('Ctrl Pts',(65.1342992176172,14.5437488222219,65.2985191076289));
#131427=CARTESIAN_POINT('Ctrl Pts',(65.1493578101058,14.5405722609322,65.2884619225297));
#131428=CARTESIAN_POINT('Ctrl Pts',(65.1747528789681,14.5352152534457,65.2715013129411));
#131429=CARTESIAN_POINT('Ctrl Pts',(65.1989388090877,14.5303694416143,65.2560677928051));
#131430=CARTESIAN_POINT('Ctrl Pts',(65.2218214051471,14.5260066845789,65.2420469573045));
#131431=CARTESIAN_POINT('Ctrl Pts',(65.2332627031767,14.5238253060612,65.2350365395543));
#131432=CARTESIAN_POINT('Ctrl Pts',(65.2443784165704,14.5217646555267,65.2283795358765));
#131433=CARTESIAN_POINT('Ctrl Pts',(65.2551582593996,14.5198210938599,65.2220630808855));
#131434=CARTESIAN_POINT('Ctrl Pts',(65.2605481808143,14.5188493130265,65.21890485339));
#131435=CARTESIAN_POINT('Ctrl Pts',(65.2658541351246,14.5179067975575,65.2158317661106));
#131436=CARTESIAN_POINT('Ctrl Pts',(65.2710749504499,14.5169931010738,65.2128423158431));
#131437=CARTESIAN_POINT('Ctrl Pts',(65.2762957657751,14.5160794045901,65.2098528655756));
#131438=CARTESIAN_POINT('Ctrl Pts',(65.2799085769594,14.5154528431045,65.2077986373233));
#131439=CARTESIAN_POINT('Ctrl Pts',(65.2864808157042,14.5143380012837,65.204123389393));
#131440=CARTESIAN_POINT('Ctrl Pts',(65.3567384846777,14.5024202681267,65.1648347447609));
#131441=CARTESIAN_POINT('Ctrl Pts',(65.4303996117143,14.4920729911742,65.1290510718699));
#131442=CARTESIAN_POINT('Ctrl Pts',(65.5070958740645,14.483608530346,65.0970873481068));
#131443=CARTESIAN_POINT('Ctrl Pts',(65.5795143800122,14.4756161772894,65.0669064103594));
#131444=CARTESIAN_POINT('Ctrl Pts',(65.6546388188878,14.4693028578232,65.0401307723377));
#131445=CARTESIAN_POINT('Ctrl Pts',(65.7321620506938,14.4648886760428,65.0170421886093));
#131446=CARTESIAN_POINT('Ctrl Pts',(65.8049708097341,14.4607429368867,64.9953577065501));
#131447=CARTESIAN_POINT('Ctrl Pts',(65.8798954386498,14.4582725686681,64.9769252656061));
#131448=CARTESIAN_POINT('Ctrl Pts',(65.9566848864551,14.4576170913444,64.9619975203067));
#131449=CARTESIAN_POINT('Ctrl Pts',(65.9707478015117,14.4574970498258,64.9592637122102));
#131450=CARTESIAN_POINT('Ctrl Pts',(65.9848732708248,14.4574377505937,64.9566475067169));
#131451=CARTESIAN_POINT('Ctrl Pts',(65.9990597670304,14.4574398737327,64.9541505386571));
#131452=CARTESIAN_POINT('Ctrl Pts',(25.8674011700191,-10.80158154637,60.29014909768));
#131453=CARTESIAN_POINT('Ctrl Pts',(25.9483639155891,-10.67317627998,60.2578289519001));
#131454=CARTESIAN_POINT('Ctrl Pts',(26.1402448136891,-10.34972776486,60.17641841982));
#131455=CARTESIAN_POINT('Ctrl Pts',(26.4133227121591,-9.809477103913,60.04060145495));
#131456=CARTESIAN_POINT('Ctrl Pts',(26.6746608848491,-9.173794293496,59.88240498685));
#131457=CARTESIAN_POINT('Ctrl Pts',(26.8930528742491,-8.50966725041199,
59.72121052569));
#131458=CARTESIAN_POINT('Ctrl Pts',(27.0742534024791,-7.80453902184299,
59.5573550630001));
#131459=CARTESIAN_POINT('Ctrl Pts',(27.2212200353591,-7.04916242399599,
59.39317676603));
#131460=CARTESIAN_POINT('Ctrl Pts',(27.3357604796091,-6.23957271011399,
59.23300930155));
#131461=CARTESIAN_POINT('Ctrl Pts',(27.4201508701391,-5.37834024197199,
59.08272261093));
#131462=CARTESIAN_POINT('Ctrl Pts',(27.4783655117691,-4.47147007015,58.94826811738));
#131463=CARTESIAN_POINT('Ctrl Pts',(27.5154691587491,-3.53139160346499,
58.8354266391701));
#131464=CARTESIAN_POINT('Ctrl Pts',(27.5369855402391,-2.57512600928299,
58.74841910647));
#131465=CARTESIAN_POINT('Ctrl Pts',(27.5481191645691,-1.62102984739999,
58.68926281351));
#131466=CARTESIAN_POINT('Ctrl Pts',(27.5529848278191,-0.692828865468586,
58.65792260557));
#131467=CARTESIAN_POINT('Ctrl Pts',(27.5536467947491,-0.0610093872017058,
58.65357386177));
#131468=CARTESIAN_POINT('Ctrl Pts',(27.5533212468091,0.257051205251114,
58.6558663386));
#131469=CARTESIAN_POINT('Ctrl Pts',(27.5532919224291,0.281757260524914,
58.65607129804));
#131470=CARTESIAN_POINT('Ctrl Pts',(27.8395702403391,-9.323660637594,64.630699852874));
#131471=CARTESIAN_POINT('Ctrl Pts',(27.9330797739191,-9.212845822649,64.59866767931));
#131472=CARTESIAN_POINT('Ctrl Pts',(28.1541305252591,-8.93370631904499,
64.518698253699));
#131473=CARTESIAN_POINT('Ctrl Pts',(28.4665607003691,-8.46745880057699,
64.388043824903));
#131474=CARTESIAN_POINT('Ctrl Pts',(28.7630789213891,-7.91883929150999,
64.23908399161));
#131475=CARTESIAN_POINT('Ctrl Pts',(29.0088575136291,-7.34565535370899,
64.0899266273461));
#131476=CARTESIAN_POINT('Ctrl Pts',(29.2112030172591,-6.737065109368,63.940452046196));
#131477=CARTESIAN_POINT('Ctrl Pts',(29.3742190560191,-6.08508333800299,
63.792406643038));
#131478=CARTESIAN_POINT('Ctrl Pts',(29.5006182945091,-5.386284106142,63.649329525158));
#131479=CARTESIAN_POINT('Ctrl Pts',(29.5935058932791,-4.64288310331099,
63.516088541777));
#131480=CARTESIAN_POINT('Ctrl Pts',(29.6576464719891,-3.86006210124599,
63.3975884347841));
#131481=CARTESIAN_POINT('Ctrl Pts',(29.6988058455691,-3.04855202192599,
63.298576769657));
#131482=CARTESIAN_POINT('Ctrl Pts',(29.7230108418491,-2.22304983625699,
63.222478230382));
#131483=CARTESIAN_POINT('Ctrl Pts',(29.7357938430891,-1.39940580633199,
63.170853244553));
#131484=CARTESIAN_POINT('Ctrl Pts',(29.7414883797391,-0.598107824388886,
63.143535409107));
#131485=CARTESIAN_POINT('Ctrl Pts',(29.7422638030691,-0.0526681594190058,
63.139745384407));
#131486=CARTESIAN_POINT('Ctrl Pts',(29.7418782228891,0.221908182666614,
63.1417428011591));
#131487=CARTESIAN_POINT('Ctrl Pts',(29.7418435361591,0.243236501092214,
63.141921385014));
#131488=CARTESIAN_POINT('Ctrl Pts',(31.8804542988291,-9.85977556851199,
67.511305247789));
#131489=CARTESIAN_POINT('Ctrl Pts',(32.0040134654391,-9.72150630571099,
67.442225131604));
#131490=CARTESIAN_POINT('Ctrl Pts',(32.2941843453491,-9.37393636982899,
67.27417511811));
#131491=CARTESIAN_POINT('Ctrl Pts',(32.6971211611091,-8.7987533155,67.018567541111));
#131492=CARTESIAN_POINT('Ctrl Pts',(33.0712071741991,-8.13380665328499,
66.752472039828));
#131493=CARTESIAN_POINT('Ctrl Pts',(33.3743008109591,-7.45473129633099,
66.508910810442));
#131494=CARTESIAN_POINT('Ctrl Pts',(33.6180362316491,-6.75303160889099,
66.285205978187));
#131495=CARTESIAN_POINT('Ctrl Pts',(33.8098260170691,-6.02348256075299,
66.081109857837));
#131496=CARTESIAN_POINT('Ctrl Pts',(33.9551252743891,-5.26605698609299,
65.898363870823));
#131497=CARTESIAN_POINT('Ctrl Pts',(34.0595863091591,-4.48602846810799,
65.739583721531));
#131498=CARTESIAN_POINT('Ctrl Pts',(34.1303183702891,-3.69048826277099,
65.60678565305));
#131499=CARTESIAN_POINT('Ctrl Pts',(34.1750618306191,-2.88866222149599,
65.501251127434));
#131500=CARTESIAN_POINT('Ctrl Pts',(34.2011679964491,-2.09146054688399,
65.423232491143));
#131501=CARTESIAN_POINT('Ctrl Pts',(34.2149297644291,-1.31041085152599,
65.371822179204));
#131502=CARTESIAN_POINT('Ctrl Pts',(34.2210737681691,-0.558921368337586,
65.3450673699811));
#131503=CARTESIAN_POINT('Ctrl Pts',(34.2219093654591,-0.0494594423831458,
65.341370578215));
#131504=CARTESIAN_POINT('Ctrl Pts',(34.2214919003791,0.207288115816814,
65.3433200745641));
#131505=CARTESIAN_POINT('Ctrl Pts',(34.2214543888891,0.227233674714814,
65.3434944532351));
#131506=CARTESIAN_POINT('Ctrl Pts',(36.2923205729991,-12.18468357669,67.721710765645));
#131507=CARTESIAN_POINT('Ctrl Pts',(36.4508071964791,-11.98544964953,67.593812075596));
#131508=CARTESIAN_POINT('Ctrl Pts',(36.8210084222691,-11.48546012732,67.285165865292));
#131509=CARTESIAN_POINT('Ctrl Pts',(37.3275808780091,-10.6641709201,66.8269871398981));
#131510=CARTESIAN_POINT('Ctrl Pts',(37.7890331764291,-9.72838021784798,
66.366596924014));
#131511=CARTESIAN_POINT('Ctrl Pts',(38.1552900169491,-8.79106802662099,
65.961853607951));
#131512=CARTESIAN_POINT('Ctrl Pts',(38.4432707802091,-7.84573037211999,
65.606494411466));
#131513=CARTESIAN_POINT('Ctrl Pts',(38.6644696814491,-6.89024097792099,
65.297713052213));
#131514=CARTESIAN_POINT('Ctrl Pts',(38.8277695481891,-5.92940344555999,
65.035205417231));
#131515=CARTESIAN_POINT('Ctrl Pts',(38.9420177955091,-4.97367707759999,
64.819031227146));
#131516=CARTESIAN_POINT('Ctrl Pts',(39.0172375459191,-4.03399312862899,
64.647689979609));
#131517=CARTESIAN_POINT('Ctrl Pts',(39.0635876386991,-3.11889813453199,
64.518020427672));
#131518=CARTESIAN_POINT('Ctrl Pts',(39.0900087734791,-2.23564392661399,
64.426059311459));
#131519=CARTESIAN_POINT('Ctrl Pts',(39.1036674799791,-1.39143522956399,
64.367456847303));
#131520=CARTESIAN_POINT('Ctrl Pts',(39.1096927058991,-0.591733253689086,
64.337569168795));
#131521=CARTESIAN_POINT('Ctrl Pts',(39.1105099132791,-0.0527313430901759,
64.333460953008));
#131522=CARTESIAN_POINT('Ctrl Pts',(39.1101021067291,0.219333464190314,
64.335629801855));
#131523=CARTESIAN_POINT('Ctrl Pts',(39.1100654948391,0.240472192012714,
64.335823912502));
#131524=CARTESIAN_POINT('',(28.7120116773549,-9.91584041054405,64.1367640219333));
#131525=CARTESIAN_POINT('Ctrl Pts',(30.8903812387966,-6.76809619335577,
63.752816963338));
#131526=CARTESIAN_POINT('Ctrl Pts',(30.605546535352,-7.34848963938884,63.8030410065974));
#131527=CARTESIAN_POINT('Ctrl Pts',(30.2797662869634,-7.90595274493995,
63.8604848541702));
#131528=CARTESIAN_POINT('Ctrl Pts',(29.5502034758413,-8.9598024251586,63.9891264618925));
#131529=CARTESIAN_POINT('Ctrl Pts',(29.1494368108939,-9.45399235856436,
64.0597924378913));
#131530=CARTESIAN_POINT('Ctrl Pts',(28.7116284843023,-9.91532477875859,
64.1369898582482));
#131531=CARTESIAN_POINT('Ctrl Pts',(29.6609510243113,-9.94007378487892,
64.9665024957973));
#131532=CARTESIAN_POINT('Ctrl Pts',(31.6715154505519,-10.0843062537526,
66.5643539924829));
#131533=CARTESIAN_POINT('Ctrl Pts',(33.9364614048553,-10.773624544685,67.4539976470912));
#131534=CARTESIAN_POINT('Ctrl Pts',(36.1591009162391,-11.87389313049,67.595688809357));
#131535=CARTESIAN_POINT('',(38.8135870865772,3.00384514409506E-5,64.3914459142308));
#131536=CARTESIAN_POINT('Ctrl Pts',(36.1592915186016,-11.873367524377,67.5967699365276));
#131537=CARTESIAN_POINT('Ctrl Pts',(36.2669689976408,-11.7330105239143,
67.5095497815776));
#131538=CARTESIAN_POINT('Ctrl Pts',(36.3709096198074,-11.5904287102527,
67.4233916251011));
#131539=CARTESIAN_POINT('Ctrl Pts',(36.4710609268351,-11.4457706775564,
67.338483268842));
#131540=CARTESIAN_POINT('Ctrl Pts',(36.6764809564459,-11.1490630434591,
67.1643280074219));
#131541=CARTESIAN_POINT('Ctrl Pts',(36.8659592292947,-10.8436207467023,
66.9954307180623));
#131542=CARTESIAN_POINT('Ctrl Pts',(37.0396680152484,-10.5307740965049,
66.833093734618));
#131543=CARTESIAN_POINT('Ctrl Pts',(37.2050431549548,-10.2329362053525,
66.6785448373402));
#131544=CARTESIAN_POINT('Ctrl Pts',(37.3561256133158,-9.92838738276226,
66.529941885612));
#131545=CARTESIAN_POINT('Ctrl Pts',(37.4934100494082,-9.61845064646555,
66.3882186911218));
#131546=CARTESIAN_POINT('Ctrl Pts',(37.5647540297729,-9.45738271292513,
66.3145679766437));
#131547=CARTESIAN_POINT('Ctrl Pts',(37.6323716366623,-9.29485967912372,
66.2427752450919));
#131548=CARTESIAN_POINT('Ctrl Pts',(37.6963876506001,-9.13107418210396,
66.1729346611957));
#131549=CARTESIAN_POINT('Ctrl Pts',(37.7517279747585,-8.98948550858375,
66.1125591345973));
#131550=CARTESIAN_POINT('Ctrl Pts',(37.8043764883067,-8.84695258256744,
66.0536422481846));
#131551=CARTESIAN_POINT('Ctrl Pts',(37.8544136268491,-8.70359951764846,
65.9962447764266));
#131552=CARTESIAN_POINT('Ctrl Pts',(37.9608898797757,-8.39855215397505,
65.8741061430377));
#131553=CARTESIAN_POINT('Ctrl Pts',(38.0555414402464,-8.08979107905725,
65.7588476438518));
#131554=CARTESIAN_POINT('Ctrl Pts',(38.1394401871514,-7.7784358182481,65.6508064746933));
#131555=CARTESIAN_POINT('Ctrl Pts',(38.2234081819392,-7.46682357275948,
65.5426761311135));
#131556=CARTESIAN_POINT('Ctrl Pts',(38.2966056056107,-7.15261285739073,
65.4417750367764));
#131557=CARTESIAN_POINT('Ctrl Pts',(38.3603322672021,-6.83683049605349,
65.3482233732188));
#131558=CARTESIAN_POINT('Ctrl Pts',(38.4239729235666,-6.52147431322542,
65.2547979665817));
#131559=CARTESIAN_POINT('Ctrl Pts',(38.4781683640289,-6.20455072395373,
65.1687021668385));
#131560=CARTESIAN_POINT('Ctrl Pts',(38.5243727106882,-5.88694167445974,
65.0898666901936));
#131561=CARTESIAN_POINT('Ctrl Pts',(38.5702075601737,-5.57187255150246,
65.011661662585));
#131562=CARTESIAN_POINT('Ctrl Pts',(38.6081786148033,-5.25612888799339,
64.9406013006287));
#131563=CARTESIAN_POINT('Ctrl Pts',(38.6398248347944,-4.94044272901774,
64.876470820854));
#131564=CARTESIAN_POINT('Ctrl Pts',(38.6710156948983,-4.62929900240211,
64.8132631194727));
#131565=CARTESIAN_POINT('Ctrl Pts',(38.6960624280192,-4.31821113828359,
64.7567873060298));
#131566=CARTESIAN_POINT('Ctrl Pts',(38.7164371727119,-4.00754868885774,
64.7067206894537));
#131567=CARTESIAN_POINT('Ctrl Pts',(38.7363728080012,-3.70358152837316,
64.6577330911655));
#131568=CARTESIAN_POINT('Ctrl Pts',(38.7518356631662,-3.40002164398495,
64.6148814090228));
#131569=CARTESIAN_POINT('Ctrl Pts',(38.7640695060587,-3.09700899262399,
64.5778465685617));
#131570=CARTESIAN_POINT('Ctrl Pts',(38.7759411598554,-2.80296718380441,
64.5419081632522));
#131571=CARTESIAN_POINT('Ctrl Pts',(38.7847721643487,-2.50944068763906,
64.5114472770169));
#131572=CARTESIAN_POINT('Ctrl Pts',(38.7915268784732,-2.21653862227863,
64.4862013713735));
#131573=CARTESIAN_POINT('Ctrl Pts',(38.7980203465799,-1.93496486730855,
64.4619318789721));
#131574=CARTESIAN_POINT('Ctrl Pts',(38.8025950242488,-1.6539681767044,64.4424817775391));
#131575=CARTESIAN_POINT('Ctrl Pts',(38.8059154064001,-1.37337909271983,
64.4276474507953));
#131576=CARTESIAN_POINT('Ctrl Pts',(38.8090729839858,-1.10654781789107,
64.41354047892));
#131577=CARTESIAN_POINT('Ctrl Pts',(38.8110962515457,-0.84008515838022,
64.4036077382365));
#131578=CARTESIAN_POINT('Ctrl Pts',(38.8122885340855,-0.573747525170082,
64.3977531549656));
#131579=CARTESIAN_POINT('Ctrl Pts',(38.8131448252488,-0.382465212306163,
64.3935484234921));
#131580=CARTESIAN_POINT('Ctrl Pts',(38.8135724911743,-0.191247388130586,
64.3914472211002));
#131581=CARTESIAN_POINT('Ctrl Pts',(38.8135869206495,-5.89859875857534E-6,
64.3914449648797));
#131582=CARTESIAN_POINT('',(29.3346501807501,-0.000166304983923139,61.2371511371894));
#131583=CARTESIAN_POINT('Origin',(36.9902838008291,9.11708457778009E-5,
54.05096298925));
#131584=CARTESIAN_POINT('',(26.0609428066925,-10.6024189297442,60.5235111130438));
#131585=CARTESIAN_POINT('Ctrl Pts',(26.0609458870592,-10.6024210452326,
60.5235102920714));
#131586=CARTESIAN_POINT('Ctrl Pts',(26.1340051539456,-10.4995374865864,
60.5325244292292));
#131587=CARTESIAN_POINT('Ctrl Pts',(26.205815570463,-10.3957845448575,60.5417420628761));
#131588=CARTESIAN_POINT('Ctrl Pts',(26.2763660096282,-10.2912186445723,
60.551115732591));
#131589=CARTESIAN_POINT('Ctrl Pts',(26.4066686286617,-10.0980914177259,
60.568428363501));
#131590=CARTESIAN_POINT('Ctrl Pts',(26.5326736501716,-9.90218734680289,
60.586274058075));
#131591=CARTESIAN_POINT('Ctrl Pts',(26.6543717528362,-9.70376604529024,
60.6044649137639));
#131592=CARTESIAN_POINT('Ctrl Pts',(26.6711113225576,-9.67647320227824,
60.6069670653212));
#131593=CARTESIAN_POINT('Ctrl Pts',(26.6877693949852,-9.64913281307989,
60.6094757416172));
#131594=CARTESIAN_POINT('Ctrl Pts',(26.7043459355548,-9.62174563018688,
60.6119904505528));
#131595=CARTESIAN_POINT('Ctrl Pts',(26.8150897230983,-9.43877860211641,
60.6287906020033));
#131596=CARTESIAN_POINT('Ctrl Pts',(26.9221952178138,-9.25371929193362,
60.6458619956123));
#131597=CARTESIAN_POINT('Ctrl Pts',(27.0256916473619,-9.06678321563396,
60.6631785262035));
#131598=CARTESIAN_POINT('Ctrl Pts',(27.0485406571303,-9.0255131519991,60.6670015138985));
#131599=CARTESIAN_POINT('Ctrl Pts',(27.0712137299627,-8.98415179397156,
60.6708363619945));
#131600=CARTESIAN_POINT('Ctrl Pts',(27.0937111268443,-8.94270176648723,
60.6746826491534));
#131601=CARTESIAN_POINT('Ctrl Pts',(27.1883240419292,-8.76838346862868,
60.6908582290334));
#131602=CARTESIAN_POINT('Ctrl Pts',(27.2798309733679,-8.59249358838892,
60.7072384651671));
#131603=CARTESIAN_POINT('Ctrl Pts',(27.3683076969092,-8.4152183524266,60.7238529822909));
#131604=CARTESIAN_POINT('Ctrl Pts',(27.3968229707421,-8.35808409502051,
60.7292076957842));
#131605=CARTESIAN_POINT('Ctrl Pts',(27.4250233906279,-8.3008062658783,60.7345865250659));
#131606=CARTESIAN_POINT('Ctrl Pts',(27.4529112094475,-8.24339203259607,
60.7399898601321));
#131607=CARTESIAN_POINT('Ctrl Pts',(27.465373696585,-8.21773480395399,60.7424044983725));
#131608=CARTESIAN_POINT('Ctrl Pts',(27.4777737553893,-8.19205034178118,
60.744824027499));
#131609=CARTESIAN_POINT('Ctrl Pts',(27.490111727036,-8.16633949305757,60.7472487306104));
#131610=CARTESIAN_POINT('Ctrl Pts',(27.5696717026261,-8.00054607454193,
60.7628841466965));
#131611=CARTESIAN_POINT('Ctrl Pts',(27.6466011738908,-7.83363559644287,
60.7786216795869));
#131612=CARTESIAN_POINT('Ctrl Pts',(27.7209360913992,-7.6656957373092,60.7943841121699));
#131613=CARTESIAN_POINT('Ctrl Pts',(27.7436866560245,-7.61429692304464,
60.7992082816605));
#131614=CARTESIAN_POINT('Ctrl Pts',(27.7661938877754,-7.56280159465106,
60.8040345841593));
#131615=CARTESIAN_POINT('Ctrl Pts',(27.7884580319085,-7.51121201955401,
60.8088603130104));
#131616=CARTESIAN_POINT('Ctrl Pts',(27.8605471700752,-7.34416998169749,
60.8244855547362));
#131617=CARTESIAN_POINT('Ctrl Pts',(27.9300912157483,-7.17614108287275,
60.8401067990999));
#131618=CARTESIAN_POINT('Ctrl Pts',(27.9971233774981,-7.00720542713339,
60.8556482213058));
#131619=CARTESIAN_POINT('Ctrl Pts',(28.03298344009,-6.91683025451935,60.8639623851121));
#131620=CARTESIAN_POINT('Ctrl Pts',(28.0681238540866,-6.82619530707491,
60.8722532523379));
#131621=CARTESIAN_POINT('Ctrl Pts',(28.1025446498989,-6.7353109499957,60.8805064763249));
#131622=CARTESIAN_POINT('Ctrl Pts',(28.1669247756048,-6.56532224998455,
60.8959431792026));
#131623=CARTESIAN_POINT('Ctrl Pts',(28.2287902220065,-6.39446245166542,
60.9112495188088));
#131624=CARTESIAN_POINT('Ctrl Pts',(28.2881562178294,-6.2228067422687,60.9263366729753));
#131625=CARTESIAN_POINT('Ctrl Pts',(28.3233436216813,-6.12106299677433,
60.9352791286567));
#131626=CARTESIAN_POINT('Ctrl Pts',(28.3576520525177,-6.01903922463956,
60.9441441547936));
#131627=CARTESIAN_POINT('Ctrl Pts',(28.3910776390518,-5.91674739756847,
60.9529100851415));
#131628=CARTESIAN_POINT('Ctrl Pts',(28.4312885744125,-5.79369046804852,
60.9634554874858));
#131629=CARTESIAN_POINT('Ctrl Pts',(28.4702222115227,-5.67024587282327,
60.9738575900759));
#131630=CARTESIAN_POINT('Ctrl Pts',(28.5078800904185,-5.54643685186405,
60.9840783438174));
#131631=CARTESIAN_POINT('Ctrl Pts',(28.5568725875443,-5.38536264159635,
60.9973754349703));
#131632=CARTESIAN_POINT('Ctrl Pts',(28.6036936117278,-5.22371262456759,
61.0103612983112));
#131633=CARTESIAN_POINT('Ctrl Pts',(28.6483637057455,-5.06146209877235,
61.0229802871025));
#131634=CARTESIAN_POINT('Ctrl Pts',(28.693312736543,-4.89819841998956,61.0356780735812));
#131635=CARTESIAN_POINT('Ctrl Pts',(28.7360838398638,-4.73432836280087,
61.0480044081514));
#131636=CARTESIAN_POINT('Ctrl Pts',(28.7766913856413,-4.56991859505214,
61.05991043261));
#131637=CARTESIAN_POINT('Ctrl Pts',(28.8089412496872,-4.43934698437749,
61.0693660070055));
#131638=CARTESIAN_POINT('Ctrl Pts',(28.8398258479387,-4.30843400606396,
61.0785562347327));
#131639=CARTESIAN_POINT('Ctrl Pts',(28.8693411221056,-4.17719291721427,
61.0874532897539));
#131640=CARTESIAN_POINT('Ctrl Pts',(28.9064349057422,-4.01225362081862,
61.098634803166));
#131641=CARTESIAN_POINT('Ctrl Pts',(28.941366418073,-3.8467981115552,61.1093531768065));
#131642=CARTESIAN_POINT('Ctrl Pts',(28.9741192877105,-3.68089353564549,
61.1195396968139));
#131643=CARTESIAN_POINT('Ctrl Pts',(29.0007130622788,-3.54618689954222,
61.1278106672574));
#131644=CARTESIAN_POINT('Ctrl Pts',(29.0258700307831,-3.41118314000499,
61.1357309106386));
#131645=CARTESIAN_POINT('Ctrl Pts',(29.0495730671724,-3.27589448461818,
61.1432629515434));
#131646=CARTESIAN_POINT('Ctrl Pts',(29.0767194006975,-3.12095269146694,
61.1518891583789));
#131647=CARTESIAN_POINT('Ctrl Pts',(29.101958714058,-2.96563784557567,61.1600059981815));
#131648=CARTESIAN_POINT('Ctrl Pts',(29.1252546356709,-2.80995284228324,
61.1675423561766));
#131649=CARTESIAN_POINT('Ctrl Pts',(29.1470495934849,-2.66429867433893,
61.1745931441773));
#131650=CARTESIAN_POINT('Ctrl Pts',(29.1671294652963,-2.51837247222515,
61.181126774727));
#131651=CARTESIAN_POINT('Ctrl Pts',(29.1855117296563,-2.37214187313919,
61.187140620576));
#131652=CARTESIAN_POINT('Ctrl Pts',(29.2080620413757,-2.19275452848295,
61.1945180630864));
#131653=CARTESIAN_POINT('Ctrl Pts',(29.228057371095,-2.01291121835345,61.2011129594027));
#131654=CARTESIAN_POINT('Ctrl Pts',(29.2455069431775,-1.83269989880674,
61.2069077148872));
#131655=CARTESIAN_POINT('Ctrl Pts',(29.2568340689288,-1.71571844684613,
61.2106692927505));
#131656=CARTESIAN_POINT('Ctrl Pts',(29.2670884527505,-1.59858067744723,
61.2140938214548));
#131657=CARTESIAN_POINT('Ctrl Pts',(29.2762732055751,-1.48129922084861,
61.2171779988336));
#131658=CARTESIAN_POINT('Ctrl Pts',(29.2919370185711,-1.28128569417749,
61.2224378004451));
#131659=CARTESIAN_POINT('Ctrl Pts',(29.30448893715,-1.08085703169033,61.226706770597));
#131660=CARTESIAN_POINT('Ctrl Pts',(29.3138822904479,-0.88013702625373,
61.2299282192372));
#131661=CARTESIAN_POINT('Ctrl Pts',(29.317922658066,-0.793801232787563,
61.2313138625061));
#131662=CARTESIAN_POINT('Ctrl Pts',(29.3213788304288,-0.707410859236777,
61.2325058918773));
#131663=CARTESIAN_POINT('Ctrl Pts',(29.3242480131973,-0.62097323986363,
61.2335006727539));
#131664=CARTESIAN_POINT('Ctrl Pts',(29.3311096570109,-0.414257877309318,
61.2358796888706));
#131665=CARTESIAN_POINT('Ctrl Pts',(29.3346124522058,-0.207273328511921,
61.2371293245613));
#131666=CARTESIAN_POINT('Ctrl Pts',(29.3346488664094,-0.000153350959778772,
61.2371523603219));
#131667=CARTESIAN_POINT('Ctrl Pts',(26.0609412665091,-10.602417872,60.52351152353));
#131668=CARTESIAN_POINT('Ctrl Pts',(26.6967356456957,-10.1833303319981,
61.8291376819548));
#131669=CARTESIAN_POINT('Ctrl Pts',(27.5872970382304,-9.94480591158098,
63.0575054451691));
#131670=CARTESIAN_POINT('Ctrl Pts',(28.712093773969,-9.9158440831149,64.1368357767385));
#131671=CARTESIAN_POINT('Ctrl Pts',(17.4667653729091,-22.5257212764,77.256905072711));
#131672=CARTESIAN_POINT('Ctrl Pts',(17.4522156153291,-22.52947690984,77.201794509167));
#131673=CARTESIAN_POINT('Ctrl Pts',(17.2326821287691,-22.58361462996,76.351112313277));
#131674=CARTESIAN_POINT('Ctrl Pts',(16.9332603507591,-22.57430986834,74.585159968858));
#131675=CARTESIAN_POINT('Ctrl Pts',(16.9282178457291,-22.22368100432,72.0018522533659));
#131676=CARTESIAN_POINT('Ctrl Pts',(17.3279784679891,-21.55585890438,69.568778249818));
#131677=CARTESIAN_POINT('Ctrl Pts',(18.0359271396891,-20.63613602496,67.425763312453));
#131678=CARTESIAN_POINT('Ctrl Pts',(18.9494515331591,-19.52905542686,65.598121631019));
#131679=CARTESIAN_POINT('Ctrl Pts',(20.0049202231791,-18.26930231769,64.050828430023));
#131680=CARTESIAN_POINT('Ctrl Pts',(21.1756845328891,-16.86079661466,62.74165530726));
#131681=CARTESIAN_POINT('Ctrl Pts',(22.4532806921391,-15.29024780344,61.65009812484));
#131682=CARTESIAN_POINT('Ctrl Pts',(23.8321876788191,-13.5386198194,60.78746444366));
#131683=CARTESIAN_POINT('Ctrl Pts',(24.9093942416691,-12.10874261238,60.35716873393));
#131684=CARTESIAN_POINT('Ctrl Pts',(25.5188775489791,-11.26992181782,60.2071336687));
#131685=CARTESIAN_POINT('Ctrl Pts',(25.6673509880891,-11.06368060085,60.17641247788));
#131686=CARTESIAN_POINT('Ctrl Pts',(18.7773649827691,-17.75527490826,76.717063290409));
#131687=CARTESIAN_POINT('Ctrl Pts',(18.7654556117691,-17.75828882524,76.674914380299));
#131688=CARTESIAN_POINT('Ctrl Pts',(18.5862635620091,-17.80174165801,76.0240512343981));
#131689=CARTESIAN_POINT('Ctrl Pts',(18.3577568645891,-17.79425534819,74.665378823862));
#131690=CARTESIAN_POINT('Ctrl Pts',(18.4246335003491,-17.51291935268,72.6770817004958));
#131691=CARTESIAN_POINT('Ctrl Pts',(18.8714641952291,-16.98119012651,70.822183427483));
#131692=CARTESIAN_POINT('Ctrl Pts',(19.6142963879091,-16.25801796827,69.218239633607));
#131693=CARTESIAN_POINT('Ctrl Pts',(20.5621683937491,-15.40160733776,67.8849620187121));
#131694=CARTESIAN_POINT('Ctrl Pts',(21.6579870981791,-14.44562122449,66.791899033372));
#131695=CARTESIAN_POINT('Ctrl Pts',(22.8780955574091,-13.40004445027,65.903735017982));
#131696=CARTESIAN_POINT('Ctrl Pts',(24.2153171433191,-12.26374841242,65.203217298719));
#131697=CARTESIAN_POINT('Ctrl Pts',(25.6646851711591,-11.03571934281,64.698047871997));
#131698=CARTESIAN_POINT('Ctrl Pts',(26.8015432713391,-10.07428690511,64.495800893793));
#131699=CARTESIAN_POINT('Ctrl Pts',(27.4463952672191,-9.53132694979998,
64.453831767256));
#131700=CARTESIAN_POINT('Ctrl Pts',(27.6035705906891,-9.399240458337,64.448068196782));
#131701=CARTESIAN_POINT('Ctrl Pts',(22.6527444970191,-14.84009533989,75.599270274124));
#131702=CARTESIAN_POINT('Ctrl Pts',(22.6450480694791,-14.8417831418,75.575183427031));
#131703=CARTESIAN_POINT('Ctrl Pts',(22.5298127564291,-14.866114563,75.203116801731));
#131704=CARTESIAN_POINT('Ctrl Pts',(22.4006621202491,-14.86192846848,74.422696506464));
#131705=CARTESIAN_POINT('Ctrl Pts',(22.5181198569391,-14.70436463479,73.2633823361753));
#131706=CARTESIAN_POINT('Ctrl Pts',(22.9377195244991,-14.4052238805,72.1556566073007));
#131707=CARTESIAN_POINT('Ctrl Pts',(23.6141508774891,-13.99538058674,71.163675788398));
#131708=CARTESIAN_POINT('Ctrl Pts',(24.4918032145691,-13.50533859052,70.299994638951));
#131709=CARTESIAN_POINT('Ctrl Pts',(25.5329266094991,-12.95204779512,69.5496905418731));
#131710=CARTESIAN_POINT('Ctrl Pts',(26.7219181594991,-12.33886835717,68.8939981611091));
#131711=CARTESIAN_POINT('Ctrl Pts',(28.0550484564891,-11.66205659809,68.32348737336));
#131712=CARTESIAN_POINT('Ctrl Pts',(29.5302626991891,-10.91639130965,67.842821810496));
#131713=CARTESIAN_POINT('Ctrl Pts',(30.7112123601191,-10.3172835446,67.571237827604));
#131714=CARTESIAN_POINT('Ctrl Pts',(31.3905930089891,-9.97074480891598,
67.457066442736));
#131715=CARTESIAN_POINT('Ctrl Pts',(31.5567731140791,-9.88587105497599,
67.431705971039));
#131716=CARTESIAN_POINT('Ctrl Pts',(27.4727097388691,-14.99894242272,74.370845864195));
#131717=CARTESIAN_POINT('Ctrl Pts',(27.4690374908891,-14.99927412475,74.362370216541));
#131718=CARTESIAN_POINT('Ctrl Pts',(27.4146355861491,-15.00404176909,74.231520094978));
#131719=CARTESIAN_POINT('Ctrl Pts',(27.3717438376491,-15.00325792021,73.9585721062895));
#131720=CARTESIAN_POINT('Ctrl Pts',(27.4972980083791,-14.97219965841,73.5156372957745));
#131721=CARTESIAN_POINT('Ctrl Pts',(27.8267501244891,-14.90490385564,73.0117077491551));
#131722=CARTESIAN_POINT('Ctrl Pts',(28.3632567205591,-14.79417301808,72.4487361234403));
#131723=CARTESIAN_POINT('Ctrl Pts',(29.0954791031191,-14.63302923949,71.833557915698));
#131724=CARTESIAN_POINT('Ctrl Pts',(30.0097285339691,-14.41300577028,71.171242909551));
#131725=CARTESIAN_POINT('Ctrl Pts',(31.1001512767791,-14.12091813026,70.4622944187711));
#131726=CARTESIAN_POINT('Ctrl Pts',(32.3671840294791,-13.73672387177,69.7064055545461));
#131727=CARTESIAN_POINT('Ctrl Pts',(33.8128240385791,-13.23052362994,68.90703904439));
#131728=CARTESIAN_POINT('Ctrl Pts',(35.0038717625891,-12.73614203142,68.297720297344));
#131729=CARTESIAN_POINT('Ctrl Pts',(35.7025055078291,-12.40446635354,67.961264321001));
#131730=CARTESIAN_POINT('Ctrl Pts',(35.8742286296091,-12.32012494619,67.879945375125));
#131731=CARTESIAN_POINT('Ctrl Pts',(29.4810590753118,-10.3417444512209,
65.2638123960938));
#131732=CARTESIAN_POINT('Ctrl Pts',(29.6345266860941,-10.3548479162145,
65.3858288214936));
#131733=CARTESIAN_POINT('Ctrl Pts',(29.7903387355854,-10.3717675925251,
65.5046171518437));
#131734=CARTESIAN_POINT('Ctrl Pts',(29.948127817785,-10.3924631647627,65.6198958223942));
#131735=CARTESIAN_POINT('Ctrl Pts',(30.1076455746656,-10.4133854694917,
65.736437440395));
#131736=CARTESIAN_POINT('Ctrl Pts',(30.26918353621,-10.438166853462,65.8493917336466));
#131737=CARTESIAN_POINT('Ctrl Pts',(30.4323438463269,-10.4667289049876,
65.9585030743414));
#131738=CARTESIAN_POINT('Ctrl Pts',(30.5955041564438,-10.4952909565132,
66.0676144150361));
#131739=CARTESIAN_POINT('Ctrl Pts',(30.7602863706003,-10.5276335464042,
66.1728825820115));
#131740=CARTESIAN_POINT('Ctrl Pts',(30.9262808011331,-10.5636428134725,
66.2740912134265));
#131741=CARTESIAN_POINT('Ctrl Pts',(31.0913257917805,-10.5994461180016,
66.3747209608927));
#131742=CARTESIAN_POINT('Ctrl Pts',(31.2575687584314,-10.6388740362011,
66.4713373530446));
#131743=CARTESIAN_POINT('Ctrl Pts',(31.4246015632957,-10.6817828365551,
66.5637694060554));
#131744=CARTESIAN_POINT('Ctrl Pts',(31.5924715009742,-10.7249066866702,
66.6566647088135));
#131745=CARTESIAN_POINT('Ctrl Pts',(31.7611387787817,-10.7715461974904,
66.7453335089057));
#131746=CARTESIAN_POINT('Ctrl Pts',(31.9301906162814,-10.8215255613416,
66.8296458007108));
#131747=CARTESIAN_POINT('Ctrl Pts',(32.0986259760348,-10.8713226665079,
66.9136506326717));
#131748=CARTESIAN_POINT('Ctrl Pts',(32.267442692503,-10.9244350361494,66.9933306894848));
#131749=CARTESIAN_POINT('Ctrl Pts',(32.4362402859212,-10.980662794166,67.0686011625235));
#131750=CARTESIAN_POINT('Ctrl Pts',(32.6071295117973,-11.0375872908111,
67.144804339408));
#131751=CARTESIAN_POINT('Ctrl Pts',(32.7779990938665,-11.0977046862795,
67.216488060209));
#131752=CARTESIAN_POINT('Ctrl Pts',(32.9484476739858,-11.1607845021936,
67.2836092914197));
#131753=CARTESIAN_POINT('Ctrl Pts',(33.1198528403072,-11.2242183326819,
67.3511072183095));
#131754=CARTESIAN_POINT('Ctrl Pts',(33.2908318931408,-11.2906476239985,
67.4139913896642));
#131755=CARTESIAN_POINT('Ctrl Pts',(33.4609969732177,-11.3598192426461,
67.472263038667));
#131756=CARTESIAN_POINT('Ctrl Pts',(33.6329763863426,-11.4297283824915,
67.5311559912798));
#131757=CARTESIAN_POINT('Ctrl Pts',(33.8041240204778,-11.5024383239172,
67.5853376584749));
#131758=CARTESIAN_POINT('Ctrl Pts',(33.9740657157468,-11.5776733361085,
67.6348536143392));
#131759=CARTESIAN_POINT('Ctrl Pts',(34.1450660047094,-11.6533769990881,
67.6846780129228));
#131760=CARTESIAN_POINT('Ctrl Pts',(34.3148449983275,-11.731636951271,67.7297786077743));
#131761=CARTESIAN_POINT('Ctrl Pts',(34.4830527710675,-11.8121627363735,
67.7702438497114));
#131762=CARTESIAN_POINT('Ctrl Pts',(34.653232272717,-11.8936324434831,67.8111834245884));
#131763=CARTESIAN_POINT('Ctrl Pts',(34.8218032405913,-11.9774210769124,
67.8473785768995));
#131764=CARTESIAN_POINT('Ctrl Pts',(34.9884394131694,-12.0632232380785,
67.8789603878941));
#131765=CARTESIAN_POINT('Ctrl Pts',(35.1256376224812,-12.13386758069,67.9049629529329));
#131766=CARTESIAN_POINT('Ctrl Pts',(35.2615248946371,-12.2058767063507,
67.9278390016601));
#131767=CARTESIAN_POINT('Ctrl Pts',(35.3959387673533,-12.2790802564028,
67.9476794933271));
#131768=CARTESIAN_POINT('Ctrl Pts',(25.3886736533591,-11.44208510792,60.2115109699));
#131769=CARTESIAN_POINT('Ctrl Pts',(25.5981770475491,-11.17175375805,60.22632667139));
#131770=CARTESIAN_POINT('Ctrl Pts',(25.8078177068491,-10.88204468039,60.24561988886));
#131771=CARTESIAN_POINT('Ctrl Pts',(26.0168787184791,-10.57129328633,60.270855635));
#131772=CARTESIAN_POINT('Ctrl Pts',(27.3087836696091,-9.624602273718,64.44463626086));
#131773=CARTESIAN_POINT('Ctrl Pts',(27.5425179224791,-9.479512324536,64.50183542974));
#131774=CARTESIAN_POINT('Ctrl Pts',(27.7759878147791,-9.32787789472698,
64.56281239081));
#131775=CARTESIAN_POINT('Ctrl Pts',(28.0092438744591,-9.16583693103399,
64.625382279757));
#131776=CARTESIAN_POINT('Ctrl Pts',(31.2407814247091,-10.04443147536,67.489770329979));
#131777=CARTESIAN_POINT('Ctrl Pts',(31.5318184331991,-9.93037722233698,
67.468249475135));
#131778=CARTESIAN_POINT('Ctrl Pts',(31.8153253258691,-9.81435677539199,
67.4542319002));
#131779=CARTESIAN_POINT('Ctrl Pts',(32.0927104552091,-9.69360679656099,
67.4456953393931));
#131780=CARTESIAN_POINT('Ctrl Pts',(35.5328635075091,-12.52520554518,68.067674694392));
#131781=CARTESIAN_POINT('Ctrl Pts',(35.8902027012991,-12.3349434155,67.879400029176));
#131782=CARTESIAN_POINT('Ctrl Pts',(36.2289341849091,-12.1371151135,67.705214293035));
#131783=CARTESIAN_POINT('Ctrl Pts',(36.5518441070791,-11.93289063421,67.547001987805));
#131784=CARTESIAN_POINT('Ctrl Pts',(36.2511910984291,-0.816951121684487,
99.13095237507));
#131785=CARTESIAN_POINT('Ctrl Pts',(36.2200982088991,-1.45683196280799,
99.1098451401801));
#131786=CARTESIAN_POINT('Ctrl Pts',(36.0778630790891,-2.85039942836099,
99.0419676728901));
#131787=CARTESIAN_POINT('Ctrl Pts',(35.6275483510391,-4.94247000735899,
98.84599903898));
#131788=CARTESIAN_POINT('Ctrl Pts',(34.9397597871691,-7.05113172994599,
98.51977184372));
#131789=CARTESIAN_POINT('Ctrl Pts',(34.0734741662491,-9.09163743804897,
98.0649602571899));
#131790=CARTESIAN_POINT('Ctrl Pts',(33.0099168483791,-11.12983443612,97.44906592845));
#131791=CARTESIAN_POINT('Ctrl Pts',(31.7699785170891,-13.12298748389,96.6589115129399));
#131792=CARTESIAN_POINT('Ctrl Pts',(30.4746258290591,-14.92251334854,95.75721789378));
#131793=CARTESIAN_POINT('Ctrl Pts',(29.1968815731991,-16.50069944243,94.7947864407199));
#131794=CARTESIAN_POINT('Ctrl Pts',(27.9225293421991,-17.92619343051,93.76208048801));
#131795=CARTESIAN_POINT('Ctrl Pts',(26.5896727465691,-19.28349187111,92.5956876894801));
#131796=CARTESIAN_POINT('Ctrl Pts',(25.1814694175691,-20.58838494568,91.25117303266));
#131797=CARTESIAN_POINT('Ctrl Pts',(23.7249591534991,-21.81419974781,89.71266771848));
#131798=CARTESIAN_POINT('Ctrl Pts',(22.2142909846591,-22.9637208008,87.91364117654));
#131799=CARTESIAN_POINT('Ctrl Pts',(20.6065395382091,-24.05476593901,85.68623624305));
#131800=CARTESIAN_POINT('Ctrl Pts',(18.9416778012191,-25.02348229969,82.825890425796));
#131801=CARTESIAN_POINT('Ctrl Pts',(17.5339994345191,-25.65356630387,79.417420667109));
#131802=CARTESIAN_POINT('Ctrl Pts',(16.9242179391691,-25.78353110717,76.926255793732));
#131803=CARTESIAN_POINT('Ctrl Pts',(16.7312453442491,-25.77964745785,75.805602355198));
#131804=CARTESIAN_POINT('Ctrl Pts',(34.9680768531591,-0.377262712455286,
92.83793248162));
#131805=CARTESIAN_POINT('Ctrl Pts',(34.9401900659091,-0.768818210978587,
92.83356221903));
#131806=CARTESIAN_POINT('Ctrl Pts',(34.8109275223991,-1.62812620872499,
92.8325719567701));
#131807=CARTESIAN_POINT('Ctrl Pts',(34.3972755661991,-2.97122279462399,
92.8255990532501));
#131808=CARTESIAN_POINT('Ctrl Pts',(33.7599966114291,-4.39375486831299,
92.76261787049));
#131809=CARTESIAN_POINT('Ctrl Pts',(32.9521573659891,-5.82931930270299,
92.61621541888));
#131810=CARTESIAN_POINT('Ctrl Pts',(31.9551618598791,-7.31697565127499,
92.35621163472));
#131811=CARTESIAN_POINT('Ctrl Pts',(30.7878189799691,-8.81951599642399,
91.9596113594201));
#131812=CARTESIAN_POINT('Ctrl Pts',(29.5643467643691,-10.21287137887,91.45281600972));
#131813=CARTESIAN_POINT('Ctrl Pts',(28.3547145027491,-11.46125770319,90.86912642514));
#131814=CARTESIAN_POINT('Ctrl Pts',(27.1462246720591,-12.60932492795,90.2068010813201));
#131815=CARTESIAN_POINT('Ctrl Pts',(25.8804633212691,-13.72121825748,89.42218714027));
#131816=CARTESIAN_POINT('Ctrl Pts',(24.5415426038291,-14.80846467629,88.4770655865801));
#131817=CARTESIAN_POINT('Ctrl Pts',(23.1553900553591,-15.84725088264,87.34998754959));
#131818=CARTESIAN_POINT('Ctrl Pts',(21.7169286490991,-16.83785256507,85.9795861337301));
#131819=CARTESIAN_POINT('Ctrl Pts',(20.1864646779891,-17.79411649535,84.2176273015201));
#131820=CARTESIAN_POINT('Ctrl Pts',(18.6056376920291,-18.65837811088,81.868380902977));
#131821=CARTESIAN_POINT('Ctrl Pts',(17.2833457609491,-19.22934869733,78.9739891356611));
#131822=CARTESIAN_POINT('Ctrl Pts',(16.7318898964791,-19.34793907064,76.820460370021));
#131823=CARTESIAN_POINT('Ctrl Pts',(16.5654152065891,-19.34439445674,75.849914932886));
#131824=CARTESIAN_POINT('Ctrl Pts',(38.6686947048191,-0.267618408180286,
87.57152762521));
#131825=CARTESIAN_POINT('Ctrl Pts',(38.6331457099391,-0.640502714598286,
87.56228047755));
#131826=CARTESIAN_POINT('Ctrl Pts',(38.4681697649291,-1.45257130791499,
87.5371031361401));
#131827=CARTESIAN_POINT('Ctrl Pts',(37.9543196144491,-2.67152049410099,
87.46697907679));
#131828=CARTESIAN_POINT('Ctrl Pts',(37.1964789572891,-3.89993484531899,
87.33954011223));
#131829=CARTESIAN_POINT('Ctrl Pts',(36.2722354399091,-5.08847143352099,
87.1482156939501));
#131830=CARTESIAN_POINT('Ctrl Pts',(35.1711071623791,-6.27550574943099,
86.8740206795701));
#131831=CARTESIAN_POINT('Ctrl Pts',(33.9234036585391,-7.436166673543,86.50611895787));
#131832=CARTESIAN_POINT('Ctrl Pts',(32.6526782149891,-8.48396598041999,
86.07171874038));
#131833=CARTESIAN_POINT('Ctrl Pts',(31.4266015655591,-9.40280963542199,
85.5959755830301));
#131834=CARTESIAN_POINT('Ctrl Pts',(30.2282183070691,-10.23269364386,85.07485106796));
#131835=CARTESIAN_POINT('Ctrl Pts',(29.0009821455491,-11.02282107056,84.4750277186701));
#131836=CARTESIAN_POINT('Ctrl Pts',(27.7349646372491,-11.7823880216,83.77066674245));
#131837=CARTESIAN_POINT('Ctrl Pts',(26.4611997445191,-12.49587308951,82.949856613029));
#131838=CARTESIAN_POINT('Ctrl Pts',(25.1820693516891,-13.16490311603,81.9728674396441));
#131839=CARTESIAN_POINT('Ctrl Pts',(23.8728795301391,-13.79985263807,80.741966022882));
#131840=CARTESIAN_POINT('Ctrl Pts',(22.5850112147791,-14.36356654138,79.133191069062));
#131841=CARTESIAN_POINT('Ctrl Pts',(21.5697113092491,-14.73019815096,77.183930116823));
#131842=CARTESIAN_POINT('Ctrl Pts',(21.1758003549191,-14.80581932552,75.7409655371681));
#131843=CARTESIAN_POINT('Ctrl Pts',(21.0646250899491,-14.8035595922,75.088550558094));
#131844=CARTESIAN_POINT('Ctrl Pts',(45.0312706731691,-0.556809233210386,
86.63588923546));
#131845=CARTESIAN_POINT('Ctrl Pts',(44.9819984429591,-1.15239083593299,
86.6032111113799));
#131846=CARTESIAN_POINT('Ctrl Pts',(44.7550297579291,-2.43387817146999,
86.47794742155));
#131847=CARTESIAN_POINT('Ctrl Pts',(44.0669849657891,-4.23139684260399,
86.1321464635101));
#131848=CARTESIAN_POINT('Ctrl Pts',(43.0931519133991,-5.87949518942999,
85.65298684557));
#131849=CARTESIAN_POINT('Ctrl Pts',(41.9506857162891,-7.33390305288999,
85.0915934778799));
#131850=CARTESIAN_POINT('Ctrl Pts',(40.6400631633491,-8.65884473130499,
84.44202906066));
#131851=CARTESIAN_POINT('Ctrl Pts',(39.2094613534091,-9.84085525044999,
83.71996478425));
#131852=CARTESIAN_POINT('Ctrl Pts',(37.8019957376891,-10.82051536224,82.99003573172));
#131853=CARTESIAN_POINT('Ctrl Pts',(36.4852355554891,-11.6168290835,82.283717786993));
#131854=CARTESIAN_POINT('Ctrl Pts',(35.2348621603691,-12.28740211764,81.586024678646));
#131855=CARTESIAN_POINT('Ctrl Pts',(33.9934103628291,-12.88127932846,80.858065721516));
#131856=CARTESIAN_POINT('Ctrl Pts',(32.7581770629291,-13.40872065919,80.08477919832));
#131857=CARTESIAN_POINT('Ctrl Pts',(31.5683175582891,-13.86272653758,79.272924596943));
#131858=CARTESIAN_POINT('Ctrl Pts',(30.4356778789491,-14.24928723071,78.407307267481));
#131859=CARTESIAN_POINT('Ctrl Pts',(29.3529211006491,-14.57798235441,77.439888248051));
#131860=CARTESIAN_POINT('Ctrl Pts',(28.3831326036191,-14.83361972799,76.336383711929));
#131861=CARTESIAN_POINT('Ctrl Pts',(27.7038229907891,-14.97888942575,75.170329705841));
#131862=CARTESIAN_POINT('Ctrl Pts',(27.4678322792991,-15.00690558171,74.365048202755));
#131863=CARTESIAN_POINT('Ctrl Pts',(27.4060630052191,-15.00607043787,73.999190543978));
#131864=CARTESIAN_POINT('Origin',(26.4624892479491,-5.,78.749546355382));
#131865=CARTESIAN_POINT('',(-5.14030444921783,-5.,85.3373981618386));
#131866=CARTESIAN_POINT('Ctrl Pts',(-5.03958561217558,-6.,84.3042121015221));
#131867=CARTESIAN_POINT('Ctrl Pts',(-5.01779961145864,-5.9999999999996,
84.4277666513109));
#131868=CARTESIAN_POINT('Ctrl Pts',(-5.00224861254975,-5.97492290499363,
84.560469325189));
#131869=CARTESIAN_POINT('Ctrl Pts',(-4.98975476340367,-5.87416764040792,
84.8064865857881));
#131870=CARTESIAN_POINT('Ctrl Pts',(-4.99272071568298,-5.798526343987,84.9198116323849));
#131871=CARTESIAN_POINT('Ctrl Pts',(-5.01199432837025,-5.62256919818321,
85.1045000068224));
#131872=CARTESIAN_POINT('Ctrl Pts',(-5.03011167864627,-5.50920575318542,
85.1870555783692));
#131873=CARTESIAN_POINT('Ctrl Pts',(-5.07864362193569,-5.26113860665341,
85.3007472862074));
#131874=CARTESIAN_POINT('Ctrl Pts',(-5.1089932976158,-5.12641933949878,
85.3318771610163));
#131875=CARTESIAN_POINT('Ctrl Pts',(-5.14030444921746,-5.,85.3373981618407));
#131876=CARTESIAN_POINT('',(-6.54682286628224,-5.,85.5854053076332));
#131877=CARTESIAN_POINT('Origin',(-6.72047103979891,-5.,84.60059755389));
#131878=CARTESIAN_POINT('',(-0.138906894980912,-5.,84.45551683178));
#131879=CARTESIAN_POINT('Origin',(-7.10051551200191,5.,84.66760964821));
#131880=CARTESIAN_POINT('',(-5.14030444921695,5.,85.3373981618436));
#131881=CARTESIAN_POINT('Ctrl Pts',(-5.14030444921696,5.,85.3373981618436));
#131882=CARTESIAN_POINT('Ctrl Pts',(-5.10929140005093,5.12521574553663,
85.3319297245216));
#131883=CARTESIAN_POINT('Ctrl Pts',(-5.07918376137443,5.2587323981861,85.301326613419));
#131884=CARTESIAN_POINT('Ctrl Pts',(-5.03087653636086,5.50495104913208,
85.1895150329288));
#131885=CARTESIAN_POINT('Ctrl Pts',(-5.01273977349526,5.61766789433613,
85.1083121247498));
#131886=CARTESIAN_POINT('Ctrl Pts',(-4.99292749239007,5.7948754580924,84.924877408976));
#131887=CARTESIAN_POINT('Ctrl Pts',(-4.98968965602442,5.87184753647394,
84.8108658563746));
#131888=CARTESIAN_POINT('Ctrl Pts',(-5.00197073577722,5.97442824468255,
84.5629279946691));
#131889=CARTESIAN_POINT('Ctrl Pts',(-5.01758370837151,6.,84.4289910985632));
#131890=CARTESIAN_POINT('Ctrl Pts',(-5.03958561217562,6.,84.3042121015219));
#131891=CARTESIAN_POINT('',(-6.54682286760695,5.,85.5854053078674));
#131892=CARTESIAN_POINT('',(-6.54682287186491,5.,85.58540530862));
#131893=CARTESIAN_POINT('Origin',(-6.72047103979891,5.,84.60059755389));
#131894=CARTESIAN_POINT('Ctrl Pts',(25.6728519466291,11.05620868577,60.1753393120401));
#131895=CARTESIAN_POINT('Ctrl Pts',(25.5908811595391,11.17010610055,60.1922130334301));
#131896=CARTESIAN_POINT('Ctrl Pts',(25.0176949940091,11.96220506401,60.3226366877));
#131897=CARTESIAN_POINT('Ctrl Pts',(23.9454509711491,13.3937300709,60.72216890038));
#131898=CARTESIAN_POINT('Ctrl Pts',(22.4585522519091,15.28518638036,61.63777386195));
#131899=CARTESIAN_POINT('Ctrl Pts',(21.0802507927691,16.97737598619,62.82703989993));
#131900=CARTESIAN_POINT('Ctrl Pts',(19.8267910571591,18.48224713566,64.271659173669));
#131901=CARTESIAN_POINT('Ctrl Pts',(18.7098146781291,19.81562337201,66.003616761918));
#131902=CARTESIAN_POINT('Ctrl Pts',(17.7716110472991,20.96488749236,68.078902873165));
#131903=CARTESIAN_POINT('Ctrl Pts',(17.1084342304291,21.8744622819,70.533431788808));
#131904=CARTESIAN_POINT('Ctrl Pts',(16.8638554479991,22.45052823568,73.2803532769174));
#131905=CARTESIAN_POINT('Ctrl Pts',(17.0786448222291,22.59937448267,75.596712572949));
#131906=CARTESIAN_POINT('Ctrl Pts',(17.3662061271091,22.55171003512,76.874515663416));
#131907=CARTESIAN_POINT('Ctrl Pts',(17.4669987734891,22.52571394401,77.2562285499651));
#131908=CARTESIAN_POINT('Ctrl Pts',(27.6093946371291,9.39445532140801,64.447920892227));
#131909=CARTESIAN_POINT('Ctrl Pts',(27.5226174428891,9.46737944809301,64.451034788112));
#131910=CARTESIAN_POINT('Ctrl Pts',(26.9160359092391,9.97752475953103,64.482341733254));
#131911=CARTESIAN_POINT('Ctrl Pts',(25.7838601800091,10.93479181558,64.661006837171));
#131912=CARTESIAN_POINT('Ctrl Pts',(24.2207011124691,12.25908842062,65.194134063823));
#131913=CARTESIAN_POINT('Ctrl Pts',(22.7783053134691,13.48485509378,65.959148542412));
#131914=CARTESIAN_POINT('Ctrl Pts',(21.4726982157391,14.6052048364,66.94431046259));
#131915=CARTESIAN_POINT('Ctrl Pts',(20.3137223160191,15.62131353079,68.176238741846));
#131916=CARTESIAN_POINT('Ctrl Pts',(19.3392518035291,16.51491733119,69.702089136366));
#131917=CARTESIAN_POINT('Ctrl Pts',(18.6353752499191,17.23396255898,71.553480602797));
#131918=CARTESIAN_POINT('Ctrl Pts',(18.3290383767791,17.69470562174,73.6596809561242));
#131919=CARTESIAN_POINT('Ctrl Pts',(18.4647369076291,17.81439079021,75.444726555105));
#131920=CARTESIAN_POINT('Ctrl Pts',(18.6950959018691,17.77610222599,76.424554931989));
#131921=CARTESIAN_POINT('Ctrl Pts',(18.7775986176291,17.7552396856,76.716506355083));
#131922=CARTESIAN_POINT('Ctrl Pts',(31.5629272267991,9.88281068194302,67.430842306303));
#131923=CARTESIAN_POINT('Ctrl Pts',(31.4711681472091,9.92967730101103,67.444807195928));
#131924=CARTESIAN_POINT('Ctrl Pts',(30.8310903628191,10.25631090589,67.5476759313801));
#131925=CARTESIAN_POINT('Ctrl Pts',(29.6521222456891,10.85487243909,67.805767900236));
#131926=CARTESIAN_POINT('Ctrl Pts',(28.0597002587091,11.65964394348,68.317830215232));
#131927=CARTESIAN_POINT('Ctrl Pts',(26.6228516811691,12.38921116325,68.938303098405));
#131928=CARTESIAN_POINT('Ctrl Pts',(25.3542093351291,13.0450930181,69.658831925755));
#131929=CARTESIAN_POINT('Ctrl Pts',(24.2590278301191,13.63170757615,70.4940295766521));
#131930=CARTESIAN_POINT('Ctrl Pts',(23.3629396071591,14.14148255666,71.468571308628));
#131931=CARTESIAN_POINT('Ctrl Pts',(22.7218359561591,14.5476997234,72.5973874861561));
#131932=CARTESIAN_POINT('Ctrl Pts',(22.4115473378591,14.8062209636,73.8396950223705));
#131933=CARTESIAN_POINT('Ctrl Pts',(22.4566140195691,14.87316749049,74.870971069554));
#131934=CARTESIAN_POINT('Ctrl Pts',(22.5996423578891,14.85173828971,75.432105059216));
#131935=CARTESIAN_POINT('Ctrl Pts',(22.6529499976691,14.84005551372,75.5989411619891));
#131936=CARTESIAN_POINT('Ctrl Pts',(35.8805628265291,12.31710390136,67.87700830848));
#131937=CARTESIAN_POINT('Ctrl Pts',(35.7857292024291,12.36372287642,67.921898444141));
#131938=CARTESIAN_POINT('Ctrl Pts',(35.1260583462191,12.68200901524,68.23708902494));
#131939=CARTESIAN_POINT('Ctrl Pts',(33.9330000499891,13.18738451274,68.8416951696051));
#131940=CARTESIAN_POINT('Ctrl Pts',(32.3705467692491,13.73746778379,69.702912182422));
#131941=CARTESIAN_POINT('Ctrl Pts',(31.0065678005891,14.14850934188,70.5189831644171));
#131942=CARTESIAN_POINT('Ctrl Pts',(29.8485481528991,14.4541608558,71.28034056044));
#131943=CARTESIAN_POINT('Ctrl Pts',(28.8962838945291,14.67861693811,71.987970801025));
#131944=CARTESIAN_POINT('Ctrl Pts',(28.1604571839791,14.83686516773,72.6398212113681));
#131945=CARTESIAN_POINT('Ctrl Pts',(27.6593550752991,14.93874245386,73.2287174375679));
#131946=CARTESIAN_POINT('Ctrl Pts',(27.4045731969891,14.99268753181,73.7451354687612));
#131947=CARTESIAN_POINT('Ctrl Pts',(27.3853582494091,15.0053667451,74.11532093663));
#131948=CARTESIAN_POINT('Ctrl Pts',(27.4474386542391,15.00123185086,74.312087977728));
#131949=CARTESIAN_POINT('Ctrl Pts',(27.4728519056491,14.99893719101,74.370762926049));
#131950=CARTESIAN_POINT('Origin',(33.8227660273614,17.5861371975626,59.0248880432778));
#131951=CARTESIAN_POINT('Ctrl Pts',(26.0076877261891,10.58495646334,60.26985796972));
#131952=CARTESIAN_POINT('Ctrl Pts',(25.7990037333791,10.89447975427,60.24482455385));
#131953=CARTESIAN_POINT('Ctrl Pts',(25.5896565743691,11.1831771459,60.22557462704));
#131954=CARTESIAN_POINT('Ctrl Pts',(25.3807021623791,11.45236674632,60.21090371374));
#131955=CARTESIAN_POINT('Ctrl Pts',(27.9987970739791,9.17295597816802,64.622590824873));
#131956=CARTESIAN_POINT('Ctrl Pts',(27.7660735618591,9.33426324017502,64.560255312909));
#131957=CARTESIAN_POINT('Ctrl Pts',(27.5333174178191,9.48524635017302,64.499674997551));
#131958=CARTESIAN_POINT('Ctrl Pts',(27.3000253208991,9.63004663000602,64.442635376589));
#131959=CARTESIAN_POINT('Ctrl Pts',(32.0801713998191,9.69904765178202,67.445984142724));
#131960=CARTESIAN_POINT('Ctrl Pts',(31.8033473372391,9.81925633458402,67.454791081483));
#131961=CARTESIAN_POINT('Ctrl Pts',(31.5208971300691,9.93468827936802,67.469340771313));
#131962=CARTESIAN_POINT('Ctrl Pts',(31.2300886277791,10.04875492352,67.490838049821));
#131963=CARTESIAN_POINT('Ctrl Pts',(36.5371673514891,11.94221289613,67.553890268911));
#131964=CARTESIAN_POINT('Ctrl Pts',(36.2147089752091,12.14570654659,67.712396250694));
#131965=CARTESIAN_POINT('Ctrl Pts',(35.8771568089191,12.34268599228,67.886973156649));
#131966=CARTESIAN_POINT('Ctrl Pts',(35.5198166400391,12.53258632276,68.07491847425));
#131967=CARTESIAN_POINT('Ctrl Pts',(29.6607179856746,9.94038469281037,64.9669467760166));
#131968=CARTESIAN_POINT('Ctrl Pts',(30.1590068583674,9.97665887137027,65.3620001554969));
#131969=CARTESIAN_POINT('Ctrl Pts',(30.6858019445019,10.0485591111603,65.7214144613769));
#131970=CARTESIAN_POINT('Ctrl Pts',(31.7706505757518,10.2607534512662,66.3509683676041));
#131971=CARTESIAN_POINT('Ctrl Pts',(32.3285497113111,10.4009981803986,66.6210514629286));
#131972=CARTESIAN_POINT('Ctrl Pts',(33.4471502167783,10.7395896426921,67.0635873838908));
#131973=CARTESIAN_POINT('Ctrl Pts',(34.0077151370051,10.9378504308792,67.2360632541964));
#131974=CARTESIAN_POINT('Ctrl Pts',(35.1057006193385,11.3778331546057,67.4848315470064));
#131975=CARTESIAN_POINT('Ctrl Pts',(35.6430402158663,11.6194638105209,67.5612071130097));
#131976=CARTESIAN_POINT('Ctrl Pts',(36.1590910689312,11.8739168214411,67.5956414534657));
#131977=CARTESIAN_POINT('Ctrl Pts',(29.1301066186391,-0.189325198801386,
61.01350638832));
#131978=CARTESIAN_POINT('Ctrl Pts',(29.1301171086491,-0.188219559987986,
61.01351029305));
#131979=CARTESIAN_POINT('Ctrl Pts',(29.1327100608491,0.0875421358441442,
61.0144753342501));
#131980=CARTESIAN_POINT('Ctrl Pts',(29.1259762223391,0.661869688765914,
61.01189519272));
#131981=CARTESIAN_POINT('Ctrl Pts',(29.0771717435891,1.54597290477701,60.99362463442));
#131982=CARTESIAN_POINT('Ctrl Pts',(28.9836009802591,2.46822553813401,60.95933878612));
#131983=CARTESIAN_POINT('Ctrl Pts',(28.8434009410291,3.40217169142201,60.90943180935));
#131984=CARTESIAN_POINT('Ctrl Pts',(28.6591089571391,4.32587075588902,60.84674448141));
#131985=CARTESIAN_POINT('Ctrl Pts',(28.4369612179591,5.21837798582801,60.77569210592));
#131986=CARTESIAN_POINT('Ctrl Pts',(28.1848437175191,6.06426036422701,60.7009064822));
#131987=CARTESIAN_POINT('Ctrl Pts',(27.9087860776491,6.86007287828601,60.6258067072));
#131988=CARTESIAN_POINT('Ctrl Pts',(27.6123385282491,7.60966710787701,60.55276423571));
#131989=CARTESIAN_POINT('Ctrl Pts',(27.2953631596791,8.32198182378201,60.48284598351));
#131990=CARTESIAN_POINT('Ctrl Pts',(26.9557511764191,9.005721841742,60.4165783700401));
#131991=CARTESIAN_POINT('Ctrl Pts',(26.5893525670591,9.66929542127001,60.35387730236));
#131992=CARTESIAN_POINT('Ctrl Pts',(26.2203209213991,10.27138042785,60.29879040396));
#131993=CARTESIAN_POINT('Ctrl Pts',(25.9689287341191,10.644849342,60.2655374623699));
#131994=CARTESIAN_POINT('Ctrl Pts',(25.8531256415191,10.80992702953,60.25094661876));
#131995=CARTESIAN_POINT('Ctrl Pts',(32.4394962150591,-0.167024129634686,
64.749778129328));
#131996=CARTESIAN_POINT('Ctrl Pts',(32.4395119001291,-0.166048254254086,
64.749778207149));
#131997=CARTESIAN_POINT('Ctrl Pts',(32.4433890940291,0.0773483601619742,
64.749797340987));
#131998=CARTESIAN_POINT('Ctrl Pts',(32.4333485056991,0.584125359624015,
64.749674192331));
#131999=CARTESIAN_POINT('Ctrl Pts',(32.3605007182391,1.36476629894001,64.749089885125));
#132000=CARTESIAN_POINT('Ctrl Pts',(32.2210472241191,2.18063018348501,64.747997284018));
#132001=CARTESIAN_POINT('Ctrl Pts',(32.0127791294291,3.00860637761601,64.7459906738651));
#132002=CARTESIAN_POINT('Ctrl Pts',(31.7401977260491,3.82775603881801,64.742789422125));
#132003=CARTESIAN_POINT('Ctrl Pts',(31.4134431009691,4.61757681790401,64.738144734598));
#132004=CARTESIAN_POINT('Ctrl Pts',(31.0452165535591,5.36205215158601,64.731695005533));
#132005=CARTESIAN_POINT('Ctrl Pts',(30.6455255091491,6.05580663071101,64.722864194901));
#132006=CARTESIAN_POINT('Ctrl Pts',(30.2207588970491,6.70093674850502,64.711266502485));
#132007=CARTESIAN_POINT('Ctrl Pts',(29.7720976663891,7.30453372749301,64.696364088189));
#132008=CARTESIAN_POINT('Ctrl Pts',(29.2980989030191,7.87385850082301,64.677553778107));
#132009=CARTESIAN_POINT('Ctrl Pts',(28.7946523707591,8.41600459963101,64.65389332063));
#132010=CARTESIAN_POINT('Ctrl Pts',(28.2960783560391,8.89829044039401,64.626420017414));
#132011=CARTESIAN_POINT('Ctrl Pts',(27.9617318331491,9.19221969143401,64.605290317917));
#132012=CARTESIAN_POINT('Ctrl Pts',(27.8087966595791,9.32115549717301,64.595039748394));
#132013=CARTESIAN_POINT('Ctrl Pts',(37.3447733550991,-0.163980749822586,
65.672020113937));
#132014=CARTESIAN_POINT('Ctrl Pts',(37.3447903319791,-0.163021244871686,
65.672013375157));
#132015=CARTESIAN_POINT('Ctrl Pts',(37.3489869127291,0.0762913557168342,
65.670347533373));
#132016=CARTESIAN_POINT('Ctrl Pts',(37.3381301106191,0.574047424134414,
65.6745698296091));
#132017=CARTESIAN_POINT('Ctrl Pts',(37.2592439496991,1.34342225796901,65.705562251813));
#132018=CARTESIAN_POINT('Ctrl Pts',(37.1076946494091,2.15544100000801,65.764984131401));
#132019=CARTESIAN_POINT('Ctrl Pts',(36.8799583449391,2.99224404832201,65.853458683805));
#132020=CARTESIAN_POINT('Ctrl Pts',(36.5791966436791,3.83427439653601,65.968635887493));
#132021=CARTESIAN_POINT('Ctrl Pts',(36.2143485134491,4.66159926833502,66.105852848797));
#132022=CARTESIAN_POINT('Ctrl Pts',(35.7971950983691,5.45638915732801,66.2592392798661));
#132023=CARTESIAN_POINT('Ctrl Pts',(35.3370171608391,6.20886237306701,66.423469431256));
#132024=CARTESIAN_POINT('Ctrl Pts',(34.8393757953291,6.91789819603101,66.595098260699));
#132025=CARTESIAN_POINT('Ctrl Pts',(34.3039881031491,7.58819161688801,66.772690714863));
#132026=CARTESIAN_POINT('Ctrl Pts',(33.7273674188191,8.22516768701401,66.955765342088));
#132027=CARTESIAN_POINT('Ctrl Pts',(33.1027247613091,8.83364473392301,67.144103602868));
#132028=CARTESIAN_POINT('Ctrl Pts',(32.4716469885691,9.37388448744801,67.323077248415));
#132029=CARTESIAN_POINT('Ctrl Pts',(32.0408207166291,9.70072437204801,67.43736279039));
#132030=CARTESIAN_POINT('Ctrl Pts',(31.8422612865091,9.84329152591,67.488269711376));
#132031=CARTESIAN_POINT('Ctrl Pts',(41.7851639409491,-0.181473624899186,
63.392785855529));
#132032=CARTESIAN_POINT('Ctrl Pts',(41.7851777637091,-0.180410219933086,
63.3927721742101));
#132033=CARTESIAN_POINT('Ctrl Pts',(41.7885946976491,0.0848151845503942,
63.389390169875));
#132034=CARTESIAN_POINT('Ctrl Pts',(41.7797551203791,0.635869761000514,
63.3980207821121));
#132035=CARTESIAN_POINT('Ctrl Pts',(41.7153723246291,1.49090770575301,63.461214595618));
#132036=CARTESIAN_POINT('Ctrl Pts',(41.5905957566191,2.40324030861401,63.5830492274001));
#132037=CARTESIAN_POINT('Ctrl Pts',(41.4001699495591,3.35995874213701,63.766573362888));
#132038=CARTESIAN_POINT('Ctrl Pts',(41.1431760010491,4.34268737770601,64.0092889910721));
#132039=CARTESIAN_POINT('Ctrl Pts',(40.8227513495791,5.33195090286801,64.304223540789));
#132040=CARTESIAN_POINT('Ctrl Pts',(40.4444080932191,6.30763911352001,64.6417970378541));
#132041=CARTESIAN_POINT('Ctrl Pts',(40.0123011460691,7.25493929209501,65.013174868938));
#132042=CARTESIAN_POINT('Ctrl Pts',(39.5278450183091,8.16940297534801,65.412835992148));
#132043=CARTESIAN_POINT('Ctrl Pts',(38.9871252392491,9.05378692831301,65.839532615121));
#132044=CARTESIAN_POINT('Ctrl Pts',(38.3827603673591,9.91205960048301,66.294105186865));
#132045=CARTESIAN_POINT('Ctrl Pts',(37.7036895340791,10.7467594847,66.778336709372));
#132046=CARTESIAN_POINT('Ctrl Pts',(36.9928132575991,11.49835899722,67.2558594670681));
#132047=CARTESIAN_POINT('Ctrl Pts',(36.4925142868991,11.95673360421,67.571962452628));
#132048=CARTESIAN_POINT('Ctrl Pts',(36.2590057995691,12.1569786201,67.715150981305));
#132049=CARTESIAN_POINT('',(28.7111341928544,9.91622892707765,64.1370768870198));
#132050=CARTESIAN_POINT('Ctrl Pts',(28.7109512875422,9.91605044034905,64.1371092663083));
#132051=CARTESIAN_POINT('Ctrl Pts',(29.148581955101,9.45497570515531,64.0599431720322));
#132052=CARTESIAN_POINT('Ctrl Pts',(29.5494667496106,8.96082664876228,63.9892563666044));
#132053=CARTESIAN_POINT('Ctrl Pts',(30.2796472512486,7.90616282799916,63.8605058433784));
#132054=CARTESIAN_POINT('Ctrl Pts',(30.6055849921346,7.34840822091101,63.803034225629));
#132055=CARTESIAN_POINT('Ctrl Pts',(30.8903745807655,6.76811552282497,63.7528181373285));
#132056=CARTESIAN_POINT('',(26.0609380919473,10.6024171740512,60.5235125955283));
#132057=CARTESIAN_POINT('Ctrl Pts',(26.0609344740391,10.60241468947,60.52351356035));
#132058=CARTESIAN_POINT('Ctrl Pts',(26.3648183022441,10.401891666185,61.146627197821));
#132059=CARTESIAN_POINT('Ctrl Pts',(26.7394129476864,10.2366073125495,61.7754982937505));
#132060=CARTESIAN_POINT('Ctrl Pts',(27.6275351327377,10.001078989055,62.9967881531343));
#132061=CARTESIAN_POINT('Ctrl Pts',(28.1411187061796,9.93108796101538,63.5888221040813));
#132062=CARTESIAN_POINT('Ctrl Pts',(28.7111243222551,9.91621952674004,64.1370786896818));
#132063=CARTESIAN_POINT('Ctrl Pts',(29.3346503782312,-0.000127443506814966,
61.2371509483293));
#132064=CARTESIAN_POINT('Ctrl Pts',(29.3346040565051,0.282953605848506,
61.2371193840476));
#132065=CARTESIAN_POINT('Ctrl Pts',(29.3281537463615,0.565553188024372,
61.2348664918606));
#132066=CARTESIAN_POINT('Ctrl Pts',(29.3154481518555,0.847407377566151,
61.2305057032888));
#132067=CARTESIAN_POINT('Ctrl Pts',(29.3021838212238,1.14165627384997,61.2259531464286));
#132068=CARTESIAN_POINT('Ctrl Pts',(29.2821023136189,1.43509359721723,61.2191030646222));
#132069=CARTESIAN_POINT('Ctrl Pts',(29.2553141053501,1.72742139194876,61.2100979542848));
#132070=CARTESIAN_POINT('Ctrl Pts',(29.2299254193272,2.00447682326973,61.2015633066271));
#132071=CARTESIAN_POINT('Ctrl Pts',(29.1985120692105,2.28053633570582,61.1910930274013));
#132072=CARTESIAN_POINT('Ctrl Pts',(29.1611184543843,2.55533716942498,61.1788202705036));
#132073=CARTESIAN_POINT('Ctrl Pts',(29.1590571741844,2.57048525072437,61.1781437488325));
#132074=CARTESIAN_POINT('Ctrl Pts',(29.1569777098301,2.58562950338368,61.1774617529707));
#132075=CARTESIAN_POINT('Ctrl Pts',(29.1548800644485,2.60076988187894,61.1767743062269));
#132076=CARTESIAN_POINT('Ctrl Pts',(29.1351359216109,2.74327909637595,61.1703036955026));
#132077=CARTESIAN_POINT('Ctrl Pts',(29.1137813215554,2.88544521608041,61.1633501010702));
#132078=CARTESIAN_POINT('Ctrl Pts',(29.0908380177679,3.02725396856825,61.1559509750705));
#132079=CARTESIAN_POINT('Ctrl Pts',(29.0484230490313,3.28941385012007,61.1422723130581));
#132080=CARTESIAN_POINT('Ctrl Pts',(29.0005809630906,3.55035400563275,61.1270704993233));
#132081=CARTESIAN_POINT('Ctrl Pts',(28.947416319256,3.80996623292663,61.1105886151822));
#132082=CARTESIAN_POINT('Ctrl Pts',(28.8951800522402,4.06504503431329,61.0943945426028));
#132083=CARTESIAN_POINT('Ctrl Pts',(28.8378053277324,4.31884238976034,61.0769648279692));
#132084=CARTESIAN_POINT('Ctrl Pts',(28.7753516804205,4.57122651109775,61.0585372022695));
#132085=CARTESIAN_POINT('Ctrl Pts',(28.7146812543561,4.81640438032536,61.0406357353308));
#132086=CARTESIAN_POINT('Ctrl Pts',(28.6492175358221,5.06024900272142,61.0217927282713));
#132087=CARTESIAN_POINT('Ctrl Pts',(28.5789805654299,5.30260498783434,61.0022306465424));
#132088=CARTESIAN_POINT('Ctrl Pts',(28.5507781664335,5.39991869816618,60.9943758425689));
#132089=CARTESIAN_POINT('Ctrl Pts',(28.5218058098204,5.49699196477918,60.9864051388434));
#132090=CARTESIAN_POINT('Ctrl Pts',(28.4920633168648,5.59381284229683,60.9783330220678));
#132091=CARTESIAN_POINT('Ctrl Pts',(28.4848734235303,5.61721813596013,60.9763816840045));
#132092=CARTESIAN_POINT('Ctrl Pts',(28.4776385217535,5.64060867527659,60.9744244196547));
#132093=CARTESIAN_POINT('Ctrl Pts',(28.4703586020432,5.66398428202551,60.9724614341921));
#132094=CARTESIAN_POINT('Ctrl Pts',(28.4590031072118,5.7004464398765,60.9693994950277));
#132095=CARTESIAN_POINT('Ctrl Pts',(28.4475380803588,5.73687226648814,60.966323635946));
#132096=CARTESIAN_POINT('Ctrl Pts',(28.4359635892217,5.77326141434145,60.9632347536892));
#132097=CARTESIAN_POINT('Ctrl Pts',(28.4264661853811,5.80312038857079,60.9607001833256));
#132098=CARTESIAN_POINT('Ctrl Pts',(28.416895075509,5.83295463521824,60.9581568278517));
#132099=CARTESIAN_POINT('Ctrl Pts',(28.4072502933072,5.86276398696542,60.9556052012388));
#132100=CARTESIAN_POINT('Ctrl Pts',(28.4024279022063,5.87766866283902,60.9543293879324));
#132101=CARTESIAN_POINT('Ctrl Pts',(28.3975870929037,5.8925671149521,60.9530515069221));
#132102=CARTESIAN_POINT('Ctrl Pts',(28.3927278679136,5.90745931329707,60.9517716181211));
#132103=CARTESIAN_POINT('Ctrl Pts',(28.3902982554186,5.91490541246956,60.9511316737206));
#132104=CARTESIAN_POINT('Ctrl Pts',(28.3878640389965,5.9223499481988,60.9504912273764));
#132105=CARTESIAN_POINT('Ctrl Pts',(28.3854252189674,5.92979291706548,60.949850286783));
#132106=CARTESIAN_POINT('Ctrl Pts',(28.3829863989383,5.93723588593217,60.9492093461897));
#132107=CARTESIAN_POINT('Ctrl Pts',(28.3801780333721,5.94578638788186,60.9484722163124));
#132108=CARTESIAN_POINT('Ctrl Pts',(28.3780949483526,5.95211711963359,60.947925989957));
#132109=CARTESIAN_POINT('Ctrl Pts',(28.3048789970587,6.17462870377922,60.9287273101853));
#132110=CARTESIAN_POINT('Ctrl Pts',(28.22739228315,6.39629757519428,60.9090858571923));
#132111=CARTESIAN_POINT('Ctrl Pts',(28.145553301647,6.61699125281535,60.8891871897609));
#132112=CARTESIAN_POINT('Ctrl Pts',(28.0652757589614,6.83347422706881,60.8696681770023));
#132113=CARTESIAN_POINT('Ctrl Pts',(27.9808100487485,7.04901915966549,60.8499020459908));
#132114=CARTESIAN_POINT('Ctrl Pts',(27.8920624579535,7.26345498945963,60.8300597329815));
#132115=CARTESIAN_POINT('Ctrl Pts',(27.805828513612,7.47181723620495,60.8107794246338));
#132116=CARTESIAN_POINT('Ctrl Pts',(27.7155513158858,7.67913243299848,60.7914275624999));
#132117=CARTESIAN_POINT('Ctrl Pts',(27.6211354006745,7.88519689102183,60.7721515041307));
#132118=CARTESIAN_POINT('Ctrl Pts',(27.5510318959288,8.03819906950659,60.7578390945508));
#132119=CARTESIAN_POINT('Ctrl Pts',(27.4786464523346,8.19051076703679,60.7435683264394));
#132120=CARTESIAN_POINT('Ctrl Pts',(27.4039391396142,8.3420307462116,60.7293940501294));
#132121=CARTESIAN_POINT('Ctrl Pts',(27.3367459515862,8.47831071774229,60.7166454345176));
#132122=CARTESIAN_POINT('Ctrl Pts',(27.2676743838534,8.6139500075147,60.7039748378232));
#132123=CARTESIAN_POINT('Ctrl Pts',(27.1966964811296,8.74886401607158,60.691417775478));
#132124=CARTESIAN_POINT('Ctrl Pts',(27.0948901072376,8.94237643995736,60.6734066912527));
#132125=CARTESIAN_POINT('Ctrl Pts',(26.9891610162539,9.13439839250478,60.6556304769479));
#132126=CARTESIAN_POINT('Ctrl Pts',(26.8794196045641,9.32469535356695,60.6381656550562));
#132127=CARTESIAN_POINT('Ctrl Pts',(26.7713769209198,9.51204663733419,60.6209711776253));
#132128=CARTESIAN_POINT('Ctrl Pts',(26.6594445193728,9.69772559687088,60.6040787935889));
#132129=CARTESIAN_POINT('Ctrl Pts',(26.5435554204452,9.88147066671254,60.5875343807167));
#132130=CARTESIAN_POINT('Ctrl Pts',(26.4299980517524,10.0615187198477,60.5713228473653));
#132131=CARTESIAN_POINT('Ctrl Pts',(26.312641021048,10.2397094160614,60.5554455552208));
#132132=CARTESIAN_POINT('Ctrl Pts',(26.1914483184166,10.4157662665093,60.5399165005658));
#132133=CARTESIAN_POINT('Ctrl Pts',(26.1484304803057,10.4782583549474,60.534404400046));
#132134=CARTESIAN_POINT('Ctrl Pts',(26.1049296699126,10.5404813492215,60.5289358943947));
#132135=CARTESIAN_POINT('Ctrl Pts',(26.0609453277637,10.6024221432137,60.5235106658849));
#132136=CARTESIAN_POINT('Ctrl Pts',(38.8135870908017,3.00384513004725E-5,
64.3914459355285));
#132137=CARTESIAN_POINT('Ctrl Pts',(38.8135820972561,0.192706244171883,
64.3914481968697));
#132138=CARTESIAN_POINT('Ctrl Pts',(38.8134083063988,0.387806629527274,
64.3935322941669));
#132139=CARTESIAN_POINT('Ctrl Pts',(38.8127385775239,0.585429506725301,
64.397923885268));
#132140=CARTESIAN_POINT('Ctrl Pts',(38.8121085403539,0.771340198272692,
64.4020552072595));
#132141=CARTESIAN_POINT('Ctrl Pts',(38.8110390230174,0.95948224467097,64.408229225816));
#132142=CARTESIAN_POINT('Ctrl Pts',(38.8093095217539,1.14994410220109,64.416628624266));
#132143=CARTESIAN_POINT('Ctrl Pts',(38.8086870405138,1.21849503983687,64.4196517316051));
#132144=CARTESIAN_POINT('Ctrl Pts',(38.8079791123787,1.2873467781357,64.4229634783117));
#132145=CARTESIAN_POINT('Ctrl Pts',(38.8071756217047,1.35650461339875,64.4265736374001));
#132146=CARTESIAN_POINT('Ctrl Pts',(38.8069873798435,1.37270691673054,64.4274194257681));
#132147=CARTESIAN_POINT('Ctrl Pts',(38.806793893207,1.38892602418888,64.4282815961541));
#132148=CARTESIAN_POINT('Ctrl Pts',(38.8065950324194,1.40516201022104,64.4291602798004));
#132149=CARTESIAN_POINT('Ctrl Pts',(38.8043449063288,1.58887352128373,64.4391026571894));
#132150=CARTESIAN_POINT('Ctrl Pts',(38.8014063278112,1.77474311766781,64.4511567002304));
#132151=CARTESIAN_POINT('Ctrl Pts',(38.7976161790703,1.96281884870537,64.4654920541126));
#132152=CARTESIAN_POINT('Ctrl Pts',(38.795522242117,2.06672472421815,64.4734118824058));
#132153=CARTESIAN_POINT('Ctrl Pts',(38.7931684751674,2.17130455486487,64.4820285567688));
#132154=CARTESIAN_POINT('Ctrl Pts',(38.7905278800185,2.27657201409169,64.4913748701255));
#132155=CARTESIAN_POINT('Ctrl Pts',(38.789267029482,2.32683588452887,64.4958376156603));
#132156=CARTESIAN_POINT('Ctrl Pts',(38.7879407867535,2.37725660874965,64.500466763006));
#132157=CARTESIAN_POINT('Ctrl Pts',(38.7865471193559,2.4278337674776,64.5052652859232));
#132158=CARTESIAN_POINT('Ctrl Pts',(38.7848700453846,2.48869594778754,64.51103960331));
#132159=CARTESIAN_POINT('Ctrl Pts',(38.7830953359685,2.54978464605298,64.517059179869));
#132160=CARTESIAN_POINT('Ctrl Pts',(38.781219494281,2.61109939041232,64.5233294322324));
#132161=CARTESIAN_POINT('Ctrl Pts',(38.7802815734372,2.64175676259198,64.5264645584142));
#132162=CARTESIAN_POINT('Ctrl Pts',(38.7793183701495,2.67247064594839,64.5296623570849));
#132163=CARTESIAN_POINT('Ctrl Pts',(38.7783294509264,2.7032410152705,64.5329235298439));
#132164=CARTESIAN_POINT('Ctrl Pts',(38.7778349913149,2.71862619993155,64.5345541162234));
#132165=CARTESIAN_POINT('Ctrl Pts',(38.7773341027581,2.7340255060635,64.536200546343));
#132166=CARTESIAN_POINT('Ctrl Pts',(38.7768267312168,2.74943893151487,64.5378629093229));
#132167=CARTESIAN_POINT('Ctrl Pts',(38.7765730454461,2.75714564424056,64.5386940908129));
#132168=CARTESIAN_POINT('Ctrl Pts',(38.7763177389317,2.76485588679473,64.5395292555312));
#132169=CARTESIAN_POINT('Ctrl Pts',(38.776060804929,2.77256965903347,64.5403684147119));
#132170=CARTESIAN_POINT('Ctrl Pts',(38.7758038709264,2.78028343127222,64.5412075738926));
#132171=CARTESIAN_POINT('Ctrl Pts',(38.7754963970519,2.7894521186308,64.5422099791408));
#132172=CARTESIAN_POINT('Ctrl Pts',(38.7752851137195,2.79572156469527,64.5428978869322));
#132173=CARTESIAN_POINT('Ctrl Pts',(38.7710886572831,2.92024372642544,64.5565609385614));
#132174=CARTESIAN_POINT('Ctrl Pts',(38.7665003779421,3.05057812754349,64.5717655398374));
#132175=CARTESIAN_POINT('Ctrl Pts',(38.7610604810182,3.18673981322833,64.5888571002793));
#132176=CARTESIAN_POINT('Ctrl Pts',(38.7549253313141,3.34030381220565,64.6081330688239));
#132177=CARTESIAN_POINT('Ctrl Pts',(38.7477065709253,3.50128046984096,64.6298086462359));
#132178=CARTESIAN_POINT('Ctrl Pts',(38.738733342239,3.66967113078567,64.654417207798));
#132179=CARTESIAN_POINT('Ctrl Pts',(38.7309997754733,3.81479842717775,64.6756260681205));
#132180=CARTESIAN_POINT('Ctrl Pts',(38.7219625628368,3.96543251726767,64.6990143256146));
#132181=CARTESIAN_POINT('Ctrl Pts',(38.711181534982,4.12156833073821,64.7249519486975));
#132182=CARTESIAN_POINT('Ctrl Pts',(38.6993179051263,4.29338288526685,64.7534941585625));
#132183=CARTESIAN_POINT('Ctrl Pts',(38.6853434491788,4.4718616116839,64.7851231239542));
#132184=CARTESIAN_POINT('Ctrl Pts',(38.6686427422749,4.65694578221642,64.8203651711238));
#132185=CARTESIAN_POINT('Ctrl Pts',(38.6566479590734,4.78987695167738,64.8456767173838));
#132186=CARTESIAN_POINT('Ctrl Pts',(38.643246518751,4.92621491879245,64.8728528240778));
#132187=CARTESIAN_POINT('Ctrl Pts',(38.6282032124862,5.0659271041141,64.9020988916168));
#132188=CARTESIAN_POINT('Ctrl Pts',(38.6144690008673,5.19348129234847,64.9287999155496));
#132189=CARTESIAN_POINT('Ctrl Pts',(38.5993665687579,5.32384849862264,64.9572264447523));
#132190=CARTESIAN_POINT('Ctrl Pts',(38.5826941727004,5.45698250875477,64.987540669278));
#132191=CARTESIAN_POINT('Ctrl Pts',(38.5731193768813,5.53344008325061,65.0049498352579));
#132192=CARTESIAN_POINT('Ctrl Pts',(38.563026619093,5.61080991664418,65.0229816761299));
#132193=CARTESIAN_POINT('Ctrl Pts',(38.5523761053502,5.6890808590101,65.0416675976743));
#132194=CARTESIAN_POINT('Ctrl Pts',(38.5470508484787,5.72821633019306,65.0510105584466));
#132195=CARTESIAN_POINT('Ctrl Pts',(38.5415861542849,5.76757707657575,65.0605170488365));
#132196=CARTESIAN_POINT('Ctrl Pts',(38.5359769028551,5.80716148728286,65.0701910325787));
#132197=CARTESIAN_POINT('Ctrl Pts',(38.5331722771402,5.82695369263642,65.0750280244498));
#132198=CARTESIAN_POINT('Ctrl Pts',(38.5303315122135,5.84680181395491,65.0799068902103));
#132199=CARTESIAN_POINT('Ctrl Pts',(38.5274539635382,5.86670564209971,65.0848281279772));
#132200=CARTESIAN_POINT('Ctrl Pts',(38.5260151892006,5.87665755617211,65.0872887468607));
#132201=CARTESIAN_POINT('Ctrl Pts',(38.5245672189318,5.88662339694342,65.0897599587801));
#132202=CARTESIAN_POINT('Ctrl Pts',(38.5231099716393,5.89660313747531,65.0922418261374));
#132203=CARTESIAN_POINT('Ctrl Pts',(38.5218348802584,5.90533541044071,65.094413460075));
#132204=CARTESIAN_POINT('Ctrl Pts',(38.5205526861564,5.91407832540984,65.0965932520843));
#132205=CARTESIAN_POINT('Ctrl Pts',(38.5192633348198,5.92283186404408,65.0987812440293));
#132206=CARTESIAN_POINT('Ctrl Pts',(38.5190791417718,5.92408236956326,65.0990938143072));
#132207=CARTESIAN_POINT('Ctrl Pts',(38.5187288748741,5.92645819778244,65.0996879815923));
#132208=CARTESIAN_POINT('Ctrl Pts',(38.518710317313,5.92658403096877,65.0997194570216));
#132209=CARTESIAN_POINT('Ctrl Pts',(38.5176144759863,5.93401459820143,65.101578110536));
#132210=CARTESIAN_POINT('Ctrl Pts',(38.515667100619,5.94740709121132,65.1049243388498));
#132211=CARTESIAN_POINT('Ctrl Pts',(38.5128218551399,5.96675695826927,65.1097938036597));
#132212=CARTESIAN_POINT('Ctrl Pts',(38.5112591083899,5.97738484330801,65.1124683497972));
#132213=CARTESIAN_POINT('Ctrl Pts',(38.5094247736796,5.98980984107125,65.1156029740003));
#132214=CARTESIAN_POINT('Ctrl Pts',(38.5073058910958,6.00403060254209,65.1192076456793));
#132215=CARTESIAN_POINT('Ctrl Pts',(38.5034388974516,6.0299837132257,65.1257862275123));
#132216=CARTESIAN_POINT('Ctrl Pts',(38.4986265569299,6.06191828979016,65.133928546497));
#132217=CARTESIAN_POINT('Ctrl Pts',(38.4927581848926,6.09982199600826,65.1437197725091));
#132218=CARTESIAN_POINT('Ctrl Pts',(38.4868802194934,6.13778766557277,65.1535270047958));
#132219=CARTESIAN_POINT('Ctrl Pts',(38.4799427498706,6.18174212272886,65.1649885645098));
#132220=CARTESIAN_POINT('Ctrl Pts',(38.4717934127655,6.23166615807523,65.1782216012355));
#132221=CARTESIAN_POINT('Ctrl Pts',(38.4636310427066,6.28167003521022,65.1914758011006));
#132222=CARTESIAN_POINT('Ctrl Pts',(38.4542529101786,6.3376627778107,65.2065071918731));
#132223=CARTESIAN_POINT('Ctrl Pts',(38.4434649420875,6.3996159803555,65.2234646158817));
#132224=CARTESIAN_POINT('Ctrl Pts',(38.4326805962475,6.46154838101719,65.2404163461353));
#132225=CARTESIAN_POINT('Ctrl Pts',(38.4204873439494,6.5294374749201,65.259292893285));
#132226=CARTESIAN_POINT('Ctrl Pts',(38.4066506692628,6.60324270730986,65.2802731239176));
#132227=CARTESIAN_POINT('Ctrl Pts',(38.39286939175,6.67675244953393,65.3011693570933));
#132228=CARTESIAN_POINT('Ctrl Pts',(38.3774578062107,6.75613134498252,65.3241525857494));
#132229=CARTESIAN_POINT('Ctrl Pts',(38.3601442014692,6.84132331852189,65.349427957903));
#132230=CARTESIAN_POINT('Ctrl Pts',(38.3547333605568,6.86794748042917,65.357327007221));
#132231=CARTESIAN_POINT('Ctrl Pts',(38.349136458325,6.89513926088066,65.3654501285514));
#132232=CARTESIAN_POINT('Ctrl Pts',(38.3433443968407,6.92289654971471,65.3738041241803));
#132233=CARTESIAN_POINT('Ctrl Pts',(38.3302782335287,6.98551350742247,65.3926496891818));
#132234=CARTESIAN_POINT('Ctrl Pts',(38.316219613751,7.05100866780108,65.4126697325342));
#132235=CARTESIAN_POINT('Ctrl Pts',(38.3010560936442,7.11935545607374,65.4339474345147));
#132236=CARTESIAN_POINT('Ctrl Pts',(38.2894153604296,7.17182392795556,65.4502819037164));
#132237=CARTESIAN_POINT('Ctrl Pts',(38.2771232685237,7.225972869957,65.4673576902076));
#132238=CARTESIAN_POINT('Ctrl Pts',(38.2641246953319,7.28178792485946,65.48521493203));
#132239=CARTESIAN_POINT('Ctrl Pts',(38.2576254087359,7.30969545231069,65.4941435529412));
#132240=CARTESIAN_POINT('Ctrl Pts',(38.2509495069607,7.33801949982202,65.5032675668473));
#132241=CARTESIAN_POINT('Ctrl Pts',(38.2440896730612,7.3667580259864,65.512592188913));
#132242=CARTESIAN_POINT('Ctrl Pts',(38.2406597561114,7.38112728906859,65.5172544999459));
#132243=CARTESIAN_POINT('Ctrl Pts',(38.2371838564442,7.39560017132269,65.5219669647981));
#132244=CARTESIAN_POINT('Ctrl Pts',(38.2336610480672,7.41017640708869,65.5267302462064));
#132245=CARTESIAN_POINT('Ctrl Pts',(38.2318996438786,7.41746452497169,65.5291118869106));
#132246=CARTESIAN_POINT('Ctrl Pts',(38.230126512532,7.42477848120126,65.5315062318641));
#132247=CARTESIAN_POINT('Ctrl Pts',(38.2283415368226,7.43211824162908,65.5339133646321));
#132248=CARTESIAN_POINT('Ctrl Pts',(38.2274490489679,7.43578812184299,65.535116931016));
#132249=CARTESIAN_POINT('Ctrl Pts',(38.2265536000237,7.43946445310452,65.5363236943605));
#132250=CARTESIAN_POINT('Ctrl Pts',(38.2256551752428,7.44314723108138,65.5375336651556));
#132251=CARTESIAN_POINT('Ctrl Pts',(38.2247567504619,7.44683000905825,65.5387436359507));
#132252=CARTESIAN_POINT('Ctrl Pts',(38.2235147663237,7.45191098024706,65.5404148952795));
#132253=CARTESIAN_POINT('Ctrl Pts',(38.2229509586165,7.4542149008017,65.5411732104112));
#132254=CARTESIAN_POINT('Ctrl Pts',(38.1916849363716,7.58197908420835,65.5832256645933));
#132255=CARTESIAN_POINT('Ctrl Pts',(38.1596549613227,7.70530747405823,65.6251569615781));
#132256=CARTESIAN_POINT('Ctrl Pts',(38.1271540676055,7.82421379407133,65.666726707534));
#132257=CARTESIAN_POINT('Ctrl Pts',(38.087141251882,7.9706028968584,65.7179044566469));
#132258=CARTESIAN_POINT('Ctrl Pts',(38.0464155863636,8.11028986157072,65.7685331157816));
#132259=CARTESIAN_POINT('Ctrl Pts',(38.0054821089969,8.24334003244639,65.8182073193746));
#132260=CARTESIAN_POINT('Ctrl Pts',(37.9645486316303,8.37639020332206,65.8678815229677));
#132261=CARTESIAN_POINT('Ctrl Pts',(37.9234072600134,8.50280361865002,65.9166012267983));
#132262=CARTESIAN_POINT('Ctrl Pts',(37.8825226040607,8.62265784585839,65.9640032148954));
#132263=CARTESIAN_POINT('Ctrl Pts',(37.8720105022222,8.65347429307648,65.9761910275263));
#132264=CARTESIAN_POINT('Ctrl Pts',(37.8615151664394,8.6838571813318,65.9882919458989));
#132265=CARTESIAN_POINT('Ctrl Pts',(37.8510440635881,8.71380795371077,66.0003002512402));
#132266=CARTESIAN_POINT('Ctrl Pts',(37.8424268442424,8.7384560140752,66.0101825150824));
#132267=CARTESIAN_POINT('Ctrl Pts',(37.8338260325903,8.7628114254635,66.0200020601993));
#132268=CARTESIAN_POINT('Ctrl Pts',(37.8252456323684,8.78687508443175,66.0297558031867));
#132269=CARTESIAN_POINT('Ctrl Pts',(37.8157422509733,8.813527236199,66.0405587421222));
#132270=CARTESIAN_POINT('Ctrl Pts',(37.8062639679525,8.83982145500476,66.051280935983));
#132271=CARTESIAN_POINT('Ctrl Pts',(37.7968160555023,8.86575901704537,66.061918341461));
#132272=CARTESIAN_POINT('Ctrl Pts',(37.7920920992772,8.87872779806568,66.0672370442));
#132273=CARTESIAN_POINT('Ctrl Pts',(37.7873757359399,8.89160741441799,66.0725345512341));
#132274=CARTESIAN_POINT('Ctrl Pts',(37.7826676268362,8.90439801829518,66.0778103637185));
#132275=CARTESIAN_POINT('Ctrl Pts',(37.7803135722843,8.91079332023378,66.0804482699607));
#132276=CARTESIAN_POINT('Ctrl Pts',(37.7779615813058,8.91716636902401,66.0830807526508));
#132277=CARTESIAN_POINT('Ctrl Pts',(37.7756117355492,8.92351718410612,66.0857077503478));
#132278=CARTESIAN_POINT('Ctrl Pts',(37.7732618897927,8.92986799918824,66.0883347480448));
#132279=CARTESIAN_POINT('Ctrl Pts',(37.7716146995104,8.93431309154039,66.0901749639149));
#132280=CARTESIAN_POINT('Ctrl Pts',(37.7685687154191,8.94250294763226,66.0935722274305));
#132281=CARTESIAN_POINT('Ctrl Pts',(37.6865595247574,9.16300425348457,66.1850391632491));
#132282=CARTESIAN_POINT('Ctrl Pts',(37.5981393895329,9.38096554045745,66.2799356242712));
#132283=CARTESIAN_POINT('Ctrl Pts',(37.5032569308291,9.5959827456451,66.377974791091));
#132284=CARTESIAN_POINT('Ctrl Pts',(37.4097025963978,9.80799023151144,66.4746416473817));
#132285=CARTESIAN_POINT('Ctrl Pts',(37.3098648312833,10.0171347851144,66.5743637156262));
#132286=CARTESIAN_POINT('Ctrl Pts',(37.2037041734696,10.2230579005808,66.6768286946188));
#132287=CARTESIAN_POINT('Ctrl Pts',(37.1603529916719,10.3071475303811,66.7186707293582));
#132288=CARTESIAN_POINT('Ctrl Pts',(37.1159475219664,10.3906995226895,66.760969733924));
#132289=CARTESIAN_POINT('Ctrl Pts',(37.0704854132497,10.4736876985386,66.8037027644647));
#132290=CARTESIAN_POINT('Ctrl Pts',(36.9539219146008,10.6864669205439,66.9132689875966));
#132291=CARTESIAN_POINT('Ctrl Pts',(36.8304107459624,10.8955419080915,67.0256912169882));
#132292=CARTESIAN_POINT('Ctrl Pts',(36.6999028887975,11.1005327456061,67.140552801349));
#132293=CARTESIAN_POINT('Ctrl Pts',(36.646808624253,11.1839287800875,67.1872817223393));
#132294=CARTESIAN_POINT('Ctrl Pts',(36.5925565519594,11.2666484735295,67.2344139344862));
#132295=CARTESIAN_POINT('Ctrl Pts',(36.5371442385606,11.3486648066635,67.2819196312367));
#132296=CARTESIAN_POINT('Ctrl Pts',(36.4166606394213,11.5269938169157,67.3852117873128));
#132297=CARTESIAN_POINT('Ctrl Pts',(36.2906906955439,11.7019983860824,67.4902710991956));
#132298=CARTESIAN_POINT('Ctrl Pts',(36.1592882551018,11.8733756711545,67.5967554170151));
#132299=CARTESIAN_POINT('Ctrl Pts',(29.9859214083691,12.46437431082,79.070188223874));
#132300=CARTESIAN_POINT('Ctrl Pts',(29.8857014163891,12.47044857532,79.090205232738));
#132301=CARTESIAN_POINT('Ctrl Pts',(29.6104280963791,12.4897806276,79.145015827581));
#132302=CARTESIAN_POINT('Ctrl Pts',(29.1457827926491,12.5346015555,79.236730680776));
#132303=CARTESIAN_POINT('Ctrl Pts',(28.5738695769491,12.60957457799,79.348292639236));
#132304=CARTESIAN_POINT('Ctrl Pts',(28.0282967728591,12.70185657079,79.453349622617));
#132305=CARTESIAN_POINT('Ctrl Pts',(27.6733467087591,12.77424630289,79.52093552273));
#132306=CARTESIAN_POINT('Ctrl Pts',(27.5249257075591,12.80670959195,79.549068580612));
#132307=CARTESIAN_POINT('Ctrl Pts',(30.0308651063291,13.45208857236,79.385705808435));
#132308=CARTESIAN_POINT('Ctrl Pts',(29.9359068375091,13.45982740229,79.399762458128));
#132309=CARTESIAN_POINT('Ctrl Pts',(29.6751805090291,13.4834545797,79.438192693413));
#132310=CARTESIAN_POINT('Ctrl Pts',(29.2355716482891,13.53421738821,79.502277776235));
#132311=CARTESIAN_POINT('Ctrl Pts',(28.6953648245591,13.61430233658,79.580029006533));
#132312=CARTESIAN_POINT('Ctrl Pts',(28.1810574803591,13.70908983217,79.653211426916));
#132313=CARTESIAN_POINT('Ctrl Pts',(27.8470766860091,13.78168016274,79.700369027776));
#132314=CARTESIAN_POINT('Ctrl Pts',(27.7075360699391,13.81397234352,79.720024504347));
#132315=CARTESIAN_POINT('Ctrl Pts',(29.9227251759491,14.31914031007,78.82563632132));
#132316=CARTESIAN_POINT('Ctrl Pts',(29.8324306026191,14.32407596873,78.834452846557));
#132317=CARTESIAN_POINT('Ctrl Pts',(29.5843934297591,14.33979311782,78.858607745173));
#132318=CARTESIAN_POINT('Ctrl Pts',(29.1656884915291,14.3762918562,78.899185618871));
#132319=CARTESIAN_POINT('Ctrl Pts',(28.6504842183591,14.4374986971,78.9490683359909));
#132320=CARTESIAN_POINT('Ctrl Pts',(28.1593784162991,14.51307015343,78.996867416962));
#132321=CARTESIAN_POINT('Ctrl Pts',(27.8401641858791,14.57254123544,79.028243803073));
#132322=CARTESIAN_POINT('Ctrl Pts',(27.7067467992491,14.59925012658,79.041431119251));
#132323=CARTESIAN_POINT('Ctrl Pts',(29.7422836619591,14.41782971493,77.8083595247319));
#132324=CARTESIAN_POINT('Ctrl Pts',(29.6525709105191,14.41758847387,77.816570606694));
#132325=CARTESIAN_POINT('Ctrl Pts',(29.4058860801291,14.41909934329,77.839219068241));
#132326=CARTESIAN_POINT('Ctrl Pts',(28.9883370206291,14.43178352124,77.877972508984));
#132327=CARTESIAN_POINT('Ctrl Pts',(28.4727542006591,14.46422443239,77.926747098128));
#132328=CARTESIAN_POINT('Ctrl Pts',(27.9794541455991,14.51321295826,77.974615773832));
#132329=CARTESIAN_POINT('Ctrl Pts',(27.6577729429091,14.55604520736,78.006646818456));
#132330=CARTESIAN_POINT('Ctrl Pts',(27.5231474917591,14.57592942316,78.020207201693));
#132331=CARTESIAN_POINT('Origin',(29.5680409582791,12.92381928297,77.694240492923));
#132332=CARTESIAN_POINT('Origin',(34.5835698427891,12.92381190166,76.809867428062));
#132333=CARTESIAN_POINT('Ctrl Pts',(33.859212171956,12.923698620032,78.460731142598));
#132334=CARTESIAN_POINT('Ctrl Pts',(33.8592330215353,12.9682330973519,78.4607308814309));
#132335=CARTESIAN_POINT('Ctrl Pts',(33.8589027995551,13.0134405826951,78.458775094831));
#132336=CARTESIAN_POINT('Ctrl Pts',(33.858195831669,13.0590476424942,78.4547074451838));
#132337=CARTESIAN_POINT('Ctrl Pts',(33.8574929818102,13.1043890450873,78.4506634892464));
#132338=CARTESIAN_POINT('Ctrl Pts',(33.8564177039448,13.1501248925192,78.4445318705706));
#132339=CARTESIAN_POINT('Ctrl Pts',(33.8549525564639,13.1959615089143,78.4362031281502));
#132340=CARTESIAN_POINT('Ctrl Pts',(33.8534967317702,13.2415064652354,78.4279273818239));
#132341=CARTESIAN_POINT('Ctrl Pts',(33.8516559441973,13.2871503581839,78.4174821624424));
#132342=CARTESIAN_POINT('Ctrl Pts',(33.8494215183369,13.3325881208068,78.4048079246059));
#132343=CARTESIAN_POINT('Ctrl Pts',(33.8485692243438,13.3499197910253,78.3999734939964));
#132344=CARTESIAN_POINT('Ctrl Pts',(33.8476597488197,13.3672213377937,78.3948152677034));
#132345=CARTESIAN_POINT('Ctrl Pts',(33.8466929517904,13.3844754437921,78.3893318777936));
#132346=CARTESIAN_POINT('Ctrl Pts',(33.8442933552275,13.4273002479616,78.3757220680998));
#132347=CARTESIAN_POINT('Ctrl Pts',(33.8415402198523,13.4698282902136,78.360106775778));
#132348=CARTESIAN_POINT('Ctrl Pts',(33.8384375007938,13.5117692111429,78.342508579162));
#132349=CARTESIAN_POINT('Ctrl Pts',(33.835341716617,13.553616389997,78.3249497162428));
#132350=CARTESIAN_POINT('Ctrl Pts',(33.8318979241246,13.5948784493562,78.3054168847981));
#132351=CARTESIAN_POINT('Ctrl Pts',(33.8281189268964,13.6352754672863,78.283982844231));
#132352=CARTESIAN_POINT('Ctrl Pts',(33.8243454303277,13.6756136838386,78.2625800027767));
#132353=CARTESIAN_POINT('Ctrl Pts',(33.8202377395313,13.7150887785906,78.2392816835676));
#132354=CARTESIAN_POINT('Ctrl Pts',(33.8158170891901,13.753439665697,78.2142084605291));
#132355=CARTESIAN_POINT('Ctrl Pts',(33.8131665113712,13.7764344747988,78.1991748062687));
#132356=CARTESIAN_POINT('Ctrl Pts',(33.810403583591,13.7990255042493,78.1835039757881));
#132357=CARTESIAN_POINT('Ctrl Pts',(33.8075342494431,13.821160836655,78.1672297083637));
#132358=CARTESIAN_POINT('Ctrl Pts',(33.8027477314033,13.8580861867245,78.1400815720378));
#132359=CARTESIAN_POINT('Ctrl Pts',(33.7976655387112,13.8937354478372,78.1112566664626));
#132360=CARTESIAN_POINT('Ctrl Pts',(33.7923212707233,13.9278946034537,78.0809456828264));
#132361=CARTESIAN_POINT('Ctrl Pts',(33.7869735948705,13.9620755412472,78.0506153708668));
#132362=CARTESIAN_POINT('Ctrl Pts',(33.7813635916826,13.9947640491257,78.0187975517465));
#132363=CARTESIAN_POINT('Ctrl Pts',(33.7755310657962,14.0257841675171,77.9857181088134));
#132364=CARTESIAN_POINT('Ctrl Pts',(33.7696813509459,14.0568957049104,77.9525411778689));
#132365=CARTESIAN_POINT('Ctrl Pts',(33.7636078935501,14.0863286700283,77.9180957071712));
#132366=CARTESIAN_POINT('Ctrl Pts',(33.7573557026574,14.1139499662343,77.8826370969955));
#132367=CARTESIAN_POINT('Ctrl Pts',(33.753619333804,14.1304567160449,77.8614466936765));
#132368=CARTESIAN_POINT('Ctrl Pts',(33.7498192191244,14.1463173315367,77.8398949514358));
#132369=CARTESIAN_POINT('Ctrl Pts',(33.7459655687823,14.1615115822075,77.8180398051419));
#132370=CARTESIAN_POINT('Ctrl Pts',(33.7391493068818,14.1883868777734,77.7793828467295));
#132371=CARTESIAN_POINT('Ctrl Pts',(33.7321663331587,14.2131715935981,77.7397810915173));
#132372=CARTESIAN_POINT('Ctrl Pts',(33.725070623432,14.2358167896528,77.6995388812372));
#132373=CARTESIAN_POINT('Ctrl Pts',(33.7179458023146,14.2585548915865,77.6591315702484));
#132374=CARTESIAN_POINT('Ctrl Pts',(33.7107074246475,14.2791359137209,77.6180791416206));
#132375=CARTESIAN_POINT('Ctrl Pts',(33.7034103001888,14.2975630174627,77.5766906447098));
#132376=CARTESIAN_POINT('Ctrl Pts',(33.6960537060775,14.3161402972723,77.5349648423925));
#132377=CARTESIAN_POINT('Ctrl Pts',(33.6886375073168,14.3325285302607,77.4928980591992));
#132378=CARTESIAN_POINT('Ctrl Pts',(33.6812164409681,14.3467833059797,77.4507988880263));
#132379=CARTESIAN_POINT('Ctrl Pts',(33.6784238764152,14.3521474112864,77.4349568718525));
#132380=CARTESIAN_POINT('Ctrl Pts',(33.6756306002789,14.3572099280516,77.4191101428676));
#132381=CARTESIAN_POINT('Ctrl Pts',(33.67283943295,14.3619756402683,77.4032745984495));
#132382=CARTESIAN_POINT('Origin',(33.9027788805691,-12.77732087006,79.976189078581));
#132383=CARTESIAN_POINT('',(35.3799890432589,11.6378875163018,79.715708490352));
#132384=CARTESIAN_POINT('Origin',(33.9027998622653,11.6379092722801,79.9761546590259));
#132385=CARTESIAN_POINT('',(35.3799958958808,-11.6378856606036,79.7157076007637));
#132386=CARTESIAN_POINT('',(35.3799907980991,-11.63788566034,79.715708499663));
#132387=CARTESIAN_POINT('Ctrl Pts',(35.3799880137154,-11.6378856588156,
79.7157026548483));
#132388=CARTESIAN_POINT('Ctrl Pts',(35.3695520560716,-11.6378709771185,
79.6565207146777));
#132389=CARTESIAN_POINT('Ctrl Pts',(35.3555553115347,-11.6378607889906,
79.5979668413592));
#132390=CARTESIAN_POINT('Ctrl Pts',(35.3380986507356,-11.637853719103,79.5404630667693));
#132391=CARTESIAN_POINT('Ctrl Pts',(35.3206441808791,-11.6378466501027,
79.4829665093374));
#132392=CARTESIAN_POINT('Ctrl Pts',(35.2997307855574,-11.63784269856,79.4265201864714));
#132393=CARTESIAN_POINT('Ctrl Pts',(35.2755091568529,-11.6378404896635,
79.3715308374448));
#132394=CARTESIAN_POINT('Ctrl Pts',(35.2512868264982,-11.637838280703,79.3165398954914));
#132395=CARTESIAN_POINT('Ctrl Pts',(35.2237562392352,-11.6378378144897,
79.2630063941493));
#132396=CARTESIAN_POINT('Ctrl Pts',(35.1931157868798,-11.6378377160928,
79.2113161033672));
#132397=CARTESIAN_POINT('Ctrl Pts',(35.1849189661822,-11.63783768977,79.1974881076041));
#132398=CARTESIAN_POINT('Ctrl Pts',(35.176499843879,-11.63783768977,79.1837918872206));
#132399=CARTESIAN_POINT('Ctrl Pts',(35.1678627706239,-11.63783768977,79.1702345196114));
#132400=CARTESIAN_POINT('Ctrl Pts',(35.1355720633058,-11.63783768977,79.1195487170784));
#132401=CARTESIAN_POINT('Ctrl Pts',(35.1002317032601,-11.63783768977,79.0708060227495));
#132402=CARTESIAN_POINT('Ctrl Pts',(35.0620964188945,-11.63783768977,79.024357767197));
#132403=CARTESIAN_POINT('Ctrl Pts',(35.0239637323516,-11.63783768977,78.977912675757));
#132404=CARTESIAN_POINT('Ctrl Pts',(34.9830367677872,-11.63783768977,78.9337620329779));
#132405=CARTESIAN_POINT('Ctrl Pts',(34.9396104809761,-11.63783768977,78.8922240273005));
#132406=CARTESIAN_POINT('Ctrl Pts',(34.8961866618653,-11.63783768977,78.8506883820219));
#132407=CARTESIAN_POINT('Ctrl Pts',(34.8502641066618,-11.63783768977,78.8117653652228));
#132408=CARTESIAN_POINT('Ctrl Pts',(34.8021737362379,-11.63783768977,78.7757354586537));
#132409=CARTESIAN_POINT('Ctrl Pts',(34.7540753816382,-11.63783768977,78.7396995702404));
#132410=CARTESIAN_POINT('Ctrl Pts',(34.7038088254441,-11.63783768977,78.7065580044565));
#132411=CARTESIAN_POINT('Ctrl Pts',(34.651736411703,-11.63783768977,78.6765496606816));
#132412=CARTESIAN_POINT('Ctrl Pts',(34.5996711332875,-11.63783768977,78.6465454288595));
#132413=CARTESIAN_POINT('Ctrl Pts',(34.5458008546994,-11.63783768977,78.6196737679673));
#132414=CARTESIAN_POINT('Ctrl Pts',(34.4905137910617,-11.63783768977,78.5961283281108));
#132415=CARTESIAN_POINT('Ctrl Pts',(34.4352229874562,-11.63783768977,78.5725812954914));
#132416=CARTESIAN_POINT('Ctrl Pts',(34.3785155912039,-11.63783768977,78.5523610981484));
#132417=CARTESIAN_POINT('Ctrl Pts',(34.3208003182326,-11.63783768977,78.535613472216));
#132418=CARTESIAN_POINT('Ctrl Pts',(34.2899453102775,-11.63783768977,78.5266600686408));
#132419=CARTESIAN_POINT('Ctrl Pts',(34.2588025590782,-11.63783768977,78.5186983117861));
#132420=CARTESIAN_POINT('Ctrl Pts',(34.2274363156242,-11.63783768977,78.5117446276497));
#132421=CARTESIAN_POINT('Ctrl Pts',(34.1687709160204,-11.63783768977,78.4987389051386));
#132422=CARTESIAN_POINT('Ctrl Pts',(34.1093232084526,-11.63783768977,78.4892626423694));
#132423=CARTESIAN_POINT('Ctrl Pts',(34.0495216251489,-11.6378376897611,
78.4833841459414));
#132424=CARTESIAN_POINT('Ctrl Pts',(33.9897275200442,-11.6378376897522,
78.4775063846205));
#132425=CARTESIAN_POINT('Ctrl Pts',(33.9295800437199,-11.6378376897345,
78.4752255297055));
#132426=CARTESIAN_POINT('Ctrl Pts',(33.8695125657921,-11.6378376896989,
78.4765580065166));
#132427=CARTESIAN_POINT('Ctrl Pts',(33.8094432159812,-11.6378376896634,
78.4778905248516));
#132428=CARTESIAN_POINT('Ctrl Pts',(33.7494542873367,-11.6378376896101,
78.4828365910624));
#132429=CARTESIAN_POINT('Ctrl Pts',(33.6899780297751,-11.6378376895301,
78.4913605369974));
#132430=CARTESIAN_POINT('Ctrl Pts',(33.6740480624911,-11.6378376895087,
78.4936435686716));
#132431=CARTESIAN_POINT('Ctrl Pts',(33.6581548467044,-11.6378376894854,
78.4961829780519));
#132432=CARTESIAN_POINT('Ctrl Pts',(33.6423066140169,-11.63783768946,78.4989774490718));
#132433=CARTESIAN_POINT('Ctrl Pts',(36.4624006913807,-13.6175309807164,
78.8714913648239));
#132434=CARTESIAN_POINT('Ctrl Pts',(36.4624006913807,-13.6175309807164,
78.8714913648239));
#132435=CARTESIAN_POINT('Ctrl Pts',(36.4624006913807,-13.6175309807164,
78.8714913648239));
#132436=CARTESIAN_POINT('Ctrl Pts',(36.4624006913807,-13.6175309807164,
78.8714913648239));
#132437=CARTESIAN_POINT('Ctrl Pts',(36.4624006913807,-13.6175309807164,
78.8714913648239));
#132438=CARTESIAN_POINT('Ctrl Pts',(36.4624006913807,-13.6175309807164,
78.8714913648239));
#132439=CARTESIAN_POINT('Ctrl Pts',(36.4624006913807,-13.6175309807164,
78.8714913648239));
#132440=CARTESIAN_POINT('Ctrl Pts',(36.4624006913807,-13.6175309807164,
78.8714913648239));
#132441=CARTESIAN_POINT('Ctrl Pts',(36.4624006913807,-13.6175309807164,
78.8714913648239));
#132442=CARTESIAN_POINT('Ctrl Pts',(36.5087707847954,-13.6295464641391,
78.8593182230073));
#132443=CARTESIAN_POINT('Ctrl Pts',(36.5147533430926,-13.621753782623,78.8765850066188));
#132444=CARTESIAN_POINT('Ctrl Pts',(36.5128106723893,-13.6240150405474,
78.8715208625787));
#132445=CARTESIAN_POINT('Ctrl Pts',(36.5203475397483,-13.605877824589,78.9100485185392));
#132446=CARTESIAN_POINT('Ctrl Pts',(36.5241109898786,-13.5968212093523,
78.9292868711512));
#132447=CARTESIAN_POINT('Ctrl Pts',(36.5278744400088,-13.5877645941156,
78.9485252237633));
#132448=CARTESIAN_POINT('Ctrl Pts',(36.539056905061,-13.5608543708176,79.0056887833431));
#132449=CARTESIAN_POINT('Ctrl Pts',(36.5502393701132,-13.5339441475196,
79.062852342923));
#132450=CARTESIAN_POINT('Ctrl Pts',(36.5614218351653,-13.5070339242215,
79.1200159025029));
#132451=CARTESIAN_POINT('Ctrl Pts',(36.554898911248,-13.6392407963244,78.8462285202114));
#132452=CARTESIAN_POINT('Ctrl Pts',(36.5644326177738,-13.6265498978342,
78.8733225560771));
#132453=CARTESIAN_POINT('Ctrl Pts',(36.5607337607929,-13.6312719831418,
78.8635158637679));
#132454=CARTESIAN_POINT('Ctrl Pts',(36.5755647018899,-13.598691414449,78.9332013525492));
#132455=CARTESIAN_POINT('Ctrl Pts',(36.5829703658806,-13.5824226731206,
78.9679980192992));
#132456=CARTESIAN_POINT('Ctrl Pts',(36.5903760298713,-13.5661539317922,
79.0027946860492));
#132457=CARTESIAN_POINT('Ctrl Pts',(36.6123807265986,-13.5178140773893,
79.1061871839961));
#132458=CARTESIAN_POINT('Ctrl Pts',(36.6343854233258,-13.4694742229864,
79.2095796819431));
#132459=CARTESIAN_POINT('Ctrl Pts',(36.6563901200531,-13.4211343685835,
79.31297217989));
#132460=CARTESIAN_POINT('Ctrl Pts',(36.646046826565,-13.6541488424738,78.8185742721227));
#132461=CARTESIAN_POINT('Ctrl Pts',(36.6560492376511,-13.6408860043036,
78.8469292136561));
#132462=CARTESIAN_POINT('Ctrl Pts',(36.6516381391679,-13.6466133680293,
78.8348889376155));
#132463=CARTESIAN_POINT('Ctrl Pts',(36.6698272747732,-13.6089261693074,
78.9158412543503));
#132464=CARTESIAN_POINT('Ctrl Pts',(36.678909815503,-13.590107489585,78.9562638851925));
#132465=CARTESIAN_POINT('Ctrl Pts',(36.6879923562327,-13.5712888098627,
78.9966865160346));
#132466=CARTESIAN_POINT('Ctrl Pts',(36.7149796128139,-13.5153722383551,
79.1167956289673));
#132467=CARTESIAN_POINT('Ctrl Pts',(36.7419668693951,-13.4594556668474,
79.2369047419));
#132468=CARTESIAN_POINT('Ctrl Pts',(36.7689541259764,-13.4035390953398,
79.3570138548327));
#132469=CARTESIAN_POINT('Ctrl Pts',(36.6910658924978,-13.6593662375177,
78.8040117096523));
#132470=CARTESIAN_POINT('Ctrl Pts',(36.6980086982724,-13.6500749817604,
78.8236273955465));
#132471=CARTESIAN_POINT('Ctrl Pts',(36.6946216542961,-13.6545438906777,
78.8142013835284));
#132472=CARTESIAN_POINT('Ctrl Pts',(36.7088642892985,-13.6262319890973,
78.8752406196854));
#132473=CARTESIAN_POINT('Ctrl Pts',(36.7159761892433,-13.6120947587846,
78.9057198772234));
#132474=CARTESIAN_POINT('Ctrl Pts',(36.7230880891881,-13.5979575284719,
78.9361991347614));
#132475=CARTESIAN_POINT('Ctrl Pts',(36.7442199149957,-13.5559511039319,
79.0267631705372));
#132476=CARTESIAN_POINT('Ctrl Pts',(36.7653517408033,-13.5139446793919,
79.1173272063129));
#132477=CARTESIAN_POINT('Ctrl Pts',(36.7864835666109,-13.4719382548519,
79.2078912420887));
#132478=CARTESIAN_POINT('Ctrl Pts',(36.735264603282,-13.662485738696,78.7888968893297));
#132479=CARTESIAN_POINT('Ctrl Pts',(36.735264603282,-13.662485738696,78.7888968893297));
#132480=CARTESIAN_POINT('Ctrl Pts',(36.735264603282,-13.662485738696,78.7888968893297));
#132481=CARTESIAN_POINT('Ctrl Pts',(36.735264603282,-13.662485738696,78.7888968893297));
#132482=CARTESIAN_POINT('Ctrl Pts',(36.735264603282,-13.662485738696,78.7888968893297));
#132483=CARTESIAN_POINT('Ctrl Pts',(36.735264603282,-13.662485738696,78.7888968893297));
#132484=CARTESIAN_POINT('Ctrl Pts',(36.735264603282,-13.662485738696,78.7888968893297));
#132485=CARTESIAN_POINT('Ctrl Pts',(36.735264603282,-13.662485738696,78.7888968893297));
#132486=CARTESIAN_POINT('Ctrl Pts',(36.735264603282,-13.662485738696,78.7888968893297));
#132487=CARTESIAN_POINT('',(36.4640508930212,-13.6179550204625,78.87106300086));
#132488=CARTESIAN_POINT('Origin',(36.6259767577074,-12.2926480245168,78.1865226505801));
#132489=CARTESIAN_POINT('',(36.646332255877,-13.6311708400759,78.8663936093756));
#132490=CARTESIAN_POINT('Ctrl Pts',(36.4640508930212,-13.6179550204625,
78.87106300086));
#132491=CARTESIAN_POINT('Ctrl Pts',(36.4641834917382,-13.6179473140954,
78.8711126536229));
#132492=CARTESIAN_POINT('Ctrl Pts',(36.4644911975365,-13.6179838279465,
78.8711182044604));
#132493=CARTESIAN_POINT('Ctrl Pts',(36.4649737737274,-13.6180415198724,
78.871125291467));
#132494=CARTESIAN_POINT('Ctrl Pts',(36.4655876503714,-13.6181149087518,
78.871134306723));
#132495=CARTESIAN_POINT('Ctrl Pts',(36.4664838602382,-13.6182233599688,
78.8711440605703));
#132496=CARTESIAN_POINT('Ctrl Pts',(36.4676360949594,-13.6183510738823,
78.8711764188561));
#132497=CARTESIAN_POINT('Ctrl Pts',(36.4690935083757,-13.6185126138598,
78.8712173474958));
#132498=CARTESIAN_POINT('Ctrl Pts',(36.4709596083455,-13.6187054886973,
78.8712931103674));
#132499=CARTESIAN_POINT('Ctrl Pts',(36.4731615799429,-13.6189260841508,
78.871383593139));
#132500=CARTESIAN_POINT('Ctrl Pts',(36.4745159257299,-13.6190617637042,
78.8714392455193));
#132501=CARTESIAN_POINT('Ctrl Pts',(36.4759971252191,-13.6192083478747,
78.8714995350199));
#132502=CARTESIAN_POINT('Ctrl Pts',(36.4775866615851,-13.6193689971118,
78.8715511966506));
#132503=CARTESIAN_POINT('Ctrl Pts',(36.481498301009,-13.6197643337036,78.8716783291124));
#132504=CARTESIAN_POINT('Ctrl Pts',(36.4860955308366,-13.6201950577805,
78.8718621100866));
#132505=CARTESIAN_POINT('Ctrl Pts',(36.4913605508575,-13.6206584093813,
78.872062869958));
#132506=CARTESIAN_POINT('Ctrl Pts',(36.4944173529083,-13.6209274252859,
78.8721794285245));
#132507=CARTESIAN_POINT('Ctrl Pts',(36.498427044011,-13.6212734725104,78.872318854442));
#132508=CARTESIAN_POINT('Ctrl Pts',(36.5021159668906,-13.6215799022322,
78.8724371945187));
#132509=CARTESIAN_POINT('Ctrl Pts',(36.5047808256736,-13.6218012654762,
78.8725226827773));
#132510=CARTESIAN_POINT('Ctrl Pts',(36.5072783975182,-13.6220034758983,
78.8725962439108));
#132511=CARTESIAN_POINT('Ctrl Pts',(36.5091329606862,-13.6221552057529,
78.8726410581783));
#132512=CARTESIAN_POINT('Ctrl Pts',(36.5113438638537,-13.6223360893281,
78.8726944831614));
#132513=CARTESIAN_POINT('Ctrl Pts',(36.513894066682,-13.6225288354596,78.8727781102579));
#132514=CARTESIAN_POINT('Ctrl Pts',(36.5167833448577,-13.6227214582233,
78.8729055097517));
#132515=CARTESIAN_POINT('Ctrl Pts',(36.5184740378156,-13.6228341735557,
78.8729800589692));
#132516=CARTESIAN_POINT('Ctrl Pts',(36.5197239075041,-13.6229146600396,
78.8730370241672));
#132517=CARTESIAN_POINT('Ctrl Pts',(36.5215109915733,-13.623017746904,78.8731367032908));
#132518=CARTESIAN_POINT('Ctrl Pts',(36.5227779114705,-13.6230908284125,
78.873207368945));
#132519=CARTESIAN_POINT('Ctrl Pts',(36.5243147509991,-13.6231754392616,
78.8732990990183));
#132520=CARTESIAN_POINT('Ctrl Pts',(36.5264694745122,-13.6232799356834,
78.8734448705763));
#132521=CARTESIAN_POINT('Ctrl Pts',(36.5316635946536,-13.6235318320244,
78.8737962636813));
#132522=CARTESIAN_POINT('Ctrl Pts',(36.5359073745668,-13.6236836049445,
78.8741393503315));
#132523=CARTESIAN_POINT('Ctrl Pts',(36.5392037712793,-13.6237853428906,
78.8744231137472));
#132524=CARTESIAN_POINT('Ctrl Pts',(36.5411147015973,-13.6238443206602,
78.8745876121863));
#132525=CARTESIAN_POINT('Ctrl Pts',(36.541964118272,-13.6238622908226,78.8746733276918));
#132526=CARTESIAN_POINT('Ctrl Pts',(36.5430437731837,-13.6238905992486,
78.87477082179));
#132527=CARTESIAN_POINT('Ctrl Pts',(36.5438265466757,-13.6239111234784,
78.8748415071497));
#132528=CARTESIAN_POINT('Ctrl Pts',(36.5447303543849,-13.6239366598944,
78.8749188999794));
#132529=CARTESIAN_POINT('Ctrl Pts',(36.5462476870491,-13.6239763351117,
78.8750492221757));
#132530=CARTESIAN_POINT('Ctrl Pts',(36.5525034608565,-13.6241399110965,
78.8755865243777));
#132531=CARTESIAN_POINT('Ctrl Pts',(36.5592164190559,-13.6243250047039,
78.8760561426797));
#132532=CARTESIAN_POINT('Ctrl Pts',(36.5659768361521,-13.6245795260801,
78.8762820986765));
#132533=CARTESIAN_POINT('Ctrl Pts',(36.5713532118987,-13.6247819400044,
78.8764617953317));
#132534=CARTESIAN_POINT('Ctrl Pts',(36.576758741326,-13.6250305635944,78.8764832172777));
#132535=CARTESIAN_POINT('Ctrl Pts',(36.5819898328604,-13.6253560057479,
78.8762639167306));
#132536=CARTESIAN_POINT('Ctrl Pts',(36.585364772629,-13.6255659710408,78.8761224307457));
#132537=CARTESIAN_POINT('Ctrl Pts',(36.5886671911254,-13.6258079351807,
78.8758810768004));
#132538=CARTESIAN_POINT('Ctrl Pts',(36.5918452765511,-13.6260865301216,
78.8755292468544));
#132539=CARTESIAN_POINT('Ctrl Pts',(36.5987888095358,-13.6266952089023,
78.8747605630377));
#132540=CARTESIAN_POINT('Ctrl Pts',(36.6053277000037,-13.6272886118807,
78.8738825820606));
#132541=CARTESIAN_POINT('Ctrl Pts',(36.6114802495672,-13.6278560793253,
78.8729530400328));
#132542=CARTESIAN_POINT('Ctrl Pts',(36.6176999701247,-13.628429742145,78.8720133496492));
#132543=CARTESIAN_POINT('Ctrl Pts',(36.6235248914239,-13.6289742806592,
78.8710195194918));
#132544=CARTESIAN_POINT('Ctrl Pts',(36.6289738469251,-13.6294787066028,
78.8700292146934));
#132545=CARTESIAN_POINT('Ctrl Pts',(36.7432179278938,-13.636198950746,78.846992041912));
#132546=CARTESIAN_POINT('Ctrl Pts',(36.7108115055979,-13.6358752288811,
78.8531074637301));
#132547=CARTESIAN_POINT('Ctrl Pts',(36.6784828947467,-13.6342021234484,
78.8595796977137));
#132548=CARTESIAN_POINT('Ctrl Pts',(36.646332255877,-13.6311708400759,78.8663936093756));
#132549=CARTESIAN_POINT('Ctrl Pts',(36.0413541965395,-13.5385524084063,
78.8219185637222));
#132550=CARTESIAN_POINT('Ctrl Pts',(36.0443390692377,-13.5362121365262,
78.8266178467828));
#132551=CARTESIAN_POINT('Ctrl Pts',(36.0545148270121,-13.5280801594399,
78.8429498748798));
#132552=CARTESIAN_POINT('Ctrl Pts',(36.0694283772597,-13.5152701077307,
78.8686972121326));
#132553=CARTESIAN_POINT('Ctrl Pts',(36.0839605510938,-13.5014873949538,
78.8964610094424));
#132554=CARTESIAN_POINT('Ctrl Pts',(36.0945588044003,-13.4901669739601,
78.9192863632301));
#132555=CARTESIAN_POINT('Ctrl Pts',(36.1008211011128,-13.4824751555828,
78.9346626965391));
#132556=CARTESIAN_POINT('Ctrl Pts',(36.1030740999561,-13.4787635377289,
78.9421913259183));
#132557=CARTESIAN_POINT('Ctrl Pts',(36.1031818402804,-13.4783683893573,
78.9428310903551));
#132558=CARTESIAN_POINT('Ctrl Pts',(36.0764411019647,-13.5628769378654,
78.8083910122847));
#132559=CARTESIAN_POINT('Ctrl Pts',(36.0795496624071,-13.5604610111995,
78.8132750854961));
#132560=CARTESIAN_POINT('Ctrl Pts',(36.0901598135502,-13.5520573333247,
78.8302669905896));
#132561=CARTESIAN_POINT('Ctrl Pts',(36.1057882041297,-13.5387628136805,
78.8571683985934));
#132562=CARTESIAN_POINT('Ctrl Pts',(36.1211176864259,-13.5243725536988,
78.8863481172406));
#132563=CARTESIAN_POINT('Ctrl Pts',(36.1324763252156,-13.5124084261907,
78.9106408618895));
#132564=CARTESIAN_POINT('Ctrl Pts',(36.1394869313789,-13.5039781844258,
78.9276665689722));
#132565=CARTESIAN_POINT('Ctrl Pts',(36.1421967665385,-13.4997783128599,
78.9362679756959));
#132566=CARTESIAN_POINT('Ctrl Pts',(36.1425452691223,-13.4990816441658,
78.9375681334444));
#132567=CARTESIAN_POINT('Ctrl Pts',(36.1120453547769,-13.5856109486442,
78.7937519683683));
#132568=CARTESIAN_POINT('Ctrl Pts',(36.1152797484648,-13.5831184353831,
78.7988231638101));
#132569=CARTESIAN_POINT('Ctrl Pts',(36.1263318291934,-13.5744396714938,
78.8164833502305));
#132570=CARTESIAN_POINT('Ctrl Pts',(36.1426874700359,-13.5606544072964,
78.8445540039736));
#132571=CARTESIAN_POINT('Ctrl Pts',(36.1588280835953,-13.545648404286,78.8751689131062));
#132572=CARTESIAN_POINT('Ctrl Pts',(36.1709603469915,-13.5330314196273,
78.9009499735806));
#132573=CARTESIAN_POINT('Ctrl Pts',(36.178732400364,-13.5238515041513,78.9196501725559));
#132574=CARTESIAN_POINT('Ctrl Pts',(36.1819071181667,-13.5191557445104,
78.9293410910961));
#132575=CARTESIAN_POINT('Ctrl Pts',(36.1825006715159,-13.5181525710206,
78.9313125421451));
#132576=CARTESIAN_POINT('Ctrl Pts',(36.1480898606898,-13.6067252227425,
78.7780424920219));
#132577=CARTESIAN_POINT('Ctrl Pts',(36.1514519573532,-13.6041553550248,
78.783302740626));
#132578=CARTESIAN_POINT('Ctrl Pts',(36.1629525353573,-13.5951987091683,
78.8016381792719));
#132579=CARTESIAN_POINT('Ctrl Pts',(36.1800462424778,-13.580917477517,78.8308907408642));
#132580=CARTESIAN_POINT('Ctrl Pts',(36.1970100325351,-13.5652888611044,
78.8629570185049));
#132581=CARTESIAN_POINT('Ctrl Pts',(36.2099274637118,-13.552011278801,78.8902441044039));
#132582=CARTESIAN_POINT('Ctrl Pts',(36.2184724316828,-13.5420720662877,
78.9106402793977));
#132583=CARTESIAN_POINT('Ctrl Pts',(36.2221190583888,-13.5368738624281,
78.9214350756853));
#132584=CARTESIAN_POINT('Ctrl Pts',(36.2229614128174,-13.5355598688766,
78.9240872545302));
#132585=CARTESIAN_POINT('',(36.1480898606898,-13.6067252227425,78.7780424920219));
#132586=CARTESIAN_POINT('',(36.1887546648804,-13.5728292529327,78.847489288857));
#132587=CARTESIAN_POINT('Origin',(36.1118745043311,-13.5960811534144,78.8009259388539));
#132588=CARTESIAN_POINT('',(36.0446752548501,-13.5408399095576,78.8206418568075));
#132589=CARTESIAN_POINT('Origin',(36.5006306047883,-12.3981418696704,77.9625345273951));
#132590=CARTESIAN_POINT('Ctrl Pts',(36.0446774732356,-13.5408384751336,
78.8206449445472));
#132591=CARTESIAN_POINT('Ctrl Pts',(36.0916850857421,-13.5518449805492,
78.8309651869554));
#132592=CARTESIAN_POINT('Ctrl Pts',(36.1397079808775,-13.562648531607,78.8400689323397));
#132593=CARTESIAN_POINT('Ctrl Pts',(36.1887545950258,-13.5728294813495,
78.8474894372116));
#132594=CARTESIAN_POINT('Ctrl Pts',(36.1480898606898,-13.6067252227425,
78.7780424920219));
#132595=CARTESIAN_POINT('Ctrl Pts',(36.1514519573532,-13.6041553550248,
78.783302740626));
#132596=CARTESIAN_POINT('Ctrl Pts',(36.1629525353573,-13.5951987091683,
78.8016381792719));
#132597=CARTESIAN_POINT('Ctrl Pts',(36.1800462424778,-13.580917477517,78.8308907408642));
#132598=CARTESIAN_POINT('Ctrl Pts',(36.1970100325351,-13.5652888611044,
78.8629570185049));
#132599=CARTESIAN_POINT('Ctrl Pts',(36.2099274637118,-13.552011278801,78.8902441044039));
#132600=CARTESIAN_POINT('Ctrl Pts',(36.2184724316828,-13.5420720662877,
78.9106402793977));
#132601=CARTESIAN_POINT('Ctrl Pts',(36.2221190583888,-13.5368738624281,
78.9214350756853));
#132602=CARTESIAN_POINT('Ctrl Pts',(36.2229614128174,-13.5355598688766,
78.9240872545302));
#132603=CARTESIAN_POINT('Ctrl Pts',(36.2992619131484,-13.6952793052796,
78.712156340383));
#132604=CARTESIAN_POINT('Ctrl Pts',(36.3031596010323,-13.692385009978,78.7182094852644));
#132605=CARTESIAN_POINT('Ctrl Pts',(36.3165411939635,-13.6822629163989,
78.7393769578717));
#132606=CARTESIAN_POINT('Ctrl Pts',(36.3367303796114,-13.6659015780555,
78.7735864867146));
#132607=CARTESIAN_POINT('Ctrl Pts',(36.357146603752,-13.6476616969434,78.8117398600354));
#132608=CARTESIAN_POINT('Ctrl Pts',(36.3733570589803,-13.6316135425576,
78.8453432748377));
#132609=CARTESIAN_POINT('Ctrl Pts',(36.3851436606838,-13.6184898088911,
78.8728524388754));
#132610=CARTESIAN_POINT('Ctrl Pts',(36.3907694915897,-13.611184334537,78.8882769411472));
#132611=CARTESIAN_POINT('Ctrl Pts',(36.3926553273718,-13.6085667496204,
78.8937841187074));
#132612=CARTESIAN_POINT('Ctrl Pts',(36.4537997192532,-13.7531348275884,
78.6295167031115));
#132613=CARTESIAN_POINT('Ctrl Pts',(36.4582503159403,-13.7499119605313,
78.6363738171947));
#132614=CARTESIAN_POINT('Ctrl Pts',(36.4735737634649,-13.7386088786915,
78.6604141624838));
#132615=CARTESIAN_POINT('Ctrl Pts',(36.4969586862089,-13.7201356487196,
78.6996601572554));
#132616=CARTESIAN_POINT('Ctrl Pts',(36.5209388506112,-13.6992391416549,
78.7440091958987));
#132617=CARTESIAN_POINT('Ctrl Pts',(36.5405496289052,-13.6803644397312,
78.784057646114));
#132618=CARTESIAN_POINT('Ctrl Pts',(36.555685304629,-13.6639792082828,78.8188515496762));
#132619=CARTESIAN_POINT('Ctrl Pts',(36.5633563690056,-13.6545122521614,
78.8390241994241));
#132620=CARTESIAN_POINT('Ctrl Pts',(36.5663212970924,-13.6505530241725,
78.8474694278411));
#132621=CARTESIAN_POINT('Ctrl Pts',(36.6061800233323,-13.7808703344089,
78.5343153943199));
#132622=CARTESIAN_POINT('Ctrl Pts',(36.6111806483402,-13.7773262453333,
78.5419593493064));
#132623=CARTESIAN_POINT('Ctrl Pts',(36.6284358515173,-13.7648680007667,
78.5688125275726));
#132624=CARTESIAN_POINT('Ctrl Pts',(36.6550000141886,-13.7443253975173,
78.6129969813538));
#132625=CARTESIAN_POINT('Ctrl Pts',(36.6825254422131,-13.7208208173866,
78.6634310023575));
#132626=CARTESIAN_POINT('Ctrl Pts',(36.7055195608249,-13.6991641521518,
78.7098238115797));
#132627=CARTESIAN_POINT('Ctrl Pts',(36.7239891966374,-13.6795575058957,
78.7518127609135));
#132628=CARTESIAN_POINT('Ctrl Pts',(36.7336966470516,-13.6679526999726,
78.7766810540519));
#132629=CARTESIAN_POINT('Ctrl Pts',(36.7377367084417,-13.6626624594582,
78.7880407996123));
#132630=CARTESIAN_POINT('Ctrl Pts',(36.1887545950258,-13.5728294813495,
78.8474894372116));
#132631=CARTESIAN_POINT('Ctrl Pts',(36.2103531003999,-13.5773124084669,
78.8507555351564));
#132632=CARTESIAN_POINT('Ctrl Pts',(36.2333779264413,-13.5820188593518,
78.8537513247424));
#132633=CARTESIAN_POINT('Ctrl Pts',(36.2700715262227,-13.5890837908734,
78.8578224956519));
#132634=CARTESIAN_POINT('Ctrl Pts',(36.2826588017725,-13.5914430098648,
78.8591009144093));
#132635=CARTESIAN_POINT('Ctrl Pts',(36.3020645457527,-13.594948564419,78.8608867383133));
#132636=CARTESIAN_POINT('Ctrl Pts',(36.3086204007986,-13.5961116785867,
78.8614596409308));
#132637=CARTESIAN_POINT('Ctrl Pts',(36.3219066323604,-13.5984171078203,
78.8625653497166));
#132638=CARTESIAN_POINT('Ctrl Pts',(36.3302025631481,-13.5998173492539,
78.8632181139596));
#132639=CARTESIAN_POINT('Ctrl Pts',(36.3774837518109,-13.607618724868,78.8668175026506));
#132640=CARTESIAN_POINT('Ctrl Pts',(36.4205818929086,-13.6132479681494,
78.8698470622943));
#132641=CARTESIAN_POINT('Ctrl Pts',(36.4640390336471,-13.6179681794182,
78.8710264250399));
#132642=CARTESIAN_POINT('Origin',(36.500517881468,-12.3982157262051,77.9623752096788));
#132643=CARTESIAN_POINT('Ctrl Pts',(33.8458695692469,-12.9128498070933,
78.4631124071519));
#132644=CARTESIAN_POINT('Ctrl Pts',(33.8804362530074,-12.9129747103335,
78.4567626655418));
#132645=CARTESIAN_POINT('Ctrl Pts',(33.9826122819526,-12.9119078622902,
78.4409210188779));
#132646=CARTESIAN_POINT('Ctrl Pts',(34.1471526591361,-12.9034887777877,
78.4290883853484));
#132647=CARTESIAN_POINT('Ctrl Pts',(34.3311801082618,-12.8847575734329,
78.4347345631763));
#132648=CARTESIAN_POINT('Ctrl Pts',(34.4943806698859,-12.8605115333373,
78.4549675889316));
#132649=CARTESIAN_POINT('Ctrl Pts',(34.6376087672186,-12.8328563598802,
78.4851552568926));
#132650=CARTESIAN_POINT('Ctrl Pts',(34.7622094291334,-12.8033920014129,
78.5216784145264));
#132651=CARTESIAN_POINT('Ctrl Pts',(34.8698019746813,-12.7733116204556,
78.5617757514179));
#132652=CARTESIAN_POINT('Ctrl Pts',(34.9620805957375,-12.7434939376387,
78.6033721543705));
#132653=CARTESIAN_POINT('Ctrl Pts',(35.0406096689484,-12.7145884065802,
78.6448937820371));
#132654=CARTESIAN_POINT('Ctrl Pts',(35.1067871905256,-12.6871002078555,
78.6851310414152));
#132655=CARTESIAN_POINT('Ctrl Pts',(35.1618042910709,-12.6614673796507,
78.7230847384953));
#132656=CARTESIAN_POINT('Ctrl Pts',(35.2067591673776,-12.638064763268,78.7579355717776));
#132657=CARTESIAN_POINT('Ctrl Pts',(35.2427975912993,-12.6171473317229,
78.7891118095416));
#132658=CARTESIAN_POINT('Ctrl Pts',(35.2711482263803,-12.5988148329409,
78.8163469814348));
#132659=CARTESIAN_POINT('Ctrl Pts',(35.2924658755658,-12.5832772605048,
78.8390556915725));
#132660=CARTESIAN_POINT('Ctrl Pts',(35.307594129335,-12.5706238579202,78.8569665984833));
#132661=CARTESIAN_POINT('Ctrl Pts',(35.3161484118183,-12.5620595878754,
78.868320030909));
#132662=CARTESIAN_POINT('Ctrl Pts',(35.3193543369156,-12.5580624372546,
78.8730441549028));
#132663=CARTESIAN_POINT('Ctrl Pts',(35.3202691478143,-12.5567666477221,
78.8744528479851));
#132664=CARTESIAN_POINT('Ctrl Pts',(33.8456503110567,-13.1996018417486,
78.4652773762441));
#132665=CARTESIAN_POINT('Ctrl Pts',(33.8817341482106,-13.1997300776071,
78.4586391357277));
#132666=CARTESIAN_POINT('Ctrl Pts',(33.9884075750797,-13.1986344466374,
78.442183999269));
#132667=CARTESIAN_POINT('Ctrl Pts',(34.1602613719234,-13.1899904211345,
78.4304739338996));
#132668=CARTESIAN_POINT('Ctrl Pts',(34.3526252622446,-13.1707383594976,
78.4377877021175));
#132669=CARTESIAN_POINT('Ctrl Pts',(34.5234134998431,-13.1457760760133,
78.4607551811517));
#132670=CARTESIAN_POINT('Ctrl Pts',(34.6735293868505,-13.117241205332,78.4944083592027));
#132671=CARTESIAN_POINT('Ctrl Pts',(34.8043784561376,-13.0867587194026,
78.5348810387088));
#132672=CARTESIAN_POINT('Ctrl Pts',(34.9176431493598,-13.0555426788163,
78.5792333474792));
#132673=CARTESIAN_POINT('Ctrl Pts',(35.0150809485904,-13.0244894070125,
78.6252639513317));
#132674=CARTESIAN_POINT('Ctrl Pts',(35.0983262747713,-12.9942599913201,
78.6713200250023));
#132675=CARTESIAN_POINT('Ctrl Pts',(35.1688308592319,-12.9653700241188,
78.7161364225069));
#132676=CARTESIAN_POINT('Ctrl Pts',(35.2278214704078,-12.9382698112071,
78.7586663017047));
#132677=CARTESIAN_POINT('Ctrl Pts',(35.2764170860985,-12.9133502711739,
78.798043119068));
#132678=CARTESIAN_POINT('Ctrl Pts',(35.3157809568853,-12.8908828291008,
78.8336565464687));
#132679=CARTESIAN_POINT('Ctrl Pts',(35.3471570245691,-12.8709847417339,
78.8652070156515));
#132680=CARTESIAN_POINT('Ctrl Pts',(35.3712663398007,-12.8538549257744,
78.8921474444993));
#132681=CARTESIAN_POINT('Ctrl Pts',(35.3889799319516,-12.8395820074481,
78.9142198800224));
#132682=CARTESIAN_POINT('Ctrl Pts',(35.3996646373259,-12.8295547046685,
78.9292177539998));
#132683=CARTESIAN_POINT('Ctrl Pts',(35.4041355774772,-12.8246203414302,
78.9362229220246));
#132684=CARTESIAN_POINT('Ctrl Pts',(35.4055167149387,-12.8229685286228,
78.9384907818235));
#132685=CARTESIAN_POINT('Ctrl Pts',(33.830959299843,-13.4811758603199,78.3886016868916));
#132686=CARTESIAN_POINT('Ctrl Pts',(33.8700008488003,-13.4813078297855,
78.3814104950211));
#132687=CARTESIAN_POINT('Ctrl Pts',(33.9854233930445,-13.4801797753416,
78.363681584177));
#132688=CARTESIAN_POINT('Ctrl Pts',(34.1714180492613,-13.4712835724188,
78.3515924091162));
#132689=CARTESIAN_POINT('Ctrl Pts',(34.379783168837,-13.451436218611,78.3607835554978));
#132690=CARTESIAN_POINT('Ctrl Pts',(34.5650427439325,-13.4256328239301,
78.3873046950815));
#132691=CARTESIAN_POINT('Ctrl Pts',(34.7282218355506,-13.3960332628245,
78.4256839226055));
#132692=CARTESIAN_POINT('Ctrl Pts',(34.8708633928763,-13.3642806825697,
78.471684431699));
#132693=CARTESIAN_POINT('Ctrl Pts',(34.9947868847451,-13.331606452154,78.5220980344836));
#132694=CARTESIAN_POINT('Ctrl Pts',(35.1018829476443,-13.2989233549325,
78.5745332487887));
#132695=CARTESIAN_POINT('Ctrl Pts',(35.1939288624648,-13.2669023334983,
78.6272195490899));
#132696=CARTESIAN_POINT('Ctrl Pts',(35.2724856408592,-13.2360689329893,
78.6788095232723));
#132697=CARTESIAN_POINT('Ctrl Pts',(35.3388534094284,-13.2068875266087,
78.7281857189888));
#132698=CARTESIAN_POINT('Ctrl Pts',(35.3941952422174,-13.1797704356727,
78.7744099921202));
#132699=CARTESIAN_POINT('Ctrl Pts',(35.4397110275899,-13.1550129019841,
78.8168114512847));
#132700=CARTESIAN_POINT('Ctrl Pts',(35.4766760070711,-13.1327600841396,
78.8550347205036));
#132701=CARTESIAN_POINT('Ctrl Pts',(35.5059391995938,-13.1131891801329,
78.8886010640387));
#132702=CARTESIAN_POINT('Ctrl Pts',(35.5284245683134,-13.0963864512112,
78.9172756129049));
#132703=CARTESIAN_POINT('Ctrl Pts',(35.5430419032332,-13.0840310911762,
78.938135949469));
#132704=CARTESIAN_POINT('Ctrl Pts',(35.5498485579447,-13.0775832102601,
78.9488534430825));
#132705=CARTESIAN_POINT('Ctrl Pts',(35.552090839722,-13.0753531353839,78.9525261362449));
#132706=CARTESIAN_POINT('Ctrl Pts',(33.8015018549743,-13.7317040852684,
78.231178210434));
#132707=CARTESIAN_POINT('Ctrl Pts',(33.8448367011614,-13.7318398987138,
78.2231897821826));
#132708=CARTESIAN_POINT('Ctrl Pts',(33.9729484993377,-13.7306782863685,
78.2035675708194));
#132709=CARTESIAN_POINT('Ctrl Pts',(34.1794028973399,-13.7215222815351,
78.1905757013909));
#132710=CARTESIAN_POINT('Ctrl Pts',(34.410851781839,-13.7010503656952,78.2017087925164));
#132711=CARTESIAN_POINT('Ctrl Pts',(34.6169343870141,-13.67434261052,78.2323749945655));
#132712=CARTESIAN_POINT('Ctrl Pts',(34.7988676057059,-13.6435683591641,
78.2764569312182));
#132713=CARTESIAN_POINT('Ctrl Pts',(34.9584049522099,-13.6103796896382,
78.3292431282214));
#132714=CARTESIAN_POINT('Ctrl Pts',(35.097572763067,-13.576019734666,78.3871814162859));
#132715=CARTESIAN_POINT('Ctrl Pts',(35.2184605265174,-13.5414149887607,
78.4476361863756));
#132716=CARTESIAN_POINT('Ctrl Pts',(35.3230564896596,-13.5072433877898,
78.5086867494384));
#132717=CARTESIAN_POINT('Ctrl Pts',(35.4130828699557,-13.4740390254729,
78.5688811234007));
#132718=CARTESIAN_POINT('Ctrl Pts',(35.4899484910174,-13.4422810794632,
78.6270120644502));
#132719=CARTESIAN_POINT('Ctrl Pts',(35.5548824783634,-13.412407270912,78.6820491833158));
#132720=CARTESIAN_POINT('Ctrl Pts',(35.609139363501,-13.3847427053007,78.7332420479501));
#132721=CARTESIAN_POINT('Ctrl Pts',(35.6540406849326,-13.3594694892852,
78.7801592442625));
#132722=CARTESIAN_POINT('Ctrl Pts',(35.6906205410342,-13.3367332240462,
78.8224176266727));
#132723=CARTESIAN_POINT('Ctrl Pts',(35.7198794129803,-13.3166160756286,
78.8598141138234));
#132724=CARTESIAN_POINT('Ctrl Pts',(35.7400793850874,-13.3011802483082,
78.8884757827741));
#132725=CARTESIAN_POINT('Ctrl Pts',(35.7502020927212,-13.2927142033317,
78.9041630984296));
#132726=CARTESIAN_POINT('Ctrl Pts',(35.7536670291066,-13.2897107768893,
78.9097209772309));
#132727=CARTESIAN_POINT('',(35.5596734607929,-13.4095846150427,78.6873016513911));
#132728=CARTESIAN_POINT('Ctrl Pts',(33.8182597453945,-13.731730151521,78.2281566277179));
#132729=CARTESIAN_POINT('Ctrl Pts',(33.8560618757607,-13.7317293665389,
78.221492864037));
#132730=CARTESIAN_POINT('Ctrl Pts',(33.8940274438895,-13.7313259452154,
78.2158292380679));
#132731=CARTESIAN_POINT('Ctrl Pts',(33.9320951477329,-13.7305213553383,
78.2111736280892));
#132732=CARTESIAN_POINT('Ctrl Pts',(34.0169064520391,-13.7287288039099,
78.2008013619744));
#132733=CARTESIAN_POINT('Ctrl Pts',(34.1022250961173,-13.7249450244162,
78.195432386092));
#132734=CARTESIAN_POINT('Ctrl Pts',(34.1873481686048,-13.7192029136075,
78.1950277686168));
#132735=CARTESIAN_POINT('Ctrl Pts',(34.2643490590768,-13.7140086973683,
78.1946617584977));
#132736=CARTESIAN_POINT('Ctrl Pts',(34.3411899190785,-13.7072120363153,
78.1983579365909));
#132737=CARTESIAN_POINT('Ctrl Pts',(34.417325725842,-13.6988484278996,78.206007871343));
#132738=CARTESIAN_POINT('Ctrl Pts',(34.4863484062467,-13.6912662048267,
78.2129430970136));
#132739=CARTESIAN_POINT('Ctrl Pts',(34.5547916210708,-13.6823961470003,
78.2231278161601));
#132740=CARTESIAN_POINT('Ctrl Pts',(34.6222345488869,-13.6722763786065,
78.2364239788855));
#132741=CARTESIAN_POINT('Ctrl Pts',(34.6834691079089,-13.6630881719989,
78.2484961810799));
#132742=CARTESIAN_POINT('Ctrl Pts',(34.7438790637868,-13.6528697458096,
78.2631333532651));
#132743=CARTESIAN_POINT('Ctrl Pts',(34.8031364780348,-13.6416615624858,
78.280190220379));
#132744=CARTESIAN_POINT('Ctrl Pts',(34.8570759116934,-13.6314592431896,
78.2957163408449));
#132745=CARTESIAN_POINT('Ctrl Pts',(34.9100603879659,-13.6204368442871,
78.3132473394726));
#132746=CARTESIAN_POINT('Ctrl Pts',(34.9618313520066,-13.6086372852596,
78.3326405258081));
#132747=CARTESIAN_POINT('Ctrl Pts',(35.0090686726923,-13.597871027299,78.3503354283277));
#132748=CARTESIAN_POINT('Ctrl Pts',(35.0552957124219,-13.586457763026,78.3695806512548));
#132749=CARTESIAN_POINT('Ctrl Pts',(35.1003030116186,-13.5744433217375,
78.3902385394434));
#132750=CARTESIAN_POINT('Ctrl Pts',(35.1414645456183,-13.5634554854884,
78.4091312608957));
#132751=CARTESIAN_POINT('Ctrl Pts',(35.1816058811802,-13.5519648211087,
78.429205544208));
#132752=CARTESIAN_POINT('Ctrl Pts',(35.2205439385965,-13.5400208429106,
78.4503268176181));
#132753=CARTESIAN_POINT('Ctrl Pts',(35.2562938277347,-13.52905481315,78.4697187244818));
#132754=CARTESIAN_POINT('Ctrl Pts',(35.2910294158456,-13.5177066633672,
78.4899931896598));
#132755=CARTESIAN_POINT('Ctrl Pts',(35.3245957725461,-13.5060284012021,
78.5110211295801));
#132756=CARTESIAN_POINT('Ctrl Pts',(35.3555447859984,-13.4952607538203,
78.5304094117601));
#132757=CARTESIAN_POINT('Ctrl Pts',(35.3854998010571,-13.484212468085,78.550438245226));
#132758=CARTESIAN_POINT('Ctrl Pts',(35.4143262731496,-13.4729390883247,
78.5709802880509));
#132759=CARTESIAN_POINT('Ctrl Pts',(35.4408701611854,-13.4625583754445,
78.5898957378159));
#132760=CARTESIAN_POINT('Ctrl Pts',(35.4664571544482,-13.4519868047037,
78.609246339248));
#132761=CARTESIAN_POINT('Ctrl Pts',(35.490971220126,-13.4412831820079,78.628905712652));
#132762=CARTESIAN_POINT('Ctrl Pts',(35.5134775053156,-13.4314562202905,
78.6469549204128));
#132763=CARTESIAN_POINT('Ctrl Pts',(35.5350794179883,-13.4215179517519,
78.6652643926028));
#132764=CARTESIAN_POINT('Ctrl Pts',(35.5556775566379,-13.4115300417887,
78.6837080606934));
#132765=CARTESIAN_POINT('Ctrl Pts',(35.5570141769009,-13.4108819228946,
78.6849048766248));
#132766=CARTESIAN_POINT('Ctrl Pts',(35.5583465680834,-13.4102335959948,
78.6861022557473));
#132767=CARTESIAN_POINT('Ctrl Pts',(35.5596745636201,-13.4095851513792,
78.687300028573));
#132768=CARTESIAN_POINT('Ctrl Pts',(33.8591397922934,-12.9236390706349,
78.4607429230119));
#132769=CARTESIAN_POINT('Ctrl Pts',(33.908472676192,-12.9380113427995,78.4520416150425));
#132770=CARTESIAN_POINT('Ctrl Pts',(33.9580236612373,-12.9521633117262,
78.4451171978411));
#132771=CARTESIAN_POINT('Ctrl Pts',(34.007638426583,-12.9661715905133,78.4398814384144));
#132772=CARTESIAN_POINT('Ctrl Pts',(34.0578196552616,-12.9803398050822,
78.4345859011027));
#132773=CARTESIAN_POINT('Ctrl Pts',(34.1080659159905,-12.9943612810097,
78.4310169990531));
#132774=CARTESIAN_POINT('Ctrl Pts',(34.1582623969643,-13.0082990936994,
78.4290584575211));
#132775=CARTESIAN_POINT('Ctrl Pts',(34.2095192959217,-13.0225313474922,
78.4270585411233));
#132776=CARTESIAN_POINT('Ctrl Pts',(34.2607242534686,-13.0366766097167,
78.4267369299929));
#132777=CARTESIAN_POINT('Ctrl Pts',(34.311803574672,-13.0507813956557,78.4279563167816));
#132778=CARTESIAN_POINT('Ctrl Pts',(34.333416528815,-13.0567494877233,78.4284722702071));
#132779=CARTESIAN_POINT('Ctrl Pts',(34.3550075773263,-13.0627100626087,
78.4292640252931));
#132780=CARTESIAN_POINT('Ctrl Pts',(34.3765736336232,-13.068665420362,78.4303210013202));
#132781=CARTESIAN_POINT('Ctrl Pts',(34.42801194318,-13.0828698502967,78.4328420491804));
#132782=CARTESIAN_POINT('Ctrl Pts',(34.4792917621374,-13.0970587752727,
78.4368698844851));
#132783=CARTESIAN_POINT('Ctrl Pts',(34.5303722969248,-13.1112753418308,
78.4422469157871));
#132784=CARTESIAN_POINT('Ctrl Pts',(34.564595068784,-13.1208001112164,78.445849401867));
#132785=CARTESIAN_POINT('Ctrl Pts',(34.5987293951249,-13.130336803972,78.4500572985107));
#132786=CARTESIAN_POINT('Ctrl Pts',(34.6327744137633,-13.1398920509902,
78.4548228733457));
#132787=CARTESIAN_POINT('Ctrl Pts',(34.6752045342199,-13.151800703069,78.4607621831884));
#132788=CARTESIAN_POINT('Ctrl Pts',(34.7174946114257,-13.1637388489874,
78.4675673950512));
#132789=CARTESIAN_POINT('Ctrl Pts',(34.7596551910158,-13.1757108017934,
78.4751458445683));
#132790=CARTESIAN_POINT('Ctrl Pts',(34.7807354808108,-13.1816967781963,
78.4789350693268));
#132791=CARTESIAN_POINT('Ctrl Pts',(34.8017834698038,-13.1876912266013,
78.4829175192826));
#132792=CARTESIAN_POINT('Ctrl Pts',(34.822802247122,-13.1936930008152,78.4870820527824));
#132793=CARTESIAN_POINT('Ctrl Pts',(34.8333116357811,-13.1966938879222,
78.4891643195323));
#132794=CARTESIAN_POINT('Ctrl Pts',(34.8438137228632,-13.1996966050832,
78.4912921044355));
#132795=CARTESIAN_POINT('Ctrl Pts',(34.8543090003529,-13.2027008853781,
78.493464063845));
#132796=CARTESIAN_POINT('Ctrl Pts',(34.8595566390978,-13.2042030255256,
78.4945500435497));
#132797=CARTESIAN_POINT('Ctrl Pts',(34.8648025755231,-13.2057055563589,
78.4956470670043));
#132798=CARTESIAN_POINT('Ctrl Pts',(34.87004683806,-13.2072084783804,78.4967549450849));
#132799=CARTESIAN_POINT('Ctrl Pts',(34.8741979733,-13.2083981275488,78.4976318942669));
#132800=CARTESIAN_POINT('Ctrl Pts',(34.8792571988079,-13.2098505351454,
78.4987096806394));
#132801=CARTESIAN_POINT('Ctrl Pts',(34.8830654949073,-13.2109417802667,
78.4995279518091));
#132802=CARTESIAN_POINT('Ctrl Pts',(34.884068341642,-13.211229140172,78.4997434289015));
#132803=CARTESIAN_POINT('Ctrl Pts',(34.8849845050134,-13.2114916755989,
78.4999406967177));
#132804=CARTESIAN_POINT('Ctrl Pts',(34.8857746690469,-13.2117183788852,
78.5001109749738));
#132805=CARTESIAN_POINT('Ctrl Pts',(34.9100945387471,-13.2186959103221,
78.5053518424715));
#132806=CARTESIAN_POINT('Ctrl Pts',(34.9342189656613,-13.2256313637476,
78.5107893280521));
#132807=CARTESIAN_POINT('Ctrl Pts',(34.9581484132018,-13.2325305233415,
78.5163921257357));
#132808=CARTESIAN_POINT('Ctrl Pts',(35.0048895547385,-13.2460065801755,
78.5273360123043));
#132809=CARTESIAN_POINT('Ctrl Pts',(35.0508840015399,-13.2593453448709,
78.5389095306765));
#132810=CARTESIAN_POINT('Ctrl Pts',(35.0961507179162,-13.2725609978667,
78.5508925589417));
#132811=CARTESIAN_POINT('Ctrl Pts',(35.1425714629307,-13.2861135704195,
78.563181082257));
#132812=CARTESIAN_POINT('Ctrl Pts',(35.1882273720385,-13.2995368995391,
78.57589963341));
#132813=CARTESIAN_POINT('Ctrl Pts',(35.233184133054,-13.3128242107358,78.5888332034734));
#132814=CARTESIAN_POINT('Ctrl Pts',(35.2787909991607,-13.3263036654158,
78.6019538016847));
#132815=CARTESIAN_POINT('Ctrl Pts',(35.3236790285745,-13.3396432619918,
78.6152952466246));
#132816=CARTESIAN_POINT('Ctrl Pts',(35.3679537683612,-13.3528108903353,
78.628663951463));
#132817=CARTESIAN_POINT('Ctrl Pts',(35.4131923761518,-13.3662651800055,
78.6423236950948));
#132818=CARTESIAN_POINT('Ctrl Pts',(35.4577914138216,-13.3795400306877,
78.6560115792164));
#132819=CARTESIAN_POINT('Ctrl Pts',(35.5018911194648,-13.3925735054304,
78.6695589811007));
#132820=CARTESIAN_POINT('Ctrl Pts',(35.5212430944352,-13.3982928968259,
78.6755038956609));
#132821=CARTESIAN_POINT('Ctrl Pts',(35.5404992028223,-13.4039654452126,
78.6814222703796));
#132822=CARTESIAN_POINT('Ctrl Pts',(35.5596723868115,-13.4095842301505,
78.6873022747948));
#132823=CARTESIAN_POINT('Ctrl Pts',(65.1557612162105,6.92938600905312,68.809717168058));
#132824=CARTESIAN_POINT('Ctrl Pts',(65.1557223413134,6.92884377002472,68.80949676108));
#132825=CARTESIAN_POINT('Ctrl Pts',(65.1547571448173,6.91548128803838,68.8040243621952));
#132826=CARTESIAN_POINT('Ctrl Pts',(65.1532329741082,6.89796927816452,68.7953802655176));
#132827=CARTESIAN_POINT('Ctrl Pts',(65.1516150584316,6.8802663389542,68.7862046028055));
#132828=CARTESIAN_POINT('Ctrl Pts',(65.1510483078126,6.87421650353521,68.7829904020141));
#132829=CARTESIAN_POINT('Ctrl Pts',(65.149557281728,6.94310530121973,68.7748362751515));
#132830=CARTESIAN_POINT('Ctrl Pts',(65.1495311999736,6.94271782251477,68.7746863566555));
#132831=CARTESIAN_POINT('Ctrl Pts',(65.1488690708498,6.93302369305127,68.7708838930986));
#132832=CARTESIAN_POINT('Ctrl Pts',(65.1473099992198,6.91515192374951,68.7620449531505));
#132833=CARTESIAN_POINT('Ctrl Pts',(65.1457440350422,6.8980165865314,68.7531641480283));
#132834=CARTESIAN_POINT('Ctrl Pts',(65.1452003608014,6.89221246259175,68.7500807649487));
#132835=CARTESIAN_POINT('Ctrl Pts',(65.1454741812578,6.95683738476643,68.7395472040424));
#132836=CARTESIAN_POINT('Ctrl Pts',(65.1454609074645,6.95660481341836,68.7394678612072));
#132837=CARTESIAN_POINT('Ctrl Pts',(65.1451021969836,6.9505825218207,68.7373374000129));
#132838=CARTESIAN_POINT('Ctrl Pts',(65.143508191757,6.93235065627285,68.7283034343758));
#132839=CARTESIAN_POINT('Ctrl Pts',(65.1419942277171,6.91578345245396,68.7197177628987));
#132840=CARTESIAN_POINT('Ctrl Pts',(65.1414736514594,6.91022527003653,68.7167653200066));
#132841=CARTESIAN_POINT('Ctrl Pts',(65.1435571535124,6.97053667058868,68.7039615141308));
#132842=CARTESIAN_POINT('Ctrl Pts',(65.1435566600202,6.97045863939525,68.7039526001507));
#132843=CARTESIAN_POINT('Ctrl Pts',(65.1435007131574,6.96809948185238,68.7034906650766));
#132844=CARTESIAN_POINT('Ctrl Pts',(65.1418718576327,6.949508378702,68.6942621387861));
#132845=CARTESIAN_POINT('Ctrl Pts',(65.1404097697371,6.93350795357761,68.6859708972127));
#132846=CARTESIAN_POINT('Ctrl Pts',(65.1399122363857,6.9281951262389,68.6831490822834));
#132847=CARTESIAN_POINT('',(65.150886598664,6.87471515335625,68.7820772040975));
#132848=CARTESIAN_POINT('',(65.1445501446421,6.89804540344547,68.7391944229629));
#132849=CARTESIAN_POINT('Origin',(66.1356794036644,6.87480345545517,68.6083476476019));
#132850=CARTESIAN_POINT('',(65.1554607867035,6.92820316509666,68.8079865227404));
#132851=CARTESIAN_POINT('Ctrl Pts',(65.1554552753629,6.92820316432873,68.8079874964246));
#132852=CARTESIAN_POINT('Ctrl Pts',(65.1551868768224,6.92440994225428,68.8064652897237));
#132853=CARTESIAN_POINT('Ctrl Pts',(65.1548906041493,6.92041985602695,68.8047850232824));
#132854=CARTESIAN_POINT('Ctrl Pts',(65.1545659556445,6.91628081087331,68.8029438300205));
#132855=CARTESIAN_POINT('Ctrl Pts',(65.1542481880873,6.91222949306833,68.8011416609773));
#132856=CARTESIAN_POINT('Ctrl Pts',(65.1539032520095,6.90803584356044,68.799185408462));
#132857=CARTESIAN_POINT('Ctrl Pts',(65.1535310020591,6.90369367510328,68.7970742510979));
#132858=CARTESIAN_POINT('Ctrl Pts',(65.1532244215364,6.90011751807833,68.7953355276207));
#132859=CARTESIAN_POINT('Ctrl Pts',(65.1528993120918,6.89643948335413,68.7934917232776));
#132860=CARTESIAN_POINT('Ctrl Pts',(65.1525557304649,6.89262942801718,68.7915431797103));
#132861=CARTESIAN_POINT('Ctrl Pts',(65.1520411631357,6.88692327307375,68.7886249303608));
#132862=CARTESIAN_POINT('Ctrl Pts',(65.1514851293121,6.88091493848609,68.7854715795498));
#132863=CARTESIAN_POINT('Ctrl Pts',(65.1508866467258,6.87471566536353,68.7820774766692));
#132864=CARTESIAN_POINT('Ctrl Pts',(65.1554552752064,6.92820316476403,68.8079874955378));
#132865=CARTESIAN_POINT('Ctrl Pts',(65.1550749035392,6.92721170906623,68.8058321165897));
#132866=CARTESIAN_POINT('Ctrl Pts',(65.1546285636395,6.92601568182351,68.803279705676));
#132867=CARTESIAN_POINT('Ctrl Pts',(65.1541213470041,6.9246723299939,68.8003307695755));
#132868=CARTESIAN_POINT('Ctrl Pts',(65.1536487850895,6.92342076041135,68.7975833145582));
#132869=CARTESIAN_POINT('Ctrl Pts',(65.1531233821133,6.92204216782181,68.7944915961647));
#132870=CARTESIAN_POINT('Ctrl Pts',(65.1525462541141,6.92053247120318,68.7910330627761));
#132871=CARTESIAN_POINT('Ctrl Pts',(65.1519056417045,6.91885670709223,68.7871940887348));
#132872=CARTESIAN_POINT('Ctrl Pts',(65.1512008572797,6.91701668953906,68.7829008645889));
#132873=CARTESIAN_POINT('Ctrl Pts',(65.1504321489964,6.91494662720502,68.7781066343339));
#132874=CARTESIAN_POINT('Ctrl Pts',(65.1499261574398,6.91358403740928,68.7749508988198));
#132875=CARTESIAN_POINT('Ctrl Pts',(65.1493923353321,6.9121192319998,68.7715771586181));
#132876=CARTESIAN_POINT('Ctrl Pts',(65.1488334069601,6.91054665220031,68.7679845589492));
#132877=CARTESIAN_POINT('Ctrl Pts',(65.1485432048206,6.9097301503992,68.7661192392362));
#132878=CARTESIAN_POINT('Ctrl Pts',(65.1482462915086,6.90888499198604,68.7641952058584));
#132879=CARTESIAN_POINT('Ctrl Pts',(65.1479436555084,6.90801551870994,68.7622155123594));
#132880=CARTESIAN_POINT('Ctrl Pts',(65.1468755595425,6.90494687883227,68.7552285622329));
#132881=CARTESIAN_POINT('Ctrl Pts',(65.1457368023009,6.90157963766923,68.7475533689889));
#132882=CARTESIAN_POINT('Ctrl Pts',(65.1445498748409,6.89804540979059,68.7391944585906));
#132883=CARTESIAN_POINT('Ctrl Pts',(65.1399122363857,6.9281951262389,68.6831490822834));
#132884=CARTESIAN_POINT('Ctrl Pts',(65.1393493185638,6.92218410168036,68.6799564321636));
#132885=CARTESIAN_POINT('Ctrl Pts',(65.1376171252306,6.90420410579108,68.6701305745004));
#132886=CARTESIAN_POINT('Ctrl Pts',(65.1342088860127,6.87246916263756,68.6508029263816));
#132887=CARTESIAN_POINT('Ctrl Pts',(65.1292353292282,6.83210489462999,68.6225959678029));
#132888=CARTESIAN_POINT('Ctrl Pts',(65.1240218446123,6.79503133510698,68.593028962644));
#132889=CARTESIAN_POINT('Ctrl Pts',(65.1203934945133,6.77172179746152,68.5724515663476));
#132890=CARTESIAN_POINT('Ctrl Pts',(65.1189319128645,6.76267723202094,68.5641625212446));
#132891=CARTESIAN_POINT('Ctrl Pts',(65.1389667820184,6.93907607603473,68.6627940727123));
#132892=CARTESIAN_POINT('Ctrl Pts',(65.1384196505658,6.93323314077171,68.6596909139631));
#132893=CARTESIAN_POINT('Ctrl Pts',(65.1367488206894,6.91589489164434,68.650212637829));
#132894=CARTESIAN_POINT('Ctrl Pts',(65.1334525332493,6.88519445031666,68.6315201924649));
#132895=CARTESIAN_POINT('Ctrl Pts',(65.128626463115,6.84602415585857,68.6041495670674));
#132896=CARTESIAN_POINT('Ctrl Pts',(65.1235483963183,6.80990900854383,68.5753505820931));
#132897=CARTESIAN_POINT('Ctrl Pts',(65.1200060341081,6.7871513123966,68.5552608472742));
#132898=CARTESIAN_POINT('Ctrl Pts',(65.118578006522,6.77831439876664,68.5471620959691));
#132899=CARTESIAN_POINT('Ctrl Pts',(65.1388177654475,6.94991825968818,68.6423717434951));
#132900=CARTESIAN_POINT('Ctrl Pts',(65.1382863641213,6.94424281485995,68.6393577572805));
#132901=CARTESIAN_POINT('Ctrl Pts',(65.1366766790788,6.92754402610895,68.6302258243284));
#132902=CARTESIAN_POINT('Ctrl Pts',(65.1334919445599,6.89787440093207,68.6121663186481));
#132903=CARTESIAN_POINT('Ctrl Pts',(65.1288128356172,6.85989382618996,68.5856290467829));
#132904=CARTESIAN_POINT('Ctrl Pts',(65.1238697041796,6.82473367649701,68.5575953457266));
#132905=CARTESIAN_POINT('Ctrl Pts',(65.1204130235043,6.80252585577276,68.5379915349674));
#132906=CARTESIAN_POINT('Ctrl Pts',(65.1190184304362,6.7938958541412,68.5300823994905));
#132907=CARTESIAN_POINT('Ctrl Pts',(65.1394699820383,6.96070828693927,68.6219065034142));
#132908=CARTESIAN_POINT('Ctrl Pts',(65.1389542351686,6.9551995268319,68.6189812607692));
#132909=CARTESIAN_POINT('Ctrl Pts',(65.1374054008223,6.93913712232853,68.6101940049127));
#132910=CARTESIAN_POINT('Ctrl Pts',(65.1343316825986,6.91049335455396,68.5927643941554));
#132911=CARTESIAN_POINT('Ctrl Pts',(65.1297988278895,6.8736967763726,68.5670564669691));
#132912=CARTESIAN_POINT('Ctrl Pts',(65.1249899827035,6.83948703027851,68.5397843684272));
#132913=CARTESIAN_POINT('Ctrl Pts',(65.1216185713916,6.81782643979757,68.5206641441865));
#132914=CARTESIAN_POINT('Ctrl Pts',(65.1202572520044,6.80940235481273,68.5129437123894));
#132915=CARTESIAN_POINT('',(65.1322122844213,6.85640303813197,68.6394073971386));
#132916=CARTESIAN_POINT('',(65.1189319128645,6.76267723202094,68.5641625212446));
#132917=CARTESIAN_POINT('Origin',(65.0612614902037,6.85286176575256,68.2371121691863));
#132918=CARTESIAN_POINT('',(65.1202119716011,6.80865446689099,68.5137529809028));
#132919=CARTESIAN_POINT('Ctrl Pts',(65.1322122597858,6.85640293841445,68.6394071751272));
#132920=CARTESIAN_POINT('Ctrl Pts',(65.1290955654378,6.84478572588336,68.6108421213684));
#132921=CARTESIAN_POINT('Ctrl Pts',(65.1265159645158,6.83473800066337,68.5838575775351));
#132922=CARTESIAN_POINT('Ctrl Pts',(65.1239761302869,6.82439218292853,68.5563457900104));
#132923=CARTESIAN_POINT('Ctrl Pts',(65.1232138928177,6.82125728420136,68.5479861954865));
#132924=CARTESIAN_POINT('Ctrl Pts',(65.1224504009973,6.81808207925492,68.5394643466061));
#132925=CARTESIAN_POINT('Ctrl Pts',(65.121941009263,6.81595673594787,68.5337465582695));
#132926=CARTESIAN_POINT('Ctrl Pts',(65.1215473922881,6.8143075610625,68.5292949851828));
#132927=CARTESIAN_POINT('Ctrl Pts',(65.1211981470453,6.8128417025367,68.5253313373399));
#132928=CARTESIAN_POINT('Ctrl Pts',(65.1207483588331,6.81094850659989,68.5201917259831));
#132929=CARTESIAN_POINT('Ctrl Pts',(65.1203129737665,6.80911846789646,68.5151650880062));
#132930=CARTESIAN_POINT('Ctrl Pts',(65.1202038189481,6.80866554628641,68.5138751223312));
#132931=CARTESIAN_POINT('Ctrl Pts',(65.1202119716011,6.80865446689099,68.5137529809029));
#132932=CARTESIAN_POINT('Origin',(66.1117715670066,6.68571538702879,68.4727063556212));
#132933=CARTESIAN_POINT('Ctrl Pts',(65.1510483078126,6.87421650353521,68.7829904020141));
#132934=CARTESIAN_POINT('Ctrl Pts',(65.1504070763793,6.86737161531276,68.7793537997567));
#132935=CARTESIAN_POINT('Ctrl Pts',(65.1483704689148,6.84620801808512,68.7678036466433));
#132936=CARTESIAN_POINT('Ctrl Pts',(65.1444068551304,6.80934107958273,68.7453248609419));
#132937=CARTESIAN_POINT('Ctrl Pts',(65.1387016410555,6.76305370293533,68.7129689894385));
#132938=CARTESIAN_POINT('Ctrl Pts',(65.1328163706566,6.72122561628415,68.6795919610231));
#132939=CARTESIAN_POINT('Ctrl Pts',(65.1287614486238,6.6951784826949,68.6565953554305));
#132940=CARTESIAN_POINT('Ctrl Pts',(65.1271334107255,6.68510379038588,68.6473622937371));
#132941=CARTESIAN_POINT('Ctrl Pts',(65.1452003608014,6.89221246259175,68.7500807649487));
#132942=CARTESIAN_POINT('Ctrl Pts',(65.1445852383808,6.88564557657838,68.7465921721086));
#132943=CARTESIAN_POINT('Ctrl Pts',(65.1426501196904,6.86554336173635,68.7356168826869));
#132944=CARTESIAN_POINT('Ctrl Pts',(65.1388716625005,6.83038738163843,68.714188656264));
#132945=CARTESIAN_POINT('Ctrl Pts',(65.1334103760025,6.78607471303712,68.6832159928414));
#132946=CARTESIAN_POINT('Ctrl Pts',(65.1277490725898,6.74583174047826,68.6511091899172));
#132947=CARTESIAN_POINT('Ctrl Pts',(65.1238363655798,6.72069729532103,68.6289191256786));
#132948=CARTESIAN_POINT('Ctrl Pts',(65.1222638226107,6.7109660375055,68.6200007901315));
#132949=CARTESIAN_POINT('Ctrl Pts',(65.1414736514594,6.91022527003653,68.7167653200066));
#132950=CARTESIAN_POINT('Ctrl Pts',(65.1408846624955,6.90393664650673,68.7134248751548));
#132951=CARTESIAN_POINT('Ctrl Pts',(65.1390511275962,6.88489680775021,68.7030249876305));
#132952=CARTESIAN_POINT('Ctrl Pts',(65.1354580003504,6.85145338791034,68.6826483040529));
#132953=CARTESIAN_POINT('Ctrl Pts',(65.1302408698022,6.80911727613949,68.6530601437148));
#132954=CARTESIAN_POINT('Ctrl Pts',(65.1248037430605,6.7704609017071,68.6222247555069));
#132955=CARTESIAN_POINT('Ctrl Pts',(65.1210333842194,6.74623999946976,68.600841987732));
#132956=CARTESIAN_POINT('Ctrl Pts',(65.1195163881358,6.73685249768201,68.5922386729879));
#132957=CARTESIAN_POINT('Ctrl Pts',(65.1399122363857,6.9281951262389,68.6831490822834));
#132958=CARTESIAN_POINT('Ctrl Pts',(65.1393493185638,6.92218410168036,68.6799564321636));
#132959=CARTESIAN_POINT('Ctrl Pts',(65.1376171252306,6.90420410579108,68.6701305745004));
#132960=CARTESIAN_POINT('Ctrl Pts',(65.1342088860127,6.87246916263756,68.6508029263816));
#132961=CARTESIAN_POINT('Ctrl Pts',(65.1292353292282,6.83210489462999,68.6225959678029));
#132962=CARTESIAN_POINT('Ctrl Pts',(65.1240218446123,6.79503133510698,68.593028962644));
#132963=CARTESIAN_POINT('Ctrl Pts',(65.1203934945133,6.77172179746152,68.5724515663476));
#132964=CARTESIAN_POINT('Ctrl Pts',(65.1189319128645,6.76267723202094,68.5641625212446));
#132965=CARTESIAN_POINT('',(65.1269899214714,6.68586921358489,68.6465524467399));
#132966=CARTESIAN_POINT('Ctrl Pts',(65.1508865027656,6.87471412864423,68.78207666023));
#132967=CARTESIAN_POINT('Ctrl Pts',(65.1502491988091,6.86802460506826,68.7784623662399));
#132968=CARTESIAN_POINT('Ctrl Pts',(65.1495817613522,6.86116856242663,68.7746771454042));
#132969=CARTESIAN_POINT('Ctrl Pts',(65.1488754684122,6.85416574004831,68.7706715562182));
#132970=CARTESIAN_POINT('Ctrl Pts',(65.1476733767521,6.8422471239859,68.7638541507448));
#132971=CARTESIAN_POINT('Ctrl Pts',(65.1463585261558,6.82990176790923,68.7563972389876));
#132972=CARTESIAN_POINT('Ctrl Pts',(65.1449099343834,6.81710107376072,68.7481818600873));
#132973=CARTESIAN_POINT('Ctrl Pts',(65.1447034677796,6.81527660126446,68.7470109288335));
#132974=CARTESIAN_POINT('Ctrl Pts',(65.1444942810936,6.8134429638408,68.7458245714453));
#132975=CARTESIAN_POINT('Ctrl Pts',(65.1442823110769,6.81160017130178,68.7446224292225));
#132976=CARTESIAN_POINT('Ctrl Pts',(65.1427531869705,6.79830650582067,68.7359503317226));
#132977=CARTESIAN_POINT('Ctrl Pts',(65.141079473815,6.78453266254534,68.7264582415822));
#132978=CARTESIAN_POINT('Ctrl Pts',(65.1392293302725,6.77023710148806,68.7159655663571));
#132979=CARTESIAN_POINT('Ctrl Pts',(65.1390293137508,6.7686916276736,68.7148312173981));
#132980=CARTESIAN_POINT('Ctrl Pts',(65.1388272326218,6.76714010483981,68.7136851594773));
#132981=CARTESIAN_POINT('Ctrl Pts',(65.1386230449928,6.76558251795905,68.712527154994));
#132982=CARTESIAN_POINT('Ctrl Pts',(65.1367344209749,6.75117569024202,68.7018162461568));
#132983=CARTESIAN_POINT('Ctrl Pts',(65.1346656938585,6.73624601825409,68.690083919913));
#132984=CARTESIAN_POINT('Ctrl Pts',(65.1323813143638,6.72077703545733,68.6771285607866));
#132985=CARTESIAN_POINT('Ctrl Pts',(65.1321721153332,6.71936041610313,68.6759421341986));
#132986=CARTESIAN_POINT('Ctrl Pts',(65.1319611071595,6.71793931029428,68.6747454473994));
#132987=CARTESIAN_POINT('Ctrl Pts',(65.1317482623707,6.71651372845993,68.6735383445911));
#132988=CARTESIAN_POINT('Ctrl Pts',(65.1302559977912,6.70651890881531,68.6650752914219));
#132989=CARTESIAN_POINT('Ctrl Pts',(65.1286734752311,6.69630338628556,68.6561003573301));
#132990=CARTESIAN_POINT('Ctrl Pts',(65.1269899309713,6.68586927237242,68.6465525006164));
#132991=CARTESIAN_POINT('Ctrl Pts',(65.1445506842445,6.89804539075522,68.7391943517073));
#132992=CARTESIAN_POINT('Ctrl Pts',(65.1388995878143,6.88121747909777,68.6994030493852));
#132993=CARTESIAN_POINT('Ctrl Pts',(65.1351670463109,6.86836305827018,68.6660352394652));
#132994=CARTESIAN_POINT('Ctrl Pts',(65.1322122844213,6.85640303813197,68.6394073971386));
#132995=CARTESIAN_POINT('Origin',(66.1117907052193,6.68589932942379,68.4728725765555));
#132996=CARTESIAN_POINT('Ctrl Pts',(65.1346705530482,6.8919798904543,68.4202960166216));
#132997=CARTESIAN_POINT('Ctrl Pts',(65.1338389881117,6.88683406911642,68.4155799705943));
#132998=CARTESIAN_POINT('Ctrl Pts',(65.1307272078985,6.86806865274327,68.3979321456351));
#132999=CARTESIAN_POINT('Ctrl Pts',(65.1247065901473,6.83491377283282,68.3637875588852));
#133000=CARTESIAN_POINT('Ctrl Pts',(65.1159503997162,6.79260266483268,68.3141287229154));
#133001=CARTESIAN_POINT('Ctrl Pts',(65.1056217526553,6.74903116432229,68.2555520583749));
#133002=CARTESIAN_POINT('Ctrl Pts',(65.0935877735642,6.70501820397611,68.187303970419));
#133003=CARTESIAN_POINT('Ctrl Pts',(65.0796903316755,6.66136171514741,68.1084876612219));
#133004=CARTESIAN_POINT('Ctrl Pts',(65.0637304459047,6.61886989600768,68.0179746511137));
#133005=CARTESIAN_POINT('Ctrl Pts',(65.0455161134506,6.57848378907752,67.9146760386274));
#133006=CARTESIAN_POINT('Ctrl Pts',(65.0248965098102,6.54163495336659,67.7977364553764));
#133007=CARTESIAN_POINT('Ctrl Pts',(65.0016762933978,6.5099268953333,67.6660480641928));
#133008=CARTESIAN_POINT('Ctrl Pts',(64.9756853622109,6.48522042825308,67.5186461686814));
#133009=CARTESIAN_POINT('Ctrl Pts',(64.9475375191463,6.46988450894962,67.3590118180421));
#133010=CARTESIAN_POINT('Ctrl Pts',(64.9279729835967,6.46669330688071,67.248055823275));
#133011=CARTESIAN_POINT('Ctrl Pts',(64.9181216456064,6.4668870503417,67.1921861092301));
#133012=CARTESIAN_POINT('Ctrl Pts',(65.1539262221606,6.9627202545652,68.3397108632764));
#133013=CARTESIAN_POINT('Ctrl Pts',(65.1532012561442,6.95823412856528,68.3355993673901));
#133014=CARTESIAN_POINT('Ctrl Pts',(65.1504777508534,6.94180854698276,68.320153544379));
#133015=CARTESIAN_POINT('Ctrl Pts',(65.1451443581134,6.91242436785244,68.2899064157574));
#133016=CARTESIAN_POINT('Ctrl Pts',(65.1372940192507,6.87447666454151,68.245384915083));
#133017=CARTESIAN_POINT('Ctrl Pts',(65.1279288955758,6.83495486124124,68.1922726644923));
#133018=CARTESIAN_POINT('Ctrl Pts',(65.116907777658,6.79463263891094,68.1297687973011));
#133019=CARTESIAN_POINT('Ctrl Pts',(65.1040642329972,6.75427238436194,68.0569294364098));
#133020=CARTESIAN_POINT('Ctrl Pts',(65.0891844235482,6.7146422157174,67.9725418434751));
#133021=CARTESIAN_POINT('Ctrl Pts',(65.0720761044474,6.67669704588737,67.8755157444185));
#133022=CARTESIAN_POINT('Ctrl Pts',(65.0526198386,6.64191840341569,67.7651737776444));
#133023=CARTESIAN_POINT('Ctrl Pts',(65.0306058055575,6.61184718228901,67.6403259922737));
#133024=CARTESIAN_POINT('Ctrl Pts',(65.0058555336308,6.58830632030332,67.4999602250676));
#133025=CARTESIAN_POINT('Ctrl Pts',(64.9789014271637,6.57360946623491,67.3470958910942));
#133026=CARTESIAN_POINT('Ctrl Pts',(64.9601115765747,6.57054055281461,67.2405333530598));
#133027=CARTESIAN_POINT('Ctrl Pts',(64.9506397889729,6.570726798958,67.1868161762322));
#133028=CARTESIAN_POINT('Ctrl Pts',(65.1900881115087,7.02858813577264,68.2614614009606));
#133029=CARTESIAN_POINT('Ctrl Pts',(65.1894624020497,7.02471626635308,68.2579128147706));
#133030=CARTESIAN_POINT('Ctrl Pts',(65.1871004279267,7.01046935549091,68.2445173233425));
#133031=CARTESIAN_POINT('Ctrl Pts',(65.1824069252406,6.98459615731431,68.2178992021798));
#133032=CARTESIAN_POINT('Ctrl Pts',(65.175400044342,6.9507113143709,68.1781611853795));
#133033=CARTESIAN_POINT('Ctrl Pts',(65.1669320781066,6.9149602716274,68.1301369686635));
#133034=CARTESIAN_POINT('Ctrl Pts',(65.1568540571083,6.87807457519367,68.0729816695171));
#133035=CARTESIAN_POINT('Ctrl Pts',(65.1449918189232,6.84078351559007,68.0057075743117));
#133036=CARTESIAN_POINT('Ctrl Pts',(65.1311176918693,6.80381789154104,67.9270234896327));
#133037=CARTESIAN_POINT('Ctrl Pts',(65.1150392056949,6.7681455309758,67.8358378633339));
#133038=CARTESIAN_POINT('Ctrl Pts',(65.096666148798,6.73529449015099,67.7316390797878));
#133039=CARTESIAN_POINT('Ctrl Pts',(65.0757752191479,6.70674736322814,67.6131607302648));
#133040=CARTESIAN_POINT('Ctrl Pts',(65.0521801518604,6.68429182132624,67.4793464541235));
#133041=CARTESIAN_POINT('Ctrl Pts',(65.0263375593267,6.67019001470368,67.3327858289185));
#133042=CARTESIAN_POINT('Ctrl Pts',(65.0082690346399,6.6672349668859,67.2303141333585));
#133043=CARTESIAN_POINT('Ctrl Pts',(64.9991506546043,6.66741423211489,67.1786012304346));
#133044=CARTESIAN_POINT('Ctrl Pts',(65.2417928776143,7.08799141016858,68.1875253039243));
#133045=CARTESIAN_POINT('Ctrl Pts',(65.2412566831725,7.08467351108365,68.1844843806276));
#133046=CARTESIAN_POINT('Ctrl Pts',(65.2392207577211,7.07239144518454,68.1729379908769));
#133047=CARTESIAN_POINT('Ctrl Pts',(65.2351043430444,7.04968464254353,68.149592708037));
#133048=CARTESIAN_POINT('Ctrl Pts',(65.2288581388817,7.0194639103142,68.1141686998238));
#133049=CARTESIAN_POINT('Ctrl Pts',(65.2211992785201,6.98711354662591,68.0707331516192));
#133050=CARTESIAN_POINT('Ctrl Pts',(65.2119717941427,6.95332709806631,68.0184014850135));
#133051=CARTESIAN_POINT('Ctrl Pts',(65.2009945520552,6.91880400710191,67.9561464521882));
#133052=CARTESIAN_POINT('Ctrl Pts',(65.1880274046423,6.88424141577304,67.8826061046348));
#133053=CARTESIAN_POINT('Ctrl Pts',(65.1728776783849,6.85061879948269,67.7966877375746));
#133054=CARTESIAN_POINT('Ctrl Pts',(65.155481518837,6.81950617573553,67.698029214202));
#133055=CARTESIAN_POINT('Ctrl Pts',(65.1356034655349,6.79233356070731,67.5852951718964));
#133056=CARTESIAN_POINT('Ctrl Pts',(65.1130502252646,6.77085682009007,67.4573893903701));
#133057=CARTESIAN_POINT('Ctrl Pts',(65.0882100570683,6.75729165994912,67.316513796091));
#133058=CARTESIAN_POINT('Ctrl Pts',(65.0707920637135,6.75443930238809,67.2177314470463));
#133059=CARTESIAN_POINT('Ctrl Pts',(65.061992406039,6.75461227184489,67.1678261084541));
#133060=CARTESIAN_POINT('',(65.0995369296605,6.72719442421048,68.2212878397353));
#133061=CARTESIAN_POINT('',(64.9199577054575,6.46687174464771,67.202598919663));
#133062=CARTESIAN_POINT('Ctrl Pts',(65.0995791195013,6.72720037365666,68.2212825822045));
#133063=CARTESIAN_POINT('Ctrl Pts',(65.0976822698379,6.72028556494202,68.2105250131428));
#133064=CARTESIAN_POINT('Ctrl Pts',(65.0957558389128,6.71350272843201,68.1995996803412));
#133065=CARTESIAN_POINT('Ctrl Pts',(65.0938019734153,6.70685605161901,68.1885187583979));
#133066=CARTESIAN_POINT('Ctrl Pts',(65.0893294910235,6.69164152173065,68.1631540501626));
#133067=CARTESIAN_POINT('Ctrl Pts',(65.0847132023982,6.67714022326058,68.1369737765162));
#133068=CARTESIAN_POINT('Ctrl Pts',(65.0799737924691,6.66336991240936,68.1100952471924));
#133069=CARTESIAN_POINT('Ctrl Pts',(65.0748169564677,6.64838677404176,68.0808493769774));
#133070=CARTESIAN_POINT('Ctrl Pts',(65.0695143561238,6.63426905803681,68.0507768360194));
#133071=CARTESIAN_POINT('Ctrl Pts',(65.0640933132977,6.62101769306386,68.0200325743827));
#133072=CARTESIAN_POINT('Ctrl Pts',(65.0581802097322,6.60656351958042,67.986497697619));
#133073=CARTESIAN_POINT('Ctrl Pts',(65.0521261861146,6.59314010997735,67.9521636235467));
#133074=CARTESIAN_POINT('Ctrl Pts',(65.0459645287121,6.58076937331775,67.9172191279448));
#133075=CARTESIAN_POINT('Ctrl Pts',(65.0392369363317,6.56726241110686,67.8790650555916));
#133076=CARTESIAN_POINT('Ctrl Pts',(65.0323810303017,6.55501037370809,67.8401832803673));
#133077=CARTESIAN_POINT('Ctrl Pts',(65.0254209754051,6.54399779743841,67.80071084757));
#133078=CARTESIAN_POINT('Ctrl Pts',(65.0178227566917,6.53197548377289,67.75761920792));
#133079=CARTESIAN_POINT('Ctrl Pts',(65.0101004148254,6.52143034243136,67.71382363089));
#133080=CARTESIAN_POINT('Ctrl Pts',(65.0022830167957,6.5123274224688,67.6694889635685));
#133081=CARTESIAN_POINT('Ctrl Pts',(64.9937552008312,6.50239726081085,67.6211253159296));
#133082=CARTESIAN_POINT('Ctrl Pts',(64.9851142669312,6.49418335930004,67.5721201445991));
#133083=CARTESIAN_POINT('Ctrl Pts',(64.9763867994217,6.48759887860092,67.522624216781));
#133084=CARTESIAN_POINT('Ctrl Pts',(64.9668634700515,6.48041395601466,67.468614732061));
#133085=CARTESIAN_POINT('Ctrl Pts',(64.9572371054031,6.47516917931563,67.4140209052397));
#133086=CARTESIAN_POINT('Ctrl Pts',(64.9475515457086,6.4717450887343,67.3590913666322));
#133087=CARTESIAN_POINT('Ctrl Pts',(64.9383987364529,6.46850933892178,67.3071832059018));
#133088=CARTESIAN_POINT('Ctrl Pts',(64.9291930728841,6.46689949148789,67.2549752934684));
#133089=CARTESIAN_POINT('Ctrl Pts',(64.9199577054575,6.4668717446477,67.202598919663));
#133090=CARTESIAN_POINT('',(65.0614282834239,6.75162228554997,67.1773189309182));
#133091=CARTESIAN_POINT('Ctrl Pts',(65.0995369296605,6.72719442421049,68.2212878397353));
#133092=CARTESIAN_POINT('Ctrl Pts',(65.0995675555563,6.72716010371951,68.221136173046));
#133093=CARTESIAN_POINT('Ctrl Pts',(65.0994719063417,6.72683619259612,68.2195356587124));
#133094=CARTESIAN_POINT('Ctrl Pts',(65.0991078651206,6.72561893193096,68.2132807572063));
#133095=CARTESIAN_POINT('Ctrl Pts',(65.0989280671564,6.72501418471105,68.210209911432));
#133096=CARTESIAN_POINT('Ctrl Pts',(65.0980260005293,6.72207473766137,68.1940983041802));
#133097=CARTESIAN_POINT('Ctrl Pts',(65.097360711155,6.71994808440332,68.1821554868447));
#133098=CARTESIAN_POINT('Ctrl Pts',(65.0967081062033,6.71792384189042,68.1704251071661));
#133099=CARTESIAN_POINT('Ctrl Pts',(65.0962753846899,6.71659547529839,68.1626520285289));
#133100=CARTESIAN_POINT('Ctrl Pts',(65.0959604444661,6.71564207815097,68.1570014255529));
#133101=CARTESIAN_POINT('Ctrl Pts',(65.0953880058314,6.71392179538477,68.1467429225592));
#133102=CARTESIAN_POINT('Ctrl Pts',(65.0945397680694,6.71136873889932,68.1324085686363));
#133103=CARTESIAN_POINT('Ctrl Pts',(65.0927881222842,6.70655433500724,68.1015604372104));
#133104=CARTESIAN_POINT('Ctrl Pts',(65.0921252586568,6.70479202834819,68.089718680223));
#133105=CARTESIAN_POINT('Ctrl Pts',(65.0910345580279,6.70206233773065,68.0695921665363));
#133106=CARTESIAN_POINT('Ctrl Pts',(65.0904652080591,6.70067637610273,68.0589379489014));
#133107=CARTESIAN_POINT('Ctrl Pts',(65.0898649673399,6.69929060171878,68.0473930398002));
#133108=CARTESIAN_POINT('Ctrl Pts',(65.0894585811012,6.69837057395887,68.0394980979976));
#133109=CARTESIAN_POINT('Ctrl Pts',(65.0891647052933,6.69772220656397,68.0337151425024));
#133110=CARTESIAN_POINT('Ctrl Pts',(65.0870987600182,6.69323358761507,67.9927505910103));
#133111=CARTESIAN_POINT('Ctrl Pts',(65.0852415502832,6.68999131681029,67.9537767255883));
#133112=CARTESIAN_POINT('Ctrl Pts',(65.0825675280683,6.68653839116838,67.8948244268623));
#133113=CARTESIAN_POINT('Ctrl Pts',(65.0816952976188,6.68562456629401,67.8750943663708));
#133114=CARTESIAN_POINT('Ctrl Pts',(65.0799871749233,6.68427009479148,67.8355045982994));
#133115=CARTESIAN_POINT('Ctrl Pts',(65.0792365216954,6.68385037915333,67.8177201330391));
#133116=CARTESIAN_POINT('Ctrl Pts',(65.0710677997279,6.68174643674947,67.6196579069018));
#133117=CARTESIAN_POINT('Ctrl Pts',(65.0645780549624,6.69992461595788,67.411398489151));
#133118=CARTESIAN_POINT('Ctrl Pts',(65.0614400430891,6.75161362534301,67.177316857372));
#133119=CARTESIAN_POINT('Ctrl Pts',(64.9199577054575,6.46687174464771,67.202598919663));
#133120=CARTESIAN_POINT('Ctrl Pts',(64.9333050247472,6.50957649447236,67.2002436743331));
#133121=CARTESIAN_POINT('Ctrl Pts',(64.9494820555029,6.55136533225673,67.1973921465925));
#133122=CARTESIAN_POINT('Ctrl Pts',(64.9683398996363,6.59186707079172,67.1940423684793));
#133123=CARTESIAN_POINT('Ctrl Pts',(64.9867017502843,6.63130354447895,67.1907806952475));
#133124=CARTESIAN_POINT('Ctrl Pts',(65.0076053315602,6.66951971007743,67.1870467099025));
#133125=CARTESIAN_POINT('Ctrl Pts',(65.0308682154119,6.70618765028569,67.1828511423827));
#133126=CARTESIAN_POINT('Ctrl Pts',(65.040651362678,6.72160826027071,67.1810867070198));
#133127=CARTESIAN_POINT('Ctrl Pts',(65.0508512121906,6.73675523607014,67.1792407850699));
#133128=CARTESIAN_POINT('Ctrl Pts',(65.0614516307786,6.75160508908749,67.1773148179911));
#133129=CARTESIAN_POINT('Ctrl Pts',(65.1432217654919,-6.97297506433017,
68.6973703391101));
#133130=CARTESIAN_POINT('Ctrl Pts',(65.1432243503256,-6.9729296867911,68.6973781401607));
#133131=CARTESIAN_POINT('Ctrl Pts',(65.1432367108929,-6.97136627551693,
68.6972928489378));
#133132=CARTESIAN_POINT('Ctrl Pts',(65.141532389107,-6.95194096119578,68.687637522311));
#133133=CARTESIAN_POINT('Ctrl Pts',(65.1400238117738,-6.93547409352959,
68.6790824101809));
#133134=CARTESIAN_POINT('Ctrl Pts',(65.1394727093545,-6.92962631050212,
68.6759566677395));
#133135=CARTESIAN_POINT('Ctrl Pts',(65.1449771131016,-6.95849924894636,
68.7351837598004));
#133136=CARTESIAN_POINT('Ctrl Pts',(65.1449653224239,-6.95827999915231,
68.7351123311065));
#133137=CARTESIAN_POINT('Ctrl Pts',(65.1446513814295,-6.95276757579234,
68.7332285542318));
#133138=CARTESIAN_POINT('Ctrl Pts',(65.1429860104,-6.93374364056231,68.7237906471918));
#133139=CARTESIAN_POINT('Ctrl Pts',(65.141417161647,-6.91661976904466,68.7148935659804));
#133140=CARTESIAN_POINT('Ctrl Pts',(65.1408375768619,-6.91047034785759,
68.7116063878611));
#133141=CARTESIAN_POINT('Ctrl Pts',(65.1491744576555,-6.94398141948418,
68.7726764498994));
#133142=CARTESIAN_POINT('Ctrl Pts',(65.1491482532267,-6.94358779616249,
68.7725255874527));
#133143=CARTESIAN_POINT('Ctrl Pts',(65.1485071429687,-6.93411497591497,
68.7688386960651));
#133144=CARTESIAN_POINT('Ctrl Pts',(65.1468808355773,-6.91549358299687,
68.7596188387069));
#133145=CARTESIAN_POINT('Ctrl Pts',(65.1452515407344,-6.89771080359099,
68.7503787973671));
#133146=CARTESIAN_POINT('Ctrl Pts',(65.1446433910398,-6.89125887007876,
68.7469297157195));
#133147=CARTESIAN_POINT('Ctrl Pts',(65.1557607443018,-6.92947588538437,
68.8097147522224));
#133148=CARTESIAN_POINT('Ctrl Pts',(65.155720141749,-6.92890803952096,68.8094845487692));
#133149=CARTESIAN_POINT('Ctrl Pts',(65.1547522172099,-6.91547825177383,
68.8039966501812));
#133150=CARTESIAN_POINT('Ctrl Pts',(65.1531649402084,-6.8972590585529,68.7949946569169));
#133151=CARTESIAN_POINT('Ctrl Pts',(65.1514752507228,-6.87881793207328,
68.7854119473515));
#133152=CARTESIAN_POINT('Ctrl Pts',(65.1508385604312,-6.87206374371237,
68.781801099976));
#133153=CARTESIAN_POINT('',(65.1441607442837,-6.89690667515947,68.7364336189164));
#133154=CARTESIAN_POINT('',(65.1506852045397,-6.87254041891262,68.7809350460487));
#133155=CARTESIAN_POINT('Origin',(66.1354906276427,-6.87281762818581,68.607288395026));
#133156=CARTESIAN_POINT('',(65.1554676900943,-6.9282418042031,68.808018444524));
#133157=CARTESIAN_POINT('Ctrl Pts',(65.1554654484591,-6.92824180453999,
68.808018841215));
#133158=CARTESIAN_POINT('Ctrl Pts',(65.1511823527249,-6.91706470348454,
68.7837161221291));
#133159=CARTESIAN_POINT('Ctrl Pts',(65.1474541412159,-6.90679031326606,
68.7598370684572));
#133160=CARTESIAN_POINT('Ctrl Pts',(65.14416106117,-6.89690666738156,68.7364335775926));
#133161=CARTESIAN_POINT('Ctrl Pts',(65.1554609455217,-6.92824180338472,
68.8080196357745));
#133162=CARTESIAN_POINT('Ctrl Pts',(65.1554598852463,-6.9282270379923,68.8080136226073));
#133163=CARTESIAN_POINT('Ctrl Pts',(65.1554588248862,-6.92821227449162,
68.8080076089597));
#133164=CARTESIAN_POINT('Ctrl Pts',(65.1554577644413,-6.92819751288013,
68.8080015948315));
#133165=CARTESIAN_POINT('Ctrl Pts',(65.1545901961715,-6.91612078396726,
68.8030813328399));
#133166=CARTESIAN_POINT('Ctrl Pts',(65.1536662468902,-6.9053125244734,68.7978413830879));
#133167=CARTESIAN_POINT('Ctrl Pts',(65.1526864112108,-6.89434361965686,
68.7922844405439));
#133168=CARTESIAN_POINT('Ctrl Pts',(65.1526345313573,-6.89376284352584,
68.7919902143066));
#133169=CARTESIAN_POINT('Ctrl Pts',(65.1525824938791,-6.89318160595316,
68.7916950941604));
#133170=CARTESIAN_POINT('Ctrl Pts',(65.1525302985756,-6.89259969156981,
68.7913990789963));
#133171=CARTESIAN_POINT('Ctrl Pts',(65.1519369363571,-6.88598442186751,
68.7880339445319));
#133172=CARTESIAN_POINT('Ctrl Pts',(65.1513231666928,-6.87928156135235,
68.7845530819381));
#133173=CARTESIAN_POINT('Ctrl Pts',(65.1506852076991,-6.87254041916445,
68.7809350467598));
#133174=CARTESIAN_POINT('Ctrl Pts',(65.1394962399547,-6.92987609657407,
68.6760901283112));
#133175=CARTESIAN_POINT('Ctrl Pts',(65.1389690427465,-6.92427743436571,
68.6730999838425));
#133176=CARTESIAN_POINT('Ctrl Pts',(65.1372553241028,-6.90657130252873,
68.6633787872026));
#133177=CARTESIAN_POINT('Ctrl Pts',(65.1338515053416,-6.87499181440707,
68.6440763568521));
#133178=CARTESIAN_POINT('Ctrl Pts',(65.1288246013982,-6.83442541808995,
68.615566793012));
#133179=CARTESIAN_POINT('Ctrl Pts',(65.1235003522383,-6.79680702773606,
68.5853716269996));
#133180=CARTESIAN_POINT('Ctrl Pts',(65.1197752963197,-6.7730817711464,68.5642457819742));
#133181=CARTESIAN_POINT('Ctrl Pts',(65.1182256999152,-6.7635933515749,68.5554575793337));
#133182=CARTESIAN_POINT('Ctrl Pts',(65.1408623196493,-6.91073297552592,
68.7117467190877));
#133183=CARTESIAN_POINT('Ctrl Pts',(65.1403080523265,-6.90484744757448,
68.7086031398901));
#133184=CARTESIAN_POINT('Ctrl Pts',(65.1384869336936,-6.88602316190435,
68.6982735918235));
#133185=CARTESIAN_POINT('Ctrl Pts',(65.134885933983,-6.85262897908219,68.6778523602412));
#133186=CARTESIAN_POINT('Ctrl Pts',(65.1295969110304,-6.80995270579319,
68.6478564387582));
#133187=CARTESIAN_POINT('Ctrl Pts',(65.1240299537541,-6.77062767825713,
68.616284755745));
#133188=CARTESIAN_POINT('Ctrl Pts',(65.1201503127629,-6.74591898706875,
68.5942822162525));
#133189=CARTESIAN_POINT('Ctrl Pts',(65.1185385200063,-6.73604970686306,
68.5851412821568));
#133190=CARTESIAN_POINT('Ctrl Pts',(65.1446693495273,-6.89153437655917,
68.7470769375128));
#133191=CARTESIAN_POINT('Ctrl Pts',(65.1440879336391,-6.88536115151044,
68.7437794789231));
#133192=CARTESIAN_POINT('Ctrl Pts',(65.1421591037656,-6.86541547152994,
68.7328398163906));
#133193=CARTESIAN_POINT('Ctrl Pts',(65.1383603516631,-6.83020133491268,
68.7112965412231));
#133194=CARTESIAN_POINT('Ctrl Pts',(65.1328084500647,-6.78540907010117,
68.6798099545433));
#133195=CARTESIAN_POINT('Ctrl Pts',(65.1269980812893,-6.74437245944551,
68.6468577653));
#133196=CARTESIAN_POINT('Ctrl Pts',(65.1229634072287,-6.71867748360566,
68.6239759906272));
#133197=CARTESIAN_POINT('Ctrl Pts',(65.121289237871,-6.70842623900873,68.614481302839));
#133198=CARTESIAN_POINT('Ctrl Pts',(65.150865733584,-6.87235211804336,68.7819552064712));
#133199=CARTESIAN_POINT('Ctrl Pts',(65.1502571922374,-6.86589144076419,
68.7785039994602));
#133200=CARTESIAN_POINT('Ctrl Pts',(65.1482207427991,-6.84482532092261,
68.766954741747));
#133201=CARTESIAN_POINT('Ctrl Pts',(65.1442244066172,-6.80779277952251,
68.7442903779965));
#133202=CARTESIAN_POINT('Ctrl Pts',(65.1384098501162,-6.76088632416654,
68.7113143948654));
#133203=CARTESIAN_POINT('Ctrl Pts',(65.1323562770159,-6.71813958716634,
68.6769828743784));
#133204=CARTESIAN_POINT('Ctrl Pts',(65.1281667018386,-6.69145916612878,
68.6532226128664));
#133205=CARTESIAN_POINT('Ctrl Pts',(65.1264302089705,-6.68082628224091,
68.6433744724751));
#133206=CARTESIAN_POINT('',(65.1309287612286,-6.85155002742103,68.6274185545369));
#133207=CARTESIAN_POINT('Ctrl Pts',(65.14416106117,-6.89690666738156,68.7364335775926));
#133208=CARTESIAN_POINT('Ctrl Pts',(65.139541879359,-6.88303685803668,68.7035889625114));
#133209=CARTESIAN_POINT('Ctrl Pts',(65.1351852092738,-6.86772274606561,
68.6676631553856));
#133210=CARTESIAN_POINT('Ctrl Pts',(65.1309287612286,-6.85155002742104,
68.6274185545369));
#133211=CARTESIAN_POINT('',(65.1263322567563,-6.68184571691787,68.6428226491504));
#133212=CARTESIAN_POINT('Origin',(65.0998354960377,-6.818067512662,68.4925520530996));
#133213=CARTESIAN_POINT('',(65.1182638051832,-6.76382675080627,68.5556736851631));
#133214=CARTESIAN_POINT('Origin',(66.1111353668526,-6.68186340008987,68.4691561841244));
#133215=CARTESIAN_POINT('Origin',(65.0627991145643,-6.85369791430341,68.2411322661509));
#133216=CARTESIAN_POINT('Ctrl Pts',(65.1393808590346,-6.96014231171326,
68.618798447603));
#133217=CARTESIAN_POINT('Ctrl Pts',(65.1389042098079,-6.95508367036459,
68.6160948227003));
#133218=CARTESIAN_POINT('Ctrl Pts',(65.1373676824532,-6.9392301048245,68.6073773797974));
#133219=CARTESIAN_POINT('Ctrl Pts',(65.1342860536698,-6.91061645632782,
68.5899030215337));
#133220=CARTESIAN_POINT('Ctrl Pts',(65.129676712871,-6.87341115490448,68.5637612683055));
#133221=CARTESIAN_POINT('Ctrl Pts',(65.1247496922159,-6.83858632048248,
68.5358189776352));
#133222=CARTESIAN_POINT('Ctrl Pts',(65.1212833835859,-6.81649988158678,
68.5161605602661));
#133223=CARTESIAN_POINT('Ctrl Pts',(65.1198454596578,-6.80768964317406,
68.508005681332));
#133224=CARTESIAN_POINT('Ctrl Pts',(65.1387132610527,-6.95001387475172,
68.6378926818026));
#133225=CARTESIAN_POINT('Ctrl Pts',(65.1382224181339,-6.94480491726722,
68.6351086082347));
#133226=CARTESIAN_POINT('Ctrl Pts',(65.1366293538061,-6.92836306631528,
68.6260709173592));
#133227=CARTESIAN_POINT('Ctrl Pts',(65.1334437409379,-6.89879243202413,
68.6080065552313));
#133228=CARTESIAN_POINT('Ctrl Pts',(65.1286958085209,-6.86047156380297,
68.5810789119924));
#133229=CARTESIAN_POINT('Ctrl Pts',(65.1236407346436,-6.82474630464972,
68.5524103685699));
#133230=CARTESIAN_POINT('Ctrl Pts',(65.1200929585004,-6.80214140449738,
68.5322899264659));
#133231=CARTESIAN_POINT('Ctrl Pts',(65.118622415774,-6.79313129599011,68.5239500579557));
#133232=CARTESIAN_POINT('Ctrl Pts',(65.1387451082755,-6.93983821679403,
68.6569520576361));
#133233=CARTESIAN_POINT('Ctrl Pts',(65.1382400054905,-6.93447824236689,
68.6540871603338));
#133234=CARTESIAN_POINT('Ctrl Pts',(65.1365901406018,-6.91744536328741,
68.6447277284193));
#133235=CARTESIAN_POINT('Ctrl Pts',(65.1333000588522,-6.88691328152396,
68.6260706116997));
#133236=CARTESIAN_POINT('Ctrl Pts',(65.1284128886725,-6.84747164548773,
68.5983534144583));
#133237=CARTESIAN_POINT('Ctrl Pts',(65.1232291645607,-6.81084176362548,
68.5689552323338));
#133238=CARTESIAN_POINT('Ctrl Pts',(65.1195995410848,-6.78771598503634,
68.5483706114342));
#133239=CARTESIAN_POINT('Ctrl Pts',(65.1180962274842,-6.77850507459625,
68.539844890886));
#133240=CARTESIAN_POINT('Ctrl Pts',(65.1394727093545,-6.92962631050212,
68.6759566677395));
#133241=CARTESIAN_POINT('Ctrl Pts',(65.1389532959058,-6.92411478117078,
68.6730106587876));
#133242=CARTESIAN_POINT('Ctrl Pts',(65.1372464281181,-6.90648876856817,
68.663328339709));
#133243=CARTESIAN_POINT('Ctrl Pts',(65.1338515053416,-6.87499181440707,
68.6440763568521));
#133244=CARTESIAN_POINT('Ctrl Pts',(65.1288246013981,-6.83442541808995,
68.615566793012));
#133245=CARTESIAN_POINT('Ctrl Pts',(65.1235117687664,-6.79688769101786,
68.5854363730231));
#133246=CARTESIAN_POINT('Ctrl Pts',(65.1198000063964,-6.77323917848776,
68.5643859198026));
#133247=CARTESIAN_POINT('Ctrl Pts',(65.1182638051832,-6.76382675080628,
68.5556736851632));
#133248=CARTESIAN_POINT('',(65.1197969390187,-6.80693156137258,68.5088219205847));
#133249=CARTESIAN_POINT('Ctrl Pts',(65.1309287467098,-6.85154997225577,
68.6274184172623));
#133250=CARTESIAN_POINT('Ctrl Pts',(65.1271634026351,-6.83714074568404,
68.5915609828876));
#133251=CARTESIAN_POINT('Ctrl Pts',(65.1234786475439,-6.82209332249245,
68.5522537135607));
#133252=CARTESIAN_POINT('Ctrl Pts',(65.1197969390187,-6.80693156137258,
68.5088219205847));
#133253=CARTESIAN_POINT('Origin',(66.1111167056211,-6.68168974877604,68.4689977647608));
#133254=CARTESIAN_POINT('Ctrl Pts',(65.1342438570207,-6.88922545630012,
68.4173762199009));
#133255=CARTESIAN_POINT('Ctrl Pts',(65.133486060561,-6.88458243975978,68.4130785355508));
#133256=CARTESIAN_POINT('Ctrl Pts',(65.1304933916005,-6.86666656489,68.3961062266279));
#133257=CARTESIAN_POINT('Ctrl Pts',(65.1246847728085,-6.83477575818617,
68.3631639449019));
#133258=CARTESIAN_POINT('Ctrl Pts',(65.1161582670608,-6.79355322048586,
68.3148077157122));
#133259=CARTESIAN_POINT('Ctrl Pts',(65.1060825958666,-6.75087779215306,
68.2576657485828));
#133260=CARTESIAN_POINT('Ctrl Pts',(65.0942790437781,-6.70741963316853,
68.1907244770599));
#133261=CARTESIAN_POINT('Ctrl Pts',(65.0806265551699,-6.66416928709678,
68.1132973669754));
#133262=CARTESIAN_POINT('Ctrl Pts',(65.0650730726838,-6.62230767446081,
68.0250891843942));
#133263=CARTESIAN_POINT('Ctrl Pts',(65.0475810184328,-6.58288451356995,
67.9258868152054));
#133264=CARTESIAN_POINT('Ctrl Pts',(65.0280726826782,-6.5470248949559,67.8152495452771));
#133265=CARTESIAN_POINT('Ctrl Pts',(65.0063045667778,-6.51580441028535,
67.6917964253113));
#133266=CARTESIAN_POINT('Ctrl Pts',(64.9820073764202,-6.49060466876522,
67.5540002113891));
#133267=CARTESIAN_POINT('Ctrl Pts',(64.9549113829709,-6.47312496298017,
67.4003311963398));
#133268=CARTESIAN_POINT('Ctrl Pts',(64.9332779206116,-6.46744580878183,
67.2776417345743));
#133269=CARTESIAN_POINT('Ctrl Pts',(64.9207216538056,-6.46711162774575,
67.2064316069159));
#133270=CARTESIAN_POINT('Ctrl Pts',(64.9182105185209,-6.46716137792081,
67.1921902510292));
#133271=CARTESIAN_POINT('Ctrl Pts',(65.1156612636186,-6.82092619803015,
68.4944428007781));
#133272=CARTESIAN_POINT('Ctrl Pts',(65.1148110828427,-6.81571710110071,
68.4896211812618));
#133273=CARTESIAN_POINT('Ctrl Pts',(65.1114622226625,-6.79567000857472,
68.4706288246759));
#133274=CARTESIAN_POINT('Ctrl Pts',(65.1050182325365,-6.76030288849035,
68.4340831623743));
#133275=CARTESIAN_POINT('Ctrl Pts',(65.095644169583,-6.71499492821166,68.3809202014195));
#133276=CARTESIAN_POINT('Ctrl Pts',(65.0846629933304,-6.66849766520989,
68.3186428586899));
#133277=CARTESIAN_POINT('Ctrl Pts',(65.0719005692391,-6.62152193749562,
68.2462635541871));
#133278=CARTESIAN_POINT('Ctrl Pts',(65.0572480016601,-6.57511671269435,
68.1631647143009));
#133279=CARTESIAN_POINT('Ctrl Pts',(65.0406747571108,-6.53052359359599,
68.0691731737046));
#133280=CARTESIAN_POINT('Ctrl Pts',(65.0221556399096,-6.48879599868487,
67.964146041071));
#133281=CARTESIAN_POINT('Ctrl Pts',(65.0015802797845,-6.4509822157624,67.847457375233));
#133282=CARTESIAN_POINT('Ctrl Pts',(64.9787112300804,-6.41819144706752,
67.7177605494007));
#133283=CARTESIAN_POINT('Ctrl Pts',(64.95327920567,-6.39182510624466,67.5735283717446));
#133284=CARTESIAN_POINT('Ctrl Pts',(64.9250419773436,-6.37362011926285,
67.4133870920872));
#133285=CARTESIAN_POINT('Ctrl Pts',(64.9025780060496,-6.36772926219258,
67.2859875800991));
#133286=CARTESIAN_POINT('Ctrl Pts',(64.8895541865461,-6.36738304863499,
67.2121258293271));
#133287=CARTESIAN_POINT('Ctrl Pts',(64.8869501391361,-6.36743465915249,
67.1973575425938));
#133288=CARTESIAN_POINT('Ctrl Pts',(65.1132982389247,-6.75037255747734,
68.5710850505295));
#133289=CARTESIAN_POINT('Ctrl Pts',(65.1123526244647,-6.74457869530585,
68.5657222020991));
#133290=CARTESIAN_POINT('Ctrl Pts',(65.1086358161119,-6.722330039128,68.5446431212891));
#133291=CARTESIAN_POINT('Ctrl Pts',(65.1015354826836,-6.68337186152832,
68.5043751401169));
#133292=CARTESIAN_POINT('Ctrl Pts',(65.0912858868476,-6.63384362941354,
68.4462467895843));
#133293=CARTESIAN_POINT('Ctrl Pts',(65.0793693171516,-6.58339838284189,
68.3786645657567));
#133294=CARTESIAN_POINT('Ctrl Pts',(65.0656163711664,-6.5327889805305,68.3006677328371));
#133295=CARTESIAN_POINT('Ctrl Pts',(65.0499307145907,-6.48312474259335,
68.2117099539833));
#133296=CARTESIAN_POINT('Ctrl Pts',(65.0323040482633,-6.43570995705239,
68.1117441616463));
#133297=CARTESIAN_POINT('Ctrl Pts',(65.0127239674143,-6.39160186470016,
68.0007000051564));
#133298=CARTESIAN_POINT('Ctrl Pts',(64.9910463631973,-6.35176941554781,
67.8777602024444));
#133299=CARTESIAN_POINT('Ctrl Pts',(64.9670400407054,-6.31735653180476,
67.7416135821254));
#133300=CARTESIAN_POINT('Ctrl Pts',(64.9404357242987,-6.28978508524634,
67.5907330061794));
#133301=CARTESIAN_POINT('Ctrl Pts',(64.9110195918763,-6.27083087740692,
67.4239058291597));
#133302=CARTESIAN_POINT('Ctrl Pts',(64.8876976986906,-6.26472132969921,
67.2916408003443));
#133303=CARTESIAN_POINT('Ctrl Pts',(64.8741908937815,-6.26436268645759,
67.2150399032216));
#133304=CARTESIAN_POINT('Ctrl Pts',(64.871490867457,-6.26441621872265,67.1997272930141));
#133305=CARTESIAN_POINT('Ctrl Pts',(65.1268063180921,-6.67931671571179,
68.6454713706));
#133306=CARTESIAN_POINT('Ctrl Pts',(65.1257645906506,-6.67293392593594,
68.6395634407853));
#133307=CARTESIAN_POINT('Ctrl Pts',(65.121677215068,-6.64846803536371,68.6163827824362));
#133308=CARTESIAN_POINT('Ctrl Pts',(65.113915866482,-6.60589323908104,68.5723659869065));
#133309=CARTESIAN_POINT('Ctrl Pts',(65.1027845057151,-6.55211469521134,
68.5092369031251));
#133310=CARTESIAN_POINT('Ctrl Pts',(65.0899258844404,-6.49769336330045,
68.4363120380258));
#133311=CARTESIAN_POINT('Ctrl Pts',(65.075175366021,-6.44342442187559,68.3526576910904));
#133312=CARTESIAN_POINT('Ctrl Pts',(65.0584492669151,-6.39047797312858,
68.2577992693084));
#133313=CARTESIAN_POINT('Ctrl Pts',(65.0397616805472,-6.34022143650729,
68.151816700473));
#133314=CARTESIAN_POINT('Ctrl Pts',(65.0191130841056,-6.2937159023197,68.0347126909168));
#133315=CARTESIAN_POINT('Ctrl Pts',(64.9963253900166,-6.25185041805988,
67.9054772557028));
#133316=CARTESIAN_POINT('Ctrl Pts',(64.9711736996225,-6.21580387304457,
67.7628349312237));
#133317=CARTESIAN_POINT('Ctrl Pts',(64.9433887468392,-6.18701874280112,
67.605258633651));
#133318=CARTESIAN_POINT('Ctrl Pts',(64.9127853188742,-6.16730998114583,
67.4316979690137));
#133319=CARTESIAN_POINT('Ctrl Pts',(64.8885993971038,-6.16098018615946,
67.2945327905948));
#133320=CARTESIAN_POINT('Ctrl Pts',(64.8746061688967,-6.16060902475923,
67.2151732498622));
#133321=CARTESIAN_POINT('Ctrl Pts',(64.8718094804788,-6.16066449245085,
67.199312441683));
#133322=CARTESIAN_POINT('',(65.0995136833054,-6.72702879152427,68.2205016222657));
#133323=CARTESIAN_POINT('Ctrl Pts',(65.1197964539582,-6.80692956382894,
68.5088161984767));
#133324=CARTESIAN_POINT('Ctrl Pts',(65.117970090298,-6.79929279591152,68.4870734254445));
#133325=CARTESIAN_POINT('Ctrl Pts',(65.1161906463661,-6.79193584047724,
68.4647514783563));
#133326=CARTESIAN_POINT('Ctrl Pts',(65.1135867664279,-6.78123706716053,
68.4304642096668));
#133327=CARTESIAN_POINT('Ctrl Pts',(65.1127294947203,-6.77772688537746,
68.4189006628725));
#133328=CARTESIAN_POINT('Ctrl Pts',(65.1110297678899,-6.770811996763,68.3955047967372));
#133329=CARTESIAN_POINT('Ctrl Pts',(65.1100610746099,-6.76690233978478,
68.3818714985991));
#133330=CARTESIAN_POINT('Ctrl Pts',(65.1064983128958,-6.75265152221011,
68.3310438611609));
#133331=CARTESIAN_POINT('Ctrl Pts',(65.103111422614,-6.73945547580017,68.2811679223586));
#133332=CARTESIAN_POINT('Ctrl Pts',(65.0994829680072,-6.72702809613026,
68.2205074846029));
#133333=CARTESIAN_POINT('',(64.8738238573791,-6.16438935871099,67.210776354606));
#133334=CARTESIAN_POINT('Ctrl Pts',(65.1263322567668,-6.68184571628219,
68.6428226485642));
#133335=CARTESIAN_POINT('Ctrl Pts',(65.1252939386827,-6.67548394330349,
68.6369340541028));
#133336=CARTESIAN_POINT('Ctrl Pts',(65.1242407634166,-6.66918005369973,
68.6309612003757));
#133337=CARTESIAN_POINT('Ctrl Pts',(65.1231735592988,-6.6629353884095,68.6249087850782));
#133338=CARTESIAN_POINT('Ctrl Pts',(65.1201122562707,-6.64502240208925,
68.607547272909));
#133339=CARTESIAN_POINT('Ctrl Pts',(65.1169355176638,-6.62759673969112,
68.5895310930464));
#133340=CARTESIAN_POINT('Ctrl Pts',(65.1136570498455,-6.61067539008644,
68.5709379781644));
#133341=CARTESIAN_POINT('Ctrl Pts',(65.1100927169032,-6.59227858793113,
68.5507236416057));
#133342=CARTESIAN_POINT('Ctrl Pts',(65.1064081408252,-6.57447787972176,
68.5298273723462));
#133343=CARTESIAN_POINT('Ctrl Pts',(65.1026212919839,-6.55729893056469,
68.5083510854263));
#133344=CARTESIAN_POINT('Ctrl Pts',(65.0984830630297,-6.53852595393328,
68.4848820228665));
#133345=CARTESIAN_POINT('Ctrl Pts',(65.094222701058,-6.5204954750822,68.4607203095474));
#133346=CARTESIAN_POINT('Ctrl Pts',(65.0898599033342,-6.50321292732108,
68.4359776542108));
#133347=CARTESIAN_POINT('Ctrl Pts',(65.0850814403227,-6.48428378587311,
68.4088776438919));
#133348=CARTESIAN_POINT('Ctrl Pts',(65.0801800926007,-6.46625188284986,
68.3810807197495));
#133349=CARTESIAN_POINT('Ctrl Pts',(65.0751779368011,-6.44910586247529,
68.3527120845897));
#133350=CARTESIAN_POINT('Ctrl Pts',(65.0697293007619,-6.43042943009645,
68.3218113341725));
#133351=CARTESIAN_POINT('Ctrl Pts',(65.0641610577563,-6.41280408151792,
68.2902322589422));
#133352=CARTESIAN_POINT('Ctrl Pts',(65.0584982023557,-6.39619966014369,
68.2581166101517));
#133353=CARTESIAN_POINT('Ctrl Pts',(65.0523870831185,-6.37828085563542,
68.2234587308216));
#133354=CARTESIAN_POINT('Ctrl Pts',(65.0461657798431,-6.36155100579428,
68.1881759667537));
#133355=CARTESIAN_POINT('Ctrl Pts',(65.0398590110274,-6.34594160392812,
68.152408503523));
#133356=CARTESIAN_POINT('Ctrl Pts',(65.0331037660103,-6.32922221286453,
68.1140976053711));
#133357=CARTESIAN_POINT('Ctrl Pts',(65.0262504682212,-6.31378828614223,
68.0752306223181));
#133358=CARTESIAN_POINT('Ctrl Pts',(65.019312337714,-6.29957015532149,68.0358825289906));
#133359=CARTESIAN_POINT('Ctrl Pts',(65.0118621859929,-6.28430275271249,
67.9936306190665));
#133360=CARTESIAN_POINT('Ctrl Pts',(65.0043142186634,-6.27043721470028,
67.9508239692352));
#133361=CARTESIAN_POINT('Ctrl Pts',(64.9966934743881,-6.25793178150374,
67.9076045808126));
#133362=CARTESIAN_POINT('Ctrl Pts',(64.988443653798,-6.24439405125804,67.8608175233269));
#133363=CARTESIAN_POINT('Ctrl Pts',(64.9801085451537,-6.23245024118954,
67.8135467732247));
#133364=CARTESIAN_POINT('Ctrl Pts',(64.9717130036401,-6.22202862475033,
67.7659332912632));
#133365=CARTESIAN_POINT('Ctrl Pts',(64.9625709513924,-6.21068034401822,
67.7140861365454));
#133366=CARTESIAN_POINT('Ctrl Pts',(64.9533572414561,-6.20113699118725,
67.6618325908494));
#133367=CARTESIAN_POINT('Ctrl Pts',(64.944105499176,-6.19329504774133,67.6093633529697));
#133368=CARTESIAN_POINT('Ctrl Pts',(64.9339962248679,-6.18472624469832,
67.5520308092821));
#133369=CARTESIAN_POINT('Ctrl Pts',(64.9238415409629,-6.17818887081409,
67.4944407349221));
#133370=CARTESIAN_POINT('Ctrl Pts',(64.9136642615231,-6.17349919156016,
67.4367225148641));
#133371=CARTESIAN_POINT('Ctrl Pts',(64.9025266470073,-6.16836699095177,
67.3735579639306));
#133372=CARTESIAN_POINT('Ctrl Pts',(64.8913619713804,-6.16544763621553,
67.3102399417465));
#133373=CARTESIAN_POINT('Ctrl Pts',(64.8801826595514,-6.16462907124658,
67.2468389134668));
#133374=CARTESIAN_POINT('Ctrl Pts',(64.8780635186918,-6.16447390476599,
67.2348206683706));
#133375=CARTESIAN_POINT('Ctrl Pts',(64.8759438519186,-6.16439422531526,
67.2227994406676));
#133376=CARTESIAN_POINT('Ctrl Pts',(64.8738238574643,-6.16438935871099,
67.210776354591));
#133377=CARTESIAN_POINT('',(64.9200365392845,-6.46714802416996,67.2025868445748));
#133378=CARTESIAN_POINT('Origin',(65.8588874291605,-6.16436606275721,67.0386110313669));
#133379=CARTESIAN_POINT('Ctrl Pts',(65.0995290409546,-6.72702913922128,
68.2204986910971));
#133380=CARTESIAN_POINT('Ctrl Pts',(65.0978779672016,-6.72101820418093,
68.2111349864784));
#133381=CARTESIAN_POINT('Ctrl Pts',(65.0962045410388,-6.71510725237692,
68.201644515001));
#133382=CARTESIAN_POINT('Ctrl Pts',(65.0945101637993,-6.70929906104744,
68.1920352241046));
#133383=CARTESIAN_POINT('Ctrl Pts',(65.0900972320726,-6.69417187968862,
68.1670082444693));
#133384=CARTESIAN_POINT('Ctrl Pts',(65.0855421738897,-6.67974170153992,
68.1411752259264));
#133385=CARTESIAN_POINT('Ctrl Pts',(65.080865553793,-6.66602823420956,68.1146527954373));
#133386=CARTESIAN_POINT('Ctrl Pts',(65.0758187507953,-6.65122926260156,
68.0860309533949));
#133387=CARTESIAN_POINT('Ctrl Pts',(65.070630379487,-6.6372649565294,68.0566062374781));
#133388=CARTESIAN_POINT('Ctrl Pts',(65.065325250278,-6.62413396216025,68.0265193546337));
#133389=CARTESIAN_POINT('Ctrl Pts',(65.0596428831358,-6.61006924704979,
67.9942930491558));
#133390=CARTESIAN_POINT('Ctrl Pts',(65.0538265628448,-6.59696056768424,
67.9613070576571));
#133391=CARTESIAN_POINT('Ctrl Pts',(65.0479081195714,-6.58482980871447,
67.9277418979278));
#133392=CARTESIAN_POINT('Ctrl Pts',(65.0415529158574,-6.57180384210533,
67.8916997466531));
#133393=CARTESIAN_POINT('Ctrl Pts',(65.0350799603681,-6.55990545579126,
67.8549897918566));
#133394=CARTESIAN_POINT('Ctrl Pts',(65.0285101932219,-6.54912373938078,
67.8177307908735));
#133395=CARTESIAN_POINT('Ctrl Pts',(65.021398112376,-6.53745202605182,67.7773961760644));
#133396=CARTESIAN_POINT('Ctrl Pts',(65.0141725772018,-6.5270889468045,67.7364181297901));
#133397=CARTESIAN_POINT('Ctrl Pts',(65.0068585115159,-6.51800755521313,
67.6949380020386));
#133398=CARTESIAN_POINT('Ctrl Pts',(64.9988940986838,-6.50811867058614,
67.6497695723414));
#133399=CARTESIAN_POINT('Ctrl Pts',(64.9908247115997,-6.49974953548232,
67.6040058040826));
#133400=CARTESIAN_POINT('Ctrl Pts',(64.9826739639034,-6.49283962908175,
67.5577806168571));
#133401=CARTESIAN_POINT('Ctrl Pts',(64.9737677268307,-6.48528924636276,
67.5072708364669));
#133402=CARTESIAN_POINT('Ctrl Pts',(64.9647643475857,-6.47948113969311,
67.4562101354345));
#133403=CARTESIAN_POINT('Ctrl Pts',(64.9556971386543,-6.47530096076753,
67.4047874382661));
#133404=CARTESIAN_POINT('Ctrl Pts',(64.945774321196,-6.47072632785289,67.3485123440143));
#133405=CARTESIAN_POINT('Ctrl Pts',(64.9357750593742,-6.46810135045388,
67.2918037122387));
#133406=CARTESIAN_POINT('Ctrl Pts',(64.9257374667552,-6.46736283728807,
67.2348776957069));
#133407=CARTESIAN_POINT('Ctrl Pts',(64.9238407956026,-6.4672232902203,67.224121139082));
#133408=CARTESIAN_POINT('Ctrl Pts',(64.9219427574521,-6.4671510987288,67.2133568298243));
#133409=CARTESIAN_POINT('Ctrl Pts',(64.9200435026063,-6.46714577790044,
67.2025856178632));
#133410=CARTESIAN_POINT('Origin',(27.4324635166691,-5.,72.98888938658));
#133411=CARTESIAN_POINT('Origin',(-6.16760765460691,-5.,58.73107688658));
#133412=CARTESIAN_POINT('Origin',(-7.28284733203891,-5.,84.2626284592));
#133413=CARTESIAN_POINT('Origin',(1.07038457110909,-5.,122.41156512159));
#133414=CARTESIAN_POINT('',(22.0949841886482,-5.0000000038066,58.2694426477661));
#133415=CARTESIAN_POINT('Ctrl Pts',(21.7837562285525,-5.99999999944872,
59.2197092315316));
#133416=CARTESIAN_POINT('Ctrl Pts',(21.7975260636522,-5.9999985274307,59.1775705921136));
#133417=CARTESIAN_POINT('Ctrl Pts',(21.8113023518639,-5.99704480733659,
59.1354341304315));
#133418=CARTESIAN_POINT('Ctrl Pts',(21.8249621981295,-5.99116480402708,
59.0936711320751));
#133419=CARTESIAN_POINT('Ctrl Pts',(21.8386209201063,-5.98528528467776,
59.0519115710685));
#133420=CARTESIAN_POINT('Ctrl Pts',(21.8521630766078,-5.97648002554931,
59.0105258475984));
#133421=CARTESIAN_POINT('Ctrl Pts',(21.8654679408015,-5.96482663022172,
58.9698786061037));
#133422=CARTESIAN_POINT('Ctrl Pts',(21.878776121166,-5.95317033034366,58.9292212334874));
#133423=CARTESIAN_POINT('Ctrl Pts',(21.891846751647,-5.9386645937448,58.8893031360823));
#133424=CARTESIAN_POINT('Ctrl Pts',(21.9045632718707,-5.92143739888266,
58.8504762134119));
#133425=CARTESIAN_POINT('Ctrl Pts',(21.9172773736486,-5.90421348031269,
58.8116566749002));
#133426=CARTESIAN_POINT('Ctrl Pts',(21.929637367193,-5.88426931977393,58.7739283008067));
#133427=CARTESIAN_POINT('Ctrl Pts',(21.9415330544524,-5.86178085100885,
58.7376235503012));
#133428=CARTESIAN_POINT('Ctrl Pts',(21.9534307647554,-5.83928855773558,
58.7013126256175));
#133429=CARTESIAN_POINT('Ctrl Pts',(21.9648638862721,-5.81425132436283,
58.6664261886119));
#133430=CARTESIAN_POINT('Ctrl Pts',(21.9757303953022,-5.78689011291116,
58.6332717274391));
#133431=CARTESIAN_POINT('Ctrl Pts',(21.9855638438665,-5.76213008513021,
58.6032692042997));
#133432=CARTESIAN_POINT('Ctrl Pts',(21.9949333352515,-5.73546765831612,
58.5746848681192));
#133433=CARTESIAN_POINT('Ctrl Pts',(22.0037703020811,-5.70709562702803,
58.5477250946227));
#133434=CARTESIAN_POINT('Ctrl Pts',(22.0135389068795,-5.67573247196329,
58.5179230847457));
#133435=CARTESIAN_POINT('Ctrl Pts',(22.0226565265249,-5.64228005043222,
58.4901071089335));
#133436=CARTESIAN_POINT('Ctrl Pts',(22.0310426905364,-5.60703366985993,
58.4645226233129));
#133437=CARTESIAN_POINT('Ctrl Pts',(22.0394282631326,-5.57178977495957,
58.4389399419808));
#133438=CARTESIAN_POINT('Ctrl Pts',(22.0470823961994,-5.53475254125243,
58.4155887017076));
#133439=CARTESIAN_POINT('Ctrl Pts',(22.0539375354772,-5.49624883268982,
58.3946749534964));
#133440=CARTESIAN_POINT('Ctrl Pts',(22.060794398555,-5.4577354419469,58.3737559462936));
#133441=CARTESIAN_POINT('Ctrl Pts',(22.0668517939827,-5.41775523860441,
58.3552758767621));
#133442=CARTESIAN_POINT('Ctrl Pts',(22.0720562180904,-5.37666121128741,
58.3393979301013));
#133443=CARTESIAN_POINT('Ctrl Pts',(22.0772596369718,-5.33557512121761,
58.3235230502412));
#133444=CARTESIAN_POINT('Ctrl Pts',(22.0816103602574,-5.29337606565423,
58.3102494521123));
#133445=CARTESIAN_POINT('Ctrl Pts',(22.0850699519827,-5.25043647287593,
58.299694352261));
#133446=CARTESIAN_POINT('Ctrl Pts',(22.088530064537,-5.20749041569762,58.2891376633777));
#133447=CARTESIAN_POINT('Ctrl Pts',(22.0910987406586,-5.16380404500724,
58.2813004028194));
#133448=CARTESIAN_POINT('Ctrl Pts',(22.0927532489339,-5.11976304124748,
58.276251875659));
#133449=CARTESIAN_POINT('Ctrl Pts',(22.0942457554333,-5.08003432829404,
58.2716976768609));
#133450=CARTESIAN_POINT('Ctrl Pts',(22.0949945426852,-5.04001743309234,
58.2694122459578));
#133451=CARTESIAN_POINT('Ctrl Pts',(22.0949941775792,-5.00000000409752,
58.2694121261103));
#133452=CARTESIAN_POINT('',(-2.29973550255637,-5.,54.9957487971611));
#133453=CARTESIAN_POINT('Origin',(1.07038457110909,-5.,122.41156512159));
#133454=CARTESIAN_POINT('Origin',(-2.24980779825091,-5.,55.99450163162));
#133455=CARTESIAN_POINT('Origin',(-2.02513312664091,-5.,60.48888938658));
#133456=CARTESIAN_POINT('Origin',(-2.02513312664091,-5.,60.48888938658));
#133457=CARTESIAN_POINT('Origin',(-2.02513312664091,25.,60.48888938658));
#133458=CARTESIAN_POINT('',(-2.29973550255644,5.,54.9957487971611));
#133459=CARTESIAN_POINT('',(-2.29973550107091,-5.,54.99574879709));
#133460=CARTESIAN_POINT('Origin',(-2.02513312664091,5.,60.48888938658));
#133461=CARTESIAN_POINT('Origin',(-2.02513312664091,5.,60.48888938658));
#133462=CARTESIAN_POINT('Origin',(-6.16760765460691,5.,58.73107688658));
#133463=CARTESIAN_POINT('Origin',(-2.24980779825091,5.,55.99450163162));
#133464=CARTESIAN_POINT('Origin',(-8.75366715310791,111.0724296188,85.97453149762));
#133465=CARTESIAN_POINT('Origin',(14.4385554303262,1.4210854715202E-14,
81.8851169135651));
#133466=CARTESIAN_POINT('',(-6.54682287186491,5.,85.58540530862));
#133467=CARTESIAN_POINT('Origin',(26.6903689106391,-17.,82.263358164095));
#133468=CARTESIAN_POINT('',(23.6515258014716,7.5,65.0292224863863));
#133469=CARTESIAN_POINT('',(23.6515258014821,10.9472980747274,65.0292224863845));
#133470=CARTESIAN_POINT('',(23.6515258014693,-17.,65.0292224863868));
#133471=CARTESIAN_POINT('',(22.9296816314691,7.5,60.93544076844));
#133472=CARTESIAN_POINT('',(22.9296816314691,7.5,60.93544076844));
#133473=CARTESIAN_POINT('',(22.9296816314691,7.5,60.93544076844));
#133474=CARTESIAN_POINT('',(22.9354959621264,10.3319876690517,60.9684154762107));
#133475=CARTESIAN_POINT('',(22.9296818159191,10.33198965144,60.93544181454));
#133476=CARTESIAN_POINT('Ctrl Pts',(22.9354959621287,10.3319876695089,60.9684154762103));
#133477=CARTESIAN_POINT('Ctrl Pts',(22.9457594205585,10.3319918659453,61.0266224414067));
#133478=CARTESIAN_POINT('Ctrl Pts',(22.9561975687024,10.3325157444919,61.0858201212103));
#133479=CARTESIAN_POINT('Ctrl Pts',(22.9668129917587,10.3335903239921,61.1460231769825));
#133480=CARTESIAN_POINT('Ctrl Pts',(22.9892670680594,10.3358633083056,61.2733665716517));
#133481=CARTESIAN_POINT('Ctrl Pts',(23.0125146365289,10.3406023501125,61.4052100839497));
#133482=CARTESIAN_POINT('Ctrl Pts',(23.0365857422537,10.3481011670225,61.5417241083182));
#133483=CARTESIAN_POINT('Ctrl Pts',(23.0416535630085,10.3496799337151,61.5704651480497));
#133484=CARTESIAN_POINT('Ctrl Pts',(23.0467578645404,10.3513809019802,61.5994130805518));
#133485=CARTESIAN_POINT('Ctrl Pts',(23.0518988894436,10.3532065840058,61.62856928162));
#133486=CARTESIAN_POINT('Ctrl Pts',(23.0639202065515,10.3574755970881,61.696745558782));
#133487=CARTESIAN_POINT('Ctrl Pts',(23.0761427749971,10.3624230092554,61.7660631888724));
#133488=CARTESIAN_POINT('Ctrl Pts',(23.0885557652515,10.3680698206311,61.8364607547481));
#133489=CARTESIAN_POINT('Ctrl Pts',(23.1081071729758,10.3769639798374,61.9473422977947));
#133490=CARTESIAN_POINT('Ctrl Pts',(23.1281309847519,10.3875956593929,62.0609029775064));
#133491=CARTESIAN_POINT('Ctrl Pts',(23.1485877002943,10.4000241324366,62.176918776601));
#133492=CARTESIAN_POINT('Ctrl Pts',(23.1595523603548,10.4066857092528,62.2391024539405));
#133493=CARTESIAN_POINT('Ctrl Pts',(23.1706413774056,10.4138626166885,62.301991394839));
#133494=CARTESIAN_POINT('Ctrl Pts',(23.1818485931706,10.4215577992017,62.3655506738587));
#133495=CARTESIAN_POINT('Ctrl Pts',(23.1956058466466,10.4310039077265,62.4435719353888));
#133496=CARTESIAN_POINT('Ctrl Pts',(23.2095416513106,10.4412362594231,62.5226058109224));
#133497=CARTESIAN_POINT('Ctrl Pts',(23.2236490156693,10.4522538270402,62.6026126499251));
#133498=CARTESIAN_POINT('Ctrl Pts',(23.2464420503796,10.4700547283803,62.7318783732788));
#133499=CARTESIAN_POINT('Ctrl Pts',(23.2696828767045,10.4899077486182,62.8636836491963));
#133500=CARTESIAN_POINT('Ctrl Pts',(23.2933466050056,10.5118045940982,62.9978873213132));
#133501=CARTESIAN_POINT('Ctrl Pts',(23.30336140994,10.521071630694,63.0546841024722));
#133502=CARTESIAN_POINT('Ctrl Pts',(23.3134519635772,10.5307041071535,63.1119104758642));
#133503=CARTESIAN_POINT('Ctrl Pts',(23.3236163926547,10.5406985620617,63.1695558176983));
#133504=CARTESIAN_POINT('Ctrl Pts',(23.339000040912,10.5558249580115,63.2568008223788));
#133505=CARTESIAN_POINT('Ctrl Pts',(23.3545532509111,10.571784067664,63.3450074594824));
#133506=CARTESIAN_POINT('Ctrl Pts',(23.3702657805519,10.5885526295178,63.4341176431629));
#133507=CARTESIAN_POINT('Ctrl Pts',(23.3946901195582,10.6146185176166,63.5726349529082));
#133508=CARTESIAN_POINT('Ctrl Pts',(23.4194993251193,10.6426424725186,63.7133349493283));
#133509=CARTESIAN_POINT('Ctrl Pts',(23.4446595190143,10.6725366399531,63.8560254995665));
#133510=CARTESIAN_POINT('Ctrl Pts',(23.4549180172403,10.6847253084854,63.9142043340614));
#133511=CARTESIAN_POINT('Ctrl Pts',(23.4652348809764,10.6972242889174,63.9727141758234));
#133512=CARTESIAN_POINT('Ctrl Pts',(23.4756078830168,10.7100251716415,64.0315423937084));
#133513=CARTESIAN_POINT('Ctrl Pts',(23.4925128798764,10.7308869126697,64.1274153950565));
#133514=CARTESIAN_POINT('Ctrl Pts',(23.5095672887138,10.7525581219184,64.2241357538275));
#133515=CARTESIAN_POINT('Ctrl Pts',(23.5267450050852,10.7749698010488,64.3215554243934));
#133516=CARTESIAN_POINT('Ctrl Pts',(23.5524968689719,10.8085681268073,64.4676015018837));
#133517=CARTESIAN_POINT('Ctrl Pts',(23.5785257124883,10.8438323226742,64.6152184088107));
#133518=CARTESIAN_POINT('Ctrl Pts',(23.6047484448564,10.8805589711191,64.7639349141785));
#133519=CARTESIAN_POINT('Ctrl Pts',(23.6150258236674,10.894953111029,64.8222208257935));
#133520=CARTESIAN_POINT('Ctrl Pts',(23.6253330169625,10.9095713396704,64.8806758237816));
#133521=CARTESIAN_POINT('Ctrl Pts',(23.6356651406205,10.9243993782852,64.939272208841));
#133522=CARTESIAN_POINT('Ctrl Pts',(23.6409456318988,10.9319776198134,64.9692193630264));
#133523=CARTESIAN_POINT('Ctrl Pts',(23.6462325813711,10.9396109140533,64.9992031434345));
#133524=CARTESIAN_POINT('Ctrl Pts',(23.6515258014821,10.9472980747274,65.0292224863845));
#133525=CARTESIAN_POINT('Origin',(21.3942017988391,7.5,60.86545763396));
#133526=CARTESIAN_POINT('Origin',(22.1743141719575,7.5,65.289694752886));
#133527=CARTESIAN_POINT('Origin',(21.4524700019691,7.5,61.19591303503));
#133528=CARTESIAN_POINT('Ctrl Pts',(16.7315271092291,25.77957474242,75.8056538642681));
#133529=CARTESIAN_POINT('Ctrl Pts',(16.8902739491491,25.78276104928,76.726755143248));
#133530=CARTESIAN_POINT('Ctrl Pts',(17.4170423638691,25.68741378017,79.011155596728));
#133531=CARTESIAN_POINT('Ctrl Pts',(18.6971928491291,25.1486541372,82.327981456666));
#133532=CARTESIAN_POINT('Ctrl Pts',(20.3541926191191,24.21296098443,85.29757061493));
#133533=CARTESIAN_POINT('Ctrl Pts',(21.9876235905991,23.12636897321,87.62326197554));
#133534=CARTESIAN_POINT('Ctrl Pts',(23.5303110581191,21.96974605327,89.49482082956));
#133535=CARTESIAN_POINT('Ctrl Pts',(25.0147293345491,20.73535636643,91.08394632963));
#133536=CARTESIAN_POINT('Ctrl Pts',(26.4477039632491,19.42122041898,92.4661164628101));
#133537=CARTESIAN_POINT('Ctrl Pts',(27.8040593501691,18.0525443245,93.66246634875));
#133538=CARTESIAN_POINT('Ctrl Pts',(29.0976297887891,16.61722673478,94.7173081814599));
#133539=CARTESIAN_POINT('Ctrl Pts',(30.3859883571291,15.03805899871,95.692928827));
#133540=CARTESIAN_POINT('Ctrl Pts',(31.6846191544191,13.2490375268,96.6017522016999));
#133541=CARTESIAN_POINT('Ctrl Pts',(32.9283641549091,11.27078505501,97.39922069443));
#133542=CARTESIAN_POINT('Ctrl Pts',(34.0024905191591,9.24026551673301,98.0256740975701));
#133543=CARTESIAN_POINT('Ctrl Pts',(34.8835248980591,7.19980133487202,98.4916705583199));
#133544=CARTESIAN_POINT('Ctrl Pts',(35.5865206621291,5.09129120886101,98.8275149094299));
#133545=CARTESIAN_POINT('Ctrl Pts',(36.0644764908891,2.94897602587201,99.0360923986901));
#133546=CARTESIAN_POINT('Ctrl Pts',(36.2175390832591,1.50759720120401,99.1082321058299));
#133547=CARTESIAN_POINT('Ctrl Pts',(36.2511547877691,0.817200229439614,
99.1309346670101));
#133548=CARTESIAN_POINT('Ctrl Pts',(16.5657307648391,19.34436604072,75.8499470296021));
#133549=CARTESIAN_POINT('Ctrl Pts',(16.7027032210391,19.34727467235,76.647687526976));
#133550=CARTESIAN_POINT('Ctrl Pts',(17.1758927443291,19.26031994756,78.623309386718));
#133551=CARTESIAN_POINT('Ctrl Pts',(18.3744374416091,18.77127275203,81.451029832546));
#133552=CARTESIAN_POINT('Ctrl Pts',(19.9464727370091,17.9342387447,83.90371085737));
#133553=CARTESIAN_POINT('Ctrl Pts',(21.5011129654591,16.97934371574,85.75395997948));
#133554=CARTESIAN_POINT('Ctrl Pts',(22.9701058542891,15.98027083986,87.18714704112));
#133555=CARTESIAN_POINT('Ctrl Pts',(24.3829496628191,14.93205005415,88.35697360021));
#133556=CARTESIAN_POINT('Ctrl Pts',(25.7455828440791,13.83506997747,89.33304121868));
#133557=CARTESIAN_POINT('Ctrl Pts',(27.0338235509591,12.71200151814,90.14134599812));
#133558=CARTESIAN_POINT('Ctrl Pts',(28.2606989614091,11.55431815225,90.82076231519));
#133559=CARTESIAN_POINT('Ctrl Pts',(29.4805515038791,10.30341122855,91.41513380966));
#133560=CARTESIAN_POINT('Ctrl Pts',(30.7073346580191,8.91606547149402,91.92891446662));
#133561=CARTESIAN_POINT('Ctrl Pts',(31.8785519228191,7.42186252822301,92.33283454608));
#133562=CARTESIAN_POINT('Ctrl Pts',(32.8858034194691,5.93611159812901,92.60136415471));
#133563=CARTESIAN_POINT('Ctrl Pts',(33.7077479385191,4.49637949617201,92.75525280737));
#133564=CARTESIAN_POINT('Ctrl Pts',(34.3594477230791,3.06936714330901,92.82352537927));
#133565=CARTESIAN_POINT('Ctrl Pts',(34.7987841186091,1.68933111557601,92.83289655037));
#133566=CARTESIAN_POINT('Ctrl Pts',(34.9379185776691,0.799874261541514,
92.83329103801));
#133567=CARTESIAN_POINT('Ctrl Pts',(34.9680789093591,0.377412282680914,
92.8379453280101));
#133568=CARTESIAN_POINT('Ctrl Pts',(21.0648245475691,14.80356751578,75.088574197736));
#133569=CARTESIAN_POINT('Ctrl Pts',(21.1562893009191,14.80542149402,75.624814594272));
#133570=CARTESIAN_POINT('Ctrl Pts',(21.4915191590391,14.74994267437,76.949273101324));
#133571=CARTESIAN_POINT('Ctrl Pts',(22.4029329257891,14.43645292234,78.850401178621));
#133572=CARTESIAN_POINT('Ctrl Pts',(23.6728411634791,13.89196197301,80.525093828825));
#133573=CARTESIAN_POINT('Ctrl Pts',(24.9938756020691,13.25961078348,81.813737319686));
#133574=CARTESIAN_POINT('Ctrl Pts',(26.2936708744891,12.5864534242,82.832583999374));
#133575=CARTESIAN_POINT('Ctrl Pts',(27.5870975206191,11.86798256843,83.68225710374));
#133576=CARTESIAN_POINT('Ctrl Pts',(28.8717832775691,11.10303997034,84.4077907698501));
#133577=CARTESIAN_POINT('Ctrl Pts',(30.1179515221891,10.306293006,85.0241310085501));
#133578=CARTESIAN_POINT('Ctrl Pts',(31.3323143284891,9.47069299188402,85.55730149859));
#133579=CARTESIAN_POINT('Ctrl Pts',(32.5667384548491,8.55128051724301,86.04034306038));
#133580=CARTESIAN_POINT('Ctrl Pts',(33.8387497469191,7.50960072681501,86.47900335892));
#133581=CARTESIAN_POINT('Ctrl Pts',(35.0880429676691,6.35762147075602,86.85127259704));
#133582=CARTESIAN_POINT('Ctrl Pts',(36.1977391360291,5.17506491544101,87.13119140558));
#133583=CARTESIAN_POINT('Ctrl Pts',(37.1355508905091,3.98655984369701,87.32815521361));
#133584=CARTESIAN_POINT('Ctrl Pts',(37.9083300473991,2.75824145710901,87.46012871543));
#133585=CARTESIAN_POINT('Ctrl Pts',(38.4524854874891,1.51002426311401,87.5351100622101));
#133586=CARTESIAN_POINT('Ctrl Pts',(38.6303209632591,0.670091817760814,
87.56162468684));
#133587=CARTESIAN_POINT('Ctrl Pts',(38.6686985395891,0.267767345835414,
87.57156379687));
#133588=CARTESIAN_POINT('Ctrl Pts',(27.4060955579191,15.00605745049,73.9992175459301));
#133589=CARTESIAN_POINT('Ctrl Pts',(27.4568706345291,15.00674148237,74.299882608077));
#133590=CARTESIAN_POINT('Ctrl Pts',(27.6563153791591,14.98607407549,75.03933020766));
#133591=CARTESIAN_POINT('Ctrl Pts',(28.2552178354491,14.86384274642,76.157719195735));
#133592=CARTESIAN_POINT('Ctrl Pts',(29.1953897033191,14.62223845856,77.28144993045));
#133593=CARTESIAN_POINT('Ctrl Pts',(30.2745666151391,14.3009152899,78.274673456111));
#133594=CARTESIAN_POINT('Ctrl Pts',(31.4158151207291,13.9175608677,79.163166612491));
#133595=CARTESIAN_POINT('Ctrl Pts',(32.6169037455491,13.46553722345,79.992694706598));
#133596=CARTESIAN_POINT('Ctrl Pts',(33.8649399941491,12.93919476597,80.780446952018));
#133597=CARTESIAN_POINT('Ctrl Pts',(35.1214740837291,12.3447503952,81.5213409775531));
#133598=CARTESIAN_POINT('Ctrl Pts',(36.3853570661891,11.67360909312,82.229199358404));
#133599=CARTESIAN_POINT('Ctrl Pts',(37.7082882345091,10.88094645291,82.940678146904));
#133600=CARTESIAN_POINT('Ctrl Pts',(39.1142274982291,9.91205347783502,83.67127064968));
#133601=CARTESIAN_POINT('Ctrl Pts',(40.5432158335391,8.74576233655301,84.3936442258099));
#133602=CARTESIAN_POINT('Ctrl Pts',(41.8604028480391,7.43460302127903,85.0471196915701));
#133603=CARTESIAN_POINT('Ctrl Pts',(43.0163443071791,5.99020112655302,85.6153164434601));
#133604=CARTESIAN_POINT('Ctrl Pts',(44.0066134889891,4.35311312370201,86.1022978834));
#133605=CARTESIAN_POINT('Ctrl Pts',(44.7332634147991,2.52355184883601,86.4665423458501));
#133606=CARTESIAN_POINT('Ctrl Pts',(44.9781481988991,1.19967484028401,86.60065479763));
#133607=CARTESIAN_POINT('Ctrl Pts',(45.0312601718991,0.557056200456914,
86.6358961446099));
#133608=CARTESIAN_POINT('',(39.4126121040966,0.605802323126824,89.303174770965));
#133609=CARTESIAN_POINT('Origin',(46.4992391344146,1.66064392498492,96.9794802088298));
#133610=CARTESIAN_POINT('Ctrl Pts',(37.5050940990142,10.7061722565098,83.1298152725198));
#133611=CARTESIAN_POINT('Ctrl Pts',(37.552217423979,10.5471910708906,83.2904075500772));
#133612=CARTESIAN_POINT('Ctrl Pts',(37.599378677488,10.3862893955955,83.4509114661969));
#133613=CARTESIAN_POINT('Ctrl Pts',(37.6466151200992,10.2232847373308,83.6111957660706));
#133614=CARTESIAN_POINT('Ctrl Pts',(37.6923853029459,10.0653398837131,83.766504703559));
#133615=CARTESIAN_POINT('Ctrl Pts',(37.7382264410281,9.90542034687216,83.9216073065561));
#133616=CARTESIAN_POINT('Ctrl Pts',(37.7841362342735,9.74333882261691,84.0763598865346));
#133617=CARTESIAN_POINT('Ctrl Pts',(37.8126492894712,9.64267534493789,84.1724715991559));
#133618=CARTESIAN_POINT('Ctrl Pts',(37.8411880929764,9.54117752683905,84.2684478260362));
#133619=CARTESIAN_POINT('Ctrl Pts',(37.86974377233,9.43879676405171,84.3642495668624));
#133620=CARTESIAN_POINT('Ctrl Pts',(37.9139822359765,9.28018846772753,84.5126656411683));
#133621=CARTESIAN_POINT('Ctrl Pts',(37.9582636609881,9.11946131063388,84.6606639083057));
#133622=CARTESIAN_POINT('Ctrl Pts',(38.002495868906,8.95642861022755,84.8080614815933));
#133623=CARTESIAN_POINT('Ctrl Pts',(38.045356649548,8.79845076696536,84.950888967564));
#133624=CARTESIAN_POINT('Ctrl Pts',(38.0881714412079,8.63830788130787,85.093152305827));
#133625=CARTESIAN_POINT('Ctrl Pts',(38.1308108615095,8.47582372812318,85.2346675575267));
#133626=CARTESIAN_POINT('Ctrl Pts',(38.1419845864,8.43324450884893,85.2717518442998));
#133627=CARTESIAN_POINT('Ctrl Pts',(38.1531460090944,8.39050448870853,85.3087846687433));
#133628=CARTESIAN_POINT('Ctrl Pts',(38.1642922319669,8.34760045463328,85.3457625296133));
#133629=CARTESIAN_POINT('Ctrl Pts',(38.2000540816169,8.20994596543751,85.4644033208424));
#133630=CARTESIAN_POINT('Ctrl Pts',(38.2356900159584,8.07059403849077,85.5824775687261));
#133631=CARTESIAN_POINT('Ctrl Pts',(38.2712115945426,7.92939023146871,85.6998388074438));
#133632=CARTESIAN_POINT('Ctrl Pts',(38.3077375849418,7.78419373105429,85.8205185646365));
#133633=CARTESIAN_POINT('Ctrl Pts',(38.3441432944549,7.63703875702918,85.9404442433346));
#133634=CARTESIAN_POINT('Ctrl Pts',(38.3803739820712,7.48776076653468,86.0594246406868));
#133635=CARTESIAN_POINT('Ctrl Pts',(38.4166046696875,7.33848277604017,86.1784050380389));
#133636=CARTESIAN_POINT('Ctrl Pts',(38.4526608349029,7.18708149166657,86.2964401025204));
#133637=CARTESIAN_POINT('Ctrl Pts',(38.4884369449348,7.03338765491548,86.4133197013914));
#133638=CARTESIAN_POINT('Ctrl Pts',(38.5205640696361,6.89536982528776,86.5182781623482));
#133639=CARTESIAN_POINT('Ctrl Pts',(38.5524923683579,6.75549952963279,86.6222935863113));
#133640=CARTESIAN_POINT('Ctrl Pts',(38.5841939839849,6.61362336899418,86.7251659839855));
#133641=CARTESIAN_POINT('Ctrl Pts',(38.5988420549672,6.54806796966731,86.7726992769566));
#133642=CARTESIAN_POINT('Ctrl Pts',(38.6134410812288,6.48208423576418,86.8199882613318));
#133643=CARTESIAN_POINT('Ctrl Pts',(38.6279847854992,6.41565671969214,86.8670118300703));
#133644=CARTESIAN_POINT('Ctrl Pts',(38.6340595331057,6.38791066636475,86.8866530649533));
#133645=CARTESIAN_POINT('Ctrl Pts',(38.6401246006179,6.36008718736758,86.9062479834196));
#133646=CARTESIAN_POINT('Ctrl Pts',(38.646179288585,6.33218524996709,86.9257950052816));
#133647=CARTESIAN_POINT('Ctrl Pts',(38.6721403751459,6.21254826520258,87.0096080653973));
#133648=CARTESIAN_POINT('Ctrl Pts',(38.6979186362708,6.09146585004635,87.092540259136));
#133649=CARTESIAN_POINT('Ctrl Pts',(38.7234769891415,5.96883836752666,87.1744532102944));
#133650=CARTESIAN_POINT('Ctrl Pts',(38.7362561655769,5.90752462626682,87.2154096858736));
#133651=CARTESIAN_POINT('Ctrl Pts',(38.7489802003326,5.8458244661527,87.2561111365291));
#133652=CARTESIAN_POINT('Ctrl Pts',(38.7616433871205,5.78372476399081,87.2965386867928));
#133653=CARTESIAN_POINT('Ctrl Pts',(38.7679749805145,5.75267491290986,87.3167524619246));
#133654=CARTESIAN_POINT('Ctrl Pts',(38.7742913485755,5.72152516801141,87.3368977468268));
#133655=CARTESIAN_POINT('Ctrl Pts',(38.7805917707051,5.69027391197471,87.3569719794879));
#133656=CARTESIAN_POINT('Ctrl Pts',(38.7837419817699,5.67464828395636,87.3670090958184));
#133657=CARTESIAN_POINT('Ctrl Pts',(38.7868882053342,5.6589972777635,87.3770284480717));
#133658=CARTESIAN_POINT('Ctrl Pts',(38.7900304108563,5.64332074742208,87.387029619085));
#133659=CARTESIAN_POINT('Ctrl Pts',(38.7916015136173,5.63548248225137,87.3920302045916));
#133660=CARTESIAN_POINT('Ctrl Pts',(38.793171611861,5.62763783596085,87.3970262447299));
#133661=CARTESIAN_POINT('Ctrl Pts',(38.7947406975676,5.61978678615472,87.4020176927));
#133662=CARTESIAN_POINT('Ctrl Pts',(38.7963097832741,5.61193573634858,87.4070091406701));
#133663=CARTESIAN_POINT('Ctrl Pts',(38.7976672957473,5.60513493051777,87.4113265501283));
#133664=CARTESIAN_POINT('Ctrl Pts',(38.7994449103682,5.59621440491363,87.4169782110083));
#133665=CARTESIAN_POINT('Ctrl Pts',(38.8268161624268,5.4588584493859,87.5040010294981));
#133666=CARTESIAN_POINT('Ctrl Pts',(38.8527567462118,5.32506777322639,87.5861152448737));
#133667=CARTESIAN_POINT('Ctrl Pts',(38.8772743032886,5.19511788675176,87.6635181014004));
#133668=CARTESIAN_POINT('Ctrl Pts',(38.8897280675518,5.12910946482259,87.7028351069842));
#133669=CARTESIAN_POINT('Ctrl Pts',(38.9018154030616,5.06409193786023,87.7409370043211));
#133670=CARTESIAN_POINT('Ctrl Pts',(38.9135415606847,5.00010079004935,87.7778523004227));
#133671=CARTESIAN_POINT('Ctrl Pts',(38.9380151229955,4.86654541806606,87.8548978961243));
#133672=CARTESIAN_POINT('Ctrl Pts',(38.9609123280281,4.73746215436914,87.9267734403203));
#133673=CARTESIAN_POINT('Ctrl Pts',(38.9823131061757,4.61317397417699,87.9937636561146));
#133674=CARTESIAN_POINT('Ctrl Pts',(39.0061356217478,4.4748211961784,88.0683345641409));
#133675=CARTESIAN_POINT('Ctrl Pts',(39.0281041862561,4.34241024754061,88.1368526571142));
#133676=CARTESIAN_POINT('Ctrl Pts',(39.0483876372309,4.21636440778313,88.1997316609947));
#133677=CARTESIAN_POINT('Ctrl Pts',(39.0554044509918,4.17276037886256,88.2214838894616));
#133678=CARTESIAN_POINT('Ctrl Pts',(39.0622200434846,4.12991789653019,88.2425613851375));
#133679=CARTESIAN_POINT('Ctrl Pts',(39.0688426197856,4.08785393259761,88.2629815187296));
#133680=CARTESIAN_POINT('Ctrl Pts',(39.0918493621927,3.94172427869416,88.3339207925283));
#133681=CARTESIAN_POINT('Ctrl Pts',(39.1124319604812,3.80500972636446,88.3969883469281));
#133682=CARTESIAN_POINT('Ctrl Pts',(39.1307949414565,3.67849151113324,88.4530154364568));
#133683=CARTESIAN_POINT('Ctrl Pts',(39.1384490160761,3.6257560722948,88.4763686994453));
#133684=CARTESIAN_POINT('Ctrl Pts',(39.1457180528506,3.57479184947902,88.4984987120231));
#133685=CARTESIAN_POINT('Ctrl Pts',(39.1526181182454,3.52565431267108,88.519464946207));
#133686=CARTESIAN_POINT('Ctrl Pts',(39.153421600476,3.51993246288875,88.5219063718521));
#133687=CARTESIAN_POINT('Ctrl Pts',(39.1542200793681,3.51423538159438,88.5243320162628));
#133688=CARTESIAN_POINT('Ctrl Pts',(39.1550135811842,3.50856315513645,88.5267419732416));
#133689=CARTESIAN_POINT('Ctrl Pts',(39.1669917121232,3.42293931679378,88.563120945114));
#133690=CARTESIAN_POINT('Ctrl Pts',(39.1778340435463,3.34297408472003,88.5959321303305));
#133691=CARTESIAN_POINT('Ctrl Pts',(39.1876199347076,3.26891537418542,88.6255169987751));
#133692=CARTESIAN_POINT('Ctrl Pts',(39.1925128802883,3.23188601891811,88.6403094329974));
#133693=CARTESIAN_POINT('Ctrl Pts',(39.1971416061376,3.19633263902273,88.6542952132579));
#133694=CARTESIAN_POINT('Ctrl Pts',(39.2015152946873,3.16228236620596,88.6675157076164));
#133695=CARTESIAN_POINT('Ctrl Pts',(39.2037021389622,3.14525722979757,88.6741259547957));
#133696=CARTESIAN_POINT('Ctrl Pts',(39.2058252034364,3.1286078582077,88.680544856444));
#133697=CARTESIAN_POINT('Ctrl Pts',(39.2078855970158,3.11233737620093,88.686777438232));
#133698=CARTESIAN_POINT('Ctrl Pts',(39.2089157938054,3.10420213519754,88.6898937291259));
#133699=CARTESIAN_POINT('Ctrl Pts',(39.2099303213754,3.09616161571765,88.6929634382969));
#133700=CARTESIAN_POINT('Ctrl Pts',(39.2109293128743,3.08821619883033,88.6959871818242));
#133701=CARTESIAN_POINT('Ctrl Pts',(39.2114288086237,3.08424349038668,88.6974990535879));
#133702=CARTESIAN_POINT('Ctrl Pts',(39.2119244202558,3.08029455753482,88.6989994338242));
#133703=CARTESIAN_POINT('Ctrl Pts',(39.2124161641733,3.07636944696151,88.7004883988127));
#133704=CARTESIAN_POINT('Ctrl Pts',(39.2126620361321,3.07440689167485,88.7012328813069));
#133705=CARTESIAN_POINT('Ctrl Pts',(39.2129069411559,3.07245029195421,88.7019745099817));
#133706=CARTESIAN_POINT('Ctrl Pts',(39.2131508812819,3.07049965357541,88.7027132943232));
#133707=CARTESIAN_POINT('Ctrl Pts',(39.2133948214078,3.0685490151966,88.7034520786646));
#133708=CARTESIAN_POINT('Ctrl Pts',(39.2134400757702,3.0681882383282,88.7035890815634));
#133709=CARTESIAN_POINT('Ctrl Pts',(39.2138798089855,3.06466562821442,88.7049211238016));
#133710=CARTESIAN_POINT('Ctrl Pts',(39.2310447207238,2.9271611377798,88.756917167442));
#133711=CARTESIAN_POINT('Ctrl Pts',(39.247089602519,2.79108612147949,88.8053255292509));
#133712=CARTESIAN_POINT('Ctrl Pts',(39.2619938081742,2.65665221882818,88.8502537192043));
#133713=CARTESIAN_POINT('Ctrl Pts',(39.2771796828001,2.51967770046989,88.8960309901025));
#133714=CARTESIAN_POINT('Ctrl Pts',(39.2911813148946,2.38440688037919,88.9381956585786));
#133715=CARTESIAN_POINT('Ctrl Pts',(39.3040289835558,2.25105544495463,88.9768759642758));
#133716=CARTESIAN_POINT('Ctrl Pts',(39.3154345014117,2.13267270813758,89.011214405664));
#133717=CARTESIAN_POINT('Ctrl Pts',(39.3259313823954,2.01580250615974,89.0428071815956));
#133718=CARTESIAN_POINT('Ctrl Pts',(39.335574287149,1.90059075916109,89.0717500576461));
#133719=CARTESIAN_POINT('Ctrl Pts',(39.3393662685198,1.85528482599282,89.0831315707487));
#133720=CARTESIAN_POINT('Ctrl Pts',(39.3430265391906,1.81023531083248,89.0941033538999));
#133721=CARTESIAN_POINT('Ctrl Pts',(39.3465613453223,1.76545096114672,89.1046710760339));
#133722=CARTESIAN_POINT('Ctrl Pts',(39.3572631219915,1.62986442803529,89.1366653065426));
#133723=CARTESIAN_POINT('Ctrl Pts',(39.366770729011,1.49685015350463,89.1649482792311));
#133724=CARTESIAN_POINT('Ctrl Pts',(39.3751201764905,1.36667079983074,89.1898546186758));
#133725=CARTESIAN_POINT('Ctrl Pts',(39.3837779490806,1.2316842342166,89.2156806896215));
#133726=CARTESIAN_POINT('Ctrl Pts',(39.3911904902059,1.0997455921959,89.2378764788459));
#133727=CARTESIAN_POINT('Ctrl Pts',(39.3974554150243,0.971144094561306,
89.2568175177896));
#133728=CARTESIAN_POINT('Ctrl Pts',(39.4035460066799,0.846121172323219,
89.2752314871642));
#133729=CARTESIAN_POINT('Ctrl Pts',(39.4085526120063,0.724252072113412,
89.2905695595766));
#133730=CARTESIAN_POINT('Ctrl Pts',(39.4126121040966,0.605802323126824,
89.303174770965));
#133731=CARTESIAN_POINT('Ctrl Pts',(38.4618783725391,10.5104216086,82.548487971909));
#133732=CARTESIAN_POINT('Ctrl Pts',(38.5526802105791,10.01289241835,83.06345078517));
#133733=CARTESIAN_POINT('Ctrl Pts',(38.7398454136791,8.95695275023301,84.12491739878));
#133734=CARTESIAN_POINT('Ctrl Pts',(39.0045880266591,7.31849282792101,85.62634736661));
#133735=CARTESIAN_POINT('Ctrl Pts',(39.2417436224691,5.61044727625601,86.9713235856));
#133736=CARTESIAN_POINT('Ctrl Pts',(39.4296302152491,3.90871748337901,88.0368814033801));
#133737=CARTESIAN_POINT('Ctrl Pts',(39.5601688728291,2.20504120005801,88.77720291884));
#133738=CARTESIAN_POINT('Ctrl Pts',(39.6063198374691,1.00828919109001,89.0389380455399));
#133739=CARTESIAN_POINT('Ctrl Pts',(39.6165263283691,0.422474636108614,
89.0968219318599));
#133740=CARTESIAN_POINT('Ctrl Pts',(39.6168726794091,0.401711040790814,
89.09878618618));
#133741=CARTESIAN_POINT('Ctrl Pts',(37.3374165872391,11.41764504428,83.62342900089));
#133742=CARTESIAN_POINT('Ctrl Pts',(37.4297627814791,10.91166281239,84.1471502934));
#133743=CARTESIAN_POINT('Ctrl Pts',(37.6207808413991,9.83411841866803,85.2304675438201));
#133744=CARTESIAN_POINT('Ctrl Pts',(37.8940999251891,8.14335594153101,86.7805370947));
#133745=CARTESIAN_POINT('Ctrl Pts',(38.1435439664991,6.34856195272902,88.1952045512));
#133746=CARTESIAN_POINT('Ctrl Pts',(38.3465988703891,4.51349428134101,89.3467861359801));
#133747=CARTESIAN_POINT('Ctrl Pts',(38.4930032378491,2.61111516505002,90.1770865634601));
#133748=CARTESIAN_POINT('Ctrl Pts',(38.5466699117291,1.22869486492401,90.48144539536));
#133749=CARTESIAN_POINT('Ctrl Pts',(38.5585559689691,0.546009918402814,
90.54885457573));
#133750=CARTESIAN_POINT('Ctrl Pts',(38.5589593261391,0.521805644301214,
90.5511421279301));
#133751=CARTESIAN_POINT('Ctrl Pts',(35.6787452111791,10.79042214836,83.3097995382401));
#133752=CARTESIAN_POINT('Ctrl Pts',(35.7700236909691,10.29028405701,83.82746552121));
#133753=CARTESIAN_POINT('Ctrl Pts',(35.9583780189791,9.22767642310003,84.8956759973201));
#133754=CARTESIAN_POINT('Ctrl Pts',(36.2257676275791,7.57307412284002,86.41211782328));
#133755=CARTESIAN_POINT('Ctrl Pts',(36.4667158628191,5.83825500221001,87.77860316929));
#133756=CARTESIAN_POINT('Ctrl Pts',(36.6592839211891,4.09537252689102,88.8707108977601));
#133757=CARTESIAN_POINT('Ctrl Pts',(36.7947192857491,2.33036967472801,89.6388030185));
#133758=CARTESIAN_POINT('Ctrl Pts',(36.8431898582791,1.07631400748201,89.91369329529));
#133759=CARTESIAN_POINT('Ctrl Pts',(36.8539147214691,0.460601898215214,
89.9745170169101));
#133760=CARTESIAN_POINT('Ctrl Pts',(36.8542786665691,0.438776390386414,
89.9765810521401));
#133761=CARTESIAN_POINT('Ctrl Pts',(35.8222578729191,9.51225498089002,82.0493759893619));
#133762=CARTESIAN_POINT('Ctrl Pts',(35.9113605431891,9.02402619420501,82.554702343344));
#133763=CARTESIAN_POINT('Ctrl Pts',(36.0942866658791,7.99185698356001,83.59212793729));
#133764=CARTESIAN_POINT('Ctrl Pts',(36.3495930731491,6.41094260374401,85.04004252327));
#133765=CARTESIAN_POINT('Ctrl Pts',(36.5732283875091,4.79834145039201,86.30834141581));
#133766=CARTESIAN_POINT('Ctrl Pts',(36.7444261455991,3.24331578276701,87.2792521488301));
#133767=CARTESIAN_POINT('Ctrl Pts',(36.8575086600591,1.75826098661201,87.9205749571999));
#133768=CARTESIAN_POINT('Ctrl Pts',(36.8953905149491,0.765789295776714,
88.13541363216));
#133769=CARTESIAN_POINT('Ctrl Pts',(36.9037490740191,0.286555752975114,
88.1828173762601));
#133770=CARTESIAN_POINT('Ctrl Pts',(36.9040327044291,0.269577741895514,
88.1844259242101));
#133771=CARTESIAN_POINT('',(36.9231015705691,0.454612543733214,88.46713451361));
#133772=CARTESIAN_POINT('Ctrl Pts',(39.4126046545741,0.605801203662559,
89.3031667019448));
#133773=CARTESIAN_POINT('Ctrl Pts',(39.3831045186586,0.60835665082592,89.3300482189441));
#133774=CARTESIAN_POINT('Ctrl Pts',(39.3518228481273,0.610817150309038,
89.3563993223594));
#133775=CARTESIAN_POINT('Ctrl Pts',(39.3187170774961,0.613149296867715,
89.3819539330426));
#133776=CARTESIAN_POINT('Ctrl Pts',(39.286414762165,0.61542484376182,89.406888350116));
#133777=CARTESIAN_POINT('Ctrl Pts',(39.2523752998365,0.617578123298112,
89.4310639775319));
#133778=CARTESIAN_POINT('Ctrl Pts',(39.216600896201,0.619575784801966,89.4542071436158));
#133779=CARTESIAN_POINT('Ctrl Pts',(39.181989572322,0.621508499320843,89.476597890505));
#133780=CARTESIAN_POINT('Ctrl Pts',(39.1457539831398,0.623295470029379,
89.4980216010856));
#133781=CARTESIAN_POINT('Ctrl Pts',(39.1079414762182,0.62490538503978,89.5182134310987));
#133782=CARTESIAN_POINT('Ctrl Pts',(39.0707821876153,0.626487488459201,
89.5380564433706));
#133783=CARTESIAN_POINT('Ctrl Pts',(39.0320997293332,0.627898515182738,
89.5567091000904));
#133784=CARTESIAN_POINT('Ctrl Pts',(38.9919878848528,0.62910886732803,89.573912709109));
#133785=CARTESIAN_POINT('Ctrl Pts',(38.9528180544733,0.630290794732382,
89.5907122967595));
#133786=CARTESIAN_POINT('Ctrl Pts',(38.9122851561905,0.631281276339598,
89.6061293842026));
#133787=CARTESIAN_POINT('Ctrl Pts',(38.8705255806283,0.632054124925481,
89.6199261912394));
#133788=CARTESIAN_POINT('Ctrl Pts',(38.8369824924627,0.632674910168289,
89.6310083803806));
#133789=CARTESIAN_POINT('Ctrl Pts',(38.8026488932324,0.633155284016311,
89.6410450494364));
#133790=CARTESIAN_POINT('Ctrl Pts',(38.7676190350803,0.633482926508632,
89.6499194058903));
#133791=CARTESIAN_POINT('Ctrl Pts',(38.7252106504547,0.633879582092383,
89.6606630155324));
#133792=CARTESIAN_POINT('Ctrl Pts',(38.6817806079962,0.634052293748719,
89.6697019627361));
#133793=CARTESIAN_POINT('Ctrl Pts',(38.6375365916026,0.633983196901231,
89.6768494372612));
#133794=CARTESIAN_POINT('Ctrl Pts',(38.5938457079763,0.633914963893276,
89.6839075550171));
#133795=CARTESIAN_POINT('Ctrl Pts',(38.5493614881786,0.633610864087447,
89.6891205653363));
#133796=CARTESIAN_POINT('Ctrl Pts',(38.504323097568,0.633058259373022,89.6923400995111));
#133797=CARTESIAN_POINT('Ctrl Pts',(38.4597464968879,0.632511320653523,
89.6955266229935));
#133798=CARTESIAN_POINT('Ctrl Pts',(38.4146275926837,0.631720896463281,
89.6967598172212));
#133799=CARTESIAN_POINT('Ctrl Pts',(38.3692296616835,0.630680106018952,
89.6959355169049));
#133800=CARTESIAN_POINT('Ctrl Pts',(38.3241942624029,0.629647626956688,
89.6951177991576));
#133801=CARTESIAN_POINT('Ctrl Pts',(38.278884954633,0.628368733852932,89.6922749404782));
#133802=CARTESIAN_POINT('Ctrl Pts',(38.2335805705822,0.626842630152893,
89.6873512332037));
#133803=CARTESIAN_POINT('Ctrl Pts',(38.1885345620774,0.625325229978679,
89.6824556063364));
#133804=CARTESIAN_POINT('Ctrl Pts',(38.1434941789864,0.623563422769541,
89.6755025961845));
#133805=CARTESIAN_POINT('Ctrl Pts',(38.0987444207698,0.621562594626665,
89.6664874308702));
#133806=CARTESIAN_POINT('Ctrl Pts',(38.0541334199269,0.619567970532022,
89.6575002192412));
#133807=CARTESIAN_POINT('Ctrl Pts',(38.0098120340049,0.617335820360408,
89.6464636073945));
#133808=CARTESIAN_POINT('Ctrl Pts',(37.9660618899869,0.614877582249971,
89.6334243368702));
#133809=CARTESIAN_POINT('Ctrl Pts',(37.9223233221598,0.61241999458387,89.620388516508));
#133810=CARTESIAN_POINT('Ctrl Pts',(37.8791564685519,0.609736475757642,
89.6053512735637));
#133811=CARTESIAN_POINT('Ctrl Pts',(37.8368302231893,0.606844175965338,
89.5884096475916));
#133812=CARTESIAN_POINT('Ctrl Pts',(37.7944288784365,0.60394674437009,89.5714379621194));
#133813=CARTESIAN_POINT('Ctrl Pts',(37.7528718357621,0.600839848338323,
89.5525554938259));
#133814=CARTESIAN_POINT('Ctrl Pts',(37.7124056615877,0.597545755861513,
89.5319062665894));
#133815=CARTESIAN_POINT('Ctrl Pts',(37.6717851806981,0.594239102261745,
89.5111782991584));
#133816=CARTESIAN_POINT('Ctrl Pts',(37.6322644978623,0.590743897019806,
89.4886706010158));
#133817=CARTESIAN_POINT('Ctrl Pts',(37.5940592138503,0.587086718114105,
89.4645689017616));
#133818=CARTESIAN_POINT('Ctrl Pts',(37.5554338119455,0.583389323663991,
89.44020217228));
#133819=CARTESIAN_POINT('Ctrl Pts',(37.5181533823027,0.579526460037029,
89.4142068334793));
#133820=CARTESIAN_POINT('Ctrl Pts',(37.4823979404021,0.575528505140439,
89.3868068410641));
#133821=CARTESIAN_POINT('Ctrl Pts',(37.4463906011989,0.571502384627633,
89.3592138155382));
#133822=CARTESIAN_POINT('Ctrl Pts',(37.4119300728137,0.567339358331094,
89.3301970339475));
#133823=CARTESIAN_POINT('Ctrl Pts',(37.3791514117944,0.563071999857544,
89.3000068278654));
#133824=CARTESIAN_POINT('Ctrl Pts',(37.3458646911807,0.558738498584144,
89.2693486824783));
#133825=CARTESIAN_POINT('Ctrl Pts',(37.3143124981168,0.554297502710505,
89.2374812493819));
#133826=CARTESIAN_POINT('Ctrl Pts',(37.2845831075364,0.549783244820651,
89.2046770404806));
#133827=CARTESIAN_POINT('Ctrl Pts',(37.2627034046058,0.54646092237631,89.1805343879869));
#133828=CARTESIAN_POINT('Ctrl Pts',(37.24180985427,0.543098924907988,89.1558845980402));
#133829=CARTESIAN_POINT('Ctrl Pts',(37.2219196441713,0.539710495501798,
89.1308360746835));
#133830=CARTESIAN_POINT('Ctrl Pts',(37.1941781887475,0.534984554304494,
89.0959001694978));
#133831=CARTESIAN_POINT('Ctrl Pts',(37.1683903997965,0.530207421110298,
89.0601895405553));
#133832=CARTESIAN_POINT('Ctrl Pts',(37.14455706585,0.52541249504094,89.0239885723349));
#133833=CARTESIAN_POINT('Ctrl Pts',(37.1203265038489,0.520537652365768,
88.9871842458008));
#133834=CARTESIAN_POINT('Ctrl Pts',(37.0981156574704,0.515644488939498,
88.9498737657369));
#133835=CARTESIAN_POINT('Ctrl Pts',(37.0778757845561,0.510764523307869,
88.912334325911));
#133836=CARTESIAN_POINT('Ctrl Pts',(37.0570110825334,0.505733907294808,
88.8736359986347));
#133837=CARTESIAN_POINT('Ctrl Pts',(37.0382404193393,0.500717379709185,
88.8346949775485));
#133838=CARTESIAN_POINT('Ctrl Pts',(37.0214652583305,0.495744645027273,
88.7957820015511));
#133839=CARTESIAN_POINT('Ctrl Pts',(37.0043895620494,0.490682821354183,
88.756171880422));
#133840=CARTESIAN_POINT('Ctrl Pts',(36.9893807934452,0.485666403661524,
88.7165911940317));
#133841=CARTESIAN_POINT('Ctrl Pts',(36.9762985638914,0.480721090680712,
88.6772842583823));
#133842=CARTESIAN_POINT('Ctrl Pts',(36.9627909027976,0.475614957091374,
88.6366990688923));
#133843=CARTESIAN_POINT('Ctrl Pts',(36.9513363870551,0.470584648266651,
88.5964060215216));
#133844=CARTESIAN_POINT('Ctrl Pts',(36.9417531125328,0.465652089719945,
88.5566250685652));
#133845=CARTESIAN_POINT('Ctrl Pts',(36.934490203723,0.461913834821746,88.5264761426404));
#133846=CARTESIAN_POINT('Ctrl Pts',(36.9283014467381,0.458231586758951,
88.4966202929128));
#133847=CARTESIAN_POINT('Ctrl Pts',(36.9231015707506,0.454612543733214,
88.467134513578));
#133848=CARTESIAN_POINT('',(35.848006166586,9.6214649594803,82.3699654947659));
#133849=CARTESIAN_POINT('Ctrl Pts',(35.8480061888895,9.62146509318402,82.3699656206012));
#133850=CARTESIAN_POINT('Ctrl Pts',(35.8840711939915,9.42298356395101,82.574500428362));
#133851=CARTESIAN_POINT('Ctrl Pts',(35.9193837200317,9.22621999154996,82.774767717099));
#133852=CARTESIAN_POINT('Ctrl Pts',(35.9539203620774,9.03104931189124,82.9706347473929));
#133853=CARTESIAN_POINT('Ctrl Pts',(35.9894216077162,8.83042754238368,83.1719723165117));
#133854=CARTESIAN_POINT('Ctrl Pts',(36.0241030425718,8.63148893673031,83.3686605057258));
#133855=CARTESIAN_POINT('Ctrl Pts',(36.0579470929178,8.43412917023835,83.5605996528873));
#133856=CARTESIAN_POINT('Ctrl Pts',(36.0693471268102,8.36765048331987,83.625252457754));
#133857=CARTESIAN_POINT('Ctrl Pts',(36.0806522129673,8.30135118823686,83.6893667874641));
#133858=CARTESIAN_POINT('Ctrl Pts',(36.0918618660515,8.23522805483293,83.7529398895296));
#133859=CARTESIAN_POINT('Ctrl Pts',(36.1080946788707,8.13947447178146,83.8450007462238));
#133860=CARTESIAN_POINT('Ctrl Pts',(36.1241273207524,8.04409016349334,83.9359263777126));
#133861=CARTESIAN_POINT('Ctrl Pts',(36.1399548504375,7.94905716829722,84.0256887590647));
#133862=CARTESIAN_POINT('Ctrl Pts',(36.1699269360555,7.76909623154801,84.1956689033256));
#133863=CARTESIAN_POINT('Ctrl Pts',(36.1991722019866,7.59041721187683,84.361527047438));
#133864=CARTESIAN_POINT('Ctrl Pts',(36.2276690111892,7.41287080158735,84.5231404839857));
#133865=CARTESIAN_POINT('Ctrl Pts',(36.2573201523836,7.22813244570188,84.6913004625973));
#133866=CARTESIAN_POINT('Ctrl Pts',(36.2861609991746,7.04462034885526,84.8548650311814));
#133867=CARTESIAN_POINT('Ctrl Pts',(36.3141757533437,6.86219513928813,85.0137445959195));
#133868=CARTESIAN_POINT('Ctrl Pts',(36.3306688043748,6.75479643528424,85.1072813356391));
#133869=CARTESIAN_POINT('Ctrl Pts',(36.3468756902773,6.647774982912,85.1991951530901));
#133870=CARTESIAN_POINT('Ctrl Pts',(36.3627944292351,6.54110664613089,85.2894748091241));
#133871=CARTESIAN_POINT('Ctrl Pts',(36.3725512678293,6.47572799096003,85.3448085911901));
#133872=CARTESIAN_POINT('Ctrl Pts',(36.3821998662822,6.41048203844461,85.3995285133107));
#133873=CARTESIAN_POINT('Ctrl Pts',(36.3917380100775,6.34536180651616,85.4536220148097));
#133874=CARTESIAN_POINT('Ctrl Pts',(36.4151586647637,6.1854608343972,85.5864471479344));
#133875=CARTESIAN_POINT('Ctrl Pts',(36.4379238621124,6.02632755772767,85.7155549932985));
#133876=CARTESIAN_POINT('Ctrl Pts',(36.4600028935504,5.86790369704439,85.8407714030872));
#133877=CARTESIAN_POINT('Ctrl Pts',(36.4827582420661,5.70462705272387,85.9698233976288));
#133878=CARTESIAN_POINT('Ctrl Pts',(36.5047847585164,5.54210395707846,86.0947419824114));
#133879=CARTESIAN_POINT('Ctrl Pts',(36.5260579787218,5.38029126230337,86.2153884103457));
#133880=CARTESIAN_POINT('Ctrl Pts',(36.5469684503834,5.22123777929047,86.3339775890421));
#133881=CARTESIAN_POINT('Ctrl Pts',(36.5671511750975,5.06287082270039,86.4484395084244));
#133882=CARTESIAN_POINT('Ctrl Pts',(36.5865908243859,4.90516767849405,86.5586872380554));
#133883=CARTESIAN_POINT('Ctrl Pts',(36.5912217730954,4.86759934784603,86.5849506532892));
#133884=CARTESIAN_POINT('Ctrl Pts',(36.5958105837709,4.83006876709066,86.6109750918747));
#133885=CARTESIAN_POINT('Ctrl Pts',(36.6003566184185,4.79257619115534,86.6367569355226));
#133886=CARTESIAN_POINT('Ctrl Pts',(36.6182300293975,4.64516855564193,86.7381220862625));
#133887=CARTESIAN_POINT('Ctrl Pts',(36.6354503671782,4.49833567642529,86.8357834752628));
#133888=CARTESIAN_POINT('Ctrl Pts',(36.6519849745124,4.35208529549298,86.9295558923853));
#133889=CARTESIAN_POINT('Ctrl Pts',(36.6688419771116,4.20298329375253,87.0251567038968));
#133890=CARTESIAN_POINT('Ctrl Pts',(36.6849862825463,4.05448672669592,87.1167156064538));
#133891=CARTESIAN_POINT('Ctrl Pts',(36.7003927145458,3.90661167622958,87.204089821805));
#133892=CARTESIAN_POINT('Ctrl Pts',(36.7162531253124,3.75437921626744,87.294038678615));
#133893=CARTESIAN_POINT('Ctrl Pts',(36.7313315593775,3.6028054167375,87.3795527288836));
#133894=CARTESIAN_POINT('Ctrl Pts',(36.7456100178923,3.45191629917935,87.4605298956186));
#133895=CARTESIAN_POINT('Ctrl Pts',(36.7498735780939,3.40686067669738,87.4847097484345));
#133896=CARTESIAN_POINT('Ctrl Pts',(36.7540658716536,3.36186615950828,87.5084854281124));
#133897=CARTESIAN_POINT('Ctrl Pts',(36.7581865714518,3.31693358625967,87.5318550785251));
#133898=CARTESIAN_POINT('Ctrl Pts',(36.7592349768714,3.30550165585511,87.5378008812641));
#133899=CARTESIAN_POINT('Ctrl Pts',(36.7602787482342,3.29407373556857,87.5437204029012));
#133900=CARTESIAN_POINT('Ctrl Pts',(36.7613178686119,3.28264988434538,87.5496135474077));
#133901=CARTESIAN_POINT('Ctrl Pts',(36.7730845101796,3.15329012435176,87.616345487808));
#133902=CARTESIAN_POINT('Ctrl Pts',(36.7842599602964,3.0244358430859,87.6797246024727));
#133903=CARTESIAN_POINT('Ctrl Pts',(36.7948211288705,2.89624577466549,87.7396199479668));
#133904=CARTESIAN_POINT('Ctrl Pts',(36.805436243692,2.76740091382348,87.7998212377418));
#133905=CARTESIAN_POINT('Ctrl Pts',(36.815430793198,2.63922710560392,87.8565031226065));
#133906=CARTESIAN_POINT('Ctrl Pts',(36.8247905074935,2.51188131067207,87.9095846926443));
#133907=CARTESIAN_POINT('Ctrl Pts',(36.8342534255052,2.38313135329914,87.9632515599587));
#133908=CARTESIAN_POINT('Ctrl Pts',(36.8430674352554,2.25522781027107,88.0132383038302));
#133909=CARTESIAN_POINT('Ctrl Pts',(36.8512270697234,2.12832799735421,88.0595139153293));
#133910=CARTESIAN_POINT('Ctrl Pts',(36.8577570806654,2.02677232471509,88.0965474675826));
#133911=CARTESIAN_POINT('Ctrl Pts',(36.8638681804114,1.92585940324179,88.1312052663135));
#133912=CARTESIAN_POINT('Ctrl Pts',(36.8695617213592,1.82566739860244,88.1634949415812));
#133913=CARTESIAN_POINT('Ctrl Pts',(36.8702935771886,1.81278857620878,88.1676455022413));
#133914=CARTESIAN_POINT('Ctrl Pts',(36.8710183827158,1.79992141933469,88.1717560780887));
#133915=CARTESIAN_POINT('Ctrl Pts',(36.871736162201,1.78706580880341,88.175826806872));
#133916=CARTESIAN_POINT('Ctrl Pts',(36.8790227325904,1.65656150634758,88.2171509912854));
#133917=CARTESIAN_POINT('Ctrl Pts',(36.8855855249633,1.52725131520177,88.254370399929));
#133918=CARTESIAN_POINT('Ctrl Pts',(36.8914577225618,1.39914210405543,88.2876732807));
#133919=CARTESIAN_POINT('Ctrl Pts',(36.8974061744229,1.26936931240779,88.3214086207968));
#133920=CARTESIAN_POINT('Ctrl Pts',(36.9026460801669,1.14082839355656,88.351125616774));
#133921=CARTESIAN_POINT('Ctrl Pts',(36.9072075243119,1.01347890114135,88.3769948657369));
#133922=CARTESIAN_POINT('Ctrl Pts',(36.9117999441885,0.885264607236343,
88.4030397868963));
#133923=CARTESIAN_POINT('Ctrl Pts',(36.9157047485802,0.758257457362063,
88.4251850441213));
#133924=CARTESIAN_POINT('Ctrl Pts',(36.9189467463333,0.632376055362981,
88.443571330873));
#133925=CARTESIAN_POINT('Ctrl Pts',(36.9204791775988,0.572874287978069,
88.4522621822617));
#133926=CARTESIAN_POINT('Ctrl Pts',(36.9218634261454,0.513623514599076,
88.4601126465874));
#133927=CARTESIAN_POINT('Ctrl Pts',(36.9231015707506,0.454612543733215,
88.467134513578));
#133928=CARTESIAN_POINT('Ctrl Pts',(37.5050981553872,10.7062004821443,83.1298391922139));
#133929=CARTESIAN_POINT('Ctrl Pts',(37.4486493927448,10.7060934330738,83.1399044895495));
#133930=CARTESIAN_POINT('Ctrl Pts',(37.3917867645175,10.7036375396935,83.1477000261519));
#133931=CARTESIAN_POINT('Ctrl Pts',(37.334903968502,10.6988391558546,83.1531809198935));
#133932=CARTESIAN_POINT('Ctrl Pts',(37.2762089392287,10.6938878999457,83.1588364298394));
#133933=CARTESIAN_POINT('Ctrl Pts',(37.2174927205558,10.6864428650605,83.1620277542348));
#133934=CARTESIAN_POINT('Ctrl Pts',(37.1591691607311,10.676547766656,83.1627445914778));
#133935=CARTESIAN_POINT('Ctrl Pts',(37.098160489066,10.6661971157104,83.1634944306187));
#133936=CARTESIAN_POINT('Ctrl Pts',(37.0375814842102,10.6531658024788,83.1615368786296));
#133937=CARTESIAN_POINT('Ctrl Pts',(36.9778831345637,10.6375391372142,83.1568983825099));
#133938=CARTESIAN_POINT('Ctrl Pts',(36.9605629018404,10.6330053857676,83.1555526194737));
#133939=CARTESIAN_POINT('Ctrl Pts',(36.9433166599605,10.6282533801909,83.1539814155578));
#133940=CARTESIAN_POINT('Ctrl Pts',(36.9261551025346,10.6232857040459,83.1521859576523));
#133941=CARTESIAN_POINT('Ctrl Pts',(36.8683516997991,10.6065536221176,83.1461385125501));
#133942=CARTESIAN_POINT('Ctrl Pts',(36.8115253014697,10.5873765401978,83.1375457685393));
#133943=CARTESIAN_POINT('Ctrl Pts',(36.7560879726994,10.5658938613993,83.1264703670938));
#133944=CARTESIAN_POINT('Ctrl Pts',(36.7008470163571,10.5444872794454,83.1154341973992));
#133945=CARTESIAN_POINT('Ctrl Pts',(36.6469852670891,10.5207913936621,83.1019329227223));
#133946=CARTESIAN_POINT('Ctrl Pts',(36.5948915091628,10.4949767860708,83.0860635508859));
#133947=CARTESIAN_POINT('Ctrl Pts',(36.5439322613576,10.4697243750796,83.0705397859644));
#133948=CARTESIAN_POINT('Ctrl Pts',(36.494664911665,10.4424444925548,83.0527499052946));
#133949=CARTESIAN_POINT('Ctrl Pts',(36.4474351482632,10.4133283745433,83.0328185619169));
#133950=CARTESIAN_POINT('Ctrl Pts',(36.4340930536825,10.4051032645205,83.0271880897461));
#133951=CARTESIAN_POINT('Ctrl Pts',(36.4209134439883,10.3967318172069,83.0213869376233));
#133952=CARTESIAN_POINT('Ctrl Pts',(36.4079038136097,10.3882188220656,83.0154184325699));
#133953=CARTESIAN_POINT('Ctrl Pts',(36.3598710697787,10.3567880663133,82.99338216667));
#133954=CARTESIAN_POINT('Ctrl Pts',(36.314170375116,10.3234347915396,82.9690687730562));
#133955=CARTESIAN_POINT('Ctrl Pts',(36.2711213983952,10.2883947419835,82.9426506901393));
#133956=CARTESIAN_POINT('Ctrl Pts',(36.2302742105267,10.2551468555955,82.9175837901053));
#133957=CARTESIAN_POINT('Ctrl Pts',(36.1918148357754,10.2203800814043,82.890621679067));
#133958=CARTESIAN_POINT('Ctrl Pts',(36.1560043315853,10.1843264971648,82.8619435718565));
#133959=CARTESIAN_POINT('Ctrl Pts',(36.122171073087,10.1502635800696,82.834848901272));
#133960=CARTESIAN_POINT('Ctrl Pts',(36.0907028358421,10.1150520863725,82.8062224489253));
#133961=CARTESIAN_POINT('Ctrl Pts',(36.0618014956011,10.078917047279,82.7762470260351));
#133962=CARTESIAN_POINT('Ctrl Pts',(36.0505806496355,10.0648877426083,82.7646091711743));
#133963=CARTESIAN_POINT('Ctrl Pts',(36.0397464753727,10.0507195466556,82.7527683331707));
#133964=CARTESIAN_POINT('Ctrl Pts',(36.0293096587076,10.0364268503567,82.7407365951547));
#133965=CARTESIAN_POINT('Ctrl Pts',(36.0019553020889,9.99896643266913,82.7092020321751));
#133966=CARTESIAN_POINT('Ctrl Pts',(35.97734245913,9.9606666476471,82.6763694076741));
#133967=CARTESIAN_POINT('Ctrl Pts',(35.9555939932428,9.92172709202522,82.6424109829633));
#133968=CARTESIAN_POINT('Ctrl Pts',(35.9348937405076,9.88466431035839,82.6100892561048));
#133969=CARTESIAN_POINT('Ctrl Pts',(35.9167897165306,9.84702175446862,82.5767472218424));
#133970=CARTESIAN_POINT('Ctrl Pts',(35.9013866724505,9.80900396939047,82.5425651082853));
#133971=CARTESIAN_POINT('Ctrl Pts',(35.8867598368852,9.77290202174963,82.5101055404448));
#133972=CARTESIAN_POINT('Ctrl Pts',(35.8745697086462,9.73646199232484,82.4768885102196));
#133973=CARTESIAN_POINT('Ctrl Pts',(35.8648878244567,9.69988801776518,82.4430996797116));
#133974=CARTESIAN_POINT('Ctrl Pts',(35.85797840509,9.67378721721952,82.4189864807394));
#133975=CARTESIAN_POINT('Ctrl Pts',(35.8523460717753,9.64761884945182,82.3945827596681));
#133976=CARTESIAN_POINT('Ctrl Pts',(35.8480061888895,9.62146509318402,82.3699656206012));
#133977=CARTESIAN_POINT('Origin',(35.6454492392491,-0.499074165591586,72.5830523519042));
#133978=CARTESIAN_POINT('Origin',(34.1682376097291,-0.499074165591586,72.8435246184046));
#133979=CARTESIAN_POINT('',(36.4721616570127,13.601148584803,78.9068347604569));
#133980=CARTESIAN_POINT('Ctrl Pts',(35.3799890432589,11.6378875163018,79.715708490352));
#133981=CARTESIAN_POINT('Ctrl Pts',(35.3749324082523,11.7220490369113,79.6870221410859));
#133982=CARTESIAN_POINT('Ctrl Pts',(35.373425518673,11.8046126959294,79.6587776786043));
#133983=CARTESIAN_POINT('Ctrl Pts',(35.3753115536373,11.8852617928397,79.6309665278877));
#133984=CARTESIAN_POINT('Ctrl Pts',(35.3772248952026,11.9670785524741,79.6027527186759));
#133985=CARTESIAN_POINT('Ctrl Pts',(35.3826298212747,12.0469244565627,79.5749851036809));
#133986=CARTESIAN_POINT('Ctrl Pts',(35.3913271476137,12.1244920829818,79.5476888454789));
#133987=CARTESIAN_POINT('Ctrl Pts',(35.400215773304,12.2037658241355,79.5197922008726));
#133988=CARTESIAN_POINT('Ctrl Pts',(35.4125429179075,12.2806595160899,79.4923881468149));
#133989=CARTESIAN_POINT('Ctrl Pts',(35.4280637952047,12.3548760684726,79.4655350257877));
#133990=CARTESIAN_POINT('Ctrl Pts',(35.4366246988836,12.3958119475572,79.4507235574545));
#133991=CARTESIAN_POINT('Ctrl Pts',(35.4461567062305,12.4359339381909,79.4360802289885));
#133992=CARTESIAN_POINT('Ctrl Pts',(35.456615237334,12.475196785861,79.4216183015939));
#133993=CARTESIAN_POINT('Ctrl Pts',(35.4761345726474,12.5484752110474,79.3946272062575));
#133994=CARTESIAN_POINT('Ctrl Pts',(35.4988824621292,12.6187583521234,79.3682667391691));
#133995=CARTESIAN_POINT('Ctrl Pts',(35.5245504448773,12.6857847818072,79.3426417792656));
#133996=CARTESIAN_POINT('Ctrl Pts',(35.5424494187773,12.7325241117848,79.3247728063509));
#133997=CARTESIAN_POINT('Ctrl Pts',(35.5617678012447,12.7776807092336,79.3072620146635));
#133998=CARTESIAN_POINT('Ctrl Pts',(35.5823956077124,12.8211787476974,79.2901504470772));
#133999=CARTESIAN_POINT('Ctrl Pts',(35.6005139328016,12.8593850205195,79.2751205918768));
#134000=CARTESIAN_POINT('Ctrl Pts',(35.6197240475077,12.8964574372431,79.2603561273214));
#134001=CARTESIAN_POINT('Ctrl Pts',(35.6398698334597,12.9321867415071,79.2459266087515));
#134002=CARTESIAN_POINT('Ctrl Pts',(35.6601964451968,12.9682367470587,79.231367572821));
#134003=CARTESIAN_POINT('Ctrl Pts',(35.6814752036809,13.0029190103381,79.2171495440437));
#134004=CARTESIAN_POINT('Ctrl Pts',(35.7035123966813,13.0360515929857,79.2033694579059));
#134005=CARTESIAN_POINT('Ctrl Pts',(35.7201597213545,13.0610805910339,79.1929597125289));
#134006=CARTESIAN_POINT('Ctrl Pts',(35.737239108389,13.0852259193827,79.1828004280045));
#134007=CARTESIAN_POINT('Ctrl Pts',(35.7546569098908,13.1084233171307,79.1729425959568));
#134008=CARTESIAN_POINT('Ctrl Pts',(35.7954313567611,13.1627275909456,79.149865765678));
#134009=CARTESIAN_POINT('Ctrl Pts',(35.8389976528179,13.213328348537,79.1275471673048));
#134010=CARTESIAN_POINT('Ctrl Pts',(35.8850246599171,13.2599453121747,79.1060565522116));
#134011=CARTESIAN_POINT('Ctrl Pts',(35.9310021019971,13.3065120754877,79.0845890796781));
#134012=CARTESIAN_POINT('Ctrl Pts',(35.9794346537849,13.3491032713937,79.0639480256613));
#134013=CARTESIAN_POINT('Ctrl Pts',(36.0299562710254,13.387476333018,79.044210147366));
#134014=CARTESIAN_POINT('Ctrl Pts',(36.0803829479537,13.4257772839172,79.0245093605263));
#134015=CARTESIAN_POINT('Ctrl Pts',(36.132890498998,13.4598756486123,79.0057085595006));
#134016=CARTESIAN_POINT('Ctrl Pts',(36.1870839697266,13.4895716938935,78.987888132682));
#134017=CARTESIAN_POINT('Ctrl Pts',(36.1930758446128,13.4928550227806,78.9859178258077));
#134018=CARTESIAN_POINT('Ctrl Pts',(36.1990883010099,13.4960845797666,78.9839595058598));
#134019=CARTESIAN_POINT('Ctrl Pts',(36.2051207847567,13.4992601283539,78.9820132829396));
#134020=CARTESIAN_POINT('Ctrl Pts',(36.259550749436,13.5279125051692,78.9644528800851));
#134021=CARTESIAN_POINT('Ctrl Pts',(36.3156128403408,13.5521640749948,78.9478773243603));
#134022=CARTESIAN_POINT('Ctrl Pts',(36.3728872414993,13.5718670326191,78.9323676256727));
#134023=CARTESIAN_POINT('Ctrl Pts',(36.4056097441414,13.5831238955435,78.9235064914483));
#134024=CARTESIAN_POINT('Ctrl Pts',(36.4387275411762,13.59289687207,78.9149932713656));
#134025=CARTESIAN_POINT('Ctrl Pts',(36.4721594611798,13.6011654789238,78.9068428925862));
#134026=CARTESIAN_POINT('Ctrl Pts',(36.7497137917856,13.6349227617825,78.8487558990981));
#134027=CARTESIAN_POINT('Ctrl Pts',(36.7468847875822,13.6349194461349,78.8492624067619));
#134028=CARTESIAN_POINT('Ctrl Pts',(36.7426787151625,13.6349315419734,78.8499636260781));
#134029=CARTESIAN_POINT('Ctrl Pts',(36.736873947881,13.6349239250663,78.8508794246839));
#134030=CARTESIAN_POINT('Ctrl Pts',(36.733483665418,13.6349194764011,78.8514142981426));
#134031=CARTESIAN_POINT('Ctrl Pts',(36.7288578444576,13.6349071712433,78.8521225574776));
#134032=CARTESIAN_POINT('Ctrl Pts',(36.7241942792919,13.6348695191711,78.8528303166485));
#134033=CARTESIAN_POINT('Ctrl Pts',(36.7207774203749,13.6348419325899,78.8533488712624));
#134034=CARTESIAN_POINT('Ctrl Pts',(36.717340287326,13.6348016235124,78.8538669156717));
#134035=CARTESIAN_POINT('Ctrl Pts',(36.7143532752961,13.6347596533172,78.854311252123));
#134036=CARTESIAN_POINT('Ctrl Pts',(36.7056794312614,13.6346377780373,78.8556015398887));
#134037=CARTESIAN_POINT('Ctrl Pts',(36.6982661745955,13.6344046896701,78.8568142260074));
#134038=CARTESIAN_POINT('Ctrl Pts',(36.6915576979266,13.6340792668169,78.8580703235985));
#134039=CARTESIAN_POINT('Ctrl Pts',(36.6873395410126,13.633874647389,78.8588601328205));
#134040=CARTESIAN_POINT('Ctrl Pts',(36.6834000513446,13.6336322545447,78.8596674527749));
#134041=CARTESIAN_POINT('Ctrl Pts',(36.6796015271321,13.6333469994752,78.8605250079955));
#134042=CARTESIAN_POINT('Ctrl Pts',(36.6697619021318,13.6326080801591,78.8627464027573));
#134043=CARTESIAN_POINT('Ctrl Pts',(36.6594157298214,13.6313826480724,78.8658247010245));
#134044=CARTESIAN_POINT('Ctrl Pts',(36.6485285247017,13.6296454571002,78.8697212645982));
#134045=CARTESIAN_POINT('Ctrl Pts',(36.6430849221418,13.6287768616141,78.871669546385));
#134046=CARTESIAN_POINT('Ctrl Pts',(36.6375059082805,13.627780369151,78.8738222161859));
#134047=CARTESIAN_POINT('Ctrl Pts',(36.6317862300815,13.6266529083236,78.8761732365801));
#134048=CARTESIAN_POINT('Ctrl Pts',(36.6303073109073,13.6263613843291,78.8767811325175));
#134049=CARTESIAN_POINT('Ctrl Pts',(36.6289104049784,13.6260808457358,78.877361111239));
#134050=CARTESIAN_POINT('Ctrl Pts',(36.6275243140171,13.6257965115786,78.8779448496941));
#134051=CARTESIAN_POINT('Ctrl Pts',(36.62412449698,13.6250990940651,78.879376648905));
#134052=CARTESIAN_POINT('Ctrl Pts',(36.6207887373414,13.6243818440834,78.880830319144));
#134053=CARTESIAN_POINT('Ctrl Pts',(36.6164755445211,13.6233980448365,78.8827804225888));
#134054=CARTESIAN_POINT('Ctrl Pts',(36.615746373096,13.6232317276026,78.8831100994122));
#134055=CARTESIAN_POINT('Ctrl Pts',(36.6149893036036,13.6230576833706,78.8834539914887));
#134056=CARTESIAN_POINT('Ctrl Pts',(36.6141993559312,13.6228745694473,78.8838144294026));
#134057=CARTESIAN_POINT('Ctrl Pts',(36.5994639910949,13.6194588362783,78.8905378926753));
#134058=CARTESIAN_POINT('Ctrl Pts',(36.5865212063194,13.6165129372762,78.895752371069));
#134059=CARTESIAN_POINT('Ctrl Pts',(36.5754711213109,13.6141643825912,78.8995604732951));
#134060=CARTESIAN_POINT('Ctrl Pts',(36.5699460788067,13.6129901052487,78.9014645244082));
#134061=CARTESIAN_POINT('Ctrl Pts',(36.5648934069248,13.6119650049175,78.9030165200554));
#134062=CARTESIAN_POINT('Ctrl Pts',(36.5603209149633,13.6111033595531,78.9042259614167));
#134063=CARTESIAN_POINT('Ctrl Pts',(36.5569937647847,13.6104763877504,78.9051060051816));
#134064=CARTESIAN_POINT('Ctrl Pts',(36.5532155524438,13.6098369441149,78.905907742029));
#134065=CARTESIAN_POINT('Ctrl Pts',(36.5505279016848,13.6094049524859,78.9064091210418));
#134066=CARTESIAN_POINT('Ctrl Pts',(36.5495219225108,13.6092432593862,78.9065967856197));
#134067=CARTESIAN_POINT('Ctrl Pts',(36.5486686510362,13.6091111684528,78.906742236496));
#134068=CARTESIAN_POINT('Ctrl Pts',(36.5480487784383,13.6090214533071,78.9068335184581));
#134069=CARTESIAN_POINT('Ctrl Pts',(36.5448171192864,13.6085537301448,78.9073094100999));
#134070=CARTESIAN_POINT('Ctrl Pts',(36.5395942224044,13.6080020236394,78.9076128636903));
#134071=CARTESIAN_POINT('Ctrl Pts',(36.5323984940512,13.6073025311191,78.9077469719079));
#134072=CARTESIAN_POINT('Ctrl Pts',(36.5294587023756,13.6070167556997,78.9078017613889));
#134073=CARTESIAN_POINT('Ctrl Pts',(36.5261895964218,13.6067057282038,78.9078284516419));
#134074=CARTESIAN_POINT('Ctrl Pts',(36.5225923495154,13.6063626979722,78.9078279197424));
#134075=CARTESIAN_POINT('Ctrl Pts',(36.5163912352713,13.6057713652917,78.9078270028275));
#134076=CARTESIAN_POINT('Ctrl Pts',(36.5092160916144,13.6050858528307,78.9077445915112));
#134077=CARTESIAN_POINT('Ctrl Pts',(36.5010800577092,13.6042641038228,78.9075853796198));
#134078=CARTESIAN_POINT('Ctrl Pts',(36.4970120407567,13.6038532293188,78.9075057736741));
#134079=CARTESIAN_POINT('Ctrl Pts',(36.4927038226765,13.6034081692886,78.9074069052325));
#134080=CARTESIAN_POINT('Ctrl Pts',(36.4881576515518,13.602922681148,78.9072896469837));
#134081=CARTESIAN_POINT('Ctrl Pts',(36.4851625366389,13.6026028311621,78.9072123947377));
#134082=CARTESIAN_POINT('Ctrl Pts',(36.4810938518181,13.6021605085673,78.9070959579087));
#134083=CARTESIAN_POINT('Ctrl Pts',(36.4778700682971,13.601798676173,78.9070028584328));
#134084=CARTESIAN_POINT('Ctrl Pts',(36.4762005933016,13.6016112969241,78.9069546457517));
#134085=CARTESIAN_POINT('Ctrl Pts',(36.4747576873657,13.6014466821658,78.9069123781233));
#134086=CARTESIAN_POINT('Ctrl Pts',(36.4738076969342,13.6013382249055,78.9068833613598));
#134087=CARTESIAN_POINT('Ctrl Pts',(36.4732593742324,13.6012756247192,78.9068666132436));
#134088=CARTESIAN_POINT('Ctrl Pts',(36.4727106942741,13.6012124119033,78.9068504133483));
#134089=CARTESIAN_POINT('Ctrl Pts',(36.4721616570127,13.601148584803,78.906834760457));
#134090=CARTESIAN_POINT('Ctrl Pts',(35.4047464453691,11.47699078912,80.070829087246));
#134091=CARTESIAN_POINT('Ctrl Pts',(35.4010430938991,11.56996412073,80.039824743627));
#134092=CARTESIAN_POINT('Ctrl Pts',(35.4016895299391,11.88007018329,79.9341244321319));
#134093=CARTESIAN_POINT('Ctrl Pts',(35.4766108372791,12.36407360515,79.7569593010479));
#134094=CARTESIAN_POINT('Ctrl Pts',(35.6840194032591,12.85992909088,79.553941580112));
#134095=CARTESIAN_POINT('Ctrl Pts',(35.9715431495691,13.22233503903,79.382321605689));
#134096=CARTESIAN_POINT('Ctrl Pts',(36.3111476474691,13.4522667151,79.2458202724909));
#134097=CARTESIAN_POINT('Ctrl Pts',(36.6410702301991,13.54317413932,79.1573907935629));
#134098=CARTESIAN_POINT('Ctrl Pts',(36.8519924730991,13.54113934177,79.1207853593));
#134099=CARTESIAN_POINT('Ctrl Pts',(36.9359089029591,13.53124995019,79.109308518752));
#134100=CARTESIAN_POINT('Ctrl Pts',(35.4799873971691,11.49461145088,78.883043833973));
#134101=CARTESIAN_POINT('Ctrl Pts',(35.4515476021091,11.57600382921,78.85030473176));
#134102=CARTESIAN_POINT('Ctrl Pts',(35.3679195444291,11.85551262843,78.742056216998));
#134103=CARTESIAN_POINT('Ctrl Pts',(35.3086113826091,12.33697706548,78.5757610906141));
#134104=CARTESIAN_POINT('Ctrl Pts',(35.4013575593891,12.89860219014,78.396444849156));
#134105=CARTESIAN_POINT('Ctrl Pts',(35.6470520231591,13.35737986134,78.24380932435));
#134106=CARTESIAN_POINT('Ctrl Pts',(36.0126298069591,13.67448865407,78.114215280491));
#134107=CARTESIAN_POINT('Ctrl Pts',(36.4059824524991,13.80651913688,78.019865391245));
#134108=CARTESIAN_POINT('Ctrl Pts',(36.6613386460491,13.80349217816,77.97561025295));
#134109=CARTESIAN_POINT('Ctrl Pts',(36.7618041096891,13.78918487375,77.960551786597));
#134110=CARTESIAN_POINT('Ctrl Pts',(34.5323713981891,11.4437981521,78.16457618897));
#134111=CARTESIAN_POINT('Ctrl Pts',(34.4868146111391,11.55294239059,78.152451057442));
#134112=CARTESIAN_POINT('Ctrl Pts',(34.3532969408491,11.9344083525,78.1132993532569));
#134113=CARTESIAN_POINT('Ctrl Pts',(34.2636399697991,12.62703032885,78.0538368049579));
#134114=CARTESIAN_POINT('Ctrl Pts',(34.4346417170091,13.47889013285,77.9728297289189));
#134115=CARTESIAN_POINT('Ctrl Pts',(34.8683475554791,14.19947679409,77.873493505207));
#134116=CARTESIAN_POINT('Ctrl Pts',(35.5086014344991,14.70855335123,77.752522500601));
#134117=CARTESIAN_POINT('Ctrl Pts',(36.1932838806191,14.92297019512,77.629734621697));
#134118=CARTESIAN_POINT('Ctrl Pts',(36.6339629540391,14.91801708291,77.552516340959));
#134119=CARTESIAN_POINT('Ctrl Pts',(36.8064748222491,14.89480530408,77.522190509913));
#134120=CARTESIAN_POINT('Ctrl Pts',(33.4121724780091,11.37014449647,78.5600906369051));
#134121=CARTESIAN_POINT('Ctrl Pts',(33.3724768335991,11.52147230307,78.572431763808));
#134122=CARTESIAN_POINT('Ctrl Pts',(33.2682192331391,12.04596603781,78.612022905951));
#134123=CARTESIAN_POINT('Ctrl Pts',(33.2793254009391,12.97397527668,78.6594970952119));
#134124=CARTESIAN_POINT('Ctrl Pts',(33.6512837556791,14.08011390146,78.663196318665));
#134125=CARTESIAN_POINT('Ctrl Pts',(34.3341433460291,14.99303163765,78.603650011164));
#134126=CARTESIAN_POINT('Ctrl Pts',(35.2513155901291,15.62661834944,78.485280541034));
#134127=CARTESIAN_POINT('Ctrl Pts',(36.1938240485491,15.89076147096,78.337053846843));
#134128=CARTESIAN_POINT('Ctrl Pts',(36.7944289755491,15.88467650615,78.231136054428));
#134129=CARTESIAN_POINT('Ctrl Pts',(37.0298390382191,15.8560634713,78.187556174812));
#134130=CARTESIAN_POINT('Ctrl Pts',(36.4721616570127,13.601148584803,78.906834760457));
#134131=CARTESIAN_POINT('Ctrl Pts',(36.4504061654935,13.598619448735,78.9062145177738));
#134132=CARTESIAN_POINT('Ctrl Pts',(36.428088693382,13.59512625113,78.9064529546472));
#134133=CARTESIAN_POINT('Ctrl Pts',(36.4052122412434,13.5905635514609,78.9074754761355));
#134134=CARTESIAN_POINT('Ctrl Pts',(36.3934853518584,13.5882246278379,78.9079996394243));
#134135=CARTESIAN_POINT('Ctrl Pts',(36.3816115827963,13.5856047262905,78.908729525301));
#134136=CARTESIAN_POINT('Ctrl Pts',(36.3695915648287,13.5826898772137,78.9096530208533));
#134137=CARTESIAN_POINT('Ctrl Pts',(36.3635815558449,13.5812324526753,78.9101147686295));
#134138=CARTESIAN_POINT('Ctrl Pts',(36.3575349823577,13.5797012811641,78.9106249156237));
#134139=CARTESIAN_POINT('Ctrl Pts',(36.3514519583453,13.5780946372335,78.9111817763396));
#134140=CARTESIAN_POINT('Ctrl Pts',(36.3472346223365,13.5769807574777,78.9115678456275));
#134141=CARTESIAN_POINT('Ctrl Pts',(36.3435292244632,13.5759772404352,78.9119216633451));
#134142=CARTESIAN_POINT('Ctrl Pts',(36.3392342676222,13.5747801330311,78.9123560774501));
#134143=CARTESIAN_POINT('Ctrl Pts',(36.3373342412936,13.5742505501575,78.9125482559207));
#134144=CARTESIAN_POINT('Ctrl Pts',(36.3353189419999,13.5736825169018,78.9127563333781));
#134145=CARTESIAN_POINT('Ctrl Pts',(36.3330936499266,13.5730465216947,78.9129907842902));
#134146=CARTESIAN_POINT('Ctrl Pts',(36.3122587859171,13.5670918545255,78.9151858906899));
#134147=CARTESIAN_POINT('Ctrl Pts',(36.2931857227023,13.5612738711274,78.9169194038706));
#134148=CARTESIAN_POINT('Ctrl Pts',(36.2758412379195,13.5558046431333,78.9182299553678));
#134149=CARTESIAN_POINT('Ctrl Pts',(36.2690256488441,13.553655486728,78.9187449421534));
#134150=CARTESIAN_POINT('Ctrl Pts',(36.2624770389035,13.5515596390135,78.9191947814029));
#134151=CARTESIAN_POINT('Ctrl Pts',(36.2561937050724,13.5495278851669,78.9195824250782));
#134152=CARTESIAN_POINT('Ctrl Pts',(36.2450570441208,13.5459267787583,78.9202694896681));
#134153=CARTESIAN_POINT('Ctrl Pts',(36.2347522538573,13.5425280212809,78.9207596890134));
#134154=CARTESIAN_POINT('Ctrl Pts',(36.2252649480616,13.5393851503123,78.9210638349686));
#134155=CARTESIAN_POINT('Ctrl Pts',(36.2239299671903,13.5389429096262,78.9211066320536));
#134156=CARTESIAN_POINT('Ctrl Pts',(36.2226111757268,13.5385057219258,78.9211457408626));
#134157=CARTESIAN_POINT('Ctrl Pts',(36.2213085307405,13.5380737218633,78.9211811859676));
#134158=CARTESIAN_POINT('Ctrl Pts',(36.2179824235124,13.5369706749508,78.9212716896898));
#134159=CARTESIAN_POINT('Ctrl Pts',(36.2147615805659,13.5359014635584,78.9213383042534));
#134160=CARTESIAN_POINT('Ctrl Pts',(36.2116452961703,13.5348682206978,78.9213814728402));
#134161=CARTESIAN_POINT('Ctrl Pts',(36.2087853143723,13.533919958152,78.921421090974));
#134162=CARTESIAN_POINT('Ctrl Pts',(36.2068846778224,13.5332829968046,78.9214485990927));
#134163=CARTESIAN_POINT('Ctrl Pts',(36.2042187359777,13.5324049186788,78.9214487403883));
#134164=CARTESIAN_POINT('Ctrl Pts',(36.2028421578516,13.5319515167625,78.9214488133474));
#134165=CARTESIAN_POINT('Ctrl Pts',(36.2012616263255,13.5314333037895,78.9214416966704));
#134166=CARTESIAN_POINT('Ctrl Pts',(36.1992406519875,13.5307688878843,78.9214263749526));
#134167=CARTESIAN_POINT('Ctrl Pts',(36.1670570918207,13.520188214563,78.9211823800541));
#134168=CARTESIAN_POINT('Ctrl Pts',(36.1351752345258,13.5094888143299,78.9192661055963));
#134169=CARTESIAN_POINT('Ctrl Pts',(36.10375519299,13.4988266822702,78.9159806720018));
#134170=CARTESIAN_POINT('Ctrl Pts',(36.0888225633727,13.4937594175182,78.9144192430348));
#134171=CARTESIAN_POINT('Ctrl Pts',(36.0739945375956,13.4887013497456,78.91254856096));
#134172=CARTESIAN_POINT('Ctrl Pts',(36.0592901050985,13.4836727766471,78.9104013418097));
#134173=CARTESIAN_POINT('Ctrl Pts',(36.0364679451207,13.475868130005,78.9070687290777));
#134174=CARTESIAN_POINT('Ctrl Pts',(36.0139347499633,13.4681316932326,78.9030690828645));
#134175=CARTESIAN_POINT('Ctrl Pts',(35.9917231242992,13.4605285167546,78.8985167430992));
#134176=CARTESIAN_POINT('Ctrl Pts',(35.9806173114672,13.4567269285156,78.8962405732166));
#134177=CARTESIAN_POINT('Ctrl Pts',(35.9695915956965,13.452958566235,78.8938261252443));
#134178=CARTESIAN_POINT('Ctrl Pts',(35.9586484977955,13.4492308986411,78.8912869754962));
#134179=CARTESIAN_POINT('Ctrl Pts',(35.9521332283931,13.4470115308866,78.8897752239967));
#134180=CARTESIAN_POINT('Ctrl Pts',(35.946232804495,13.4449969559354,78.888371918885));
#134181=CARTESIAN_POINT('Ctrl Pts',(35.9399018577183,13.4428519618481,78.8868063897854));
#134182=CARTESIAN_POINT('Ctrl Pts',(35.9355992963306,13.4413942069399,78.8857424438556));
#134183=CARTESIAN_POINT('Ctrl Pts',(35.9310978609088,13.4398753672442,78.88460376303));
#134184=CARTESIAN_POINT('Ctrl Pts',(35.9260687135604,13.4381769231713,78.8833084515107));
#134185=CARTESIAN_POINT('Ctrl Pts',(35.899945135366,13.4293544661078,78.8765800402282));
#134186=CARTESIAN_POINT('Ctrl Pts',(35.8741882104117,13.4206854200628,78.8692741996048));
#134187=CARTESIAN_POINT('Ctrl Pts',(35.8485408966571,13.4121822154005,78.8614124658743));
#134188=CARTESIAN_POINT('Ctrl Pts',(35.82250526924,13.4035502677994,78.8534317014084));
#134189=CARTESIAN_POINT('Ctrl Pts',(35.7965825163458,13.3950891138958,78.844878072982));
#134190=CARTESIAN_POINT('Ctrl Pts',(35.7705075977699,13.3867622396569,78.8357933863257));
#134191=CARTESIAN_POINT('Ctrl Pts',(35.7640936161502,13.3847139717721,78.8335587096166));
#134192=CARTESIAN_POINT('Ctrl Pts',(35.7576704489817,13.382673600299,78.8312919907959));
#134193=CARTESIAN_POINT('Ctrl Pts',(35.7512341970586,13.380640136617,78.8289940301167));
#134194=CARTESIAN_POINT('Ctrl Pts',(35.7253016081509,13.3724470176477,78.8197352145307));
#134195=CARTESIAN_POINT('Ctrl Pts',(35.699156188398,13.364369732452,78.8099677195824));
#134196=CARTESIAN_POINT('Ctrl Pts',(35.6725345118184,13.3563152336591,78.7997573802145));
#134197=CARTESIAN_POINT('Ctrl Pts',(35.6583696149245,13.3520295852855,78.7943246493357));
#134198=CARTESIAN_POINT('Ctrl Pts',(35.644069970644,13.347749596578,78.7887668669451));
#134199=CARTESIAN_POINT('Ctrl Pts',(35.6295965665019,13.3434556875699,78.7830962085536));
#134200=CARTESIAN_POINT('Ctrl Pts',(35.5957491463823,13.3334139765305,78.7698348392829));
#134201=CARTESIAN_POINT('Ctrl Pts',(35.5610961675901,13.3234052337112,78.7559509003528));
#134202=CARTESIAN_POINT('Ctrl Pts',(35.5254411255284,13.3134447719003,78.7415837844168));
#134203=CARTESIAN_POINT('Ctrl Pts',(35.4890666251392,13.303283324849,78.7269267644277));
#134204=CARTESIAN_POINT('Ctrl Pts',(35.4516484315061,13.2931726331318,78.7117663479471));
#134205=CARTESIAN_POINT('Ctrl Pts',(35.4129822688164,13.2830990650404,78.6963000244749));
#134206=CARTESIAN_POINT('Ctrl Pts',(35.3774872942956,13.2738516761643,78.6821021646567));
#134207=CARTESIAN_POINT('Ctrl Pts',(35.3409400501456,13.2646354930113,78.6676469707998));
#134208=CARTESIAN_POINT('Ctrl Pts',(35.3031958978858,13.2554129208036,78.6531274388204));
#134209=CARTESIAN_POINT('Ctrl Pts',(35.2998237639228,13.2545889587563,78.651830236367));
#134210=CARTESIAN_POINT('Ctrl Pts',(35.2964420893669,13.253764926886,78.6505325463469));
#134211=CARTESIAN_POINT('Ctrl Pts',(35.2930507794226,13.2529407870952,78.6492345216881));
#134212=CARTESIAN_POINT('Ctrl Pts',(35.2565394350175,13.244067976224,78.6352597962448));
#134213=CARTESIAN_POINT('Ctrl Pts',(35.2189214988429,13.2351963570681,78.6212427822176));
#134214=CARTESIAN_POINT('Ctrl Pts',(35.1800835948419,13.2262912408389,78.6073783241714));
#134215=CARTESIAN_POINT('Ctrl Pts',(35.1533790067126,13.2201681642399,78.597845249427));
#134216=CARTESIAN_POINT('Ctrl Pts',(35.1260979765889,13.2140287947895,78.5883851016776));
#134217=CARTESIAN_POINT('Ctrl Pts',(35.0982113352202,13.207855117831,78.579071407501));
#134218=CARTESIAN_POINT('Ctrl Pts',(35.0763291035399,13.2030107255737,78.5717630905517));
#134219=CARTESIAN_POINT('Ctrl Pts',(35.0540757775653,13.1981444782573,78.5645460778694));
#134220=CARTESIAN_POINT('Ctrl Pts',(35.0314390924283,13.193246632164,78.5574578386157));
#134221=CARTESIAN_POINT('Ctrl Pts',(35.0186740463358,13.1904846892931,78.5534607118174));
#134222=CARTESIAN_POINT('Ctrl Pts',(35.0057871537928,13.187712659575,78.5495045921738));
#134223=CARTESIAN_POINT('Ctrl Pts',(34.9927763607437,13.1849282282858,78.5455966860617));
#134224=CARTESIAN_POINT('Ctrl Pts',(34.9743582771188,13.180986586286,78.5400646526723));
#134225=CARTESIAN_POINT('Ctrl Pts',(34.9554131454896,13.1769677477061,78.5345457685357));
#134226=CARTESIAN_POINT('Ctrl Pts',(34.9363618770901,13.1729421492203,78.5291938283296));
#134227=CARTESIAN_POINT('Ctrl Pts',(34.9180893898604,13.169081109872,78.524060665696));
#134228=CARTESIAN_POINT('Ctrl Pts',(34.8997196252843,13.1652138258829,78.5190810386885));
#134229=CARTESIAN_POINT('Ctrl Pts',(34.8816401240329,13.1614272575593,78.5143564196021));
#134230=CARTESIAN_POINT('Ctrl Pts',(34.8391099224564,13.1525197378306,78.5032422301495));
#134231=CARTESIAN_POINT('Ctrl Pts',(34.7955882146145,13.1434492907672,78.4928655648522));
#134232=CARTESIAN_POINT('Ctrl Pts',(34.7510398756842,13.1341533320885,78.4834200768374));
#134233=CARTESIAN_POINT('Ctrl Pts',(34.7074698710593,13.1250615236765,78.4741820229307));
#134234=CARTESIAN_POINT('Ctrl Pts',(34.6629172741695,13.1157539344517,78.4658352247198));
#134235=CARTESIAN_POINT('Ctrl Pts',(34.6173892125664,13.1061531878966,78.4585819459816));
#134236=CARTESIAN_POINT('Ctrl Pts',(34.5732100030488,13.0968368810158,78.4515435588907));
#134237=CARTESIAN_POINT('Ctrl Pts',(34.5281119258475,13.0872443608496,78.445535517776));
#134238=CARTESIAN_POINT('Ctrl Pts',(34.4821460687883,13.0772887589311,78.4407539859881));
#134239=CARTESIAN_POINT('Ctrl Pts',(34.4556942684274,13.0715596458183,78.4380023757199));
#134240=CARTESIAN_POINT('Ctrl Pts',(34.4289559538174,13.0657100025855,78.4356571048377));
#134241=CARTESIAN_POINT('Ctrl Pts',(34.4019484562768,13.0597211322695,78.4337559236378));
#134242=CARTESIAN_POINT('Ctrl Pts',(34.3575430466552,13.0498743021752,78.4306300238828));
#134243=CARTESIAN_POINT('Ctrl Pts',(34.3124132438406,13.0396630086552,78.4287031985923));
#134244=CARTESIAN_POINT('Ctrl Pts',(34.2666189774245,13.0290012971378,78.4281398834861));
#134245=CARTESIAN_POINT('Ctrl Pts',(34.2216993254271,13.0185432112564,78.4275873270088));
#134246=CARTESIAN_POINT('Ctrl Pts',(34.1761401095282,13.0076515539986,78.4283474448037));
#134247=CARTESIAN_POINT('Ctrl Pts',(34.1300448615253,12.9962314458899,78.4305751618034));
#134248=CARTESIAN_POINT('Ctrl Pts',(34.0851465644316,12.9851078826394,78.4327450318882));
#134249=CARTESIAN_POINT('Ctrl Pts',(34.0397397518139,12.9734826841811,78.4363080260802));
#134250=CARTESIAN_POINT('Ctrl Pts',(33.9939664444587,12.9612584436044,78.4413960448565));
#134251=CARTESIAN_POINT('Ctrl Pts',(33.9493383893727,12.9493400546271,78.4463567609451));
#134252=CARTESIAN_POINT('Ctrl Pts',(33.9043622022559,12.9368519188894,78.4527678284234));
#134253=CARTESIAN_POINT('Ctrl Pts',(33.8592119939158,12.9236986194734,78.4607301343571));
#134254=CARTESIAN_POINT('Ctrl Pts',(35.28916359171,12.25029619447,78.8322534413786));
#134255=CARTESIAN_POINT('Ctrl Pts',(35.2779279497709,12.2624028118831,78.8186638264655));
#134256=CARTESIAN_POINT('Ctrl Pts',(35.2666923078319,12.2745094292961,78.8050742115524));
#134257=CARTESIAN_POINT('Ctrl Pts',(35.2554566658928,12.2866160467092,78.7914845966393));
#134258=CARTESIAN_POINT('Ctrl Pts',(35.2498393249075,12.2926688382236,78.7846903697282));
#134259=CARTESIAN_POINT('Ctrl Pts',(35.2378447957871,12.3055931709764,78.7701828736105));
#134260=CARTESIAN_POINT('Ctrl Pts',(35.1977745566455,12.3335999215784,78.7309978424039));
#134261=CARTESIAN_POINT('Ctrl Pts',(35.1455449414878,12.3640756612257,78.6882977707834));
#134262=CARTESIAN_POINT('Ctrl Pts',(35.0806760308514,12.3962322793046,78.6430241955527));
#134263=CARTESIAN_POINT('Ctrl Pts',(35.0054940744708,12.4283335028473,78.5983814367481));
#134264=CARTESIAN_POINT('Ctrl Pts',(34.9213590600735,12.4595076387769,78.5559499882088));
#134265=CARTESIAN_POINT('Ctrl Pts',(34.8297226352172,12.4890184640333,78.5171196827213));
#134266=CARTESIAN_POINT('Ctrl Pts',(34.7318182707934,12.5163508899825,78.4828709295655));
#134267=CARTESIAN_POINT('Ctrl Pts',(34.6286945809858,12.5411170357543,78.4539359247313));
#134268=CARTESIAN_POINT('Ctrl Pts',(34.521309326854,12.5630211819863,78.4308698615195));
#134269=CARTESIAN_POINT('Ctrl Pts',(34.410582224273,12.5818286325215,78.4141056081173));
#134270=CARTESIAN_POINT('Ctrl Pts',(34.2973831835532,12.5973569512455,78.4039606649909));
#134271=CARTESIAN_POINT('Ctrl Pts',(34.182550136185,12.6094541243224,78.4006770615684));
#134272=CARTESIAN_POINT('Ctrl Pts',(34.0668631558752,12.6180352212567,78.4043475217904));
#134273=CARTESIAN_POINT('Ctrl Pts',(33.9511293651193,12.6229294807815,78.4152033744343));
#134274=CARTESIAN_POINT('Ctrl Pts',(33.8358811094663,12.6244155387313,78.4326287066328));
#134275=CARTESIAN_POINT('Ctrl Pts',(33.7603444272674,12.6222852452232,78.4500993196882));
#134276=CARTESIAN_POINT('Ctrl Pts',(33.7225560295391,12.62121953283,78.458839265043));
#134277=CARTESIAN_POINT('Ctrl Pts',(35.4366085353606,13.1319050302734,79.1874339641305));
#134278=CARTESIAN_POINT('Ctrl Pts',(35.4207517619085,13.1486721140446,79.1625108794446));
#134279=CARTESIAN_POINT('Ctrl Pts',(35.4048949884563,13.1654391978158,79.1375877947585));
#134280=CARTESIAN_POINT('Ctrl Pts',(35.3890382150042,13.1822062815871,79.1126647100726));
#134281=CARTESIAN_POINT('Ctrl Pts',(35.3811105056762,13.1905891071864,79.1002042324384));
#134282=CARTESIAN_POINT('Ctrl Pts',(35.3641827206898,13.2084886874374,79.0735977717966));
#134283=CARTESIAN_POINT('Ctrl Pts',(35.3177304804994,13.2419830464803,79.0201443411684));
#134284=CARTESIAN_POINT('Ctrl Pts',(35.2588716100858,13.2776620254717,78.9634162208831));
#134285=CARTESIAN_POINT('Ctrl Pts',(35.1873965239757,13.3144101862539,78.9051574459597));
#134286=CARTESIAN_POINT('Ctrl Pts',(35.1056278786597,13.350605956571,78.8484493715112));
#134287=CARTESIAN_POINT('Ctrl Pts',(35.0149498370101,13.3853905016559,78.7949465547076));
#134288=CARTESIAN_POINT('Ctrl Pts',(34.9168131164966,13.4180705017977,78.7460465944024));
#134289=CARTESIAN_POINT('Ctrl Pts',(34.8124542051494,13.4481598270206,78.7027629943066));
#134290=CARTESIAN_POINT('Ctrl Pts',(34.7029353862565,13.4752955310091,78.6658669209103));
#134291=CARTESIAN_POINT('Ctrl Pts',(34.5892300455026,13.4992036211595,78.6359530878952));
#134292=CARTESIAN_POINT('Ctrl Pts',(34.4722724330095,13.5196689246599,78.6134911795104));
#134293=CARTESIAN_POINT('Ctrl Pts',(34.3529487854807,13.536525360577,78.5988334811408));
#134294=CARTESIAN_POINT('Ctrl Pts',(34.2321151716127,13.5496335413214,78.5922569555576));
#134295=CARTESIAN_POINT('Ctrl Pts',(34.1105699318438,13.5589198993391,78.5938744656302));
#134296=CARTESIAN_POINT('Ctrl Pts',(33.9891475214067,13.5642122072015,78.6039717921799));
#134297=CARTESIAN_POINT('Ctrl Pts',(33.8683813111162,13.5658193574116,78.621834011338));
#134298=CARTESIAN_POINT('Ctrl Pts',(33.7893531292966,13.5635153199518,78.6406889999889));
#134299=CARTESIAN_POINT('Ctrl Pts',(33.7498180546891,13.56236268945,78.650121500723));
#134300=CARTESIAN_POINT('Ctrl Pts',(36.2117870627125,13.731466576071,79.1317548552529));
#134301=CARTESIAN_POINT('Ctrl Pts',(36.1637348888923,13.7660243550344,79.0619065056057));
#134302=CARTESIAN_POINT('Ctrl Pts',(36.1156827150721,13.8005821339978,78.9920581559585));
#134303=CARTESIAN_POINT('Ctrl Pts',(36.067630541252,13.8351399129612,78.9222098063113));
#134304=CARTESIAN_POINT('Ctrl Pts',(36.0436065071205,13.852417326142,78.8872886153943));
#134305=CARTESIAN_POINT('Ctrl Pts',(35.9923087529454,13.8893092356887,78.8127225097455));
#134306=CARTESIAN_POINT('Ctrl Pts',(35.9013880959124,13.9401153189454,78.7100025341022));
#134307=CARTESIAN_POINT('Ctrl Pts',(35.7958684940579,13.9911722275058,78.606777171674));
#134308=CARTESIAN_POINT('Ctrl Pts',(35.6773128854183,14.0400985472753,78.5080807209751));
#134309=CARTESIAN_POINT('Ctrl Pts',(35.5479476310375,14.0862484994258,78.415498960707));
#134310=CARTESIAN_POINT('Ctrl Pts',(35.4092346850833,14.1290516801646,78.330544171871));
#134311=CARTESIAN_POINT('Ctrl Pts',(35.2625355537129,14.16820270898,78.254228706184));
#134312=CARTESIAN_POINT('Ctrl Pts',(35.1090331574187,14.2034821063204,78.1874101995993));
#134313=CARTESIAN_POINT('Ctrl Pts',(34.9498411966155,14.2347418113983,78.1307946248619));
#134314=CARTESIAN_POINT('Ctrl Pts',(34.786010574763,14.2618838966983,78.0849619730775));
#134315=CARTESIAN_POINT('Ctrl Pts',(34.6185511567095,14.2848431924266,78.0503886163853));
#134316=CARTESIAN_POINT('Ctrl Pts',(34.4484483884156,14.3035755304223,78.0274544727356));
#134317=CARTESIAN_POINT('Ctrl Pts',(34.2766775950479,14.3180385947544,78.0164841582442));
#134318=CARTESIAN_POINT('Ctrl Pts',(34.1041767867636,14.3282324593606,78.017610234519));
#134319=CARTESIAN_POINT('Ctrl Pts',(33.9319683359579,14.3340234493632,78.031253517041));
#134320=CARTESIAN_POINT('Ctrl Pts',(33.7606990047544,14.3357830595542,78.0563719770334));
#134321=CARTESIAN_POINT('Ctrl Pts',(33.6485441033515,14.3332597659042,78.0834328777287));
#134322=CARTESIAN_POINT('Ctrl Pts',(33.5924368730891,14.33199744909,78.096970513333));
#134323=CARTESIAN_POINT('Ctrl Pts',(37.0959814013386,13.6477787622855,78.702474297618));
#134324=CARTESIAN_POINT('Ctrl Pts',(37.0097034037152,13.7013526595415,78.5841710380778));
#134325=CARTESIAN_POINT('Ctrl Pts',(36.9234254060918,13.7549265567976,78.4658677785376));
#134326=CARTESIAN_POINT('Ctrl Pts',(36.8371474084684,13.8085004540536,78.3475645189974));
#134327=CARTESIAN_POINT('Ctrl Pts',(36.7940120954343,13.8352851140162,78.2884179431172));
#134328=CARTESIAN_POINT('Ctrl Pts',(36.7019066367019,13.8924775445173,78.1621241452819));
#134329=CARTESIAN_POINT('Ctrl Pts',(36.5581875931855,13.9608351698212,78.0081066363786));
#134330=CARTESIAN_POINT('Ctrl Pts',(36.3971992371637,14.0271544164863,77.8570288914372));
#134331=CARTESIAN_POINT('Ctrl Pts',(36.222593119429,14.0876963855601,77.7175015279586));
#134332=CARTESIAN_POINT('Ctrl Pts',(36.0364710403563,14.142999223141,77.5892429153225));
#134333=CARTESIAN_POINT('Ctrl Pts',(35.8403743068097,14.192863522938,77.4735019242573));
#134334=CARTESIAN_POINT('Ctrl Pts',(35.6355466289455,14.2374572864306,77.3707704377697));
#134335=CARTESIAN_POINT('Ctrl Pts',(35.4230966202696,14.276886944725,77.2816655621943));
#134336=CARTESIAN_POINT('Ctrl Pts',(35.2041927400843,14.311265480877,77.2067675372761));
#134337=CARTESIAN_POINT('Ctrl Pts',(34.9799734310699,14.3407075552358,77.1465972403352));
#134338=CARTESIAN_POINT('Ctrl Pts',(34.7515346550071,14.3653281048325,77.1016031279655));
#134339=CARTESIAN_POINT('Ctrl Pts',(34.5199775631649,14.3852288528339,77.0721671077446));
#134340=CARTESIAN_POINT('Ctrl Pts',(34.2864180549368,14.4004840439715,77.0586422814665));
#134341=CARTESIAN_POINT('Ctrl Pts',(34.0519617518984,14.4111803943695,77.061167287698));
#134342=CARTESIAN_POINT('Ctrl Pts',(33.8178537815412,14.4172370026292,77.080288199522));
#134343=CARTESIAN_POINT('Ctrl Pts',(33.5848907865268,14.4190784205302,77.1146266745727));
#134344=CARTESIAN_POINT('Ctrl Pts',(33.4321409917259,14.416437075733,77.1512239629719));
#134345=CARTESIAN_POINT('Ctrl Pts',(33.3557255359391,14.415115702,77.169532324546));
#134346=CARTESIAN_POINT('Origin',(58.0152958556891,-0.499074165591486,68.638644839116));
#134347=CARTESIAN_POINT('',(69.9613704439522,11.9506555274059,75.9079901281648));
#134348=CARTESIAN_POINT('',(70.5465864373914,11.5358766795373,76.3475297110445));
#134349=CARTESIAN_POINT('Ctrl Pts',(69.9613704417151,11.95065551084,75.9079901160842));
#134350=CARTESIAN_POINT('Ctrl Pts',(69.9615209599404,11.9500108384424,75.9088462703833));
#134351=CARTESIAN_POINT('Ctrl Pts',(69.9616732757947,11.9493665883909,75.909701329011));
#134352=CARTESIAN_POINT('Ctrl Pts',(69.9618273824786,11.9487227594097,75.9105552952276));
#134353=CARTESIAN_POINT('Ctrl Pts',(69.9652026681753,11.9346214453371,75.9292590910818));
#134354=CARTESIAN_POINT('Ctrl Pts',(69.9694325138086,11.9207229649935,75.9474390034307));
#134355=CARTESIAN_POINT('Ctrl Pts',(69.9744552735693,11.907002133724,75.965153413181));
#134356=CARTESIAN_POINT('Ctrl Pts',(69.9796461127933,11.892822154483,75.9834606102881));
#134357=CARTESIAN_POINT('Ctrl Pts',(69.9856840690767,11.8788312841992,76.0012713858033));
#134358=CARTESIAN_POINT('Ctrl Pts',(69.9925567342574,11.8649965119743,76.0186414871835));
#134359=CARTESIAN_POINT('Ctrl Pts',(69.999429399438,11.8511617397494,76.0360115885636));
#134360=CARTESIAN_POINT('Ctrl Pts',(70.007137210894,11.837482415808,76.0529417523489));
#134361=CARTESIAN_POINT('Ctrl Pts',(70.0157168351401,11.8239301149553,76.0694679524188));
#134362=CARTESIAN_POINT('Ctrl Pts',(70.0203011593225,11.8166887558067,76.078298345971));
#134363=CARTESIAN_POINT('Ctrl Pts',(70.0251185502922,11.8094823846021,76.0870177768771));
#134364=CARTESIAN_POINT('Ctrl Pts',(70.0301626360558,11.8023273164306,76.0956060680119));
#134365=CARTESIAN_POINT('Ctrl Pts',(70.041856427489,11.7857395979006,76.1155164521738));
#134366=CARTESIAN_POINT('Ctrl Pts',(70.0547716746612,11.7694286456886,76.1347198592858));
#134367=CARTESIAN_POINT('Ctrl Pts',(70.0687605648971,11.7536201996829,76.1529698102241));
#134368=CARTESIAN_POINT('Ctrl Pts',(70.0819348412068,11.738732325649,76.1701570132291));
#134369=CARTESIAN_POINT('Ctrl Pts',(70.0960605979567,11.7242907164731,76.1864980767739));
#134370=CARTESIAN_POINT('Ctrl Pts',(70.1109807244523,11.7104662987638,76.2018184769042));
#134371=CARTESIAN_POINT('Ctrl Pts',(70.1119032907124,11.7096114842053,76.2027657935543));
#134372=CARTESIAN_POINT('Ctrl Pts',(70.1128288849219,11.708759021985,76.2037092195967));
#134373=CARTESIAN_POINT('Ctrl Pts',(70.1137574663665,11.707908949425,76.2046487185943));
#134374=CARTESIAN_POINT('Ctrl Pts',(70.1269673712688,11.6958159039061,76.2180139354918));
#134375=CARTESIAN_POINT('Ctrl Pts',(70.1407853915092,11.6842152396375,76.2305725267381));
#134376=CARTESIAN_POINT('Ctrl Pts',(70.1551548756988,11.6731568727412,76.2422830906839));
#134377=CARTESIAN_POINT('Ctrl Pts',(70.1770158002945,11.6563332956608,76.2600988836529));
#134378=CARTESIAN_POINT('Ctrl Pts',(70.2001503279608,11.6407646475148,76.275953100659));
#134379=CARTESIAN_POINT('Ctrl Pts',(70.2242568536363,11.6266454419759,76.2897076010034));
#134380=CARTESIAN_POINT('Ctrl Pts',(70.2308104620605,11.6228069898651,76.2934469042335));
#134381=CARTESIAN_POINT('Ctrl Pts',(70.2374361978791,11.6190756679541,76.2970309202755));
#134382=CARTESIAN_POINT('Ctrl Pts',(70.2441285749294,11.6154554353968,76.3004566166471));
#134383=CARTESIAN_POINT('Ctrl Pts',(70.2636026522798,11.6049209588846,76.3104250143655));
#134384=CARTESIAN_POINT('Ctrl Pts',(70.2836308477456,11.5952996211569,76.3190897115059));
#134385=CARTESIAN_POINT('Ctrl Pts',(70.3039992462445,11.5867074310029,76.3263646979402));
#134386=CARTESIAN_POINT('Ctrl Pts',(70.3087115952567,11.5847195771819,76.3280478089192));
#134387=CARTESIAN_POINT('Ctrl Pts',(70.3134421864876,11.5827866695546,76.329656700523));
#134388=CARTESIAN_POINT('Ctrl Pts',(70.3181884448014,11.5809098859167,76.3311906113044));
#134389=CARTESIAN_POINT('Ctrl Pts',(70.3385421726943,11.5728615368899,76.3377685934946));
#134390=CARTESIAN_POINT('Ctrl Pts',(70.3591820291187,11.5658477224918,76.3429650876769));
#134391=CARTESIAN_POINT('Ctrl Pts',(70.3798508972394,11.5598993598248,76.3468012621473));
#134392=CARTESIAN_POINT('Ctrl Pts',(70.3843330575984,11.558609423908,76.347633158168));
#134393=CARTESIAN_POINT('Ctrl Pts',(70.3888166800923,11.5573694772226,76.3484012058652));
#134394=CARTESIAN_POINT('Ctrl Pts',(70.3932993148755,11.5561796438526,76.3491058224419));
#134395=CARTESIAN_POINT('Ctrl Pts',(70.4086833100591,11.5520962438616,76.3515240024957));
#134396=CARTESIAN_POINT('Ctrl Pts',(70.4240634684271,11.5486366102045,76.3531516559179));
#134397=CARTESIAN_POINT('Ctrl Pts',(70.4394636545303,11.5457823417567,76.3540132419426));
#134398=CARTESIAN_POINT('Ctrl Pts',(70.4545216765585,11.542991489953,76.3548556850957));
#134399=CARTESIAN_POINT('Ctrl Pts',(70.4695994969117,11.5407791919864,76.3549658203571));
#134400=CARTESIAN_POINT('Ctrl Pts',(70.4847292631062,11.5391574455067,76.3543277140276));
#134401=CARTESIAN_POINT('Ctrl Pts',(70.4887566369168,11.5387257548106,76.3541578572905));
#134402=CARTESIAN_POINT('Ctrl Pts',(70.492787717123,11.5383360820643,76.3539347604712));
#134403=CARTESIAN_POINT('Ctrl Pts',(70.4968231425723,11.537989046077,76.3536576266829));
#134404=CARTESIAN_POINT('Ctrl Pts',(70.5119504136597,11.5366881405039,76.3526187577966));
#134405=CARTESIAN_POINT('Ctrl Pts',(70.5271393428903,11.5359838640424,76.3508236001816));
#134406=CARTESIAN_POINT('Ctrl Pts',(70.5424074352129,11.5358880698067,76.3482528518716));
#134407=CARTESIAN_POINT('Ctrl Pts',(70.5437998025831,11.535879333891,76.3480184135418));
#134408=CARTESIAN_POINT('Ctrl Pts',(70.5451928217474,11.5358756809335,76.3477774978885));
#134409=CARTESIAN_POINT('Ctrl Pts',(70.5465865013678,11.5358771335693,76.3475300739397));
#134410=CARTESIAN_POINT('',(69.083187826262,14.427762175719,70.9275690136187));
#134411=CARTESIAN_POINT('Origin',(68.3580209600691,-0.499074165591386,66.814943349163));
#134412=CARTESIAN_POINT('',(69.4827796255522,14.56707483593,70.3143821819286));
#134413=CARTESIAN_POINT('Ctrl Pts',(69.4827796254708,14.5670748341177,70.314382181467));
#134414=CARTESIAN_POINT('Ctrl Pts',(69.4361546598912,14.5670801487892,70.3225810935552));
#134415=CARTESIAN_POINT('Ctrl Pts',(69.3929252775548,14.5654384467918,70.3371198467491));
#134416=CARTESIAN_POINT('Ctrl Pts',(69.3523201741882,14.5622038470913,70.357789469697));
#134417=CARTESIAN_POINT('Ctrl Pts',(69.3464431011719,14.561735679865,70.3607811351088));
#134418=CARTESIAN_POINT('Ctrl Pts',(69.3406210002134,14.5612340569392,70.3639012146385));
#134419=CARTESIAN_POINT('Ctrl Pts',(69.3348515290093,14.5606990571707,70.3671490540045));
#134420=CARTESIAN_POINT('Ctrl Pts',(69.2892203485125,14.5564677038735,70.3928364591566));
#134421=CARTESIAN_POINT('Ctrl Pts',(69.2468815147492,14.5501525445106,70.4265166668452));
#134422=CARTESIAN_POINT('Ctrl Pts',(69.2107930600392,14.5419632084295,70.466287573233));
#134423=CARTESIAN_POINT('Ctrl Pts',(69.1747046053292,14.5337738723484,70.5060584796207));
#134424=CARTESIAN_POINT('Ctrl Pts',(69.1448663859906,14.5237071471177,70.5519192698477));
#134425=CARTESIAN_POINT('Ctrl Pts',(69.1225129952057,14.5120087061897,70.6020288875747));
#134426=CARTESIAN_POINT('Ctrl Pts',(69.1048716394728,14.5027762653526,70.6415755317713));
#134427=CARTESIAN_POINT('Ctrl Pts',(69.0918919799643,14.492523915542,70.6837676073393));
#134428=CARTESIAN_POINT('Ctrl Pts',(69.0838883173712,14.4816669226518,70.7266921111021));
#134429=CARTESIAN_POINT('Ctrl Pts',(69.0817505259648,14.4787670020429,70.738157316463));
#134430=CARTESIAN_POINT('Ctrl Pts',(69.0799677501241,14.4758242191456,70.7496748414087));
#134431=CARTESIAN_POINT('Ctrl Pts',(69.0785460067399,14.472847127587,70.7612083884841));
#134432=CARTESIAN_POINT('Ctrl Pts',(69.0718014080478,14.4587241233547,70.815922303375));
#134433=CARTESIAN_POINT('Ctrl Pts',(69.0731819728056,14.4438345223755,70.8709984930405));
#134434=CARTESIAN_POINT('Ctrl Pts',(69.0831878262661,14.4277621757181,70.9275690136177));
#134435=CARTESIAN_POINT('',(86.2245113351368,14.5670697090797,67.3623619192218));
#134436=CARTESIAN_POINT('',(86.2245112270591,14.56706714654,67.362361309341));
#134437=CARTESIAN_POINT('',(88.2224712053084,14.9706018766884,64.2964292184508));
#134438=CARTESIAN_POINT('Ctrl Pts',(88.2224711443474,14.9705962804753,64.2964288732062));
#134439=CARTESIAN_POINT('Ctrl Pts',(88.2354174097173,14.9659270873237,64.3698241832643));
#134440=CARTESIAN_POINT('Ctrl Pts',(88.2440702868443,14.9611459120881,64.4370977395704));
#134441=CARTESIAN_POINT('Ctrl Pts',(88.2498443108715,14.9565213241849,64.4979844054106));
#134442=CARTESIAN_POINT('Ctrl Pts',(88.2556032614391,14.9519088090647,64.55871212271));
#134443=CARTESIAN_POINT('Ctrl Pts',(88.2584984067044,14.9474520828081,64.6130864601102));
#134444=CARTESIAN_POINT('Ctrl Pts',(88.2599335408691,14.9433657903529,64.660846100787));
#134445=CARTESIAN_POINT('Ctrl Pts',(88.260279627699,14.9423803688941,64.6723634787769));
#134446=CARTESIAN_POINT('Ctrl Pts',(88.2605408080041,14.9414162521163,64.6834961810361));
#134447=CARTESIAN_POINT('Ctrl Pts',(88.2607367681307,14.940475995797,64.6942405386883));
#134448=CARTESIAN_POINT('Ctrl Pts',(88.2615381757232,14.9366306800897,64.73818116041));
#134449=CARTESIAN_POINT('Ctrl Pts',(88.2612428319285,14.9331827046254,64.7756951912911));
#134450=CARTESIAN_POINT('Ctrl Pts',(88.2605168109006,14.9302585107549,64.8068121861044));
#134451=CARTESIAN_POINT('Ctrl Pts',(88.2597778818599,14.9272823272991,64.8384824136122));
#134452=CARTESIAN_POINT('Ctrl Pts',(88.2585928411687,14.9248486301795,64.863526205497));
#134453=CARTESIAN_POINT('Ctrl Pts',(88.2576632884832,14.9230369568775,64.8819711113012));
#134454=CARTESIAN_POINT('Ctrl Pts',(88.2574282754275,14.9225789227226,64.8866344227448));
#134455=CARTESIAN_POINT('Ctrl Pts',(88.2572095893997,14.9221603881518,64.8908759129916));
#134456=CARTESIAN_POINT('Ctrl Pts',(88.2570185607416,14.9217821181808,64.8946959828093));
#134457=CARTESIAN_POINT('Ctrl Pts',(88.2565963132184,14.9209459946378,64.9031398206904));
#134458=CARTESIAN_POINT('Ctrl Pts',(88.2562712022575,14.9203072488869,64.9095280000816));
#134459=CARTESIAN_POINT('Ctrl Pts',(88.2560899903014,14.9198719047267,64.9138655813363));
#134460=CARTESIAN_POINT('Ctrl Pts',(88.2560673388069,14.9198174867067,64.9144077789932));
#134461=CARTESIAN_POINT('Ctrl Pts',(88.2560468972339,14.9197662418315,64.9149179318388));
#134462=CARTESIAN_POINT('Ctrl Pts',(88.256028723928,14.9197181776152,64.9153960459549));
#134463=CARTESIAN_POINT('Ctrl Pts',(88.256010550622,14.919670113399,64.9158741600709));
#134464=CARTESIAN_POINT('Ctrl Pts',(88.2558562461538,14.9192592168772,64.9199572610432));
#134465=CARTESIAN_POINT('Ctrl Pts',(88.2557457474718,14.9189792843175,64.9227300865272));
#134466=CARTESIAN_POINT('Ctrl Pts',(88.2555247501079,14.918419419198,64.9282757374953));
#134467=CARTESIAN_POINT('Ctrl Pts',(88.2552877605797,14.9178571301713,64.9338196072238));
#134468=CARTESIAN_POINT('Ctrl Pts',(88.2550348046356,14.9172924397025,64.9393616051558));
#134469=CARTESIAN_POINT('Ctrl Pts',(88.2545288927474,14.9161630587648,64.95044560102));
#134470=CARTESIAN_POINT('Ctrl Pts',(88.2539591151671,14.915024071526,64.9615221095362));
#134471=CARTESIAN_POINT('Ctrl Pts',(88.2533253068796,14.9138756948231,64.9725901620931));
#134472=CARTESIAN_POINT('Ctrl Pts',(88.2507900737295,14.9092821880115,65.0168623723205));
#134473=CARTESIAN_POINT('Ctrl Pts',(88.2472303467211,14.9045383476269,65.0609992727766));
#134474=CARTESIAN_POINT('Ctrl Pts',(88.2426573629239,14.8996570010548,65.1049540329731));
#134475=CARTESIAN_POINT('Ctrl Pts',(88.2335113953295,14.8898943079108,65.1928635533662));
#134476=CARTESIAN_POINT('Ctrl Pts',(88.2203306558311,14.8795792338678,65.2800557341386));
#134477=CARTESIAN_POINT('Ctrl Pts',(88.2033243438967,14.868814256945,65.3662407316185));
#134478=CARTESIAN_POINT('Ctrl Pts',(88.1863180319623,14.8580492800221,65.4524257290985));
#134479=CARTESIAN_POINT('Ctrl Pts',(88.1652121891123,14.8467374872076,65.538371625361));
#134480=CARTESIAN_POINT('Ctrl Pts',(88.1397815886332,14.8350748453393,65.6231584256026));
#134481=CARTESIAN_POINT('Ctrl Pts',(88.1143509881541,14.823412203471,65.7079452258441));
#134482=CARTESIAN_POINT('Ctrl Pts',(88.0845956189412,14.8113991791083,65.7915728670862));
#134483=CARTESIAN_POINT('Ctrl Pts',(88.0502920910252,14.7992858156939,65.8731317712184));
#134484=CARTESIAN_POINT('Ctrl Pts',(88.0159885631092,14.7871724522795,65.9546906753507));
#134485=CARTESIAN_POINT('Ctrl Pts',(87.9773977777193,14.7749447602975,66.034244508071));
#134486=CARTESIAN_POINT('Ctrl Pts',(87.934822257459,14.7627705061534,66.1114563460231));
#134487=CARTESIAN_POINT('Ctrl Pts',(87.9135344973288,14.7566833790813,66.1500622649992));
#134488=CARTESIAN_POINT('Ctrl Pts',(87.8912508018819,14.7506097358628,66.1880826405594));
#134489=CARTESIAN_POINT('Ctrl Pts',(87.8680103019539,14.744571231414,66.2254747634526));
#134490=CARTESIAN_POINT('Ctrl Pts',(87.8563900519898,14.7415519791896,66.2441708248993));
#134491=CARTESIAN_POINT('Ctrl Pts',(87.8445306010193,14.7385415169717,66.2627098238248));
#134492=CARTESIAN_POINT('Ctrl Pts',(87.8324369300872,14.7355425866634,66.2810863695465));
#134493=CARTESIAN_POINT('Ctrl Pts',(87.8263900946211,14.7340431215092,66.2902746424073));
#134494=CARTESIAN_POINT('Ctrl Pts',(87.8202847041712,14.732546539589,66.2994223020043));
#134495=CARTESIAN_POINT('Ctrl Pts',(87.8141213836461,14.731053185234,66.3085286732507));
#134496=CARTESIAN_POINT('Ctrl Pts',(87.8094988932523,14.7299331694678,66.3153584516855));
#134497=CARTESIAN_POINT('Ctrl Pts',(87.8048438171917,14.728814969226,66.3221650054258));
#134498=CARTESIAN_POINT('Ctrl Pts',(87.8001564201215,14.7276987301555,66.3289480490743));
#134499=CARTESIAN_POINT('Ctrl Pts',(87.7985939544314,14.7273266504653,66.3312090636238));
#134500=CARTESIAN_POINT('Ctrl Pts',(87.7958048109861,14.7266652022143,66.3352252043825));
#134501=CARTESIAN_POINT('Ctrl Pts',(87.7954582592733,14.7265831502223,66.3357232454002));
#134502=CARTESIAN_POINT('Ctrl Pts',(87.7892255990741,14.7251074622792,66.3446804091176));
#134503=CARTESIAN_POINT('Ctrl Pts',(87.7771203691377,14.7220802144287,66.3629316915066));
#134504=CARTESIAN_POINT('Ctrl Pts',(87.7582190801493,14.7175870837742,66.3897974811068));
#134505=CARTESIAN_POINT('Ctrl Pts',(87.7434896619196,14.7140856717483,66.4107334845367));
#134506=CARTESIAN_POINT('Ctrl Pts',(87.7246330858878,14.7096923853249,66.4369005971158));
#134507=CARTESIAN_POINT('Ctrl Pts',(87.7012115473724,14.7044267669997,66.4679728232031));
#134508=CARTESIAN_POINT('Ctrl Pts',(87.674473121858,14.6984154478336,66.5034454033777));
#134509=CARTESIAN_POINT('Ctrl Pts',(87.6416817796703,14.6912835176468,66.5452343893276));
#134510=CARTESIAN_POINT('Ctrl Pts',(87.6016632841941,14.6831867054477,66.5922686344081));
#134511=CARTESIAN_POINT('Ctrl Pts',(87.581654036456,14.6791382993481,66.6157857569484));
#134512=CARTESIAN_POINT('Ctrl Pts',(87.5598333021963,14.6748502795821,66.6406073953481));
#134513=CARTESIAN_POINT('Ctrl Pts',(87.5360298823028,14.6703529806913,66.666560780772));
#134514=CARTESIAN_POINT('Ctrl Pts',(87.5241281723561,14.6681043312459,66.6795374734839));
#134515=CARTESIAN_POINT('Ctrl Pts',(87.5117305795691,14.6658034992355,66.6927966415966));
#134516=CARTESIAN_POINT('Ctrl Pts',(87.4988146086698,14.6634551870718,66.7063137579672));
#134517=CARTESIAN_POINT('Ctrl Pts',(87.4923566232201,14.6622810309899,66.7130723161525));
#134518=CARTESIAN_POINT('Ctrl Pts',(87.4857690433586,14.6610950078844,66.7198953620615));
#134519=CARTESIAN_POINT('Ctrl Pts',(87.4790489920845,14.6598977774674,66.7267795971394));
#134520=CARTESIAN_POINT('Ctrl Pts',(87.4756889664475,14.6592991622588,66.7302217146783));
#134521=CARTESIAN_POINT('Ctrl Pts',(87.4722958229659,14.6586977454466,66.7336791295583));
#134522=CARTESIAN_POINT('Ctrl Pts',(87.468869200926,14.6580936125992,66.7371514217866));
#134523=CARTESIAN_POINT('Ctrl Pts',(87.465442578886,14.6574894797517,66.7406237140148));
#134524=CARTESIAN_POINT('Ctrl Pts',(87.4605108792611,14.6566259272614,66.7455857192466));
#134525=CARTESIAN_POINT('Ctrl Pts',(87.4584885375708,14.6562731534097,66.7476125064636));
#134526=CARTESIAN_POINT('Ctrl Pts',(87.4054627353892,14.647023422484,66.8007548703619));
#134527=CARTESIAN_POINT('Ctrl Pts',(87.3528925759193,14.6387686224732,66.8482170400251));
#134528=CARTESIAN_POINT('Ctrl Pts',(87.3017326677347,14.6314687994132,66.890577180893));
#134529=CARTESIAN_POINT('Ctrl Pts',(87.2904548578659,14.6298596093371,66.8999151494641));
#134530=CARTESIAN_POINT('Ctrl Pts',(87.2792455724829,14.6282966269739,66.9090051493782));
#134531=CARTESIAN_POINT('Ctrl Pts',(87.2681150271531,14.6267791040544,66.9178533143707));
#134532=CARTESIAN_POINT('Ctrl Pts',(87.2373038209364,14.6225783474673,66.9423465110782));
#134533=CARTESIAN_POINT('Ctrl Pts',(87.2070887730209,14.6187264164645,66.9649875047977));
#134534=CARTESIAN_POINT('Ctrl Pts',(87.1776452324069,14.6152048017754,66.9859073994173));
#134535=CARTESIAN_POINT('Ctrl Pts',(87.1629234620999,14.6134439944308,66.9963673467271));
#134536=CARTESIAN_POINT('Ctrl Pts',(87.1483941537617,14.611765699395,67.0063969940054));
#134537=CARTESIAN_POINT('Ctrl Pts',(87.1340767958401,14.61016726836,67.0160124828669));
#134538=CARTESIAN_POINT('Ctrl Pts',(87.1269181168793,14.6093680528425,67.0208202272977));
#134539=CARTESIAN_POINT('Ctrl Pts',(87.1198124253448,14.608588798866,67.0255244311162));
#134540=CARTESIAN_POINT('Ctrl Pts',(87.1127619828297,14.6078291613001,67.0301270865025));
#134541=CARTESIAN_POINT('Ctrl Pts',(87.1092367615721,14.6074493425172,67.0324284141957));
#134542=CARTESIAN_POINT('Ctrl Pts',(87.1057253525592,14.6070744275826,67.034704354724));
#134543=CARTESIAN_POINT('Ctrl Pts',(87.1022280339322,14.6067043722668,67.036955155796));
#134544=CARTESIAN_POINT('Ctrl Pts',(87.1004793746187,14.6065193446089,67.0380805563319));
#134545=CARTESIAN_POINT('Ctrl Pts',(87.098734237901,14.6063355318405,67.0391996720004));
#134546=CARTESIAN_POINT('Ctrl Pts',(87.0969926579404,14.6061529283869,67.0403125336566));
#134547=CARTESIAN_POINT('Ctrl Pts',(87.0952510779798,14.6059703249333,67.0414253953128));
#134548=CARTESIAN_POINT('Ctrl Pts',(87.092477517043,14.6056813486228,67.0431889842275));
#134549=CARTESIAN_POINT('Ctrl Pts',(87.09177862231,14.6056087403507,67.0436323873999));
#134550=CARTESIAN_POINT('Ctrl Pts',(87.0639156806064,14.6027140554189,67.0613096085345));
#134551=CARTESIAN_POINT('Ctrl Pts',(87.0183425494523,14.5983355081594,67.0885690084124));
#134552=CARTESIAN_POINT('Ctrl Pts',(86.9535310488286,14.5933892370839,67.1214652454699));
#134553=CARTESIAN_POINT('Ctrl Pts',(86.9142985945187,14.5903951025228,67.1413783797887));
#134554=CARTESIAN_POINT('Ctrl Pts',(86.8680167117813,14.5871934479021,67.1633571067526));
#134555=CARTESIAN_POINT('Ctrl Pts',(86.8143468322071,14.5839974444716,67.186528560568));
#134556=CARTESIAN_POINT('Ctrl Pts',(86.7417455207952,14.5796740876432,67.2178734778228));
#134557=CARTESIAN_POINT('Ctrl Pts',(86.6554329600215,14.5753575824665,67.2514350519375));
#134558=CARTESIAN_POINT('Ctrl Pts',(86.5547790289479,14.5721621883357,67.2826899772011));
#134559=CARTESIAN_POINT('Ctrl Pts',(86.4581051615004,14.5690931466663,67.3127090183829));
#134560=CARTESIAN_POINT('Ctrl Pts',(86.3482018854432,14.567063355292,67.3406014193676));
#134561=CARTESIAN_POINT('Ctrl Pts',(86.2245115502461,14.5670748341591,67.3623631391674));
#134562=CARTESIAN_POINT('',(88.0908006755043,14.9994907909963,63.5496885367596));
#134563=CARTESIAN_POINT('Origin',(88.0541760202691,-0.499074165591386,63.341979795825));
#134564=CARTESIAN_POINT('',(91.9155428748487,14.9991665202061,62.8752788267285));
#134565=CARTESIAN_POINT('Ctrl Pts',(91.9155428714327,14.9991665204673,62.8752788073534));
#134566=CARTESIAN_POINT('Ctrl Pts',(90.6406264262798,14.9978694380589,63.1000630531378));
#134567=CARTESIAN_POINT('Ctrl Pts',(89.3657116351699,14.9978694380387,63.3248649304237));
#134568=CARTESIAN_POINT('Ctrl Pts',(88.0907987597691,14.99868011451,63.549677672236));
#134569=CARTESIAN_POINT('',(94.5611372758984,0.791525290730867,77.8791831282366));
#134570=CARTESIAN_POINT('Ctrl Pts',(94.5611183165859,0.791951999546357,
77.8790756181347));
#134571=CARTESIAN_POINT('Ctrl Pts',(94.5585207580642,0.993626479914886,
77.8644747740234));
#134572=CARTESIAN_POINT('Ctrl Pts',(94.5463339987654,1.68049538207119,77.7953921430714));
#134573=CARTESIAN_POINT('Ctrl Pts',(94.5098935016048,2.87766921816737,77.5886537952174));
#134574=CARTESIAN_POINT('Ctrl Pts',(94.4423986509273,4.30232735919002,77.2059804831616));
#134575=CARTESIAN_POINT('Ctrl Pts',(94.3207402637469,6.15219286716509,76.5155669569138));
#134576=CARTESIAN_POINT('Ctrl Pts',(94.1113738053345,8.32212312656844,75.3288542270853));
#134577=CARTESIAN_POINT('Ctrl Pts',(93.6699846192174,11.3677656920828,72.8250722276183));
#134578=CARTESIAN_POINT('Ctrl Pts',(93.087946136268,13.5971623798519,69.524355250224));
#134579=CARTESIAN_POINT('Ctrl Pts',(92.4297040189939,14.7677508337306,65.7913701368731));
#134580=CARTESIAN_POINT('Ctrl Pts',(92.0866907650382,14.9860768541558,63.8460104975704));
#134581=CARTESIAN_POINT('Ctrl Pts',(91.9155428748487,14.9991665202061,62.8752788267284));
#134582=CARTESIAN_POINT('',(88.0594949212713,0.791921988601748,79.0254659908079));
#134583=CARTESIAN_POINT('',(91.3065552302825,0.793741304715882,78.4527675754261));
#134584=CARTESIAN_POINT('',(80.8776257882291,11.5357844058001,74.5260054838839));
#134585=CARTESIAN_POINT('Ctrl Pts',(88.0594324394305,0.791351947310389,
79.025455896363));
#134586=CARTESIAN_POINT('Ctrl Pts',(88.0477203701159,0.973879312121693,
79.0119992383338));
#134587=CARTESIAN_POINT('Ctrl Pts',(88.0320804261398,1.15611822191438,78.9959592578232));
#134588=CARTESIAN_POINT('Ctrl Pts',(88.0125470385509,1.33793703208646,78.9773660909821));
#134589=CARTESIAN_POINT('Ctrl Pts',(87.9931417220772,1.51856374295249,78.9588948306769));
#134590=CARTESIAN_POINT('Ctrl Pts',(87.9698935769308,1.69877638732119,78.9379035863993));
#134591=CARTESIAN_POINT('Ctrl Pts',(87.9427961451028,1.87842090265091,78.9144027844327));
#134592=CARTESIAN_POINT('Ctrl Pts',(87.9211783458309,2.02173777110342,78.8956543058732));
#134593=CARTESIAN_POINT('Ctrl Pts',(87.8971098401237,2.16469267454061,78.8753082141352));
#134594=CARTESIAN_POINT('Ctrl Pts',(87.8705704964911,2.30719242424511,78.853362054785));
#134595=CARTESIAN_POINT('Ctrl Pts',(87.8361333749774,2.49209832335759,78.824884991947));
#134596=CARTESIAN_POINT('Ctrl Pts',(87.7975366690727,2.67623903058067,78.7937140384208));
#134597=CARTESIAN_POINT('Ctrl Pts',(87.7548208470993,2.85957500628548,78.7599011198712));
#134598=CARTESIAN_POINT('Ctrl Pts',(87.7122905662646,3.04211464086624,78.7262350716643));
#134599=CARTESIAN_POINT('Ctrl Pts',(87.6656764501589,3.22385684472079,78.6899496925974));
#134600=CARTESIAN_POINT('Ctrl Pts',(87.6149908274805,3.4047205988487,78.6510856509235));
#134601=CARTESIAN_POINT('Ctrl Pts',(87.5721441382589,3.55761233924866,78.6182322414653));
#134602=CARTESIAN_POINT('Ctrl Pts',(87.5263873425785,3.709875733188,78.5835358498526));
#134603=CARTESIAN_POINT('Ctrl Pts',(87.4777157295167,3.86143569573502,78.5470172182685));
#134604=CARTESIAN_POINT('Ctrl Pts',(87.4198385260649,4.04166121602626,78.5035915716335));
#134605=CARTESIAN_POINT('Ctrl Pts',(87.3578374371053,4.220915970472,78.4575823211593));
#134606=CARTESIAN_POINT('Ctrl Pts',(87.2917265304253,4.39898836359106,78.4090258963552));
#134607=CARTESIAN_POINT('Ctrl Pts',(87.2195795766543,4.59331909295807,78.3560361808672));
#134608=CARTESIAN_POINT('Ctrl Pts',(87.1425377435868,4.78624112568613,78.3000124822576));
#134609=CARTESIAN_POINT('Ctrl Pts',(87.0606094891262,4.9776696797924,78.2410222443041));
#134610=CARTESIAN_POINT('Ctrl Pts',(87.0095176912571,5.09704765332733,78.2042349682465));
#134611=CARTESIAN_POINT('Ctrl Pts',(86.9565254694602,5.21584382961004,78.1662941261412));
#134612=CARTESIAN_POINT('Ctrl Pts',(86.9016348008891,5.33402749986044,78.1272179048115));
#134613=CARTESIAN_POINT('Ctrl Pts',(86.8162754043854,5.51781259542876,78.0664512434249));
#134614=CARTESIAN_POINT('Ctrl Pts',(86.7263296708448,5.70009605369247,78.0029471940521));
#134615=CARTESIAN_POINT('Ctrl Pts',(86.6318090499446,5.88075710407649,77.9367702818263));
#134616=CARTESIAN_POINT('Ctrl Pts',(86.6025492456507,5.9366825405306,77.9162845562559));
#134617=CARTESIAN_POINT('Ctrl Pts',(86.5728510453442,5.99245213998999,77.8955427711251));
#134618=CARTESIAN_POINT('Ctrl Pts',(86.5427148301024,6.0480613217974,77.8745470633363));
#134619=CARTESIAN_POINT('Ctrl Pts',(86.4789708368259,6.16568562474364,77.8301370322362));
#134620=CARTESIAN_POINT('Ctrl Pts',(86.4132669540331,6.28259506106173,77.7845898555511));
#134621=CARTESIAN_POINT('Ctrl Pts',(86.3456058938825,6.39875192413486,77.7379209342159));
#134622=CARTESIAN_POINT('Ctrl Pts',(86.3168914034263,6.44804741446146,77.7181152395771));
#134623=CARTESIAN_POINT('Ctrl Pts',(86.2878243493149,6.49720740280034,77.6981074633652));
#134624=CARTESIAN_POINT('Ctrl Pts',(86.2584050800181,6.54622874504472,77.6778986926338));
#134625=CARTESIAN_POINT('Ctrl Pts',(86.253163470472,6.55496284149277,77.6742981108344));
#134626=CARTESIAN_POINT('Ctrl Pts',(86.2479106800764,6.56369253576868,77.6706911487874));
#134627=CARTESIAN_POINT('Ctrl Pts',(86.2426466960718,6.57241782802459,77.6670778101688));
#134628=CARTESIAN_POINT('Ctrl Pts',(86.2252422795267,6.60126643789267,77.6551309557747));
#134629=CARTESIAN_POINT('Ctrl Pts',(86.2077156177023,6.63006680114151,77.6431144372659));
#134630=CARTESIAN_POINT('Ctrl Pts',(86.1900667695632,6.65881836985443,77.6310285888921));
#134631=CARTESIAN_POINT('Ctrl Pts',(86.1812423454936,6.67319415421089,77.6249856647052));
#134632=CARTESIAN_POINT('Ctrl Pts',(86.1723873748607,6.68755773998491,77.6189254081387));
#134633=CARTESIAN_POINT('Ctrl Pts',(86.1635018651202,6.70190905903075,77.6128478614586));
#134634=CARTESIAN_POINT('Ctrl Pts',(86.1555510918172,6.71475065030288,77.6074096595655));
#134635=CARTESIAN_POINT('Ctrl Pts',(86.1481823015576,6.72660935050173,77.602372145213));
#134636=CARTESIAN_POINT('Ctrl Pts',(86.1397676972441,6.7400973297256,77.5966226230958));
#134637=CARTESIAN_POINT('Ctrl Pts',(86.1387784302936,6.74168305040569,77.5959466777989));
#134638=CARTESIAN_POINT('Ctrl Pts',(86.1377746666064,6.74329125227717,77.5952608751832));
#134639=CARTESIAN_POINT('Ctrl Pts',(86.1367537260879,6.74492614805065,77.5945633936618));
#134640=CARTESIAN_POINT('Ctrl Pts',(86.00881390989,6.94980416100596,77.5071580492268));
#134641=CARTESIAN_POINT('Ctrl Pts',(85.8747726359394,7.15144056709324,77.4165864361061));
#134642=CARTESIAN_POINT('Ctrl Pts',(85.7346650950376,7.34973594036529,77.3230461454545));
#134643=CARTESIAN_POINT('Ctrl Pts',(85.5980353985829,7.54310909133311,77.2318277753671));
#134644=CARTESIAN_POINT('Ctrl Pts',(85.4556365520976,7.73330486201888,77.1377859535212));
#134645=CARTESIAN_POINT('Ctrl Pts',(85.3075056162184,7.92019078118287,77.0411321728384));
#134646=CARTESIAN_POINT('Ctrl Pts',(85.2388152472846,8.00685237323805,76.9963124745454));
#134647=CARTESIAN_POINT('Ctrl Pts',(85.1688923952485,8.09280168547449,76.9509315582908));
#134648=CARTESIAN_POINT('Ctrl Pts',(85.0977413507567,8.17802259737751,76.9050129474954));
#134649=CARTESIAN_POINT('Ctrl Pts',(84.9969947592835,8.29869147100831,76.839994316274));
#134650=CARTESIAN_POINT('Ctrl Pts',(84.8937705370257,8.41791117900397,76.7738927940239));
#134651=CARTESIAN_POINT('Ctrl Pts',(84.7881066860137,8.53565033322103,76.7067595560638));
#134652=CARTESIAN_POINT('Ctrl Pts',(84.693484094356,8.6410864289615,76.646641351954));
#134653=CARTESIAN_POINT('Ctrl Pts',(84.596905332987,8.74533506168276,76.5856957563942));
#134654=CARTESIAN_POINT('Ctrl Pts',(84.498353570467,8.84837818683794,76.5239687584006));
#134655=CARTESIAN_POINT('Ctrl Pts',(84.3940519360044,8.95743322653478,76.4586403805354));
#134656=CARTESIAN_POINT('Ctrl Pts',(84.2875543154507,9.06513757121163,76.3924346762747));
#134657=CARTESIAN_POINT('Ctrl Pts',(84.1788694032987,9.17147009623087,76.3254009623234));
#134658=CARTESIAN_POINT('Ctrl Pts',(84.1245269472227,9.22463635874049,76.2918841053477));
#134659=CARTESIAN_POINT('Ctrl Pts',(84.0696376676571,9.27745966607002,76.2581602424503));
#134660=CARTESIAN_POINT('Ctrl Pts',(84.0142026276105,9.32993746418419,76.2242354005939));
#134661=CARTESIAN_POINT('Ctrl Pts',(83.9864851075872,9.35617636324127,76.2072729796657));
#134662=CARTESIAN_POINT('Ctrl Pts',(83.958631147334,9.3823288843911,76.1902603133487));
#134663=CARTESIAN_POINT('Ctrl Pts',(83.9306408784229,9.4083947073915,76.1731981474495));
#134664=CARTESIAN_POINT('Ctrl Pts',(83.9091818797392,9.42837831180883,76.160117280069));
#134665=CARTESIAN_POINT('Ctrl Pts',(83.8882122260337,9.44778514997001,76.1473541205618));
#134666=CARTESIAN_POINT('Ctrl Pts',(83.8664227891014,9.46782515105231,76.1341113943047));
#134667=CARTESIAN_POINT('Ctrl Pts',(83.859790946544,9.473924534549,76.1300808323476));
#134668=CARTESIAN_POINT('Ctrl Pts',(83.8530829427933,9.48008228762863,76.1260058335305));
#134669=CARTESIAN_POINT('Ctrl Pts',(83.8462612763603,9.48633175977909,76.1218638914719));
#134670=CARTESIAN_POINT('Ctrl Pts',(83.6909822796265,9.62858611583186,76.0275824407875));
#134671=CARTESIAN_POINT('Ctrl Pts',(83.5339563944129,9.76553363640028,75.9337084657981));
#134672=CARTESIAN_POINT('Ctrl Pts',(83.3753719479445,9.89746523305497,75.8405159414567));
#134673=CARTESIAN_POINT('Ctrl Pts',(83.2891838353113,9.96916794770057,75.7898672936014));
#134674=CARTESIAN_POINT('Ctrl Pts',(83.2025346840625,10.0393887572179,75.7394193684984));
#134675=CARTESIAN_POINT('Ctrl Pts',(83.1154500868582,10.1081720505422,75.6892123862321));
#134676=CARTESIAN_POINT('Ctrl Pts',(82.9579334742314,10.2325856864502,75.5983991536893));
#134677=CARTESIAN_POINT('Ctrl Pts',(82.7989946428256,10.3522969956233,75.5083764411655));
#134678=CARTESIAN_POINT('Ctrl Pts',(82.6387110277812,10.4675211445887,75.419473812973));
#134679=CARTESIAN_POINT('Ctrl Pts',(82.4753962995857,10.5849242900358,75.3288899528878));
#134680=CARTESIAN_POINT('Ctrl Pts',(82.3106853535623,10.6976690143454,75.2394687192886));
#134681=CARTESIAN_POINT('Ctrl Pts',(82.1446200741637,10.8059675085606,75.1515243932705));
#134682=CARTESIAN_POINT('Ctrl Pts',(81.9734552235275,10.9175916581335,75.0608794524273));
#134683=CARTESIAN_POINT('Ctrl Pts',(81.8008515311353,11.0244924141495,74.9718033227587));
#134684=CARTESIAN_POINT('Ctrl Pts',(81.6268137343084,11.1268846371928,74.8846071328486));
#134685=CARTESIAN_POINT('Ctrl Pts',(81.5572992342724,11.1677823290862,74.8497790687317));
#134686=CARTESIAN_POINT('Ctrl Pts',(81.4875554957942,11.2079605398945,74.8152505821908));
#134687=CARTESIAN_POINT('Ctrl Pts',(81.4175811060443,11.247432161209,74.7810402061456));
#134688=CARTESIAN_POINT('Ctrl Pts',(81.256957695813,11.3380376876818,74.7025116575534));
#134689=CARTESIAN_POINT('Ctrl Pts',(81.0951223899492,11.4249207260478,74.6256609860501));
#134690=CARTESIAN_POINT('Ctrl Pts',(80.9320695380522,11.5081527096928,74.5508783706375));
#134691=CARTESIAN_POINT('Ctrl Pts',(80.9139367883308,11.5174087558808,74.5425619601423));
#134692=CARTESIAN_POINT('Ctrl Pts',(80.8957889348062,11.5266196385521,74.5342711021844));
#134693=CARTESIAN_POINT('Ctrl Pts',(80.8776259354588,11.5357854481567,74.5260063163204));
#134694=CARTESIAN_POINT('',(70.5465863094891,11.53587577156,76.347528985137));
#134695=CARTESIAN_POINT('Origin',(63.4339821949991,-0.499074165591486,67.683184237498));
#134696=CARTESIAN_POINT('',(65.1554518235812,13.43008177675,68.8079679196157));
#134697=CARTESIAN_POINT('Origin',(63.6783172724722,13.4301641189394,69.0684179803352));
#134698=CARTESIAN_POINT('',(67.333842554444,0.665543397954793,81.1622356683442));
#134699=CARTESIAN_POINT('Origin',(64.9111938245191,-0.499074165591386,67.422711970998));
#134700=CARTESIAN_POINT('Origin',(65.8566295019347,0.665611037261871,81.4226998345101));
#134701=CARTESIAN_POINT('Origin',(64.4693974219391,1.4210854715202E-14,
73.5553157898091));
#134702=CARTESIAN_POINT('',(67.3338425586293,-0.665543403176102,81.1622356920742));
#134703=CARTESIAN_POINT('Origin',(65.9466090514591,1.4210854715202E-14,
73.2948435233078));
#134704=CARTESIAN_POINT('Origin',(65.8566323754803,-0.665476912000534,81.4227161320649));
#134705=CARTESIAN_POINT('Origin',(64.4693974219391,1.4210854715202E-14,
73.5553157898091));
#134706=CARTESIAN_POINT('Origin',(62.8196722231591,1.4210854715202E-14,
73.84620685311));
#134707=CARTESIAN_POINT('',(94.5668566070113,1.85499763697787E-13,77.9116179430035));
#134708=CARTESIAN_POINT('Origin',(94.1728845515327,3.42614080963416,75.6787268466269));
#134709=CARTESIAN_POINT('',(94.5611364251491,-0.79152367744104,77.8791780069701));
#134710=CARTESIAN_POINT('Origin',(94.1728845250001,-3.42614191077933,75.6787266825563));
#134711=CARTESIAN_POINT('',(88.0594917515577,-0.791960232028162,79.0254638190457));
#134712=CARTESIAN_POINT('',(91.3040130871753,-0.793741771912361,78.4532214918126));
#134713=CARTESIAN_POINT('Origin',(82.8491886620102,-4.65600993454496E-7,
72.5661599447829));
#134714=CARTESIAN_POINT('Origin',(62.8196722231591,1.4210854715202E-14,
73.84620685311));
#134715=CARTESIAN_POINT('',(44.7346267930369,9.30978071375613E-8,86.6983316276));
#134716=CARTESIAN_POINT('Origin',(37.4857771329516,-0.268313559242106,83.3762268319904));
#134717=CARTESIAN_POINT('Origin',(37.5708463135294,0.26765030096014,83.4145770345828));
#134718=CARTESIAN_POINT('Ctrl Pts',(88.3300732516691,1.02797677064201,78.929837570272));
#134719=CARTESIAN_POINT('Ctrl Pts',(88.3504557367691,0.829610805066913,
78.9472771505469));
#134720=CARTESIAN_POINT('Ctrl Pts',(88.3844025449691,0.364027776906714,
78.976250751736));
#134721=CARTESIAN_POINT('Ctrl Pts',(88.3864239591691,-0.325044243107086,
78.977972504701));
#134722=CARTESIAN_POINT('Ctrl Pts',(88.3524181702692,-0.810557832525686,
78.948954580408));
#134723=CARTESIAN_POINT('Ctrl Pts',(88.3300322943691,-1.02835836804799,
78.9298017468989));
#134724=CARTESIAN_POINT('Ctrl Pts',(87.0482634675391,0.955316939249614,
79.392387743809));
#134725=CARTESIAN_POINT('Ctrl Pts',(87.0680695837392,0.771048317590214,
79.410443610716));
#134726=CARTESIAN_POINT('Ctrl Pts',(87.1010648505991,0.338398308666014,
79.440446636557));
#134727=CARTESIAN_POINT('Ctrl Pts',(87.1030300333491,-0.302162842145186,
79.442229937658));
#134728=CARTESIAN_POINT('Ctrl Pts',(87.0699766830691,-0.753349368884286,
79.412180128005));
#134729=CARTESIAN_POINT('Ctrl Pts',(87.0482237482091,-0.955671368820286,
79.392350572629));
#134730=CARTESIAN_POINT('Ctrl Pts',(85.9392714052091,0.783680110261714,
78.615892494063));
#134731=CARTESIAN_POINT('Ctrl Pts',(85.9549454524891,0.632390227145814,
78.632561950362));
#134732=CARTESIAN_POINT('Ctrl Pts',(85.9810378503591,0.277431166609014,
78.660241182834));
#134733=CARTESIAN_POINT('Ctrl Pts',(85.982590889989,-0.247718294763486,
78.6618849678071));
#134734=CARTESIAN_POINT('Ctrl Pts',(85.9564544208491,-0.617858911184986,
78.6341659430299));
#134735=CARTESIAN_POINT('Ctrl Pts',(85.9392398380891,-0.783971188810686,
78.615858527218));
#134736=CARTESIAN_POINT('Ctrl Pts',(85.9409580116291,0.658217438893014,
77.257024303179));
#134737=CARTESIAN_POINT('Ctrl Pts',(85.9524387298491,0.530897975386414,
77.271477122028));
#134738=CARTESIAN_POINT('Ctrl Pts',(85.9715146025091,0.232685512903214,
77.295444546582));
#134739=CARTESIAN_POINT('Ctrl Pts',(85.9726481316892,-0.207753685037586,
77.296865738237));
#134740=CARTESIAN_POINT('Ctrl Pts',(85.9535434649091,-0.518669073028486,
77.272869052471));
#134741=CARTESIAN_POINT('Ctrl Pts',(85.9409346167292,-0.658462558413086,
77.256995382944));
#134742=CARTESIAN_POINT('Ctrl Pts',(88.0595159253563,-0.790233462113526,
79.0256009152192));
#134743=CARTESIAN_POINT('Ctrl Pts',(88.0115976870962,-0.787497376323707,
79.0342820975747));
#134744=CARTESIAN_POINT('Ctrl Pts',(87.962523231512,-0.784546129529816,
79.0411633131422));
#134745=CARTESIAN_POINT('Ctrl Pts',(87.9124786883384,-0.781377432771924,
79.0460185829796));
#134746=CARTESIAN_POINT('Ctrl Pts',(87.8636188139199,-0.778283746310966,
79.0507589174792));
#134747=CARTESIAN_POINT('Ctrl Pts',(87.8138344699327,-0.774982752994071,
79.0535674336194));
#134748=CARTESIAN_POINT('Ctrl Pts',(87.7633439937735,-0.771476934775263,
79.0542538663812));
#134749=CARTESIAN_POINT('Ctrl Pts',(87.7134935528966,-0.768015557558482,
79.0549315976764));
#134750=CARTESIAN_POINT('Ctrl Pts',(87.6629550882688,-0.764354492275542,
79.0535400629856));
#134751=CARTESIAN_POINT('Ctrl Pts',(87.611979293738,-0.76050108358359,79.0499255435374));
#134752=CARTESIAN_POINT('Ctrl Pts',(87.5618006799654,-0.756707936105629,
79.0463675494535));
#134753=CARTESIAN_POINT('Ctrl Pts',(87.5111987980573,-0.752728411193017,
79.0406550275279));
#134754=CARTESIAN_POINT('Ctrl Pts',(87.4604462803083,-0.748574534984207,
79.0326786585723));
#134755=CARTESIAN_POINT('Ctrl Pts',(87.4352918048017,-0.746515748898587,
79.0287253300199));
#134756=CARTESIAN_POINT('Ctrl Pts',(87.41010080336,-0.744414212157575,79.0242165199435));
#134757=CARTESIAN_POINT('Ctrl Pts',(87.3849089575827,-0.742271852738476,
79.0191429675415));
#134758=CARTESIAN_POINT('Ctrl Pts',(87.3348606636315,-0.738015656709632,
79.0090634106785));
#134759=CARTESIAN_POINT('Ctrl Pts',(87.2848081894561,-0.733598098828918,
78.9967517500166));
#134760=CARTESIAN_POINT('Ctrl Pts',(87.2350455907678,-0.729037222401108,
78.9821710322096));
#134761=CARTESIAN_POINT('Ctrl Pts',(87.1832191844151,-0.724287192432773,
78.9669856072942));
#134762=CARTESIAN_POINT('Ctrl Pts',(87.1317079557453,-0.719381712102373,
78.9493383050321));
#134763=CARTESIAN_POINT('Ctrl Pts',(87.080855677245,-0.714346282895627,
78.9292470049815));
#134764=CARTESIAN_POINT('Ctrl Pts',(87.0328008475358,-0.709587859081028,
78.9102609530083));
#134765=CARTESIAN_POINT('Ctrl Pts',(86.9853352518275,-0.704713477305003,
78.8890928356417));
#134766=CARTESIAN_POINT('Ctrl Pts',(86.938747481068,-0.699748338979591,
78.8658102316267));
#134767=CARTESIAN_POINT('Ctrl Pts',(86.892300276527,-0.694798181639693,
78.8425978766823));
#134768=CARTESIAN_POINT('Ctrl Pts',(86.8467263411344,-0.689757877297502,
78.8172839288121));
#134769=CARTESIAN_POINT('Ctrl Pts',(86.8022989455266,-0.684655114927824,
78.7899853926447));
#134770=CARTESIAN_POINT('Ctrl Pts',(86.7579230677471,-0.679558269700754,
78.7627185117495));
#134771=CARTESIAN_POINT('Ctrl Pts',(86.7146917516815,-0.674399182542361,
78.7334719678742));
#134772=CARTESIAN_POINT('Ctrl Pts',(86.6728539796854,-0.669207152221488,
78.7024087800593));
#134773=CARTESIAN_POINT('Ctrl Pts',(86.6309867960358,-0.664011471940562,
78.6713237550463));
#134774=CARTESIAN_POINT('Ctrl Pts',(86.590515699779,-0.658782877845103,
78.6384200104976));
#134775=CARTESIAN_POINT('Ctrl Pts',(86.5516572818512,-0.653551332452891,
78.603901378124));
#134776=CARTESIAN_POINT('Ctrl Pts',(86.5125912920345,-0.648291841461844,
78.5691983559037));
#134777=CARTESIAN_POINT('Ctrl Pts',(86.4751557303154,-0.643029443972041,
78.5328637427483));
#134778=CARTESIAN_POINT('Ctrl Pts',(86.4395293635135,-0.637794042230455,
78.4951374517933));
#134779=CARTESIAN_POINT('Ctrl Pts',(86.4037592935678,-0.632537522879708,
78.4572589874031));
#134780=CARTESIAN_POINT('Ctrl Pts',(86.3698133364644,-0.627308288868703,
78.4179782984031));
#134781=CARTESIAN_POINT('Ctrl Pts',(86.337825082915,-0.62213493953996,78.3775613343045));
#134782=CARTESIAN_POINT('Ctrl Pts',(86.3055413922718,-0.616913810194435,
78.3367710872319));
#134783=CARTESIAN_POINT('Ctrl Pts',(86.2752518803994,-0.611749666848358,
78.2948242271959));
#134784=CARTESIAN_POINT('Ctrl Pts',(86.2470423321364,-0.606669180465398,
78.252006638812));
#134785=CARTESIAN_POINT('Ctrl Pts',(86.2360595918244,-0.604691209670451,
78.2353365932791));
#134786=CARTESIAN_POINT('Ctrl Pts',(86.2253915644109,-0.602725885089282,
78.2185346388739));
#134787=CARTESIAN_POINT('Ctrl Pts',(86.2150411923762,-0.600774640746418,
78.2016177766988));
#134788=CARTESIAN_POINT('Ctrl Pts',(86.1880884478564,-0.59569352964312,
78.1575656534754));
#134789=CARTESIAN_POINT('Ctrl Pts',(86.1632933633963,-0.590708158946545,
78.1127349228115));
#134790=CARTESIAN_POINT('Ctrl Pts',(86.1406714482072,-0.585841286813566,
78.0674221018018));
#134791=CARTESIAN_POINT('Ctrl Pts',(86.1176168671584,-0.580881331075714,
78.0212426295609));
#134792=CARTESIAN_POINT('Ctrl Pts',(86.096819142508,-0.576044486020728,
77.9745631808592));
#134793=CARTESIAN_POINT('Ctrl Pts',(86.0782425606724,-0.571350078325953,
77.9276828680263));
#134794=CARTESIAN_POINT('Ctrl Pts',(86.0594470512591,-0.566600346389369,
77.8802500642441));
#134795=CARTESIAN_POINT('Ctrl Pts',(86.0429248803045,-0.561996439892889,
77.8326122452984));
#134796=CARTESIAN_POINT('Ctrl Pts',(86.0285916654781,-0.557553194866169,
77.785053992061));
#134797=CARTESIAN_POINT('Ctrl Pts',(86.0139578015265,-0.55301674969237,
77.7364981714669));
#134798=CARTESIAN_POINT('Ctrl Pts',(86.0016051422168,-0.548647776129665,
77.6880258181732));
#134799=CARTESIAN_POINT('Ctrl Pts',(85.9914024393367,-0.544456599778991,
77.6399048044329));
#134800=CARTESIAN_POINT('Ctrl Pts',(85.9865247883617,-0.542452905693841,
77.6168993800519));
#134801=CARTESIAN_POINT('Ctrl Pts',(85.9821379714158,-0.540489768759733,
77.5939736968655));
#134802=CARTESIAN_POINT('Ctrl Pts',(85.9782249940484,-0.538567898256704,
77.5711538245528));
#134803=CARTESIAN_POINT('Ctrl Pts',(88.0595203094199,0.790170290888587,
79.0256099738597));
#134804=CARTESIAN_POINT('Ctrl Pts',(88.0092098807286,0.78727734973052,79.0347261560292));
#134805=CARTESIAN_POINT('Ctrl Pts',(87.9580761965518,0.784180082109564,
79.0417740492722));
#134806=CARTESIAN_POINT('Ctrl Pts',(87.9063804748335,0.780885940482608,
79.0466121389104));
#134807=CARTESIAN_POINT('Ctrl Pts',(87.8551739204214,0.777622969450282,
79.0514044484494));
#134808=CARTESIAN_POINT('Ctrl Pts',(87.8034165227893,0.77416684437289,79.0540281564928));
#134809=CARTESIAN_POINT('Ctrl Pts',(87.7513891315324,0.770529824401712,
79.0543887488271));
#134810=CARTESIAN_POINT('Ctrl Pts',(87.6995895365358,0.766908728725948,
79.054747762347));
#134811=CARTESIAN_POINT('Ctrl Pts',(87.6475229935954,0.763108345196423,
79.0528631405066));
#134812=CARTESIAN_POINT('Ctrl Pts',(87.5954838982341,0.759145489286064,
79.0486898505836));
#134813=CARTESIAN_POINT('Ctrl Pts',(87.5435877275265,0.7551935173045,79.0445280225435));
#134814=CARTESIAN_POINT('Ctrl Pts',(87.4917195966933,0.751080007056776,
79.0380899585497));
#134815=CARTESIAN_POINT('Ctrl Pts',(87.4401779206803,0.746825818483686,
79.0293822268949));
#134816=CARTESIAN_POINT('Ctrl Pts',(87.3920138591992,0.742850414192706,
79.0212451278476));
#134817=CARTESIAN_POINT('Ctrl Pts',(87.344135423887,0.738752241542805,79.0111266002128));
#134818=CARTESIAN_POINT('Ctrl Pts',(87.2967824789059,0.734551054033569,
78.9990729707082));
#134819=CARTESIAN_POINT('Ctrl Pts',(87.2462388709382,0.730066788597694,
78.986207162161));
#134820=CARTESIAN_POINT('Ctrl Pts',(87.1962945801456,0.725465121249223,
78.9711363065946));
#134821=CARTESIAN_POINT('Ctrl Pts',(87.147228031733,0.720773238356931,78.9539651191248));
#134822=CARTESIAN_POINT('Ctrl Pts',(87.0978467927006,0.716051263852679,
78.9366838034352));
#134823=CARTESIAN_POINT('Ctrl Pts',(87.049355265712,0.711237986875821,78.9172754944996));
#134824=CARTESIAN_POINT('Ctrl Pts',(87.0020113270475,0.70636262969103,78.8958931161929));
#134825=CARTESIAN_POINT('Ctrl Pts',(86.9544627578656,0.701466200181208,
78.8744183187242));
#134826=CARTESIAN_POINT('Ctrl Pts',(86.9080722619709,0.696507230134741,
78.8509528929625));
#134827=CARTESIAN_POINT('Ctrl Pts',(86.863065762847,0.691515690155872,78.8256912702073));
#134828=CARTESIAN_POINT('Ctrl Pts',(86.8175405624627,0.686466622528131,
78.8001385064876));
#134829=CARTESIAN_POINT('Ctrl Pts',(86.7734318832503,0.681384306791206,
78.7727485405377));
#134830=CARTESIAN_POINT('Ctrl Pts',(86.7309299367083,0.676298961111208,
78.7437540428812));
#134831=CARTESIAN_POINT('Ctrl Pts',(86.6920888218353,0.671651632887533,
78.7172569361417));
#134832=CARTESIAN_POINT('Ctrl Pts',(86.6545891480054,0.667001800965946,
78.6894205862759));
#134833=CARTESIAN_POINT('Ctrl Pts',(86.6185412289497,0.662371180898521,
78.6604379072944));
#134834=CARTESIAN_POINT('Ctrl Pts',(86.5784683109295,0.657223520140154,
78.628219112167));
#134835=CARTESIAN_POINT('Ctrl Pts',(86.54019037328,0.652099710092061,78.5945842386416));
#134836=CARTESIAN_POINT('Ctrl Pts',(86.5038107624633,0.647027058822199,
78.5598100226415));
#134837=CARTESIAN_POINT('Ctrl Pts',(86.4666557946016,0.641846294358978,
78.5242946653055));
#134838=CARTESIAN_POINT('Ctrl Pts',(86.4314809103927,0.636718946712025,
78.4875916542119));
#134839=CARTESIAN_POINT('Ctrl Pts',(86.3983415904109,0.631670280497705,
78.4499961141552));
#134840=CARTESIAN_POINT('Ctrl Pts',(86.3647782353993,0.626557013943672,
78.411919519389));
#134841=CARTESIAN_POINT('Ctrl Pts',(86.3333025802584,0.621524486678621,
78.372928126645));
#134842=CARTESIAN_POINT('Ctrl Pts',(86.3039193424151,0.616594410867282,
78.3333173997979));
#134843=CARTESIAN_POINT('Ctrl Pts',(86.2738463955409,0.611548612009062,
78.2927768953621));
#134844=CARTESIAN_POINT('Ctrl Pts',(86.2459648711422,0.606610152131991,
78.2515883055234));
#134845=CARTESIAN_POINT('Ctrl Pts',(86.2202297511519,0.601797167259691,
78.2100460870321));
#134846=CARTESIAN_POINT('Ctrl Pts',(86.2038362292661,0.598731249056467,
78.1835832895677));
#134847=CARTESIAN_POINT('Ctrl Pts',(86.1883126817497,0.595716140142255,
78.1569764994874));
#134848=CARTESIAN_POINT('Ctrl Pts',(86.1736384964732,0.592755446686942,
78.130295614134));
#134849=CARTESIAN_POINT('Ctrl Pts',(86.1499235582225,0.587970672530877,
78.0871766581775));
#134850=CARTESIAN_POINT('Ctrl Pts',(86.1284286765579,0.58332836379019,78.0438664796944));
#134851=CARTESIAN_POINT('Ctrl Pts',(86.1090365218737,0.578839063866426,
78.0006310467195));
#134852=CARTESIAN_POINT('Ctrl Pts',(86.0889994335244,0.574200461263284,
77.9559577133822));
#134853=CARTESIAN_POINT('Ctrl Pts',(86.0712066149924,0.569725195969271,
77.9113645546615));
#134854=CARTESIAN_POINT('Ctrl Pts',(86.055496550876,0.565419402890934,77.8670996202735));
#134855=CARTESIAN_POINT('Ctrl Pts',(86.0394673054545,0.561026129033146,
77.821935355404));
#134856=CARTESIAN_POINT('Ctrl Pts',(86.0256055582469,0.556809238688697,
77.7771128860643));
#134857=CARTESIAN_POINT('Ctrl Pts',(86.0137178036998,0.552770126362036,
77.7328456993623));
#134858=CARTESIAN_POINT('Ctrl Pts',(86.0014595910415,0.548605143172438,
77.6871990142608));
#134859=CARTESIAN_POINT('Ctrl Pts',(85.9912995970003,0.54462914126965,77.6421427707851));
#134860=CARTESIAN_POINT('Ctrl Pts',(85.9830139446466,0.540838980814236,
77.5978574237659));
#134861=CARTESIAN_POINT('Ctrl Pts',(85.9813426232461,0.540074457272821,
77.5889245063513));
#134862=CARTESIAN_POINT('Ctrl Pts',(85.9797475481615,0.539317481949964,
77.5800227864653));
#134863=CARTESIAN_POINT('Ctrl Pts',(85.9782268654482,0.53856800990077,77.5711534942689));
#134864=CARTESIAN_POINT('Ctrl Pts',(80.848502459919,11.73661091945,74.241762346478));
#134865=CARTESIAN_POINT('Ctrl Pts',(81.1081094445191,11.633752433,74.322364138331));
#134866=CARTESIAN_POINT('Ctrl Pts',(82.0306236000289,11.23751074128,74.627356027073));
#134867=CARTESIAN_POINT('Ctrl Pts',(83.6166033891791,10.35667619639,75.2431312468769));
#134868=CARTESIAN_POINT('Ctrl Pts',(85.5127588197891,8.86506960620401,76.080446752923));
#134869=CARTESIAN_POINT('Ctrl Pts',(87.190145346969,6.95063939189201,76.8836477281941));
#134870=CARTESIAN_POINT('Ctrl Pts',(88.4365047595691,4.76169476788001,77.517745773655));
#134871=CARTESIAN_POINT('Ctrl Pts',(89.1412933993689,2.60934775846201,77.904463418106));
#134872=CARTESIAN_POINT('Ctrl Pts',(89.333960700069,1.21084850319901,78.032284899087));
#134873=CARTESIAN_POINT('Ctrl Pts',(89.368876214269,0.592587120183914,78.065563981149));
#134874=CARTESIAN_POINT('Ctrl Pts',(79.7312718086691,10.84772626501,76.16889230891));
#134875=CARTESIAN_POINT('Ctrl Pts',(79.9583593560691,10.78136985098,76.2474763667561));
#134876=CARTESIAN_POINT('Ctrl Pts',(80.780761401509,10.51543876535,76.547621989527));
#134877=CARTESIAN_POINT('Ctrl Pts',(82.2712335217692,9.85918473546302,77.171744493571));
#134878=CARTESIAN_POINT('Ctrl Pts',(84.1515576035891,8.62511070427802,78.045485899963));
#134879=CARTESIAN_POINT('Ctrl Pts',(85.8953437067791,6.91340464913602,78.905155887249));
#134880=CARTESIAN_POINT('Ctrl Pts',(87.2468356366392,4.83565870565902,79.600172027965));
#134881=CARTESIAN_POINT('Ctrl Pts',(88.0377922459692,2.70714470495302,80.031932373865));
#134882=CARTESIAN_POINT('Ctrl Pts',(88.2608915130691,1.29568079722601,80.175396060954));
#134883=CARTESIAN_POINT('Ctrl Pts',(88.3030331051691,0.670012739913314,
80.2125795690181));
#134884=CARTESIAN_POINT('Ctrl Pts',(79.0494024224791,8.66262403025101,75.453156756963));
#134885=CARTESIAN_POINT('Ctrl Pts',(79.2376340536491,8.60492377676502,75.5423376805901));
#134886=CARTESIAN_POINT('Ctrl Pts',(79.9168939222491,8.37610563642901,75.8785940986931));
#134887=CARTESIAN_POINT('Ctrl Pts',(81.1360155378491,7.82614458542902,76.554666819415));
#134888=CARTESIAN_POINT('Ctrl Pts',(82.6587891246792,6.81693899330302,77.47520250753));
#134889=CARTESIAN_POINT('Ctrl Pts',(84.0584024217591,5.44055771549901,78.36261756888));
#134890=CARTESIAN_POINT('Ctrl Pts',(85.1345531405991,3.79029526869902,79.067792236814));
#134891=CARTESIAN_POINT('Ctrl Pts',(85.7607667741192,2.11336906824801,79.499496090843));
#134892=CARTESIAN_POINT('Ctrl Pts',(85.9370342427891,1.00572501746301,79.641066725641));
#134893=CARTESIAN_POINT('Ctrl Pts',(85.9704058165791,0.514984673010614,
79.677294432062));
#134894=CARTESIAN_POINT('Ctrl Pts',(79.8524902757991,8.54481423012501,73.1962815772969));
#134895=CARTESIAN_POINT('Ctrl Pts',(80.055340106059,8.45459986811801,73.2923622975862));
#134896=CARTESIAN_POINT('Ctrl Pts',(80.7687653141991,8.11256935884601,73.6501015201404));
#134897=CARTESIAN_POINT('Ctrl Pts',(81.9583812039191,7.38699783676102,74.341760845944));
#134898=CARTESIAN_POINT('Ctrl Pts',(83.332259704859,6.22385841296701,75.247429141669));
#134899=CARTESIAN_POINT('Ctrl Pts',(84.5069102018391,4.79923984093301,76.091157573338));
#134900=CARTESIAN_POINT('Ctrl Pts',(85.3510764575991,3.23472385359101,76.740094262514));
#134901=CARTESIAN_POINT('Ctrl Pts',(85.815223686549,1.74201483404001,77.126729388828));
#134902=CARTESIAN_POINT('Ctrl Pts',(85.939483396599,0.787307726399214,77.2517856728581));
#134903=CARTESIAN_POINT('Ctrl Pts',(85.9615884733991,0.366136356086714,
77.283668607651));
#134904=CARTESIAN_POINT('',(80.3938476406748,10.4339876816843,75.1766107359184));
#134905=CARTESIAN_POINT('Ctrl Pts',(80.3938505465934,10.4339853760665,75.1766007796959));
#134906=CARTESIAN_POINT('Ctrl Pts',(80.3794956831756,10.4043236969974,75.1792779571772));
#134907=CARTESIAN_POINT('Ctrl Pts',(80.3681799513873,10.3731852311496,75.1822081054656));
#134908=CARTESIAN_POINT('Ctrl Pts',(80.3598138015333,10.3408757778269,75.185327398614));
#134909=CARTESIAN_POINT('Ctrl Pts',(80.3514342490384,10.3085145644937,75.1884516888957));
#134910=CARTESIAN_POINT('Ctrl Pts',(80.3460138121778,10.2749790675551,75.1917657423984));
#134911=CARTESIAN_POINT('Ctrl Pts',(80.3434557634103,10.2405725763164,75.1952574190916));
#134912=CARTESIAN_POINT('Ctrl Pts',(80.3419194802506,10.2199091262095,75.1973544096461));
#134913=CARTESIAN_POINT('Ctrl Pts',(80.3414154746935,10.1989314150935,75.1995164760688));
#134914=CARTESIAN_POINT('Ctrl Pts',(80.3419214521968,10.1777033896151,75.2017497411212));
#134915=CARTESIAN_POINT('Ctrl Pts',(80.3430222180311,10.1315213261305,75.2066082612192));
#134916=CARTESIAN_POINT('Ctrl Pts',(80.3488943629579,10.0841513673407,75.2118020083656));
#134917=CARTESIAN_POINT('Ctrl Pts',(80.3587399708604,10.0360620573974,75.2172498509544));
#134918=CARTESIAN_POINT('Ctrl Pts',(80.3684790861479,9.98849289373798,75.2226387682835));
#134919=CARTESIAN_POINT('Ctrl Pts',(80.3821062313102,9.94021889979879,75.2282775112244));
#134920=CARTESIAN_POINT('Ctrl Pts',(80.3988649310452,9.89164931798805,75.2341048459053));
#134921=CARTESIAN_POINT('Ctrl Pts',(80.4159555526203,9.84211776984164,75.2400475964407));
#134922=CARTESIAN_POINT('Ctrl Pts',(80.4361874576856,9.79236538991005,75.2461429831938));
#134923=CARTESIAN_POINT('Ctrl Pts',(80.4590421234356,9.74250323912191,75.2524219427782));
#134924=CARTESIAN_POINT('Ctrl Pts',(80.4828593033625,9.69054116582547,75.2589653379786));
#134925=CARTESIAN_POINT('Ctrl Pts',(80.5095245260965,9.63845899488816,75.265708498635));
#134926=CARTESIAN_POINT('Ctrl Pts',(80.5384695241847,9.58635298852964,75.2726459446336));
#134927=CARTESIAN_POINT('Ctrl Pts',(80.5677742386363,9.53359943045728,75.2796696063174));
#134928=CARTESIAN_POINT('Ctrl Pts',(80.5994156032385,9.48082042202425,75.286892562903));
#134929=CARTESIAN_POINT('Ctrl Pts',(80.6328241879231,9.42810235486638,75.2942615131889));
#134930=CARTESIAN_POINT('Ctrl Pts',(80.6596310629284,9.38580165131496,75.3001743206634));
#134931=CARTESIAN_POINT('Ctrl Pts',(80.6875761077926,9.34353977947596,75.3061801571795));
#134932=CARTESIAN_POINT('Ctrl Pts',(80.7163753358332,9.30136134543792,75.3122294516991));
#134933=CARTESIAN_POINT('Ctrl Pts',(80.7580602573791,9.24031093424897,75.3209853935981));
#134934=CARTESIAN_POINT('Ctrl Pts',(80.8016277183823,9.17937597468941,75.3298715087046));
#134935=CARTESIAN_POINT('Ctrl Pts',(80.8467191242501,9.11852787641061,75.3389213826274));
#134936=CARTESIAN_POINT('Ctrl Pts',(80.89237086256,9.05692364372325,75.3480837156287));
#134937=CARTESIAN_POINT('Ctrl Pts',(80.9395844286924,8.99540768739869,75.3574136933392));
#134938=CARTESIAN_POINT('Ctrl Pts',(80.9880017803453,8.93395060728147,75.3668943788865));
#134939=CARTESIAN_POINT('Ctrl Pts',(81.037189216702,8.87151604376801,75.3765258560544));
#134940=CARTESIAN_POINT('Ctrl Pts',(81.087618799575,8.8091415919427,75.3863125557427));
#134941=CARTESIAN_POINT('Ctrl Pts',(81.138933129947,8.74680748229801,75.396187602513));
#134942=CARTESIAN_POINT('Ctrl Pts',(81.1477877166934,8.73605136841898,75.3978915993813));
#134943=CARTESIAN_POINT('Ctrl Pts',(81.1566686948946,8.72529649517431,75.3995981175479));
#134944=CARTESIAN_POINT('Ctrl Pts',(81.1655742892056,8.71454281415756,75.4013066804546));
#134945=CARTESIAN_POINT('Ctrl Pts',(81.2271636357191,8.64017246184747,75.4131227669758));
#134946=CARTESIAN_POINT('Ctrl Pts',(81.2899742554949,8.56584216025802,75.4250668983327));
#134947=CARTESIAN_POINT('Ctrl Pts',(81.3537329467453,8.4914766887375,75.4371557885758));
#134948=CARTESIAN_POINT('Ctrl Pts',(81.4191635386663,8.41516118218237,75.4495616775417));
#134949=CARTESIAN_POINT('Ctrl Pts',(81.4855922124784,8.33880799469124,75.462119659779));
#134950=CARTESIAN_POINT('Ctrl Pts',(81.552738473848,8.26234763978692,75.4747959347963));
#134951=CARTESIAN_POINT('Ctrl Pts',(81.5917296022156,8.21794791518118,75.4821569144897));
#134952=CARTESIAN_POINT('Ctrl Pts',(81.6309630061373,8.17351233078151,75.4895568478986));
#134953=CARTESIAN_POINT('Ctrl Pts',(81.6703866518846,8.12903021326751,75.4969822402694));
#134954=CARTESIAN_POINT('Ctrl Pts',(81.6950453081994,8.1012075898865,75.5016266660956));
#134955=CARTESIAN_POINT('Ctrl Pts',(81.7197802155452,8.07336477096924,75.506281210966));
#134956=CARTESIAN_POINT('Ctrl Pts',(81.7445850781898,8.04549809771702,75.5109468154525));
#134957=CARTESIAN_POINT('Ctrl Pts',(81.8289357622139,7.95073551088164,75.5268125324072));
#134958=CARTESIAN_POINT('Ctrl Pts',(81.9140949701358,7.85569637818219,75.5428103106627));
#134959=CARTESIAN_POINT('Ctrl Pts',(81.9998081566341,7.76023375751805,75.5589691434916));
#134960=CARTESIAN_POINT('Ctrl Pts',(82.0877991469408,7.66223424457641,75.5755573927553));
#134961=CARTESIAN_POINT('Ctrl Pts',(82.1763735768846,7.56378785292534,75.5923148302763));
#134962=CARTESIAN_POINT('Ctrl Pts',(82.2652659129091,7.46475040757157,75.6092188800251));
#134963=CARTESIAN_POINT('Ctrl Pts',(82.3579357872776,7.36150430077359,75.6268412784972));
#134964=CARTESIAN_POINT('Ctrl Pts',(82.4509507670458,7.25761530954014,75.6446224383545));
#134965=CARTESIAN_POINT('Ctrl Pts',(82.5440266443157,7.15294479678162,75.6624874827657));
#134966=CARTESIAN_POINT('Ctrl Pts',(82.6089620675702,7.07992024683802,75.6749512301333));
#134967=CARTESIAN_POINT('Ctrl Pts',(82.673927494531,7.0065158574105,75.6874547530637));
#134968=CARTESIAN_POINT('Ctrl Pts',(82.7388322903256,6.93269290689744,75.6999617663264));
#134969=CARTESIAN_POINT('Ctrl Pts',(82.8448503955217,6.81210752892094,75.7203912250671));
#134970=CARTESIAN_POINT('Ctrl Pts',(82.9507217184122,6.69040801412927,75.7408568289677));
#134971=CARTESIAN_POINT('Ctrl Pts',(83.0562164481922,6.56736387199933,75.7613649477384));
#134972=CARTESIAN_POINT('Ctrl Pts',(83.0971173405337,6.51965897507221,75.7693160592273));
#134973=CARTESIAN_POINT('Ctrl Pts',(83.1379615312657,6.47175183804246,75.7772730197448));
#134974=CARTESIAN_POINT('Ctrl Pts',(83.1787353184465,6.42362861819271,75.7852341770899));
#134975=CARTESIAN_POINT('Ctrl Pts',(83.2876169880677,6.29512114103467,75.8064935244249));
#134976=CARTESIAN_POINT('Ctrl Pts',(83.3959975402901,6.1650728848407,75.8277865031236));
#134977=CARTESIAN_POINT('Ctrl Pts',(83.5035391676682,6.03323799801862,75.8490553375103));
#134978=CARTESIAN_POINT('Ctrl Pts',(83.6042434339213,5.90978500713803,75.8689719262136));
#134979=CARTESIAN_POINT('Ctrl Pts',(83.7042119487058,5.78476517016213,75.888866746447));
#134980=CARTESIAN_POINT('Ctrl Pts',(83.8031578769549,5.65797623157721,75.9086520659686));
#134981=CARTESIAN_POINT('Ctrl Pts',(80.8776258353147,11.5357847450604,74.5260057583377));
#134982=CARTESIAN_POINT('Ctrl Pts',(80.8241739589715,11.4290971482,74.6680655050188));
#134983=CARTESIAN_POINT('Ctrl Pts',(80.7695837405888,11.3036362609338,74.7920292317203));
#134984=CARTESIAN_POINT('Ctrl Pts',(80.7104997231134,11.1628322965241,74.8935242557125));
#134985=CARTESIAN_POINT('Ctrl Pts',(80.6942685092337,11.124151459318,74.9214063719351));
#134986=CARTESIAN_POINT('Ctrl Pts',(80.6776981555813,11.0843127079775,74.9475928168453));
#134987=CARTESIAN_POINT('Ctrl Pts',(80.6607375632814,11.0435148107972,74.9719321664642));
#134988=CARTESIAN_POINT('Ctrl Pts',(80.6194446553415,10.9441866869546,75.0311896797254));
#134989=CARTESIAN_POINT('Ctrl Pts',(80.5758387607439,10.8391735670981,75.0794984832658));
#134990=CARTESIAN_POINT('Ctrl Pts',(80.5291823535934,10.731343510345,75.1146733552099));
#134991=CARTESIAN_POINT('Ctrl Pts',(80.4869168772856,10.6336615629484,75.146537847304));
#134992=CARTESIAN_POINT('Ctrl Pts',(80.4421480523026,10.5336679203548,75.1676242054091));
#134993=CARTESIAN_POINT('Ctrl Pts',(80.3938476406443,10.4339876816213,75.1766107359241));
#134994=CARTESIAN_POINT('Ctrl Pts',(89.3691702808691,-0.592509543609686,
78.06499762776));
#134995=CARTESIAN_POINT('Ctrl Pts',(89.333364493069,-1.22675245987899,78.0308677484269));
#134996=CARTESIAN_POINT('Ctrl Pts',(89.1350209057691,-2.64413304960699,
77.899881169114));
#134997=CARTESIAN_POINT('Ctrl Pts',(88.4141708296692,-4.81338885261599,
77.50526087718));
#134998=CARTESIAN_POINT('Ctrl Pts',(87.1543010728991,-7.00151860831499,
76.865195019139));
#134999=CARTESIAN_POINT('Ctrl Pts',(85.4673513115891,-8.90801815554399,
76.05874833561));
#135000=CARTESIAN_POINT('Ctrl Pts',(83.5693396104491,-10.38775332569,75.222772426747));
#135001=CARTESIAN_POINT('Ctrl Pts',(81.9994121956191,-11.2524563877,74.615701488007));
#135002=CARTESIAN_POINT('Ctrl Pts',(81.0940117744891,-11.63968033551,74.317387098816));
#135003=CARTESIAN_POINT('Ctrl Pts',(80.848841500759,-11.73682984029,74.24126399703));
#135004=CARTESIAN_POINT('Ctrl Pts',(88.3037963433691,-0.670020240532286,
80.212989738538));
#135005=CARTESIAN_POINT('Ctrl Pts',(88.2605722655691,-1.31191574234599,
80.17485818836));
#135006=CARTESIAN_POINT('Ctrl Pts',(88.0309623922691,-2.74242877837699,
80.027804792461));
#135007=CARTESIAN_POINT('Ctrl Pts',(87.2224252329291,-4.88633006170198,
79.587339822944));
#135008=CARTESIAN_POINT('Ctrl Pts',(85.8573754622091,-6.96092439909799,
78.8861235752561));
#135009=CARTESIAN_POINT('Ctrl Pts',(84.1054574799991,-8.66266365324199,
78.023501439213));
#135010=CARTESIAN_POINT('Ctrl Pts',(82.2255471495491,-9.884161731605,77.151746893156));
#135011=CARTESIAN_POINT('Ctrl Pts',(80.7522513198091,-10.52642329792,76.536966540696));
#135012=CARTESIAN_POINT('Ctrl Pts',(79.9459230821792,-10.78575655111,76.243563881432));
#135013=CARTESIAN_POINT('Ctrl Pts',(79.7314542668592,-10.84842834365,76.16935458938));
#135014=CARTESIAN_POINT('Ctrl Pts',(85.9704220108091,-0.514982056589186,
79.677973373886));
#135015=CARTESIAN_POINT('Ctrl Pts',(85.9361932564492,-1.01843012321199,
79.640819503283));
#135016=CARTESIAN_POINT('Ctrl Pts',(85.7547895194892,-2.14099621798999,
79.495685929435));
#135017=CARTESIAN_POINT('Ctrl Pts',(85.1146074343491,-3.83019701732299,
79.055137172574));
#135018=CARTESIAN_POINT('Ctrl Pts',(84.0275042605191,-5.47826347261898,
78.343392903102));
#135019=CARTESIAN_POINT('Ctrl Pts',(82.6211065505191,-6.84703129507799,
77.452501919721));
#135020=CARTESIAN_POINT('Ctrl Pts',(81.0983702081792,-7.84636772488399,
76.53350254654));
#135021=CARTESIAN_POINT('Ctrl Pts',(79.8930386155091,-8.38493617109999,
75.866968193567));
#135022=CARTESIAN_POINT('Ctrl Pts',(79.2269700371691,-8.60816371974399,
75.5380273818501));
#135023=CARTESIAN_POINT('Ctrl Pts',(79.0492114403891,-8.66265061663799,
75.4538070962019));
#135024=CARTESIAN_POINT('Ctrl Pts',(85.961594855169,-0.366097390925386,
77.2836790921491));
#135025=CARTESIAN_POINT('Ctrl Pts',(85.9389255120391,-0.798156683534387,
77.250976980684));
#135026=CARTESIAN_POINT('Ctrl Pts',(85.8109804217291,-1.76582270548099,
77.1227940400109));
#135027=CARTESIAN_POINT('Ctrl Pts',(85.3359900028191,-3.27105037820099,
76.7280513880721));
#135028=CARTESIAN_POINT('Ctrl Pts',(84.4820233966991,-4.83629425178999,
76.072610788049));
#135029=CARTESIAN_POINT('Ctrl Pts',(83.2996589358591,-6.25653437109799,
75.224881302974));
#135030=CARTESIAN_POINT('Ctrl Pts',(81.9232512000892,-7.41183271016798,
74.319910758465));
#135031=CARTESIAN_POINT('Ctrl Pts',(80.7446490589091,-8.12510609244499,
73.6372601504587));
#135032=CARTESIAN_POINT('Ctrl Pts',(80.0440787679191,-8.45960257608299,
73.2870471296229));
#135033=CARTESIAN_POINT('Ctrl Pts',(79.852518768739,-8.54479915548399,73.1963043351081));
#135034=CARTESIAN_POINT('',(80.8778404067288,-11.5358771726413,74.525851299618));
#135035=CARTESIAN_POINT('Ctrl Pts',(80.8778403488691,-11.53587675694,74.525850965447));
#135036=CARTESIAN_POINT('Ctrl Pts',(81.3969169389546,-11.2739281687296,
74.7620470766188));
#135037=CARTESIAN_POINT('Ctrl Pts',(81.9044940104665,-10.9762832390086,
75.0181676961644));
#135038=CARTESIAN_POINT('Ctrl Pts',(82.6466403385913,-10.4673809179007,
75.4210629555873));
#135039=CARTESIAN_POINT('Ctrl Pts',(82.8908135114496,-10.2873411024514,
75.5584479718167));
#135040=CARTESIAN_POINT('Ctrl Pts',(83.2519588597215,-10.0006051938715,
75.7674482995734));
#135041=CARTESIAN_POINT('Ctrl Pts',(83.4312523337386,-9.85306899184976,
75.8726757764798));
#135042=CARTESIAN_POINT('Ctrl Pts',(83.6381171526523,-9.67342660579858,
75.9963039271245));
#135043=CARTESIAN_POINT('Ctrl Pts',(83.7262701415434,-9.59480336358862,
76.0494259686177));
#135044=CARTESIAN_POINT('Ctrl Pts',(83.7849260230865,-9.54202232590022,
76.0848662368444));
#135045=CARTESIAN_POINT('Ctrl Pts',(83.8150378412129,-9.51467944670708,
76.1031094855966));
#135046=CARTESIAN_POINT('Ctrl Pts',(84.2974032165774,-9.07288821655665,
76.3960663128352));
#135047=CARTESIAN_POINT('Ctrl Pts',(84.7160086697936,-8.63505965462778,
76.6588486116176));
#135048=CARTESIAN_POINT('Ctrl Pts',(85.2900464084644,-7.94763758112796,
77.0291165601318));
#135049=CARTESIAN_POINT('Ctrl Pts',(85.4724140397087,-7.7133904318713,77.1485556698116));
#135050=CARTESIAN_POINT('Ctrl Pts',(85.732400814426,-7.35471642757629,77.3211874942504));
#135051=CARTESIAN_POINT('Ctrl Pts',(85.8590030575354,-7.17355425421414,
77.4058718313578));
#135052=CARTESIAN_POINT('Ctrl Pts',(86.0007501877189,-6.95908918789543,
77.5016959600908));
#135053=CARTESIAN_POINT('Ctrl Pts',(86.0701322830086,-6.85109047841624,
77.5488497237172));
#135054=CARTESIAN_POINT('Ctrl Pts',(86.0995475883965,-6.80464234068808,
77.5688944119908));
#135055=CARTESIAN_POINT('Ctrl Pts',(86.1190866771446,-6.77364083372217,
77.58222090351));
#135056=CARTESIAN_POINT('Ctrl Pts',(86.129581954462,-6.7569024593158,77.5893859904182));
#135057=CARTESIAN_POINT('Ctrl Pts',(86.7104950006951,-5.82628527351812,
77.986299807247));
#135058=CARTESIAN_POINT('Ctrl Pts',(87.1575629529062,-4.85933241118305,
78.3065330622175));
#135059=CARTESIAN_POINT('Ctrl Pts',(87.7986061785262,-2.86235283752183,
78.7878566954693));
#135060=CARTESIAN_POINT('Ctrl Pts',(87.9926711462578,-1.8324008091606,78.9489796710299));
#135061=CARTESIAN_POINT('Ctrl Pts',(88.059439280893,-0.791398763418655,
79.0255044521198));
#135062=CARTESIAN_POINT('',(80.3938333635145,-10.4339884044026,75.1766012116704));
#135063=CARTESIAN_POINT('Ctrl Pts',(80.3938307448211,-10.4339904821502,
75.1766101838327));
#135064=CARTESIAN_POINT('Ctrl Pts',(80.4421453858671,-10.5336704769535,
75.1676281080308));
#135065=CARTESIAN_POINT('Ctrl Pts',(80.4869279350663,-10.633663298453,75.1465444690012));
#135066=CARTESIAN_POINT('Ctrl Pts',(80.5292078186286,-10.7313459535512,
75.1146810599036));
#135067=CARTESIAN_POINT('Ctrl Pts',(80.5758916995727,-10.8392035221319,
75.0794986641292));
#135068=CARTESIAN_POINT('Ctrl Pts',(80.6195243861941,-10.9442446065244,
75.0311738317282));
#135069=CARTESIAN_POINT('Ctrl Pts',(80.6608418244781,-11.0435938413397,
74.9718949947255));
#135070=CARTESIAN_POINT('Ctrl Pts',(80.6777947163431,-11.0843576666066,
74.9475723901468));
#135071=CARTESIAN_POINT('Ctrl Pts',(80.6943577989013,-11.1241631896455,
74.9214056769664));
#135072=CARTESIAN_POINT('Ctrl Pts',(80.7105818981162,-11.162811763929,74.893546047618));
#135073=CARTESIAN_POINT('Ctrl Pts',(80.769710077265,-11.3036651816639,74.7920125736594));
#135074=CARTESIAN_POINT('Ctrl Pts',(80.8243358251592,-11.4291518569876,
74.6679935591501));
#135075=CARTESIAN_POINT('Ctrl Pts',(80.8778405813924,-11.5358784198398,
74.525852301822));
#135076=CARTESIAN_POINT('Ctrl Pts',(83.8031819186192,-5.65795202609479,
75.9086537965711));
#135077=CARTESIAN_POINT('Ctrl Pts',(83.6949583155237,-5.79663127872643,
75.8870127524824));
#135078=CARTESIAN_POINT('Ctrl Pts',(83.5855117972911,-5.93319230169319,
75.8652409078052));
#135079=CARTESIAN_POINT('Ctrl Pts',(83.4752159873789,-6.06790048259671,
75.8434516164506));
#135080=CARTESIAN_POINT('Ctrl Pts',(83.3649201774668,-6.20260866350022,
75.821662325096));
#135081=CARTESIAN_POINT('Ctrl Pts',(83.2537750899658,-6.33546424712983,
75.7998557959442));
#135082=CARTESIAN_POINT('Ctrl Pts',(83.142141371957,-6.46673210215424,75.7780894655796));
#135083=CARTESIAN_POINT('Ctrl Pts',(83.0369680456649,-6.5904033118424,75.7575827816989));
#135084=CARTESIAN_POINT('Ctrl Pts',(82.9313605871511,-6.71266582993158,
75.7371116414454));
#135085=CARTESIAN_POINT('Ctrl Pts',(82.8255497425663,-6.83375266287503,
75.7166853181176));
#135086=CARTESIAN_POINT('Ctrl Pts',(82.7966651662695,-6.8668073263967,75.7111092762956));
#135087=CARTESIAN_POINT('Ctrl Pts',(82.7677653913127,-6.89977431904788,
75.7055362855964));
#135088=CARTESIAN_POINT('Ctrl Pts',(82.7388550041916,-6.93265823475957,
75.6999658762941));
#135089=CARTESIAN_POINT('Ctrl Pts',(82.6462278702881,-7.03801631423271,
75.6821186213894));
#135090=CARTESIAN_POINT('Ctrl Pts',(82.5534717057814,-7.14252558161222,
75.6642760957885));
#135091=CARTESIAN_POINT('Ctrl Pts',(82.4608543677029,-7.24630029078847,
75.6465407625238));
#135092=CARTESIAN_POINT('Ctrl Pts',(82.3706833984402,-7.3473339234269,75.6292738854589));
#135093=CARTESIAN_POINT('Ctrl Pts',(82.280644304359,-7.4476715982538,75.6121092748401));
#135094=CARTESIAN_POINT('Ctrl Pts',(82.1910024291584,-7.54744439154357,
75.5951053605184));
#135095=CARTESIAN_POINT('Ctrl Pts',(82.1051550617223,-7.64299383901446,
75.5788212156659));
#135096=CARTESIAN_POINT('Ctrl Pts',(82.0196723344532,-7.73802568404422,
75.5626848734953));
#135097=CARTESIAN_POINT('Ctrl Pts',(81.9347996244226,-7.8326731617615,75.5467064736755));
#135098=CARTESIAN_POINT('Ctrl Pts',(81.8590240022107,-7.91717584244927,
75.5324407198442));
#135099=CARTESIAN_POINT('Ctrl Pts',(81.7837349587665,-8.0013726371851,75.5183006467202));
#135100=CARTESIAN_POINT('Ctrl Pts',(81.7091125429145,-8.08536627130556,
75.5042595553665));
#135101=CARTESIAN_POINT('Ctrl Pts',(81.696182828616,-8.09991972256654,75.5018266764847));
#135102=CARTESIAN_POINT('Ctrl Pts',(81.6832731355542,-8.1144670855565,75.4993966830922));
#135103=CARTESIAN_POINT('Ctrl Pts',(81.6703843730783,-8.1290088775968,75.4969694336617));
#135104=CARTESIAN_POINT('Ctrl Pts',(81.6022415642135,-8.20589124372036,
75.4841365806772));
#135105=CARTESIAN_POINT('Ctrl Pts',(81.5346702893315,-8.28263226615724,
75.4713835484874));
#135106=CARTESIAN_POINT('Ctrl Pts',(81.4679410651791,-8.35929276064737,
75.458769962743));
#135107=CARTESIAN_POINT('Ctrl Pts',(81.4029018398334,-8.43401173482386,
75.4464758314075));
#135108=CARTESIAN_POINT('Ctrl Pts',(81.3386628796318,-8.50865474452786,
75.4343145697313));
#135109=CARTESIAN_POINT('Ctrl Pts',(81.2754907693696,-8.58329344530985,
75.4222975957938));
#135110=CARTESIAN_POINT('Ctrl Pts',(81.2384771239911,-8.62702556682338,
75.4152566403785));
#135111=CARTESIAN_POINT('Ctrl Pts',(81.2018300096906,-8.67075646661488,
75.4082643596455));
#135112=CARTESIAN_POINT('Ctrl Pts',(81.1656050134525,-8.71450187273681,
75.4013150054122));
#135113=CARTESIAN_POINT('Ctrl Pts',(81.1141320169016,-8.77666080640869,
75.391440495443));
#135114=CARTESIAN_POINT('Ctrl Pts',(81.063478630063,-8.8388587546476,75.381636850763));
#135115=CARTESIAN_POINT('Ctrl Pts',(81.0139956332105,-8.90111247007968,
75.3719783385541));
#135116=CARTESIAN_POINT('Ctrl Pts',(80.9650931467855,-8.96263585523153,
75.3624331353079));
#135117=CARTESIAN_POINT('Ctrl Pts',(80.9173339662622,-9.02421430425923,
75.3530300340532));
#135118=CARTESIAN_POINT('Ctrl Pts',(80.8710743650251,-9.08587610974556,
75.3437948427317));
#135119=CARTESIAN_POINT('Ctrl Pts',(80.8256376474274,-9.14644105123925,
75.3347239305575));
#135120=CARTESIAN_POINT('Ctrl Pts',(80.7816478632713,-9.20708711251621,
75.3258151868051));
#135121=CARTESIAN_POINT('Ctrl Pts',(80.739456477262,-9.26784327404333,75.3170446753161));
#135122=CARTESIAN_POINT('Ctrl Pts',(80.7317068667288,-9.27900281711263,
75.3154337292286));
#135123=CARTESIAN_POINT('Ctrl Pts',(80.724017962384,-9.29016606341629,75.3138273094398));
#135124=CARTESIAN_POINT('Ctrl Pts',(80.7163919846255,-9.30133316972677,
75.3122250801437));
#135125=CARTESIAN_POINT('Ctrl Pts',(80.6805114603629,-9.353874842625,75.3046865285043));
#135126=CARTESIAN_POINT('Ctrl Pts',(80.6459531886258,-9.40654633460277,
75.2972159848387));
#135127=CARTESIAN_POINT('Ctrl Pts',(80.6132706656793,-9.45926088566441,
75.2899059484022));
#135128=CARTESIAN_POINT('Ctrl Pts',(80.5807729794489,-9.5116773084414,75.282637254035));
#135129=CARTESIAN_POINT('Ctrl Pts',(80.5501300103034,-9.5641371706498,75.2755273211528));
#135130=CARTESIAN_POINT('Ctrl Pts',(80.5219072198447,-9.61655348817482,
75.2686204065309));
#135131=CARTESIAN_POINT('Ctrl Pts',(80.4941261501928,-9.66814942693174,
75.2618215934769));
#135132=CARTESIAN_POINT('Ctrl Pts',(80.4686902370224,-9.71970415366564,
75.255219285462));
#135133=CARTESIAN_POINT('Ctrl Pts',(80.446157482063,-9.77111939827723,75.2488114990542));
#135134=CARTESIAN_POINT('Ctrl Pts',(80.4430015386915,-9.77832063047093,
75.2479140228655));
#135135=CARTESIAN_POINT('Ctrl Pts',(80.4399025746111,-9.78551908723602,
75.247020294269));
#135136=CARTESIAN_POINT('Ctrl Pts',(80.4368621503838,-9.79271445619721,
75.246130241967));
#135137=CARTESIAN_POINT('Ctrl Pts',(80.4228985573425,-9.82576024074726,
75.2420425465659));
#135138=CARTESIAN_POINT('Ctrl Pts',(80.4101694983428,-9.85874141842604,
75.2380329443838));
#135139=CARTESIAN_POINT('Ctrl Pts',(80.3988281371886,-9.89162371531827,
75.2340908897384));
#135140=CARTESIAN_POINT('Ctrl Pts',(80.3819749010759,-9.94048673148717,
75.2282330057678));
#135141=CARTESIAN_POINT('Ctrl Pts',(80.3682876237009,-9.98907031929511,
75.2225640783406));
#135142=CARTESIAN_POINT('Ctrl Pts',(80.3585351980045,-10.0369369490896,
75.2171447714278));
#135143=CARTESIAN_POINT('Ctrl Pts',(80.3487958809904,-10.0847392391529,
75.2117327488538));
#135144=CARTESIAN_POINT('Ctrl Pts',(80.342980808203,-10.1318272875854,75.206568468694));
#135145=CARTESIAN_POINT('Ctrl Pts',(80.3418707948709,-10.1777210736054,
75.2017347817589));
#135146=CARTESIAN_POINT('Ctrl Pts',(80.3410240003497,-10.2127320103516,
75.1980473128833));
#135147=CARTESIAN_POINT('Ctrl Pts',(80.3429534869955,-10.2470637310563,
75.1945611852141));
#135148=CARTESIAN_POINT('Ctrl Pts',(80.3477336040891,-10.2804270866782,
75.191248594403));
#135149=CARTESIAN_POINT('Ctrl Pts',(80.3525057999656,-10.3137351552889,
75.1879414929452));
#135150=CARTESIAN_POINT('Ctrl Pts',(80.3601191070685,-10.3460775732638,
75.1848072246402));
#135151=CARTESIAN_POINT('Ctrl Pts',(80.370639260543,-10.3771592615142,75.1818691173166));
#135152=CARTESIAN_POINT('Ctrl Pts',(80.3772263692291,-10.3966208082636,
75.1800294452701));
#135153=CARTESIAN_POINT('Ctrl Pts',(80.3849529585172,-10.4155879636399,
75.178267714747));
#135154=CARTESIAN_POINT('Ctrl Pts',(80.393833729897,-10.4339881123427,75.1765999544888));
#135155=CARTESIAN_POINT('Ctrl Pts',(82.2802684813891,-4.44949575811698,
74.675770956836));
#135156=CARTESIAN_POINT('Ctrl Pts',(82.2515547398691,-4.47459854592499,
74.682359802912));
#135157=CARTESIAN_POINT('Ctrl Pts',(81.9823906719391,-4.70957506713498,
74.744877050762));
#135158=CARTESIAN_POINT('Ctrl Pts',(81.4784721044692,-5.14545068164199,
74.875238035718));
#135159=CARTESIAN_POINT('Ctrl Pts',(80.7929408853791,-5.76164297262998,
75.086564528771));
#135160=CARTESIAN_POINT('Ctrl Pts',(80.1708842271991,-6.36930087556499,
75.310730256588));
#135161=CARTESIAN_POINT('Ctrl Pts',(79.627849910789,-6.97242199968299,75.535523321951));
#135162=CARTESIAN_POINT('Ctrl Pts',(79.1658598934692,-7.58148319945498,
75.754792199969));
#135163=CARTESIAN_POINT('Ctrl Pts',(78.7839122270891,-8.21774497486598,
75.963729042074));
#135164=CARTESIAN_POINT('Ctrl Pts',(78.4905471606791,-8.91099832424997,
76.154488077099));
#135165=CARTESIAN_POINT('Ctrl Pts',(78.3164477158992,-9.69317749973099,
76.310267280487));
#135166=CARTESIAN_POINT('Ctrl Pts',(78.3332530958491,-10.5751191833,76.397661386524));
#135167=CARTESIAN_POINT('Ctrl Pts',(78.552159943209,-11.24208048039,76.382057866807));
#135168=CARTESIAN_POINT('Ctrl Pts',(78.7265238604091,-11.55499571287,76.348377280967));
#135169=CARTESIAN_POINT('Ctrl Pts',(78.7578974474891,-11.60737125339,76.341975098692));
#135170=CARTESIAN_POINT('Ctrl Pts',(83.1759968014491,-5.145175158979,74.314617629455));
#135171=CARTESIAN_POINT('Ctrl Pts',(83.1446436833991,-5.170233981977,74.314575250006));
#135172=CARTESIAN_POINT('Ctrl Pts',(82.8506132385191,-5.403970611904,74.315005581851));
#135173=CARTESIAN_POINT('Ctrl Pts',(82.2978958470191,-5.823239271777,74.330549238132));
#135174=CARTESIAN_POINT('Ctrl Pts',(81.5377842120691,-6.38454221490099,
74.390669473468));
#135175=CARTESIAN_POINT('Ctrl Pts',(80.8370587913791,-6.91472737682399,
74.483185378663));
#135176=CARTESIAN_POINT('Ctrl Pts',(80.2140754539491,-7.42515657005799,
74.599258127461));
#135177=CARTESIAN_POINT('Ctrl Pts',(79.6697283221492,-7.93290551323299,
74.731448452699));
#135178=CARTESIAN_POINT('Ctrl Pts',(79.2030231249391,-8.462495291134,74.8734975621001));
#135179=CARTESIAN_POINT('Ctrl Pts',(78.8228979343391,-9.04669161529399,
75.016582905033));
#135180=CARTESIAN_POINT('Ctrl Pts',(78.5624521075091,-9.721849384846,75.143445470533));
#135181=CARTESIAN_POINT('Ctrl Pts',(78.5012064800991,-10.50497709738,75.219507140925));
#135182=CARTESIAN_POINT('Ctrl Pts',(78.6770469362391,-11.10230153997,75.205989286091));
#135183=CARTESIAN_POINT('Ctrl Pts',(78.8330573272891,-11.37723786725,75.176271341392));
#135184=CARTESIAN_POINT('Ctrl Pts',(78.8613872357791,-11.42306524829,75.170636169063));
#135185=CARTESIAN_POINT('Ctrl Pts',(83.9722471046291,-5.62773758024599,
75.056136835834));
#135186=CARTESIAN_POINT('Ctrl Pts',(83.9438214655291,-5.65632355297999,
75.050655356093));
#135187=CARTESIAN_POINT('Ctrl Pts',(83.6770236031091,-5.92266876826999,
74.9996667050681));
#135188=CARTESIAN_POINT('Ctrl Pts',(83.1717502749291,-6.39475408463199,
74.9113173165371));
#135189=CARTESIAN_POINT('Ctrl Pts',(82.4700265622691,-7.00227131693099,
74.81064511086));
#135190=CARTESIAN_POINT('Ctrl Pts',(81.8180959209991,-7.54608119591799,
74.738536463235));
#135191=CARTESIAN_POINT('Ctrl Pts',(81.2363061342691,-8.034963233551,74.694203501958));
#135192=CARTESIAN_POINT('Ctrl Pts',(80.7264020875791,-8.48630143485999,
74.673073572076));
#135193=CARTESIAN_POINT('Ctrl Pts',(80.2885564578391,-8.91928079144999,
74.671182615835));
#135194=CARTESIAN_POINT('Ctrl Pts',(79.9302124268591,-9.35507338522099,
74.68366879445));
#135195=CARTESIAN_POINT('Ctrl Pts',(79.6752781953791,-9.81353295040099,
74.702418045188));
#135196=CARTESIAN_POINT('Ctrl Pts',(79.5756251446291,-10.30108863856,74.711599114768));
#135197=CARTESIAN_POINT('Ctrl Pts',(79.6608402008991,-10.64975679698,74.695800898555));
#135198=CARTESIAN_POINT('Ctrl Pts',(79.7520930242391,-10.80610135726,74.6798452933831));
#135199=CARTESIAN_POINT('Ctrl Pts',(79.7689255810191,-10.83203863183,74.676940461329));
#135200=CARTESIAN_POINT('Ctrl Pts',(83.9545624191291,-5.46419092780999,
76.234980550845));
#135201=CARTESIAN_POINT('Ctrl Pts',(83.9320043553292,-5.49671033498799,
76.230132474877));
#135202=CARTESIAN_POINT('Ctrl Pts',(83.7201028686891,-5.80025368320099,
76.184529837611));
#135203=CARTESIAN_POINT('Ctrl Pts',(83.3159460310292,-6.34718810348699,
76.0964325131561));
#135204=CARTESIAN_POINT('Ctrl Pts',(82.7531884472392,-7.06055624972298,
75.969657019754));
#135205=CARTESIAN_POINT('Ctrl Pts',(82.2337337008491,-7.69686316050198,
75.847662890942));
#135206=CARTESIAN_POINT('Ctrl Pts',(81.7773180167191,-8.25467658193697,
75.735167157942));
#135207=CARTESIAN_POINT('Ctrl Pts',(81.3877522714791,-8.74512160944298,
75.632045987688));
#135208=CARTESIAN_POINT('Ctrl Pts',(81.0664882854092,-9.17823841639897,
75.538316722994));
#135209=CARTESIAN_POINT('Ctrl Pts',(80.8189229673591,-9.55943980782899,
75.454461873142));
#135210=CARTESIAN_POINT('Ctrl Pts',(80.6564128816691,-9.88596265458298,
75.382908707838));
#135211=CARTESIAN_POINT('Ctrl Pts',(80.5924580838091,-10.14639820296,75.329671426931));
#135212=CARTESIAN_POINT('Ctrl Pts',(80.6208048058091,-10.2905041774,75.309272938575));
#135213=CARTESIAN_POINT('Ctrl Pts',(80.6590014868791,-10.35405375722,75.304530742518));
#135214=CARTESIAN_POINT('Ctrl Pts',(80.6661993264591,-10.3646059106,75.30386970992));
#135215=CARTESIAN_POINT('',(82.3561757813562,-4.7644135527838,74.6407035195125));
#135216=CARTESIAN_POINT('Ctrl Pts',(82.3561756416491,-4.76441355133499,
74.640702721084));
#135217=CARTESIAN_POINT('Ctrl Pts',(83.0512807828209,-5.28772211312453,
74.5181259705316));
#135218=CARTESIAN_POINT('Ctrl Pts',(83.6506984183361,-5.657776597521,75.0433097570123));
#135219=CARTESIAN_POINT('Ctrl Pts',(83.8031649527491,-5.65793925324699,
75.908656789893));
#135220=CARTESIAN_POINT('',(79.7232095658691,-10.75961935955,75.104974613695));
#135221=CARTESIAN_POINT('Ctrl Pts',(79.7232075621687,-10.7596193609995,
75.1049632444806));
#135222=CARTESIAN_POINT('Ctrl Pts',(79.7630725189922,-10.7392515715418,
75.0979348824883));
#135223=CARTESIAN_POINT('Ctrl Pts',(79.8035264705227,-10.7187747365093,
75.0928921008376));
#135224=CARTESIAN_POINT('Ctrl Pts',(79.8443296875199,-10.6983123783093,
75.0899236141334));
#135225=CARTESIAN_POINT('Ctrl Pts',(79.8849266519198,-10.6779534534863,
75.086970132572));
#135226=CARTESIAN_POINT('Ctrl Pts',(79.9258687109959,-10.6576092029207,
75.0860703188784));
#135227=CARTESIAN_POINT('Ctrl Pts',(79.9669032426091,-10.637405650997,75.0872629107693));
#135228=CARTESIAN_POINT('Ctrl Pts',(80.0078270615794,-10.6172566089834,
75.0884522850042));
#135229=CARTESIAN_POINT('Ctrl Pts',(80.048842150844,-10.5972478633285,75.0917228906908));
#135230=CARTESIAN_POINT('Ctrl Pts',(80.0896916129765,-10.5775035253354,
75.0970616829426));
#135231=CARTESIAN_POINT('Ctrl Pts',(80.1305204886073,-10.5577691377022,
75.1023977846557));
#135232=CARTESIAN_POINT('Ctrl Pts',(80.1711831903889,-10.5382992363802,
75.1097998906766));
#135233=CARTESIAN_POINT('Ctrl Pts',(80.2114275641653,-10.5192115693662,
75.1192034346234));
#135234=CARTESIAN_POINT('Ctrl Pts',(80.2518036430065,-10.5000614354236,
75.1286377529182));
#135235=CARTESIAN_POINT('Ctrl Pts',(80.2917579677754,-10.4812963575788,
75.140086349217));
#135236=CARTESIAN_POINT('Ctrl Pts',(80.3310508541424,-10.4630240216372,
75.1534349448914));
#135237=CARTESIAN_POINT('Ctrl Pts',(80.3521815758161,-10.4531976209625,
75.1606134824336));
#135238=CARTESIAN_POINT('Ctrl Pts',(80.3731213285904,-10.4435134999413,
75.1683406847968));
#135239=CARTESIAN_POINT('Ctrl Pts',(80.3938356163,-10.4339866196942,75.1765934966013));
#135240=CARTESIAN_POINT('Ctrl Pts',(82.3561757813562,-4.7644135527838,74.6407035195124));
#135241=CARTESIAN_POINT('Ctrl Pts',(82.3221239964285,-4.81104613577596,
74.6467080292841));
#135242=CARTESIAN_POINT('Ctrl Pts',(82.2819510045132,-4.86594979744543,
74.6537921579147));
#135243=CARTESIAN_POINT('Ctrl Pts',(82.2353302578256,-4.92949163792966,
74.6620132425268));
#135244=CARTESIAN_POINT('Ctrl Pts',(82.1963898194681,-4.98256558672512,
74.6688799845101));
#135245=CARTESIAN_POINT('Ctrl Pts',(82.1529502963756,-5.04166596062972,
74.6765400536491));
#135246=CARTESIAN_POINT('Ctrl Pts',(82.1048406200159,-5.10703723698665,
74.6850232781176));
#135247=CARTESIAN_POINT('Ctrl Pts',(82.0744718091815,-5.14830228127526,
74.6903782390868));
#135248=CARTESIAN_POINT('Ctrl Pts',(82.0422424927113,-5.19206666016719,
74.6960611264546));
#135249=CARTESIAN_POINT('Ctrl Pts',(82.0081167610943,-5.2384002206557,74.7020781786132));
#135250=CARTESIAN_POINT('Ctrl Pts',(81.9530318251687,-5.31319074058829,
74.7117907596162));
#135251=CARTESIAN_POINT('Ctrl Pts',(81.9029879776772,-5.38115981935113,
74.7206139398688));
#135252=CARTESIAN_POINT('Ctrl Pts',(81.8580159512924,-5.44231213731585,
74.728542600352));
#135253=CARTESIAN_POINT('Ctrl Pts',(81.8545255151115,-5.44705838248937,
74.7291579714091));
#135254=CARTESIAN_POINT('Ctrl Pts',(81.8510656072557,-5.45176355720081,
74.7297679581739));
#135255=CARTESIAN_POINT('Ctrl Pts',(81.8476362310092,-5.45642766055757,
74.7303725602019));
#135256=CARTESIAN_POINT('Ctrl Pts',(81.7897173888807,-5.5351998472664,74.7405837026627));
#135257=CARTESIAN_POINT('Ctrl Pts',(81.7405128536315,-5.60225686290772,
74.7492581479741));
#135258=CARTESIAN_POINT('Ctrl Pts',(81.6999946187848,-5.6575950026414,74.7564016288351));
#135259=CARTESIAN_POINT('Ctrl Pts',(81.6893579677409,-5.67212210343909,
74.758276900881));
#135260=CARTESIAN_POINT('Ctrl Pts',(81.6793196375855,-5.68584165827859,
74.7600467078884));
#135261=CARTESIAN_POINT('Ctrl Pts',(81.6698786644967,-5.69875383118292,
74.7617112172398));
#135262=CARTESIAN_POINT('Ctrl Pts',(81.6686886663476,-5.70038136064545,
74.7619210222068));
#135263=CARTESIAN_POINT('Ctrl Pts',(81.6683273437372,-5.7008754568627,74.7619847257784));
#135264=CARTESIAN_POINT('Ctrl Pts',(81.6663372235841,-5.70359793366945,
74.7623355989125));
#135265=CARTESIAN_POINT('Ctrl Pts',(81.5948817180262,-5.801348793734,74.7749337413662));
#135266=CARTESIAN_POINT('Ctrl Pts',(81.5267190804947,-5.89510372642465,
74.7869527340684));
#135267=CARTESIAN_POINT('Ctrl Pts',(81.4618889464816,-5.98487156474155,
74.7983854107181));
#135268=CARTESIAN_POINT('Ctrl Pts',(81.4078304522936,-6.0597243201739,74.8079185282048));
#135269=CARTESIAN_POINT('Ctrl Pts',(81.3560877708969,-6.13180382130643,
74.8170441209648));
#135270=CARTESIAN_POINT('Ctrl Pts',(81.306661090005,-6.20110051149391,74.8257610770255));
#135271=CARTESIAN_POINT('Ctrl Pts',(81.2481693983869,-6.28310643540894,
74.8360767505959));
#135272=CARTESIAN_POINT('Ctrl Pts',(81.1929221026482,-6.36121851360164,
74.8458198412785));
#135273=CARTESIAN_POINT('Ctrl Pts',(81.1409094522912,-6.43545153318075,
74.8549918064151));
#135274=CARTESIAN_POINT('Ctrl Pts',(81.1046125165828,-6.48725491410077,
74.8613924460018));
#135275=CARTESIAN_POINT('Ctrl Pts',(81.0698899954668,-6.53716790196466,
74.8675151243425));
#135276=CARTESIAN_POINT('Ctrl Pts',(81.0367299620014,-6.58518392843638,
74.8733620037368));
#135277=CARTESIAN_POINT('Ctrl Pts',(81.0340476590933,-6.58906792715362,
74.8738349556601));
#135278=CARTESIAN_POINT('Ctrl Pts',(81.032028582115,-6.59199285596816,74.8741909645567));
#135279=CARTESIAN_POINT('Ctrl Pts',(81.0287139553208,-6.5967987589946,74.8747754050657));
#135280=CARTESIAN_POINT('Ctrl Pts',(80.9667110097929,-6.68669730928631,
74.8857078675397));
#135281=CARTESIAN_POINT('Ctrl Pts',(80.9076641870499,-6.77336666141212,
74.8961180734007));
#135282=CARTESIAN_POINT('Ctrl Pts',(80.851588657655,-6.85680944092805,74.9060037059959));
#135283=CARTESIAN_POINT('Ctrl Pts',(80.8423562546751,-6.8705476503496,74.90763129908));
#135284=CARTESIAN_POINT('Ctrl Pts',(80.8332043271957,-6.8841983055889,74.9092446841864));
#135285=CARTESIAN_POINT('Ctrl Pts',(80.8241328663999,-6.89776131979979,
74.9108438639246));
#135286=CARTESIAN_POINT('Ctrl Pts',(80.77311800239,-6.97403517922627,74.9198371163572));
#135287=CARTESIAN_POINT('Ctrl Pts',(80.7246506285624,-7.04754099513986,
74.928380878209));
#135288=CARTESIAN_POINT('Ctrl Pts',(80.6787380567842,-7.11829359512274,
74.9364755325432));
#135289=CARTESIAN_POINT('Ctrl Pts',(80.626784219497,-7.19835595984763,74.9456352972413));
#135290=CARTESIAN_POINT('Ctrl Pts',(80.5781015087018,-7.27489212079903,
74.9542199644315));
#135291=CARTESIAN_POINT('Ctrl Pts',(80.532660148748,-7.34787246637765,74.9622340772334));
#135292=CARTESIAN_POINT('Ctrl Pts',(80.5296548706722,-7.35269904359167,
74.9627640930059));
#135293=CARTESIAN_POINT('Ctrl Pts',(80.5266637578906,-7.35751005453043,
74.9632916146101));
#135294=CARTESIAN_POINT('Ctrl Pts',(80.5236867969952,-7.36230548535573,
74.9638166439294));
#135295=CARTESIAN_POINT('Ctrl Pts',(80.5150756114505,-7.37617679440315,
74.9653353487574));
#135296=CARTESIAN_POINT('Ctrl Pts',(80.5073241553266,-7.38871501544494,
74.9667024535959));
#135297=CARTESIAN_POINT('Ctrl Pts',(80.4983501549054,-7.40330432530424,
74.9682851937703));
#135298=CARTESIAN_POINT('Ctrl Pts',(80.4977500467791,-7.40427993963376,
74.9683910345543));
#135299=CARTESIAN_POINT('Ctrl Pts',(80.4971444854725,-7.40526473955174,
74.9684978372034));
#135300=CARTESIAN_POINT('Ctrl Pts',(80.4965328545644,-7.40625974310928,
74.9686057104389));
#135301=CARTESIAN_POINT('Ctrl Pts',(80.46837446561,-7.45206792057731,74.9735720005396));
#135302=CARTESIAN_POINT('Ctrl Pts',(80.440705411131,-7.4978088530134,74.9784521857506));
#135303=CARTESIAN_POINT('Ctrl Pts',(80.4135176054478,-7.54347000097511,
74.9832471695868));
#135304=CARTESIAN_POINT('Ctrl Pts',(80.3685775476264,-7.61894555253318,
74.9911730336069));
#135305=CARTESIAN_POINT('Ctrl Pts',(80.3249538825194,-7.69420657960239,
74.9988656263258));
#135306=CARTESIAN_POINT('Ctrl Pts',(80.2826641860576,-7.76928408816456,
75.0063220008348));
#135307=CARTESIAN_POINT('Ctrl Pts',(80.2376597238191,-7.84918115959677,
75.0142570335521));
#135308=CARTESIAN_POINT('Ctrl Pts',(80.1941661592217,-7.92887004618887,
75.0219245605863));
#135309=CARTESIAN_POINT('Ctrl Pts',(80.1521764989142,-8.00833548164509,
75.029327703204));
#135310=CARTESIAN_POINT('Ctrl Pts',(80.1334129141781,-8.04384556724371,
75.0326358865235));
#135311=CARTESIAN_POINT('Ctrl Pts',(80.1149492620323,-8.07931039451579,
75.0358913599496));
#135312=CARTESIAN_POINT('Ctrl Pts',(80.0967831423889,-8.11472588878158,
75.0390947913165));
#135313=CARTESIAN_POINT('Ctrl Pts',(80.0906365109561,-8.12670896466862,
75.0401786943359));
#135314=CARTESIAN_POINT('Ctrl Pts',(80.0848331226111,-8.13808014782504,
75.0412021145088));
#135315=CARTESIAN_POINT('Ctrl Pts',(80.0786613749382,-8.15023621169719,
75.0422905554439));
#135316=CARTESIAN_POINT('Ctrl Pts',(80.0767917592039,-8.15391866429993,
75.0426202783046));
#135317=CARTESIAN_POINT('Ctrl Pts',(80.0748884873749,-8.15767325589699,
75.0429559423772));
#135318=CARTESIAN_POINT('Ctrl Pts',(80.072932208086,-8.16153915038168,75.0433009601853));
#135319=CARTESIAN_POINT('Ctrl Pts',(80.043613191896,-8.21947782183391,75.0484717876623));
#135320=CARTESIAN_POINT('Ctrl Pts',(80.0156502083981,-8.27609885371883,
75.0534042929127));
#135321=CARTESIAN_POINT('Ctrl Pts',(79.9890818078875,-8.33144904932179,
75.0580896385779));
#135322=CARTESIAN_POINT('Ctrl Pts',(79.9608350316895,-8.39029582058631,
75.0630709663158));
#135323=CARTESIAN_POINT('Ctrl Pts',(79.9341643577204,-8.4477054531432,75.0677730730202));
#135324=CARTESIAN_POINT('Ctrl Pts',(79.9090774098314,-8.50368695604994,
75.0721954540087));
#135325=CARTESIAN_POINT('Ctrl Pts',(79.8812033453984,-8.56588790715731,
75.0771091538802));
#135326=CARTESIAN_POINT('Ctrl Pts',(79.8552843213017,-8.6263251588515,75.0816776561257));
#135327=CARTESIAN_POINT('Ctrl Pts',(79.8312871038823,-8.68496473123229,
75.085910083439));
#135328=CARTESIAN_POINT('Ctrl Pts',(79.8254713788145,-8.69917603019671,
75.0869358120971));
#135329=CARTESIAN_POINT('Ctrl Pts',(79.8197683525908,-8.71328157761121,
75.0879418373131));
#135330=CARTESIAN_POINT('Ctrl Pts',(79.8141772391394,-8.72728060331489,
75.0889283496757));
#135331=CARTESIAN_POINT('Ctrl Pts',(79.8046653956645,-8.75109634993732,
75.0906066470777));
#135332=CARTESIAN_POINT('Ctrl Pts',(79.795477694382,-8.77460396542405,75.0922283974265));
#135333=CARTESIAN_POINT('Ctrl Pts',(79.7866194227751,-8.79780470966671,
75.0937919953709));
#135334=CARTESIAN_POINT('Ctrl Pts',(79.7802486673301,-8.81449038767148,
75.0949165149792));
#135335=CARTESIAN_POINT('Ctrl Pts',(79.7742737074603,-8.83041144080335,
75.0959711805973));
#135336=CARTESIAN_POINT('Ctrl Pts',(79.7682783263875,-8.8466781920646,75.0970293115271));
#135337=CARTESIAN_POINT('Ctrl Pts',(79.7644494819658,-8.8570666659696,75.0977050681902));
#135338=CARTESIAN_POINT('Ctrl Pts',(79.7606130668678,-8.86759659475772,
75.0983821064623));
#135339=CARTESIAN_POINT('Ctrl Pts',(79.7566703009177,-8.87856264167374,
75.0990778206578));
#135340=CARTESIAN_POINT('Ctrl Pts',(79.7351734430435,-8.93835202683703,
75.1028710128913));
#135341=CARTESIAN_POINT('Ctrl Pts',(79.7152579742709,-8.99804003517536,
75.1063816931034));
#135342=CARTESIAN_POINT('Ctrl Pts',(79.6969295737615,-9.05763451574551,
75.1096098269183));
#135343=CARTESIAN_POINT('Ctrl Pts',(79.6769678574295,-9.12253969475887,
75.113125632428));
#135344=CARTESIAN_POINT('Ctrl Pts',(79.6588885374546,-9.18733260356596,
75.1163064075041));
#135345=CARTESIAN_POINT('Ctrl Pts',(79.6426434504958,-9.25200807264128,
75.11917148176));
#135346=CARTESIAN_POINT('Ctrl Pts',(79.639742788396,-9.26355628302679,75.1196830587266));
#135347=CARTESIAN_POINT('Ctrl Pts',(79.6369004788179,-9.27510074573733,
75.120184613422));
#135348=CARTESIAN_POINT('Ctrl Pts',(79.6341160902083,-9.2866414416212,75.120676308863));
#135349=CARTESIAN_POINT('Ctrl Pts',(79.6263836928899,-9.31869057642894,
75.1220417736176));
#135350=CARTESIAN_POINT('Ctrl Pts',(79.61909868291,-9.35071065533344,75.1233309327924));
#135351=CARTESIAN_POINT('Ctrl Pts',(79.6123009130382,-9.38270283214319,
75.1245337281322));
#135352=CARTESIAN_POINT('Ctrl Pts',(79.6070714399134,-9.4073141726246,75.1254590295212));
#135353=CARTESIAN_POINT('Ctrl Pts',(79.6021955212803,-9.43153028046108,
75.1263217229009));
#135354=CARTESIAN_POINT('Ctrl Pts',(79.5975563075042,-9.4558487462413,75.1271417835214));
#135355=CARTESIAN_POINT('Ctrl Pts',(79.5932086114474,-9.47863909453801,
75.127910313384));
#135356=CARTESIAN_POINT('Ctrl Pts',(79.5890685290809,-9.50151949673387,
75.128641461581));
#135357=CARTESIAN_POINT('Ctrl Pts',(79.5850822443732,-9.52491545505902,
75.1293444826069));
#135358=CARTESIAN_POINT('Ctrl Pts',(79.5836856738333,-9.53311208639536,
75.1295907817365));
#135359=CARTESIAN_POINT('Ctrl Pts',(79.5823084003387,-9.541372138301,75.1298335565016));
#135360=CARTESIAN_POINT('Ctrl Pts',(79.5809495788261,-9.54971437395797,
75.1300729528898));
#135361=CARTESIAN_POINT('Ctrl Pts',(79.5721197715963,-9.60392335728163,
75.1316285832214));
#135362=CARTESIAN_POINT('Ctrl Pts',(79.5650408348773,-9.65723474203919,
75.132869710263));
#135363=CARTESIAN_POINT('Ctrl Pts',(79.5596463435658,-9.7097450737704,75.1338145482961));
#135364=CARTESIAN_POINT('Ctrl Pts',(79.5554914375936,-9.75018920062338,
75.134542274593));
#135365=CARTESIAN_POINT('Ctrl Pts',(79.5523341231431,-9.79015859311037,
75.1350947484855));
#135366=CARTESIAN_POINT('Ctrl Pts',(79.5501298052424,-9.82971155303763,
75.1354849314204));
#135367=CARTESIAN_POINT('Ctrl Pts',(79.5479574546926,-9.8686909099715,75.1358694558635));
#135368=CARTESIAN_POINT('Ctrl Pts',(79.5467119299754,-9.90726279713684,
75.1360958039005));
#135369=CARTESIAN_POINT('Ctrl Pts',(79.5464278727914,-9.94536583373473,
75.1361518654945));
#135370=CARTESIAN_POINT('Ctrl Pts',(79.5461164371936,-9.98714137275784,
75.1362133304988));
#135371=CARTESIAN_POINT('Ctrl Pts',(79.5469598782716,-10.0283533260274,
75.1360703538199));
#135372=CARTESIAN_POINT('Ctrl Pts',(79.5489855899427,-10.0689808890031,
75.1357154900053));
#135373=CARTESIAN_POINT('Ctrl Pts',(79.5511059017912,-10.1115057479858,
75.1353440541481));
#135374=CARTESIAN_POINT('Ctrl Pts',(79.5545202284435,-10.1533908886193,
75.13474085066));
#135375=CARTESIAN_POINT('Ctrl Pts',(79.5592581195504,-10.1946704171859,
75.1339011255562));
#135376=CARTESIAN_POINT('Ctrl Pts',(79.5641087126388,-10.2369318772835,
75.1330414255984));
#135377=CARTESIAN_POINT('Ctrl Pts',(79.5703452491432,-10.278559263329,75.1319342008308));
#135378=CARTESIAN_POINT('Ctrl Pts',(79.5780177252569,-10.3196387049876,
75.1305723363191));
#135379=CARTESIAN_POINT('Ctrl Pts',(79.5793401065986,-10.3267189078285,
75.1303376136307));
#135380=CARTESIAN_POINT('Ctrl Pts',(79.5807052148809,-10.3337829357129,
75.1300953139451));
#135381=CARTESIAN_POINT('Ctrl Pts',(79.5821134039448,-10.3408313516033,
75.1298453823846));
#135382=CARTESIAN_POINT('Ctrl Pts',(79.5890482516137,-10.375542379944,75.1286145552577));
#135383=CARTESIAN_POINT('Ctrl Pts',(79.5970246912381,-10.4098719194339,
75.1271993692909));
#135384=CARTESIAN_POINT('Ctrl Pts',(79.6059698498263,-10.4437654138459,
75.1256157332226));
#135385=CARTESIAN_POINT('Ctrl Pts',(79.6154126888406,-10.4795446354452,
75.1239439886356));
#135386=CARTESIAN_POINT('Ctrl Pts',(79.625934712514,-10.5148388029595,75.1220846122702));
#135387=CARTESIAN_POINT('Ctrl Pts',(79.6374969220201,-10.5496153933239,
75.1200456353118));
#135388=CARTESIAN_POINT('Ctrl Pts',(79.6495130050908,-10.5857571358272,
75.1179266184839));
#135389=CARTESIAN_POINT('Ctrl Pts',(79.6626522281328,-10.6213410362105,
75.1156137189209));
#135390=CARTESIAN_POINT('Ctrl Pts',(79.6769247672827,-10.6563478055494,
75.1131033722144));
#135391=CARTESIAN_POINT('Ctrl Pts',(79.6911973064326,-10.6913545748884,
75.110593025508));
#135392=CARTESIAN_POINT('Ctrl Pts',(79.7066031008277,-10.7257855013312,
75.1078852865875));
#135393=CARTESIAN_POINT('Ctrl Pts',(79.7232075620335,-10.759619360724,75.1049632445044));
#135394=CARTESIAN_POINT('Origin',(76.0272472665391,1.4210854715202E-14,
75.756664172774));
#135395=CARTESIAN_POINT('',(70.6107670387343,10.7594267271077,76.7115217636943));
#135396=CARTESIAN_POINT('',(70.610804188022,15.19124921296,76.7117292269897));
#135397=CARTESIAN_POINT('',(79.7231084232435,10.7594837524526,75.1049862577436));
#135398=CARTESIAN_POINT('',(70.6108041880485,10.75942685431,76.7117292269834));
#135399=CARTESIAN_POINT('',(82.3561326928982,4.76438284010808,74.6407108908467));
#135400=CARTESIAN_POINT('Ctrl Pts',(79.7231078884045,10.7594837533888,75.1049832214982));
#135401=CARTESIAN_POINT('Ctrl Pts',(79.7070082779656,10.726820962897,75.1078091201574));
#135402=CARTESIAN_POINT('Ctrl Pts',(79.6920518177104,10.6931496567333,75.1104327299098));
#135403=CARTESIAN_POINT('Ctrl Pts',(79.6781973871937,10.658469790198,75.1128661223029));
#135404=CARTESIAN_POINT('Ctrl Pts',(79.6648230633814,10.6249917079157,75.1152151887468));
#135405=CARTESIAN_POINT('Ctrl Pts',(79.6524756942354,10.5905725491408,75.1173869962559));
#135406=CARTESIAN_POINT('Ctrl Pts',(79.6411639813269,10.5552105178972,75.1193817573135));
#135407=CARTESIAN_POINT('Ctrl Pts',(79.633830050797,10.5322836028813,75.1206750573767));
#135408=CARTESIAN_POINT('Ctrl Pts',(79.6269323777341,10.5089603238528,75.1218937225791));
#135409=CARTESIAN_POINT('Ctrl Pts',(79.620484386902,10.4852436765249,75.1230352328094));
#135410=CARTESIAN_POINT('Ctrl Pts',(79.6114627338706,10.4520607256136,75.124632367405));
#135411=CARTESIAN_POINT('Ctrl Pts',(79.6032995916269,10.4180937995382,75.1260824053101));
#135412=CARTESIAN_POINT('Ctrl Pts',(79.5959883440864,10.3833556959088,75.1273839093862));
#135413=CARTESIAN_POINT('Ctrl Pts',(79.5912317856939,10.3607557473439,75.1282306431483));
#135414=CARTESIAN_POINT('Ctrl Pts',(79.5868366108061,10.3378294547095,75.1290143143681));
#135415=CARTESIAN_POINT('Ctrl Pts',(79.5828116799533,10.3145854786651,75.1297320293526));
#135416=CARTESIAN_POINT('Ctrl Pts',(79.5792932827944,10.2942667347497,75.1303594205936));
#135417=CARTESIAN_POINT('Ctrl Pts',(79.5760582626127,10.2737056656046,75.1309363036806));
#135418=CARTESIAN_POINT('Ctrl Pts',(79.5730919731977,10.2528807038193,75.131464874312));
#135419=CARTESIAN_POINT('Ctrl Pts',(79.5713315872362,10.2405218388381,75.1317785619496));
#135420=CARTESIAN_POINT('Ctrl Pts',(79.5696194381391,10.2277538194173,75.1320834751498));
#135421=CARTESIAN_POINT('Ctrl Pts',(79.5680312437019,10.2150153947845,75.1323661160601));
#135422=CARTESIAN_POINT('Ctrl Pts',(79.566395837817,10.2018983014856,75.1326571588929));
#135423=CARTESIAN_POINT('Ctrl Pts',(79.5648917760965,10.1888127234786,75.132924598392));
#135424=CARTESIAN_POINT('Ctrl Pts',(79.5635468212511,10.1762414066899,75.1331634348129));
#135425=CARTESIAN_POINT('Ctrl Pts',(79.563335072354,10.1742621859944,75.133201037078));
#135426=CARTESIAN_POINT('Ctrl Pts',(79.5631271639158,10.1722957169947,75.1332379487389));
#135427=CARTESIAN_POINT('Ctrl Pts',(79.5629230928202,10.1703438878504,75.1332741701308));
#135428=CARTESIAN_POINT('Ctrl Pts',(79.5589306391852,10.1321582381965,75.1339828066339));
#135429=CARTESIAN_POINT('Ctrl Pts',(79.555918953989,10.0939607728326,75.1345142386359));
#135430=CARTESIAN_POINT('Ctrl Pts',(79.5538527889503,10.0556979012006,75.1348750924712));
#135431=CARTESIAN_POINT('Ctrl Pts',(79.551752688671,10.0168065900539,75.1352418730652));
#135432=CARTESIAN_POINT('Ctrl Pts',(79.5506303572892,9.97784751617017,75.1354321980372));
#135433=CARTESIAN_POINT('Ctrl Pts',(79.5504708272491,9.93881356657663,75.1354515644425));
#135434=CARTESIAN_POINT('Ctrl Pts',(79.550311178441,9.89975055670353,75.135470945266));
#135435=CARTESIAN_POINT('Ctrl Pts',(79.5511167030462,9.86061244466846,75.1353188680087));
#135436=CARTESIAN_POINT('Ctrl Pts',(79.552880091036,9.82144305966724,75.1350029516353));
#135437=CARTESIAN_POINT('Ctrl Pts',(79.5530813947466,9.81697158623648,75.1349668874574));
#135438=CARTESIAN_POINT('Ctrl Pts',(79.5532951806317,9.81249976102359,75.1349286927825));
#135439=CARTESIAN_POINT('Ctrl Pts',(79.5535214357738,9.80802769258847,75.1348883829843));
#135440=CARTESIAN_POINT('Ctrl Pts',(79.5554633733376,9.76964413322029,75.1345424058251));
#135441=CARTESIAN_POINT('Ctrl Pts',(79.5583236194021,9.73124042997169,75.1340405635673));
#135442=CARTESIAN_POINT('Ctrl Pts',(79.5621872529113,9.69276973148076,75.1333629948776));
#135443=CARTESIAN_POINT('Ctrl Pts',(79.5643905906368,9.67083081281542,75.1329765936694));
#135444=CARTESIAN_POINT('Ctrl Pts',(79.5669372443528,9.64853832588428,75.1325300942824));
#135445=CARTESIAN_POINT('Ctrl Pts',(79.5697919943059,9.62631094002634,75.1320290018005));
#135446=CARTESIAN_POINT('Ctrl Pts',(79.5727801100865,9.60304515369211,75.131504499698));
#135447=CARTESIAN_POINT('Ctrl Pts',(79.5761056023998,9.57985087973573,75.1309201955627));
#135448=CARTESIAN_POINT('Ctrl Pts',(79.5796725514381,9.55719464793694,75.1302925377443));
#135449=CARTESIAN_POINT('Ctrl Pts',(79.5809847096477,9.54886019733674,75.1300616439608));
#135450=CARTESIAN_POINT('Ctrl Pts',(79.5823290394124,9.54059841602428,75.1298249768127));
#135451=CARTESIAN_POINT('Ctrl Pts',(79.5836991450315,9.53243203649979,75.1295836577841));
#135452=CARTESIAN_POINT('Ctrl Pts',(79.5912973542496,9.48714365922797,75.128245372296));
#135453=CARTESIAN_POINT('Ctrl Pts',(79.6001170930243,9.44123006425086,75.1266880721847));
#135454=CARTESIAN_POINT('Ctrl Pts',(79.6101544028514,9.3946257529472,75.1249135801248));
#135455=CARTESIAN_POINT('Ctrl Pts',(79.6190959753332,9.35310906823115,75.1233328030395));
#135456=CARTESIAN_POINT('Ctrl Pts',(79.6290041575734,9.31104459616811,75.1215795440022));
#135457=CARTESIAN_POINT('Ctrl Pts',(79.6398429807233,9.26838909153277,75.1196660781351));
#135458=CARTESIAN_POINT('Ctrl Pts',(79.6560516620485,9.20460084885738,75.1168046274003));
#135459=CARTESIAN_POINT('Ctrl Pts',(79.6743381454125,9.13949070888761,75.1135862443996));
#135460=CARTESIAN_POINT('Ctrl Pts',(79.6949050531781,9.07293568106988,75.109963852423));
#135461=CARTESIAN_POINT('Ctrl Pts',(79.7117269136601,9.01849971990908,75.1070010651563));
#135462=CARTESIAN_POINT('Ctrl Pts',(79.7300746113099,8.96309822499194,75.1037678757341));
#135463=CARTESIAN_POINT('Ctrl Pts',(79.7500221789991,8.90665503474601,75.1002492468614));
#135464=CARTESIAN_POINT('Ctrl Pts',(79.754463101825,8.89408909909735,75.0994658952508));
#135465=CARTESIAN_POINT('Ctrl Pts',(79.7589831423494,8.88147146004617,75.0986684496512));
#135466=CARTESIAN_POINT('Ctrl Pts',(79.7635827824328,8.86880112587223,75.0978568459067));
#135467=CARTESIAN_POINT('Ctrl Pts',(79.7773044742438,8.83100285958951,75.0954356615852));
#135468=CARTESIAN_POINT('Ctrl Pts',(79.7918795735844,8.79239252981469,75.092862743707));
#135469=CARTESIAN_POINT('Ctrl Pts',(79.8071842401293,8.75324530252362,75.0901616548501));
#135470=CARTESIAN_POINT('Ctrl Pts',(79.8125917316084,8.7394136847366,75.0892072978939));
#135471=CARTESIAN_POINT('Ctrl Pts',(79.8180899015046,8.72551478939534,75.0882370294827));
#135472=CARTESIAN_POINT('Ctrl Pts',(79.8236720223815,8.71155991451721,75.087252177119));
#135473=CARTESIAN_POINT('Ctrl Pts',(79.8415668027282,8.6668243335047,75.0840950049416));
#135474=CARTESIAN_POINT('Ctrl Pts',(79.8603273193853,8.62151576697663,75.0807874286856));
#135475=CARTESIAN_POINT('Ctrl Pts',(79.879771670602,8.57602561894005,75.0773597580627));
#135476=CARTESIAN_POINT('Ctrl Pts',(79.8911250151272,8.54946441782781,75.075358378584));
#135477=CARTESIAN_POINT('Ctrl Pts',(79.902710683486,8.52284070338079,75.0733162053902));
#135478=CARTESIAN_POINT('Ctrl Pts',(79.9144862264433,8.49622725323734,75.0712404748654));
#135479=CARTESIAN_POINT('Ctrl Pts',(79.948623841926,8.41907414607641,75.065222876292));
#135480=CARTESIAN_POINT('Ctrl Pts',(79.9840849050885,8.34254582030358,75.0589706569375));
#135481=CARTESIAN_POINT('Ctrl Pts',(80.020876997391,8.26665047317756,75.0524819528386));
#135482=CARTESIAN_POINT('Ctrl Pts',(80.0369322254888,8.23353147848552,75.0496504306868));
#135483=CARTESIAN_POINT('Ctrl Pts',(80.0532404759853,8.20053259600165,75.046774052383));
#135484=CARTESIAN_POINT('Ctrl Pts',(80.0698003682878,8.16765215996091,75.0438534924458));
#135485=CARTESIAN_POINT('Ctrl Pts',(80.075115914082,8.15709789666547,75.0429160243871));
#135486=CARTESIAN_POINT('Ctrl Pts',(80.08070748445,8.1460649251352,75.041929900323));
#135487=CARTESIAN_POINT('Ctrl Pts',(80.0860636261943,8.13555918782317,75.0409853404909));
#135488=CARTESIAN_POINT('Ctrl Pts',(80.0885538792637,8.13067471205022,75.040546182393));
#135489=CARTESIAN_POINT('Ctrl Pts',(80.0909930374926,8.12590404984408,75.040116044511));
#135490=CARTESIAN_POINT('Ctrl Pts',(80.0933287711423,8.12134760111213,75.0397041525492));
#135491=CARTESIAN_POINT('Ctrl Pts',(80.1259859114226,8.05764145660503,75.0339452709327));
#135492=CARTESIAN_POINT('Ctrl Pts',(80.1614580645366,7.99078064940021,75.0276914898257));
#135493=CARTESIAN_POINT('Ctrl Pts',(80.1997498623677,7.9207730884256,75.0209405741994));
#135494=CARTESIAN_POINT('Ctrl Pts',(80.2132341063598,7.89612031454328,75.0185632767459));
#135495=CARTESIAN_POINT('Ctrl Pts',(80.2270677787215,7.87107697126626,75.0161243674933));
#135496=CARTESIAN_POINT('Ctrl Pts',(80.2412502141385,7.84564198354711,75.0136238965939));
#135497=CARTESIAN_POINT('Ctrl Pts',(80.2537627413835,7.82320183363941,75.011417843167));
#135498=CARTESIAN_POINT('Ctrl Pts',(80.2669903513467,7.79967091032429,75.0090856555643));
#135499=CARTESIAN_POINT('Ctrl Pts',(80.2800178675766,7.77667701216853,75.0067886517101));
#135500=CARTESIAN_POINT('Ctrl Pts',(80.2858897676175,7.76631295894936,75.005753321814));
#135501=CARTESIAN_POINT('Ctrl Pts',(80.291720465817,7.75605752068295,75.0047252376859));
#135502=CARTESIAN_POINT('Ctrl Pts',(80.2974236300149,7.74605749375833,75.0037196216616));
#135503=CARTESIAN_POINT('Ctrl Pts',(80.3341362693609,7.68168491580153,74.997246229499));
#135504=CARTESIAN_POINT('Ctrl Pts',(80.3713257017052,7.61779994526875,74.9906878882944));
#135505=CARTESIAN_POINT('Ctrl Pts',(80.4089919611734,7.55440258182021,74.9840447954842));
#135506=CARTESIAN_POINT('Ctrl Pts',(80.4123996965283,7.54866690644703,74.9834437827329));
#135507=CARTESIAN_POINT('Ctrl Pts',(80.4158207173055,7.54291963320371,74.9828404221964));
#135508=CARTESIAN_POINT('Ctrl Pts',(80.4192525011407,7.53716499829019,74.9822351592188));
#135509=CARTESIAN_POINT('Ctrl Pts',(80.4421807333016,7.49871747023126,74.9781913118393));
#135510=CARTESIAN_POINT('Ctrl Pts',(80.4655926542994,7.4599444154685,74.9740619850969));
#135511=CARTESIAN_POINT('Ctrl Pts',(80.4887216130273,7.42210259000131,74.9699827347123));
#135512=CARTESIAN_POINT('Ctrl Pts',(80.5003949765524,7.40300352936788,74.9679239056396));
#135513=CARTESIAN_POINT('Ctrl Pts',(80.5119956206347,7.38414107161203,74.9658779424929));
#135514=CARTESIAN_POINT('Ctrl Pts',(80.5234215035191,7.36567331268513,74.9638628633655));
#135515=CARTESIAN_POINT('Ctrl Pts',(80.5691421296126,7.29177464689076,74.9557995320446));
#135516=CARTESIAN_POINT('Ctrl Pts',(80.6171836659155,7.21567229807172,74.9473280496147));
#135517=CARTESIAN_POINT('Ctrl Pts',(80.6675700432805,7.13739027779629,74.9384446819144));
#135518=CARTESIAN_POINT('Ctrl Pts',(80.7145949842145,7.06433070153476,74.9301539520933));
#135519=CARTESIAN_POINT('Ctrl Pts',(80.7636625121015,6.98937310146812,74.9215044753442));
#135520=CARTESIAN_POINT('Ctrl Pts',(80.8147666497352,6.91250481183277,74.9124953349109));
#135521=CARTESIAN_POINT('Ctrl Pts',(80.8709348331921,6.8280194375719,74.9025934546313));
#135522=CARTESIAN_POINT('Ctrl Pts',(80.9295626386359,6.74122532433875,74.8922569264201));
#135523=CARTESIAN_POINT('Ctrl Pts',(80.990643650238,6.65212799426251,74.8814869623144));
#135524=CARTESIAN_POINT('Ctrl Pts',(81.0034595898712,6.6334337065651,74.8792272222379));
#135525=CARTESIAN_POINT('Ctrl Pts',(81.0163834300284,6.61463787203028,74.8769484178491));
#135526=CARTESIAN_POINT('Ctrl Pts',(81.0294149479476,6.59574028291107,74.8746505893709));
#135527=CARTESIAN_POINT('Ctrl Pts',(81.0356148525333,6.58674952295774,74.8735573692712));
#135528=CARTESIAN_POINT('Ctrl Pts',(81.0429569835255,6.57611940119855,74.8722627305951));
#135529=CARTESIAN_POINT('Ctrl Pts',(81.0480881216829,6.56869910851812,74.8713579507368));
#135530=CARTESIAN_POINT('Ctrl Pts',(81.0952901848121,6.50043879028162,74.8630347532938));
#135531=CARTESIAN_POINT('Ctrl Pts',(81.1458682724802,6.42805597799933,74.8541157555898));
#135532=CARTESIAN_POINT('Ctrl Pts',(81.1998509741463,6.35155770879548,74.8445960348589));
#135533=CARTESIAN_POINT('Ctrl Pts',(81.2211447097429,6.32138259958922,74.8408409353559));
#135534=CARTESIAN_POINT('Ctrl Pts',(81.2429678750177,6.29056675285114,74.8369924256807));
#135535=CARTESIAN_POINT('Ctrl Pts',(81.2653208450812,6.25910868413534,74.8330504750036));
#135536=CARTESIAN_POINT('Ctrl Pts',(81.3236026068405,6.17708684716751,74.8227724748285));
#135537=CARTESIAN_POINT('Ctrl Pts',(81.3854886357688,6.09070017487662,74.811858887219));
#135538=CARTESIAN_POINT('Ctrl Pts',(81.4509817974625,5.99996393598028,74.8003102486381));
#135539=CARTESIAN_POINT('Ctrl Pts',(81.5116542981529,5.91590638898266,74.7896116540955));
#135540=CARTESIAN_POINT('Ctrl Pts',(81.5754228369729,5.82811668083589,74.7783680252541));
#135541=CARTESIAN_POINT('Ctrl Pts',(81.6422547371113,5.73658116761233,74.766584770311));
#135542=CARTESIAN_POINT('Ctrl Pts',(81.6475647858335,5.72930832284767,74.7656485458773));
#135543=CARTESIAN_POINT('Ctrl Pts',(81.6528941518874,5.72201181362249,74.7647089177965));
#135544=CARTESIAN_POINT('Ctrl Pts',(81.658242807361,5.71469162347861,74.7637658903752));
#135545=CARTESIAN_POINT('Ctrl Pts',(81.6601629436174,5.71206371772394,74.763427349007));
#135546=CARTESIAN_POINT('Ctrl Pts',(81.66326315078,5.70782163301846,74.7628807484576));
#135547=CARTESIAN_POINT('Ctrl Pts',(81.6640107439547,5.70679877827081,74.7627489396177));
#135548=CARTESIAN_POINT('Ctrl Pts',(81.6820712998922,5.68208837960556,74.7595646663972));
#135549=CARTESIAN_POINT('Ctrl Pts',(81.709573624922,5.64457759598908,74.7547157559832));
#135550=CARTESIAN_POINT('Ctrl Pts',(81.7465266716699,5.5942442761862,74.7482004881556));
#135551=CARTESIAN_POINT('Ctrl Pts',(81.7561074991364,5.58119434132866,74.7465112727201));
#135552=CARTESIAN_POINT('Ctrl Pts',(81.7663236195077,5.56728275206466,74.7447100391271));
#135553=CARTESIAN_POINT('Ctrl Pts',(81.7771750774218,5.5525096269153,74.7427967681625));
#135554=CARTESIAN_POINT('Ctrl Pts',(81.8076290683302,5.51104970304621,74.7374272835254));
#135555=CARTESIAN_POINT('Ctrl Pts',(81.8430884180969,5.4628038378542,74.7311751286016));
#135556=CARTESIAN_POINT('Ctrl Pts',(81.8835443613486,5.40778106533438,74.7240418188966));
#135557=CARTESIAN_POINT('Ctrl Pts',(81.9180946272034,5.36079040671102,74.7179498154251));
#135558=CARTESIAN_POINT('Ctrl Pts',(81.9571909747051,5.307630835837,74.7110561303366));
#135559=CARTESIAN_POINT('Ctrl Pts',(81.9983050426644,5.25174170406474,74.7038065921594));
#135560=CARTESIAN_POINT('Ctrl Pts',(82.0010104014637,5.2480641269742,74.7033295631795));
#135561=CARTESIAN_POINT('Ctrl Pts',(82.0037244899494,5.2443747138067,74.7028509946115));
#135562=CARTESIAN_POINT('Ctrl Pts',(82.0064465853113,5.24067443695834,74.7023710139139));
#135563=CARTESIAN_POINT('Ctrl Pts',(82.0581749918029,5.17035749375995,74.6932498651909));
#135564=CARTESIAN_POINT('Ctrl Pts',(82.1047779125546,5.10703436772081,74.6850323825771));
#135565=CARTESIAN_POINT('Ctrl Pts',(82.1462269620154,5.05066588751002,74.6777236571409));
#135566=CARTESIAN_POINT('Ctrl Pts',(82.1926906200799,4.98747780903283,74.6695307040099));
#135567=CARTESIAN_POINT('Ctrl Pts',(82.2326792188266,4.93302931311516,74.6624794640148));
#135568=CARTESIAN_POINT('Ctrl Pts',(82.2661944956993,4.88731790017762,74.6565696842625));
#135569=CARTESIAN_POINT('Ctrl Pts',(82.2922097950288,4.85183569023323,74.6519823824833));
#135570=CARTESIAN_POINT('Ctrl Pts',(82.3143258827971,4.82161901374268,74.648082639237));
#135571=CARTESIAN_POINT('Ctrl Pts',(82.3325496921101,4.79668191808424,74.6448692347889));
#135572=CARTESIAN_POINT('Ctrl Pts',(82.3413098557611,4.78469468560195,74.6433245550593));
#135573=CARTESIAN_POINT('Ctrl Pts',(82.349170640157,4.77392756708913,74.6419384647133));
#135574=CARTESIAN_POINT('Ctrl Pts',(82.3561326848172,4.76438284010716,74.6407108450246));
#135575=CARTESIAN_POINT('Origin',(76.0272472665991,1.4210854715202E-14,
75.756664173113));
#135576=CARTESIAN_POINT('',(70.6107884237591,-10.75942680297,76.71163854688));
#135577=CARTESIAN_POINT('',(79.7232081440958,-10.75961935955,75.1049665504179));
#135578=CARTESIAN_POINT('',(70.6108046249791,15.19124921296,76.7117291499424));
#135579=CARTESIAN_POINT('Origin',(76.6422369709091,1.4210854715202E-14,
79.244444102405));
#135580=CARTESIAN_POINT('Origin',(76.9027092374091,1.4210854715202E-14,
80.721655731923));
#135581=CARTESIAN_POINT('Ctrl Pts',(84.761279993589,1.01916108789501,82.134994479025));
#135582=CARTESIAN_POINT('Ctrl Pts',(84.7732730139091,0.938468758587613,
82.139847664892));
#135583=CARTESIAN_POINT('Ctrl Pts',(84.8096488123091,0.660239861587714,
82.154593658101));
#135584=CARTESIAN_POINT('Ctrl Pts',(84.8337698688191,0.312978103185414,
82.164415977497));
#135585=CARTESIAN_POINT('Ctrl Pts',(84.836850135019,0.0467873211332242,
82.165668020133));
#135586=CARTESIAN_POINT('Ctrl Pts',(84.8366553313491,-0.0200748059259058,
82.165588413034));
#135587=CARTESIAN_POINT('Ctrl Pts',(84.5809173493991,0.995359843725814,
82.174776982057));
#135588=CARTESIAN_POINT('Ctrl Pts',(84.5926714924792,0.916555418610414,
82.1796767163611));
#135589=CARTESIAN_POINT('Ctrl Pts',(84.6283234134691,0.644831872479714,
82.194563930964));
#135590=CARTESIAN_POINT('Ctrl Pts',(84.6519656862891,0.305675624410314,
82.204479935355));
#135591=CARTESIAN_POINT('Ctrl Pts',(84.6549847954192,0.0456956593620242,
82.2057439237761));
#135592=CARTESIAN_POINT('Ctrl Pts',(84.6547938588891,-0.0196064101613658,
82.2056635572961));
#135593=CARTESIAN_POINT('Ctrl Pts',(84.4304376221692,0.967037811556315,
82.068788726581));
#135594=CARTESIAN_POINT('Ctrl Pts',(84.4417750514292,0.890447491682914,
82.073688402416));
#135595=CARTESIAN_POINT('Ctrl Pts',(84.4761583942091,0.626392695906014,
82.0885737356621));
#135596=CARTESIAN_POINT('Ctrl Pts',(84.4989506696391,0.296922598800314,
82.0984857915431));
#135597=CARTESIAN_POINT('Ctrl Pts',(84.5018613118091,0.0443872372795342,
82.099749605468));
#135598=CARTESIAN_POINT('Ctrl Pts',(84.5016772295791,-0.0190450268719158,
82.0996693174671));
#135599=CARTESIAN_POINT('Ctrl Pts',(84.4060067611391,0.952294539800014,
81.884762831103));
#135600=CARTESIAN_POINT('Ctrl Pts',(84.417015946189,0.876829574608914,81.889615878929));
#135601=CARTESIAN_POINT('Ctrl Pts',(84.450396710689,0.616706117970314,81.904357430372));
#135602=CARTESIAN_POINT('Ctrl Pts',(84.4725109764891,0.292312756701114,
81.914170427584));
#135603=CARTESIAN_POINT('Ctrl Pts',(84.4753351589791,0.0436982183603942,
81.915422058245));
#135604=CARTESIAN_POINT('Ctrl Pts',(84.4751565378891,-0.0187494150606258,
81.91534263643));
#135605=CARTESIAN_POINT('',(84.7549733371667,0.998148603023009,82.1380581359606));
#135606=CARTESIAN_POINT('Origin',(84.7030401686601,0.973190333485317,81.8436101836762));
#135607=CARTESIAN_POINT('',(84.8242224574765,-4.37596713747203E-12,82.1680724930567));
#135608=CARTESIAN_POINT('Origin',(84.7721268038191,1.61954280611347E-8,
81.872630608394));
#135609=CARTESIAN_POINT('Origin',(78.7905139183666,0.196679718677362,79.5581506211462));
#135610=CARTESIAN_POINT('Origin',(60.0158221861891,1.4210854715202E-14,
74.357344709869));
#135611=CARTESIAN_POINT('',(84.7549627479325,-0.99814350218451,82.1379981311978));
#135612=CARTESIAN_POINT('Origin',(68.4696192519035,0.303986406784001,75.1006252905782));
#135613=CARTESIAN_POINT('',(94.9937559642379,-0.99814863954275,80.3326845061067));
#135614=CARTESIAN_POINT('',(62.0923792317741,-0.998148599370046,86.1340849298962));
#135615=CARTESIAN_POINT('',(95.0009770511691,1.4210854715202E-14,80.37363732553));
#135616=CARTESIAN_POINT('Origin',(92.9168980472373,7.21782711207708E-5,
68.5542381272426));
#135617=CARTESIAN_POINT('',(94.9937559642119,0.998148641326583,80.3326845059602));
#135618=CARTESIAN_POINT('Origin',(92.9168981020881,-7.21782753166342E-5,
68.554238117227));
#135619=CARTESIAN_POINT('',(62.0923792317078,0.998148602984376,86.1340849296003));
#135620=CARTESIAN_POINT('Origin',(60.0158221861891,1.4210854715202E-14,
74.357344709869));
#135621=CARTESIAN_POINT('',(69.9536255526515,4.5030342410532E-9,84.7901609152031));
#135622=CARTESIAN_POINT('',(70.0084327588244,0.998148594771459,84.7382711127335));
#135623=CARTESIAN_POINT('Origin',(82.9054078707814,-0.300965714281284,72.554181695039));
#135624=CARTESIAN_POINT('',(45.1145255780036,0.998148899244916,89.1277385792758));
#135625=CARTESIAN_POINT('',(62.092379227415,0.998148899153649,86.1340849052551));
#135626=CARTESIAN_POINT('',(45.1145147830591,-0.998148588064286,89.12774050813));
#135627=CARTESIAN_POINT('Origin',(33.434640608385,-0.00348829429348399,
82.0882160785412));
#135628=CARTESIAN_POINT('',(70.0084221937706,-0.998143435151018,84.7382111936731));
#135629=CARTESIAN_POINT('',(62.0923792319381,-0.998148588051504,86.1340849308266));
#135630=CARTESIAN_POINT('Origin',(82.9047265017384,0.317497967067761,72.554660600933));
#135631=CARTESIAN_POINT('Origin',(58.9775436614391,-0.499074165591686,68.468974588834));
#135632=CARTESIAN_POINT('',(91.9214587222691,17.49925882517,62.90882101338));
#135633=CARTESIAN_POINT('Ctrl Pts',(94.9937559636691,0.998148678733514,
80.332684502887));
#135634=CARTESIAN_POINT('Ctrl Pts',(94.9618224451266,3.20135410881214,80.1515805199092));
#135635=CARTESIAN_POINT('Ctrl Pts',(94.8586253251175,5.36962766443818,79.5663205693643));
#135636=CARTESIAN_POINT('Ctrl Pts',(94.5234359225885,9.34778727496904,77.665367004673));
#135637=CARTESIAN_POINT('Ctrl Pts',(94.2915459635635,11.156458914409,76.3502536959021));
#135638=CARTESIAN_POINT('Ctrl Pts',(93.7300322273922,14.1723129419968,73.1657510524878));
#135639=CARTESIAN_POINT('Ctrl Pts',(93.4005798639225,15.3785746783534,71.297333853112));
#135640=CARTESIAN_POINT('Ctrl Pts',(92.6881230943526,17.0272550257457,67.2567907285858));
#135641=CARTESIAN_POINT('Ctrl Pts',(92.3053361804104,17.4691703430208,65.0858982627576));
#135642=CARTESIAN_POINT('Ctrl Pts',(91.9214587222691,17.49925882517,62.90882101338));
#135643=CARTESIAN_POINT('',(27.1339043807878,17.4992593331729,74.3325770047843));
#135644=CARTESIAN_POINT('',(91.9214587222691,17.49925882517,62.90882101338));
#135645=CARTESIAN_POINT('Ctrl Pts',(45.1145255783225,0.998148899398187,
89.1277385810842));
#135646=CARTESIAN_POINT('Ctrl Pts',(44.9976684612899,2.21249084100214,89.0454209483036));
#135647=CARTESIAN_POINT('Ctrl Pts',(44.7078984407656,3.38431261135296,88.8727869361181));
#135648=CARTESIAN_POINT('Ctrl Pts',(44.2680522680653,4.5092437997717,88.6185778110664));
#135649=CARTESIAN_POINT('Ctrl Pts',(43.828206164389,5.63417481165772,88.364368725907));
#135650=CARTESIAN_POINT('Ctrl Pts',(43.2382839566064,6.71221526059232,88.0285845542609));
#135651=CARTESIAN_POINT('Ctrl Pts',(42.5452098960251,7.71206894624626,87.6315673683517));
#135652=CARTESIAN_POINT('Ctrl Pts',(41.8521358354439,8.7119226319002,87.2345501824426));
#135653=CARTESIAN_POINT('Ctrl Pts',(41.0559099194567,9.63358955770964,86.776299979814));
#135654=CARTESIAN_POINT('Ctrl Pts',(40.183589985931,10.4852190692797,86.2627573696543));
#135655=CARTESIAN_POINT('Ctrl Pts',(39.3112700524052,11.3368485808498,85.7492147594946));
#135656=CARTESIAN_POINT('Ctrl Pts',(38.3628561006925,12.1184406783657,85.1803797401492));
#135657=CARTESIAN_POINT('Ctrl Pts',(37.3872637706894,12.8188260449958,84.57196131843));
#135658=CARTESIAN_POINT('Ctrl Pts',(36.4116714406863,13.519211411626,83.9635428967109));
#135659=CARTESIAN_POINT('Ctrl Pts',(35.4089007309014,14.1383900461859,83.3155410718192));
#135660=CARTESIAN_POINT('Ctrl Pts',(34.3926908331965,14.6910771465553,82.6100092150662));
#135661=CARTESIAN_POINT('Ctrl Pts',(33.3764809354915,15.2437642469246,81.9044773583132));
#135662=CARTESIAN_POINT('Ctrl Pts',(32.3468318509836,15.7299598132973,81.1414154690442));
#135663=CARTESIAN_POINT('Ctrl Pts',(31.3767033281954,16.1355562382722,80.3185366650299));
#135664=CARTESIAN_POINT('Ctrl Pts',(30.8916390668014,16.3383544507596,79.9070972630227));
#135665=CARTESIAN_POINT('Ctrl Pts',(30.4214549456321,16.5210028773661,79.4807036324811));
#135666=CARTESIAN_POINT('Ctrl Pts',(29.9750215051742,16.6834373562275,79.030614851117));
#135667=CARTESIAN_POINT('Ctrl Pts',(29.5285880647162,16.8458718350889,78.5805260697528));
#135668=CARTESIAN_POINT('Ctrl Pts',(29.1059053050508,16.9880923662971,78.1067421374872));
#135669=CARTESIAN_POINT('Ctrl Pts',(28.7262323167119,17.1065284396786,77.6082728149804));
#135670=CARTESIAN_POINT('Ctrl Pts',(28.3465593283731,17.2249645130601,77.1098034924735));
#135671=CARTESIAN_POINT('Ctrl Pts',(28.009896111389,17.3196161285739,76.5866487795488));
#135672=CARTESIAN_POINT('Ctrl Pts',(27.7386129171228,17.3861177803941,76.0413307805799));
#135673=CARTESIAN_POINT('Ctrl Pts',(27.4673297244896,17.452619431814,75.4960127848936));
#135674=CARTESIAN_POINT('Ctrl Pts',(27.2614265536846,17.4909711198445,74.9285315036144));
#135675=CARTESIAN_POINT('Ctrl Pts',(27.1339043807867,17.4992593326678,74.3325770047782));
#135676=CARTESIAN_POINT('Ctrl Pts',(70.0084327588244,0.99814859477146,84.7382711127335));
#135677=CARTESIAN_POINT('Ctrl Pts',(70.0408249552918,1.28828368766016,84.7079688264717));
#135678=CARTESIAN_POINT('Ctrl Pts',(70.0873703993869,1.5739891510914,84.6683487276227));
#135679=CARTESIAN_POINT('Ctrl Pts',(70.1481706976984,1.85499710789222,84.6199870557848));
#135680=CARTESIAN_POINT('Ctrl Pts',(70.1839312559019,2.02027592516656,84.5915424522448));
#135681=CARTESIAN_POINT('Ctrl Pts',(70.2246230843227,2.183930710078,84.5600737409244));
#135682=CARTESIAN_POINT('Ctrl Pts',(70.2702666820332,2.34591528311728,84.5256971778405));
#135683=CARTESIAN_POINT('Ctrl Pts',(70.3318902336131,2.56461111763809,84.4792852818769));
#135684=CARTESIAN_POINT('Ctrl Pts',(70.4025397942232,2.78026172095382,84.4275732130301));
#135685=CARTESIAN_POINT('Ctrl Pts',(70.4822652821103,2.99277020937439,84.3708440717458));
#135686=CARTESIAN_POINT('Ctrl Pts',(70.5221280260539,3.09902445358468,84.3424795011036));
#135687=CARTESIAN_POINT('Ctrl Pts',(70.5642597412934,3.20449346788007,84.3128606026717));
#135688=CARTESIAN_POINT('Ctrl Pts',(70.6086665968864,3.30916689917204,84.2820223629132));
#135689=CARTESIAN_POINT('Ctrl Pts',(70.6308700246829,3.36150361481803,84.2666032430339));
#135690=CARTESIAN_POINT('Ctrl Pts',(70.6536422374628,3.41364143458008,84.2508792872282));
#135691=CARTESIAN_POINT('Ctrl Pts',(70.6769840006127,3.46557919132123,84.2348548362182));
#135692=CARTESIAN_POINT('Ctrl Pts',(70.6886548821876,3.4915480696918,84.2268426107132));
#135693=CARTESIAN_POINT('Ctrl Pts',(70.7004681513421,3.5174669322909,84.2187552613336));
#135694=CARTESIAN_POINT('Ctrl Pts',(70.7124239035289,3.54333563686625,84.2105933294197));
#135695=CARTESIAN_POINT('Ctrl Pts',(70.7243796557158,3.5692043414416,84.2024313975057));
#135696=CARTESIAN_POINT('Ctrl Pts',(70.7359459374217,3.59390306696996,84.1945560381431));
#135697=CARTESIAN_POINT('Ctrl Pts',(70.7487187045076,3.62079113635154,84.1858843266664));
#135698=CARTESIAN_POINT('Ctrl Pts',(70.8461589156814,3.82591342042526,84.1197300319982));
#135699=CARTESIAN_POINT('Ctrl Pts',(70.9508954747235,4.02431467555368,84.0500370558852));
#135700=CARTESIAN_POINT('Ctrl Pts',(71.0630373621699,4.21603094905015,83.97742345766));
#135701=CARTESIAN_POINT('Ctrl Pts',(71.1764589010252,4.40993489750997,83.9039812654509));
#135702=CARTESIAN_POINT('Ctrl Pts',(71.2974557581051,4.5970008058511,83.8275515361351));
#135703=CARTESIAN_POINT('Ctrl Pts',(71.426133100678,4.77729687882636,83.7487307029305));
#135704=CARTESIAN_POINT('Ctrl Pts',(71.5567245337391,4.96027487692887,83.6687374006331));
#135705=CARTESIAN_POINT('Ctrl Pts',(71.695226669071,5.1362805086737,83.5862814490635));
#135706=CARTESIAN_POINT('Ctrl Pts',(71.8417413389003,5.3054110421532,83.5019403674784));
#135707=CARTESIAN_POINT('Ctrl Pts',(71.8571753661282,5.32322745099356,83.4930557789855));
#135708=CARTESIAN_POINT('Ctrl Pts',(71.8726982990893,5.34096758888549,83.4841502293356));
#135709=CARTESIAN_POINT('Ctrl Pts',(71.8883102515518,5.35863158337501,83.4752243637404));
#135710=CARTESIAN_POINT('Ctrl Pts',(71.964015424898,5.44428747862736,83.4319412315525));
#135711=CARTESIAN_POINT('Ctrl Pts',(72.0418138959197,5.52815279928536,83.3881806293742));
#135712=CARTESIAN_POINT('Ctrl Pts',(72.1217183024344,5.61024285765931,83.3440142298299));
#135713=CARTESIAN_POINT('Ctrl Pts',(72.1616705056917,5.65128788684629,83.3219310300577));
#135714=CARTESIAN_POINT('Ctrl Pts',(72.2021491862545,5.69188908667612,83.2997463436959));
#135715=CARTESIAN_POINT('Ctrl Pts',(72.2431558690364,5.73204852559375,83.2774688189602));
#135716=CARTESIAN_POINT('Ctrl Pts',(72.2776528574498,5.76583276769884,83.2587277879732));
#135717=CARTESIAN_POINT('Ctrl Pts',(72.3134065669243,5.80012927619304,83.2394514719083));
#135718=CARTESIAN_POINT('Ctrl Pts',(72.3481892195389,5.83285725628534,83.2208296824366));
#135719=CARTESIAN_POINT('Ctrl Pts',(72.354752819675,5.83903313300668,83.2173156899512));
#135720=CARTESIAN_POINT('Ctrl Pts',(72.3612818659429,5.84515320903061,83.2138251429461));
#135721=CARTESIAN_POINT('Ctrl Pts',(72.3677614219254,5.85120357486777,83.2103662245637));
#135722=CARTESIAN_POINT('Ctrl Pts',(72.5080057922845,5.98215849671336,83.1355009356496));
#135723=CARTESIAN_POINT('Ctrl Pts',(72.651975851741,6.10597780332322,83.0609436593224));
#135724=CARTESIAN_POINT('Ctrl Pts',(72.7997490509113,6.22280030375475,82.9871336398563));
#135725=CARTESIAN_POINT('Ctrl Pts',(72.9481295964232,6.34010294347164,82.9130202619629));
#135726=CARTESIAN_POINT('Ctrl Pts',(73.1003445984089,6.450351485015,82.8396602437358));
#135727=CARTESIAN_POINT('Ctrl Pts',(73.2564633129398,6.55368553317688,82.7674463558738));
#135728=CARTESIAN_POINT('Ctrl Pts',(73.4132970739346,6.65749286633834,82.6949017178815));
#135729=CARTESIAN_POINT('Ctrl Pts',(73.5740703789479,6.75432253000789,82.6235136789544));
#135730=CARTESIAN_POINT('Ctrl Pts',(73.7388443628456,6.8443102417177,82.5536289521462));
#135731=CARTESIAN_POINT('Ctrl Pts',(73.8171991831552,6.8871020151172,82.5203967325815));
#135732=CARTESIAN_POINT('Ctrl Pts',(73.8964585374665,6.92834651867607,82.4875037102065));
#135733=CARTESIAN_POINT('Ctrl Pts',(73.9766282944521,6.96805759472821,82.4549831679167));
#135734=CARTESIAN_POINT('Ctrl Pts',(74.0739145429824,7.01624710857323,82.4155193890741));
#135735=CARTESIAN_POINT('Ctrl Pts',(74.1725414662957,7.06217856006159,82.3766042630444));
#135736=CARTESIAN_POINT('Ctrl Pts',(74.2725186684865,7.10587547603901,82.3382922573529));
#135737=CARTESIAN_POINT('Ctrl Pts',(74.3225072695819,7.12772393402772,82.3191362545071));
#135738=CARTESIAN_POINT('Ctrl Pts',(74.3728334265893,7.14901372090103,82.3001309534408));
#135739=CARTESIAN_POINT('Ctrl Pts',(74.4234982485887,7.16974765838724,82.2812826440585));
#135740=CARTESIAN_POINT('Ctrl Pts',(74.4741630705881,7.19048159587344,82.2624343346763));
#135741=CARTESIAN_POINT('Ctrl Pts',(74.5265056732342,7.21117152426198,82.2432597716744));
#135742=CARTESIAN_POINT('Ctrl Pts',(74.5765097637604,7.23028458917864,82.2252146696162));
#135743=CARTESIAN_POINT('Ctrl Pts',(74.7417299164944,7.29343669276685,82.1655912570758));
#135744=CARTESIAN_POINT('Ctrl Pts',(74.907909297554,7.34990495573201,82.1085724539664));
#135745=CARTESIAN_POINT('Ctrl Pts',(75.0750870566551,7.39978443221359,82.0543596574019));
#135746=CARTESIAN_POINT('Ctrl Pts',(75.2423672067323,7.44969445826296,82.0001136572511));
#135747=CARTESIAN_POINT('Ctrl Pts',(75.41064694741,7.49300777252423,81.9486770408288));
#135748=CARTESIAN_POINT('Ctrl Pts',(75.5799570925337,7.52980013287031,81.900203892247));
#135749=CARTESIAN_POINT('Ctrl Pts',(75.7492864642117,7.56659667129038,81.851725239142));
#135750=CARTESIAN_POINT('Ctrl Pts',(75.9196464655635,7.59687088235073,81.8062106770198));
#135751=CARTESIAN_POINT('Ctrl Pts',(76.0910596620054,7.62067716530175,81.7637675037834));
#135752=CARTESIAN_POINT('Ctrl Pts',(76.2624810430379,7.64448458494867,81.7213223039819));
#135753=CARTESIAN_POINT('Ctrl Pts',(76.4349557138269,7.66182352815182,81.6819487528516));
#135754=CARTESIAN_POINT('Ctrl Pts',(76.608498094561,7.67272569012792,81.6457079514525));
#135755=CARTESIAN_POINT('Ctrl Pts',(76.7542143825673,7.68187978014144,81.6152780643441));
#135756=CARTESIAN_POINT('Ctrl Pts',(76.900683292054,7.68649538445319,81.5870560432818));
#135757=CARTESIAN_POINT('Ctrl Pts',(77.0479089573794,7.68657849705202,81.5610530932745));
#135758=CARTESIAN_POINT('Ctrl Pts',(77.223218355197,7.68667746362568,81.5300900034003));
#135759=CARTESIAN_POINT('Ctrl Pts',(77.3986015539164,7.68034817596246,81.5024518303399));
#135760=CARTESIAN_POINT('Ctrl Pts',(77.5740545830778,7.66757898161181,81.4781160564969));
#135761=CARTESIAN_POINT('Ctrl Pts',(77.7495048183896,7.65480999059312,81.4537806701678));
#135762=CARTESIAN_POINT('Ctrl Pts',(77.9250248851518,7.6356012608945,81.432747596216));
#135763=CARTESIAN_POINT('Ctrl Pts',(78.1006027241673,7.60991774884212,81.4149484435362));
#135764=CARTESIAN_POINT('Ctrl Pts',(78.2761579227927,7.58423754862415,81.3971515860195));
#135765=CARTESIAN_POINT('Ctrl Pts',(78.451770885019,7.5520841606714,81.3825878512363));
#135766=CARTESIAN_POINT('Ctrl Pts',(78.6274213983951,7.51340001043409,81.3711426086793));
#135767=CARTESIAN_POINT('Ctrl Pts',(78.7380622968593,7.48903316369782,81.3639333390033));
#135768=CARTESIAN_POINT('Ctrl Pts',(78.848717931472,7.46207469518769,81.3579604522603));
#135769=CARTESIAN_POINT('Ctrl Pts',(78.9593815684807,7.43250587062521,81.3531857594439));
#135770=CARTESIAN_POINT('Ctrl Pts',(79.0656768329959,7.4041042554856,81.3485995444087));
#135771=CARTESIAN_POINT('Ctrl Pts',(79.1719794737027,7.37329427042475,81.3451187554495));
#135772=CARTESIAN_POINT('Ctrl Pts',(79.2782823783977,7.34005658147724,81.3427030572568));
#135773=CARTESIAN_POINT('Ctrl Pts',(79.3314338307452,7.32343773700349,81.3414952081604));
#135774=CARTESIAN_POINT('Ctrl Pts',(79.3845853320286,7.30621191919041,81.3405535349978));
#135775=CARTESIAN_POINT('Ctrl Pts',(79.4377358860987,7.28837648441645,81.3398723883246));
#135776=CARTESIAN_POINT('Ctrl Pts',(79.4908864401688,7.2705410496425,81.3391912416514));
#135777=CARTESIAN_POINT('Ctrl Pts',(79.5425882552996,7.25261513739578,81.3387751495482));
#135778=CARTESIAN_POINT('Ctrl Pts',(79.5971836411002,7.233038511023,81.3386044846345));
#135779=CARTESIAN_POINT('Ctrl Pts',(79.7857856516985,7.16541024829538,81.3380149156554));
#135780=CARTESIAN_POINT('Ctrl Pts',(79.9713248235223,7.09110427453467,81.3406701687274));
#135781=CARTESIAN_POINT('Ctrl Pts',(80.1537542859587,7.01000292279281,81.3463044273957));
#135782=CARTESIAN_POINT('Ctrl Pts',(80.3358408968339,6.9290539900993,81.351928097235));
#135783=CARTESIAN_POINT('Ctrl Pts',(80.5148294890063,6.84133495666976,81.3605196602627));
#135784=CARTESIAN_POINT('Ctrl Pts',(80.6906647240559,6.74671618626887,81.3717652767044));
#135785=CARTESIAN_POINT('Ctrl Pts',(80.8657827511281,6.6524833529467,81.3829650238081));
#135786=CARTESIAN_POINT('Ctrl Pts',(81.037773103144,6.55140667405553,81.3967972758552));
#135787=CARTESIAN_POINT('Ctrl Pts',(81.2065722766861,6.4433494501232,81.4129018870683));
#135788=CARTESIAN_POINT('Ctrl Pts',(81.288338740854,6.3910064383457,81.4207029745267));
#135789=CARTESIAN_POINT('Ctrl Pts',(81.3693562799857,6.33702537853851,81.4290365004588));
#135790=CARTESIAN_POINT('Ctrl Pts',(81.4496169145499,6.28139031486415,81.4378572106945));
#135791=CARTESIAN_POINT('Ctrl Pts',(81.5461173604788,6.21449813935357,81.4484626896542));
#135792=CARTESIAN_POINT('Ctrl Pts',(81.6415236397101,6.14521489446578,81.4597726094186));
#135793=CARTESIAN_POINT('Ctrl Pts',(81.7358209135696,6.07351267745926,81.471702815685));
#135794=CARTESIAN_POINT('Ctrl Pts',(81.7829695504994,6.037661568956,81.4776679188183));
#135795=CARTESIAN_POINT('Ctrl Pts',(81.8298409215836,6.00120568493967,81.4837880113286));
#135796=CARTESIAN_POINT('Ctrl Pts',(81.8764330685024,5.96414159187196,81.4900519870319));
#135797=CARTESIAN_POINT('Ctrl Pts',(81.9177073832813,5.93130783885908,81.4956010188334));
#135798=CARTESIAN_POINT('Ctrl Pts',(81.9578519764763,5.89875352494833,81.501132511256));
#135799=CARTESIAN_POINT('Ctrl Pts',(81.9992854773298,5.86446517396627,81.5069853745834));
#135800=CARTESIAN_POINT('Ctrl Pts',(82.0046238191941,5.86004742176729,81.5077394645029));
#135801=CARTESIAN_POINT('Ctrl Pts',(82.0099835454754,5.8556008594935,81.5084988238638));
#135802=CARTESIAN_POINT('Ctrl Pts',(82.0153698185917,5.85112115822791,81.509264118107));
#135803=CARTESIAN_POINT('Ctrl Pts',(82.2015453597434,5.69628110661652,81.535716373087));
#135804=CARTESIAN_POINT('Ctrl Pts',(82.3795555066486,5.53455025116332,81.5637737486441));
#135805=CARTESIAN_POINT('Ctrl Pts',(82.5493047637065,5.36580530934802,81.5928946623141));
#135806=CARTESIAN_POINT('Ctrl Pts',(82.7225984719925,5.19353688692007,81.6226236355422));
#135807=CARTESIAN_POINT('Ctrl Pts',(82.8872827416686,5.01395787070318,81.6534612300521));
#135808=CARTESIAN_POINT('Ctrl Pts',(83.0432468258943,4.82695827935064,81.684779369301));
#135809=CARTESIAN_POINT('Ctrl Pts',(83.1992109101201,4.6399586879981,81.7160975085499));
#135810=CARTESIAN_POINT('Ctrl Pts',(83.3464548080814,4.44553800507966,81.7478961879203));
#135811=CARTESIAN_POINT('Ctrl Pts',(83.484858501528,4.24361505436675,81.7794947500919));
#135812=CARTESIAN_POINT('Ctrl Pts',(83.5535885431426,4.14334191526296,81.795186314666));
#135813=CARTESIAN_POINT('Ctrl Pts',(83.6201384227432,4.04121919074353,81.8108277155241));
#135814=CARTESIAN_POINT('Ctrl Pts',(83.6844925963318,3.93724022648501,81.8263307982717));
#135815=CARTESIAN_POINT('Ctrl Pts',(83.7166696831261,3.88525074435576,81.8340823396455));
#135816=CARTESIAN_POINT('Ctrl Pts',(83.7482978367049,3.83279719257951,81.841799263423));
#135817=CARTESIAN_POINT('Ctrl Pts',(83.7793750594448,3.77987902508754,81.8494702405201));
#135818=CARTESIAN_POINT('Ctrl Pts',(83.7949136708148,3.75341994134156,81.8533057290687));
#135819=CARTESIAN_POINT('Ctrl Pts',(83.810314549073,3.72684470306123,81.857129728667));
#135820=CARTESIAN_POINT('Ctrl Pts',(83.8255774415903,3.70015325027683,81.8609408065833));
#135821=CARTESIAN_POINT('Ctrl Pts',(83.8399802554224,3.67496588654937,81.8645371265904));
#135822=CARTESIAN_POINT('Ctrl Pts',(83.8548412394187,3.64863145971816,81.8682691271197));
#135823=CARTESIAN_POINT('Ctrl Pts',(83.8685152708665,3.62410422449756,81.8717188749887));
#135824=CARTESIAN_POINT('Ctrl Pts',(83.8693318295698,3.62263955568618,81.8719248801934));
#135825=CARTESIAN_POINT('Ctrl Pts',(83.8701441581997,3.62118133485766,81.8721298936447));
#135826=CARTESIAN_POINT('Ctrl Pts',(83.8709519074023,3.61973019242326,81.872333831851));
#135827=CARTESIAN_POINT('Ctrl Pts',(84.0183892479838,3.35485517844943,81.9095583895194));
#135828=CARTESIAN_POINT('Ctrl Pts',(84.1489902741974,3.08463837448672,81.9445913018005));
#135829=CARTESIAN_POINT('Ctrl Pts',(84.2626499120171,2.80925089465851,81.9768366642815));
#135830=CARTESIAN_POINT('Ctrl Pts',(84.3751137249479,2.53676079519157,82.0087427699451));
#135831=CARTESIAN_POINT('Ctrl Pts',(84.4709907163675,2.25920809161474,82.0379194350411));
#135832=CARTESIAN_POINT('Ctrl Pts',(84.5501771425858,1.9768081545852,82.063778299866));
#135833=CARTESIAN_POINT('Ctrl Pts',(84.6282424776673,1.69840632785724,82.0892710647727));
#135834=CARTESIAN_POINT('Ctrl Pts',(84.6900864546966,1.41529344313058,82.1115390551691));
#135835=CARTESIAN_POINT('Ctrl Pts',(84.7356084100877,1.1277261993533,82.13001137949));
#135836=CARTESIAN_POINT('Ctrl Pts',(84.7424300286744,1.08463327774595,82.1327795196071));
#135837=CARTESIAN_POINT('Ctrl Pts',(84.7488851177831,1.04144042388919,82.1354624149764));
#135838=CARTESIAN_POINT('Ctrl Pts',(84.7549733371667,0.99814860302301,82.1380581359606));
#135839=CARTESIAN_POINT('Ctrl Pts',(69.6467142128891,0.785419361948713,
84.5431073525001));
#135840=CARTESIAN_POINT('Ctrl Pts',(69.6932298573291,1.31770282807001,84.49792214893));
#135841=CARTESIAN_POINT('Ctrl Pts',(69.9015994638491,2.45488886695201,84.33269026631));
#135842=CARTESIAN_POINT('Ctrl Pts',(70.5657769153691,4.08265548317301,83.88089933277));
#135843=CARTESIAN_POINT('Ctrl Pts',(71.6147694030391,5.55740671721501,83.25266276915));
#135844=CARTESIAN_POINT('Ctrl Pts',(72.9604189620991,6.71218455213701,82.569190226542));
#135845=CARTESIAN_POINT('Ctrl Pts',(74.5029817396891,7.48371999717802,81.9471764438769));
#135846=CARTESIAN_POINT('Ctrl Pts',(76.1535633017791,7.86342804363901,81.4678565067189));
#135847=CARTESIAN_POINT('Ctrl Pts',(77.8566888949492,7.86401665948,81.167249222321));
#135848=CARTESIAN_POINT('Ctrl Pts',(79.5728282472391,7.48520878558501,81.052512962104));
#135849=CARTESIAN_POINT('Ctrl Pts',(81.2376327103791,6.71339956417001,81.1092150367));
#135850=CARTESIAN_POINT('Ctrl Pts',(82.7377717224591,5.55727078208801,81.291474417738));
#135851=CARTESIAN_POINT('Ctrl Pts',(83.9388845251391,4.08125982842501,81.523214938505));
#135852=CARTESIAN_POINT('Ctrl Pts',(84.7169256774691,2.45387688843001,81.7204854573311));
#135853=CARTESIAN_POINT('Ctrl Pts',(84.9689920528791,1.31732416127501,81.80441443773));
#135854=CARTESIAN_POINT('Ctrl Pts',(85.0281079295492,0.785594937471314,
81.830940382969));
#135855=CARTESIAN_POINT('Ctrl Pts',(69.7131001219592,0.800479551205414,
84.78138913421));
#135856=CARTESIAN_POINT('Ctrl Pts',(69.7612232582491,1.33806790374101,84.73541059712));
#135857=CARTESIAN_POINT('Ctrl Pts',(69.9756538400191,2.48539832882801,84.56741528251));
#135858=CARTESIAN_POINT('Ctrl Pts',(70.6537549411791,4.11873126524301,84.10990240609));
#135859=CARTESIAN_POINT('Ctrl Pts',(71.7147266250591,5.58568200595701,83.47782034655));
#135860=CARTESIAN_POINT('Ctrl Pts',(73.0616884062191,6.72241378017701,82.795461872428));
#135861=CARTESIAN_POINT('Ctrl Pts',(74.5902699815791,7.47385793838302,82.179480822702));
#135862=CARTESIAN_POINT('Ctrl Pts',(76.2132276098791,7.84057298012902,81.708053004936));
#135863=CARTESIAN_POINT('Ctrl Pts',(77.8828743052091,7.84113956683401,81.413354483289));
#135864=CARTESIAN_POINT('Ctrl Pts',(79.5703075102091,7.47530120987402,81.300662572887));
#135865=CARTESIAN_POINT('Ctrl Pts',(81.2198565698392,6.72360904533501,81.356479029792));
#135866=CARTESIAN_POINT('Ctrl Pts',(82.7208490445491,5.58555316282103,81.537239976425));
#135867=CARTESIAN_POINT('Ctrl Pts',(83.9345496642491,4.11733640075101,81.76849788775));
#135868=CARTESIAN_POINT('Ctrl Pts',(84.7276253707291,2.48437788623201,81.966383439229));
#135869=CARTESIAN_POINT('Ctrl Pts',(84.9863259944791,1.33768534536301,82.050835901607));
#135870=CARTESIAN_POINT('Ctrl Pts',(85.0472221659491,0.800656874293014,
82.0775572867141));
#135871=CARTESIAN_POINT('Ctrl Pts',(69.9501060829392,0.786177546583314,
84.852354313));
#135872=CARTESIAN_POINT('Ctrl Pts',(69.9975371008791,1.31184806627701,84.80626783169));
#135873=CARTESIAN_POINT('Ctrl Pts',(70.2085206123191,2.43317701879001,84.63811593324));
#135874=CARTESIAN_POINT('Ctrl Pts',(70.873528140399,4.02522621269901,84.18143831868));
#135875=CARTESIAN_POINT('Ctrl Pts',(71.9096656973891,5.44894304416801,83.55295341525));
#135876=CARTESIAN_POINT('Ctrl Pts',(73.2189510831691,6.54640141231401,82.8778451648939));
#135877=CARTESIAN_POINT('Ctrl Pts',(74.6980547553291,7.26795848633102,82.272197496043));
#135878=CARTESIAN_POINT('Ctrl Pts',(76.2631781069791,7.61855497908201,81.812330154294));
#135879=CARTESIAN_POINT('Ctrl Pts',(77.8717848917391,7.61909572214601,81.528397109963));
#135880=CARTESIAN_POINT('Ctrl Pts',(79.5008623467592,7.26934102286101,81.4246339445011));
#135881=CARTESIAN_POINT('Ctrl Pts',(81.1002916501491,6.54755501071102,81.487675127427));
#135882=CARTESIAN_POINT('Ctrl Pts',(82.5633528474692,5.44882107944701,81.67451639658));
#135883=CARTESIAN_POINT('Ctrl Pts',(83.7524812891091,4.02386927061101,81.910890495113));
#135884=CARTESIAN_POINT('Ctrl Pts',(84.5329796997091,2.43217997060401,82.112466891796));
#135885=CARTESIAN_POINT('Ctrl Pts',(84.7884979941891,1.31147393282401,82.198244230732));
#135886=CARTESIAN_POINT('Ctrl Pts',(84.8487811433091,0.786350937502314,
82.225303450051));
#135887=CARTESIAN_POINT('Ctrl Pts',(70.1340181617991,0.756013252073015,
84.68901765668));
#135888=CARTESIAN_POINT('Ctrl Pts',(70.1791107533991,1.26379266360201,84.64361051084));
#135889=CARTESIAN_POINT('Ctrl Pts',(70.3803928968891,2.34751751437501,84.4780566788099));
#135890=CARTESIAN_POINT('Ctrl Pts',(71.0176488742091,3.89040132568301,84.0279831130701));
#135891=CARTESIAN_POINT('Ctrl Pts',(72.0155803335091,5.27626004995501,83.40714260132));
#135892=CARTESIAN_POINT('Ctrl Pts',(73.283764093069,6.35028849871101,82.7385771211889));
#135893=CARTESIAN_POINT('Ctrl Pts',(74.7245961904991,7.06037361530101,82.1378096282151));
#135894=CARTESIAN_POINT('Ctrl Pts',(76.2562656742691,7.40694058571701,81.6822589903259));
#135895=CARTESIAN_POINT('Ctrl Pts',(77.833888139419,7.40747606488501,81.4037864218081));
#135896=CARTESIAN_POINT('Ctrl Pts',(79.4300432208991,7.06173752758101,81.3074084030879));
#135897=CARTESIAN_POINT('Ctrl Pts',(80.9917973006791,6.35141784042201,81.3789651146941));
#135898=CARTESIAN_POINT('Ctrl Pts',(82.413946454709,5.27613825742201,81.5737261440561));
#135899=CARTESIAN_POINT('Ctrl Pts',(83.5645368175391,3.88908364255101,81.815985970834));
#135900=CARTESIAN_POINT('Ctrl Pts',(84.3167180044791,2.34655363670601,82.020845174075));
#135901=CARTESIAN_POINT('Ctrl Pts',(84.5622412464891,1.26343131915301,82.107498210764));
#135902=CARTESIAN_POINT('Ctrl Pts',(84.6200966982691,0.756180742730514,
82.134718771215));
#135903=CARTESIAN_POINT('Ctrl Pts',(70.3179302406591,0.725848957562814,
84.52568100036));
#135904=CARTESIAN_POINT('Ctrl Pts',(70.3606844059291,1.21573726092701,84.4809531899901));
#135905=CARTESIAN_POINT('Ctrl Pts',(70.5522651814691,2.26185800996101,84.31799742439));
#135906=CARTESIAN_POINT('Ctrl Pts',(71.1617696080291,3.75557643866701,83.87452790746));
#135907=CARTESIAN_POINT('Ctrl Pts',(72.1214949696291,5.10357705574302,83.26133178739));
#135908=CARTESIAN_POINT('Ctrl Pts',(73.3485771029692,6.15417558510801,82.599309077484));
#135909=CARTESIAN_POINT('Ctrl Pts',(74.7511376256591,6.85278874427201,82.0034217603881));
#135910=CARTESIAN_POINT('Ctrl Pts',(76.2493532415691,7.19532619235201,81.552187826359));
#135911=CARTESIAN_POINT('Ctrl Pts',(77.7959913870991,7.19585640762402,81.279175733652));
#135912=CARTESIAN_POINT('Ctrl Pts',(79.3592240950391,6.85413403230101,81.1901828616749));
#135913=CARTESIAN_POINT('Ctrl Pts',(80.8833029512191,6.15528067013201,81.27025510196));
#135914=CARTESIAN_POINT('Ctrl Pts',(82.2645400619392,5.10345543539701,81.472935891533));
#135915=CARTESIAN_POINT('Ctrl Pts',(83.3765923459791,3.75429801449001,81.721081446555));
#135916=CARTESIAN_POINT('Ctrl Pts',(84.1004563092491,2.26092730280701,81.929223456353));
#135917=CARTESIAN_POINT('Ctrl Pts',(84.3359844987991,1.21538870548301,82.016752190797));
#135918=CARTESIAN_POINT('Ctrl Pts',(84.3914122532191,0.726010547958614,
82.044134092379));
#135919=CARTESIAN_POINT('Ctrl Pts',(70.2751507164491,0.708294960791114,
84.2822187406399));
#135920=CARTESIAN_POINT('Ctrl Pts',(70.3161274275591,1.19120660018001,84.23831630919));
#135921=CARTESIAN_POINT('Ctrl Pts',(70.5009098227891,2.22361576577601,84.07826090145));
#135922=CARTESIAN_POINT('Ctrl Pts',(71.0941998788891,3.70669520774501,83.6409305469399));
#135923=CARTESIAN_POINT('Ctrl Pts',(72.0384105536192,5.057948427186,83.03221038356));
#135924=CARTESIAN_POINT('Ctrl Pts',(73.2597623498791,6.12307642092401,82.369847158899));
#135925=CARTESIAN_POINT('Ctrl Pts',(74.6713828128091,6.83946132401601,81.768780332156));
#135926=CARTESIAN_POINT('Ctrl Pts',(76.192102641159,7.19386181068701,81.310544720065));
#135927=CARTESIAN_POINT('Ctrl Pts',(77.7670586812291,7.19441231048701,81.032533866219));
#135928=CARTESIAN_POINT('Ctrl Pts',(79.3538783771191,6.84084767825001,80.942411577904));
#135929=CARTESIAN_POINT('Ctrl Pts',(80.8882888229391,6.12419755563401,81.024252198021));
#135930=CARTESIAN_POINT('Ctrl Pts',(82.2642506938791,5.05782011026801,81.2292165899171));
#135931=CARTESIAN_POINT('Ctrl Pts',(83.3601757425891,3.70542032188201,81.47846177581));
#135932=CARTESIAN_POINT('Ctrl Pts',(84.0667116606391,2.22269669503301,81.686379856903));
#135933=CARTESIAN_POINT('Ctrl Pts',(84.2948665735391,1.19086312606301,81.773508524379));
#135934=CARTESIAN_POINT('Ctrl Pts',(84.3483435002091,0.708454252188914,
81.80072298139));
#135935=CARTESIAN_POINT('Ctrl Pts',(70.0460599054191,0.719920776125714,
84.18843902109));
#135936=CARTESIAN_POINT('Ctrl Pts',(70.0874979035891,1.21335558682101,84.1447289228899));
#135937=CARTESIAN_POINT('Ctrl Pts',(70.2748020122591,2.26888828273301,83.98513846763));
#135938=CARTESIAN_POINT('Ctrl Pts',(70.8787198966591,3.78989745330101,83.5476875299399));
#135939=CARTESIAN_POINT('Ctrl Pts',(71.8447518705991,5.18244379829901,82.936049957039));
#135940=CARTESIAN_POINT('Ctrl Pts',(73.1011535809691,6.28634603308001,82.266784350285));
#135941=CARTESIAN_POINT('Ctrl Pts',(74.5606136683391,7.03297133186201,81.655367355105));
#135942=CARTESIAN_POINT('Ctrl Pts',(76.1385536828191,7.40392969533601,81.1854206853431));
#135943=CARTESIAN_POINT('Ctrl Pts',(77.774400092089,7.40450688118101,80.8966702485669));
#135944=CARTESIAN_POINT('Ctrl Pts',(79.419051980679,7.03441967967101,80.797970056011));
#135945=CARTESIAN_POINT('Ctrl Pts',(81.0020486672191,6.28750837427602,80.873162703487));
#135946=CARTESIAN_POINT('Ctrl Pts',(82.4133514899292,5.18230823705901,81.0726190089751));
#135947=CARTESIAN_POINT('Ctrl Pts',(83.530782916899,3.78858704523601,81.3171397681949));
#135948=CARTESIAN_POINT('Ctrl Pts',(84.247336203049,2.26794833049001,81.5215385554099));
#135949=CARTESIAN_POINT('Ctrl Pts',(84.477699375629,1.21300469000201,81.6073690211719));
#135950=CARTESIAN_POINT('Ctrl Pts',(84.5315437634291,0.720083539852114,
81.6342453016709));
#135951=CARTESIAN_POINT('Origin',(69.9560096372196,0.973231869956287,84.4436697031834));
#135952=CARTESIAN_POINT('Ctrl Pts',(69.9410902066692,-0.0200749179659658,
84.7920798508299));
#135953=CARTESIAN_POINT('Ctrl Pts',(69.9410243575191,0.00807640976446622,
84.7921397125799));
#135954=CARTESIAN_POINT('Ctrl Pts',(69.9416531080391,0.254907774005214,
84.7915720445599));
#135955=CARTESIAN_POINT('Ctrl Pts',(69.9574697196891,0.602587781192914,
84.7772449914899));
#135956=CARTESIAN_POINT('Ctrl Pts',(69.9895755752191,0.919382073654714,
84.7482586599001));
#135957=CARTESIAN_POINT('Ctrl Pts',(70.0014582496291,1.01916091177701,84.7375477247));
#135958=CARTESIAN_POINT('Ctrl Pts',(70.1256916253091,-0.0196065190321158,
84.7675386824));
#135959=CARTESIAN_POINT('Ctrl Pts',(70.1256274227291,0.00788796798874821,
84.7675982874601));
#135960=CARTESIAN_POINT('Ctrl Pts',(70.1262404858491,0.248960167223414,
84.76703309691));
#135961=CARTESIAN_POINT('Ctrl Pts',(70.1416623917691,0.588526916119514,
84.75276801805));
#135962=CARTESIAN_POINT('Ctrl Pts',(70.1729656463091,0.897915264457314,
84.72390818689));
#135963=CARTESIAN_POINT('Ctrl Pts',(70.1845510765691,0.995359642174814,
84.71324418904));
#135964=CARTESIAN_POINT('Ctrl Pts',(70.2333228313691,-0.0190451304001758,
84.6155670875601));
#135965=CARTESIAN_POINT('Ctrl Pts',(70.2332613314891,0.00766210207465321,
84.61562565729));
#135966=CARTESIAN_POINT('Ctrl Pts',(70.2338484032691,0.241831420262514,
84.61506984276));
#135967=CARTESIAN_POINT('Ctrl Pts',(70.2486158835091,0.571683637382613,
84.60104674069));
#135968=CARTESIAN_POINT('Ctrl Pts',(70.2786051836591,0.872330962898515,
84.57266800438));
#135969=CARTESIAN_POINT('Ctrl Pts',(70.2897064325991,0.967037502858313,
84.56218029236));
#135970=CARTESIAN_POINT('Ctrl Pts',(70.1952002761691,-0.0187495170019758,
84.43328509289));
#135971=CARTESIAN_POINT('Ctrl Pts',(70.1951408079091,0.00754315546745622,
84.4333425102999));
#135972=CARTESIAN_POINT('Ctrl Pts',(70.1957081946091,0.238077279840414,
84.4327969784399));
#135973=CARTESIAN_POINT('Ctrl Pts',(70.2099797510591,0.562821928084014,
84.4190412163801));
#135974=CARTESIAN_POINT('Ctrl Pts',(70.2389834482391,0.858979251046915,
84.39119071749));
#135975=CARTESIAN_POINT('Ctrl Pts',(70.2497230029891,0.952294237575714,
84.3808959813399));
#135976=CARTESIAN_POINT('Origin',(69.9015319855191,-1.31377662151953E-8,
84.4947179233));
#135977=CARTESIAN_POINT('Ctrl Pts',(69.7564804663291,-1.18130795621199,
84.6242643184));
#135978=CARTESIAN_POINT('Ctrl Pts',(69.7401068344391,-1.05954295648899,
84.63874639282));
#135979=CARTESIAN_POINT('Ctrl Pts',(69.7030507545791,-0.732436278044086,
84.67159393454));
#135980=CARTESIAN_POINT('Ctrl Pts',(69.6774028986991,-0.282494314856486,
84.69441260833));
#135981=CARTESIAN_POINT('Ctrl Pts',(69.6768465603291,0.0447208421045242,
84.6949039456));
#135982=CARTESIAN_POINT('Ctrl Pts',(69.6790678296691,0.164690824891014,
84.6929285177001));
#135983=CARTESIAN_POINT('Ctrl Pts',(69.8967461732791,-1.18166250822699,
84.77938870072));
#135984=CARTESIAN_POINT('Ctrl Pts',(69.8801437431891,-1.05993924015199,
84.79407745808));
#135985=CARTESIAN_POINT('Ctrl Pts',(69.8425571861291,-0.732848144525486,
84.8274028272));
#135986=CARTESIAN_POINT('Ctrl Pts',(69.8165254859392,-0.282676461232986,
84.85056404238));
#135987=CARTESIAN_POINT('Ctrl Pts',(69.8159607204191,0.0447499039312942,
84.85106211981));
#135988=CARTESIAN_POINT('Ctrl Pts',(69.8182151861391,0.164792365768414,
84.84905716968));
#135989=CARTESIAN_POINT('Ctrl Pts',(70.1035892209992,-1.15296456351699,
84.76796001164));
#135990=CARTESIAN_POINT('Ctrl Pts',(70.0873962121891,-1.03421196443699,
84.78259973814));
#135991=CARTESIAN_POINT('Ctrl Pts',(70.0507344739592,-0.715085683656586,
84.81581554535));
#135992=CARTESIAN_POINT('Ctrl Pts',(70.0253405075491,-0.275829379908586,
84.8389025823201));
#135993=CARTESIAN_POINT('Ctrl Pts',(70.0247895466191,0.0436659991401842,
84.8393989572201));
#135994=CARTESIAN_POINT('Ctrl Pts',(70.0269887758291,0.160799851340314,
84.8374004511201));
#135995=CARTESIAN_POINT('Ctrl Pts',(70.2208705491191,-1.11687726314599,
84.5986053952399));
#135996=CARTESIAN_POINT('Ctrl Pts',(70.2054161223391,-1.00178180941899,
84.6129773888799));
#135997=CARTESIAN_POINT('Ctrl Pts',(70.1704363834391,-0.692557196949986,
84.64557894957));
#135998=CARTESIAN_POINT('Ctrl Pts',(70.1462203244891,-0.267121708920386,
84.66823108342));
#135999=CARTESIAN_POINT('Ctrl Pts',(70.1456949792692,0.0422873320530842,
84.6687185983001));
#136000=CARTESIAN_POINT('Ctrl Pts',(70.1477922353091,0.155727100336014,
84.66675763812));
#136001=CARTESIAN_POINT('Ctrl Pts',(70.3381518772391,-1.08078996277499,
84.42925077884));
#136002=CARTESIAN_POINT('Ctrl Pts',(70.3234360324891,-0.969351654400286,
84.4433550396201));
#136003=CARTESIAN_POINT('Ctrl Pts',(70.2901382929191,-0.670028710243386,
84.47534235379));
#136004=CARTESIAN_POINT('Ctrl Pts',(70.2671001414291,-0.258414037932286,
84.49755958453));
#136005=CARTESIAN_POINT('Ctrl Pts',(70.2666004119091,0.0409086649659842,
84.49803823939));
#136006=CARTESIAN_POINT('Ctrl Pts',(70.2685956947891,0.150654349331714,
84.49611482512));
#136007=CARTESIAN_POINT('Ctrl Pts',(70.2773396420792,-1.06455443102999,
84.2298105032));
#136008=CARTESIAN_POINT('Ctrl Pts',(70.2631340086391,-0.954699084796287,
84.24363043191));
#136009=CARTESIAN_POINT('Ctrl Pts',(70.2310057625491,-0.659740216438386,
84.27496248958));
#136010=CARTESIAN_POINT('Ctrl Pts',(70.2087965283391,-0.254418913679886,
84.29671238647));
#136011=CARTESIAN_POINT('Ctrl Pts',(70.2083148891791,0.0402759463338542,
84.29718171195));
#136012=CARTESIAN_POINT('Ctrl Pts',(70.2102384384591,0.148330615786914,
84.29529860328));
#136013=CARTESIAN_POINT('Ctrl Pts',(70.0843390135691,-1.08042634050399,
84.15083551784));
#136014=CARTESIAN_POINT('Ctrl Pts',(70.0700300788791,-0.968884846785787,
84.16456914826));
#136015=CARTESIAN_POINT('Ctrl Pts',(70.0376760079891,-0.669458163442587,
84.19569957119));
#136016=CARTESIAN_POINT('Ctrl Pts',(70.0153209782991,-0.258152124963886,
84.21730247854));
#136017=CARTESIAN_POINT('Ctrl Pts',(70.0148362483192,0.0408667947848142,
84.2177690477299));
#136018=CARTESIAN_POINT('Ctrl Pts',(70.0167724529091,0.150510010251614,
84.21589857897));
#136019=CARTESIAN_POINT('Origin',(69.9565232205078,-0.973190806778888,84.4438203202395));
#136020=CARTESIAN_POINT('Ctrl Pts',(84.8366580532091,0.0200750409221942,
82.165589037612));
#136021=CARTESIAN_POINT('Ctrl Pts',(84.836751259439,-0.0117694511617658,
82.165627235365));
#136022=CARTESIAN_POINT('Ctrl Pts',(84.8357393583291,-0.266091686437686,
82.165216682068));
#136023=CARTESIAN_POINT('Ctrl Pts',(84.8151322061391,-0.613726406334186,
82.156819280891));
#136024=CARTESIAN_POINT('Ctrl Pts',(84.775011662459,-0.926769367276586,
82.140549742704));
#136025=CARTESIAN_POINT('Ctrl Pts',(84.7612796644692,-1.01916123813399,
82.134992792959));
#136026=CARTESIAN_POINT('Ctrl Pts',(84.6547958874591,0.0196066388531642,
82.205665345244));
#136027=CARTESIAN_POINT('Ctrl Pts',(84.6548872431291,-0.0114948418582758,
82.2057039075881));
#136028=CARTESIAN_POINT('Ctrl Pts',(84.6538954366891,-0.259883136404086,
82.205289437392));
#136029=CARTESIAN_POINT('Ctrl Pts',(84.6336971379591,-0.599405443717186,
82.1968119957));
#136030=CARTESIAN_POINT('Ctrl Pts',(84.5943748685691,-0.905129725272486,
82.1803866832581));
#136031=CARTESIAN_POINT('Ctrl Pts',(84.5809163839991,-0.995359963007886,
82.174776434602));
#136032=CARTESIAN_POINT('Ctrl Pts',(84.5016782566291,0.0190452493532842,
82.099670842561));
#136033=CARTESIAN_POINT('Ctrl Pts',(84.5017663374991,-0.0111656970980658,
82.099709346569));
#136034=CARTESIAN_POINT('Ctrl Pts',(84.5008101478991,-0.252441591377686,
82.099294800995));
#136035=CARTESIAN_POINT('Ctrl Pts',(84.4813393368691,-0.582252377763186,
82.090821072537));
#136036=CARTESIAN_POINT('Ctrl Pts',(84.4434170859791,-0.879342716401286,
82.074398259715));
#136037=CARTESIAN_POINT('Ctrl Pts',(84.4304357389791,-0.967037815738486,
82.0687880860861));
#136038=CARTESIAN_POINT('Ctrl Pts',(84.4751575973991,0.0187496379689842,
81.915343126508));
#136039=CARTESIAN_POINT('Ctrl Pts',(84.475243072029,-0.0109923624607558,
81.915381186535));
#136040=CARTESIAN_POINT('Ctrl Pts',(84.474315259909,-0.248522697782586,
81.914970455274));
#136041=CARTESIAN_POINT('Ctrl Pts',(84.4554256573791,-0.573229168182786,
81.906581820792));
#136042=CARTESIAN_POINT('Ctrl Pts',(84.418610463479,-0.865887969031586,
81.89031818404));
#136043=CARTESIAN_POINT('Ctrl Pts',(84.4060049552891,-0.952294548179087,
81.884761411431));
#136044=CARTESIAN_POINT('Origin',(84.703419321545,-0.973227037640828,81.8433412100757));
#136045=CARTESIAN_POINT('Ctrl Pts',(85.0281338392691,-0.785442429272785,
81.830954919499));
#136046=CARTESIAN_POINT('Ctrl Pts',(84.9678505702292,-1.32789691945799,
81.803904430336));
#136047=CARTESIAN_POINT('Ctrl Pts',(84.7111038549791,-2.47360497699299,
81.718691486301));
#136048=CARTESIAN_POINT('Ctrl Pts',(83.9232885536391,-4.10503857870399,
81.519756430079));
#136049=CARTESIAN_POINT('Ctrl Pts',(82.7216600039292,-5.57202437394999,
81.2890121320651));
#136050=CARTESIAN_POINT('Ctrl Pts',(81.226056711349,-6.71948616520598,81.108544375771));
#136051=CARTESIAN_POINT('Ctrl Pts',(79.569064807179,-7.48586908240599,81.052830407459));
#136052=CARTESIAN_POINT('Ctrl Pts',(77.8597106364491,-7.86330763548499,
81.1670786168599));
#136053=CARTESIAN_POINT('Ctrl Pts',(76.1616397228791,-7.86398436055798,
81.46614911781));
#136054=CARTESIAN_POINT('Ctrl Pts',(74.5148178179191,-7.48758304592898,
81.9432097462369));
#136055=CARTESIAN_POINT('Ctrl Pts',(72.9741081702291,-6.72095167631398,
82.5630023793679));
#136056=CARTESIAN_POINT('Ctrl Pts',(71.6285374682991,-5.57206334237799,
83.2450686800099));
#136057=CARTESIAN_POINT('Ctrl Pts',(70.5777712225591,-4.10373939010499,
83.8732652363599));
#136058=CARTESIAN_POINT('Ctrl Pts',(69.9060018891791,-2.47264156110999,
84.3293618700599));
#136059=CARTESIAN_POINT('Ctrl Pts',(69.6940862081691,-1.32753454776999,
84.49710121691));
#136060=CARTESIAN_POINT('Ctrl Pts',(69.6467257282991,-0.785616277860386,
84.5431000349299));
#136061=CARTESIAN_POINT('Ctrl Pts',(85.0472461895191,-0.800502691495985,
82.0775712267681));
#136062=CARTESIAN_POINT('Ctrl Pts',(84.9851471753292,-1.34836358114699,
82.050322866006));
#136063=CARTESIAN_POINT('Ctrl Pts',(84.7216504272292,-2.50426266210099,
81.964575828032));
#136064=CARTESIAN_POINT('Ctrl Pts',(83.9187195090792,-4.14108424026399,
81.7650369409531));
#136065=CARTESIAN_POINT('Ctrl Pts',(82.7046613300891,-5.60012874920398,
81.534791048907));
#136066=CARTESIAN_POINT('Ctrl Pts',(81.2083600665691,-6.72954445694999,
81.355816937138));
#136067=CARTESIAN_POINT('Ctrl Pts',(79.5666132765091,-7.47593236707499,
81.300973241494));
#136068=CARTESIAN_POINT('Ctrl Pts',(77.8858425823791,-7.84045426776599,
81.413185255052));
#136069=CARTESIAN_POINT('Ctrl Pts',(76.2211447682492,-7.84110567342098,
81.706377531878));
#136070=CARTESIAN_POINT('Ctrl Pts',(74.6019362569691,-7.47759387726698,
82.1755699227481));
#136071=CARTESIAN_POINT('Ctrl Pts',(73.0753129150491,-6.73098529397899,
82.7893114006941));
#136072=CARTESIAN_POINT('Ctrl Pts',(71.7285752976792,-5.60017339364298,
83.4702096729801));
#136073=CARTESIAN_POINT('Ctrl Pts',(70.6659436097491,-4.13978608838599,
84.1021953465));
#136074=CARTESIAN_POINT('Ctrl Pts',(69.9801822737691,-2.50329122298799,
84.5640276126));
#136075=CARTESIAN_POINT('Ctrl Pts',(69.7621119598991,-1.34799747674499,
84.73457509318));
#136076=CARTESIAN_POINT('Ctrl Pts',(69.7131142654991,-0.800678270688187,
84.7813801232101));
#136077=CARTESIAN_POINT('Ctrl Pts',(84.8488051384291,-0.786200190774086,
82.225315821893));
#136078=CARTESIAN_POINT('Ctrl Pts',(84.7873311119291,-1.32191566921299,
82.1977236032581));
#136079=CARTESIAN_POINT('Ctrl Pts',(84.5270803868991,-2.45160526767999,
82.1106264707551));
#136080=CARTESIAN_POINT('Ctrl Pts',(83.7369373580592,-4.04696374136098,
81.907358225748));
#136081=CARTESIAN_POINT('Ctrl Pts',(82.5475410294591,-5.46291975204299,
81.672000048526));
#136082=CARTESIAN_POINT('Ctrl Pts',(81.0891311949791,-6.55325925884998,
81.486962840279));
#136083=CARTESIAN_POINT('Ctrl Pts',(79.4972997300592,-7.26994271334799,
81.424922709271));
#136084=CARTESIAN_POINT('Ctrl Pts',(77.8746492819691,-7.61844194255998,
81.528241411345));
#136085=CARTESIAN_POINT('Ctrl Pts',(76.2708038416291,-7.619063639597,81.810706638627));
#136086=CARTESIAN_POINT('Ctrl Pts',(74.7093158197091,-7.27153427949499,
82.268368564623));
#136087=CARTESIAN_POINT('Ctrl Pts',(73.2321591228391,-6.55464945045899,
82.87177871305));
#136088=CARTESIAN_POINT('Ctrl Pts',(71.9231550752991,-5.46296592454899,
83.54540390462));
#136089=CARTESIAN_POINT('Ctrl Pts',(70.8854551199492,-4.04570102716299,
84.1737588213101));
#136090=CARTESIAN_POINT('Ctrl Pts',(70.2129742283391,-2.45065611591499,
84.63472359839));
#136091=CARTESIAN_POINT('Ctrl Pts',(69.9984125344692,-1.32155762322899,
84.8054295158));
#136092=CARTESIAN_POINT('Ctrl Pts',(69.9501192544392,-0.786371876604886,
84.8523437644201));
#136093=CARTESIAN_POINT('Ctrl Pts',(84.6201212081591,-0.756035202698286,
82.134731082037));
#136094=CARTESIAN_POINT('Ctrl Pts',(84.5611229699591,-1.27351763615699,
82.1069735901909));
#136095=CARTESIAN_POINT('Ctrl Pts',(84.3110503697891,-2.36533664275899,
82.018984730497));
#136096=CARTESIAN_POINT('Ctrl Pts',(83.5495281178791,-3.91151837616499,
81.8123817792899));
#136097=CARTESIAN_POINT('Ctrl Pts',(82.398606548459,-5.28991034745799,81.5711261636109));
#136098=CARTESIAN_POINT('Ctrl Pts',(80.980911438569,-6.35702795855899,81.378192136185));
#136099=CARTESIAN_POINT('Ctrl Pts',(79.4265499277991,-7.06233584602099,
81.30768165016));
#136100=CARTESIAN_POINT('Ctrl Pts',(77.8366962050891,-7.40683034689099,
81.403644412078));
#136101=CARTESIAN_POINT('Ctrl Pts',(76.2637432396491,-7.40744598837599,
81.6806591353349));
#136102=CARTESIAN_POINT('Ctrl Pts',(74.7355998470391,-7.06390599830199,
82.1340120919569));
#136103=CARTESIAN_POINT('Ctrl Pts',(73.2965980661991,-6.35838933813399,
82.732562583319));
#136104=CARTESIAN_POINT('Ctrl Pts',(72.0286109742291,-5.28995245772899,
83.3996747765199));
#136105=CARTESIAN_POINT('Ctrl Pts',(71.0291066107991,-3.91029205061899,
84.0204061706));
#136106=CARTESIAN_POINT('Ctrl Pts',(70.3846430642991,-2.36441905166499,
84.47471916893));
#136107=CARTESIAN_POINT('Ctrl Pts',(70.1799414212691,-1.27317183330099,
84.6427842761299));
#136108=CARTESIAN_POINT('Ctrl Pts',(70.1340292806191,-0.756201046184986,
84.6890076573999));
#136109=CARTESIAN_POINT('Ctrl Pts',(84.3914372778792,-0.725870214622486,
82.044146342181));
#136110=CARTESIAN_POINT('Ctrl Pts',(84.3349148279891,-1.22511960310099,
82.016223577123));
#136111=CARTESIAN_POINT('Ctrl Pts',(84.0950203526892,-2.27906801783799,
81.92734299024));
#136112=CARTESIAN_POINT('Ctrl Pts',(83.3621188776991,-3.77607301096799,
81.717405332832));
#136113=CARTESIAN_POINT('Ctrl Pts',(82.2496720674591,-5.11690094287299,
81.470252278697));
#136114=CARTESIAN_POINT('Ctrl Pts',(80.8726916821591,-6.16079665826698,
81.26942143209));
#136115=CARTESIAN_POINT('Ctrl Pts',(79.3558001255291,-6.85472897869398,
81.1904405910481));
#136116=CARTESIAN_POINT('Ctrl Pts',(77.7987431282091,-7.19521875122099,
81.2790474128101));
#136117=CARTESIAN_POINT('Ctrl Pts',(76.2566826376691,-7.19582833715499,
81.5506116320421));
#136118=CARTESIAN_POINT('Ctrl Pts',(74.7618838743691,-6.85627771710999,
81.999655619291));
#136119=CARTESIAN_POINT('Ctrl Pts',(73.361037009559,-6.162129225809,82.5933464535881));
#136120=CARTESIAN_POINT('Ctrl Pts',(72.1340668731491,-5.11693899090998,
83.2539456484301));
#136121=CARTESIAN_POINT('Ctrl Pts',(71.1727581016391,-3.77488307407499,
83.86705351989));
#136122=CARTESIAN_POINT('Ctrl Pts',(70.5563119002591,-2.27818198741599,
84.31471473947));
#136123=CARTESIAN_POINT('Ctrl Pts',(70.3614703080691,-1.22478604337199,
84.48013903646));
#136124=CARTESIAN_POINT('Ctrl Pts',(70.3179393067991,-0.726030215765186,
84.52567155037));
#136125=CARTESIAN_POINT('Ctrl Pts',(84.3483675511692,-0.708315777590186,
81.800736122662));
#136126=CARTESIAN_POINT('Ctrl Pts',(84.2938347685092,-1.20045484352899,
81.772982672117));
#136127=CARTESIAN_POINT('Ctrl Pts',(84.0614432845091,-2.24061799304199,
81.6845104357261));
#136128=CARTESIAN_POINT('Ctrl Pts',(83.3459800322391,-3.72715103435799,
81.474780386873));
#136129=CARTESIAN_POINT('Ctrl Pts',(82.2495041742791,-5.07139646376999,
81.2265113930151));
#136130=CARTESIAN_POINT('Ctrl Pts',(80.8776307673491,-6.12984397173298,
81.0234038922981));
#136131=CARTESIAN_POINT('Ctrl Pts',(79.3503955238792,-6.84146712689498,
80.942674030654));
#136132=CARTESIAN_POINT('Ctrl Pts',(77.7698545693192,-7.193750217943,81.032405630159));
#136133=CARTESIAN_POINT('Ctrl Pts',(76.1995669341991,-7.19438311728998,
81.3089406769521));
#136134=CARTESIAN_POINT('Ctrl Pts',(74.6822626061291,-6.84306319438998,
81.764964470253));
#136135=CARTESIAN_POINT('Ctrl Pts',(73.2722441158392,-6.13119675659699,
82.363854399566));
#136136=CARTESIAN_POINT('Ctrl Pts',(72.0508580000791,-5.07142869365499,
83.0248483636501));
#136137=CARTESIAN_POINT('Ctrl Pts',(71.1049554729691,-3.72596408947099,
83.63353586708));
#136138=CARTESIAN_POINT('Ctrl Pts',(70.5048176610391,-2.23974300617899,
84.0750396996601));
#136139=CARTESIAN_POINT('Ctrl Pts',(70.3168805484591,-1.20012615522599,
84.23751662696));
#136140=CARTESIAN_POINT('Ctrl Pts',(70.2751598299691,-0.708473502053986,
84.28221030427));
#136141=CARTESIAN_POINT('Ctrl Pts',(84.531565980199,-0.719941702880786,
81.6342578001199));
#136142=CARTESIAN_POINT('Ctrl Pts',(84.4766586765791,-1.22280467433099,
81.6068484341241));
#136143=CARTESIAN_POINT('Ctrl Pts',(84.2420129006891,-2.28627993701699,
81.519699179736));
#136144=CARTESIAN_POINT('Ctrl Pts',(83.5163452015191,-3.81093039657899,
81.31352309037));
#136145=CARTESIAN_POINT('Ctrl Pts',(82.398261345009,-5.19634904981199,81.0699730023531));
#136146=CARTESIAN_POINT('Ctrl Pts',(80.9910666415091,-6.29338645392199,
80.872357969515));
#136147=CARTESIAN_POINT('Ctrl Pts',(79.4154375811891,-7.03506828713499,
80.7982513399819));
#136148=CARTESIAN_POINT('Ctrl Pts',(77.7772987323591,-7.40381091052299,
80.896526746002));
#136149=CARTESIAN_POINT('Ctrl Pts',(76.1463082214191,-7.40447448647799,
81.183761937356));
#136150=CARTESIAN_POINT('Ctrl Pts',(74.5718913655091,-7.03673575225599,
81.6514660023639));
#136151=CARTESIAN_POINT('Ctrl Pts',(73.1140318986091,-6.29478940213099,
82.2607063002199));
#136152=CARTESIAN_POINT('Ctrl Pts',(71.8575260548191,-5.19637919744099,
82.928630174457));
#136153=CARTESIAN_POINT('Ctrl Pts',(70.8896983141291,-3.80971022286699,
83.5402728946901));
#136154=CARTESIAN_POINT('Ctrl Pts',(70.2787662816691,-2.28538505246999,
83.9819257520999));
#136155=CARTESIAN_POINT('Ctrl Pts',(70.0882608690891,-1.22246888756199,
84.1439308024));
#136156=CARTESIAN_POINT('Ctrl Pts',(70.0460708324691,-0.720102865311186,
84.1884294602499));
#136157=CARTESIAN_POINT('Ctrl Pts',(84.7549627479325,-0.99814350218451,
82.1379981311978));
#136158=CARTESIAN_POINT('Ctrl Pts',(84.7360744487648,-1.13241223971952,
82.1299177820536));
#136159=CARTESIAN_POINT('Ctrl Pts',(84.7136170682954,-1.26571601940023,
82.1210096891642));
#136160=CARTESIAN_POINT('Ctrl Pts',(84.6876572285705,-1.39804856021889,
82.1113348976728));
#136161=CARTESIAN_POINT('Ctrl Pts',(84.6614814584809,-1.53148182485237,
82.1015796326007));
#136162=CARTESIAN_POINT('Ctrl Pts',(84.6317445010843,-1.66392813449533,
82.0910446876825));
#136163=CARTESIAN_POINT('Ctrl Pts',(84.5984643610126,-1.79536714138599,
82.0797821861936));
#136164=CARTESIAN_POINT('Ctrl Pts',(84.5650886283709,-1.92718368852826,
82.0684873347368));
#136165=CARTESIAN_POINT('Ctrl Pts',(84.5281490881766,-2.05798764684406,
82.0564605808227));
#136166=CARTESIAN_POINT('Ctrl Pts',(84.4876170667267,-2.18773691933232,
82.0437465570486));
#136167=CARTESIAN_POINT('Ctrl Pts',(84.4724313855847,-2.23634863446342,
82.0389831353351));
#136168=CARTESIAN_POINT('Ctrl Pts',(84.4567409789409,-2.28481204838324,
82.0341231745087));
#136169=CARTESIAN_POINT('Ctrl Pts',(84.4405427555362,-2.33312394443514,
82.0291688025217));
#136170=CARTESIAN_POINT('Ctrl Pts',(84.4390468242843,-2.33758562355486,
82.0287112585242));
#136171=CARTESIAN_POINT('Ctrl Pts',(84.4375465613714,-2.34204600997798,
82.0282529092394));
#136172=CARTESIAN_POINT('Ctrl Pts',(84.4360419658959,-2.34650510524211,
82.0277937580412));
#136173=CARTESIAN_POINT('Ctrl Pts',(84.3879187107657,-2.48912561855823,
82.0131081826739));
#136174=CARTESIAN_POINT('Ctrl Pts',(84.3354085581316,-2.63044179820462,
81.9975928703134));
#136175=CARTESIAN_POINT('Ctrl Pts',(84.2785407679911,-2.7704378407857,81.9813486682572));
#136176=CARTESIAN_POINT('Ctrl Pts',(84.2481717672931,-2.84519966825197,
81.9726738071034));
#136177=CARTESIAN_POINT('Ctrl Pts',(84.2165592642238,-2.91958456298685,
81.9637910023635));
#136178=CARTESIAN_POINT('Ctrl Pts',(84.1837027095352,-2.99358666842466,
81.9547153285447));
#136179=CARTESIAN_POINT('Ctrl Pts',(84.1365114894892,-3.09987442971577,
81.9416801176313));
#136180=CARTESIAN_POINT('Ctrl Pts',(84.0867580073447,-3.2053758055543,81.9282459220336));
#136181=CARTESIAN_POINT('Ctrl Pts',(84.034448766139,-3.31008109859886,81.9144497094881));
#136182=CARTESIAN_POINT('Ctrl Pts',(84.0082941455361,-3.36243374512114,
81.9075516032154));
#136183=CARTESIAN_POINT('Ctrl Pts',(83.9815005706135,-3.41458735658898,
81.9005629111546));
#136184=CARTESIAN_POINT('Ctrl Pts',(83.9540687613753,-3.46654073992166,
81.8934877212652));
#136185=CARTESIAN_POINT('Ctrl Pts',(83.9403528567561,-3.49251743158801,
81.8899501263205));
#136186=CARTESIAN_POINT('Ctrl Pts',(83.9264773926352,-3.51844406489059,
81.886390901512));
#136187=CARTESIAN_POINT('Ctrl Pts',(83.9124424531876,-3.5443204855787,81.8828105236135));
#136188=CARTESIAN_POINT('Ctrl Pts',(83.9021601880128,-3.56327804647741,
81.8801874702604));
#136189=CARTESIAN_POINT('Ctrl Pts',(83.8921228909752,-3.58160738984613,
81.877636985306));
#136190=CARTESIAN_POINT('Ctrl Pts',(83.8816051507227,-3.60063058216534,
81.874974903863));
#136191=CARTESIAN_POINT('Ctrl Pts',(83.8777665361195,-3.60757339517311,
81.8740033354028));
#136192=CARTESIAN_POINT('Ctrl Pts',(83.8738635042219,-3.61460838629155,
81.8730168606676));
#136193=CARTESIAN_POINT('Ctrl Pts',(83.8698592890158,-3.62179895102489,
81.8720063837862));
#136194=CARTESIAN_POINT('Ctrl Pts',(83.8055567097488,-3.73727023189799,
81.8557794163486));
#136195=CARTESIAN_POINT('Ctrl Pts',(83.7386745311195,-3.85060309564398,
81.8392979899471));
#136196=CARTESIAN_POINT('Ctrl Pts',(83.6692606961145,-3.96180672417764,
81.822653964058));
#136197=CARTESIAN_POINT('Ctrl Pts',(83.5909232222349,-4.08730636477421,
81.8038702310565));
#136198=CARTESIAN_POINT('Ctrl Pts',(83.5093615914043,-4.21009506539025,
81.784879210787));
#136199=CARTESIAN_POINT('Ctrl Pts',(83.4246113298914,-4.33020869538295,
81.7658426068169));
#136200=CARTESIAN_POINT('Ctrl Pts',(83.3385057774693,-4.45224313255535,
81.7465015773991));
#136201=CARTESIAN_POINT('Ctrl Pts',(83.2491083602584,-4.57151647204202,
81.7271131680751));
#136202=CARTESIAN_POINT('Ctrl Pts',(83.1564231635584,-4.68802431461752,
81.707849683635));
#136203=CARTESIAN_POINT('Ctrl Pts',(83.1199550191273,-4.73386577562394,
81.700270225881));
#136204=CARTESIAN_POINT('Ctrl Pts',(83.0829775630784,-4.77927863195264,
81.69271016344));
#136205=CARTESIAN_POINT('Ctrl Pts',(83.0454898973026,-4.82426075402366,
81.6851802546591));
#136206=CARTESIAN_POINT('Ctrl Pts',(82.9501617902535,-4.93864665827622,
81.6660323046475));
#136207=CARTESIAN_POINT('Ctrl Pts',(82.8515564168775,-5.05027360440036,
81.6470681875175));
#136208=CARTESIAN_POINT('Ctrl Pts',(82.7497100436443,-5.15917427335519,
81.6284219468575));
#136209=CARTESIAN_POINT('Ctrl Pts',(82.6861528954071,-5.22713364922855,
81.6167857751994));
#136210=CARTESIAN_POINT('Ctrl Pts',(82.6213327335815,-5.29403071669238,
81.6052733983345));
#136211=CARTESIAN_POINT('Ctrl Pts',(82.5552505652913,-5.35986676314358,
81.5939182192025));
#136212=CARTESIAN_POINT('Ctrl Pts',(82.5384537895867,-5.37660097956119,
81.5910319580234));
#136213=CARTESIAN_POINT('Ctrl Pts',(82.5215755786135,-5.39326681014543,
81.5881557678984));
#136214=CARTESIAN_POINT('Ctrl Pts',(82.5046160985963,-5.40986432477732,
81.5852901326943));
#136215=CARTESIAN_POINT('Ctrl Pts',(82.4347552855232,-5.47823410179861,
81.5734857846171));
#136216=CARTESIAN_POINT('Ctrl Pts',(82.3635160576312,-5.54544506882284,
81.5618604322946));
#136217=CARTESIAN_POINT('Ctrl Pts',(82.2909042280843,-5.61150565977019,
81.550453444742));
#136218=CARTESIAN_POINT('Ctrl Pts',(82.2457846535634,-5.65255442241319,
81.5433653651804));
#136219=CARTESIAN_POINT('Ctrl Pts',(82.2001352523272,-5.69315901295719,
81.5363615340839));
#136220=CARTESIAN_POINT('Ctrl Pts',(82.15395761102,-5.73332162022948,81.5294509463107));
#136221=CARTESIAN_POINT('Ctrl Pts',(82.1279475844843,-5.75594361761455,
81.5255584874005));
#136222=CARTESIAN_POINT('Ctrl Pts',(82.1013153617168,-5.77881549905558,
81.5216285233666));
#136223=CARTESIAN_POINT('Ctrl Pts',(82.0748265419983,-5.80127511088066,
81.5177767301801));
#136224=CARTESIAN_POINT('Ctrl Pts',(82.0542876812979,-5.81868981049962,
81.5147901326441));
#136225=CARTESIAN_POINT('Ctrl Pts',(82.0338357770383,-5.83585745707664,
81.5118503788618));
#136226=CARTESIAN_POINT('Ctrl Pts',(82.0138415095347,-5.85248560413429,
81.5090076667125));
#136227=CARTESIAN_POINT('Ctrl Pts',(81.8986996425497,-5.9482428453725,81.4926372153268));
#136228=CARTESIAN_POINT('Ctrl Pts',(81.7817255834563,-6.04015142672838,
81.4771184995858));
#136229=CARTESIAN_POINT('Ctrl Pts',(81.662976231238,-6.12830999999474,81.462606173832));
#136230=CARTESIAN_POINT('Ctrl Pts',(81.5421023396451,-6.21804581437126,
81.447834208704));
#136231=CARTESIAN_POINT('Ctrl Pts',(81.4193886010348,-6.30389644475892,
81.4341046199841));
#136232=CARTESIAN_POINT('Ctrl Pts',(81.2948623372305,-6.38592298340322,
81.4215837817183));
#136233=CARTESIAN_POINT('Ctrl Pts',(81.2160303171265,-6.43785032423818,
81.4136573978075));
#136234=CARTESIAN_POINT('Ctrl Pts',(81.1364712807916,-6.4882442571981,81.4062155196424));
#136235=CARTESIAN_POINT('Ctrl Pts',(81.0561868626913,-6.53711103817155,
81.3993019051947));
#136236=CARTESIAN_POINT('Ctrl Pts',(80.9915799369693,-6.5764353873208,81.3937383427295));
#136237=CARTESIAN_POINT('Ctrl Pts',(80.9265031831495,-6.61477064596132,
81.3885168921367));
#136238=CARTESIAN_POINT('Ctrl Pts',(80.8609607459812,-6.65211621421108,
81.3836595627514));
#136239=CARTESIAN_POINT('Ctrl Pts',(80.7366263364312,-6.72296098865415,
81.3744451788009));
#136240=CARTESIAN_POINT('Ctrl Pts',(80.6106167089957,-6.79027164309577,
81.3665297512573));
#136241=CARTESIAN_POINT('Ctrl Pts',(80.4829624543209,-6.85410722446704,
81.3600260293172));
#136242=CARTESIAN_POINT('Ctrl Pts',(80.4042283439736,-6.89347949388779,
81.3560146881973));
#136243=CARTESIAN_POINT('Ctrl Pts',(80.3248678990058,-6.93152908843398,
81.3525405705145));
#136244=CARTESIAN_POINT('Ctrl Pts',(80.244882277825,-6.96826245974566,81.3496327876378));
#136245=CARTESIAN_POINT('Ctrl Pts',(80.1400477816455,-7.01640766906684,
81.3458216532317));
#136246=CARTESIAN_POINT('Ctrl Pts',(80.0341430047996,-7.06229648467652,
81.342980692216));
#136247=CARTESIAN_POINT('Ctrl Pts',(79.9271780363573,-7.10595372188797,
81.3411672326213));
#136248=CARTESIAN_POINT('Ctrl Pts',(79.8736955521362,-7.12778234049369,
81.340260502824));
#136249=CARTESIAN_POINT('Ctrl Pts',(79.8199480149917,-7.14905305259735,
81.3396106217187));
#136250=CARTESIAN_POINT('Ctrl Pts',(79.7659366481784,-7.16976899764375,
81.3392245662652));
#136251=CARTESIAN_POINT('Ctrl Pts',(79.7337719231639,-7.18210570962021,
81.3389946634089));
#136252=CARTESIAN_POINT('Ctrl Pts',(79.7010237910141,-7.19442951282771,
81.3388564533094));
#136253=CARTESIAN_POINT('Ctrl Pts',(79.6685665191181,-7.20640952989372,
81.3388161853128));
#136254=CARTESIAN_POINT('Ctrl Pts',(79.6465211761977,-7.21454649178191,
81.338788834838));
#136255=CARTESIAN_POINT('Ctrl Pts',(79.6246103822755,-7.22252580680398,
81.3388062332073));
#136256=CARTESIAN_POINT('Ctrl Pts',(79.6031122661378,-7.2302556298964,81.3388647593018));
#136257=CARTESIAN_POINT('Ctrl Pts',(79.5584502322042,-7.24631422866124,
81.3389863464401));
#136258=CARTESIAN_POINT('Ctrl Pts',(79.5137873203361,-7.26192891990934,
81.3392941039157));
#136259=CARTESIAN_POINT('Ctrl Pts',(79.4691233092725,-7.27710452603065,
81.3397909651462));
#136260=CARTESIAN_POINT('Ctrl Pts',(79.3345029844086,-7.32284482067527,
81.3412885382182));
#136261=CARTESIAN_POINT('Ctrl Pts',(79.1998747063359,-7.3645999865306,81.344502458572));
#136262=CARTESIAN_POINT('Ctrl Pts',(79.0652674206663,-7.40249677718022,
81.3494555717584));
#136263=CARTESIAN_POINT('Ctrl Pts',(78.933472145338,-7.43960188581444,81.35430521205));
#136264=CARTESIAN_POINT('Ctrl Pts',(78.8016963053603,-7.47300794763936,
81.3608221119125));
#136265=CARTESIAN_POINT('Ctrl Pts',(78.6699471663124,-7.50278713154373,
81.3690474907127));
#136266=CARTESIAN_POINT('Ctrl Pts',(78.533981488312,-7.5335193773794,81.3775361170026));
#136267=CARTESIAN_POINT('Ctrl Pts',(78.3980437019746,-7.56038914233644,
81.3878441265407));
#136268=CARTESIAN_POINT('Ctrl Pts',(78.2621295209197,-7.58342428445968,
81.4000401022841));
#136269=CARTESIAN_POINT('Ctrl Pts',(78.1262153398648,-7.60645942658291,
81.4122360780274));
#136270=CARTESIAN_POINT('Ctrl Pts',(77.9903241708066,-7.62565997343611,
81.4263199514631));
#136271=CARTESIAN_POINT('Ctrl Pts',(77.8544483957737,-7.6410013238083,81.4423850973286));
#136272=CARTESIAN_POINT('Ctrl Pts',(77.7209526142816,-7.65607395582517,
81.4581688468717));
#136273=CARTESIAN_POINT('Ctrl Pts',(77.5874711687472,-7.66742130973048,
81.4758650585326));
#136274=CARTESIAN_POINT('Ctrl Pts',(77.4540138689537,-7.67503337615444,
81.4954788561316));
#136275=CARTESIAN_POINT('Ctrl Pts',(77.3205565691602,-7.6826454425784,81.5150926537307));
#136276=CARTESIAN_POINT('Ctrl Pts',(77.1871229045546,-7.68652218089232,
81.5366242464878));
#136277=CARTESIAN_POINT('Ctrl Pts',(77.0537354665173,-7.68660419195478,
81.5601015030313));
#136278=CARTESIAN_POINT('Ctrl Pts',(76.9202673858979,-7.68668625259899,
81.5835929533145));
#136279=CARTESIAN_POINT('Ctrl Pts',(76.7874208243268,-7.68303005328711,
81.6088991951285));
#136280=CARTESIAN_POINT('Ctrl Pts',(76.6551998873563,-7.67566113397853,
81.6360063004115));
#136281=CARTESIAN_POINT('Ctrl Pts',(76.5229789503857,-7.66829221466995,
81.6631134056944));
#136282=CARTESIAN_POINT('Ctrl Pts',(76.3913831051237,-7.65721057010139,
81.6920214619695));
#136283=CARTESIAN_POINT('Ctrl Pts',(76.2604215554106,-7.64239141385766,
81.7227409989038));
#136284=CARTESIAN_POINT('Ctrl Pts',(76.1309714136242,-7.62774328331012,
81.7531060061938));
#136285=CARTESIAN_POINT('Ctrl Pts',(76.0021406178159,-7.60944320485009,
81.7852412915906));
#136286=CARTESIAN_POINT('Ctrl Pts',(75.8739036080351,-7.58748086647297,
81.8190837299511));
#136287=CARTESIAN_POINT('Ctrl Pts',(75.8490812052546,-7.58322969116773,
81.8256344958921));
#136288=CARTESIAN_POINT('Ctrl Pts',(75.824281097167,-7.57884115868288,81.8322492794074));
#136289=CARTESIAN_POINT('Ctrl Pts',(75.7995031705135,-7.57431499439249,
81.8389276969693));
#136290=CARTESIAN_POINT('Ctrl Pts',(75.6703568634415,-7.55072394048887,
81.8737366209468));
#136291=CARTESIAN_POINT('Ctrl Pts',(75.5418227299606,-7.52338594290897,
81.9102768687294));
#136292=CARTESIAN_POINT('Ctrl Pts',(75.4138856636451,-7.49228417086409,
81.9484803963819));
#136293=CARTESIAN_POINT('Ctrl Pts',(75.3378562073981,-7.47380124886977,
81.9711836951037));
#136294=CARTESIAN_POINT('Ctrl Pts',(75.2620377881377,-7.45398821726154,
81.9944747601753));
#136295=CARTESIAN_POINT('Ctrl Pts',(75.186429615227,-7.43283364015822,82.0183421750203));
#136296=CARTESIAN_POINT('Ctrl Pts',(75.0850114487219,-7.40445762814239,
82.0503570929796));
#136297=CARTESIAN_POINT('Ctrl Pts',(74.9839698448508,-7.37367323551073,
82.0834066995368));
#136298=CARTESIAN_POINT('Ctrl Pts',(74.8832988954068,-7.34046442508238,
82.1174574003437));
#136299=CARTESIAN_POINT('Ctrl Pts',(74.8329634206847,-7.32386001986821,
82.1344827507471));
#136300=CARTESIAN_POINT('Ctrl Pts',(74.782720607907,-7.30664950030032,82.1517583620035));
#136301=CARTESIAN_POINT('Ctrl Pts',(74.7325697048827,-7.28883083654385,
82.1692799170975));
#136302=CARTESIAN_POINT('Ctrl Pts',(74.7240302608494,-7.2857967639206,82.1722633995491));
#136303=CARTESIAN_POINT('Ctrl Pts',(74.7155330656988,-7.28275913879809,
82.1752401765379));
#136304=CARTESIAN_POINT('Ctrl Pts',(74.7070577589877,-7.27971106113057,
82.1782171902271));
#136305=CARTESIAN_POINT('Ctrl Pts',(74.6776617970466,-7.26913903369103,
82.188542737619));
#136306=CARTESIAN_POINT('Ctrl Pts',(74.6485275155047,-7.25844464497075,
82.1988700083502));
#136307=CARTESIAN_POINT('Ctrl Pts',(74.6188180851307,-7.24731174775921,
82.2094977507359));
#136308=CARTESIAN_POINT('Ctrl Pts',(74.6067881907205,-7.24280383305841,
82.2138011189631));
#136309=CARTESIAN_POINT('Ctrl Pts',(74.5946642400973,-7.23822351646149,
82.2181539192958));
#136310=CARTESIAN_POINT('Ctrl Pts',(74.5823917165411,-7.23354770312353,
82.2225766637255));
#136311=CARTESIAN_POINT('Ctrl Pts',(74.4580746745002,-7.18618309382779,
82.2673777596604));
#136312=CARTESIAN_POINT('Ctrl Pts',(74.3357407315584,-7.13550734464184,
82.3131825148036));
#136313=CARTESIAN_POINT('Ctrl Pts',(74.2153309053991,-7.0815174423743,82.3598796338195));
#136314=CARTESIAN_POINT('Ctrl Pts',(74.0935049939706,-7.02689258939118,
82.40712593644));
#136315=CARTESIAN_POINT('Ctrl Pts',(73.973648537563,-6.96887488323718,82.4552861201515));
#136316=CARTESIAN_POINT('Ctrl Pts',(73.8557364363267,-6.90742206970627,
82.5042519222903));
#136317=CARTESIAN_POINT('Ctrl Pts',(73.7369227152364,-6.84549935464542,
82.5535921435));
#136318=CARTESIAN_POINT('Ctrl Pts',(73.6200830207485,-6.78008853136454,
82.6037508515811));
#136319=CARTESIAN_POINT('Ctrl Pts',(73.50523071568,-6.71111110896202,82.654617501447));
#136320=CARTESIAN_POINT('Ctrl Pts',(73.474673851995,-6.69275942074431,82.6681507543072));
#136321=CARTESIAN_POINT('Ctrl Pts',(73.4442578854804,-6.67415509260198,
82.6817340957715));
#136322=CARTESIAN_POINT('Ctrl Pts',(73.4139835532656,-6.65529626560641,
82.6953653726223));
#136323=CARTESIAN_POINT('Ctrl Pts',(73.3532577660512,-6.61746827630128,
82.7227076773718));
#136324=CARTESIAN_POINT('Ctrl Pts',(73.2930910845494,-6.57862296025367,
82.7502418956387));
#136325=CARTESIAN_POINT('Ctrl Pts',(73.233481559248,-6.53875599409344,82.7779467051893));
#136326=CARTESIAN_POINT('Ctrl Pts',(73.1187118027947,-6.46199775833156,
82.8312884190953));
#136327=CARTESIAN_POINT('Ctrl Pts',(73.006005545972,-6.38145478231525,82.8852628427268));
#136328=CARTESIAN_POINT('Ctrl Pts',(72.8953331151939,-6.29706100314168,
82.9397174782743));
#136329=CARTESIAN_POINT('Ctrl Pts',(72.8890306839395,-6.29225505474236,
82.9428184908265));
#136330=CARTESIAN_POINT('Ctrl Pts',(72.8827348566264,-6.28743660724246,
82.9459210592896));
#136331=CARTESIAN_POINT('Ctrl Pts',(72.876445630877,-6.28260564440167,82.9490251549171));
#136332=CARTESIAN_POINT('Ctrl Pts',(72.7894002484549,-6.21574319984927,
82.9919870713344));
#136333=CARTESIAN_POINT('Ctrl Pts',(72.7036179244276,-6.14648865782259,
83.03524015749));
#136334=CARTESIAN_POINT('Ctrl Pts',(72.6190838017302,-6.0748140055321,83.0787001451335));
#136335=CARTESIAN_POINT('Ctrl Pts',(72.5768167403815,-6.03897667938686,
83.1004301389553));
#136336=CARTESIAN_POINT('Ctrl Pts',(72.534861713998,-6.00253429108223,83.1222117709614));
#136337=CARTESIAN_POINT('Ctrl Pts',(72.4932167522304,-5.96548337269157,
83.1440338661608));
#136338=CARTESIAN_POINT('Ctrl Pts',(72.4684716255418,-5.94346799242492,
83.1570003929002));
#136339=CARTESIAN_POINT('Ctrl Pts',(72.4442122146909,-5.92157790891612,
83.1697828502902));
#136340=CARTESIAN_POINT('Ctrl Pts',(72.4197650747079,-5.89920874176838,
83.1827325478749));
#136341=CARTESIAN_POINT('Ctrl Pts',(72.4030687514654,-5.8839315827378,83.1915766227612));
#136342=CARTESIAN_POINT('Ctrl Pts',(72.3862855263746,-5.86843017263442,
83.2004986849878));
#136343=CARTESIAN_POINT('Ctrl Pts',(72.36921001917,-5.85250144408564,83.209609964908));
#136344=CARTESIAN_POINT('Ctrl Pts',(72.2664577427722,-5.75664993590502,
83.2644373115564));
#136345=CARTESIAN_POINT('Ctrl Pts',(72.1668936099123,-5.65813854884049,
83.3187729618543));
#136346=CARTESIAN_POINT('Ctrl Pts',(72.0704444321277,-5.55696396556987,
83.3724839663531));
#136347=CARTESIAN_POINT('Ctrl Pts',(72.0239516868539,-5.50819336704083,
83.3983750325906));
#136348=CARTESIAN_POINT('Ctrl Pts',(71.9781833304177,-5.45880339191821,
83.4241209393293));
#136349=CARTESIAN_POINT('Ctrl Pts',(71.9331344087398,-5.40879086198571,
83.4497065171101));
#136350=CARTESIAN_POINT('Ctrl Pts',(71.8384680863801,-5.3036939561272,83.5034723446536));
#136351=CARTESIAN_POINT('Ctrl Pts',(71.7469760400854,-5.19584976202539,
83.5565309520128));
#136352=CARTESIAN_POINT('Ctrl Pts',(71.6586524489669,-5.08522986784536,
83.6087501663433));
#136353=CARTESIAN_POINT('Ctrl Pts',(71.5905511639268,-4.99993717481426,
83.6490134250567));
#136354=CARTESIAN_POINT('Ctrl Pts',(71.5243343689076,-4.91299360910555,
83.6887775636091));
#136355=CARTESIAN_POINT('Ctrl Pts',(71.4600165668395,-4.82437529006003,
83.7279761120231));
#136356=CARTESIAN_POINT('Ctrl Pts',(71.3770393817778,-4.71004771009223,
83.7785466399534));
#136357=CARTESIAN_POINT('Ctrl Pts',(71.2971899486146,-4.59294591585182,
83.8281775698261));
#136358=CARTESIAN_POINT('Ctrl Pts',(71.2204294110572,-4.47306146190551,
83.8767110777767));
#136359=CARTESIAN_POINT('Ctrl Pts',(71.1724066958443,-4.39805968138773,
83.9070744767935));
#136360=CARTESIAN_POINT('Ctrl Pts',(71.1255935713537,-4.32196797949701,
83.9370082301691));
#136361=CARTESIAN_POINT('Ctrl Pts',(71.0799873234695,-4.2447766950706,83.9664715749255));
#136362=CARTESIAN_POINT('Ctrl Pts',(71.0249406041176,-4.15160685174068,
84.0020338179343));
#136363=CARTESIAN_POINT('Ctrl Pts',(70.9716483317067,-4.05683928399666,
84.0369103266833));
#136364=CARTESIAN_POINT('Ctrl Pts',(70.9200963792618,-3.96046726874635,
84.0710235032939));
#136365=CARTESIAN_POINT('Ctrl Pts',(70.9161579623552,-3.95310473141867,
84.0736296492327));
#136366=CARTESIAN_POINT('Ctrl Pts',(70.9122297077862,-3.94573282279201,
84.076231338417));
#136367=CARTESIAN_POINT('Ctrl Pts',(70.9083116133528,-3.93835154817217,
84.0788285415872));
#136368=CARTESIAN_POINT('Ctrl Pts',(70.8807095955352,-3.88635227223872,
84.0971252032424));
#136369=CARTESIAN_POINT('Ctrl Pts',(70.8536115023071,-3.8338881617024,84.1151993319809));
#136370=CARTESIAN_POINT('Ctrl Pts',(70.8270155955156,-3.78095909067874,
84.1330410827773));
#136371=CARTESIAN_POINT('Ctrl Pts',(70.8137176421198,-3.75449455516691,
84.1419619581755));
#136372=CARTESIAN_POINT('Ctrl Pts',(70.8005452341496,-3.72791377663219,
84.15082473169));
#136373=CARTESIAN_POINT('Ctrl Pts',(70.7874981462678,-3.70121673421146,
84.1596281235744));
#136374=CARTESIAN_POINT('Ctrl Pts',(70.7780962506347,-3.68197850964915,
84.1659719584948));
#136375=CARTESIAN_POINT('Ctrl Pts',(70.7684676576691,-3.66207455726415,
84.1724822999379));
#136376=CARTESIAN_POINT('Ctrl Pts',(70.7592441592484,-3.64281282634221,
84.1787315082593));
#136377=CARTESIAN_POINT('Ctrl Pts',(70.7556681330659,-3.63534489487485,
84.1811543777127));
#136378=CARTESIAN_POINT('Ctrl Pts',(70.7521525557527,-3.62797378993837,
84.1835382034184));
#136379=CARTESIAN_POINT('Ctrl Pts',(70.74873261181,-3.62077678971988,84.1858588405169));
#136380=CARTESIAN_POINT('Ctrl Pts',(70.688329356344,-3.49366293929857,84.2268460724291));
#136381=CARTESIAN_POINT('Ctrl Pts',(70.6315071694851,-3.36531292644329,
84.2660184693106));
#136382=CARTESIAN_POINT('Ctrl Pts',(70.5781646283892,-3.23577268923496,
84.3033262527094));
#136383=CARTESIAN_POINT('Ctrl Pts',(70.5245696607706,-3.10561944426687,
84.3408105832663));
#136384=CARTESIAN_POINT('Ctrl Pts',(70.474487159193,-2.97426429595224,84.3764129514617));
#136385=CARTESIAN_POINT('Ctrl Pts',(70.4278502244862,-2.84171706529408,
84.4100715443734));
#136386=CARTESIAN_POINT('Ctrl Pts',(70.3812679668711,-2.70932523286541,
84.4436906759872));
#136387=CARTESIAN_POINT('Ctrl Pts',(70.3381230335348,-2.5757437198833,84.4753709110724));
#136388=CARTESIAN_POINT('Ctrl Pts',(70.2983871952725,-2.44095161278315,
84.5050344211557));
#136389=CARTESIAN_POINT('Ctrl Pts',(70.2876629873508,-2.4045729016259,84.5130402331313));
#136390=CARTESIAN_POINT('Ctrl Pts',(70.2771873200981,-2.36810585696577,
84.5208990415673));
#136391=CARTESIAN_POINT('Ctrl Pts',(70.2669601445328,-2.33154973971516,
84.5286090662555));
#136392=CARTESIAN_POINT('Ctrl Pts',(70.229543400307,-2.19780695996857,84.556816660805));
#136393=CARTESIAN_POINT('Ctrl Pts',(70.1954495382031,-2.0628735825815,84.5830346153964));
#136394=CARTESIAN_POINT('Ctrl Pts',(70.1646701972361,-1.92681521965721,
84.6072227704094));
#136395=CARTESIAN_POINT('Ctrl Pts',(70.1339904801362,-1.79119723848968,
84.6313326353271));
#136396=CARTESIAN_POINT('Ctrl Pts',(70.10660374315,-1.65446098223881,84.6534259993471));
#136397=CARTESIAN_POINT('Ctrl Pts',(70.0825437781818,-1.51665518632324,
84.6734379987387));
#136398=CARTESIAN_POINT('Ctrl Pts',(70.058800614693,-1.3806639017788,84.6931864968732));
#136399=CARTESIAN_POINT('Ctrl Pts',(70.0382971263697,-1.2436305189225,84.7109082196508));
#136400=CARTESIAN_POINT('Ctrl Pts',(70.021108087152,-1.10559420119456,84.7265140592814));
#136401=CARTESIAN_POINT('Ctrl Pts',(70.0166563193025,-1.06984434725915,
84.7305557962425));
#136402=CARTESIAN_POINT('Ctrl Pts',(70.0124270949701,-1.03402720429941,
84.7344554625199));
#136403=CARTESIAN_POINT('Ctrl Pts',(70.0084221937706,-0.998143435151018,
84.7382111936731));
#136404=CARTESIAN_POINT('Origin',(58.9775436614391,0.499074165591714,68.468974588834));
#136405=CARTESIAN_POINT('',(27.1339039101791,-17.49925933285,74.332577093855));
#136406=CARTESIAN_POINT('Ctrl Pts',(27.1339039101784,-17.4992593325406,
74.3325770938509));
#136407=CARTESIAN_POINT('Ctrl Pts',(27.1982913289528,-17.4950745137893,
74.6334817214542));
#136408=CARTESIAN_POINT('Ctrl Pts',(27.2828755029589,-17.4830576398145,
74.9272738053655));
#136409=CARTESIAN_POINT('Ctrl Pts',(27.3853788653411,-17.4637140526782,
75.2141944686376));
#136410=CARTESIAN_POINT('Ctrl Pts',(27.4863721644485,-17.4446554321992,
75.4968882622118));
#136411=CARTESIAN_POINT('Ctrl Pts',(27.6047606718065,-17.4184843758367,
75.7729121468281));
#136412=CARTESIAN_POINT('Ctrl Pts',(27.7383735353809,-17.3856492136401,
76.0425394622034));
#136413=CARTESIAN_POINT('Ctrl Pts',(27.8752459130299,-17.352013030715,76.3187443929808));
#136414=CARTESIAN_POINT('Ctrl Pts',(28.0280945594496,-17.3113838307385,
76.5882371363484));
#136415=CARTESIAN_POINT('Ctrl Pts',(28.1945927667414,-17.2642047518374,
76.8513508114181));
#136416=CARTESIAN_POINT('Ctrl Pts',(28.3604515551069,-17.2172068592474,
77.1134540259771));
#136417=CARTESIAN_POINT('Ctrl Pts',(28.5398553429514,-17.1637092839206,
77.3692275095003));
#136418=CARTESIAN_POINT('Ctrl Pts',(28.730509915084,-17.1041109159427,77.61903338945));
#136419=CARTESIAN_POINT('Ctrl Pts',(28.9399583222007,-17.0386376199178,
77.8934639633333));
#136420=CARTESIAN_POINT('Ctrl Pts',(29.1629774015092,-16.9658061284426,
78.1606496886631));
#136421=CARTESIAN_POINT('Ctrl Pts',(29.3963622189773,-16.8861931968548,
78.4208392935282));
#136422=CARTESIAN_POINT('Ctrl Pts',(29.5855699599087,-16.8216500826194,
78.6317779821903));
#136423=CARTESIAN_POINT('Ctrl Pts',(29.7815907945949,-16.7526500206384,
78.838119475292));
#136424=CARTESIAN_POINT('Ctrl Pts',(29.9827213544611,-16.6795013769138,
79.0400210135803));
#136425=CARTESIAN_POINT('Ctrl Pts',(30.1852441501547,-16.605846394607,79.2433201244473));
#136426=CARTESIAN_POINT('Ctrl Pts',(30.3929478467462,-16.5279897126078,
79.4421186857153));
#136427=CARTESIAN_POINT('Ctrl Pts',(30.6044386189885,-16.4461190354791,
79.6368566889028));
#136428=CARTESIAN_POINT('Ctrl Pts',(30.8188237598271,-16.3631279126954,
79.834259789744));
#136429=CARTESIAN_POINT('Ctrl Pts',(31.0371004033291,-16.2760121129733,
80.0274907773708));
#136430=CARTESIAN_POINT('Ctrl Pts',(31.257816792588,-16.1849137907709,80.2170084150241));
#136431=CARTESIAN_POINT('Ctrl Pts',(31.3023319280142,-16.1665406461052,
80.2552312372355));
#136432=CARTESIAN_POINT('Ctrl Pts',(31.3469463029,-16.148005335896,80.2933030041325));
#136433=CARTESIAN_POINT('Ctrl Pts',(31.391648004194,-16.1293087719458,80.3312274622805));
#136434=CARTESIAN_POINT('Ctrl Pts',(31.5979455906182,-16.0430244492983,
80.5062481875747));
#136435=CARTESIAN_POINT('Ctrl Pts',(31.8061017853515,-15.9533132910267,
80.6781242881749));
#136436=CARTESIAN_POINT('Ctrl Pts',(32.0158754047086,-15.8601965732316,
80.8471509506169));
#136437=CARTESIAN_POINT('Ctrl Pts',(32.2270784857348,-15.7664453296117,
81.017329412488));
#136438=CARTESIAN_POINT('Ctrl Pts',(32.4399211648802,-15.6692418259999,
81.1846197827002));
#136439=CARTESIAN_POINT('Ctrl Pts',(32.6541546846915,-15.56855720567,81.3493085237292));
#136440=CARTESIAN_POINT('Ctrl Pts',(32.7273779099949,-15.5341440445293,
81.4055977580186));
#136441=CARTESIAN_POINT('Ctrl Pts',(32.800763589346,-15.4993237904429,81.4615829181366));
#136442=CARTESIAN_POINT('Ctrl Pts',(32.8743017032979,-15.4640939912119,
81.5172749492701));
#136443=CARTESIAN_POINT('Ctrl Pts',(33.2821956378359,-15.2686848265071,
81.8261819973396));
#136444=CARTESIAN_POINT('Ctrl Pts',(33.6947782118764,-15.0606809876076,
82.1260641652557));
#136445=CARTESIAN_POINT('Ctrl Pts',(34.1084197158662,-14.8406064781875,
82.4171159496633));
#136446=CARTESIAN_POINT('Ctrl Pts',(34.2042488545752,-14.7896213848491,
82.4845444875409));
#136447=CARTESIAN_POINT('Ctrl Pts',(34.3001348340015,-14.7379882161778,
82.5514991156476));
#136448=CARTESIAN_POINT('Ctrl Pts',(34.3960325283857,-14.6857130992848,
82.6179822923526));
#136449=CARTESIAN_POINT('Ctrl Pts',(34.7537904431313,-14.4906944710184,
82.8660058013264));
#136450=CARTESIAN_POINT('Ctrl Pts',(35.1117127901067,-14.2867413796121,
83.1074757483565));
#136451=CARTESIAN_POINT('Ctrl Pts',(35.4674621532407,-14.0740785882671,
83.3426103575327));
#136452=CARTESIAN_POINT('Ctrl Pts',(35.6186855505316,-13.983679017341,83.4425623408814));
#136453=CARTESIAN_POINT('Ctrl Pts',(35.7695162523914,-13.8917050394001,
83.5413692964044));
#136454=CARTESIAN_POINT('Ctrl Pts',(35.9197744880949,-13.7981714029223,
83.6390466762019));
#136455=CARTESIAN_POINT('Ctrl Pts',(36.1573782913382,-13.6502663802506,
83.7935042127361));
#136456=CARTESIAN_POINT('Ctrl Pts',(36.3935505923242,-13.4984665969623,
83.9451369988048));
#136457=CARTESIAN_POINT('Ctrl Pts',(36.627934024532,-13.3426521202487,84.0941320905792));
#136458=CARTESIAN_POINT('Ctrl Pts',(36.8616537748734,-13.1872788489639,
84.2427052867458));
#136459=CARTESIAN_POINT('Ctrl Pts',(37.0935948225531,-13.0279133343153,
84.3886559872256));
#136460=CARTESIAN_POINT('Ctrl Pts',(37.3233966571362,-12.8643989719943,
84.5321346656806));
#136461=CARTESIAN_POINT('Ctrl Pts',(37.3517202451919,-12.8442454625675,
84.5498187324362));
#136462=CARTESIAN_POINT('Ctrl Pts',(37.3800113279564,-12.8240288832378,
84.5674651995495));
#136463=CARTESIAN_POINT('Ctrl Pts',(37.4082692233398,-12.8037489039716,
84.5850743085344));
#136464=CARTESIAN_POINT('Ctrl Pts',(37.6721007149409,-12.6144036924174,
84.7494827836253));
#136465=CARTESIAN_POINT('Ctrl Pts',(37.9330389136035,-12.4195387807628,
84.910632971492));
#136466=CARTESIAN_POINT('Ctrl Pts',(38.1907510642886,-12.2190247507161,
85.0684847317907));
#136467=CARTESIAN_POINT('Ctrl Pts',(38.4091796349929,-12.0490754764082,
85.2022748316891));
#136468=CARTESIAN_POINT('Ctrl Pts',(38.6252906002273,-11.8750674671407,
85.3336948424002));
#136469=CARTESIAN_POINT('Ctrl Pts',(38.8388767635722,-11.6969091604009,
85.4626942795363));
#136470=CARTESIAN_POINT('Ctrl Pts',(39.1270776544536,-11.4565125826627,
85.6367587045141));
#136471=CARTESIAN_POINT('Ctrl Pts',(39.4106809652526,-11.2085529188707,
85.8064124729285));
#136472=CARTESIAN_POINT('Ctrl Pts',(39.6883537137141,-10.9532280783211,
85.9712624875313));
#136473=CARTESIAN_POINT('Ctrl Pts',(39.8592578972352,-10.7960787590286,
86.0727256570546));
#136474=CARTESIAN_POINT('Ctrl Pts',(40.0279154407973,-10.6361403353735,
86.1723690806801));
#136475=CARTESIAN_POINT('Ctrl Pts',(40.1940157028205,-10.4734687442745,
86.2701020081475));
#136476=CARTESIAN_POINT('Ctrl Pts',(40.4577034541812,-10.2152240820163,
86.4252551401406));
#136477=CARTESIAN_POINT('Ctrl Pts',(40.7149464230308,-9.95008648200096,
86.575594196585));
#136478=CARTESIAN_POINT('Ctrl Pts',(40.9645956540344,-9.67833462016586,
86.720735668409));
#136479=CARTESIAN_POINT('Ctrl Pts',(41.1277037924083,-9.50078574446779,
86.81556374048));
#136480=CARTESIAN_POINT('Ctrl Pts',(41.2875704671745,-9.32041449813221,
86.9081733664075));
#136481=CARTESIAN_POINT('Ctrl Pts',(41.4438758282522,-9.13731015598172,
86.9984609032528));
#136482=CARTESIAN_POINT('Ctrl Pts',(41.6201794994561,-8.93077873881247,
87.1003001754316));
#136483=CARTESIAN_POINT('Ctrl Pts',(41.7919523874227,-8.72077832621035,
87.199185857265));
#136484=CARTESIAN_POINT('Ctrl Pts',(41.9588973073281,-8.50711064257257,
87.2951279169551));
#136485=CARTESIAN_POINT('Ctrl Pts',(42.1240576117314,-8.29572703359078,
87.390044370792));
#136486=CARTESIAN_POINT('Ctrl Pts',(42.2844926409153,-8.0807538024963,87.482079936388));
#136487=CARTESIAN_POINT('Ctrl Pts',(42.4399061015799,-7.86198528229721,
87.571195846887));
#136488=CARTESIAN_POINT('Ctrl Pts',(42.4798420701361,-7.80576922027538,
87.5940956020583));
#136489=CARTESIAN_POINT('Ctrl Pts',(42.5194464116305,-7.74930249330274,
87.6168023108442));
#136490=CARTESIAN_POINT('Ctrl Pts',(42.5587140031694,-7.69258150586829,
87.6393147742221));
#136491=CARTESIAN_POINT('Ctrl Pts',(42.7077371246306,-7.47732158620972,
87.7247510699781));
#136492=CARTESIAN_POINT('Ctrl Pts',(42.8519095415155,-7.25839729428666,
87.8073860353505));
#136493=CARTESIAN_POINT('Ctrl Pts',(42.9907582766186,-7.03615374217394,
87.8869286456913));
#136494=CARTESIAN_POINT('Ctrl Pts',(43.1288681098162,-6.81509288851389,
87.9660479595122));
#136495=CARTESIAN_POINT('Ctrl Pts',(43.2617107345816,-6.59074824536283,
88.0421075322903));
#136496=CARTESIAN_POINT('Ctrl Pts',(43.3888275786924,-6.36349230427373,
88.1148600590489));
#136497=CARTESIAN_POINT('Ctrl Pts',(43.5156337971883,-6.13679169097714,
88.1874348060764));
#136498=CARTESIAN_POINT('Ctrl Pts',(43.6367421491539,-5.9071942407316,88.2567184512936));
#136499=CARTESIAN_POINT('Ctrl Pts',(43.751704839413,-5.67509888870081,88.3225075991413));
#136500=CARTESIAN_POINT('Ctrl Pts',(43.8663745942534,-5.44359493679249,
88.3881291102408));
#136501=CARTESIAN_POINT('Ctrl Pts',(43.974929938052,-5.20960607161433,88.4502737462847));
#136502=CARTESIAN_POINT('Ctrl Pts',(44.0769343622043,-4.97355330867935,
88.5087843081332));
#136503=CARTESIAN_POINT('Ctrl Pts',(44.1464226989862,-4.81274740221558,
88.5486433795491));
#136504=CARTESIAN_POINT('Ctrl Pts',(44.2128710981111,-4.65098421905349,
88.5868169065546));
#136505=CARTESIAN_POINT('Ctrl Pts',(44.2761437580013,-4.48840253804638,
88.6232676465585));
#136506=CARTESIAN_POINT('Ctrl Pts',(44.3762043421766,-4.23129278470233,
88.6809115380077));
#136507=CARTESIAN_POINT('Ctrl Pts',(44.4683241866109,-3.97213157424582,
88.7342549993688));
#136508=CARTESIAN_POINT('Ctrl Pts',(44.5522953596013,-3.71081561019567,
88.7832791000227));
#136509=CARTESIAN_POINT('Ctrl Pts',(44.6354995476277,-3.45188648210521,
88.8318554190541));
#136510=CARTESIAN_POINT('Ctrl Pts',(44.7107032491022,-3.19084136186465,
88.8761909579907));
#136511=CARTESIAN_POINT('Ctrl Pts',(44.7776953346401,-2.92757671872878,
88.9162171463247));
#136512=CARTESIAN_POINT('Ctrl Pts',(44.8441968372951,-2.66623996194838,
88.9559502229767));
#136513=CARTESIAN_POINT('Ctrl Pts',(44.9026065573288,-2.40271565605888,
88.9914368688759));
#136514=CARTESIAN_POINT('Ctrl Pts',(44.952709117092,-2.13690571923174,89.0225598028839));
#136515=CARTESIAN_POINT('Ctrl Pts',(45.0021618408937,-1.87454336785105,
89.0532790688589));
#136516=CARTESIAN_POINT('Ctrl Pts',(45.0435214918964,-1.60995389394597,
89.0797470578205));
#136517=CARTESIAN_POINT('Ctrl Pts',(45.0765723089672,-1.34305209460568,
89.1018019043616));
#136518=CARTESIAN_POINT('Ctrl Pts',(45.0907559739345,-1.22851193988243,
89.1112666795765));
#136519=CARTESIAN_POINT('Ctrl Pts',(45.1034093144603,-1.11354608029957,
89.1199180806114));
#136520=CARTESIAN_POINT('Ctrl Pts',(45.1145147830323,-0.998148588051396,
89.1277405079779));
#136521=CARTESIAN_POINT('',(91.9214475326691,-17.49925970194,62.90875755409));
#136522=CARTESIAN_POINT('',(27.1339039101791,-17.49925933285,74.332577093855));
#136523=CARTESIAN_POINT('Ctrl Pts',(91.9214475326691,-17.49925970194,62.90875755409));
#136524=CARTESIAN_POINT('Ctrl Pts',(92.3053259419944,-17.4691790615711,
65.0858401978147));
#136525=CARTESIAN_POINT('Ctrl Pts',(92.6881140569403,-17.0272695410026,
67.2567394748733));
#136526=CARTESIAN_POINT('Ctrl Pts',(93.400573325857,-15.3785962058232,71.2972967738997));
#136527=CARTESIAN_POINT('Ctrl Pts',(93.7300269848005,-14.1723356877064,
73.1657213202724));
#136528=CARTESIAN_POINT('Ctrl Pts',(94.2915430224096,-11.1564801229904,
76.3502370157891));
#136529=CARTESIAN_POINT('Ctrl Pts',(94.523433985036,-9.34780573756797,77.6653560162659));
#136530=CARTESIAN_POINT('Ctrl Pts',(94.8586248200716,-5.36963819152602,
79.5663177051065));
#136531=CARTESIAN_POINT('Ctrl Pts',(94.9618223675578,-3.20135946055536,
80.1515800799944));
#136532=CARTESIAN_POINT('Ctrl Pts',(94.9937559636691,-0.998148678735586,
80.332684502886));
#136533=CARTESIAN_POINT('Ctrl Pts',(94.5010653292691,0.271395986764614,
80.458308728496));
#136534=CARTESIAN_POINT('Ctrl Pts',(96.7480709862691,0.273309186559814,
80.062047303158));
#136535=CARTESIAN_POINT('Ctrl Pts',(101.075637772369,0.277199406335714,
79.298871480375));
#136536=CARTESIAN_POINT('Ctrl Pts',(106.443694708969,0.282511544310714,
78.353143604676));
#136537=CARTESIAN_POINT('Ctrl Pts',(110.084319043969,0.286361092968914,
77.709147420917));
#136538=CARTESIAN_POINT('Ctrl Pts',(111.775396016869,0.288211127596014,
77.413751883086));
#136539=CARTESIAN_POINT('Ctrl Pts',(112.489943251869,0.289007101963614,
77.28503103697));
#136540=CARTESIAN_POINT('Ctrl Pts',(112.751175106569,0.289282890086814,
77.242567650816));
#136541=CARTESIAN_POINT('Ctrl Pts',(113.006167906869,0.289653838855314,
77.183975946042));
#136542=CARTESIAN_POINT('Ctrl Pts',(113.328591681969,0.289983672853814,
77.111221001818));
#136543=CARTESIAN_POINT('Ctrl Pts',(114.612842666369,0.291414265154114,
76.810397989321));
#136544=CARTESIAN_POINT('Ctrl Pts',(116.776314331769,0.293771628264714,
76.212440481214));
#136545=CARTESIAN_POINT('Ctrl Pts',(120.750299755769,0.297915106635414,
74.787245381488));
#136546=CARTESIAN_POINT('Ctrl Pts',(124.528351856069,0.301393775126614,
72.86985978332));
#136547=CARTESIAN_POINT('Ctrl Pts',(127.965747787169,0.304277195172014,
70.412480183491));
#136548=CARTESIAN_POINT('Ctrl Pts',(130.333310528569,0.306311939856314,
68.306131684901));
#136549=CARTESIAN_POINT('Ctrl Pts',(132.447053549369,0.308402827782414,
65.942396934738));
#136550=CARTESIAN_POINT('Ctrl Pts',(134.292447465669,0.310751914886114,
63.363026900454));
#136551=CARTESIAN_POINT('Ctrl Pts',(135.902727419669,0.313393793906214,
60.63324875935));
#136552=CARTESIAN_POINT('Ctrl Pts',(136.924148492969,0.315444210411514,
58.59002833958));
#136553=CARTESIAN_POINT('Ctrl Pts',(137.445518530069,0.316570291628914,
57.48076137169));
#136554=CARTESIAN_POINT('Ctrl Pts',(137.517690719469,0.316725377312314,
57.32787172523));
#136555=CARTESIAN_POINT('Ctrl Pts',(94.5045898659691,-0.391944427092286,
80.474860038171));
#136556=CARTESIAN_POINT('Ctrl Pts',(96.7489959251691,-0.394461845619086,
80.079326957343));
#136557=CARTESIAN_POINT('Ctrl Pts',(101.071548853969,-0.399670518957686,
79.317433953307));
#136558=CARTESIAN_POINT('Ctrl Pts',(106.433267535669,-0.406985840309386,
78.373020946999));
#136559=CARTESIAN_POINT('Ctrl Pts',(110.069594033769,-0.412377925771286,
77.729798875547));
#136560=CARTESIAN_POINT('Ctrl Pts',(111.758480158269,-0.414989404441086,
77.434719128118));
#136561=CARTESIAN_POINT('Ctrl Pts',(112.472526008569,-0.416116539930086,
77.30617199322));
#136562=CARTESIAN_POINT('Ctrl Pts',(112.732216228169,-0.416506671346586,
77.263625252347));
#136563=CARTESIAN_POINT('Ctrl Pts',(112.993369304269,-0.417036659726086,
77.205783041926));
#136564=CARTESIAN_POINT('Ctrl Pts',(113.314294777669,-0.417503094204386,
77.132922464813));
#136565=CARTESIAN_POINT('Ctrl Pts',(114.600497973669,-0.419534148736686,
76.832518581053));
#136566=CARTESIAN_POINT('Ctrl Pts',(116.767017756869,-0.422893026034286,
76.234797701647));
#136567=CARTESIAN_POINT('Ctrl Pts',(120.749908756769,-0.428836605210586,
74.808474794112));
#136568=CARTESIAN_POINT('Ctrl Pts',(124.539140129969,-0.433883045948486,
72.8865424998045));
#136569=CARTESIAN_POINT('Ctrl Pts',(127.985466074869,-0.438134496061686,
70.422019976291));
#136570=CARTESIAN_POINT('Ctrl Pts',(130.357485033669,-0.441174799508086,
68.310135147826));
#136571=CARTESIAN_POINT('Ctrl Pts',(132.472991956769,-0.444336740905886,
65.941867636944));
#136572=CARTESIAN_POINT('Ctrl Pts',(134.317626905469,-0.447916848216786,
63.36094910574));
#136573=CARTESIAN_POINT('Ctrl Pts',(135.926029587169,-0.451965219963786,
60.63261837717));
#136574=CARTESIAN_POINT('Ctrl Pts',(136.945697916469,-0.455126418189086,
58.59256372079));
#136575=CARTESIAN_POINT('Ctrl Pts',(137.466114009069,-0.456868308193486,
57.48538563185));
#136576=CARTESIAN_POINT('Ctrl Pts',(137.538154739269,-0.457108150346786,
57.33278041094));
#136577=CARTESIAN_POINT('Ctrl Pts',(94.4917696614691,-1.62653903695399,
80.388080157788));
#136578=CARTESIAN_POINT('Ctrl Pts',(96.7251100426691,-1.64079859934899,
79.993118959704));
#136579=CARTESIAN_POINT('Ctrl Pts',(101.026458471769,-1.66878149008799,
79.2329765847));
#136580=CARTESIAN_POINT('Ctrl Pts',(106.361947261869,-1.70470855576399,
78.292262003841));
#136581=CARTESIAN_POINT('Ctrl Pts',(109.980616118269,-1.72972033570599,
77.652304985682));
#136582=CARTESIAN_POINT('Ctrl Pts',(111.660992166569,-1.74151397354599,
77.358869004343));
#136583=CARTESIAN_POINT('Ctrl Pts',(112.372181585169,-1.74654816345699,
77.231135964501));
#136584=CARTESIAN_POINT('Ctrl Pts',(112.628477516769,-1.74829694560499,
77.188621965177));
#136585=CARTESIAN_POINT('Ctrl Pts',(112.899581170269,-1.75058962364099,
77.132307511686));
#136586=CARTESIAN_POINT('Ctrl Pts',(113.217019764069,-1.75268289638599,
77.059556568771));
#136587=CARTESIAN_POINT('Ctrl Pts',(114.503042211069,-1.76167159692399,
76.761105443198));
#136588=CARTESIAN_POINT('Ctrl Pts',(116.668876258069,-1.77634825257999,
76.166361663691));
#136589=CARTESIAN_POINT('Ctrl Pts',(120.656347418569,-1.80169977690999,
74.744518803754));
#136590=CARTESIAN_POINT('Ctrl Pts',(124.454818894169,-1.82235294021599,
72.8236298001459));
#136591=CARTESIAN_POINT('Ctrl Pts',(127.907560783969,-1.83870632291999,
70.35800518595));
#136592=CARTESIAN_POINT('Ctrl Pts',(130.281095772069,-1.84979591424999,
68.246000480916));
#136593=CARTESIAN_POINT('Ctrl Pts',(132.394030826169,-1.86076654056799,
65.880166190254));
#136594=CARTESIAN_POINT('Ctrl Pts',(134.232064870669,-1.87277787282499,
63.307347157382));
#136595=CARTESIAN_POINT('Ctrl Pts',(135.831863833569,-1.88603586839099,
60.592619078));
#136596=CARTESIAN_POINT('Ctrl Pts',(136.844484227669,-1.89610879742999,
58.56638963221));
#136597=CARTESIAN_POINT('Ctrl Pts',(137.361072184969,-1.90157570216799,
57.46742495816));
#136598=CARTESIAN_POINT('Ctrl Pts',(137.432585302369,-1.90232921860299,
57.31594512813));
#136599=CARTESIAN_POINT('Ctrl Pts',(94.4309652584691,-3.97364311980699,
79.989330260271));
#136600=CARTESIAN_POINT('Ctrl Pts',(96.6215442512691,-4.01169264542499,
79.594451364535));
#136601=CARTESIAN_POINT('Ctrl Pts',(100.840786175369,-4.08465026300699,
78.836243627137));
#136602=CARTESIAN_POINT('Ctrl Pts',(106.074691078369,-4.17431672897299,
77.901971576044));
#136603=CARTESIAN_POINT('Ctrl Pts',(109.624729243069,-4.23483510476799,
77.268298018584));
#136604=CARTESIAN_POINT('Ctrl Pts',(111.272721866769,-4.26293361266799,
76.978069056252));
#136605=CARTESIAN_POINT('Ctrl Pts',(111.971449487369,-4.27484978147099,
76.851954396361));
#136606=CARTESIAN_POINT('Ctrl Pts',(112.219310861169,-4.27899269673599,
76.809543041334));
#136607=CARTESIAN_POINT('Ctrl Pts',(112.504070747669,-4.28434331979599,
76.75599781504));
#136608=CARTESIAN_POINT('Ctrl Pts',(112.812264044869,-4.28929908170699,
76.683735558641));
#136609=CARTESIAN_POINT('Ctrl Pts',(114.084082260069,-4.31044323461999,
76.389871123831));
#136610=CARTESIAN_POINT('Ctrl Pts',(116.225387968569,-4.34464562068499,
75.803524995651));
#136611=CARTESIAN_POINT('Ctrl Pts',(120.177534500969,-4.40262868470399,
74.399493491444));
#136612=CARTESIAN_POINT('Ctrl Pts',(123.950655853569,-4.44814620623399,
72.496847968071));
#136613=CARTESIAN_POINT('Ctrl Pts',(127.376994494769,-4.48208320683399,
70.051519337007));
#136614=CARTESIAN_POINT('Ctrl Pts',(129.727278560469,-4.50391800270399,
67.958092508844));
#136615=CARTESIAN_POINT('Ctrl Pts',(131.812162782869,-4.52449284930599,
65.616466683786));
#136616=CARTESIAN_POINT('Ctrl Pts',(133.616536214469,-4.54639756885499,
63.077404462912));
#136617=CARTESIAN_POINT('Ctrl Pts',(135.178848514569,-4.57011609389099,
60.40502284092));
#136618=CARTESIAN_POINT('Ctrl Pts',(136.162260621769,-4.58765299989899,
58.41602012162));
#136619=CARTESIAN_POINT('Ctrl Pts',(136.662957925869,-4.59700952188599,
57.33845516432));
#136620=CARTESIAN_POINT('Ctrl Pts',(136.732281158069,-4.59830067204899,
57.18991365398));
#136621=CARTESIAN_POINT('Ctrl Pts',(94.2946923201691,-6.70804124817899,
79.112010850242));
#136622=CARTESIAN_POINT('Ctrl Pts',(96.4018922775691,-6.77081804645399,
78.714410710852));
#136623=CARTESIAN_POINT('Ctrl Pts',(100.461102932469,-6.88895937391199,
77.954609507465));
#136624=CARTESIAN_POINT('Ctrl Pts',(105.497454600769,-7.02880980603999,
77.026576208225));
#136625=CARTESIAN_POINT('Ctrl Pts',(108.914058256569,-7.12055052930399,
76.400938200377));
#136626=CARTESIAN_POINT('Ctrl Pts',(110.499660565269,-7.16252676436099,
76.115032764168));
#136627=CARTESIAN_POINT('Ctrl Pts',(111.173165327269,-7.18021962643399,
75.991147187523));
#136628=CARTESIAN_POINT('Ctrl Pts',(111.408225108969,-7.18635419350799,
75.949001332739));
#136629=CARTESIAN_POINT('Ctrl Pts',(111.700693228269,-7.19430470928699,
75.898572630968));
#136630=CARTESIAN_POINT('Ctrl Pts',(111.994181897569,-7.20161151815999,
75.827463650124));
#136631=CARTESIAN_POINT('Ctrl Pts',(113.228310289369,-7.23275451518899,
75.540921750577));
#136632=CARTESIAN_POINT('Ctrl Pts',(115.305714966569,-7.28245852194699,
74.970021382884));
#136633=CARTESIAN_POINT('Ctrl Pts',(119.150002336769,-7.36432237457899,
73.6050086640061));
#136634=CARTESIAN_POINT('Ctrl Pts',(122.829165031769,-7.42430540347799,
71.754540381793));
#136635=CARTESIAN_POINT('Ctrl Pts',(126.167856447969,-7.46373591418299,
69.375045120244));
#136636=CARTESIAN_POINT('Ctrl Pts',(128.453230587369,-7.48631180618699,
67.33878584061));
#136637=CARTESIAN_POINT('Ctrl Pts',(130.472696968569,-7.50545576601199,
65.062710327142));
#136638=CARTESIAN_POINT('Ctrl Pts',(132.208627615269,-7.52508893813999,
62.59881514699));
#136639=CARTESIAN_POINT('Ctrl Pts',(133.698071052769,-7.54598850132699,
60.00898250641));
#136640=CARTESIAN_POINT('Ctrl Pts',(134.625480995269,-7.56064429820999,
58.0861089762));
#136641=CARTESIAN_POINT('Ctrl Pts',(135.095677359169,-7.56813519765099,
57.04564624104));
#136642=CARTESIAN_POINT('Ctrl Pts',(135.160797579369,-7.56917204693599,
56.90220721139));
#136643=CARTESIAN_POINT('Ctrl Pts',(94.0331412950691,-9.72819839798099,
77.461391565822));
#136644=CARTESIAN_POINT('Ctrl Pts',(96.0072255155691,-9.80312259694499,
77.061683166786));
#136645=CARTESIAN_POINT('Ctrl Pts',(99.8110683163691,-9.94225626317999,
76.303613526659));
#136646=CARTESIAN_POINT('Ctrl Pts',(104.532674733669,-10.10237277876,75.390554672224));
#136647=CARTESIAN_POINT('Ctrl Pts',(107.736774407169,-10.20506710756,74.780870036665));
#136648=CARTESIAN_POINT('Ctrl Pts',(109.223468801269,-10.25150545695,74.503201540156));
#136649=CARTESIAN_POINT('Ctrl Pts',(109.856025930669,-10.2709864892,74.383369290596));
#136650=CARTESIAN_POINT('Ctrl Pts',(110.073541803969,-10.27768940791,74.342100727107));
#136651=CARTESIAN_POINT('Ctrl Pts',(110.363390117669,-10.2866439161,74.29539812619));
#136652=CARTESIAN_POINT('Ctrl Pts',(110.636083672869,-10.29455426583,74.226981390702));
#136653=CARTESIAN_POINT('Ctrl Pts',(111.802366463169,-10.32851663231,73.9536960572392));
#136654=CARTESIAN_POINT('Ctrl Pts',(113.765631696269,-10.38176050765,73.4123027455414));
#136655=CARTESIAN_POINT('Ctrl Pts',(117.408936777569,-10.46588100582,72.1259277537728));
#136656=CARTESIAN_POINT('Ctrl Pts',(120.906767485869,-10.52044842901,70.388769104978));
#136657=CARTESIAN_POINT('Ctrl Pts',(124.083745239269,-10.54709619697,68.155531276342));
#136658=CARTESIAN_POINT('Ctrl Pts',(126.256740506469,-10.55719661026,66.243657042203));
#136659=CARTESIAN_POINT('Ctrl Pts',(128.171601052569,-10.56185077472,64.103935177044));
#136660=CARTESIAN_POINT('Ctrl Pts',(129.805209314969,-10.56596145084,61.7842775069));
#136661=CARTESIAN_POINT('Ctrl Pts',(131.187259144569,-10.57057132432,59.34216081812));
#136662=CARTESIAN_POINT('Ctrl Pts',(132.031680827369,-10.57263717675,57.53092481926));
#136663=CARTESIAN_POINT('Ctrl Pts',(132.456503474169,-10.57307296402,56.55202285407));
#136664=CARTESIAN_POINT('Ctrl Pts',(132.515372864869,-10.57313948151,56.4170597467));
#136665=CARTESIAN_POINT('Ctrl Pts',(93.6821615622691,-12.38223409115,75.27715826278));
#136666=CARTESIAN_POINT('Ctrl Pts',(95.5036033007691,-12.45177258484,74.883599759386));
#136667=CARTESIAN_POINT('Ctrl Pts',(99.0144766641691,-12.5802692937,74.142647600746));
#136668=CARTESIAN_POINT('Ctrl Pts',(103.374764814069,-12.72653556026,73.2619966330297));
#136669=CARTESIAN_POINT('Ctrl Pts',(106.334684719569,-12.81951619743,72.6790624888142));
#136670=CARTESIAN_POINT('Ctrl Pts',(107.707954093569,-12.86137745058,72.4142380691917));
#136671=CARTESIAN_POINT('Ctrl Pts',(108.292895990869,-12.87891347918,72.3004044412196));
#136672=CARTESIAN_POINT('Ctrl Pts',(108.492143327769,-12.88488451512,72.2607679061845));
#136673=CARTESIAN_POINT('Ctrl Pts',(108.768958348269,-12.89325414546,72.2179669987607));
#136674=CARTESIAN_POINT('Ctrl Pts',(109.019525278469,-12.90021960472,72.1537748655661));
#136675=CARTESIAN_POINT('Ctrl Pts',(110.102605128169,-12.93055535856,71.899044541544));
#136676=CARTESIAN_POINT('Ctrl Pts',(111.926525841569,-12.9773529257,71.399025133737));
#136677=CARTESIAN_POINT('Ctrl Pts',(115.320061967569,-13.04832119269,70.223065623371));
#136678=CARTESIAN_POINT('Ctrl Pts',(118.590293578969,-13.08784543436,68.64729371565));
#136679=CARTESIAN_POINT('Ctrl Pts',(121.570885042369,-13.09763726794,66.622368575163));
#136680=CARTESIAN_POINT('Ctrl Pts',(123.613187646469,-13.09445150359,64.885470371931));
#136681=CARTESIAN_POINT('Ctrl Pts',(125.413286174969,-13.08547415731,62.93331204737));
#136682=CARTESIAN_POINT('Ctrl Pts',(126.940103658769,-13.07597683247,60.80415135462));
#136683=CARTESIAN_POINT('Ctrl Pts',(128.210308454669,-13.06716939491,58.54935029097));
#136684=CARTESIAN_POINT('Ctrl Pts',(128.966948564269,-13.05967497397,56.8745529502));
#136685=CARTESIAN_POINT('Ctrl Pts',(129.343483874869,-13.05498314335,55.96997774857));
#136686=CARTESIAN_POINT('Ctrl Pts',(129.395703783069,-13.05434233444,55.84525666692));
#136687=CARTESIAN_POINT('Ctrl Pts',(93.2525522503691,-14.56494720251,72.6292784804675));
#136688=CARTESIAN_POINT('Ctrl Pts',(94.9099069943691,-14.61582723887,72.2566981640195));
#136689=CARTESIAN_POINT('Ctrl Pts',(98.1053359090691,-14.71078585591,71.558752332215));
#136690=CARTESIAN_POINT('Ctrl Pts',(102.075446269569,-14.8211612689,70.735832604723));
#136691=CARTESIAN_POINT('Ctrl Pts',(104.771012343469,-14.89256300333,70.193284594267));
#136692=CARTESIAN_POINT('Ctrl Pts',(106.021560527069,-14.92503651236,69.946645860606));
#136693=CARTESIAN_POINT('Ctrl Pts',(106.554407446069,-14.93870838161,69.840964041424));
#136694=CARTESIAN_POINT('Ctrl Pts',(106.735454910169,-14.9433096718,69.803778649846));
#136695=CARTESIAN_POINT('Ctrl Pts',(106.989614914069,-14.95016974445,69.765111926735));
#136696=CARTESIAN_POINT('Ctrl Pts',(107.217710549069,-14.95547553046,69.70673385112));
#136697=CARTESIAN_POINT('Ctrl Pts',(108.206162207169,-14.97909147355,69.476010576657));
#136698=CARTESIAN_POINT('Ctrl Pts',(109.872101016469,-15.01529544008,69.028920839883));
#136699=CARTESIAN_POINT('Ctrl Pts',(112.979053178569,-15.06915909587,67.992654212769));
#136700=CARTESIAN_POINT('Ctrl Pts',(115.986803650169,-15.09616756986,66.620973578397));
#136701=CARTESIAN_POINT('Ctrl Pts',(118.747134698169,-15.0978837308,64.858171703176));
#136702=CARTESIAN_POINT('Ctrl Pts',(120.648236384269,-15.09059048003,63.339220675778));
#136703=CARTESIAN_POINT('Ctrl Pts',(122.330929139869,-15.07917832172,61.61678074719));
#136704=CARTESIAN_POINT('Ctrl Pts',(123.753705899769,-15.06867596534,59.71388200454));
#136705=CARTESIAN_POINT('Ctrl Pts',(124.914541955869,-15.0603582609,57.67407819686));
#136706=CARTESIAN_POINT('Ctrl Pts',(125.583377083969,-15.05453785733,56.15087193636));
#136707=CARTESIAN_POINT('Ctrl Pts',(125.911215285669,-15.05112088214,55.32792490375));
#136708=CARTESIAN_POINT('Ctrl Pts',(125.956732969069,-15.05065234144,55.21446089957));
#136709=CARTESIAN_POINT('Ctrl Pts',(92.7615318988691,-16.20464967702,69.620536734241));
#136710=CARTESIAN_POINT('Ctrl Pts',(94.2482285258691,-16.23101253952,69.28827995804));
#136711=CARTESIAN_POINT('Ctrl Pts',(97.1146507180691,-16.28269288864,68.665777442556));
#136712=CARTESIAN_POINT('Ctrl Pts',(100.675648889369,-16.34879084479,67.928895074072));
#136713=CARTESIAN_POINT('Ctrl Pts',(103.092866435569,-16.39470354547,67.439878040069));
#136714=CARTESIAN_POINT('Ctrl Pts',(104.214137922869,-16.41636882877,67.215955123965));
#136715=CARTESIAN_POINT('Ctrl Pts',(104.691547007069,-16.42563822416,67.120132104085));
#136716=CARTESIAN_POINT('Ctrl Pts',(104.854874208569,-16.42872819769,67.086043494429));
#136717=CARTESIAN_POINT('Ctrl Pts',(105.077166774169,-16.43364643686,67.051562487782));
#136718=CARTESIAN_POINT('Ctrl Pts',(105.282954985669,-16.43718598195,67.000347697702));
#136719=CARTESIAN_POINT('Ctrl Pts',(106.167370916869,-16.4533828966,66.798047782311));
#136720=CARTESIAN_POINT('Ctrl Pts',(107.659994694069,-16.47861830463,66.413110357911));
#136721=CARTESIAN_POINT('Ctrl Pts',(110.449346482569,-16.51753051004,65.539506830122));
#136722=CARTESIAN_POINT('Ctrl Pts',(113.164900595469,-16.5391631641,64.405441646321));
#136723=CARTESIAN_POINT('Ctrl Pts',(115.685632177769,-16.54470350357,62.94652020938));
#136724=CARTESIAN_POINT('Ctrl Pts',(117.438110061369,-16.54407453157,61.67801064453));
#136725=CARTESIAN_POINT('Ctrl Pts',(119.003522973169,-16.54227130612,60.2155314398));
#136726=CARTESIAN_POINT('Ctrl Pts',(120.327462124369,-16.54346569086,58.56130716037));
#136727=CARTESIAN_POINT('Ctrl Pts',(121.383545670869,-16.54890359416,56.7494057631));
#136728=CARTESIAN_POINT('Ctrl Pts',(121.965858310969,-16.55497485232,55.38123587483));
#136729=CARTESIAN_POINT('Ctrl Pts',(122.245228728369,-16.55854218877,54.6406482838));
#136730=CARTESIAN_POINT('Ctrl Pts',(122.284080188769,-16.55903132032,54.53855286788));
#136731=CARTESIAN_POINT('Ctrl Pts',(92.3160179092691,-17.05845633753,66.898897397011));
#136732=CARTESIAN_POINT('Ctrl Pts',(93.6568424647691,-17.06736861268,66.616905163633));
#136733=CARTESIAN_POINT('Ctrl Pts',(96.2410780501691,-17.08777775176,66.084296328605));
#136734=CARTESIAN_POINT('Ctrl Pts',(99.4489334442691,-17.12067117079,65.440189739954));
#136735=CARTESIAN_POINT('Ctrl Pts',(101.624696234569,-17.14672195508,65.003809046661));
#136736=CARTESIAN_POINT('Ctrl Pts',(102.633720717169,-17.15974422671,64.800948051197));
#136737=CARTESIAN_POINT('Ctrl Pts',(103.062536021769,-17.16544430497,64.714017968606));
#136738=CARTESIAN_POINT('Ctrl Pts',(103.211636753469,-17.16734450314,64.682771588846));
#136739=CARTESIAN_POINT('Ctrl Pts',(103.399836092569,-17.17046418614,64.651541526049));
#136740=CARTESIAN_POINT('Ctrl Pts',(103.587344926369,-17.17265333749,64.60706354595));
#136741=CARTESIAN_POINT('Ctrl Pts',(104.377911634569,-17.18284853984,64.430665787025));
#136742=CARTESIAN_POINT('Ctrl Pts',(105.714438850969,-17.19933510361,64.102439610754));
#136743=CARTESIAN_POINT('Ctrl Pts',(108.215174535469,-17.22692014645,63.377387806248));
#136744=CARTESIAN_POINT('Ctrl Pts',(110.664078907169,-17.24638005472,62.4617307178));
#136745=CARTESIAN_POINT('Ctrl Pts',(112.970350336469,-17.25840009369,61.2819001994));
#136746=CARTESIAN_POINT('Ctrl Pts',(114.593636762369,-17.26584272015,60.24176555596));
#136747=CARTESIAN_POINT('Ctrl Pts',(116.062124964169,-17.27413543879,59.01301835956));
#136748=CARTESIAN_POINT('Ctrl Pts',(117.308594600169,-17.28622002581,57.57589495172));
#136749=CARTESIAN_POINT('Ctrl Pts',(118.281647748769,-17.30325651225,55.95516825802));
#136750=CARTESIAN_POINT('Ctrl Pts',(118.793119890869,-17.31878215848,54.71170764927));
#136751=CARTESIAN_POINT('Ctrl Pts',(119.032366787569,-17.32781681205,54.03627261275));
#136752=CARTESIAN_POINT('Ctrl Pts',(119.065703705269,-17.329056353,53.94318115434));
#136753=CARTESIAN_POINT('Ctrl Pts',(91.9339282292691,-17.4341963447,64.566704269957));
#136754=CARTESIAN_POINT('Ctrl Pts',(93.1521736193691,-17.43521999266,64.333201342115));
#136755=CARTESIAN_POINT('Ctrl Pts',(95.4987864019691,-17.43932140529,63.88538165894));
#136756=CARTESIAN_POINT('Ctrl Pts',(98.4081188271691,-17.4493281509,63.323852177671));
#136757=CARTESIAN_POINT('Ctrl Pts',(100.379158684869,-17.45848054895,62.93137508751));
#136758=CARTESIAN_POINT('Ctrl Pts',(101.292974475169,-17.46329630395,62.7451797869));
#136759=CARTESIAN_POINT('Ctrl Pts',(101.680293297669,-17.46544498611,62.66516022947));
#136760=CARTESIAN_POINT('Ctrl Pts',(101.818048062769,-17.46615169702,62.63611238732));
#136761=CARTESIAN_POINT('Ctrl Pts',(101.973349896169,-17.46740733325,62.60711074564));
#136762=CARTESIAN_POINT('Ctrl Pts',(102.146036955169,-17.46821299911,62.56830582003));
#136763=CARTESIAN_POINT('Ctrl Pts',(102.854852085869,-17.47209930056,62.41320992242));
#136764=CARTESIAN_POINT('Ctrl Pts',(104.055600475469,-17.47846541605,62.1325348399));
#136765=CARTESIAN_POINT('Ctrl Pts',(106.303934729469,-17.4893232793,61.53434726652));
#136766=CARTESIAN_POINT('Ctrl Pts',(108.519326841369,-17.49710260775,60.80864805725));
#136767=CARTESIAN_POINT('Ctrl Pts',(110.640815547969,-17.50195369933,59.87303699715));
#136768=CARTESIAN_POINT('Ctrl Pts',(112.155484622169,-17.50507153116,59.03228889222));
#136769=CARTESIAN_POINT('Ctrl Pts',(113.546077712669,-17.50880752966,58.00598025268));
#136770=CARTESIAN_POINT('Ctrl Pts',(114.733439685769,-17.51475423024,56.75316932502));
#136771=CARTESIAN_POINT('Ctrl Pts',(115.642433562169,-17.52398002372,55.29003282689));
#136772=CARTESIAN_POINT('Ctrl Pts',(116.097511363769,-17.53322921597,54.14607296181));
#136773=CARTESIAN_POINT('Ctrl Pts',(116.304500203969,-17.53882514575,53.52193271673));
#136774=CARTESIAN_POINT('Ctrl Pts',(116.333406458469,-17.53959102319,53.43593682679));
#136775=CARTESIAN_POINT('Ctrl Pts',(91.7332982817691,-17.50195372971,63.342887103518));
#136776=CARTESIAN_POINT('Ctrl Pts',(92.8878681996691,-17.50179983727,63.135222319627));
#136777=CARTESIAN_POINT('Ctrl Pts',(95.1109254058691,-17.50192227436,62.73200794642));
#136778=CARTESIAN_POINT('Ctrl Pts',(97.8647643030691,-17.50290970614,62.21234046008));
#136779=CARTESIAN_POINT('Ctrl Pts',(99.7290153100691,-17.50390275863,61.84108070543));
#136780=CARTESIAN_POINT('Ctrl Pts',(100.593172064669,-17.50443116352,61.66256696193));
#136781=CARTESIAN_POINT('Ctrl Pts',(100.958742773169,-17.50466844116,61.585695238));
#136782=CARTESIAN_POINT('Ctrl Pts',(101.090860291969,-17.50473393574,61.55763501945));
#136783=CARTESIAN_POINT('Ctrl Pts',(101.227465085569,-17.50493912834,61.52952220183));
#136784=CARTESIAN_POINT('Ctrl Pts',(101.392690067069,-17.50499758326,61.49357700272));
#136785=CARTESIAN_POINT('Ctrl Pts',(102.058053275069,-17.50539027309,61.3490168858));
#136786=CARTESIAN_POINT('Ctrl Pts',(103.186735740569,-17.50590773878,61.09253083144));
#136787=CARTESIAN_POINT('Ctrl Pts',(105.300699706669,-17.50624097075,60.56055645071));
#136788=CARTESIAN_POINT('Ctrl Pts',(107.391848487069,-17.50516827901,59.93616891045));
#136789=CARTESIAN_POINT('Ctrl Pts',(109.416461786669,-17.50251851211,59.13193578514));
#136790=CARTESIAN_POINT('Ctrl Pts',(110.875433230569,-17.49995815976,58.39852460632));
#136791=CARTESIAN_POINT('Ctrl Pts',(112.227768617769,-17.49718667402,57.48085879437));
#136792=CARTESIAN_POINT('Ctrl Pts',(113.387641718569,-17.4949747375,56.32592812353));
#136793=CARTESIAN_POINT('Ctrl Pts',(114.266500764269,-17.4943355846,54.94512241615));
#136794=CARTESIAN_POINT('Ctrl Pts',(114.694184237269,-17.49556162849,53.8521807202));
#136795=CARTESIAN_POINT('Ctrl Pts',(114.885356344869,-17.49666826989,53.25414284847));
#136796=CARTESIAN_POINT('Ctrl Pts',(114.912091474169,-17.49681664757,53.17175964758));
#136797=CARTESIAN_POINT('Ctrl Pts',(91.6256651679691,-17.50087323455,62.6865987037));
#136798=CARTESIAN_POINT('Ctrl Pts',(92.7462347895691,-17.50094842656,62.49253283427));
#136799=CARTESIAN_POINT('Ctrl Pts',(94.9032917810691,-17.50020019636,62.11262574012));
#136800=CARTESIAN_POINT('Ctrl Pts',(97.5740108379691,-17.49697626082,61.61434289845));
#136801=CARTESIAN_POINT('Ctrl Pts',(99.3811417969691,-17.49355583457,61.25357815157));
#136802=CARTESIAN_POINT('Ctrl Pts',(100.218740387169,-17.49165921143,61.07872701066));
#136803=CARTESIAN_POINT('Ctrl Pts',(100.572648403969,-17.49079874116,61.0033456655));
#136804=CARTESIAN_POINT('Ctrl Pts',(100.701837613969,-17.49049444435,60.97574535699));
#136805=CARTESIAN_POINT('Ctrl Pts',(100.827969879369,-17.49009249956,60.94800687329));
#136806=CARTESIAN_POINT('Ctrl Pts',(100.989287633669,-17.48971654682,60.91354003403));
#136807=CARTESIAN_POINT('Ctrl Pts',(101.631166208969,-17.48806898008,60.77435960452));
#136808=CARTESIAN_POINT('Ctrl Pts',(102.720935232469,-17.48508413693,60.5305219036));
#136809=CARTESIAN_POINT('Ctrl Pts',(104.762242093969,-17.47881650364,60.03389490008));
#136810=CARTESIAN_POINT('Ctrl Pts',(106.786272863569,-17.47167663677,59.46446863206));
#136811=CARTESIAN_POINT('Ctrl Pts',(108.759059563469,-17.46330836921,58.73198247683));
#136812=CARTESIAN_POINT('Ctrl Pts',(110.188668690969,-17.45621320481,58.05726949414));
#136813=CARTESIAN_POINT('Ctrl Pts',(111.521433399769,-17.44821259642,57.19897765626));
#136814=CARTESIAN_POINT('Ctrl Pts',(112.667811977369,-17.43960128686,56.09731370129));
#136815=CARTESIAN_POINT('Ctrl Pts',(113.531742275669,-17.43136124665,54.76100557254));
#136816=CARTESIAN_POINT('Ctrl Pts',(113.945520944869,-17.42641977624,53.69542143466));
#136817=CARTESIAN_POINT('Ctrl Pts',(114.128610933769,-17.42406662281,53.11133790473));
#136818=CARTESIAN_POINT('Ctrl Pts',(114.154237126469,-17.42373918761,53.03088647436));
#136819=CARTESIAN_POINT('',(114.384013244638,-17.4511073706868,53.3319431971496));
#136820=CARTESIAN_POINT('Ctrl Pts',(114.384012850693,-17.4511074291882,
53.3319430705208));
#136821=CARTESIAN_POINT('Ctrl Pts',(114.220888472494,-17.4519988842083,
53.8398358110967));
#136822=CARTESIAN_POINT('Ctrl Pts',(113.829481233474,-17.4543725662864,
54.8352104074227));
#136823=CARTESIAN_POINT('Ctrl Pts',(112.960679338991,-17.4596410224806,
56.1902373905027));
#136824=CARTESIAN_POINT('Ctrl Pts',(111.808327125295,-17.4657668375024,
57.3134151931793));
#136825=CARTESIAN_POINT('Ctrl Pts',(110.467194168512,-17.4717374796403,
58.1951861692835));
#136826=CARTESIAN_POINT('Ctrl Pts',(109.028402063985,-17.4770568190849,
58.8957505557642));
#136827=CARTESIAN_POINT('Ctrl Pts',(107.031015069744,-17.4832149765507,
59.6550380994632));
#136828=CARTESIAN_POINT('Ctrl Pts',(104.468739305416,-17.4891377436966,
60.3958819176082));
#136829=CARTESIAN_POINT('Ctrl Pts',(101.35178149711,-17.4940454558258,61.1211273764285));
#136830=CARTESIAN_POINT('Ctrl Pts',(98.2162369710537,-17.4971942144887,
61.7585815172283));
#136831=CARTESIAN_POINT('Ctrl Pts',(95.071694526759,-17.4989202182121,62.3491703657761));
#136832=CARTESIAN_POINT('Ctrl Pts',(92.9717518845374,-17.4992596243613,
62.7235663753691));
#136833=CARTESIAN_POINT('Ctrl Pts',(91.9214475326691,-17.49925970194,62.90875755409));
#136834=CARTESIAN_POINT('',(137.305407436204,-9.29834912769915E-12,57.7874348564604));
#136835=CARTESIAN_POINT('Ctrl Pts',(137.305407436201,-9.29561982943028E-12,
57.7874348564612));
#136836=CARTESIAN_POINT('Ctrl Pts',(137.305407495695,-1.34472964465863,
57.7874347379193));
#136837=CARTESIAN_POINT('Ctrl Pts',(137.075117022675,-2.66554501472644,
57.7426704534051));
#136838=CARTESIAN_POINT('Ctrl Pts',(136.207322767474,-5.20088375491933,
57.5739872507397));
#136839=CARTESIAN_POINT('Ctrl Pts',(135.580897995914,-6.39181951377924,
57.4522218871268));
#136840=CARTESIAN_POINT('Ctrl Pts',(133.336328816589,-9.6643571443166,57.0159193422835));
#136841=CARTESIAN_POINT('Ctrl Pts',(131.322433877513,-11.5113308194662,
56.624455689254));
#136842=CARTESIAN_POINT('Ctrl Pts',(127.008689974315,-14.4665207294624,
55.7859443455056));
#136843=CARTESIAN_POINT('Ctrl Pts',(124.584096632227,-15.6695033005887,
55.314648673862));
#136844=CARTESIAN_POINT('Ctrl Pts',(118.850738143645,-17.5212377256219,
54.2001909378701));
#136845=CARTESIAN_POINT('Ctrl Pts',(116.347111372697,-17.6025946223322,
53.7135327557499));
#136846=CARTESIAN_POINT('Ctrl Pts',(114.384013344373,-17.4511059084411,
53.3319432645659));
#136847=CARTESIAN_POINT('Ctrl Pts',(95.0009770511696,1.41900380334903E-14,
80.3736373255327));
#136848=CARTESIAN_POINT('Ctrl Pts',(97.0803868675694,1.61737654382892E-12,
80.0069812709578));
#136849=CARTESIAN_POINT('Ctrl Pts',(99.1597966839195,1.75226639535239E-10,
79.6403252163851));
#136850=CARTESIAN_POINT('Ctrl Pts',(101.239237748174,2.37870695363185E-10,
79.2738274979082));
#136851=CARTESIAN_POINT('Ctrl Pts',(103.318678812429,3.00514713466124E-10,
78.9073297794313));
#136852=CARTESIAN_POINT('Ctrl Pts',(105.398151124589,2.52193602934045E-10,
78.5409903970502));
#136853=CARTESIAN_POINT('Ctrl Pts',(107.477432973366,2.43303190095023E-10,
78.1736859184611));
#136854=CARTESIAN_POINT('Ctrl Pts',(108.517073897755,2.38858067986138E-10,
77.9900336791664));
#136855=CARTESIAN_POINT('Ctrl Pts',(109.556667206299,2.44270592801756E-10,
77.8061401658197));
#136856=CARTESIAN_POINT('Ctrl Pts',(110.596551246173,2.46179396312662E-10,
77.6237198161581));
#136857=CARTESIAN_POINT('Ctrl Pts',(111.116493266109,2.4713382950139E-10,
77.5325096413276));
#136858=CARTESIAN_POINT('Ctrl Pts',(111.636507968877,2.47212066916387E-10,
77.4416677574185));
#136859=CARTESIAN_POINT('Ctrl Pts',(112.156094597342,2.47661648133946E-10,
77.3486567797055));
#136860=CARTESIAN_POINT('Ctrl Pts',(112.285991254459,2.4777404800645E-10,
77.3254040352771));
#136861=CARTESIAN_POINT('Ctrl Pts',(112.415861156932,2.47909381658537E-10,
77.3020157224859));
#136862=CARTESIAN_POINT('Ctrl Pts',(112.54601291089,2.48033642236134E-10,
77.2800555834686));
#136863=CARTESIAN_POINT('Ctrl Pts',(112.611088787869,2.48095820884867E-10,
77.2690755139599));
#136864=CARTESIAN_POINT('Ctrl Pts',(112.67623512772,2.48153283270535E-10,
77.2584524878953));
#136865=CARTESIAN_POINT('Ctrl Pts',(112.740991784632,2.48221304621765E-10,
77.2458558104383));
#136866=CARTESIAN_POINT('Ctrl Pts',(112.805748441545,2.4828932697814E-10,
77.2332591329813));
#136867=CARTESIAN_POINT('Ctrl Pts',(112.870115415519,2.48376480234793E-10,
77.2186888041303));
#136868=CARTESIAN_POINT('Ctrl Pts',(112.934479385948,2.48448171757953E-10,
77.2041226313424));
#136869=CARTESIAN_POINT('Ctrl Pts',(113.063207326806,2.48591558390765E-10,
77.1749902857666));
#136870=CARTESIAN_POINT('Ctrl Pts',(113.191923253486,2.4870328328373E-10,
77.1458745644437));
#136871=CARTESIAN_POINT('Ctrl Pts',(113.320527988354,2.48823461834746E-10,
77.1162858196239));
#136872=CARTESIAN_POINT('Ctrl Pts',(113.44913272322,2.48943552136221E-10,
77.0866970748045));
#136873=CARTESIAN_POINT('Ctrl Pts',(113.577626266275,2.49064188873619E-10,
77.0566353064879));
#136874=CARTESIAN_POINT('Ctrl Pts',(113.705989992107,2.49189731349464E-10,
77.0260066290821));
#136875=CARTESIAN_POINT('Ctrl Pts',(114.732899798777,2.50194018712686E-10,
76.7809772098333));
#136876=CARTESIAN_POINT('Ctrl Pts',(115.751501303018,2.51147685891077E-10,
76.4996656091634));
#136877=CARTESIAN_POINT('Ctrl Pts',(116.75796074466,2.52056604754802E-10,
76.1808266875528));
#136878=CARTESIAN_POINT('Ctrl Pts',(117.7644201863,2.52965460192699E-10,
75.8619877659428));
#136879=CARTESIAN_POINT('Ctrl Pts',(118.758737566024,2.53960974327935E-10,
75.5056215220171));
#136880=CARTESIAN_POINT('Ctrl Pts',(119.736805721593,2.54712154146297E-10,
75.1081300375498));
#136881=CARTESIAN_POINT('Ctrl Pts',(121.692942032732,2.56214528961853E-10,
74.3131470686145));
#136882=CARTESIAN_POINT('Ctrl Pts',(123.58408144016,2.56831564688639E-10,
73.3536631749867));
#136883=CARTESIAN_POINT('Ctrl Pts',(125.361375841541,2.59188642770525E-10,
72.2138533985717));
#136884=CARTESIAN_POINT('Ctrl Pts',(126.250023042232,2.60367181450065E-10,
71.6439485103637));
#136885=CARTESIAN_POINT('Ctrl Pts',(127.110208988119,2.6077903821463E-10,
71.0289621207599));
#136886=CARTESIAN_POINT('Ctrl Pts',(127.935165389,2.61042402971423E-10,
70.3700832646172));
#136887=CARTESIAN_POINT('Ctrl Pts',(128.760121789881,2.6130574685733E-10,
69.7112044084745));
#136888=CARTESIAN_POINT('Ctrl Pts',(129.549848682753,2.59856007144552E-10,
69.0084331956421));
#136889=CARTESIAN_POINT('Ctrl Pts',(130.2970945887,2.6277636316907E-10,
68.262834677594));
#136890=CARTESIAN_POINT('Ctrl Pts',(131.044340494645,2.65696716392728E-10,
67.5172361595471));
#136891=CARTESIAN_POINT('Ctrl Pts',(131.749105184572,2.65887614767794E-10,
66.728809956919));
#136892=CARTESIAN_POINT('Ctrl Pts',(132.408971868912,2.64547238282287E-10,
65.9046542110124));
#136893=CARTESIAN_POINT('Ctrl Pts',(133.068838553253,2.6320681047808E-10,
65.0804984651044));
#136894=CARTESIAN_POINT('Ctrl Pts',(133.683808222283,2.53115900951374E-10,
64.2206142302005));
#136895=CARTESIAN_POINT('Ctrl Pts',(134.259531000955,2.6650029405495E-10,
63.3358425354513));
#136896=CARTESIAN_POINT('Ctrl Pts',(134.835253779626,2.79884673425092E-10,
62.4510708407035));
#136897=CARTESIAN_POINT('Ctrl Pts',(135.371726233848,3.59572997301272E-10,
61.5414091247388));
#136898=CARTESIAN_POINT('Ctrl Pts',(135.876171533849,2.68671404568543E-10,
60.6140360578227));
#136899=CARTESIAN_POINT('Ctrl Pts',(136.380640904218,1.77765306356043E-10,
59.6866187399019));
#136900=CARTESIAN_POINT('Ctrl Pts',(136.853086992978,-1.4415087307438E-11,
58.7414924351101));
#136901=CARTESIAN_POINT('Ctrl Pts',(137.305407436203,-9.30262811227323E-12,
57.7874348564578));
#136902=CARTESIAN_POINT('Ctrl Pts',(94.5010623932691,-0.271390781348986,
80.458309380968));
#136903=CARTESIAN_POINT('Ctrl Pts',(96.7480690176691,-0.273303947139986,
80.062047787126));
#136904=CARTESIAN_POINT('Ctrl Pts',(101.075636752369,-0.277194096347286,
79.29887180002));
#136905=CARTESIAN_POINT('Ctrl Pts',(106.443694627169,-0.282506136256786,
78.353143760582));
#136906=CARTESIAN_POINT('Ctrl Pts',(110.084318928469,-0.286355612428486,
77.709147582895));
#136907=CARTESIAN_POINT('Ctrl Pts',(111.775395884169,-0.288205612061686,
77.413752047541));
#136908=CARTESIAN_POINT('Ctrl Pts',(112.489943115269,-0.289001571345486,
77.285031202788));
#136909=CARTESIAN_POINT('Ctrl Pts',(112.751174957869,-0.289277354245586,
77.24256781598));
#136910=CARTESIAN_POINT('Ctrl Pts',(113.006167806469,-0.289648295947586,
77.183976117084));
#136911=CARTESIAN_POINT('Ctrl Pts',(113.328591569869,-0.289978123700586,
77.111221172032));
#136912=CARTESIAN_POINT('Ctrl Pts',(114.612842569469,-0.291408688849486,
76.810398162822));
#136913=CARTESIAN_POINT('Ctrl Pts',(116.776314258869,-0.293766007124886,
76.212440656571));
#136914=CARTESIAN_POINT('Ctrl Pts',(120.750299752669,-0.297909406378086,
74.787245547999));
#136915=CARTESIAN_POINT('Ctrl Pts',(124.528351940669,-0.301388008002886,
72.8698599141694));
#136916=CARTESIAN_POINT('Ctrl Pts',(127.965747941769,-0.304271372086086,
70.412480258316));
#136917=CARTESIAN_POINT('Ctrl Pts',(130.333310718269,-0.306306076964386,
68.306131716301));
#136918=CARTESIAN_POINT('Ctrl Pts',(132.447053752769,-0.308396923690086,
65.942396930586));
#136919=CARTESIAN_POINT('Ctrl Pts',(134.292447663169,-0.310745964288386,
63.363026884157));
#136920=CARTESIAN_POINT('Ctrl Pts',(135.902727602469,-0.313387790833686,
60.63324875441));
#136921=CARTESIAN_POINT('Ctrl Pts',(136.924194019969,-0.315438257512286,
58.58993762679));
#136922=CARTESIAN_POINT('Ctrl Pts',(137.445604913769,-0.316564411408386,
57.48057796111));
#136923=CARTESIAN_POINT('Ctrl Pts',(137.517820678669,-0.316719586679086,
57.32759679869));
#136924=CARTESIAN_POINT('Ctrl Pts',(94.5045868697691,0.391947887872814,
80.474860316371));
#136925=CARTESIAN_POINT('Ctrl Pts',(96.7489938846691,0.394465340288714,
80.079327063307));
#136926=CARTESIAN_POINT('Ctrl Pts',(101.071547740669,0.399674078560414,
79.317433890141));
#136927=CARTESIAN_POINT('Ctrl Pts',(106.433267335469,0.406989481539114,
78.3730207204));
#136928=CARTESIAN_POINT('Ctrl Pts',(110.069593784169,0.412381622051114,
77.729798658109));
#136929=CARTESIAN_POINT('Ctrl Pts',(111.758479884769,0.414993126484714,
77.434718915293));
#136930=CARTESIAN_POINT('Ctrl Pts',(112.472525726969,0.416120272936414,
77.306171782679));
#136931=CARTESIAN_POINT('Ctrl Pts',(112.732215937069,0.416510408165114,
77.263625041898));
#136932=CARTESIAN_POINT('Ctrl Pts',(112.993369041169,0.417040401490514,
77.205782835764));
#136933=CARTESIAN_POINT('Ctrl Pts',(113.314294504769,0.417506840533414,
77.132922258958));
#136934=CARTESIAN_POINT('Ctrl Pts',(114.600497700269,0.419537914587914,
76.832518380677));
#136935=CARTESIAN_POINT('Ctrl Pts',(116.767017481569,0.422896823641614,
76.234797509625));
#136936=CARTESIAN_POINT('Ctrl Pts',(120.749908494269,0.428840457273914,
74.808474614661));
#136937=CARTESIAN_POINT('Ctrl Pts',(124.539139893469,0.433886941802114,
72.88654232328));
#136938=CARTESIAN_POINT('Ctrl Pts',(127.985465856269,0.438138425871614,
70.422019796674));
#136939=CARTESIAN_POINT('Ctrl Pts',(130.357484819269,0.441178751903214,
68.310134967873));
#136940=CARTESIAN_POINT('Ctrl Pts',(132.472991735269,0.444340715211014,
65.941867463818));
#136941=CARTESIAN_POINT('Ctrl Pts',(134.317626665369,0.447920846178814,
63.360948955341));
#136942=CARTESIAN_POINT('Ctrl Pts',(135.926029322969,0.451969243766714,
60.63261826494));
#136943=CARTESIAN_POINT('Ctrl Pts',(136.945742912569,0.455130601764614,
58.59247305525));
#136944=CARTESIAN_POINT('Ctrl Pts',(137.466199778869,0.456872649911514,
57.48520248006));
#136945=CARTESIAN_POINT('Ctrl Pts',(137.538284005369,0.457112636783714,
57.33250591017));
#136946=CARTESIAN_POINT('Ctrl Pts',(94.4917666714691,1.62654072710201,80.388080388391));
#136947=CARTESIAN_POINT('Ctrl Pts',(96.7251080033691,1.64080031285201,79.993119016481));
#136948=CARTESIAN_POINT('Ctrl Pts',(101.026457354669,1.66878324250101,79.232976468964));
#136949=CARTESIAN_POINT('Ctrl Pts',(106.361947052669,1.70471035391701,78.292261719665));
#136950=CARTESIAN_POINT('Ctrl Pts',(109.980615859169,1.72972215971201,77.652304706081));
#136951=CARTESIAN_POINT('Ctrl Pts',(111.660991883869,1.74151580942401,77.358868727078));
#136952=CARTESIAN_POINT('Ctrl Pts',(112.372181293369,1.74655000434601,77.231135688414));
#136953=CARTESIAN_POINT('Ctrl Pts',(112.628477218869,1.74829878823701,77.188621689165));
#136954=CARTESIAN_POINT('Ctrl Pts',(112.899580882369,1.75059146850001,77.13230723769));
#136955=CARTESIAN_POINT('Ctrl Pts',(113.217019469369,1.75268474332801,77.059556295131));
#136956=CARTESIAN_POINT('Ctrl Pts',(114.503041906069,1.76167345271701,76.761105172898));
#136957=CARTESIAN_POINT('Ctrl Pts',(116.668875935169,1.77635012259001,76.166361399505));
#136958=CARTESIAN_POINT('Ctrl Pts',(120.656347069869,1.80170167067901,74.744518552537));
#136959=CARTESIAN_POINT('Ctrl Pts',(124.454818527069,1.82235485208901,72.8236295622119));
#136960=CARTESIAN_POINT('Ctrl Pts',(127.907560397669,1.83870824759601,70.358004962794));
#136961=CARTESIAN_POINT('Ctrl Pts',(130.281095368769,1.84979784675001,68.246000271287));
#136962=CARTESIAN_POINT('Ctrl Pts',(132.394030402469,1.86076848006101,65.880165998251));
#136963=CARTESIAN_POINT('Ctrl Pts',(134.232064422569,1.87277981952201,63.307346989957));
#136964=CARTESIAN_POINT('Ctrl Pts',(135.831863358169,1.88603782270401,60.59261894141));
#136965=CARTESIAN_POINT('Ctrl Pts',(136.844528698069,1.89611120448401,58.56629954457));
#136966=CARTESIAN_POINT('Ctrl Pts',(137.361157107969,1.90157856884701,57.46724312117));
#136967=CARTESIAN_POINT('Ctrl Pts',(137.432713405869,1.90233253674001,57.3156726068));
#136968=CARTESIAN_POINT('Ctrl Pts',(94.4309623691691,3.97364306962101,79.989330781101));
#136969=CARTESIAN_POINT('Ctrl Pts',(96.6215423249691,4.01169261211601,79.594451710704));
#136970=CARTESIAN_POINT('Ctrl Pts',(100.840785212069,4.08465024650501,78.836243799081));
#136971=CARTESIAN_POINT('Ctrl Pts',(106.074691078369,4.17431672897301,77.901971576044));
#136972=CARTESIAN_POINT('Ctrl Pts',(109.624729243069,4.23483510476801,77.268298018584));
#136973=CARTESIAN_POINT('Ctrl Pts',(111.272721866769,4.26293361266801,76.978069056252));
#136974=CARTESIAN_POINT('Ctrl Pts',(111.971449487369,4.27484978147101,76.851954396361));
#136975=CARTESIAN_POINT('Ctrl Pts',(112.219310861169,4.27899269673601,76.809543041334));
#136976=CARTESIAN_POINT('Ctrl Pts',(112.504070747669,4.28434331979601,76.75599781504));
#136977=CARTESIAN_POINT('Ctrl Pts',(112.812264044869,4.28929908170701,76.683735558641));
#136978=CARTESIAN_POINT('Ctrl Pts',(114.084082260069,4.31044323462001,76.389871123831));
#136979=CARTESIAN_POINT('Ctrl Pts',(116.225387968569,4.34464562068501,75.803524995651));
#136980=CARTESIAN_POINT('Ctrl Pts',(120.177534500969,4.40262868470401,74.399493491444));
#136981=CARTESIAN_POINT('Ctrl Pts',(123.950655853569,4.44814620623401,72.496847968071));
#136982=CARTESIAN_POINT('Ctrl Pts',(127.376994494769,4.48208320683401,70.051519337007));
#136983=CARTESIAN_POINT('Ctrl Pts',(129.727278560469,4.50391800270401,67.958092508844));
#136984=CARTESIAN_POINT('Ctrl Pts',(131.812162782869,4.52449284930601,65.616466683786));
#136985=CARTESIAN_POINT('Ctrl Pts',(133.616536214469,4.54639756885501,63.077404462912));
#136986=CARTESIAN_POINT('Ctrl Pts',(135.178848514569,4.57011609389101,60.40502284092));
#136987=CARTESIAN_POINT('Ctrl Pts',(136.162304291869,4.58765377865501,58.41593179657));
#136988=CARTESIAN_POINT('Ctrl Pts',(136.663040729269,4.59701106923501,57.33827696026));
#136989=CARTESIAN_POINT('Ctrl Pts',(136.732405833069,4.59830299412501,57.18964650883));
#136990=CARTESIAN_POINT('Ctrl Pts',(94.2946895408691,6.70804116537901,79.112011374661));
#136991=CARTESIAN_POINT('Ctrl Pts',(96.4018904242691,6.77081799251501,78.714411057748));
#136992=CARTESIAN_POINT('Ctrl Pts',(100.461102005569,6.88895934817401,77.954609678261));
#136993=CARTESIAN_POINT('Ctrl Pts',(105.497454600769,7.02880980604001,77.026576208225));
#136994=CARTESIAN_POINT('Ctrl Pts',(108.914058256569,7.12055052930401,76.400938200377));
#136995=CARTESIAN_POINT('Ctrl Pts',(110.499660565269,7.16252676436101,76.115032764168));
#136996=CARTESIAN_POINT('Ctrl Pts',(111.173165327269,7.18021962643401,75.991147187523));
#136997=CARTESIAN_POINT('Ctrl Pts',(111.408225108969,7.18635419350801,75.949001332739));
#136998=CARTESIAN_POINT('Ctrl Pts',(111.700693228269,7.19430470928701,75.898572630968));
#136999=CARTESIAN_POINT('Ctrl Pts',(111.994181897569,7.20161151816001,75.827463650124));
#137000=CARTESIAN_POINT('Ctrl Pts',(113.228310289369,7.23275451518901,75.540921750577));
#137001=CARTESIAN_POINT('Ctrl Pts',(115.305714966569,7.28245852194701,74.970021382884));
#137002=CARTESIAN_POINT('Ctrl Pts',(119.150002336769,7.36432237457901,73.6050086640061));
#137003=CARTESIAN_POINT('Ctrl Pts',(122.829165031769,7.42430540347801,71.754540381793));
#137004=CARTESIAN_POINT('Ctrl Pts',(126.167856447969,7.46373591418301,69.375045120244));
#137005=CARTESIAN_POINT('Ctrl Pts',(128.453230587369,7.48631180618701,67.33878584061));
#137006=CARTESIAN_POINT('Ctrl Pts',(130.472696968569,7.50545576601201,65.062710327142));
#137007=CARTESIAN_POINT('Ctrl Pts',(132.208627615269,7.52508893814001,62.59881514699));
#137008=CARTESIAN_POINT('Ctrl Pts',(133.698071052769,7.54598850132701,60.00898250641));
#137009=CARTESIAN_POINT('Ctrl Pts',(134.625522178469,7.56064494902501,58.08602358773));
#137010=CARTESIAN_POINT('Ctrl Pts',(135.095755118369,7.56813643646701,57.04547417283));
#137011=CARTESIAN_POINT('Ctrl Pts',(135.160914695369,7.56917391166701,56.9019492428));
#137012=CARTESIAN_POINT('Ctrl Pts',(94.0331386912691,9.72819829915901,77.461392093022));
#137013=CARTESIAN_POINT('Ctrl Pts',(96.0072237788691,9.80312253342201,77.061683512892));
#137014=CARTESIAN_POINT('Ctrl Pts',(99.8110674473691,9.94225623371201,76.303613694699));
#137015=CARTESIAN_POINT('Ctrl Pts',(104.532674733669,10.10237277876,75.390554672224));
#137016=CARTESIAN_POINT('Ctrl Pts',(107.736774407169,10.20506710756,74.780870036665));
#137017=CARTESIAN_POINT('Ctrl Pts',(109.223468801269,10.25150545695,74.503201540156));
#137018=CARTESIAN_POINT('Ctrl Pts',(109.856025930669,10.2709864892,74.383369290596));
#137019=CARTESIAN_POINT('Ctrl Pts',(110.073541803969,10.27768940791,74.342100727107));
#137020=CARTESIAN_POINT('Ctrl Pts',(110.363390117669,10.2866439161,74.29539812619));
#137021=CARTESIAN_POINT('Ctrl Pts',(110.636083672869,10.29455426583,74.226981390702));
#137022=CARTESIAN_POINT('Ctrl Pts',(111.802366463169,10.32851663231,73.9536960572392));
#137023=CARTESIAN_POINT('Ctrl Pts',(113.765631696269,10.38176050765,73.4123027455414));
#137024=CARTESIAN_POINT('Ctrl Pts',(117.408936777569,10.46588100582,72.1259277537728));
#137025=CARTESIAN_POINT('Ctrl Pts',(120.906767485869,10.52044842901,70.388769104978));
#137026=CARTESIAN_POINT('Ctrl Pts',(124.083745239269,10.54709619697,68.155531276342));
#137027=CARTESIAN_POINT('Ctrl Pts',(126.256740506469,10.55719661026,66.243657042203));
#137028=CARTESIAN_POINT('Ctrl Pts',(128.171601052569,10.56185077472,64.103935177044));
#137029=CARTESIAN_POINT('Ctrl Pts',(129.805209314969,10.56596145084,61.7842775069));
#137030=CARTESIAN_POINT('Ctrl Pts',(131.187259144569,10.57057132432,59.34216081812));
#137031=CARTESIAN_POINT('Ctrl Pts',(132.031718325369,10.57263726849,57.53084438825));
#137032=CARTESIAN_POINT('Ctrl Pts',(132.456573729769,10.57307303608,56.55186096657));
#137033=CARTESIAN_POINT('Ctrl Pts',(132.515478739069,10.57313960115,56.41681702166));
#137034=CARTESIAN_POINT('Ctrl Pts',(93.6821591598691,12.38223399943,75.277158781868));
#137035=CARTESIAN_POINT('Ctrl Pts',(95.5036016978691,12.45177252617,74.883600097677));
#137036=CARTESIAN_POINT('Ctrl Pts',(99.0144758616691,12.58026926678,74.142647762821));
#137037=CARTESIAN_POINT('Ctrl Pts',(103.374764814069,12.72653556026,73.2619966330297));
#137038=CARTESIAN_POINT('Ctrl Pts',(106.334684719569,12.81951619743,72.6790624888142));
#137039=CARTESIAN_POINT('Ctrl Pts',(107.707954093569,12.86137745058,72.4142380691917));
#137040=CARTESIAN_POINT('Ctrl Pts',(108.292895990869,12.87891347918,72.3004044412196));
#137041=CARTESIAN_POINT('Ctrl Pts',(108.492143327769,12.88488451512,72.2607679061845));
#137042=CARTESIAN_POINT('Ctrl Pts',(108.768958348269,12.89325414546,72.2179669987607));
#137043=CARTESIAN_POINT('Ctrl Pts',(109.019525278469,12.90021960472,72.1537748655661));
#137044=CARTESIAN_POINT('Ctrl Pts',(110.102605128169,12.93055535856,71.899044541544));
#137045=CARTESIAN_POINT('Ctrl Pts',(111.926525841569,12.9773529257,71.399025133737));
#137046=CARTESIAN_POINT('Ctrl Pts',(115.320061967569,13.04832119269,70.223065623371));
#137047=CARTESIAN_POINT('Ctrl Pts',(118.590293578969,13.08784543436,68.64729371565));
#137048=CARTESIAN_POINT('Ctrl Pts',(121.570885042369,13.09763726794,66.622368575163));
#137049=CARTESIAN_POINT('Ctrl Pts',(123.613187646469,13.09445150359,64.885470371931));
#137050=CARTESIAN_POINT('Ctrl Pts',(125.413286174969,13.08547415731,62.93331204737));
#137051=CARTESIAN_POINT('Ctrl Pts',(126.940103658769,13.07597683247,60.80415135462));
#137052=CARTESIAN_POINT('Ctrl Pts',(128.210308454669,13.06716939491,58.54935029097));
#137053=CARTESIAN_POINT('Ctrl Pts',(128.966982164169,13.05967464117,56.87447857797));
#137054=CARTESIAN_POINT('Ctrl Pts',(129.343546144769,13.05498236743,55.96982815299));
#137055=CARTESIAN_POINT('Ctrl Pts',(129.395797698569,13.05434118198,55.8450323617));
#137056=CARTESIAN_POINT('Ctrl Pts',(93.2525500644691,14.5649471354,72.6292789718861));
#137057=CARTESIAN_POINT('Ctrl Pts',(94.9099055354691,14.61582719551,72.2566984826754));
#137058=CARTESIAN_POINT('Ctrl Pts',(98.1053351783691,14.7107858356,71.558752483666));
#137059=CARTESIAN_POINT('Ctrl Pts',(102.075446269569,14.8211612689,70.735832604723));
#137060=CARTESIAN_POINT('Ctrl Pts',(104.771012343469,14.89256300333,70.193284594267));
#137061=CARTESIAN_POINT('Ctrl Pts',(106.021560527069,14.92503651236,69.946645860606));
#137062=CARTESIAN_POINT('Ctrl Pts',(106.554407446069,14.93870838161,69.840964041424));
#137063=CARTESIAN_POINT('Ctrl Pts',(106.735454910169,14.9433096718,69.803778649846));
#137064=CARTESIAN_POINT('Ctrl Pts',(106.989614914069,14.95016974445,69.765111926735));
#137065=CARTESIAN_POINT('Ctrl Pts',(107.217710549069,14.95547553046,69.70673385112));
#137066=CARTESIAN_POINT('Ctrl Pts',(108.206162207169,14.97909147355,69.476010576657));
#137067=CARTESIAN_POINT('Ctrl Pts',(109.872101016469,15.01529544008,69.028920839883));
#137068=CARTESIAN_POINT('Ctrl Pts',(112.979053178569,15.06915909587,67.992654212769));
#137069=CARTESIAN_POINT('Ctrl Pts',(115.986803650169,15.09616756986,66.620973578397));
#137070=CARTESIAN_POINT('Ctrl Pts',(118.747134698169,15.0978837308,64.858171703176));
#137071=CARTESIAN_POINT('Ctrl Pts',(120.648236384269,15.09059048003,63.339220675778));
#137072=CARTESIAN_POINT('Ctrl Pts',(122.330929139869,15.07917832172,61.61678074719));
#137073=CARTESIAN_POINT('Ctrl Pts',(123.753705899769,15.06867596534,59.71388200454));
#137074=CARTESIAN_POINT('Ctrl Pts',(124.914541955869,15.0603582609,57.67407819686));
#137075=CARTESIAN_POINT('Ctrl Pts',(125.583406784669,15.05453759886,56.1508042958));
#137076=CARTESIAN_POINT('Ctrl Pts',(125.911269502169,15.05112031705,55.32778880756));
#137077=CARTESIAN_POINT('Ctrl Pts',(125.956814830969,15.05065149879,55.2142568397));
#137078=CARTESIAN_POINT('Ctrl Pts',(92.7615299379691,16.20464964225,69.620537172474));
#137079=CARTESIAN_POINT('Ctrl Pts',(94.2482272171691,16.23101251592,69.288280242251));
#137080=CARTESIAN_POINT('Ctrl Pts',(97.1146500626691,16.28269287648,68.665777578172));
#137081=CARTESIAN_POINT('Ctrl Pts',(100.675648889369,16.34879084479,67.928895074072));
#137082=CARTESIAN_POINT('Ctrl Pts',(103.092866435569,16.39470354547,67.439878040069));
#137083=CARTESIAN_POINT('Ctrl Pts',(104.214137922869,16.41636882877,67.215955123965));
#137084=CARTESIAN_POINT('Ctrl Pts',(104.691547007069,16.42563822416,67.120132104085));
#137085=CARTESIAN_POINT('Ctrl Pts',(104.854874208569,16.42872819769,67.086043494429));
#137086=CARTESIAN_POINT('Ctrl Pts',(105.077166774169,16.43364643686,67.051562487782));
#137087=CARTESIAN_POINT('Ctrl Pts',(105.282954985669,16.43718598195,67.000347697702));
#137088=CARTESIAN_POINT('Ctrl Pts',(106.167370916869,16.4533828966,66.798047782311));
#137089=CARTESIAN_POINT('Ctrl Pts',(107.659994694069,16.47861830463,66.413110357911));
#137090=CARTESIAN_POINT('Ctrl Pts',(110.449346482569,16.51753051004,65.539506830122));
#137091=CARTESIAN_POINT('Ctrl Pts',(113.164900595469,16.5391631641,64.405441646321));
#137092=CARTESIAN_POINT('Ctrl Pts',(115.685632177769,16.54470350357,62.94652020938));
#137093=CARTESIAN_POINT('Ctrl Pts',(117.438110061369,16.54407453157,61.67801064453));
#137094=CARTESIAN_POINT('Ctrl Pts',(119.003522973169,16.54227130612,60.2155314398));
#137095=CARTESIAN_POINT('Ctrl Pts',(120.327462124369,16.54346569086,58.56130716037));
#137096=CARTESIAN_POINT('Ctrl Pts',(121.383545670869,16.54890359416,56.7494057631));
#137097=CARTESIAN_POINT('Ctrl Pts',(121.965884169569,16.55497512192,55.38117511892));
#137098=CARTESIAN_POINT('Ctrl Pts',(122.245274929469,16.55854277873,54.64052580792));
#137099=CARTESIAN_POINT('Ctrl Pts',(122.284150061769,16.5590322,54.53836925391));
#137100=CARTESIAN_POINT('Ctrl Pts',(92.3160161407691,17.05845632578,66.898897768948));
#137101=CARTESIAN_POINT('Ctrl Pts',(93.6568412849691,17.06736860337,66.616905406802));
#137102=CARTESIAN_POINT('Ctrl Pts',(96.2410774598691,17.08777774571,66.084296447147));
#137103=CARTESIAN_POINT('Ctrl Pts',(99.4489334442691,17.12067117079,65.440189739954));
#137104=CARTESIAN_POINT('Ctrl Pts',(101.624696234569,17.14672195508,65.003809046661));
#137105=CARTESIAN_POINT('Ctrl Pts',(102.633720717169,17.15974422671,64.800948051197));
#137106=CARTESIAN_POINT('Ctrl Pts',(103.062536021769,17.16544430497,64.714017968606));
#137107=CARTESIAN_POINT('Ctrl Pts',(103.211636753469,17.16734450314,64.682771588846));
#137108=CARTESIAN_POINT('Ctrl Pts',(103.399836092569,17.17046418614,64.651541526049));
#137109=CARTESIAN_POINT('Ctrl Pts',(103.587344926369,17.17265333749,64.60706354595));
#137110=CARTESIAN_POINT('Ctrl Pts',(104.377911634569,17.18284853984,64.430665787025));
#137111=CARTESIAN_POINT('Ctrl Pts',(105.714438850969,17.19933510361,64.102439610754));
#137112=CARTESIAN_POINT('Ctrl Pts',(108.215174535469,17.22692014645,63.377387806248));
#137113=CARTESIAN_POINT('Ctrl Pts',(110.664078907169,17.24638005472,62.4617307178));
#137114=CARTESIAN_POINT('Ctrl Pts',(112.970350336469,17.25840009369,61.2819001994));
#137115=CARTESIAN_POINT('Ctrl Pts',(114.593636762369,17.26584272015,60.24176555596));
#137116=CARTESIAN_POINT('Ctrl Pts',(116.062124964169,17.27413543879,59.01301835956));
#137117=CARTESIAN_POINT('Ctrl Pts',(117.308594600169,17.28622002581,57.57589495172));
#137118=CARTESIAN_POINT('Ctrl Pts',(118.281647748769,17.30325651225,55.95516825802));
#137119=CARTESIAN_POINT('Ctrl Pts',(118.793142603669,17.31878284792,54.71165243129));
#137120=CARTESIAN_POINT('Ctrl Pts',(119.032406353169,17.32781830618,54.03616091157));
#137121=CARTESIAN_POINT('Ctrl Pts',(119.065763660669,17.32905858225,53.9430137336));
#137122=CARTESIAN_POINT('Ctrl Pts',(91.9339550857691,17.43416835301,64.566878312127));
#137123=CARTESIAN_POINT('Ctrl Pts',(93.1522101427691,17.4351925881,64.333371668602));
#137124=CARTESIAN_POINT('Ctrl Pts',(95.4988411627691,17.43929521558,63.885545568036));
#137125=CARTESIAN_POINT('Ctrl Pts',(98.4081963615691,17.44930366796,63.32400983193));
#137126=CARTESIAN_POINT('Ctrl Pts',(100.379251469769,17.45845732483,62.93152947122));
#137127=CARTESIAN_POINT('Ctrl Pts',(101.293074352569,17.46327369117,62.74533292911));
#137128=CARTESIAN_POINT('Ctrl Pts',(101.680396266369,17.46542263789,62.66531285689));
#137129=CARTESIAN_POINT('Ctrl Pts',(101.818151876569,17.46612943771,62.63626485097));
#137130=CARTESIAN_POINT('Ctrl Pts',(101.973456160669,17.46738521279,62.60726304328));
#137131=CARTESIAN_POINT('Ctrl Pts',(102.146144323769,17.46819098171,62.56845769507));
#137132=CARTESIAN_POINT('Ctrl Pts',(102.854965544569,17.47207775314,62.41336021059));
#137133=CARTESIAN_POINT('Ctrl Pts',(104.055724048769,17.47844462254,62.13268158581));
#137134=CARTESIAN_POINT('Ctrl Pts',(106.304077105169,17.48930373187,61.53448456181));
#137135=CARTESIAN_POINT('Ctrl Pts',(108.519486612369,17.49708393044,60.80877120184));
#137136=CARTESIAN_POINT('Ctrl Pts',(110.640989084169,17.50193555607,59.87314194888));
#137137=CARTESIAN_POINT('Ctrl Pts',(112.155666249669,17.50505371007,59.03237899087));
#137138=CARTESIAN_POINT('Ctrl Pts',(113.546265142869,17.50879004802,58.00605527088));
#137139=CARTESIAN_POINT('Ctrl Pts',(114.733631519169,17.51473720583,56.75323061307));
#137140=CARTESIAN_POINT('Ctrl Pts',(115.642630167569,17.52396358116,55.29008237542));
#137141=CARTESIAN_POINT('Ctrl Pts',(116.097732378869,17.53321365172,54.14606429834));
#137142=CARTESIAN_POINT('Ctrl Pts',(116.304737644669,17.5388103524,53.52186781304));
#137143=CARTESIAN_POINT('Ctrl Pts',(116.333661985569,17.53957671709,53.4358199528));
#137144=CARTESIAN_POINT('Ctrl Pts',(91.7333543710691,17.50193427032,63.343238804133));
#137145=CARTESIAN_POINT('Ctrl Pts',(92.8879430816691,17.50178071582,63.135566510854));
#137146=CARTESIAN_POINT('Ctrl Pts',(95.1110362757691,17.50190429546,62.7323392405));
#137147=CARTESIAN_POINT('Ctrl Pts',(97.8649203306691,17.50289431744,62.21265963756));
#137148=CARTESIAN_POINT('Ctrl Pts',(99.7292020028691,17.50388971296,61.84139379018));
#137149=CARTESIAN_POINT('Ctrl Pts',(100.593373017269,17.50441934898,61.66287784085));
#137150=CARTESIAN_POINT('Ctrl Pts',(100.958949970969,17.50465717549,61.58600521299));
#137151=CARTESIAN_POINT('Ctrl Pts',(101.091069108469,17.5047228542,61.55794471084));
#137152=CARTESIAN_POINT('Ctrl Pts',(101.227679271069,17.50492834844,61.52983163798));
#137153=CARTESIAN_POINT('Ctrl Pts',(101.392906395369,17.50498701793,61.49388561767));
#137154=CARTESIAN_POINT('Ctrl Pts',(102.058282080869,17.50538071097,61.34932247533));
#137155=CARTESIAN_POINT('Ctrl Pts',(103.186985240469,17.50589985612,61.09282947493));
#137156=CARTESIAN_POINT('Ctrl Pts',(105.300987791769,17.50623611027,60.56083608065));
#137157=CARTESIAN_POINT('Ctrl Pts',(107.392172249469,17.50516596038,59.93641944816));
#137158=CARTESIAN_POINT('Ctrl Pts',(109.416813367469,17.50251834733,59.13214859692));
#137159=CARTESIAN_POINT('Ctrl Pts',(110.875800805269,17.49995962543,58.39870659569));
#137160=CARTESIAN_POINT('Ctrl Pts',(112.228147178369,17.49719000828,57.48100958633));
#137161=CARTESIAN_POINT('Ctrl Pts',(113.388028172869,17.49498041446,56.32605080859));
#137162=CARTESIAN_POINT('Ctrl Pts',(114.266895872169,17.49434409422,54.9452214594));
#137163=CARTESIAN_POINT('Ctrl Pts',(114.694606203969,17.49557249646,53.85221657865));
#137164=CARTESIAN_POINT('Ctrl Pts',(114.885795476969,17.49668055561,53.25412084327));
#137165=CARTESIAN_POINT('Ctrl Pts',(114.912547697369,17.49682919454,53.1716873435));
#137166=CARTESIAN_POINT('Ctrl Pts',(91.6257501351691,17.5008740942,62.68712605541));
#137167=CARTESIAN_POINT('Ctrl Pts',(92.7463475571691,17.50094910285,62.49304918148));
#137168=CARTESIAN_POINT('Ctrl Pts',(94.9034580498691,17.50020157244,62.11312328629));
#137169=CARTESIAN_POINT('Ctrl Pts',(97.5742443556691,17.49698101879,61.61482317768));
#137170=CARTESIAN_POINT('Ctrl Pts',(99.3814211904691,17.4935641372,61.25405000158));
#137171=CARTESIAN_POINT('Ctrl Pts',(100.219041110869,17.49166946169,61.07919591897));
#137172=CARTESIAN_POINT('Ctrl Pts',(100.572958494569,17.49080987306,61.00381337677));
#137173=CARTESIAN_POINT('Ctrl Pts',(100.702150056369,17.49050587323,60.97621269887));
#137174=CARTESIAN_POINT('Ctrl Pts',(100.828290732669,17.49010441605,60.9484739145));
#137175=CARTESIAN_POINT('Ctrl Pts',(100.989611625069,17.4897288122,60.91400588789));
#137176=CARTESIAN_POINT('Ctrl Pts',(101.631509061969,17.48808288405,60.77482113764));
#137177=CARTESIAN_POINT('Ctrl Pts',(102.721309338569,17.48510085369,60.53097327818));
#137178=CARTESIAN_POINT('Ctrl Pts',(104.762674554169,17.47883852165,60.0343178855));
#137179=CARTESIAN_POINT('Ctrl Pts',(106.786759229369,17.47170352733,59.46484747566));
#137180=CARTESIAN_POINT('Ctrl Pts',(108.759587553569,17.4633398522,58.73230369738));
#137181=CARTESIAN_POINT('Ctrl Pts',(110.189220263469,17.4562483296,58.05754357168));
#137182=CARTESIAN_POINT('Ctrl Pts',(111.522000690569,17.44825192058,57.19920404805));
#137183=CARTESIAN_POINT('Ctrl Pts',(112.668390106469,17.43964575023,56.09749731227));
#137184=CARTESIAN_POINT('Ctrl Pts',(113.532332395069,17.43141181414,54.76115344552));
#137185=CARTESIAN_POINT('Ctrl Pts',(113.946140607069,17.42647507754,53.69550001546));
#137186=CARTESIAN_POINT('Ctrl Pts',(114.129248991669,17.42412453312,53.11135600252));
#137187=CARTESIAN_POINT('Ctrl Pts',(114.154891885069,17.42379728054,53.03085492537));
#137188=CARTESIAN_POINT('',(114.384105937906,17.4511140883104,53.3319645993539));
#137189=CARTESIAN_POINT('Ctrl Pts',(114.384106000532,17.4511131438857,53.3319646520768));
#137190=CARTESIAN_POINT('Ctrl Pts',(116.347347433182,17.6026023327896,53.7135820476909));
#137191=CARTESIAN_POINT('Ctrl Pts',(118.851091663061,17.5211983263482,54.200263045881));
#137192=CARTESIAN_POINT('Ctrl Pts',(124.584741871326,15.6692377812452,55.3147771283751));
#137193=CARTESIAN_POINT('Ctrl Pts',(127.009446406625,14.4661198773037,55.7860941811001));
#137194=CARTESIAN_POINT('Ctrl Pts',(131.323096521923,11.5107569636489,56.6245867223739));
#137195=CARTESIAN_POINT('Ctrl Pts',(133.336771014781,9.66385111634966,57.0160071673924));
#137196=CARTESIAN_POINT('Ctrl Pts',(135.581104357009,6.39144737287628,57.4522632366775));
#137197=CARTESIAN_POINT('Ctrl Pts',(136.207456627177,5.20057247572336,57.5740142769302));
#137198=CARTESIAN_POINT('Ctrl Pts',(137.075144789367,2.66538159270485,57.7426763665124));
#137199=CARTESIAN_POINT('Ctrl Pts',(137.305407382829,1.3446443670393,57.7874349761847));
#137200=CARTESIAN_POINT('Ctrl Pts',(137.305407436207,-9.29645249669875E-12,
57.7874348564623));
#137201=CARTESIAN_POINT('Ctrl Pts',(114.384105646626,17.4511131146219,53.3319645061305));
#137202=CARTESIAN_POINT('Ctrl Pts',(114.371589774419,17.4511819034599,53.3703524107852));
#137203=CARTESIAN_POINT('Ctrl Pts',(114.357320213996,17.4512575190875,53.4134407155842));
#137204=CARTESIAN_POINT('Ctrl Pts',(114.341143340837,17.45134138163,53.4611755752132));
#137205=CARTESIAN_POINT('Ctrl Pts',(114.325809473745,17.4514208739441,53.5064228851237));
#137206=CARTESIAN_POINT('Ctrl Pts',(114.308762036051,17.4515077781385,53.5558453044607));
#137207=CARTESIAN_POINT('Ctrl Pts',(114.289827745447,17.4516035983617,53.6093757289036));
#137208=CARTESIAN_POINT('Ctrl Pts',(114.285716357714,17.4516244047441,53.6209993135934));
#137209=CARTESIAN_POINT('Ctrl Pts',(114.281515834125,17.4516456326073,53.6328164989034));
#137210=CARTESIAN_POINT('Ctrl Pts',(114.277224105706,17.4516672991808,53.6448264394875));
#137211=CARTESIAN_POINT('Ctrl Pts',(114.258540385167,17.4517616229974,53.6971108227662));
#137212=CARTESIAN_POINT('Ctrl Pts',(114.238131584234,17.4518642423489,53.7530503429297));
#137213=CARTESIAN_POINT('Ctrl Pts',(114.215800873513,17.4519767262012,53.8125605070917));
#137214=CARTESIAN_POINT('Ctrl Pts',(114.211283543716,17.4519994808132,53.8245989523145));
#137215=CARTESIAN_POINT('Ctrl Pts',(114.206687418172,17.4520226398948,53.8367834311851));
#137216=CARTESIAN_POINT('Ctrl Pts',(114.202010636999,17.452046217648,53.849113109929));
#137217=CARTESIAN_POINT('Ctrl Pts',(114.186407098532,17.4521248820898,53.8902496543791));
#137218=CARTESIAN_POINT('Ctrl Pts',(114.169654599657,17.4522094553237,53.9336529273905));
#137219=CARTESIAN_POINT('Ctrl Pts',(114.152096554589,17.4522984297842,53.9781912391146));
#137220=CARTESIAN_POINT('Ctrl Pts',(114.138377180561,17.4523679519832,54.0129922522513));
#137221=CARTESIAN_POINT('Ctrl Pts',(114.12416655042,17.4524401550677,54.0484863843268));
#137222=CARTESIAN_POINT('Ctrl Pts',(114.109649605634,17.4525141353038,54.0841415616067));
#137223=CARTESIAN_POINT('Ctrl Pts',(114.067083963232,17.4527310553459,54.1886873560771));
#137224=CARTESIAN_POINT('Ctrl Pts',(114.026117877619,17.4529477408174,54.2844675121801));
#137225=CARTESIAN_POINT('Ctrl Pts',(113.987376113768,17.4531583366583,54.371707940627));
#137226=CARTESIAN_POINT('Ctrl Pts',(113.947900494458,17.4533729216544,54.4606008974683));
#137227=CARTESIAN_POINT('Ctrl Pts',(113.91073816483,17.4535811767367,54.5406304621533));
#137228=CARTESIAN_POINT('Ctrl Pts',(113.876535028894,17.4537778853062,54.6120707171014));
#137229=CARTESIAN_POINT('Ctrl Pts',(113.866007534157,17.4538384308783,54.6340595461213));
#137230=CARTESIAN_POINT('Ctrl Pts',(113.855760052481,17.4538978898741,54.6552347304349));
#137231=CARTESIAN_POINT('Ctrl Pts',(113.845810293893,17.4539561299282,54.6756042812164));
#137232=CARTESIAN_POINT('Ctrl Pts',(113.833476788596,17.4540283230382,54.7008539352894));
#137233=CARTESIAN_POINT('Ctrl Pts',(113.821600821234,17.4540986425022,54.7248657155462));
#137234=CARTESIAN_POINT('Ctrl Pts',(113.810214497995,17.454166856576,54.7476545088773));
#137235=CARTESIAN_POINT('Ctrl Pts',(113.801855403344,17.4542169348925,54.764384552145));
#137236=CARTESIAN_POINT('Ctrl Pts',(113.793335740895,17.4542684884077,54.7812963178437));
#137237=CARTESIAN_POINT('Ctrl Pts',(113.785601101182,17.4543156932661,54.7965429892002));
#137238=CARTESIAN_POINT('Ctrl Pts',(113.783009019611,17.4543315128579,54.8016525505132));
#137239=CARTESIAN_POINT('Ctrl Pts',(113.780505517019,17.4543468415418,54.8065753082894));
#137240=CARTESIAN_POINT('Ctrl Pts',(113.778127313472,17.4543614533325,54.8112423088825));
#137241=CARTESIAN_POINT('Ctrl Pts',(113.777935556687,17.4543626314949,54.8116186135216));
#137242=CARTESIAN_POINT('Ctrl Pts',(113.77774461476,17.4543638049951,54.8119932555158));
#137243=CARTESIAN_POINT('Ctrl Pts',(113.777554507073,17.4543649737138,54.8123661987807));
#137244=CARTESIAN_POINT('Ctrl Pts',(113.760997352661,17.4544667615813,54.844847153788));
#137245=CARTESIAN_POINT('Ctrl Pts',(113.742187397006,17.4545848856968,54.8812806335243));
#137246=CARTESIAN_POINT('Ctrl Pts',(113.720936292063,17.4547203115329,54.9215653752202));
#137247=CARTESIAN_POINT('Ctrl Pts',(113.699938910622,17.4548541204781,54.9613691449496));
#137248=CARTESIAN_POINT('Ctrl Pts',(113.676558220886,17.4550048241377,55.0049330567655));
#137249=CARTESIAN_POINT('Ctrl Pts',(113.650573073102,17.455173446629,55.0521281496504));
#137250=CARTESIAN_POINT('Ctrl Pts',(113.625154667817,17.4553383914221,55.0982939058894));
#137251=CARTESIAN_POINT('Ctrl Pts',(113.597244014884,17.4555204858377,55.1479344381161));
#137252=CARTESIAN_POINT('Ctrl Pts',(113.566598142364,17.4557207219892,55.2008949254065));
#137253=CARTESIAN_POINT('Ctrl Pts',(113.5501664346,17.455828084634,55.2292912861119));
#137254=CARTESIAN_POINT('Ctrl Pts',(113.532947775678,17.4559406630743,55.258641488683));
#137255=CARTESIAN_POINT('Ctrl Pts',(113.514900538785,17.4560586081969,55.2889170572746));
#137256=CARTESIAN_POINT('Ctrl Pts',(113.494743755401,17.4561903399573,55.3227315454167));
#137257=CARTESIAN_POINT('Ctrl Pts',(113.473553439861,17.4563287667806,55.3577004992569));
#137258=CARTESIAN_POINT('Ctrl Pts',(113.451267303754,17.4564740880957,55.3937788901019));
#137259=CARTESIAN_POINT('Ctrl Pts',(113.440124235701,17.4565467487532,55.4118180855244));
#137260=CARTESIAN_POINT('Ctrl Pts',(113.428707212121,17.4566211401046,55.4301346399296));
#137261=CARTESIAN_POINT('Ctrl Pts',(113.41700792369,17.4566972750741,55.4487222204307));
#137262=CARTESIAN_POINT('Ctrl Pts',(113.40763168092,17.4567582924566,55.463618995419));
#137263=CARTESIAN_POINT('Ctrl Pts',(113.397662857599,17.4568231073498,55.479335314175));
#137264=CARTESIAN_POINT('Ctrl Pts',(113.388085467126,17.4568853036446,55.4943156320338));
#137265=CARTESIAN_POINT('Ctrl Pts',(113.385712585373,17.4569007133173,55.498027136019));
#137266=CARTESIAN_POINT('Ctrl Pts',(113.383363945006,17.4569159613581,55.5016935984257));
#137267=CARTESIAN_POINT('Ctrl Pts',(113.381054924302,17.456930948487,55.5052916296858));
#137268=CARTESIAN_POINT('Ctrl Pts',(113.334198945699,17.457235075942,55.5783049532101));
#137269=CARTESIAN_POINT('Ctrl Pts',(113.288749634299,17.4575253378865,55.6463050848044));
#137270=CARTESIAN_POINT('Ctrl Pts',(113.24511861625,17.4577997228023,55.7095128221076));
#137271=CARTESIAN_POINT('Ctrl Pts',(113.201487627675,17.4580741075328,55.7727205167098));
#137272=CARTESIAN_POINT('Ctrl Pts',(113.159674881288,17.4583326225352,55.8311365761762));
#137273=CARTESIAN_POINT('Ctrl Pts',(113.12004017196,17.4585737507042,55.8849822108195));
#137274=CARTESIAN_POINT('Ctrl Pts',(113.081271647035,17.4588096092129,55.9376510928206));
#137275=CARTESIAN_POINT('Ctrl Pts',(113.044586785714,17.4590288397472,55.9859477052673));
#137276=CARTESIAN_POINT('Ctrl Pts',(113.010274955306,17.4592303863066,56.0300697377023));
#137277=CARTESIAN_POINT('Ctrl Pts',(112.992863499198,17.4593326606251,56.0524593573176));
#137278=CARTESIAN_POINT('Ctrl Pts',(112.976062363385,17.4594303864457,56.0737738059339));
#137279=CARTESIAN_POINT('Ctrl Pts',(112.959904764964,17.4595234526901,56.0940372932867));
#137280=CARTESIAN_POINT('Ctrl Pts',(112.951825965753,17.4595699858123,56.1041690369631));
#137281=CARTESIAN_POINT('Ctrl Pts',(112.943908050731,17.4596153574017,56.114038040181));
#137282=CARTESIAN_POINT('Ctrl Pts',(112.936154828112,17.4596595514036,56.1236471771745));
#137283=CARTESIAN_POINT('Ctrl Pts',(112.932278216802,17.4596816484046,56.1284517456712));
#137284=CARTESIAN_POINT('Ctrl Pts',(112.928442778582,17.459703451225,56.1331913476027));
#137285=CARTESIAN_POINT('Ctrl Pts',(112.924648979998,17.4597249584811,56.1378663366714));
#137286=CARTESIAN_POINT('Ctrl Pts',(112.922752080705,17.4597357121092,56.1402038312057));
#137287=CARTESIAN_POINT('Ctrl Pts',(112.920865591321,17.4597463918598,56.1425251725237));
#137288=CARTESIAN_POINT('Ctrl Pts',(112.918989568944,17.4597569975594,56.1448304042441));
#137289=CARTESIAN_POINT('Ctrl Pts',(112.917113546568,17.4597676032591,56.1471356359646));
#137290=CARTESIAN_POINT('Ctrl Pts',(112.916020739977,17.459773778669,56.1484778736131));
#137291=CARTESIAN_POINT('Ctrl Pts',(112.913392959572,17.4597885923618,56.1516978140407));
#137292=CARTESIAN_POINT('Ctrl Pts',(112.913390689335,17.4597886051599,56.1517005958662));
#137293=CARTESIAN_POINT('Ctrl Pts',(112.913388419096,17.459788617958,56.15170337769));
#137294=CARTESIAN_POINT('Ctrl Pts',(112.913386148855,17.4597886307561,56.151706159512));
#137295=CARTESIAN_POINT('Ctrl Pts',(112.745210152272,17.460736694941,56.3577793044755));
#137296=CARTESIAN_POINT('Ctrl Pts',(112.565150469579,17.461708681726,56.5542011869675));
#137297=CARTESIAN_POINT('Ctrl Pts',(112.375139748759,17.46268621933,56.7407485428551));
#137298=CARTESIAN_POINT('Ctrl Pts',(112.280133105854,17.4631749947299,56.8340234799187));
#137299=CARTESIAN_POINT('Ctrl Pts',(112.182638636455,17.4636651526536,56.9248297189269));
#137300=CARTESIAN_POINT('Ctrl Pts',(112.082898074606,17.4641543518052,57.0131390517288));
#137301=CARTESIAN_POINT('Ctrl Pts',(112.033027793681,17.464398951381,57.0572937181298));
#137302=CARTESIAN_POINT('Ctrl Pts',(111.982595989662,17.4646433108442,57.1008241579985));
#137303=CARTESIAN_POINT('Ctrl Pts',(111.931632896949,17.4648871353774,57.1437268418812));
#137304=CARTESIAN_POINT('Ctrl Pts',(111.906151350592,17.465009047644,57.1651781838226));
#137305=CARTESIAN_POINT('Ctrl Pts',(111.880536982064,17.4651308261497,57.1864725867688));
#137306=CARTESIAN_POINT('Ctrl Pts',(111.854793571691,17.4652524338651,57.2076096087177));
#137307=CARTESIAN_POINT('Ctrl Pts',(111.830659124467,17.4653664410983,57.2274255667948));
#137308=CARTESIAN_POINT('Ctrl Pts',(111.806411261559,17.465480298222,57.2471032017298));
#137309=CARTESIAN_POINT('Ctrl Pts',(111.782053098436,17.4655939746343,57.2666421490116));
#137310=CARTESIAN_POINT('Ctrl Pts',(111.780429220894,17.4656015530618,57.2679447454971));
#137311=CARTESIAN_POINT('Ctrl Pts',(111.777792341615,17.4656138520919,57.2700576557719));
#137312=CARTESIAN_POINT('Ctrl Pts',(111.777179996071,17.4656167074982,57.270548089188));
#137313=CARTESIAN_POINT('Ctrl Pts',(111.776395605827,17.4656203651599,57.2711763148544));
#137314=CARTESIAN_POINT('Ctrl Pts',(111.775598150403,17.4656240892754,57.2718148987131));
#137315=CARTESIAN_POINT('Ctrl Pts',(111.774787618582,17.4656278798337,57.2724638263153));
#137316=CARTESIAN_POINT('Ctrl Pts',(111.760604535374,17.4656942088818,57.2838190796654));
#137317=CARTESIAN_POINT('Ctrl Pts',(111.742420120335,17.465780887691,57.2983450544814));
#137318=CARTESIAN_POINT('Ctrl Pts',(111.720157327019,17.4658878287095,57.3159423469922));
#137319=CARTESIAN_POINT('Ctrl Pts',(111.697136922665,17.4659984089701,57.3341384818336));
#137320=CARTESIAN_POINT('Ctrl Pts',(111.669755695092,17.4661306561564,57.3556185664265));
#137321=CARTESIAN_POINT('Ctrl Pts',(111.637895660831,17.4662843890616,57.3802271302202));
#137322=CARTESIAN_POINT('Ctrl Pts',(111.604130975223,17.4664473124022,57.4063068391424));
#137323=CARTESIAN_POINT('Ctrl Pts',(111.56533571254,17.4666343715798,57.4359003749058));
#137324=CARTESIAN_POINT('Ctrl Pts',(111.521336071247,17.4668452057531,57.4687707712478));
#137325=CARTESIAN_POINT('Ctrl Pts',(111.477336429953,17.4670560399264,57.5016411675897));
#137326=CARTESIAN_POINT('Ctrl Pts',(111.428131607977,17.4672906533659,57.5377879032397));
#137327=CARTESIAN_POINT('Ctrl Pts',(111.373524006893,17.4675484798121,57.5769274428994));
#137328=CARTESIAN_POINT('Ctrl Pts',(111.337953740903,17.4677164226458,57.6024221324442));
#137329=CARTESIAN_POINT('Ctrl Pts',(111.300090628467,17.4678942104067,57.629185713148));
#137330=CARTESIAN_POINT('Ctrl Pts',(111.259877307962,17.4680816222481,57.6571308871485));
#137331=CARTESIAN_POINT('Ctrl Pts',(111.23977064771,17.4681753281688,57.6711034741488));
#137332=CARTESIAN_POINT('Ctrl Pts',(111.219076435305,17.4682714447304,57.6853714592458));
#137333=CARTESIAN_POINT('Ctrl Pts',(111.197787444961,17.4683699324149,57.6999232647248));
#137334=CARTESIAN_POINT('Ctrl Pts',(111.187142949789,17.4684191762571,57.7071991674643));
#137335=CARTESIAN_POINT('Ctrl Pts',(111.176349760127,17.4684690130712,57.71454602529));
#137336=CARTESIAN_POINT('Ctrl Pts',(111.165406982368,17.4685194385309,57.7219623780656));
#137337=CARTESIAN_POINT('Ctrl Pts',(111.155657403354,17.4685643656064,57.7285700529149));
#137338=CARTESIAN_POINT('Ctrl Pts',(111.144636782127,17.4686150532942,57.7360084489736));
#137339=CARTESIAN_POINT('Ctrl Pts',(111.135424344395,17.4686573498515,57.7422034172612));
#137340=CARTESIAN_POINT('Ctrl Pts',(111.134296883493,17.4686625263005,57.7429615862423));
#137341=CARTESIAN_POINT('Ctrl Pts',(111.133196542218,17.4686675771778,57.7437011845906));
#137342=CARTESIAN_POINT('Ctrl Pts',(111.132128993479,17.468672476629,57.7444184518172));
#137343=CARTESIAN_POINT('Ctrl Pts',(111.071704874938,17.4689497895145,57.7850163546245));
#137344=CARTESIAN_POINT('Ctrl Pts',(111.014241928657,17.469209739296,57.8226602437051));
#137345=CARTESIAN_POINT('Ctrl Pts',(110.959910551484,17.4694526426504,57.8575777780466));
#137346=CARTESIAN_POINT('Ctrl Pts',(110.904095672232,17.4697021784086,57.8934487252678));
#137347=CARTESIAN_POINT('Ctrl Pts',(110.851585419274,17.4699337263767,57.9264422793881));
#137348=CARTESIAN_POINT('Ctrl Pts',(110.802525020451,17.4701476770414,57.9567642234572));
#137349=CARTESIAN_POINT('Ctrl Pts',(110.751292573144,17.4703710999328,57.9884286093784));
#137350=CARTESIAN_POINT('Ctrl Pts',(110.703821995689,17.4705753353621,58.0171795755969));
#137351=CARTESIAN_POINT('Ctrl Pts',(110.660240003903,17.470760841675,58.0432082184106));
#137352=CARTESIAN_POINT('Ctrl Pts',(110.628203113416,17.4708972063795,58.0623417353787));
#137353=CARTESIAN_POINT('Ctrl Pts',(110.598266636585,17.4710234509446,58.0800032780499));
#137354=CARTESIAN_POINT('Ctrl Pts',(110.570469576052,17.4711397500975,58.0962550110909));
#137355=CARTESIAN_POINT('Ctrl Pts',(110.547624402729,17.4712353312222,58.1096115909241));
#137356=CARTESIAN_POINT('Ctrl Pts',(110.526224099794,17.4713241947182,58.1220156960866));
#137357=CARTESIAN_POINT('Ctrl Pts',(110.506286149657,17.4714064277931,58.1334963711835));
#137358=CARTESIAN_POINT('Ctrl Pts',(110.496317174589,17.4714475443306,58.1392367087319));
#137359=CARTESIAN_POINT('Ctrl Pts',(110.486713787606,17.4714870080712,58.1447461885291));
#137360=CARTESIAN_POINT('Ctrl Pts',(110.477477796359,17.4715248232401,58.1500279186985));
#137361=CARTESIAN_POINT('Ctrl Pts',(110.472859800735,17.4715437308245,58.1526687837832));
#137362=CARTESIAN_POINT('Ctrl Pts',(110.468333654039,17.471562226548,58.1552527114472));
#137363=CARTESIAN_POINT('Ctrl Pts',(110.463899573078,17.4715803116796,58.1577800758039));
#137364=CARTESIAN_POINT('Ctrl Pts',(110.459465492116,17.4715983968111,58.1603074401607));
#137365=CARTESIAN_POINT('Ctrl Pts',(110.453789037814,17.4716214930161,58.1635364414641));
#137366=CARTESIAN_POINT('Ctrl Pts',(110.4508737383,17.4716333370874,58.1651928444699));
#137367=CARTESIAN_POINT('Ctrl Pts',(110.450871060701,17.4716333479658,58.1651943658172));
#137368=CARTESIAN_POINT('Ctrl Pts',(110.450868383044,17.4716333588444,58.1651958871963));
#137369=CARTESIAN_POINT('Ctrl Pts',(110.450865705331,17.4716333697233,58.1651974086071));
#137370=CARTESIAN_POINT('Ctrl Pts',(110.424150203037,17.4717419080043,58.1803764985696));
#137371=CARTESIAN_POINT('Ctrl Pts',(110.391741195077,17.4718758027233,58.1987191894422));
#137372=CARTESIAN_POINT('Ctrl Pts',(110.353555787436,17.4720344129501,58.220073765757));
#137373=CARTESIAN_POINT('Ctrl Pts',(110.312314412423,17.4722057167086,58.243137342774));
#137374=CARTESIAN_POINT('Ctrl Pts',(110.264334916551,17.4724058552091,58.2697142697748));
#137375=CARTESIAN_POINT('Ctrl Pts',(110.209484453875,17.4726336795687,58.2995559249602));
#137376=CARTESIAN_POINT('Ctrl Pts',(110.150435248625,17.4728789436324,58.3316819260199));
#137377=CARTESIAN_POINT('Ctrl Pts',(110.083422210429,17.4731563016772,58.3675911586784));
#137378=CARTESIAN_POINT('Ctrl Pts',(110.008254233598,17.4734638408916,58.4069116875536));
#137379=CARTESIAN_POINT('Ctrl Pts',(109.914932187883,17.4738456549278,58.4557286485513));
#137380=CARTESIAN_POINT('Ctrl Pts',(109.80903794466,17.4742740311308,58.5098027933334));
#137381=CARTESIAN_POINT('Ctrl Pts',(109.690191365439,17.4747441717411,58.568335905514));
#137382=CARTESIAN_POINT('Ctrl Pts',(109.644759030211,17.4749238957681,58.5907117786099));
#137383=CARTESIAN_POINT('Ctrl Pts',(109.597434018789,17.475109709447,58.6137386222985));
#137384=CARTESIAN_POINT('Ctrl Pts',(109.548196424467,17.4753012924258,58.6373705006825));
#137385=CARTESIAN_POINT('Ctrl Pts',(109.470298483254,17.4756043925229,58.6747580842652));
#137386=CARTESIAN_POINT('Ctrl Pts',(109.387612572138,17.47592194347,58.7136596031847));
#137387=CARTESIAN_POINT('Ctrl Pts',(109.30006910572,17.4762525214668,58.7538958831759));
#137388=CARTESIAN_POINT('Ctrl Pts',(109.256297372511,17.4764178104652,58.7740140231715));
#137389=CARTESIAN_POINT('Ctrl Pts',(109.211311250656,17.4765863456859,58.7944658539154));
#137390=CARTESIAN_POINT('Ctrl Pts',(109.165103823356,17.4767579389749,58.8152299777297));
#137391=CARTESIAN_POINT('Ctrl Pts',(109.142000109706,17.4768437356193,58.8256120396368));
#137392=CARTESIAN_POINT('Ctrl Pts',(109.118591069714,17.4769302956955,58.8360721748612));
#137393=CARTESIAN_POINT('Ctrl Pts',(109.094875930883,17.4770175935859,58.8466077877838));
#137394=CARTESIAN_POINT('Ctrl Pts',(109.083018361468,17.4770612425311,58.8518755942451));
#137395=CARTESIAN_POINT('Ctrl Pts',(109.071084267344,17.4771050758497,58.8571622701346));
#137396=CARTESIAN_POINT('Ctrl Pts',(109.059073559752,17.4771490902105,58.8624674965145));
#137397=CARTESIAN_POINT('Ctrl Pts',(109.053068205956,17.477171097391,58.8651201097044));
#137398=CARTESIAN_POINT('Ctrl Pts',(109.047043698793,17.4771931498265,58.8677773605172));
#137399=CARTESIAN_POINT('Ctrl Pts',(109.041000027737,17.4772152470961,58.8704392095162));
#137400=CARTESIAN_POINT('Ctrl Pts',(109.035722234518,17.4772345441125,58.87276373851));
#137401=CARTESIAN_POINT('Ctrl Pts',(109.029040845196,17.4772589448399,58.8757021475603));
#137402=CARTESIAN_POINT('Ctrl Pts',(109.024594720515,17.4772751673272,58.8776552791828));
#137403=CARTESIAN_POINT('Ctrl Pts',(109.02394952882,17.4772775214253,58.8779387045006));
#137404=CARTESIAN_POINT('Ctrl Pts',(109.023351416907,17.47727970346,58.8782014046281));
#137405=CARTESIAN_POINT('Ctrl Pts',(109.022811512541,17.4772816729723,58.8784385117749));
#137406=CARTESIAN_POINT('Ctrl Pts',(108.894616013314,17.4777493161777,58.9347374990424));
#137407=CARTESIAN_POINT('Ctrl Pts',(108.768938169259,17.4781914309708,58.9881074799368));
#137408=CARTESIAN_POINT('Ctrl Pts',(108.645940054624,17.4786100115034,59.0388676027788));
#137409=CARTESIAN_POINT('Ctrl Pts',(108.520461269671,17.4790370341191,59.0906514740775));
#137410=CARTESIAN_POINT('Ctrl Pts',(108.3977713007,17.4794395627121,59.1397189720536));
#137411=CARTESIAN_POINT('Ctrl Pts',(108.278015551975,17.4798195257597,59.1863611953479));
#137412=CARTESIAN_POINT('Ctrl Pts',(108.154689973338,17.4802108152235,59.2343937886722));
#137413=CARTESIAN_POINT('Ctrl Pts',(108.034476085892,17.4805781734427,59.2798542298973));
#137414=CARTESIAN_POINT('Ctrl Pts',(107.917505897425,17.4809235174297,59.3230125996528));
#137415=CARTESIAN_POINT('Ctrl Pts',(107.904174509995,17.480962877155,59.3279314679181));
#137416=CARTESIAN_POINT('Ctrl Pts',(107.890885230248,17.4810019507274,59.3328203845218));
#137417=CARTESIAN_POINT('Ctrl Pts',(107.877638233044,17.481040740837,59.3376797126102));
#137418=CARTESIAN_POINT('Ctrl Pts',(107.818808889225,17.4812130060425,59.3592597792801));
#137419=CARTESIAN_POINT('Ctrl Pts',(107.760813566222,17.4813796816511,59.3802565130386));
#137420=CARTESIAN_POINT('Ctrl Pts',(107.703666621925,17.4815409952453,59.4007000127499));
#137421=CARTESIAN_POINT('Ctrl Pts',(107.675093149776,17.4816216520424,59.4109217626055));
#137422=CARTESIAN_POINT('Ctrl Pts',(107.646731772284,17.4817009700903,59.4210052038805));
#137423=CARTESIAN_POINT('Ctrl Pts',(107.618584116815,17.4817789744635,59.4309538003569));
#137424=CARTESIAN_POINT('Ctrl Pts',(107.60451028908,17.4818179766501,59.4359280985951));
#137425=CARTESIAN_POINT('Ctrl Pts',(107.59048989185,17.4818566505234,59.4408686856294));
#137426=CARTESIAN_POINT('Ctrl Pts',(107.576523124441,17.4818949995002,59.4457759870934));
#137427=CARTESIAN_POINT('Ctrl Pts',(107.569539740736,17.4819141739886,59.4482296378254));
#137428=CARTESIAN_POINT('Ctrl Pts',(107.562569764487,17.4819332672591,59.4506749671646));
#137429=CARTESIAN_POINT('Ctrl Pts',(107.555613220062,17.481952279732,59.4531120273421));
#137430=CARTESIAN_POINT('Ctrl Pts',(107.552134947849,17.4819617859685,59.4543305574308));
#137431=CARTESIAN_POINT('Ctrl Pts',(107.548660033593,17.481971272006,59.4555470202291));
#137432=CARTESIAN_POINT('Ctrl Pts',(107.545188480304,17.4819807378965,59.4567614222034));
#137433=CARTESIAN_POINT('Ctrl Pts',(107.542670430008,17.4819876038687,59.457642274374));
#137434=CARTESIAN_POINT('Ctrl Pts',(107.539562333622,17.4819960701084,59.4587288813542));
#137435=CARTESIAN_POINT('Ctrl Pts',(107.53715197661,17.4820026310721,59.4595711238867));
#137436=CARTESIAN_POINT('Ctrl Pts',(107.536239253527,17.4820051154937,59.4598900534879));
#137437=CARTESIAN_POINT('Ctrl Pts',(107.535426584075,17.4820073268524,59.4601739606438));
#137438=CARTESIAN_POINT('Ctrl Pts',(107.534783906329,17.4820090751799,59.4603984520891));
#137439=CARTESIAN_POINT('Ctrl Pts',(107.465097798596,17.4821986478588,59.4847402550293));
#137440=CARTESIAN_POINT('Ctrl Pts',(107.38419840039,17.4824130222309,59.5126143740575));
#137441=CARTESIAN_POINT('Ctrl Pts',(107.291997713868,17.4826501715579,59.5437396635183));
#137442=CARTESIAN_POINT('Ctrl Pts',(107.189531181776,17.4829137256597,59.5783305173583));
#137443=CARTESIAN_POINT('Ctrl Pts',(107.073106034246,17.4832054111588,59.6169360157368));
#137444=CARTESIAN_POINT('Ctrl Pts',(106.942587169386,17.483521877318,59.6591031651156));
#137445=CARTESIAN_POINT('Ctrl Pts',(106.811979200765,17.483838559525,59.7012991015333));
#137446=CARTESIAN_POINT('Ctrl Pts',(106.667257041664,17.4841800456896,59.7470587048764));
#137447=CARTESIAN_POINT('Ctrl Pts',(106.508286258143,17.4845425150198,59.7958945385632));
#137448=CARTESIAN_POINT('Ctrl Pts',(106.431489682309,17.4847176189149,59.8194864510021));
#137449=CARTESIAN_POINT('Ctrl Pts',(106.351368001573,17.4848976137749,59.843796034588));
#137450=CARTESIAN_POINT('Ctrl Pts',(106.267907549805,17.4850820428647,59.8687688203452));
#137451=CARTESIAN_POINT('Ctrl Pts',(106.226177323922,17.4851742574096,59.8812552132238));
#137452=CARTESIAN_POINT('Ctrl Pts',(106.183612405287,17.4852675794758,59.8939074066797));
#137453=CARTESIAN_POINT('Ctrl Pts',(106.140211266131,17.4853619519497,59.9067187973344));
#137454=CARTESIAN_POINT('Ctrl Pts',(106.118510696552,17.4854091381866,59.9131244926617));
#137455=CARTESIAN_POINT('Ctrl Pts',(106.096601071844,17.485456586923,59.9195699872922));
#137456=CARTESIAN_POINT('Ctrl Pts',(106.074482210197,17.4855042909056,59.9260544707709));
#137457=CARTESIAN_POINT('Ctrl Pts',(106.05236334855,17.4855519948882,59.9325389542496));
#137458=CARTESIAN_POINT('Ctrl Pts',(106.028026569481,17.4856042505556,59.9396472395218));
#137459=CARTESIAN_POINT('Ctrl Pts',(106.007497736749,17.4856481610672,59.9456240832683));
#137460=CARTESIAN_POINT('Ctrl Pts',(105.871684204389,17.4859386618359,59.9851653602722));
#137461=CARTESIAN_POINT('Ctrl Pts',(105.741825421019,17.4862113759084,60.0222184875221));
#137462=CARTESIAN_POINT('Ctrl Pts',(105.617995399476,17.4864678570325,60.0570291801906));
#137463=CARTESIAN_POINT('Ctrl Pts',(105.490158559993,17.4867326372197,60.0929662564787));
#137464=CARTESIAN_POINT('Ctrl Pts',(105.368746790353,17.486980116041,60.1265131316419));
#137465=CARTESIAN_POINT('Ctrl Pts',(105.25382206313,17.4872117552075,60.1578862729108));
#137466=CARTESIAN_POINT('Ctrl Pts',(105.132685686557,17.487455914406,60.1909551236868));
#137467=CARTESIAN_POINT('Ctrl Pts',(105.018756426988,17.4876824751316,60.2216087253473));
#137468=CARTESIAN_POINT('Ctrl Pts',(104.912087673554,17.487892886475,60.2500452427954));
#137469=CARTESIAN_POINT('Ctrl Pts',(104.862368767094,17.4879909603867,60.2632996636591));
#137470=CARTESIAN_POINT('Ctrl Pts',(104.814226986751,17.488085522199,60.2760716723553));
#137471=CARTESIAN_POINT('Ctrl Pts',(104.767666547077,17.4881767010475,60.2883777438329));
#137472=CARTESIAN_POINT('Ctrl Pts',(104.712162742519,17.488285393599,60.3030475749378));
#137473=CARTESIAN_POINT('Ctrl Pts',(104.658906133875,17.4883892791678,60.3170553585036));
#137474=CARTESIAN_POINT('Ctrl Pts',(104.607902669725,17.488488556856,60.3304252570649));
#137475=CARTESIAN_POINT('Ctrl Pts',(104.582400937649,17.4885381957001,60.3371102063456));
#137476=CARTESIAN_POINT('Ctrl Pts',(104.557462491691,17.4885866839262,60.3436356843401));
#137477=CARTESIAN_POINT('Ctrl Pts',(104.53308794685,17.4886340426396,60.3500042942641));
#137478=CARTESIAN_POINT('Ctrl Pts',(104.52090067443,17.4886577219963,60.3531885992261));
#137479=CARTESIAN_POINT('Ctrl Pts',(104.508854377289,17.4886811190529,60.3563336871684));
#137480=CARTESIAN_POINT('Ctrl Pts',(104.496949129782,17.4887042366459,60.3594398743735));
#137481=CARTESIAN_POINT('Ctrl Pts',(104.490996506029,17.4887157954424,60.360992967976));
#137482=CARTESIAN_POINT('Ctrl Pts',(104.485079144685,17.4887272843775,60.3625363363941));
#137483=CARTESIAN_POINT('Ctrl Pts',(104.479197054648,17.4887387037962,60.3640700178451));
#137484=CARTESIAN_POINT('Ctrl Pts',(104.47625600963,17.4887444135055,60.3648368585706));
#137485=CARTESIAN_POINT('Ctrl Pts',(104.473323782439,17.4887501058361,60.3656012775543));
#137486=CARTESIAN_POINT('Ctrl Pts',(104.470400374162,17.4887557808304,60.3663632794904));
#137487=CARTESIAN_POINT('Ctrl Pts',(104.467476965886,17.4887614558246,60.3671252814265));
#137488=CARTESIAN_POINT('Ctrl Pts',(104.463225821211,17.488769707859,60.3682331399835));
#137489=CARTESIAN_POINT('Ctrl Pts',(104.461656607159,17.4887727538472,60.3686420388256));
#137490=CARTESIAN_POINT('Ctrl Pts',(104.461654620551,17.4887727577033,60.368642556487));
#137491=CARTESIAN_POINT('Ctrl Pts',(104.461652633928,17.4887727615596,60.3686430741524));
#137492=CARTESIAN_POINT('Ctrl Pts',(104.46165064729,17.4887727654158,60.3686435918218));
#137493=CARTESIAN_POINT('Ctrl Pts',(104.401089705658,17.488890319779,60.3844242917302));
#137494=CARTESIAN_POINT('Ctrl Pts',(104.32621244764,17.4890362204498,60.4039121781988));
#137495=CARTESIAN_POINT('Ctrl Pts',(104.23697820632,17.4892080200877,60.4269529138905));
#137496=CARTESIAN_POINT('Ctrl Pts',(104.139363991414,17.4893959534026,60.4521574014521));
#137497=CARTESIAN_POINT('Ctrl Pts',(104.024569659901,17.4896148896923,60.481613205935));
#137498=CARTESIAN_POINT('Ctrl Pts',(103.892524141172,17.4898603670786,60.5150569402054));
#137499=CARTESIAN_POINT('Ctrl Pts',(103.739662280845,17.4901445427954,60.5537729184988));
#137500=CARTESIAN_POINT('Ctrl Pts',(103.563681221673,17.4904643127914,60.5978322073689));
#137501=CARTESIAN_POINT('Ctrl Pts',(103.364448222258,17.4908107974363,60.6467547950338));
#137502=CARTESIAN_POINT('Ctrl Pts',(103.224908719071,17.4910534695607,60.6810193676571));
#137503=CARTESIAN_POINT('Ctrl Pts',(103.073962711404,17.4913092001858,60.7176677287305));
#137504=CARTESIAN_POINT('Ctrl Pts',(102.911561096065,17.4915744310346,60.7565269092083));
#137505=CARTESIAN_POINT('Ctrl Pts',(102.720876078408,17.4918858537319,60.8021536937697));
#137506=CARTESIAN_POINT('Ctrl Pts',(102.514396679508,17.4922103795442,60.8508255120447));
#137507=CARTESIAN_POINT('Ctrl Pts',(102.292057342075,17.4925416529916,60.9022926937826));
#137508=CARTESIAN_POINT('Ctrl Pts',(102.181980547703,17.4927056613924,60.9277733057449));
#137509=CARTESIAN_POINT('Ctrl Pts',(102.068016539687,17.4928713150982,60.9539396507437));
#137510=CARTESIAN_POINT('Ctrl Pts',(101.95015896678,17.4930378017596,60.9807662437774));
#137511=CARTESIAN_POINT('Ctrl Pts',(101.855388027447,17.4931716760359,61.0023378862116));
#137512=CARTESIAN_POINT('Ctrl Pts',(101.758099528033,17.4933060883184,61.0243364946143));
#137513=CARTESIAN_POINT('Ctrl Pts',(101.658290869385,17.4934406079925,61.0467510037277));
#137514=CARTESIAN_POINT('Ctrl Pts',(101.608386540061,17.4935078678295,61.0579582582844));
#137515=CARTESIAN_POINT('Ctrl Pts',(101.557852170928,17.4935751540335,61.0692694880241));
#137516=CARTESIAN_POINT('Ctrl Pts',(101.506687518559,17.4936424127867,61.0806835666572));
#137517=CARTESIAN_POINT('Ctrl Pts',(101.481105192374,17.4936760421634,61.0863906059737));
#137518=CARTESIAN_POINT('Ctrl Pts',(101.45536529538,17.4937096646441,61.092123357514));
#137519=CARTESIAN_POINT('Ctrl Pts',(101.429467800125,17.4937432734173,61.0978816900964));
#137520=CARTESIAN_POINT('Ctrl Pts',(101.416519052497,17.4937600778038,61.1007608563875));
#137521=CARTESIAN_POINT('Ctrl Pts',(101.403530905305,17.4937768787617,61.1036464179393));
#137522=CARTESIAN_POINT('Ctrl Pts',(101.39050335542,17.4937936754383,61.1065383593248));
#137523=CARTESIAN_POINT('Ctrl Pts',(101.380732693007,17.4938062729458,61.1087073153639));
#137524=CARTESIAN_POINT('Ctrl Pts',(101.37093986658,17.493818868045,61.1108798600595));
#137525=CARTESIAN_POINT('Ctrl Pts',(101.361124874889,17.4938314603758,61.113055987125));
#137526=CARTESIAN_POINT('Ctrl Pts',(101.35902556238,17.4938341537289,61.1135214353812));
#137527=CARTESIAN_POINT('Ctrl Pts',(101.356472721471,17.4938374271047,61.1140873592338));
#137528=CARTESIAN_POINT('Ctrl Pts',(101.35433743764,17.4938401634771,61.1145606492379));
#137529=CARTESIAN_POINT('Ctrl Pts',(101.353144998232,17.4938416915917,61.114824955858));
#137530=CARTESIAN_POINT('Ctrl Pts',(101.352082779859,17.4938430523437,61.1150603780317));
#137531=CARTESIAN_POINT('Ctrl Pts',(101.351302494755,17.4938440517714,61.1152333080974));
#137532=CARTESIAN_POINT('Ctrl Pts',(101.287051625161,17.4939263474572,61.1294728559702));
#137533=CARTESIAN_POINT('Ctrl Pts',(101.223030660778,17.4940069319958,61.1435964727026));
#137534=CARTESIAN_POINT('Ctrl Pts',(101.159246416405,17.4940860895325,61.1576075224112));
#137535=CARTESIAN_POINT('Ctrl Pts',(101.093940945311,17.4941671349424,61.1719527296132));
#137536=CARTESIAN_POINT('Ctrl Pts',(101.028884439126,17.4942467139571,61.1861800242748));
#137537=CARTESIAN_POINT('Ctrl Pts',(100.964031974283,17.4943232536764,61.2002873979025));
#137538=CARTESIAN_POINT('Ctrl Pts',(100.931409334339,17.4943617553387,61.2073838092962));
#137539=CARTESIAN_POINT('Ctrl Pts',(100.898837965544,17.4943994755923,61.2144498474929));
#137540=CARTESIAN_POINT('Ctrl Pts',(100.866342995605,17.4944372461246,61.2214870603931));
#137541=CARTESIAN_POINT('Ctrl Pts',(100.833715473761,17.4944751707287,61.2285529791508));
#137542=CARTESIAN_POINT('Ctrl Pts',(100.801165285133,17.4945131559579,61.2355898468858));
#137543=CARTESIAN_POINT('Ctrl Pts',(100.768675764999,17.4945506989153,61.2425979800308));
#137544=CARTESIAN_POINT('Ctrl Pts',(100.703294203028,17.4946262499601,61.2567010720317));
#137545=CARTESIAN_POINT('Ctrl Pts',(100.638157731775,17.4946999920661,61.2706878073948));
#137546=CARTESIAN_POINT('Ctrl Pts',(100.573274503652,17.4947721938095,61.2845605728875));
#137547=CARTESIAN_POINT('Ctrl Pts',(100.30816172466,17.4950672100317,61.3412446732083));
#137548=CARTESIAN_POINT('Ctrl Pts',(100.047279365178,17.4953366103002,61.3960277355345));
#137549=CARTESIAN_POINT('Ctrl Pts',(99.7906802196189,17.4955847117602,61.4490877200565));
#137550=CARTESIAN_POINT('Ctrl Pts',(99.5091437520911,17.4958569247035,61.5073042841719));
#137551=CARTESIAN_POINT('Ctrl Pts',(99.2327633342877,17.4961035016865,61.5634469666845));
#137552=CARTESIAN_POINT('Ctrl Pts',(98.9616049770858,17.4963293230433,61.6177163292878));
#137553=CARTESIAN_POINT('Ctrl Pts',(98.8355378727401,17.4964343120426,61.6429472735548));
#137554=CARTESIAN_POINT('Ctrl Pts',(98.7105993971195,17.4965348024916,61.6677728386518));
#137555=CARTESIAN_POINT('Ctrl Pts',(98.5867955406294,17.496631224476,61.6922108690025));
#137556=CARTESIAN_POINT('Ctrl Pts',(98.5248936123844,17.4966794354682,61.7044298841779));
#137557=CARTESIAN_POINT('Ctrl Pts',(98.4632753389212,17.4967266287093,61.7165520156652));
#137558=CARTESIAN_POINT('Ctrl Pts',(98.4019414248222,17.4967728546863,61.7285793385115));
#137559=CARTESIAN_POINT('Ctrl Pts',(98.3712744677727,17.4967959676748,61.7345929999346));
#137560=CARTESIAN_POINT('Ctrl Pts',(98.3406786005642,17.4968188388104,61.7405829591975));
#137561=CARTESIAN_POINT('Ctrl Pts',(98.3101539101087,17.4968414741929,61.7465494717433));
#137562=CARTESIAN_POINT('Ctrl Pts',(98.287260392267,17.4968584507298,61.7510243561526));
#137563=CARTESIAN_POINT('Ctrl Pts',(98.2644069113487,17.4968752946523,61.7554860517835));
#137564=CARTESIAN_POINT('Ctrl Pts',(98.2415935035095,17.4968920084843,61.7599346646255));
#137565=CARTESIAN_POINT('Ctrl Pts',(98.2350605450253,17.4968967947385,61.7612085910469));
#137566=CARTESIAN_POINT('Ctrl Pts',(98.2272178784105,17.4969025293887,61.7627373134558));
#137567=CARTESIAN_POINT('Ctrl Pts',(98.2214494621805,17.4969067405201,61.7638613805773));
#137568=CARTESIAN_POINT('Ctrl Pts',(98.2205033486733,17.4969074312137,61.7640457457556));
#137569=CARTESIAN_POINT('Ctrl Pts',(98.2196130357078,17.4969080809985,61.7642192279549));
#137570=CARTESIAN_POINT('Ctrl Pts',(98.2187934546568,17.4969086790445,61.7643789203052));
#137571=CARTESIAN_POINT('Ctrl Pts',(97.9395998248513,17.4971124058273,61.8187787711454));
#137572=CARTESIAN_POINT('Ctrl Pts',(97.6176562614074,17.4973327272939,61.8806636085485));
#137573=CARTESIAN_POINT('Ctrl Pts',(97.2529227856745,17.4975567818557,61.9495667300436));
#137574=CARTESIAN_POINT('Ctrl Pts',(96.9673494327301,17.4977322086172,62.0035154261268));
#137575=CARTESIAN_POINT('Ctrl Pts',(96.6555444295688,17.4979098745043,62.0617643138665));
#137576=CARTESIAN_POINT('Ctrl Pts',(96.3175040235945,17.4980825240508,62.1241144775376));
#137577=CARTESIAN_POINT('Ctrl Pts',(96.2238001826425,17.498130382015,62.1413977659159));
#137578=CARTESIAN_POINT('Ctrl Pts',(96.1280805677447,17.498177848875,62.1589964558432));
#137579=CARTESIAN_POINT('Ctrl Pts',(96.0303453756578,17.4982247570068,62.1769070473104));
#137580=CARTESIAN_POINT('Ctrl Pts',(95.8802390887399,17.4982968007133,62.2044149728001));
#137581=CARTESIAN_POINT('Ctrl Pts',(95.7253783623984,17.4983675280424,62.2326584756737));
#137582=CARTESIAN_POINT('Ctrl Pts',(95.5657645979641,17.498436304944,62.2616269799026));
#137583=CARTESIAN_POINT('Ctrl Pts',(95.4859577157469,17.4984706933949,62.2761112320171));
#137584=CARTESIAN_POINT('Ctrl Pts',(95.4049625740064,17.4985045942078,62.2907767344701));
#137585=CARTESIAN_POINT('Ctrl Pts',(95.3227794507625,17.4985379245222,62.3056224962104));
#137586=CARTESIAN_POINT('Ctrl Pts',(95.2816878891406,17.4985545896794,62.3130453770807));
#137587=CARTESIAN_POINT('Ctrl Pts',(95.2402993321428,17.498571112214,62.3205133227727));
#137588=CARTESIAN_POINT('Ctrl Pts',(95.1986138181634,17.4985874816507,62.3280262223119));
#137589=CARTESIAN_POINT('Ctrl Pts',(95.1777710611737,17.4985956663691,62.3317826720814));
#137590=CARTESIAN_POINT('Ctrl Pts',(95.1568540649386,17.4986038128135,62.3355503603128));
#137591=CARTESIAN_POINT('Ctrl Pts',(95.135862834657,17.498611919662,62.3393292744713));
#137592=CARTESIAN_POINT('Ctrl Pts',(95.1149645103485,17.49861999063,62.3430914633741));
#137593=CARTESIAN_POINT('Ctrl Pts',(95.0951917916129,17.4986275669728,62.3466491388768));
#137594=CARTESIAN_POINT('Ctrl Pts',(95.0729630543763,17.4986360074748,62.3506463463487));
#137595=CARTESIAN_POINT('Ctrl Pts',(95.0728642338951,17.498636044998,62.3506641164075));
#137596=CARTESIAN_POINT('Ctrl Pts',(95.072765364874,17.4986360825382,62.3506818951486));
#137597=CARTESIAN_POINT('Ctrl Pts',(95.0726664469983,17.4986361200954,62.3506996826287));
#137598=CARTESIAN_POINT('Ctrl Pts',(94.7539491580066,17.4987571308559,62.4080116435298));
#137599=CARTESIAN_POINT('Ctrl Pts',(94.4540862260824,17.498854098322,62.4615626426501));
#137600=CARTESIAN_POINT('Ctrl Pts',(94.1730878885652,17.4989323784167,62.5115348283151));
#137601=CARTESIAN_POINT('Ctrl Pts',(93.8708845850804,17.499016565759,62.5652780629681));
#137602=CARTESIAN_POINT('Ctrl Pts',(93.5905003663791,17.4990791528839,62.6148817985568));
#137603=CARTESIAN_POINT('Ctrl Pts',(93.3319416781723,17.499126020286,62.6605119366226));
#137604=CARTESIAN_POINT('Ctrl Pts',(93.0602342843467,17.4991752710761,62.708462543039));
#137605=CARTESIAN_POINT('Ctrl Pts',(92.8126285372438,17.4992071759936,62.7520246011495));
#137606=CARTESIAN_POINT('Ctrl Pts',(92.5891272193619,17.4992275110013,62.7913319494329));
#137607=CARTESIAN_POINT('Ctrl Pts',(92.335540307397,17.4992505833118,62.8359304742344));
#137608=CARTESIAN_POINT('Ctrl Pts',(92.1129838065121,17.4992588015865,62.8750517396529));
#137609=CARTESIAN_POINT('Ctrl Pts',(91.9214587222694,17.4992588252864,62.9088210133816));
#137610=CARTESIAN_POINT('Ctrl Pts',(91.6420934838691,17.49285958709,63.189615652045));
#137611=CARTESIAN_POINT('Ctrl Pts',(91.4789922092691,17.53610702643,62.18563192847));
#137612=CARTESIAN_POINT('Ctrl Pts',(91.2383773640691,17.31069605489,60.70627724341));
#137613=CARTESIAN_POINT('Ctrl Pts',(90.9525691952691,16.49526955095,58.9431717031));
#137614=CARTESIAN_POINT('Ctrl Pts',(90.7669853929691,15.69349549193,57.79357798411));
#137615=CARTESIAN_POINT('Ctrl Pts',(90.6082909803691,14.70024762493,56.80299770092));
#137616=CARTESIAN_POINT('Ctrl Pts',(90.5020501966691,13.74144627107,56.13084913298));
#137617=CARTESIAN_POINT('Ctrl Pts',(90.4359017984691,12.91166468527,55.70386232152));
#137618=CARTESIAN_POINT('Ctrl Pts',(90.3919674335691,12.26996490143,55.4170156774));
#137619=CARTESIAN_POINT('Ctrl Pts',(90.3493777568691,11.625304524,55.14038529705));
#137620=CARTESIAN_POINT('Ctrl Pts',(90.2953449889691,10.75812458152,54.79028890357));
#137621=CARTESIAN_POINT('Ctrl Pts',(90.2336264398691,9.65880570576201,54.39205929398));
#137622=CARTESIAN_POINT('Ctrl Pts',(90.1482830071691,7.87135436875902,53.83794898949));
#137623=CARTESIAN_POINT('Ctrl Pts',(90.0307622873691,4.60885046054901,53.0684560992));
#137624=CARTESIAN_POINT('Ctrl Pts',(89.9936930987691,1.72466757533901,52.81072925206));
#137625=CARTESIAN_POINT('Ctrl Pts',(89.9978563170691,-0.222741235654886,
52.82471933133));
#137626=CARTESIAN_POINT('Ctrl Pts',(92.8081742635691,17.49302494713,62.98048707022));
#137627=CARTESIAN_POINT('Ctrl Pts',(92.5986957331691,17.53515279357,62.00241380564));
#137628=CARTESIAN_POINT('Ctrl Pts',(92.2904281843691,17.31896818594,60.55914785523));
#137629=CARTESIAN_POINT('Ctrl Pts',(91.9177634399691,16.52369843295,58.82356961025));
#137630=CARTESIAN_POINT('Ctrl Pts',(91.6714076249691,15.73549484237,57.68441568033));
#137631=CARTESIAN_POINT('Ctrl Pts',(91.4546567602691,14.75116789232,56.69582182933));
#137632=CARTESIAN_POINT('Ctrl Pts',(91.3031505320691,13.79449439958,56.02158047908));
#137633=CARTESIAN_POINT('Ctrl Pts',(91.2028409584691,12.96185490683,55.59044131214));
#137634=CARTESIAN_POINT('Ctrl Pts',(91.1354530152691,12.32146797839,55.30843405596));
#137635=CARTESIAN_POINT('Ctrl Pts',(91.0705758403691,11.6762140863,55.03376811454));
#137636=CARTESIAN_POINT('Ctrl Pts',(90.9888550570691,10.80763428018,54.68635453666));
#137637=CARTESIAN_POINT('Ctrl Pts',(90.8964011661691,9.70473219682602,54.29014956108));
#137638=CARTESIAN_POINT('Ctrl Pts',(90.7663353867691,7.91003779904601,53.73885583037));
#137639=CARTESIAN_POINT('Ctrl Pts',(90.5830034095691,4.63059635124401,52.97296192257));
#137640=CARTESIAN_POINT('Ctrl Pts',(90.5158616249691,1.73018539026001,52.71855132778));
#137641=CARTESIAN_POINT('Ctrl Pts',(90.5140275106691,-0.223476692403986,
52.73371084717));
#137642=CARTESIAN_POINT('Ctrl Pts',(95.0334241451691,17.49340335946,62.57726075376));
#137643=CARTESIAN_POINT('Ctrl Pts',(94.7354399602691,17.53146746781,61.64878450661));
#137644=CARTESIAN_POINT('Ctrl Pts',(94.2980792778691,17.3287395782,60.27468725031));
#137645=CARTESIAN_POINT('Ctrl Pts',(93.7599791478691,16.56684333187,58.59467001799));
#137646=CARTESIAN_POINT('Ctrl Pts',(93.3979525790691,15.80201717449,57.47859068081));
#137647=CARTESIAN_POINT('Ctrl Pts',(93.0707154216691,14.83409351927,56.49734889427));
#137648=CARTESIAN_POINT('Ctrl Pts',(92.8329885552691,13.88266802702,55.82142820774));
#137649=CARTESIAN_POINT('Ctrl Pts',(92.6675763969691,13.04676841354,55.3837256506));
#137650=CARTESIAN_POINT('Ctrl Pts',(92.5552464285691,12.40954656296,55.10962258496));
#137651=CARTESIAN_POINT('Ctrl Pts',(92.4477320239691,11.76404691488,54.83811150331));
#137652=CARTESIAN_POINT('Ctrl Pts',(92.3130280801691,10.89384905739,54.49495852329));
#137653=CARTESIAN_POINT('Ctrl Pts',(92.1617766247691,9.78542268762302,54.1017826688));
#137654=CARTESIAN_POINT('Ctrl Pts',(91.9461684628691,7.97909093036001,53.55434070925));
#137655=CARTESIAN_POINT('Ctrl Pts',(91.6370372572691,4.67110183200301,52.79259801177));
#137656=CARTESIAN_POINT('Ctrl Pts',(91.5126236727691,1.74147908297301,52.54249043603));
#137657=CARTESIAN_POINT('Ctrl Pts',(91.4993303696691,-0.224968888493586,
52.55999386635));
#137658=CARTESIAN_POINT('Ctrl Pts',(98.3123086382691,17.49367872538,61.95032016408));
#137659=CARTESIAN_POINT('Ctrl Pts',(97.8838690771691,17.52132588781,61.0961871323));
#137660=CARTESIAN_POINT('Ctrl Pts',(97.2563270796691,17.3278166254,59.82631141409));
#137661=CARTESIAN_POINT('Ctrl Pts',(96.4754412409691,16.60157660903,58.23885952741));
#137662=CARTESIAN_POINT('Ctrl Pts',(95.9439265902691,15.8644449042,57.16729227158));
#137663=CARTESIAN_POINT('Ctrl Pts',(95.4548753321691,14.91906406746,56.20859012133));
#137664=CARTESIAN_POINT('Ctrl Pts',(95.0906828307691,13.97865602756,55.53812427992));
#137665=CARTESIAN_POINT('Ctrl Pts',(94.8297011904691,13.1440013253,55.09570191083));
#137666=CARTESIAN_POINT('Ctrl Pts',(94.6507179597691,12.51318114468,54.83035115667));
#137667=CARTESIAN_POINT('Ctrl Pts',(94.4801736252691,11.86966475712,54.56265476203));
#137668=CARTESIAN_POINT('Ctrl Pts',(94.2671175844691,10.99981417036,54.22446202571));
#137669=CARTESIAN_POINT('Ctrl Pts',(94.0289868932691,9.88660333602602,53.83473114943));
#137670=CARTESIAN_POINT('Ctrl Pts',(93.6870297939691,8.06867605678801,53.29066962107));
#137671=CARTESIAN_POINT('Ctrl Pts',(93.1923467916691,4.72816996048401,52.5304743899));
#137672=CARTESIAN_POINT('Ctrl Pts',(92.9840367818691,1.75997518098801,52.28237290523));
#137673=CARTESIAN_POINT('Ctrl Pts',(92.9537596435691,-0.227382347777086,
52.30357915893));
#137674=CARTESIAN_POINT('Ctrl Pts',(101.476063383869,17.49353152741,61.29633982016));
#137675=CARTESIAN_POINT('Ctrl Pts',(100.921772906669,17.50678730304,60.51612407986));
#137676=CARTESIAN_POINT('Ctrl Pts',(100.110868018069,17.31209403281,59.35052803616));
#137677=CARTESIAN_POINT('Ctrl Pts',(99.0967857761691,16.60753119682,57.86441562302));
#137678=CARTESIAN_POINT('Ctrl Pts',(98.4027331908691,15.89075779816,56.84705199828));
#137679=CARTESIAN_POINT('Ctrl Pts',(97.7585857601691,14.96553329684,55.92243481635));
#137680=CARTESIAN_POINT('Ctrl Pts',(97.2730114467691,14.03873742039,55.26579785069));
#137681=CARTESIAN_POINT('Ctrl Pts',(96.9202344708691,13.21083938854,54.82435903563));
#137682=CARTESIAN_POINT('Ctrl Pts',(96.6766080013691,12.58779566903,54.56550800276));
#137683=CARTESIAN_POINT('Ctrl Pts',(96.4451267608691,11.9483583019,54.30142844987));
#137684=CARTESIAN_POINT('Ctrl Pts',(96.1563018818691,11.08137533143,53.96772273336));
#137685=CARTESIAN_POINT('Ctrl Pts',(95.8342360423691,9.96667796475001,53.5814680127));
#137686=CARTESIAN_POINT('Ctrl Pts',(95.3702583734691,8.14278530794401,53.04015645856));
#137687=CARTESIAN_POINT('Ctrl Pts',(94.6966272138691,4.78001049072901,52.27965855516));
#137688=CARTESIAN_POINT('Ctrl Pts',(94.4079250495691,1.77918161124201,52.03051117877));
#137689=CARTESIAN_POINT('Ctrl Pts',(94.3611452467691,-0.229864186975786,
52.05546697121));
#137690=CARTESIAN_POINT('Ctrl Pts',(104.621046699869,17.49157360923,60.55369177597));
#137691=CARTESIAN_POINT('Ctrl Pts',(103.941719998769,17.49095598093,59.85125262095));
#137692=CARTESIAN_POINT('Ctrl Pts',(102.948813513369,17.29010700753,58.79646558991));
#137693=CARTESIAN_POINT('Ctrl Pts',(101.704261160469,16.59820570304,57.42793899511));
#137694=CARTESIAN_POINT('Ctrl Pts',(100.849876330569,15.89691605225,56.47926166912));
#137695=CARTESIAN_POINT('Ctrl Pts',(100.052867821069,14.99073822913,55.60442015319));
#137696=CARTESIAN_POINT('Ctrl Pts',(99.4475331754691,14.08024912469,54.97301510726));
#137697=CARTESIAN_POINT('Ctrl Pts',(99.0041424461691,13.26410825573,54.54036692231));
#137698=CARTESIAN_POINT('Ctrl Pts',(98.6960975395691,12.64985632218,54.28771822127));
#137699=CARTESIAN_POINT('Ctrl Pts',(98.4040997745691,12.01595884731,54.02882577639));
#137700=CARTESIAN_POINT('Ctrl Pts',(98.0400351694691,11.15329344622,53.70144103815));
#137701=CARTESIAN_POINT('Ctrl Pts',(97.6347501637691,10.03867108199,53.32138367282));
#137702=CARTESIAN_POINT('Ctrl Pts',(97.0498718249691,8.21126455271101,52.78612552645));
#137703=CARTESIAN_POINT('Ctrl Pts',(96.1992862091691,4.83024970546001,52.02935270629));
#137704=CARTESIAN_POINT('Ctrl Pts',(95.8317275561691,1.79882218783101,51.77865520573));
#137705=CARTESIAN_POINT('Ctrl Pts',(95.7685464794691,-0.232393034910786,
51.80735253732));
#137706=CARTESIAN_POINT('Ctrl Pts',(107.206331732069,17.48793196066,59.79698581959));
#137707=CARTESIAN_POINT('Ctrl Pts',(106.424335049069,17.47679956275,59.16535434663));
#137708=CARTESIAN_POINT('Ctrl Pts',(105.282246068869,17.26723075518,58.21301206074));
#137709=CARTESIAN_POINT('Ctrl Pts',(103.849819279169,16.57860703868,56.96285248062));
#137710=CARTESIAN_POINT('Ctrl Pts',(102.865084831869,15.8861456528,56.08863860426));
#137711=CARTESIAN_POINT('Ctrl Pts',(101.944004472769,14.9947548764,55.27363787577));
#137712=CARTESIAN_POINT('Ctrl Pts',(101.241437676969,14.09987468339,54.67719491956));
#137713=CARTESIAN_POINT('Ctrl Pts',(100.724490474169,13.29748172548,54.26189382541));
#137714=CARTESIAN_POINT('Ctrl Pts',(100.363674930769,12.69122630203,54.01677538362));
#137715=CARTESIAN_POINT('Ctrl Pts',(100.022315310469,12.06297792511,53.76608434928));
#137716=CARTESIAN_POINT('Ctrl Pts',(99.5969390137691,11.20486683145,53.44885422607));
#137717=CARTESIAN_POINT('Ctrl Pts',(99.1240602916691,10.09129477713,53.08026985688));
#137718=CARTESIAN_POINT('Ctrl Pts',(98.4411431664691,8.26255458396301,52.55881082705));
#137719=CARTESIAN_POINT('Ctrl Pts',(97.4476761906691,4.86917168282301,51.8176534126));
#137720=CARTESIAN_POINT('Ctrl Pts',(97.0175166613691,1.81445350612301,51.56911166491));
#137721=CARTESIAN_POINT('Ctrl Pts',(96.9414792205691,-0.234402174419586,
51.60056036597));
#137722=CARTESIAN_POINT('Ctrl Pts',(109.221604211669,17.48372544845,59.02333129694));
#137723=CARTESIAN_POINT('Ctrl Pts',(108.359784642469,17.46375567822,58.45574398136));
#137724=CARTESIAN_POINT('Ctrl Pts',(107.102015888569,17.24379846808,57.59775863006));
#137725=CARTESIAN_POINT('Ctrl Pts',(105.524816585069,16.55226120142,56.46376307926));
#137726=CARTESIAN_POINT('Ctrl Pts',(104.439982558469,15.8637820089,55.66640186783));
#137727=CARTESIAN_POINT('Ctrl Pts',(103.423883984169,14.98313091293,54.9173947312));
#137728=CARTESIAN_POINT('Ctrl Pts',(102.646954741169,14.10173774314,54.36322879206));
#137729=CARTESIAN_POINT('Ctrl Pts',(102.073834275069,13.31262966272,53.97252742131));
#137730=CARTESIAN_POINT('Ctrl Pts',(101.672467124869,12.71315223001,53.73834234543));
#137731=CARTESIAN_POINT('Ctrl Pts',(101.293368480369,12.09006135913,53.49997643624));
#137732=CARTESIAN_POINT('Ctrl Pts',(100.821239581369,11.23624367659,53.19828953843));
#137733=CARTESIAN_POINT('Ctrl Pts',(100.297134086169,10.12429194288,52.84806009283));
#137734=CARTESIAN_POINT('Ctrl Pts',(99.5401819745691,8.29592164133101,52.35088649986));
#137735=CARTESIAN_POINT('Ctrl Pts',(98.4397626213691,4.89564257240101,51.64188202533));
#137736=CARTESIAN_POINT('Ctrl Pts',(97.9644651398691,1.82535593403501,51.40219205419));
#137737=CARTESIAN_POINT('Ctrl Pts',(97.8800497432691,-0.235801263741986,
51.43506172539));
#137738=CARTESIAN_POINT('Ctrl Pts',(110.673215030269,17.48001284702,58.31066582355));
#137739=CARTESIAN_POINT('Ctrl Pts',(109.754172542369,17.4528430433,57.7969602139));
#137740=CARTESIAN_POINT('Ctrl Pts',(108.413728072469,17.22294323409,57.01954740541));
#137741=CARTESIAN_POINT('Ctrl Pts',(106.733762387369,16.52601355492,55.98868535554));
#137742=CARTESIAN_POINT('Ctrl Pts',(105.578169273769,15.83872897935,55.26157469267));
#137743=CARTESIAN_POINT('Ctrl Pts',(104.495167177069,14.96539903947,54.57518563264));
#137744=CARTESIAN_POINT('Ctrl Pts',(103.666047098169,14.0945150779,54.06328095415));
#137745=CARTESIAN_POINT('Ctrl Pts',(103.053623379069,13.31645894672,53.69908149772));
#137746=CARTESIAN_POINT('Ctrl Pts',(102.623789120869,12.72222884999,53.4775456014));
#137747=CARTESIAN_POINT('Ctrl Pts',(102.218370147569,12.10331314131,53.25326699941));
#137748=CARTESIAN_POINT('Ctrl Pts',(101.713794163769,11.25304338524,52.96950594007));
#137749=CARTESIAN_POINT('Ctrl Pts',(101.154507689069,10.14273559401,52.64069966665));
#137750=CARTESIAN_POINT('Ctrl Pts',(100.347069733169,8.31549541333901,52.17289680127));
#137751=CARTESIAN_POINT('Ctrl Pts',(99.1749900388691,4.91197175937601,51.50467231339));
#137752=CARTESIAN_POINT('Ctrl Pts',(98.6719824568691,1.83221907747001,51.27785989188));
#137753=CARTESIAN_POINT('Ctrl Pts',(98.5843309607691,-0.236680889114086,
51.31085228728));
#137754=CARTESIAN_POINT('Ctrl Pts',(112.026178776769,17.47584264663,57.41496060291));
#137755=CARTESIAN_POINT('Ctrl Pts',(111.054304371469,17.44067220964,56.96322273142));
#137756=CARTESIAN_POINT('Ctrl Pts',(109.637898310969,17.19839289674,56.27995401627));
#137757=CARTESIAN_POINT('Ctrl Pts',(107.864525222969,16.49257767027,55.37376659663));
#137758=CARTESIAN_POINT('Ctrl Pts',(106.645070431869,15.8045298653,54.73368567427));
#137759=CARTESIAN_POINT('Ctrl Pts',(105.502119542669,14.93766113307,54.1273069539));
#137760=CARTESIAN_POINT('Ctrl Pts',(104.626551783569,14.0776072634,53.6717926103));
#137761=CARTESIAN_POINT('Ctrl Pts',(103.979374836369,13.31165186547,53.34497834332));
#137762=CARTESIAN_POINT('Ctrl Pts',(103.524307770069,12.72281268686,53.14263950197));
#137763=CARTESIAN_POINT('Ctrl Pts',(103.095833717869,12.1083681819,52.93935575519));
#137764=CARTESIAN_POINT('Ctrl Pts',(102.563125775069,11.2619717921,52.68248156474));
#137765=CARTESIAN_POINT('Ctrl Pts',(101.973995647869,10.15375628522,52.38598466337));
#137766=CARTESIAN_POINT('Ctrl Pts',(101.124401221169,8.32857766047701,51.96347806666));
#137767=CARTESIAN_POINT('Ctrl Pts',(99.8948724104691,4.92400200723901,51.35987931168));
#137768=CARTESIAN_POINT('Ctrl Pts',(99.3745994012691,1.83743075427201,51.15495858885));
#137769=CARTESIAN_POINT('Ctrl Pts',(99.2892524687691,-0.237347620061986,
51.18649564272));
#137770=CARTESIAN_POINT('Ctrl Pts',(113.188445942169,17.47166983262,56.27542203421));
#137771=CARTESIAN_POINT('Ctrl Pts',(112.172263619869,17.42788547533,55.89634925378));
#137772=CARTESIAN_POINT('Ctrl Pts',(110.692758979669,17.17098864104,55.32530572893));
#137773=CARTESIAN_POINT('Ctrl Pts',(108.843546518669,16.45293860262,54.57208052895));
#137774=CARTESIAN_POINT('Ctrl Pts',(107.573079972769,15.7622252762,54.04093228966));
#137775=CARTESIAN_POINT('Ctrl Pts',(106.383104391469,14.90097081599,53.53723091173));
#137776=CARTESIAN_POINT('Ctrl Pts',(105.471805752069,14.05204799653,53.15666631614));
#137777=CARTESIAN_POINT('Ctrl Pts',(104.798395092669,13.29921052309,52.88163095715));
#137778=CARTESIAN_POINT('Ctrl Pts',(104.324299692669,12.7158750262,52.70763929966));
#137779=CARTESIAN_POINT('Ctrl Pts',(103.878996809469,12.10616052631,52.53481596519));
#137780=CARTESIAN_POINT('Ctrl Pts',(103.326404821569,11.26390566317,52.3171231399));
#137781=CARTESIAN_POINT('Ctrl Pts',(102.717650256469,10.15814664048,52.06780970547));
#137782=CARTESIAN_POINT('Ctrl Pts',(101.841943206069,8.33580711274201,51.71237805453));
#137783=CARTESIAN_POINT('Ctrl Pts',(100.582659540169,4.93206502020601,51.2059184364));
#137784=CARTESIAN_POINT('Ctrl Pts',(100.066369037669,1.84107373378501,51.03478639303));
#137785=CARTESIAN_POINT('Ctrl Pts',(99.9955851491691,-0.237812507849086,
51.06184076114));
#137786=CARTESIAN_POINT('Ctrl Pts',(114.125881804469,17.46819840414,54.80511293345));
#137787=CARTESIAN_POINT('Ctrl Pts',(113.075997776769,17.41492096989,54.51469436962));
#137788=CARTESIAN_POINT('Ctrl Pts',(111.549470398169,17.14056046656,54.08239064277));
#137789=CARTESIAN_POINT('Ctrl Pts',(109.646785590869,16.40654507693,53.5223372395));
#137790=CARTESIAN_POINT('Ctrl Pts',(108.341891044269,15.7114208792,53.13068024962));
#137791=CARTESIAN_POINT('Ctrl Pts',(107.121834027869,14.85569373811,52.76062809667));
#137792=CARTESIAN_POINT('Ctrl Pts',(106.189106230169,14.01930261972,52.47974204073));
#137793=CARTESIAN_POINT('Ctrl Pts',(105.501006553569,13.28178778393,52.27521181241));
#137794=CARTESIAN_POINT('Ctrl Pts',(105.016385994269,12.70458531254,52.14111418883));
#137795=CARTESIAN_POINT('Ctrl Pts',(104.562932235469,12.10030644958,52.0107829688));
#137796=CARTESIAN_POINT('Ctrl Pts',(104.002143959169,11.26286251636,51.84785983031));
#137797=CARTESIAN_POINT('Ctrl Pts',(103.388634838669,10.16016220358,51.66454860331));
#137798=CARTESIAN_POINT('Ctrl Pts',(102.510622200469,8.34157678397201,51.40350477807));
#137799=CARTESIAN_POINT('Ctrl Pts',(101.264203279969,4.93999315991101,51.03437259754));
#137800=CARTESIAN_POINT('Ctrl Pts',(100.787670666569,1.84502567070201,50.91043616355));
#137801=CARTESIAN_POINT('Ctrl Pts',(100.754059651069,-0.238314140392786,
50.9279295742));
#137802=CARTESIAN_POINT('Ctrl Pts',(114.539534408869,17.46722107301,53.67912966544));
#137803=CARTESIAN_POINT('Ctrl Pts',(113.476828137169,17.4073581895,53.45462064778));
#137804=CARTESIAN_POINT('Ctrl Pts',(111.933342665269,17.11996315362,53.12635989279));
#137805=CARTESIAN_POINT('Ctrl Pts',(110.014547047469,16.37339715948,52.71350806941));
#137806=CARTESIAN_POINT('Ctrl Pts',(108.700990537169,15.67453448001,52.42915265115));
#137807=CARTESIAN_POINT('Ctrl Pts',(107.475303053069,14.82273438004,52.1628920189));
#137808=CARTESIAN_POINT('Ctrl Pts',(106.540338441969,13.9958275305,51.96016673408));
#137809=CARTESIAN_POINT('Ctrl Pts',(105.852098050869,13.2701199685,51.81147738317));
#137810=CARTESIAN_POINT('Ctrl Pts',(105.367562667669,12.69751801236,51.70901280385));
#137811=CARTESIAN_POINT('Ctrl Pts',(104.915851437869,12.09743795773,51.61240634049));
#137812=CARTESIAN_POINT('Ctrl Pts',(104.359190902469,11.26379112788,51.49296213066));
#137813=CARTESIAN_POINT('Ctrl Pts',(103.754568792369,10.16369897044,51.36207880897));
#137814=CARTESIAN_POINT('Ctrl Pts',(102.894237682569,8.34833379260701,51.17605601973));
#137815=CARTESIAN_POINT('Ctrl Pts',(101.690546558169,4.94875024428401,50.91587031644));
#137816=CARTESIAN_POINT('Ctrl Pts',(101.268979457369,1.84978306717701,50.82795847283));
#137817=CARTESIAN_POINT('Ctrl Pts',(101.278306997869,-0.238915478837686,
50.83534589793));
#137818=CARTESIAN_POINT('Ctrl Pts',(114.722328637469,17.46712808947,53.051289402));
#137819=CARTESIAN_POINT('Ctrl Pts',(113.654564451069,17.40365408808,52.86334352169));
#137820=CARTESIAN_POINT('Ctrl Pts',(112.104688863969,17.10888025502,52.59292283969));
#137821=CARTESIAN_POINT('Ctrl Pts',(110.180954315469,16.35510969368,52.262432252));
#137822=CARTESIAN_POINT('Ctrl Pts',(108.865472379469,15.65410379572,52.03831580661));
#137823=CARTESIAN_POINT('Ctrl Pts',(107.639522339869,14.80461369374,51.83047343371));
#137824=CARTESIAN_POINT('Ctrl Pts',(106.705667287469,13.98326026859,51.67177167508));
#137825=CARTESIAN_POINT('Ctrl Pts',(106.019208150569,13.26447423575,51.55455277005));
#137826=CARTESIAN_POINT('Ctrl Pts',(105.536071241069,12.69456042945,51.46969752251));
#137827=CARTESIAN_POINT('Ctrl Pts',(105.086676320869,12.0969679499,51.39195280225));
#137828=CARTESIAN_POINT('Ctrl Pts',(104.534087620169,11.26560740794,51.29681409481));
#137829=CARTESIAN_POINT('Ctrl Pts',(103.936593793969,10.16715557418,51.19525657912));
#137830=CARTESIAN_POINT('Ctrl Pts',(103.089545611369,8.35379901046901,51.05114625581));
#137831=CARTESIAN_POINT('Ctrl Pts',(101.915640831969,4.95541579057301,50.85167903847));
#137832=CARTESIAN_POINT('Ctrl Pts',(101.529527658769,1.85347521690601,50.78336841914));
#137833=CARTESIAN_POINT('Ctrl Pts',(101.565834902869,-0.239381754617886,
50.78456512415));
#137834=CARTESIAN_POINT('',(101.414238575321,-1.58575583955758E-11,50.8108648870179));
#137835=CARTESIAN_POINT('Ctrl Pts',(101.414232124329,-1.74238401484672E-11,
50.8108622891728));
#137836=CARTESIAN_POINT('Ctrl Pts',(101.414231512955,2.34246738429908,50.8108623969735));
#137837=CARTESIAN_POINT('Ctrl Pts',(101.783910643607,4.68273078873375,50.8827213256914));
#137838=CARTESIAN_POINT('Ctrl Pts',(103.178130714759,8.98192555702816,51.1537320224966));
#137839=CARTESIAN_POINT('Ctrl Pts',(104.036052367674,10.5874908373517,51.3204960861428));
#137840=CARTESIAN_POINT('Ctrl Pts',(105.408020839001,12.7886822580781,51.5871812855231));
#137841=CARTESIAN_POINT('Ctrl Pts',(106.527871835993,14.0475405981964,51.8048594765732));
#137842=CARTESIAN_POINT('Ctrl Pts',(108.895550762846,15.7646605470862,52.2650921011255));
#137843=CARTESIAN_POINT('Ctrl Pts',(109.922967445704,16.3125473846403,52.4648027231681));
#137844=CARTESIAN_POINT('Ctrl Pts',(112.097867784466,17.1144886571945,52.8875627106287));
#137845=CARTESIAN_POINT('Ctrl Pts',(113.233562723013,17.3623385458543,53.1083205694869));
#137846=CARTESIAN_POINT('Ctrl Pts',(114.384105789773,17.4511159784776,53.3319646111095));
#137847=CARTESIAN_POINT('',(90.732949730332,1.38578833057197E-14,52.6942600470911));
#137848=CARTESIAN_POINT('',(90.7329496419691,1.4210854715202E-14,52.69425954596));
#137849=CARTESIAN_POINT('',(90.1948181095954,4.38657743647023,53.1165555002035));
#137850=CARTESIAN_POINT('Ctrl Pts',(90.7329498186953,1.3510709105438E-14,
52.6942605482239));
#137851=CARTESIAN_POINT('Ctrl Pts',(90.7329485107428,0.219822085862891,
52.6942607788508));
#137852=CARTESIAN_POINT('Ctrl Pts',(90.7292741915679,0.43943636238306,52.6973774297948));
#137853=CARTESIAN_POINT('Ctrl Pts',(90.7218295116067,0.658717449913899,
52.7036013862621));
#137854=CARTESIAN_POINT('Ctrl Pts',(90.716851108255,0.805355009462212,52.7077634678961));
#137855=CARTESIAN_POINT('Ctrl Pts',(90.7101855631875,0.95184333440204,52.7133151173478));
#137856=CARTESIAN_POINT('Ctrl Pts',(90.7017909963613,1.09814271743628,52.7202539366756));
#137857=CARTESIAN_POINT('Ctrl Pts',(90.6890221508373,1.32067644203491,52.7308084672368));
#137858=CARTESIAN_POINT('Ctrl Pts',(90.672255291451,1.54277324072251,52.7445723874834));
#137859=CARTESIAN_POINT('Ctrl Pts',(90.6512991909533,1.76428767234441,52.7615386845998));
#137860=CARTESIAN_POINT('Ctrl Pts',(90.6464708510102,1.81532517229662,52.7654477634888));
#137861=CARTESIAN_POINT('Ctrl Pts',(90.6414199063934,1.86633173329605,52.7695268501241));
#137862=CARTESIAN_POINT('Ctrl Pts',(90.6361436310377,1.91730553703418,52.7737758750406));
#137863=CARTESIAN_POINT('Ctrl Pts',(90.629541216305,1.98109109978426,52.7790928501447));
#137864=CARTESIAN_POINT('Ctrl Pts',(90.6224695805114,2.04579464308325,52.7847639911231));
#137865=CARTESIAN_POINT('Ctrl Pts',(90.6151687013308,2.10936825487059,52.7906050704508));
#137866=CARTESIAN_POINT('Ctrl Pts',(90.6120838169945,2.13623039494425,52.7930731367864));
#137867=CARTESIAN_POINT('Ctrl Pts',(90.6089579305889,2.16289088087897,52.7955709051654));
#137868=CARTESIAN_POINT('Ctrl Pts',(90.6058088683883,2.18919559519112,52.798081728641));
#137869=CARTESIAN_POINT('Ctrl Pts',(90.5822808745777,2.38572939354042,52.8168411673025));
#137870=CARTESIAN_POINT('Ctrl Pts',(90.554990387312,2.58427754605148,52.838383537977));
#137871=CARTESIAN_POINT('Ctrl Pts',(90.5237507685048,2.78470597157349,52.8628583306962));
#137872=CARTESIAN_POINT('Ctrl Pts',(90.492846253712,2.98298442303857,52.8870705849593));
#137873=CARTESIAN_POINT('Ctrl Pts',(90.4580769981051,3.18310296691071,52.9141526371188));
#137874=CARTESIAN_POINT('Ctrl Pts',(90.4192138488107,3.38491904070291,52.9442554065099));
#137875=CARTESIAN_POINT('Ctrl Pts',(90.3809087028403,3.58383740697335,52.973925955515));
#137876=CARTESIAN_POINT('Ctrl Pts',(90.3386264457378,3.7844048324515,53.006531054824));
#137877=CARTESIAN_POINT('Ctrl Pts',(90.2920989964633,3.98647333373282,53.0422219666209));
#137878=CARTESIAN_POINT('Ctrl Pts',(90.2615363499203,4.11920676912283,53.0656663793075));
#137879=CARTESIAN_POINT('Ctrl Pts',(90.2291409815297,4.25258765915242,53.0904424057959));
#137880=CARTESIAN_POINT('Ctrl Pts',(90.194825018716,4.38657155579178,53.1165946859612));
#137881=CARTESIAN_POINT('',(90.6495102260087,12.954682194379,55.6952426313253));
#137882=CARTESIAN_POINT('Origin',(94.1069496688351,2.20409106096583,75.3033561008651));
#137883=CARTESIAN_POINT('Ctrl Pts',(91.9214587222691,17.49925882517,62.90882101338));
#137884=CARTESIAN_POINT('Ctrl Pts',(91.7897413843421,17.5095848512144,62.1618148632487));
#137885=CARTESIAN_POINT('Ctrl Pts',(91.6577816154482,17.411296596711,61.4134338249997));
#137886=CARTESIAN_POINT('Ctrl Pts',(91.4039281348835,17.0053502190289,59.9737591958263));
#137887=CARTESIAN_POINT('Ctrl Pts',(91.2820620248445,16.6977362346282,59.2826221415342));
#137888=CARTESIAN_POINT('Ctrl Pts',(91.0581949381514,15.8978221226527,58.0130088027607));
#137889=CARTESIAN_POINT('Ctrl Pts',(90.9562183026917,15.4056089701893,57.4346705640518));
#137890=CARTESIAN_POINT('Ctrl Pts',(90.7803324463945,14.27602564985,56.4371723049057));
#137891=CARTESIAN_POINT('Ctrl Pts',(90.7064423497252,13.638778302204,56.0181207430154));
#137892=CARTESIAN_POINT('Ctrl Pts',(90.6495104561691,12.95468496362,55.69524393663));
#137893=CARTESIAN_POINT('Origin',(59.0011724705691,9.5,68.602980224451));
#137894=CARTESIAN_POINT('',(83.7957739555191,12.95454545455,56.90402403487));
#137895=CARTESIAN_POINT('',(57.7481818513099,12.9545454545505,61.4969173053291));
#137896=CARTESIAN_POINT('',(62.2792373804991,12.95454545455,60.69796996444));
#137897=CARTESIAN_POINT('Ctrl Pts',(83.7957739555191,12.95454545455,56.90402403487));
#137898=CARTESIAN_POINT('Ctrl Pts',(83.0133127087731,13.2847992676121,57.2025428398695));
#137899=CARTESIAN_POINT('Ctrl Pts',(82.217562215713,13.5674612430145,57.5082348281082));
#137900=CARTESIAN_POINT('Ctrl Pts',(81.0003150353501,13.9277132722418,57.9566193292432));
#137901=CARTESIAN_POINT('Ctrl Pts',(80.5906421136752,14.0372001888329,58.1044625659918));
#137902=CARTESIAN_POINT('Ctrl Pts',(79.9698970938941,14.1865988501334,58.3218159564353));
#137903=CARTESIAN_POINT('Ctrl Pts',(79.7619435503995,14.2339265143701,58.3935360164034));
#137904=CARTESIAN_POINT('Ctrl Pts',(79.4484180778543,14.301340535532,58.4998076676419));
#137905=CARTESIAN_POINT('Ctrl Pts',(79.2912566167019,14.3341531242538,58.5526167490743));
#137906=CARTESIAN_POINT('Ctrl Pts',(79.1071963062216,14.3708970404008,58.6136129848518));
#137907=CARTESIAN_POINT('Ctrl Pts',(79.0149889433721,14.388888047566,58.6439524683737));
#137908=CARTESIAN_POINT('Ctrl Pts',(78.9754334348911,14.3965172099578,58.6569205768522));
#137909=CARTESIAN_POINT('Ctrl Pts',(78.9490546261753,14.4015852985292,58.6655582511411));
#137910=CARTESIAN_POINT('Ctrl Pts',(78.9373941718083,14.4038180465107,58.6693724089674));
#137911=CARTESIAN_POINT('Ctrl Pts',(77.9798750059046,14.5863595677044,58.982145272868));
#137912=CARTESIAN_POINT('Ctrl Pts',(77.0389885802272,14.7155633134542,59.2616322996393));
#137913=CARTESIAN_POINT('Ctrl Pts',(75.1580251893373,14.8862983920454,59.7466792551828));
#137914=CARTESIAN_POINT('Ctrl Pts',(74.2194735186116,14.9279095443054,59.9520359248502));
#137915=CARTESIAN_POINT('Ctrl Pts',(72.3362019298778,14.9285030082817,60.2846641550829));
#137916=CARTESIAN_POINT('Ctrl Pts',(71.3813453465866,14.8873352533677,60.4135762102816));
#137917=CARTESIAN_POINT('Ctrl Pts',(69.929932584552,14.7597504534105,60.5548297946571));
#137918=CARTESIAN_POINT('Ctrl Pts',(69.4429550025655,14.7061728352107,60.5933116755178));
#137919=CARTESIAN_POINT('Ctrl Pts',(68.707957642145,14.6081459867842,60.6394292750915));
#137920=CARTESIAN_POINT('Ctrl Pts',(68.4622043899207,14.5725229325201,60.6528734602013));
#137921=CARTESIAN_POINT('Ctrl Pts',(68.0924816871676,14.5144985780408,60.6703648438653));
#137922=CARTESIAN_POINT('Ctrl Pts',(67.9073472349735,14.4843386444438,60.678442409307));
#137923=CARTESIAN_POINT('Ctrl Pts',(67.6908886492797,14.4471035306693,60.6867510899369));
#137924=CARTESIAN_POINT('Ctrl Pts',(67.5825435380976,14.4279686423172,60.6906339004071));
#137925=CARTESIAN_POINT('Ctrl Pts',(67.5360852400895,14.4196565580321,60.6922405669924));
#137926=CARTESIAN_POINT('Ctrl Pts',(67.5051075729281,14.4140903461212,60.6932990127326));
#137927=CARTESIAN_POINT('Ctrl Pts',(67.4880470149196,14.4110104881042,60.6938742152985));
#137928=CARTESIAN_POINT('Ctrl Pts',(66.5829022554768,14.246975254239,60.7240530637672));
#137929=CARTESIAN_POINT('Ctrl Pts',(65.7032005986795,14.0487671761914,60.7324930540725));
#137930=CARTESIAN_POINT('Ctrl Pts',(63.9702005699335,13.5677992372404,60.7259230034294));
#137931=CARTESIAN_POINT('Ctrl Pts',(63.1168951126647,13.2849117826608,60.7108727796349));
#137932=CARTESIAN_POINT('Ctrl Pts',(62.2792373804991,12.95454545455,60.69796996444));
#137933=CARTESIAN_POINT('',(35.8057492453862,12.954533742859,65.3659544670989));
#137934=CARTESIAN_POINT('',(35.8057492437391,12.9545337474,65.365954457758));
#137935=CARTESIAN_POINT('Ctrl Pts',(27.1339043807864,17.4992593326224,74.332577004777));
#137936=CARTESIAN_POINT('Ctrl Pts',(27.1004755498448,17.5013230293304,74.1844849117931));
#137937=CARTESIAN_POINT('Ctrl Pts',(27.0833154043488,17.4990844600161,74.0324117451327));
#137938=CARTESIAN_POINT('Ctrl Pts',(27.0823021127142,17.4923856215589,73.8767964544402));
#137939=CARTESIAN_POINT('Ctrl Pts',(27.0821988672121,17.4917030688602,73.8609406255081));
#137940=CARTESIAN_POINT('Ctrl Pts',(27.0822632579981,17.4909742525328,73.8450480376792));
#137941=CARTESIAN_POINT('Ctrl Pts',(27.0824951578953,17.4901990342879,73.8291191649141));
#137942=CARTESIAN_POINT('Ctrl Pts',(27.083749085873,17.4860072780265,73.7429886428489));
#137943=CARTESIAN_POINT('Ctrl Pts',(27.0898942862776,17.4804584368264,73.6557991836374));
#137944=CARTESIAN_POINT('Ctrl Pts',(27.1008711748689,17.4735341927033,73.5676395575947));
#137945=CARTESIAN_POINT('Ctrl Pts',(27.1063596191646,17.4700720706418,73.5235597445734));
#137946=CARTESIAN_POINT('Ctrl Pts',(27.1130555616134,17.4662661865554,73.4792375515588));
#137947=CARTESIAN_POINT('Ctrl Pts',(27.1209489341839,17.4621148189795,73.4346850580882));
#137948=CARTESIAN_POINT('Ctrl Pts',(27.1248956204691,17.4600391351915,73.4124088113529));
#137949=CARTESIAN_POINT('Ctrl Pts',(27.1291416643071,17.4578770862192,73.3900749896304));
#137950=CARTESIAN_POINT('Ctrl Pts',(27.1336856062651,17.4556284958465,73.3676851765544));
#137951=CARTESIAN_POINT('Ctrl Pts',(27.1359575772442,17.4545042006602,73.3564902700165));
#137952=CARTESIAN_POINT('Ctrl Pts',(27.1383040227537,17.453358270503,73.3452813656432));
#137953=CARTESIAN_POINT('Ctrl Pts',(27.1407247545212,17.4521906857515,73.3340586634897));
#137954=CARTESIAN_POINT('Ctrl Pts',(27.141935120405,17.4516068933757,73.328447312413));
#137955=CARTESIAN_POINT('Ctrl Pts',(27.1431640578532,17.4510176873753,73.3228325118908));
#137956=CARTESIAN_POINT('Ctrl Pts',(27.1444115426407,17.450423065456,73.3172142871795));
#137957=CARTESIAN_POINT('Ctrl Pts',(27.1450352850345,17.4501257544963,73.3144051748238));
#137958=CARTESIAN_POINT('Ctrl Pts',(27.1456636642631,17.4498270895585,73.3115952064208));
#137959=CARTESIAN_POINT('Ctrl Pts',(27.1462966772528,17.4495270703657,73.3087843851438));
#137960=CARTESIAN_POINT('Ctrl Pts',(27.1469296902425,17.4492270511729,73.3059735638669));
#137961=CARTESIAN_POINT('Ctrl Pts',(27.148048434925,17.4486989193247,73.3010551686142));
#137962=CARTESIAN_POINT('Ctrl Pts',(27.1482096144174,17.4486229497522,73.3003493658695));
#137963=CARTESIAN_POINT('Ctrl Pts',(27.150160414395,17.4477034690033,73.2918068400282));
#137964=CARTESIAN_POINT('Ctrl Pts',(27.1531238189679,17.44622437278,73.2781678243283));
#137965=CARTESIAN_POINT('Ctrl Pts',(27.1574605143924,17.4441195119101,73.2594149631964));
#137966=CARTESIAN_POINT('Ctrl Pts',(27.1618294381679,17.44199900867,73.2405227393166));
#137967=CARTESIAN_POINT('Ctrl Pts',(27.1675921197014,17.4392433624406,73.2164402649787));
#137968=CARTESIAN_POINT('Ctrl Pts',(27.175118673911,17.4357324635244,73.1871573227636));
#137969=CARTESIAN_POINT('Ctrl Pts',(27.1798738414059,17.4335143286463,73.1686567857185));
#137970=CARTESIAN_POINT('Ctrl Pts',(27.1853330904777,17.4309936843549,73.1480806187073));
#137971=CARTESIAN_POINT('Ctrl Pts',(27.1915900942525,17.4281297140575,73.1254281615822));
#137972=CARTESIAN_POINT('Ctrl Pts',(27.2017238681702,17.423491259528,73.0887404932591));
#137973=CARTESIAN_POINT('Ctrl Pts',(27.2140254713927,17.4179557691698,73.0466003184545));
#137974=CARTESIAN_POINT('Ctrl Pts',(27.2291892582858,17.4113126615092,72.9990018979463));
#137975=CARTESIAN_POINT('Ctrl Pts',(27.2334716706586,17.4094365782696,72.9855596050448));
#137976=CARTESIAN_POINT('Ctrl Pts',(27.2379823734776,17.4074718479973,72.9716820713348));
#137977=CARTESIAN_POINT('Ctrl Pts',(27.2427370439477,17.405413012191,72.9573693812311));
#137978=CARTESIAN_POINT('Ctrl Pts',(27.2535323926152,17.4007384820595,72.9248728115929));
#137979=CARTESIAN_POINT('Ctrl Pts',(27.2655909865458,17.395579465856,72.8901326364219));
#137980=CARTESIAN_POINT('Ctrl Pts',(27.2791261782035,17.3898672147487,72.8531515151637));
#137981=CARTESIAN_POINT('Ctrl Pts',(27.2858937740323,17.387011089195,72.8346609545345));
#137982=CARTESIAN_POINT('Ctrl Pts',(27.2930307851191,17.3840165437743,72.815610211533));
#137983=CARTESIAN_POINT('Ctrl Pts',(27.3005652978913,17.3808743509666,72.7960000009259));
#137984=CARTESIAN_POINT('Ctrl Pts',(27.3043325542774,17.3793032545628,72.7861948956223));
#137985=CARTESIAN_POINT('Ctrl Pts',(27.3081991863097,17.3776952390278,72.7762499246924));
#137986=CARTESIAN_POINT('Ctrl Pts',(27.3121687931104,17.3760491150648,72.7661652096357));
#137987=CARTESIAN_POINT('Ctrl Pts',(27.3141535965107,17.3752260530833,72.7611228521074));
#137988=CARTESIAN_POINT('Ctrl Pts',(27.3161641436162,17.3743934635576,72.7560455586216));
#137989=CARTESIAN_POINT('Ctrl Pts',(27.3182008861748,17.373551195464,72.7509333458515));
#137990=CARTESIAN_POINT('Ctrl Pts',(27.3202376287334,17.3727089273704,72.7458211330813));
#137991=CARTESIAN_POINT('Ctrl Pts',(27.3230518402653,17.3715471437269,72.7388108924576));
#137992=CARTESIAN_POINT('Ctrl Pts',(27.3243901532579,17.370995202871,72.7354919671642));
#137993=CARTESIAN_POINT('Ctrl Pts',(27.3586789474081,17.3568539769431,72.6504580873365));
#137994=CARTESIAN_POINT('Ctrl Pts',(27.3948271474531,17.3423208187618,72.5695377921547));
#137995=CARTESIAN_POINT('Ctrl Pts',(27.4317540105819,17.327729922424,72.4927918293785));
#137996=CARTESIAN_POINT('Ctrl Pts',(27.4409480584284,17.3240970820556,72.4736836248356));
#137997=CARTESIAN_POINT('Ctrl Pts',(27.4501903682747,17.3204604130413,72.4548341453743));
#137998=CARTESIAN_POINT('Ctrl Pts',(27.4594642451486,17.3168245836903,72.4362442479077));
#137999=CARTESIAN_POINT('Ctrl Pts',(27.4827249273224,17.307705218389,72.3896171789382));
#138000=CARTESIAN_POINT('Ctrl Pts',(27.5061926001715,17.29859169437,72.3446219551981));
#138001=CARTESIAN_POINT('Ctrl Pts',(27.5296499512157,17.2895528123642,72.3012647331953));
#138002=CARTESIAN_POINT('Ctrl Pts',(27.5413786267377,17.2850333713613,72.2795861221939));
#138003=CARTESIAN_POINT('Ctrl Pts',(27.5531052823504,17.2805324687434,72.2583168748899));
#138004=CARTESIAN_POINT('Ctrl Pts',(27.5648031624215,17.276058236252,72.2374584671607));
#138005=CARTESIAN_POINT('Ctrl Pts',(27.570652102457,17.2738211200063,72.2270292632961));
#138006=CARTESIAN_POINT('Ctrl Pts',(27.5764938488926,17.2715906652919,72.2167027709439));
#138007=CARTESIAN_POINT('Ctrl Pts',(27.5823252955446,17.2693678466743,72.2064791177919));
#138008=CARTESIAN_POINT('Ctrl Pts',(27.5878485743336,17.267262494837,72.19679574247));
#138009=CARTESIAN_POINT('Ctrl Pts',(27.5925029488425,17.2654901196184,72.1886875932158));
#138010=CARTESIAN_POINT('Ctrl Pts',(27.5987284984472,17.2631248903857,72.1779409680902));
#138011=CARTESIAN_POINT('Ctrl Pts',(27.5990758490682,17.2629929239097,72.1773413669067));
#138012=CARTESIAN_POINT('Ctrl Pts',(27.599428091347,17.262859098644,72.1767335553565));
#138013=CARTESIAN_POINT('Ctrl Pts',(27.5997856493164,17.2627232487334,72.1761168028097));
#138014=CARTESIAN_POINT('Ctrl Pts',(27.6731296190087,17.2348570771554,72.0496056242957));
#138015=CARTESIAN_POINT('Ctrl Pts',(27.7532636202495,17.2048468369855,71.9236412018619));
#138016=CARTESIAN_POINT('Ctrl Pts',(27.8389310916625,17.1729569092371,71.7987901761038));
#138017=CARTESIAN_POINT('Ctrl Pts',(27.8797101576983,17.1577768012208,71.7393591208848));
#138018=CARTESIAN_POINT('Ctrl Pts',(27.9217429902264,17.1421714406541,71.6801799654615));
#138019=CARTESIAN_POINT('Ctrl Pts',(27.9648936660156,17.1261728112818,71.6213116197419));
#138020=CARTESIAN_POINT('Ctrl Pts',(28.0317938438829,17.1013687698372,71.5300429958473));
#138021=CARTESIAN_POINT('Ctrl Pts',(28.1013819438649,17.0756201944387,71.4395217235677));
#138022=CARTESIAN_POINT('Ctrl Pts',(28.1733653960537,17.0490115864612,71.3498049863921));
#138023=CARTESIAN_POINT('Ctrl Pts',(28.209357122148,17.0357072824725,71.3049466178042));
#138024=CARTESIAN_POINT('Ctrl Pts',(28.2459476825176,17.0221879445018,71.2602893615747));
#138025=CARTESIAN_POINT('Ctrl Pts',(28.2831003535614,17.008463870423,71.2158399693841));
#138026=CARTESIAN_POINT('Ctrl Pts',(28.3016766890833,17.0016018333835,71.1936152732888));
#138027=CARTESIAN_POINT('Ctrl Pts',(28.3203935521594,16.9946886107542,71.1714425425548));
#138028=CARTESIAN_POINT('Ctrl Pts',(28.3392463464684,16.9877254772434,71.1493226090831));
#138029=CARTESIAN_POINT('Ctrl Pts',(28.3486727436229,16.9842439104881,71.1382626423472));
#138030=CARTESIAN_POINT('Ctrl Pts',(28.3581331235798,16.9807498659209,71.1272158748941));
#138031=CARTESIAN_POINT('Ctrl Pts',(28.3676269112532,16.977243501931,71.1161824095321));
#138032=CARTESIAN_POINT('Ctrl Pts',(28.3759339754674,16.9741754334398,71.1065281273403));
#138033=CARTESIAN_POINT('Ctrl Pts',(28.384266617464,16.9710979328851,71.0968840295599));
#138034=CARTESIAN_POINT('Ctrl Pts',(28.3926244517788,16.9680111060067,71.0872501846531));
#138035=CARTESIAN_POINT('Ctrl Pts',(28.3938184281095,16.9675701307383,71.085873921095));
#138036=CARTESIAN_POINT('Ctrl Pts',(28.396011528671,16.9667601442857,71.0833481357132));
#138037=CARTESIAN_POINT('Ctrl Pts',(28.3962079220283,16.9666876095051,71.0831220218952));
#138038=CARTESIAN_POINT('Ctrl Pts',(28.4028245292768,16.9642438702571,71.0755041149173));
#138039=CARTESIAN_POINT('Ctrl Pts',(28.4139881583462,16.9600125484294,71.0623773395018));
#138040=CARTESIAN_POINT('Ctrl Pts',(28.4298813084446,16.953960153376,71.0438049802813));
#138041=CARTESIAN_POINT('Ctrl Pts',(28.4459334925285,16.9478471953442,71.0250467777077));
#138042=CARTESIAN_POINT('Ctrl Pts',(28.4668103103473,16.9398763984077,71.0007333945629));
#138043=CARTESIAN_POINT('Ctrl Pts',(28.4927033905768,16.9299635737908,70.9709504280054));
#138044=CARTESIAN_POINT('Ctrl Pts',(28.519012725448,16.9198913915686,70.9406886733715));
#138045=CARTESIAN_POINT('Ctrl Pts',(28.5505008736301,16.9078141092849,70.9047799095888));
#138046=CARTESIAN_POINT('Ctrl Pts',(28.5873728555423,16.8935943466494,70.8633366170196));
#138047=CARTESIAN_POINT('Ctrl Pts',(28.6147878724832,16.8830216837946,70.8325227440203));
#138048=CARTESIAN_POINT('Ctrl Pts',(28.6451792624566,16.8712635678662,70.7986497232713));
#138049=CARTESIAN_POINT('Ctrl Pts',(28.6786328453021,16.858247180522,70.7617725771743));
#138050=CARTESIAN_POINT('Ctrl Pts',(28.7254438564832,16.8400335782205,70.7101710340379));
#138051=CARTESIAN_POINT('Ctrl Pts',(28.7783196309919,16.8193690026626,70.6527006291921));
#138052=CARTESIAN_POINT('Ctrl Pts',(28.8376378439644,16.7960271061273,70.5895420513129));
#138053=CARTESIAN_POINT('Ctrl Pts',(28.8838583335065,16.7778392034472,70.5403291663984));
#138054=CARTESIAN_POINT('Ctrl Pts',(28.9339904209272,16.7580247761307,70.4876632911371));
#138055=CARTESIAN_POINT('Ctrl Pts',(28.9882152012452,16.7364598942736,70.4316436451738));
#138056=CARTESIAN_POINT('Ctrl Pts',(29.0501229505528,16.7118395400364,70.367686720346));
#138057=CARTESIAN_POINT('Ctrl Pts',(29.1173684817007,16.6849368572625,70.2993549323575));
#138058=CARTESIAN_POINT('Ctrl Pts',(29.1902208716677,16.6555381225991,70.22679954364));
#138059=CARTESIAN_POINT('Ctrl Pts',(29.2266470666512,16.6408387552674,70.1905218492813));
#138060=CARTESIAN_POINT('Ctrl Pts',(29.2644748191839,16.6255149672994,70.1531884917144));
#138061=CARTESIAN_POINT('Ctrl Pts',(29.3037357471969,16.6095371671074,70.114819153979));
#138062=CARTESIAN_POINT('Ctrl Pts',(29.3233662112033,16.6015482670114,70.0956344851113));
#138063=CARTESIAN_POINT('Ctrl Pts',(29.3433549711418,16.5933958376689,70.0761908328954));
#138064=CARTESIAN_POINT('Ctrl Pts',(29.3637057369433,16.5850759688277,70.0564906734208));
#138065=CARTESIAN_POINT('Ctrl Pts',(29.373881119844,16.5809160344071,70.0466405936834));
#138066=CARTESIAN_POINT('Ctrl Pts',(29.3841470043436,16.5767142384171,70.0367263878862));
#138067=CARTESIAN_POINT('Ctrl Pts',(29.3945038436147,16.5724700796614,70.0267483679313));
#138068=CARTESIAN_POINT('Ctrl Pts',(29.3996822632502,16.5703480002836,70.0217593579538));
#138069=CARTESIAN_POINT('Ctrl Pts',(29.4048834215875,16.568215330108,70.0167543944867));
#138070=CARTESIAN_POINT('Ctrl Pts',(29.410107374287,16.566072005633,70.0117335165982));
#138071=CARTESIAN_POINT('Ctrl Pts',(29.4127193506368,16.5650003433955,70.009223077654));
#138072=CARTESIAN_POINT('Ctrl Pts',(29.4153370255777,16.5639260175764,70.0067086601076));
#138073=CARTESIAN_POINT('Ctrl Pts',(29.4179604059968,16.5628490201828,70.0041902688462));
#138074=CARTESIAN_POINT('Ctrl Pts',(29.4205837864159,16.5617720227891,70.0016718775848));
#138075=CARTESIAN_POINT('Ctrl Pts',(29.424205760984,16.560284485163,69.9981974973265));
#138076=CARTESIAN_POINT('Ctrl Pts',(29.4258476705543,16.5596100052536,69.9966231788122));
#138077=CARTESIAN_POINT('Ctrl Pts',(29.5731714058286,16.4990908990772,69.855364190961));
#138078=CARTESIAN_POINT('Ctrl Pts',(29.7237179933999,16.4362228320212,69.7157522642118));
#138079=CARTESIAN_POINT('Ctrl Pts',(29.8768576760397,16.3710141156729,69.5777144562597));
#138080=CARTESIAN_POINT('Ctrl Pts',(30.0311166199704,16.3053288044226,69.4386677630046));
#138081=CARTESIAN_POINT('Ctrl Pts',(30.188006633286,16.2372682938278,69.3012178920274));
#138082=CARTESIAN_POINT('Ctrl Pts',(30.3468876316625,16.1667922714889,69.1653106062159));
#138083=CARTESIAN_POINT('Ctrl Pts',(30.4802922276503,16.1076170058309,69.0511959119431));
#138084=CARTESIAN_POINT('Ctrl Pts',(30.6151005391363,16.0467378435994,68.9381690077916));
#138085=CARTESIAN_POINT('Ctrl Pts',(30.7509361135523,15.984106325019,68.8262117122634));
#138086=CARTESIAN_POINT('Ctrl Pts',(30.9800432215038,15.8784688574391,68.6373789097902));
#138087=CARTESIAN_POINT('Ctrl Pts',(31.2122750465286,15.7680432382575,68.4518448887416));
#138088=CARTESIAN_POINT('Ctrl Pts',(31.4463514062206,15.6531308717712,68.2701385686671));
#138089=CARTESIAN_POINT('Ctrl Pts',(31.5633895860667,15.5956746885281,68.1792854086299));
#138090=CARTESIAN_POINT('Ctrl Pts',(31.6808886741266,15.537097401388,68.0893890476009));
#138091=CARTESIAN_POINT('Ctrl Pts',(31.798687387191,15.4774338689085,68.0005085340514));
#138092=CARTESIAN_POINT('Ctrl Pts',(31.8575867437232,15.4476021026688,67.9560682772767));
#138093=CARTESIAN_POINT('Ctrl Pts',(31.9165610000085,15.4174982654751,67.9118813578827));
#138094=CARTESIAN_POINT('Ctrl Pts',(31.9755899880513,15.3871250965545,67.8679533533156));
#138095=CARTESIAN_POINT('Ctrl Pts',(32.0051044820726,15.3719385120942,67.845989351032));
#138096=CARTESIAN_POINT('Ctrl Pts',(32.034632659388,15.3566845944791,67.8240900794668));
#138097=CARTESIAN_POINT('Ctrl Pts',(32.06417199853,15.3413636826288,67.8022562455776));
#138098=CARTESIAN_POINT('Ctrl Pts',(32.0900189202792,15.3279578847597,67.7831516409246));
#138099=CARTESIAN_POINT('Ctrl Pts',(32.1158743878235,15.3145007944122,67.7640971371143));
#138100=CARTESIAN_POINT('Ctrl Pts',(32.1417367124484,15.3009926380724,67.7450932124781));
#138101=CARTESIAN_POINT('Ctrl Pts',(32.145431330252,15.2990629014524,67.7423783661015));
#138102=CARTESIAN_POINT('Ctrl Pts',(32.1479130755241,15.2977663283766,67.7405551425058));
#138103=CARTESIAN_POINT('Ctrl Pts',(32.1528209807404,15.2952003023608,67.7369517714385));
#138104=CARTESIAN_POINT('Ctrl Pts',(32.3674042552043,15.1830085951946,67.5794052972008));
#138105=CARTESIAN_POINT('Ctrl Pts',(32.5818793710549,15.0673300016252,67.4254656364288));
#138106=CARTESIAN_POINT('Ctrl Pts',(32.795626850551,14.9481755404271,67.2752501948076));
#138107=CARTESIAN_POINT('Ctrl Pts',(33.0082233998999,14.8296626702406,67.1258435930415));
#138108=CARTESIAN_POINT('Ctrl Pts',(33.2201000592884,14.7077107704291,66.9801208237245));
#138109=CARTESIAN_POINT('Ctrl Pts',(33.4306541547144,14.5822979782621,66.8382362586377));
#138110=CARTESIAN_POINT('Ctrl Pts',(33.6281592547383,14.4646575875059,66.7051449256829));
#138111=CARTESIAN_POINT('Ctrl Pts',(33.8245006551659,14.3439713652497,66.5754308735912));
#138112=CARTESIAN_POINT('Ctrl Pts',(34.0191872456239,14.2202007978378,66.4492573184544));
#138113=CARTESIAN_POINT('Ctrl Pts',(34.1910295959593,14.1109532879997,66.3378887839607));
#138114=CARTESIAN_POINT('Ctrl Pts',(34.3617795191168,13.9992396404704,66.2291951224791));
#138115=CARTESIAN_POINT('Ctrl Pts',(34.5313274049966,13.884910999406,66.1232213719099));
#138116=CARTESIAN_POINT('Ctrl Pts',(34.6992531288876,13.771676206105,66.0182615330689));
#138117=CARTESIAN_POINT('Ctrl Pts',(34.8659996684362,13.6558758152753,65.9159695916096));
#138118=CARTESIAN_POINT('Ctrl Pts',(35.0314688615146,13.5373489443009,65.8164365574236));
#138119=CARTESIAN_POINT('Ctrl Pts',(35.1940003305946,13.420926387893,65.7186706230687));
#138120=CARTESIAN_POINT('Ctrl Pts',(35.355299383326,13.3018728903959,65.6235663722552));
#138121=CARTESIAN_POINT('Ctrl Pts',(35.5152815034465,13.1800262567294,65.5312583148745));
#138122=CARTESIAN_POINT('Ctrl Pts',(35.6125969994222,13.1059081891647,65.4751082627324));
#138123=CARTESIAN_POINT('Ctrl Pts',(35.7094253755256,13.0307564497627,65.41999379509));
#138124=CARTESIAN_POINT('Ctrl Pts',(35.8057492503273,12.9545337292362,65.3659544951215));
#138125=CARTESIAN_POINT('Ctrl Pts',(27.3191400010791,17.49826943671,74.421637315687));
#138126=CARTESIAN_POINT('Ctrl Pts',(26.9498075064491,17.49016994831,74.507602053806));
#138127=CARTESIAN_POINT('Ctrl Pts',(26.4148506048091,17.51742193092,74.633280388995));
#138128=CARTESIAN_POINT('Ctrl Pts',(25.7230268640091,17.62730114969,74.798040434501));
#138129=CARTESIAN_POINT('Ctrl Pts',(25.2463297175291,17.7348343146,74.912517844996));
#138130=CARTESIAN_POINT('Ctrl Pts',(24.7773466811991,17.87289212671,75.026106644434));
#138131=CARTESIAN_POINT('Ctrl Pts',(24.1186923675691,18.11371974695,75.187036750685));
#138132=CARTESIAN_POINT('Ctrl Pts',(23.6367652953191,18.35052078424,75.30659770678));
#138133=CARTESIAN_POINT('Ctrl Pts',(23.3168213892291,18.53758431057,75.386865081271));
#138134=CARTESIAN_POINT('Ctrl Pts',(27.1799956085391,17.51200319618,73.9592992548583));
#138135=CARTESIAN_POINT('Ctrl Pts',(26.8048647613891,17.50670814829,74.002495728156));
#138136=CARTESIAN_POINT('Ctrl Pts',(26.2612602759991,17.53721130111,74.06386792449));
#138137=CARTESIAN_POINT('Ctrl Pts',(25.5574177012091,17.64971366655,74.141020185911));
#138138=CARTESIAN_POINT('Ctrl Pts',(25.0720160815391,17.7583874709,74.193250720675));
#138139=CARTESIAN_POINT('Ctrl Pts',(24.5939754596591,17.89690459352,74.243706306264));
#138140=CARTESIAN_POINT('Ctrl Pts',(23.9217915560591,18.1374439731,74.313235070235));
#138141=CARTESIAN_POINT('Ctrl Pts',(23.4288088080691,18.37287922197,74.362412782871));
#138142=CARTESIAN_POINT('Ctrl Pts',(23.1008469738591,18.55854189444,74.394250202332));
#138143=CARTESIAN_POINT('Ctrl Pts',(27.2466786265891,17.46814185615,73.2575872353228));
#138144=CARTESIAN_POINT('Ctrl Pts',(26.8556174534391,17.45360018152,73.2420308847567));
#138145=CARTESIAN_POINT('Ctrl Pts',(26.2878069083791,17.47344346426,73.2150078795167));
#138146=CARTESIAN_POINT('Ctrl Pts',(25.5515499179291,17.57740259896,73.1712133705486));
#138147=CARTESIAN_POINT('Ctrl Pts',(25.0435347167691,17.68239329966,73.1372119678006));
#138148=CARTESIAN_POINT('Ctrl Pts',(24.5431543670891,17.81947498135,73.0998283922469));
#138149=CARTESIAN_POINT('Ctrl Pts',(23.8397272546891,18.06108459844,73.0415257181794));
#138150=CARTESIAN_POINT('Ctrl Pts',(23.3243855329991,18.30113729463,72.9912760097607));
#138151=CARTESIAN_POINT('Ctrl Pts',(22.9821563396191,18.4915383548,72.9540702371875));
#138152=CARTESIAN_POINT('Ctrl Pts',(27.6908059692291,17.31239362199,72.32988049079));
#138153=CARTESIAN_POINT('Ctrl Pts',(27.2686542733791,17.26783708843,72.2493782757269));
#138154=CARTESIAN_POINT('Ctrl Pts',(26.6529460569991,17.25236955023,72.1211498844787));
#138155=CARTESIAN_POINT('Ctrl Pts',(25.8538764569291,17.32739312776,71.933840809013));
#138156=CARTESIAN_POINT('Ctrl Pts',(25.3030891218091,17.41958132242,71.795811473092));
#138157=CARTESIAN_POINT('Ctrl Pts',(24.7620003303291,17.5512068623,71.651135627332));
#138158=CARTESIAN_POINT('Ctrl Pts',(24.0045728644791,17.79520593481,71.435364902963));
#138159=CARTESIAN_POINT('Ctrl Pts',(23.4552604763591,18.04938472156,71.261698407729));
#138160=CARTESIAN_POINT('Ctrl Pts',(23.0945336287391,18.25428407142,71.13914291643));
#138161=CARTESIAN_POINT('Ctrl Pts',(28.1400244369891,17.16084343501,71.67068573287));
#138162=CARTESIAN_POINT('Ctrl Pts',(27.6924228005891,17.08797999477,71.550588326742));
#138163=CARTESIAN_POINT('Ctrl Pts',(27.0368869496491,17.03881028412,71.358054994454));
#138164=CARTESIAN_POINT('Ctrl Pts',(26.1855308687891,17.08595396583,71.075775732564));
#138165=CARTESIAN_POINT('Ctrl Pts',(25.5993319865391,17.1657036723,70.867651396577));
#138166=CARTESIAN_POINT('Ctrl Pts',(25.0249494825691,17.29190890746,70.649703725504));
#138167=CARTESIAN_POINT('Ctrl Pts',(24.2242629266291,17.53789465026,70.325403445397));
#138168=CARTESIAN_POINT('Ctrl Pts',(23.6493371619591,17.80529216506,70.065939095621));
#138169=CARTESIAN_POINT('Ctrl Pts',(23.2759003039191,18.02368015424,69.884235493212));
#138170=CARTESIAN_POINT('Ctrl Pts',(28.6742783680191,16.97751618649,71.032681520933));
#138171=CARTESIAN_POINT('Ctrl Pts',(28.1995866711491,16.87164529692,70.881260223481));
#138172=CARTESIAN_POINT('Ctrl Pts',(27.5009153879891,16.7825926448,70.634282550969));
#138173=CARTESIAN_POINT('Ctrl Pts',(26.5927471971891,16.79636360817,70.266373192438));
#138174=CARTESIAN_POINT('Ctrl Pts',(25.9682367963491,16.86108071599,69.993353846621));
#138175=CARTESIAN_POINT('Ctrl Pts',(25.3582383912691,16.98057465604,69.7062492802));
#138176=CARTESIAN_POINT('Ctrl Pts',(24.5122060337491,17.22851317371,69.278160128787));
#138177=CARTESIAN_POINT('Ctrl Pts',(23.9121159264291,17.51120598981,68.935601892025));
#138178=CARTESIAN_POINT('Ctrl Pts',(23.5275237426991,17.74508268167,68.696786815993));
#138179=CARTESIAN_POINT('Ctrl Pts',(29.4637252782291,16.69573371735,70.214944809297));
#138180=CARTESIAN_POINT('Ctrl Pts',(28.9514579649091,16.54179580496,70.032096099575));
#138181=CARTESIAN_POINT('Ctrl Pts',(28.1919676268391,16.39358977803,69.724912954889));
#138182=CARTESIAN_POINT('Ctrl Pts',(27.2035620142491,16.3570658,69.254403728281));
#138183=CARTESIAN_POINT('Ctrl Pts',(26.5252463207491,16.39879570663,68.901220520825));
#138184=CARTESIAN_POINT('Ctrl Pts',(25.8658896109391,16.50762402452,68.526884021015));
#138185=CARTESIAN_POINT('Ctrl Pts',(24.9584926272791,16.75742057013,67.966148168991));
#138186=CARTESIAN_POINT('Ctrl Pts',(24.3270071090491,17.06184500929,67.516248000898));
#138187=CARTESIAN_POINT('Ctrl Pts',(23.9306200607191,17.31759555138,67.204119706507));
#138188=CARTESIAN_POINT('Ctrl Pts',(30.5643228338091,16.27458129194,69.243614535439));
#138189=CARTESIAN_POINT('Ctrl Pts',(30.0032041656191,16.05501205067,69.039943888873));
#138190=CARTESIAN_POINT('Ctrl Pts',(29.1623979624891,15.82351514044,68.679348902864));
#138191=CARTESIAN_POINT('Ctrl Pts',(28.0660514701691,15.71423060732,68.099666962869));
#138192=CARTESIAN_POINT('Ctrl Pts',(27.3158303509791,15.72189536398,67.65602497559));
#138193=CARTESIAN_POINT('Ctrl Pts',(26.5917298473491,15.81393917483,67.179483204152));
#138194=CARTESIAN_POINT('Ctrl Pts',(25.6066793437291,16.06376175979,66.459804783254));
#138195=CARTESIAN_POINT('Ctrl Pts',(24.9407056051391,16.39642789448,65.879059404692));
#138196=CARTESIAN_POINT('Ctrl Pts',(24.5357382278291,16.68036788396,65.478569084817));
#138197=CARTESIAN_POINT('Ctrl Pts',(31.9721783881791,15.65771573836,68.134435860703));
#138198=CARTESIAN_POINT('Ctrl Pts',(31.3495795968991,15.35736259841,67.934796110749));
#138199=CARTESIAN_POINT('Ctrl Pts',(30.4027791865191,15.01732558252,67.544277564079));
#138200=CARTESIAN_POINT('Ctrl Pts',(29.1653871408091,14.80802142551,66.859150797452));
#138201=CARTESIAN_POINT('Ctrl Pts',(28.3226115049791,14.76665268063,66.317249241228));
#138202=CARTESIAN_POINT('Ctrl Pts',(27.5181196124491,14.83186560328,65.721961974247));
#138203=CARTESIAN_POINT('Ctrl Pts',(26.4431662662991,15.07435073545,64.810545576925));
#138204=CARTESIAN_POINT('Ctrl Pts',(25.7491319290091,15.43721005654,64.067609764873));
#138205=CARTESIAN_POINT('Ctrl Pts',(25.3476825194191,15.75121540699,63.559397667783));
#138206=CARTESIAN_POINT('Ctrl Pts',(33.9349740065291,14.66621205402,66.73160281835));
#138207=CARTESIAN_POINT('Ctrl Pts',(33.2278434897891,14.26458094051,66.575078838193));
#138208=CARTESIAN_POINT('Ctrl Pts',(32.1291768053591,13.77747533735,66.191659990382));
#138209=CARTESIAN_POINT('Ctrl Pts',(30.6880826567591,13.42159104386,65.400693368417));
#138210=CARTESIAN_POINT('Ctrl Pts',(29.7134712804291,13.30352866128,64.740908745675));
#138211=CARTESIAN_POINT('Ctrl Pts',(28.7987684121191,13.32093273385,63.990845152437));
#138212=CARTESIAN_POINT('Ctrl Pts',(27.6104240691691,13.53598846397,62.81924348911));
#138213=CARTESIAN_POINT('Ctrl Pts',(26.8996906205291,13.92434475631,61.85109790423));
#138214=CARTESIAN_POINT('Ctrl Pts',(26.5224611273491,14.26533563258,61.1967983039));
#138215=CARTESIAN_POINT('Ctrl Pts',(35.3622032127791,13.75469237915,65.830333025965));
#138216=CARTESIAN_POINT('Ctrl Pts',(34.5908441824791,13.30161722205,65.748234026521));
#138217=CARTESIAN_POINT('Ctrl Pts',(33.3708021106091,12.72238358321,65.428350962473));
#138218=CARTESIAN_POINT('Ctrl Pts',(31.7667737502791,12.25520144588,64.605780509743));
#138219=CARTESIAN_POINT('Ctrl Pts',(30.6899215020291,12.0705356095,63.877833376471));
#138220=CARTESIAN_POINT('Ctrl Pts',(29.6962823484591,12.03664559044,63.02007166273));
#138221=CARTESIAN_POINT('Ctrl Pts',(28.4414020511891,12.20135845414,61.65313517891));
#138222=CARTESIAN_POINT('Ctrl Pts',(27.7497515268791,12.5766773768,60.50898741333));
#138223=CARTESIAN_POINT('Ctrl Pts',(27.4156275891691,12.91072398446,59.74451354692));
#138224=CARTESIAN_POINT('Ctrl Pts',(36.2861062865691,13.03336630118,65.305951484901));
#138225=CARTESIAN_POINT('Ctrl Pts',(35.4712170914491,12.56970047636,65.286339892556));
#138226=CARTESIAN_POINT('Ctrl Pts',(34.1668107446491,11.95485361461,65.031531154156));
#138227=CARTESIAN_POINT('Ctrl Pts',(32.4498758951991,11.42267707437,64.209981525113));
#138228=CARTESIAN_POINT('Ctrl Pts',(31.3039856908491,11.18982977636,63.447072574633));
#138229=CARTESIAN_POINT('Ctrl Pts',(30.2605887651091,11.10856325397,62.52302045754));
#138230=CARTESIAN_POINT('Ctrl Pts',(28.9718152012291,11.20940972601,61.02865012207));
#138231=CARTESIAN_POINT('Ctrl Pts',(28.3078068268491,11.54159885331,59.76710225));
#138232=CARTESIAN_POINT('Ctrl Pts',(28.0119699420191,11.84565233006,58.93127622062));
#138233=CARTESIAN_POINT('Ctrl Pts',(35.8057492437391,12.9545337474,65.365954457758));
#138234=CARTESIAN_POINT('Ctrl Pts',(35.0880473119254,12.5659947139585,65.3035861089168));
#138235=CARTESIAN_POINT('Ctrl Pts',(33.9193435259554,12.0333674552047,65.0326040360676));
#138236=CARTESIAN_POINT('Ctrl Pts',(32.3449940438637,11.5497171457426,64.2716514600773));
#138237=CARTESIAN_POINT('Ctrl Pts',(31.20966790579,11.3242173664052,63.5141788914939));
#138238=CARTESIAN_POINT('Ctrl Pts',(30.1739125038161,11.2501013629597,62.6003206815515));
#138239=CARTESIAN_POINT('Ctrl Pts',(28.9865858783025,11.3522173259346,61.2359961916097));
#138240=CARTESIAN_POINT('Ctrl Pts',(28.3556953002107,11.6353649591875,60.1235372995198));
#138241=CARTESIAN_POINT('Ctrl Pts',(28.0568193741291,11.88244542754,59.40530601881));
#138242=CARTESIAN_POINT('Ctrl Pts',(23.3999522633791,18.46444455386,75.10151114459));
#138243=CARTESIAN_POINT('Ctrl Pts',(23.6808182067591,18.30904759158,75.042523107842));
#138244=CARTESIAN_POINT('Ctrl Pts',(24.1204792021491,18.10012856,74.950661190046));
#138245=CARTESIAN_POINT('Ctrl Pts',(24.7331798418691,17.87739478943,74.823594240219));
#138246=CARTESIAN_POINT('Ctrl Pts',(25.2046454214491,17.73925026023,74.726279248655));
#138247=CARTESIAN_POINT('Ctrl Pts',(25.6837459162591,17.63150329689,74.62784130659));
#138248=CARTESIAN_POINT('Ctrl Pts',(26.3276494863891,17.52927130737,74.496133232865));
#138249=CARTESIAN_POINT('Ctrl Pts',(26.8131230416891,17.49914820964,74.397483178755));
#138250=CARTESIAN_POINT('Ctrl Pts',(27.1339043807891,17.4992593337,74.332577004792));
#138251=CARTESIAN_POINT('Ctrl Pts',(45.5703178693691,0.707960234922114,
89.0822394094));
#138252=CARTESIAN_POINT('Ctrl Pts',(44.5186432780591,0.659835674446814,
89.20897170224));
#138253=CARTESIAN_POINT('Ctrl Pts',(42.8940207028191,0.604436397099514,
89.73263017053));
#138254=CARTESIAN_POINT('Ctrl Pts',(41.0311875536291,0.588130384116814,
91.15056935081));
#138255=CARTESIAN_POINT('Ctrl Pts',(39.9406430951691,0.603176446704114,
92.40648659842));
#138256=CARTESIAN_POINT('Ctrl Pts',(39.1329334447691,0.644538603476814,
93.85993788124));
#138257=CARTESIAN_POINT('Ctrl Pts',(38.4383242748091,0.736745229573714,
96.09055788542));
#138258=CARTESIAN_POINT('Ctrl Pts',(38.5013499324291,0.838281509416614,
97.79112213109));
#138259=CARTESIAN_POINT('Ctrl Pts',(38.7409464403291,0.910299463671814,
98.81933316041));
#138260=CARTESIAN_POINT('Ctrl Pts',(45.4721796702991,2.06232273559201,89.00677780565));
#138261=CARTESIAN_POINT('Ctrl Pts',(44.4284729920291,1.94009833564701,89.1407783658));
#138262=CARTESIAN_POINT('Ctrl Pts',(42.8175742166591,1.79034687547301,89.67184802681));
#138263=CARTESIAN_POINT('Ctrl Pts',(40.9686565618091,1.71580235048201,91.08770003869));
#138264=CARTESIAN_POINT('Ctrl Pts',(39.8842055812591,1.72275806456501,92.33729386425));
#138265=CARTESIAN_POINT('Ctrl Pts',(39.0776934503791,1.79009011946901,93.78055230646));
#138266=CARTESIAN_POINT('Ctrl Pts',(38.3772852098791,1.96457065015301,95.99347428737));
#138267=CARTESIAN_POINT('Ctrl Pts',(38.4275709545191,2.17502790110001,97.68027461616));
#138268=CARTESIAN_POINT('Ctrl Pts',(38.6573676897591,2.32868442717401,98.70126826354));
#138269=CARTESIAN_POINT('Ctrl Pts',(44.8750464017491,4.56348845765001,88.64530949828));
#138270=CARTESIAN_POINT('Ctrl Pts',(43.8784111675091,4.31519214834701,88.82035926586));
#138271=CARTESIAN_POINT('Ctrl Pts',(42.3489435586691,4.00766266409601,89.39434894904));
#138272=CARTESIAN_POINT('Ctrl Pts',(40.5839167302391,3.83775650537201,90.80141261252));
#138273=CARTESIAN_POINT('Ctrl Pts',(39.5371780607291,3.83261063261101,92.01797786687));
#138274=CARTESIAN_POINT('Ctrl Pts',(38.7399707710991,3.94455189574301,93.40690693377));
#138275=CARTESIAN_POINT('Ctrl Pts',(38.0091199376791,4.25844260235601,95.52524061768));
#138276=CARTESIAN_POINT('Ctrl Pts',(37.9876278087191,4.65417059800001,97.13918259124));
#138277=CARTESIAN_POINT('Ctrl Pts',(38.1619562805791,4.94855385665801,98.1228027417));
#138278=CARTESIAN_POINT('Ctrl Pts',(43.0040757822791,7.92565778104501,87.57336120223));
#138279=CARTESIAN_POINT('Ctrl Pts',(42.1314449640691,7.58314091906501,87.84274208492));
#138280=CARTESIAN_POINT('Ctrl Pts',(40.8109212819391,7.17442879063501,88.50086965325));
#138281=CARTESIAN_POINT('Ctrl Pts',(39.2628767731891,6.95638763849201,89.85599220205));
#138282=CARTESIAN_POINT('Ctrl Pts',(38.3185027453891,6.95368779388401,90.97257180576));
#138283=CARTESIAN_POINT('Ctrl Pts',(37.5569107613691,7.10414768348401,92.21235388849));
#138284=CARTESIAN_POINT('Ctrl Pts',(36.7719385589291,7.52355677267901,94.07900873911));
#138285=CARTESIAN_POINT('Ctrl Pts',(36.5857472469691,8.06070624920501,95.50005965187));
#138286=CARTESIAN_POINT('Ctrl Pts',(36.6231609183791,8.47348086431201,96.38244933991));
#138287=CARTESIAN_POINT('Ctrl Pts',(40.5611902232291,10.69087199582,86.169912153));
#138288=CARTESIAN_POINT('Ctrl Pts',(39.8202100664191,10.3459022151,86.51638878304));
#138289=CARTESIAN_POINT('Ctrl Pts',(38.7145503345591,9.95494845055102,87.21990143235));
#138290=CARTESIAN_POINT('Ctrl Pts',(37.3925003291091,9.76608299487901,88.47454628703));
#138291=CARTESIAN_POINT('Ctrl Pts',(36.5609603027891,9.78111156877201,89.46176171597));
#138292=CARTESIAN_POINT('Ctrl Pts',(35.8513385718791,9.94505616679701,90.52793264081));
#138293=CARTESIAN_POINT('Ctrl Pts',(35.0423804786691,10.38071351751,92.11239180277));
#138294=CARTESIAN_POINT('Ctrl Pts',(34.7147333582191,10.93606492626,93.31812773795));
#138295=CARTESIAN_POINT('Ctrl Pts',(34.6211328961591,11.37571793371,94.08326873557));
#138296=CARTESIAN_POINT('Ctrl Pts',(37.6648628651591,13.01212937041,84.45051386252));
#138297=CARTESIAN_POINT('Ctrl Pts',(37.0485114028091,12.72504052521,84.83528003923));
#138298=CARTESIAN_POINT('Ctrl Pts',(36.1397513800491,12.42041285003,85.52537905717));
#138299=CARTESIAN_POINT('Ctrl Pts',(35.0291247089391,12.30120930116,86.62813233824));
#138300=CARTESIAN_POINT('Ctrl Pts',(34.3098104197691,12.34107474934,87.46222226458));
#138301=CARTESIAN_POINT('Ctrl Pts',(33.6646869438991,12.5044895076,88.34115329029));
#138302=CARTESIAN_POINT('Ctrl Pts',(32.8688746226891,12.90715384858,89.63210632856));
#138303=CARTESIAN_POINT('Ctrl Pts',(32.4461188939691,13.40839785764,90.61443544277));
#138304=CARTESIAN_POINT('Ctrl Pts',(32.2490596322791,13.81460990432,91.25188364405));
#138305=CARTESIAN_POINT('Ctrl Pts',(34.6138161202091,14.83524066691,82.512754421903));
#138306=CARTESIAN_POINT('Ctrl Pts',(34.1021116145691,14.63448763363,82.887519522589));
#138307=CARTESIAN_POINT('Ctrl Pts',(33.3541271725091,14.44059566195,83.5053711923));
#138308=CARTESIAN_POINT('Ctrl Pts',(32.4209056113491,14.40140301801,84.41848947981));
#138309=CARTESIAN_POINT('Ctrl Pts',(31.8014684235891,14.46612570875,85.08838789903));
#138310=CARTESIAN_POINT('Ctrl Pts',(31.2239907584391,14.6225382638,85.78068774631));
#138311=CARTESIAN_POINT('Ctrl Pts',(30.4702465367691,14.97297661061,86.78797330942));
#138312=CARTESIAN_POINT('Ctrl Pts',(30.0032175967391,15.38999825496,87.55450823221));
#138313=CARTESIAN_POINT('Ctrl Pts',(29.7415966793991,15.73193890552,88.06198850603));
#138314=CARTESIAN_POINT('Ctrl Pts',(32.0109525733291,16.02018950073,80.626324032147));
#138315=CARTESIAN_POINT('Ctrl Pts',(31.5698153999191,15.89672173437,80.952027168743));
#138316=CARTESIAN_POINT('Ctrl Pts',(30.9280379274291,15.7943497689,81.463551765629));
#138317=CARTESIAN_POINT('Ctrl Pts',(30.1155556593891,15.81791239968,82.186276359872));
#138318=CARTESIAN_POINT('Ctrl Pts',(29.5676182319791,15.90095742703,82.706753402063));
#138319=CARTESIAN_POINT('Ctrl Pts',(29.0444936137691,16.05004143134,83.23817878262));
#138320=CARTESIAN_POINT('Ctrl Pts',(28.3388309664491,16.35525555443,84.00675759992));
#138321=CARTESIAN_POINT('Ctrl Pts',(27.8654686878691,16.69852697646,84.59147024585));
#138322=CARTESIAN_POINT('Ctrl Pts',(27.5770904290591,16.97909376117,84.98370283207));
#138323=CARTESIAN_POINT('Ctrl Pts',(30.1132980125691,16.72999540751,78.946185718569));
#138324=CARTESIAN_POINT('Ctrl Pts',(29.7137407941691,16.65934526971,79.210897567761));
#138325=CARTESIAN_POINT('Ctrl Pts',(29.1340526716791,16.61720595081,79.615340806471));
#138326=CARTESIAN_POINT('Ctrl Pts',(28.3933628948891,16.68117614212,80.172130006458));
#138327=CARTESIAN_POINT('Ctrl Pts',(27.8889896965391,16.77573676935,80.56865339757));
#138328=CARTESIAN_POINT('Ctrl Pts',(27.4006391487591,16.91970666313,80.970498491355));
#138329=CARTESIAN_POINT('Ctrl Pts',(26.7293418797291,17.1948500933,81.549382547162));
#138330=CARTESIAN_POINT('Ctrl Pts',(26.2594753174191,17.48867903209,81.989427557792));
#138331=CARTESIAN_POINT('Ctrl Pts',(25.9607500271791,17.72646700966,82.286884785861));
#138332=CARTESIAN_POINT('Ctrl Pts',(28.8360405155491,17.14364644213,77.547996582545));
#138333=CARTESIAN_POINT('Ctrl Pts',(28.4591298614191,17.10612249352,77.7565186051));
#138334=CARTESIAN_POINT('Ctrl Pts',(27.9131147582991,17.10100848932,78.069500245689));
#138335=CARTESIAN_POINT('Ctrl Pts',(27.2114257336291,17.1895306756,78.492997722336));
#138336=CARTESIAN_POINT('Ctrl Pts',(26.7308206771491,17.29099595334,78.792251113258));
#138337=CARTESIAN_POINT('Ctrl Pts',(26.2616100161191,17.43172986728,79.093840232636));
#138338=CARTESIAN_POINT('Ctrl Pts',(25.6095490746191,17.68828983474,79.526837436468));
#138339=CARTESIAN_POINT('Ctrl Pts',(25.1422058870291,17.95143027748,79.855318404731));
#138340=CARTESIAN_POINT('Ctrl Pts',(24.8380947587091,18.16211819104,80.078213338469));
#138341=CARTESIAN_POINT('Ctrl Pts',(27.7757217083991,17.43097964734,75.935707638512));
#138342=CARTESIAN_POINT('Ctrl Pts',(27.4109041085991,17.41739952321,76.076412741866));
#138343=CARTESIAN_POINT('Ctrl Pts',(26.8827892158591,17.43865574786,76.284524941454));
#138344=CARTESIAN_POINT('Ctrl Pts',(26.2010864915091,17.54453132413,76.561822608305));
#138345=CARTESIAN_POINT('Ctrl Pts',(25.7321757229291,17.65084167707,76.756297187885));
#138346=CARTESIAN_POINT('Ctrl Pts',(25.2716674990791,17.78924911077,76.95111769228));
#138347=CARTESIAN_POINT('Ctrl Pts',(24.6267935566291,18.03257374984,77.229569264194));
#138348=CARTESIAN_POINT('Ctrl Pts',(24.1570693932891,18.27376550526,77.439744979685));
#138349=CARTESIAN_POINT('Ctrl Pts',(23.8465745131891,18.46478090637,77.582383835345));
#138350=CARTESIAN_POINT('Ctrl Pts',(27.3559829090791,17.50227562775,74.737748587929));
#138351=CARTESIAN_POINT('Ctrl Pts',(26.9886729618591,17.49501040547,74.829545064085));
#138352=CARTESIAN_POINT('Ctrl Pts',(26.4568742846691,17.5231506785,74.963967484974));
#138353=CARTESIAN_POINT('Ctrl Pts',(25.7693264362491,17.63352646129,75.140665286621));
#138354=CARTESIAN_POINT('Ctrl Pts',(25.2957536935691,17.74108044178,75.26361100159));
#138355=CARTESIAN_POINT('Ctrl Pts',(24.8298434891491,17.87886333591,75.385823935064));
#138356=CARTESIAN_POINT('Ctrl Pts',(24.1759661689291,18.11870473769,75.559169478868));
#138357=CARTESIAN_POINT('Ctrl Pts',(23.6975268624191,18.35411537331,75.688361893926));
#138358=CARTESIAN_POINT('Ctrl Pts',(23.3799146126391,18.53989443776,75.775287078776));
#138359=CARTESIAN_POINT('Ctrl Pts',(27.2374127596391,17.5024417656,74.063277809669));
#138360=CARTESIAN_POINT('Ctrl Pts',(26.8654749426391,17.49516466441,74.128758125854));
#138361=CARTESIAN_POINT('Ctrl Pts',(26.3267139877291,17.52329437382,74.223606886666));
#138362=CARTESIAN_POINT('Ctrl Pts',(25.6296536722291,17.63366412477,74.346321907819));
#138363=CARTESIAN_POINT('Ctrl Pts',(25.1493092353391,17.74121690541,74.430883836857));
#138364=CARTESIAN_POINT('Ctrl Pts',(24.6765124261091,17.87900164837,74.514115976861));
#138365=CARTESIAN_POINT('Ctrl Pts',(24.0126415485491,18.11885073386,74.630983591579));
#138366=CARTESIAN_POINT('Ctrl Pts',(23.5264635813191,18.35427499937,74.7165680779));
#138367=CARTESIAN_POINT('Ctrl Pts',(23.2035020446091,18.54006963518,74.773419590361));
#138368=CARTESIAN_POINT('Ctrl Pts',(38.6333955078091,1.20463046452501,98.36582747163));
#138369=CARTESIAN_POINT('Ctrl Pts',(38.4753072726105,1.12679210517909,97.4433768413534));
#138370=CARTESIAN_POINT('Ctrl Pts',(38.4718338960078,1.01542204172217,95.9047402985046));
#138371=CARTESIAN_POINT('Ctrl Pts',(39.1178057748741,0.912164862004577,
93.839260600352));
#138372=CARTESIAN_POINT('Ctrl Pts',(39.9251685220998,0.864777045730714,
92.3885218066525));
#138373=CARTESIAN_POINT('Ctrl Pts',(41.0140425215617,0.851590513166468,
91.1342818091396));
#138374=CARTESIAN_POINT('Ctrl Pts',(42.7385836460012,0.879209305050257,
89.819425823229));
#138375=CARTESIAN_POINT('Ctrl Pts',(44.1903166991323,0.944541149739843,
89.2952475883841));
#138376=CARTESIAN_POINT('Ctrl Pts',(45.1145255779391,0.998148899213914,
89.12773857891));
#138377=CARTESIAN_POINT('Ctrl Pts',(45.2621172516992,-1.15864950900999,
89.08880321312));
#138378=CARTESIAN_POINT('Ctrl Pts',(40.5154296034891,-0.834138914950386,
89.85429588814));
#138379=CARTESIAN_POINT('Ctrl Pts',(37.7466329253491,-0.935506535982887,
93.79723450388));
#138380=CARTESIAN_POINT('Ctrl Pts',(38.6479058880891,-1.40084793775299,
98.50842201768));
#138381=CARTESIAN_POINT('Ctrl Pts',(45.3589510903891,-0.390141862995886,
89.14750817678));
#138382=CARTESIAN_POINT('Ctrl Pts',(40.5597617275791,-0.273423176279186,
89.8799349496001));
#138383=CARTESIAN_POINT('Ctrl Pts',(37.7778654476491,-0.307631400561986,
93.8550658461399));
#138384=CARTESIAN_POINT('Ctrl Pts',(38.7306673927291,-0.471664968376586,
98.61944068779));
#138385=CARTESIAN_POINT('Ctrl Pts',(45.3590610166491,0.389380164346614,
89.14757463976));
#138386=CARTESIAN_POINT('Ctrl Pts',(40.5598094357291,0.272875683534014,
89.87996448328));
#138387=CARTESIAN_POINT('Ctrl Pts',(37.7779005857991,0.307017177882314,
93.85512864424));
#138388=CARTESIAN_POINT('Ctrl Pts',(38.7307611829491,0.470744074667514,
98.61956668849));
#138389=CARTESIAN_POINT('Ctrl Pts',(45.2620963482791,1.15881536706201,89.0887905755001));
#138390=CARTESIAN_POINT('Ctrl Pts',(40.5154205858591,0.834257573969314,
89.85429029489));
#138391=CARTESIAN_POINT('Ctrl Pts',(37.7466262750891,0.935639663228715,
93.79722263086));
#138392=CARTESIAN_POINT('Ctrl Pts',(38.6478880539091,1.40104845952501,98.50839805774));
#138393=CARTESIAN_POINT('Ctrl Pts',(38.633398543612,-1.20459248515192,98.3658322832796));
#138394=CARTESIAN_POINT('Ctrl Pts',(38.4750595671407,-1.12662990155636,
97.4420569298962));
#138395=CARTESIAN_POINT('Ctrl Pts',(38.4730057154008,-1.05234132108018,
96.4153551870171));
#138396=CARTESIAN_POINT('Ctrl Pts',(38.688099235323,-0.993182043686503,
95.3844390851496));
#138397=CARTESIAN_POINT('Ctrl Pts',(38.7956643429362,-0.963597358655216,
94.8688930962344));
#138398=CARTESIAN_POINT('Ctrl Pts',(38.9575348153517,-0.937796299191181,
94.3522931567739));
#138399=CARTESIAN_POINT('Ctrl Pts',(39.1730608688322,-0.917015017058684,
93.8523939206696));
#138400=CARTESIAN_POINT('Ctrl Pts',(39.388586922313,-0.89623373492617,93.3524946845649));
#138401=CARTESIAN_POINT('Ctrl Pts',(39.6577685563747,-0.880472231343552,
92.8692961516738));
#138402=CARTESIAN_POINT('Ctrl Pts',(39.973796875558,-0.870404943100818,
92.4188366157056));
#138403=CARTESIAN_POINT('Ctrl Pts',(40.2898251947411,-0.860337654858091,
91.9683770797378));
#138404=CARTESIAN_POINT('Ctrl Pts',(40.6527001985936,-0.855964583453665,
91.5506565403542));
#138405=CARTESIAN_POINT('Ctrl Pts',(41.04965023065,-0.857235390346154,91.1775461714496));
#138406=CARTESIAN_POINT('Ctrl Pts',(41.4466002627064,-0.858506197238643,
90.8044358025451));
#138407=CARTESIAN_POINT('Ctrl Pts',(41.8776253226757,-0.86542088368976,
90.4759356036829));
#138408=CARTESIAN_POINT('Ctrl Pts',(42.3262312945887,-0.87728971852162,
90.1987272975449));
#138409=CARTESIAN_POINT('Ctrl Pts',(43.223278104326,-0.901023019208226,
89.6444127270248));
#138410=CARTESIAN_POINT('Ctrl Pts',(44.1906226700922,-0.944565655229909,
89.2951902027352));
#138411=CARTESIAN_POINT('Ctrl Pts',(45.1145147831368,-0.998148588101653,
89.1277405085709));
#138412=CARTESIAN_POINT('Ctrl Pts',(27.2376871946991,-17.50242971854,74.064711156945));
#138413=CARTESIAN_POINT('Ctrl Pts',(26.8658614035591,-17.49515074741,74.130158119919));
#138414=CARTESIAN_POINT('Ctrl Pts',(26.3273110298991,-17.52325375652,74.224981944857));
#138415=CARTESIAN_POINT('Ctrl Pts',(25.6305562435091,-17.63353027567,74.347718111042));
#138416=CARTESIAN_POINT('Ctrl Pts',(25.1504846035391,-17.74097529298,74.432308612216));
#138417=CARTESIAN_POINT('Ctrl Pts',(24.6779517816891,-17.87862088949,74.515594757026));
#138418=CARTESIAN_POINT('Ctrl Pts',(24.0138164969491,-18.11845385552,74.632686329655));
#138419=CARTESIAN_POINT('Ctrl Pts',(23.5273164623691,-18.35399576693,74.718503829381));
#138420=CARTESIAN_POINT('Ctrl Pts',(23.2039932885991,-18.54001387247,74.775558557214));
#138421=CARTESIAN_POINT('Ctrl Pts',(27.4622817506591,-17.50215063165,75.344035218027));
#138422=CARTESIAN_POINT('Ctrl Pts',(27.0993410480891,-17.4949504767,75.459863317511));
#138423=CARTESIAN_POINT('Ctrl Pts',(26.5741073480191,-17.52312828209,75.630219120973));
#138424=CARTESIAN_POINT('Ctrl Pts',(25.8954617502391,-17.63344814792,75.855590909026));
#138425=CARTESIAN_POINT('Ctrl Pts',(25.4282471079291,-17.74090226414,76.012993057361));
#138426=CARTESIAN_POINT('Ctrl Pts',(24.9687583406291,-17.87853649113,76.170072411934));
#138427=CARTESIAN_POINT('Ctrl Pts',(24.3235268820491,-18.11832265721,76.393972063008));
#138428=CARTESIAN_POINT('Ctrl Pts',(23.8516161818191,-18.35378673397,76.562026007774));
#138429=CARTESIAN_POINT('Ctrl Pts',(23.5383556626691,-18.53972438058,76.67570803482));
#138430=CARTESIAN_POINT('Ctrl Pts',(28.3553575821991,-17.3000243591,77.031526632576));
#138431=CARTESIAN_POINT('Ctrl Pts',(27.9871351116891,-17.27423244174,77.21725093699));
#138432=CARTESIAN_POINT('Ctrl Pts',(27.4540754692791,-17.28222627378,77.494120215153));
#138433=CARTESIAN_POINT('Ctrl Pts',(26.7674832235591,-17.37939031724,77.866659505309));
#138434=CARTESIAN_POINT('Ctrl Pts',(26.2961871648991,-17.483225832,78.129325170163));
#138435=CARTESIAN_POINT('Ctrl Pts',(25.8345528030491,-17.62271428892,78.393813226736));
#138436=CARTESIAN_POINT('Ctrl Pts',(25.1896731535291,-17.87276274756,78.774035747848));
#138437=CARTESIAN_POINT('Ctrl Pts',(24.7231787828791,-18.12528329555,79.063320155367));
#138438=CARTESIAN_POINT('Ctrl Pts',(24.4168763580191,-18.32674912521,79.260661805121));
#138439=CARTESIAN_POINT('Ctrl Pts',(30.1193998698591,-16.72712396501,78.954400989807));
#138440=CARTESIAN_POINT('Ctrl Pts',(29.7196308839791,-16.65610278602,79.218655211296));
#138441=CARTESIAN_POINT('Ctrl Pts',(29.1397569070191,-16.61352754412,79.622692280116));
#138442=CARTESIAN_POINT('Ctrl Pts',(28.3990365457491,-16.67711876983,80.179492293071));
#138443=CARTESIAN_POINT('Ctrl Pts',(27.8947871921491,-16.77147652606,80.576206493652));
#138444=CARTESIAN_POINT('Ctrl Pts',(27.4066386321391,-16.91531277421,80.978475817268));
#138445=CARTESIAN_POINT('Ctrl Pts',(26.7351116874891,-17.19062376,81.558839194189));
#138446=CARTESIAN_POINT('Ctrl Pts',(26.2651731610791,-17.48497135719,82.000528837247));
#138447=CARTESIAN_POINT('Ctrl Pts',(25.9663983567091,-17.7233890594,82.299404522218));
#138448=CARTESIAN_POINT('Ctrl Pts',(31.5561577943991,-16.18994150244,80.22094136623));
#138449=CARTESIAN_POINT('Ctrl Pts',(31.1252443032691,-16.07925352154,80.532043662118));
#138450=CARTESIAN_POINT('Ctrl Pts',(30.4987078973991,-15.99141036723,81.017800973616));
#138451=CARTESIAN_POINT('Ctrl Pts',(29.7037869514191,-16.02460055635,81.700406797817));
#138452=CARTESIAN_POINT('Ctrl Pts',(29.1665363909691,-16.11026999969,82.190788103002));
#138453=CARTESIAN_POINT('Ctrl Pts',(28.6519091810491,-16.25790421064,82.690692942473));
#138454=CARTESIAN_POINT('Ctrl Pts',(27.9539338991491,-16.55575169532,83.41372255913));
#138455=CARTESIAN_POINT('Ctrl Pts',(27.4808216495891,-16.88723154289,83.9637329239));
#138456=CARTESIAN_POINT('Ctrl Pts',(27.1894469550491,-17.15778055581,84.3333305677));
#138457=CARTESIAN_POINT('Ctrl Pts',(33.0578858065291,-15.54336585756,81.389299787288));
#138458=CARTESIAN_POINT('Ctrl Pts',(32.5880867582691,-15.38869757245,81.734403671999));
#138459=CARTESIAN_POINT('Ctrl Pts',(31.9034088135191,-15.24938125701,82.2882617717));
#138460=CARTESIAN_POINT('Ctrl Pts',(31.0424761811091,-15.24749815586,83.08721118401));
#138461=CARTESIAN_POINT('Ctrl Pts',(30.4660563986391,-15.32299129414,83.66757894853));
#138462=CARTESIAN_POINT('Ctrl Pts',(29.9214516069391,-15.47480379595,84.26363113591));
#138463=CARTESIAN_POINT('Ctrl Pts',(29.1964456396391,-15.79815807595,85.12912638987));
#138464=CARTESIAN_POINT('Ctrl Pts',(28.7258139100191,-16.17140621328,85.78811940437));
#138465=CARTESIAN_POINT('Ctrl Pts',(28.4483807343891,-16.47717452847,86.22779003313));
#138466=CARTESIAN_POINT('Ctrl Pts',(34.6049178055991,-14.78277420146,82.480029194831));
#138467=CARTESIAN_POINT('Ctrl Pts',(34.0899124633891,-14.58252420113,82.848023844388));
#138468=CARTESIAN_POINT('Ctrl Pts',(33.3369620788591,-14.38812926471,83.45824711867));
#138469=CARTESIAN_POINT('Ctrl Pts',(32.3994019289691,-14.34794908773,84.36615210939));
#138470=CARTESIAN_POINT('Ctrl Pts',(31.7784092493091,-14.41206214076,85.03407623603));
#138471=CARTESIAN_POINT('Ctrl Pts',(31.2011411103491,-14.56803185909,85.72574244534));
#138472=CARTESIAN_POINT('Ctrl Pts',(30.4498066469591,-14.91828463801,86.73422814589));
#138473=CARTESIAN_POINT('Ctrl Pts',(29.9883414176491,-15.33534062518,87.50228846636));
#138474=CARTESIAN_POINT('Ctrl Pts',(29.7317228173191,-15.67683330334,88.01029890114));
#138475=CARTESIAN_POINT('Ctrl Pts',(36.1557734484991,-13.91129254351,83.49443968804));
#138476=CARTESIAN_POINT('Ctrl Pts',(35.5907542250291,-13.66696468785,83.87370698997));
#138477=CARTESIAN_POINT('Ctrl Pts',(34.7611060909791,-13.41714938065,84.52732824685));
#138478=CARTESIAN_POINT('Ctrl Pts',(33.7381310519291,-13.33737915323,85.53560671627));
#138479=CARTESIAN_POINT('Ctrl Pts',(33.0684097051491,-13.38932909829,86.28806646301));
#138480=CARTESIAN_POINT('Ctrl Pts',(32.4570980029091,-13.54895837645,87.07443382171));
#138481=CARTESIAN_POINT('Ctrl Pts',(31.6820799917791,-13.92554710058,88.22604588797));
#138482=CARTESIAN_POINT('Ctrl Pts',(31.2378322667491,-14.38531781278,89.10291972624));
#138483=CARTESIAN_POINT('Ctrl Pts',(31.0092985950491,-14.76017803516,89.67723077357));
#138484=CARTESIAN_POINT('Ctrl Pts',(37.6697908381991,-12.93342159556,84.43736943397));
#138485=CARTESIAN_POINT('Ctrl Pts',(37.0505468967491,-12.64931175638,84.81611293096));
#138486=CARTESIAN_POINT('Ctrl Pts',(36.1365854207591,-12.34691554832,85.49916954727));
#138487=CARTESIAN_POINT('Ctrl Pts',(35.0208060078891,-12.22821099738,86.5981509169));
#138488=CARTESIAN_POINT('Ctrl Pts',(34.2994459610991,-12.26764960418,87.43159373777));
#138489=CARTESIAN_POINT('Ctrl Pts',(33.6542855854991,-12.42996124639,88.31146584508));
#138490=CARTESIAN_POINT('Ctrl Pts',(32.8608868434491,-12.8303717258,89.60620123627));
#138491=CARTESIAN_POINT('Ctrl Pts',(32.4441203154791,-13.32873869874,90.59169511767));
#138492=CARTESIAN_POINT('Ctrl Pts',(32.2519928613791,-13.73206374234,91.23040310054));
#138493=CARTESIAN_POINT('Ctrl Pts',(39.1273312888591,-11.8403276167,85.31977033749));
#138494=CARTESIAN_POINT('Ctrl Pts',(38.4474756767491,-11.52446324037,85.68454099069));
#138495=CARTESIAN_POINT('Ctrl Pts',(37.4387918460291,-11.17680143917,86.38047210049));
#138496=CARTESIAN_POINT('Ctrl Pts',(36.2212968557791,-11.02262212161,87.55888335763));
#138497=CARTESIAN_POINT('Ctrl Pts',(35.4455092049291,-11.04980237437,88.4695866419));
#138498=CARTESIAN_POINT('Ctrl Pts',(34.7681392980591,-11.21304523729,89.44254871937));
#138499=CARTESIAN_POINT('Ctrl Pts',(33.9655380969891,-11.63176263852,90.8826799955));
#138500=CARTESIAN_POINT('Ctrl Pts',(33.5912508076991,-12.16011199612,91.97939523496));
#138501=CARTESIAN_POINT('Ctrl Pts',(33.4470797619991,-12.58335502103,92.68277286242));
#138502=CARTESIAN_POINT('Ctrl Pts',(40.5143347257491,-10.62442344881,86.13753768628));
#138503=CARTESIAN_POINT('Ctrl Pts',(39.7704791065591,-10.28796359687,86.47738091817));
#138504=CARTESIAN_POINT('Ctrl Pts',(38.6600450862691,-9.90660226357599,
87.17143604644));
#138505=CARTESIAN_POINT('Ctrl Pts',(37.3343124845091,-9.72320040582899,
88.41839063577));
#138506=CARTESIAN_POINT('Ctrl Pts',(36.5021983603491,-9.73897061260399,
89.40229438399));
#138507=CARTESIAN_POINT('Ctrl Pts',(35.7943862373391,-9.90058283852199,
90.46707941507));
#138508=CARTESIAN_POINT('Ctrl Pts',(34.9907319257591,-10.32907754693,92.05293918629));
#138509=CARTESIAN_POINT('Ctrl Pts',(34.6711977041091,-10.87458861386,93.26106621997));
#138510=CARTESIAN_POINT('Ctrl Pts',(34.5833472293291,-11.30624036383,94.02751284757));
#138511=CARTESIAN_POINT('Ctrl Pts',(41.7958013258191,-9.28987808742799,
86.87970286268));
#138512=CARTESIAN_POINT('Ctrl Pts',(40.9877508719891,-8.94697080201899,
87.18647982707));
#138513=CARTESIAN_POINT('Ctrl Pts',(39.7729888752691,-8.54808012355799,
87.86595909715));
#138514=CARTESIAN_POINT('Ctrl Pts',(38.3365366245991,-8.34497648694099,
89.17012596732));
#138515=CARTESIAN_POINT('Ctrl Pts',(37.4480998536291,-8.35094758626199,
90.22184936653));
#138516=CARTESIAN_POINT('Ctrl Pts',(36.7124380878191,-8.50750595763099,
91.37510535399));
#138517=CARTESIAN_POINT('Ctrl Pts',(35.9152797461691,-8.93394304236699,
93.10327895919));
#138518=CARTESIAN_POINT('Ctrl Pts',(35.6596789728091,-9.47940936258599,
94.41963511778));
#138519=CARTESIAN_POINT('Ctrl Pts',(35.6331349407091,-9.90524587332399,
95.24555986742));
#138520=CARTESIAN_POINT('Ctrl Pts',(43.3219632460591,-7.36135345490399,
87.75528993168));
#138521=CARTESIAN_POINT('Ctrl Pts',(42.4290781817991,-7.03416672139499,
88.00906536633));
#138522=CARTESIAN_POINT('Ctrl Pts',(41.0743404925991,-6.64178586828799,
88.65318138295));
#138523=CARTESIAN_POINT('Ctrl Pts',(39.4905266686191,-6.43118382119999,
90.01661339155));
#138524=CARTESIAN_POINT('Ctrl Pts',(38.5292058215891,-6.42772090807399,
91.14933865191));
#138525=CARTESIAN_POINT('Ctrl Pts',(37.7614435355091,-6.57146966826899,
92.4133885279));
#138526=CARTESIAN_POINT('Ctrl Pts',(36.9839460387491,-6.97338480763799,
94.32296649059));
#138527=CARTESIAN_POINT('Ctrl Pts',(36.8244342451791,-7.48783164222599,
95.77749406464));
#138528=CARTESIAN_POINT('Ctrl Pts',(36.8845638606391,-7.88177804932599,
96.67778125325));
#138529=CARTESIAN_POINT('Ctrl Pts',(44.8847825465991,-4.53379995664999,
88.65117139258));
#138530=CARTESIAN_POINT('Ctrl Pts',(43.8875433874391,-4.28701338408699,
88.82538752989));
#138531=CARTESIAN_POINT('Ctrl Pts',(42.3572012561891,-3.98133338461999,
89.39823867593));
#138532=CARTESIAN_POINT('Ctrl Pts',(40.5912760574091,-3.81238616029299,
90.80439331935));
#138533=CARTESIAN_POINT('Ctrl Pts',(39.5441584350891,-3.80718625688099,
92.02046230176));
#138534=CARTESIAN_POINT('Ctrl Pts',(38.7467026882691,-3.91832816602299,
93.40922179908));
#138535=CARTESIAN_POINT('Ctrl Pts',(38.0150490895291,-4.23041625890299,
95.52979012452));
#138536=CARTESIAN_POINT('Ctrl Pts',(37.9944515607391,-4.62428373692299,
97.1464303542));
#138537=CARTESIAN_POINT('Ctrl Pts',(38.1700698731891,-4.91739601039799,
98.13189991486));
#138538=CARTESIAN_POINT('Ctrl Pts',(45.4723589720291,-2.05622846366899,
89.00701499552));
#138539=CARTESIAN_POINT('Ctrl Pts',(44.4289451307191,-1.93443369721799,
89.14097418644));
#138540=CARTESIAN_POINT('Ctrl Pts',(42.8186744917191,-1.78523787771199,
89.67173154877));
#138541=CARTESIAN_POINT('Ctrl Pts',(40.9703371621991,-1.71096995167399,
91.08656561906));
#138542=CARTESIAN_POINT('Ctrl Pts',(39.8861319792491,-1.71788080442199,
92.33509446141));
#138543=CARTESIAN_POINT('Ctrl Pts',(39.0794495206591,-1.78492357597099,
93.77723356639));
#138544=CARTESIAN_POINT('Ctrl Pts',(38.3775544718791,-1.95885807874699,
95.99082783574));
#138545=CARTESIAN_POINT('Ctrl Pts',(38.4274398112191,-2.16887299505599,
97.67915781703));
#138546=CARTESIAN_POINT('Ctrl Pts',(38.6575428468991,-2.32228900990999,
98.70137587772));
#138547=CARTESIAN_POINT('Ctrl Pts',(45.5703559106791,-0.706838991786186,
89.08233472503));
#138548=CARTESIAN_POINT('Ctrl Pts',(44.5190093055891,-0.658776199678386,
89.20902470915));
#138549=CARTESIAN_POINT('Ctrl Pts',(42.8950488879291,-0.603452424076586,
89.73237110619));
#138550=CARTESIAN_POINT('Ctrl Pts',(41.0328038634091,-0.587152567652286,
91.14929043576));
#138551=CARTESIAN_POINT('Ctrl Pts',(39.9424972960391,-0.602152125724686,
92.40413647438));
#138552=CARTESIAN_POINT('Ctrl Pts',(39.1345984995491,-0.643420016667986,
93.85645551823));
#138553=CARTESIAN_POINT('Ctrl Pts',(38.4384727545291,-0.735528951145086,
96.08773389849));
#138554=CARTESIAN_POINT('Ctrl Pts',(38.5010964114291,-0.837059021185586,
97.78980341537));
#138555=CARTESIAN_POINT('Ctrl Pts',(38.7410049107391,-0.909108343223786,
98.81920581999));
#138556=CARTESIAN_POINT('Ctrl Pts',(23.3999522626291,-18.46444455277,75.101511144727));
#138557=CARTESIAN_POINT('Ctrl Pts',(23.6819559758774,-18.3084167846969,
75.0422841334927));
#138558=CARTESIAN_POINT('Ctrl Pts',(24.1224882166048,-18.099220390028,74.9502420759054));
#138559=CARTESIAN_POINT('Ctrl Pts',(24.7357218717077,-17.8765903523576,
74.8230687141201));
#138560=CARTESIAN_POINT('Ctrl Pts',(25.2059849516925,-17.7389322063629,
74.7260037905263));
#138561=CARTESIAN_POINT('Ctrl Pts',(25.6838350115992,-17.6315140604179,
74.6278234280083));
#138562=CARTESIAN_POINT('Ctrl Pts',(26.3272794229534,-17.5293070988979,
74.4962086120361));
#138563=CARTESIAN_POINT('Ctrl Pts',(26.8127282037799,-17.4991473899451,
74.3975630489114));
#138564=CARTESIAN_POINT('Ctrl Pts',(27.1339039101791,-17.49925933285,74.332577093855));
#138565=CARTESIAN_POINT('Ctrl Pts',(36.2847637417591,-13.03008673973,65.304882352288));
#138566=CARTESIAN_POINT('Ctrl Pts',(35.4698014376591,-12.56680377023,65.284703747679));
#138567=CARTESIAN_POINT('Ctrl Pts',(33.7713459763991,-11.76550621918,64.954403657768));
#138568=CARTESIAN_POINT('Ctrl Pts',(31.2509181992091,-11.10983496554,63.528029780689));
#138569=CARTESIAN_POINT('Ctrl Pts',(29.1719527512791,-11.10598381288,61.40902742803));
#138570=CARTESIAN_POINT('Ctrl Pts',(28.3093846275791,-11.53960369611,59.76597835192));
#138571=CARTESIAN_POINT('Ctrl Pts',(28.0133963045591,-11.84319082917,58.93048676556));
#138572=CARTESIAN_POINT('Ctrl Pts',(35.3612714178091,-13.75149761196,65.828779517486));
#138573=CARTESIAN_POINT('Ctrl Pts',(34.5898538310391,-13.29877169444,65.746262964501));
#138574=CARTESIAN_POINT('Ctrl Pts',(33.0012696328491,-12.54391137714,65.330700476229));
#138575=CARTESIAN_POINT('Ctrl Pts',(30.6472653659591,-11.99120018154,63.94211678041));
#138576=CARTESIAN_POINT('Ctrl Pts',(28.6504997586391,-12.08505199754,61.9975050885));
#138577=CARTESIAN_POINT('Ctrl Pts',(27.7514021894691,-12.57465019834,60.50747334694));
#138578=CARTESIAN_POINT('Ctrl Pts',(27.4172271538291,-12.90829735611,59.74325498279));
#138579=CARTESIAN_POINT('Ctrl Pts',(33.9310055689291,-14.66551773857,66.731530388817));
#138580=CARTESIAN_POINT('Ctrl Pts',(33.2239791263591,-14.26430514063,66.574557910788));
#138581=CARTESIAN_POINT('Ctrl Pts',(31.7938275819191,-13.62995645862,66.075552147711));
#138582=CARTESIAN_POINT('Ctrl Pts',(29.6808305514691,-13.23557272568,64.786213365519));
#138583=CARTESIAN_POINT('Ctrl Pts',(27.8237882040291,-13.4193547387,63.112257346372));
#138584=CARTESIAN_POINT('Ctrl Pts',(26.8992667269091,-13.92561452162,61.85204205614));
#138585=CARTESIAN_POINT('Ctrl Pts',(26.5219839729091,-14.26629883929,61.19814887933));
#138586=CARTESIAN_POINT('Ctrl Pts',(31.9653864880491,-15.65866033563,68.137112684262));
#138587=CARTESIAN_POINT('Ctrl Pts',(31.3430676569791,-15.35884927897,67.937246194186));
#138588=CARTESIAN_POINT('Ctrl Pts',(30.1109982698091,-14.91655490052,67.428984529203));
#138589=CARTESIAN_POINT('Ctrl Pts',(28.2990532332591,-14.715846867,66.347539498663));
#138590=CARTESIAN_POINT('Ctrl Pts',(26.6499274220891,-14.96778503067,65.039851765409));
#138591=CARTESIAN_POINT('Ctrl Pts',(25.7469355071991,-15.4403980032,64.07345053952));
#138592=CARTESIAN_POINT('Ctrl Pts',(25.3455324472891,-15.75408920875,63.565837580849));
#138593=CARTESIAN_POINT('Ctrl Pts',(30.7929135889891,-16.17250423569,69.060223736395));
#138594=CARTESIAN_POINT('Ctrl Pts',(30.2218145303891,-15.93993030477,68.857014383728));
#138595=CARTESIAN_POINT('Ctrl Pts',(29.1046827678391,-15.6154113433,68.381023828893));
#138596=CARTESIAN_POINT('Ctrl Pts',(27.4656460240191,-15.52077373642,67.452927434318));
#138597=CARTESIAN_POINT('Ctrl Pts',(25.9460657515691,-15.79931084072,66.37136947448));
#138598=CARTESIAN_POINT('Ctrl Pts',(25.0733613416891,-16.2390237074,65.580737057625));
#138599=CARTESIAN_POINT('Ctrl Pts',(24.6690559172891,-16.52770085378,65.16275338086));
#138600=CARTESIAN_POINT('Ctrl Pts',(29.8953539876391,-16.52906213236,69.832873012479));
#138601=CARTESIAN_POINT('Ctrl Pts',(29.3639102670391,-16.34951665805,69.641956269545));
#138602=CARTESIAN_POINT('Ctrl Pts',(28.3335435871991,-16.11400158648,69.215018188098));
#138603=CARTESIAN_POINT('Ctrl Pts',(26.8248918532791,-16.09500778036,68.425440053671));
#138604=CARTESIAN_POINT('Ctrl Pts',(25.4087624306691,-16.38876032548,67.526783025968));
#138605=CARTESIAN_POINT('Ctrl Pts',(24.5693720645591,-16.79958429557,66.874208922604));
#138606=CARTESIAN_POINT('Ctrl Pts',(24.1698056852491,-17.06622361444,66.52747591034));
#138607=CARTESIAN_POINT('Ctrl Pts',(29.2502102588991,-16.77062600901,70.433798567399));
#138608=CARTESIAN_POINT('Ctrl Pts',(28.7480655049691,-16.62976631616,70.259448042778));
#138609=CARTESIAN_POINT('Ctrl Pts',(27.7806025530991,-16.45760049426,69.880735221407));
#138610=CARTESIAN_POINT('Ctrl Pts',(26.3660736362391,-16.49066456513,69.204010259922));
#138611=CARTESIAN_POINT('Ctrl Pts',(25.0269527850791,-16.79338156446,68.445873273539));
#138612=CARTESIAN_POINT('Ctrl Pts',(24.2161158147491,-17.18210581398,67.897653773474));
#138613=CARTESIAN_POINT('Ctrl Pts',(23.8230728735191,-17.43180749021,67.605233264723));
#138614=CARTESIAN_POINT('Ctrl Pts',(28.6545914816891,-16.98327424387,71.053055016883));
#138615=CARTESIAN_POINT('Ctrl Pts',(28.1808726772791,-16.87866687246,70.902653141502));
#138616=CARTESIAN_POINT('Ctrl Pts',(27.2732594603691,-16.7646019857,70.583475740074));
#138617=CARTESIAN_POINT('Ctrl Pts',(25.9477619708291,-16.84407223426,70.02876229231));
#138618=CARTESIAN_POINT('Ctrl Pts',(24.6834075254991,-17.1536727076,69.415215054408));
#138619=CARTESIAN_POINT('Ctrl Pts',(23.9034829216691,-17.52101768117,68.972833511437));
#138620=CARTESIAN_POINT('Ctrl Pts',(23.5194027135091,-17.75422570749,68.735949323231));
#138621=CARTESIAN_POINT('Ctrl Pts',(27.9475189385191,-17.22587397515,71.899449525734));
#138622=CARTESIAN_POINT('Ctrl Pts',(27.5097123036091,-17.16491155286,71.790690508363));
#138623=CARTESIAN_POINT('Ctrl Pts',(26.6764981741391,-17.11951879115,71.565626599136));
#138624=CARTESIAN_POINT('Ctrl Pts',(25.4614629953291,-17.25252680212,71.185898966309));
#138625=CARTESIAN_POINT('Ctrl Pts',(24.2924439417591,-17.56896510761,70.771196353781));
#138626=CARTESIAN_POINT('Ctrl Pts',(23.5559636381791,-17.90994030748,70.472334572156));
#138627=CARTESIAN_POINT('Ctrl Pts',(23.1867259327591,-18.12267084568,70.311239709512));
#138628=CARTESIAN_POINT('Ctrl Pts',(27.2648539692091,-17.45480313428,73.0469627073486));
#138629=CARTESIAN_POINT('Ctrl Pts',(26.8690285353091,-17.43758746319,73.0138154548454));
#138630=CARTESIAN_POINT('Ctrl Pts',(26.1203911687191,-17.4593694823,72.9441921949709));
#138631=CARTESIAN_POINT('Ctrl Pts',(25.0299860121291,-17.64326059802,72.8224812819406));
#138632=CARTESIAN_POINT('Ctrl Pts',(23.9723631160091,-17.96516190501,72.6844389313152));
#138633=CARTESIAN_POINT('Ctrl Pts',(23.2930064261891,-18.27939241191,72.5801519585368));
#138634=CARTESIAN_POINT('Ctrl Pts',(22.9467037503691,-18.47108761386,72.5222039840777));
#138635=CARTESIAN_POINT('Ctrl Pts',(27.1796563116291,-17.51202862775,73.966572328327));
#138636=CARTESIAN_POINT('Ctrl Pts',(26.8047259968491,-17.50681468964,74.010390650564));
#138637=CARTESIAN_POINT('Ctrl Pts',(26.0973706850791,-17.54661535838,74.091520290779));
#138638=CARTESIAN_POINT('Ctrl Pts',(25.0695200383991,-17.74366607108,74.205156866572));
#138639=CARTESIAN_POINT('Ctrl Pts',(24.0728463316691,-18.06641523507,74.311387761375));
#138640=CARTESIAN_POINT('Ctrl Pts',(23.4314520398391,-18.37286820423,74.376831020544));
#138641=CARTESIAN_POINT('Ctrl Pts',(23.1037448949791,-18.55843326238,74.409426084866));
#138642=CARTESIAN_POINT('Ctrl Pts',(27.3183431738691,-17.49816102492,74.423860311524));
#138643=CARTESIAN_POINT('Ctrl Pts',(26.9491251864291,-17.49012345996,74.509981767913));
#138644=CARTESIAN_POINT('Ctrl Pts',(26.2528371755791,-17.52566114193,74.673916363871));
#138645=CARTESIAN_POINT('Ctrl Pts',(25.2425967226391,-17.71957244634,74.916046457473));
#138646=CARTESIAN_POINT('Ctrl Pts',(24.2650229396191,-18.04208213438,75.154402189595));
#138647=CARTESIAN_POINT('Ctrl Pts',(23.6378329271991,-18.35032103048,75.310373646596));
#138648=CARTESIAN_POINT('Ctrl Pts',(23.3180557494591,-18.5372869207,75.390793748559));
#138649=CARTESIAN_POINT('',(35.8057502945591,-12.95453430026,65.365954576197));
#138650=CARTESIAN_POINT('Origin',(34.5527802604367,-16.4090907755983,58.2598936512312));
#138651=CARTESIAN_POINT('Ctrl Pts',(35.8057502945591,-12.95453430026,65.365954576197));
#138652=CARTESIAN_POINT('Ctrl Pts',(34.9431064727227,-13.6345772355473,
65.8486570716842));
#138653=CARTESIAN_POINT('Ctrl Pts',(34.0393676425824,-14.2331179686743,
66.4149091822397));
#138654=CARTESIAN_POINT('Ctrl Pts',(32.1844391548707,-15.3036240490635,
67.6946158550174));
#138655=CARTESIAN_POINT('Ctrl Pts',(31.2351899347247,-15.7743557463479,
68.4071218684895));
#138656=CARTESIAN_POINT('Ctrl Pts',(29.8938281053855,-16.3687270422503,
69.5547353783046));
#138657=CARTESIAN_POINT('Ctrl Pts',(29.4577386201557,-16.5493254346668,
69.9518867018678));
#138658=CARTESIAN_POINT('Ctrl Pts',(28.6465905917344,-16.8721898444551,
70.7770253045269));
#138659=CARTESIAN_POINT('Ctrl Pts',(28.272150570333,-17.0138051923601,71.2027210720561));
#138660=CARTESIAN_POINT('Ctrl Pts',(27.6399192608511,-17.2504252448796,
72.0812690648473));
#138661=CARTESIAN_POINT('Ctrl Pts',(27.1275711711326,-17.4401614887824,
72.9890886567126));
#138662=CARTESIAN_POINT('Ctrl Pts',(27.0341870140578,-17.5053411484124,
73.896354193606));
#138663=CARTESIAN_POINT('Ctrl Pts',(27.1339039101791,-17.49925933285,74.332577093855));
#138664=CARTESIAN_POINT('Origin',(59.0011724705691,-9.5,68.602980224451));
#138665=CARTESIAN_POINT('',(62.2792373804991,-12.95454545455,60.69796996444));
#138666=CARTESIAN_POINT('',(35.8057502945591,-12.95453430026,65.365954576197));
#138667=CARTESIAN_POINT('',(83.7957739555191,-12.95454545455,56.90402403487));
#138668=CARTESIAN_POINT('Ctrl Pts',(62.2792373804991,-12.95454545455,60.69796996444));
#138669=CARTESIAN_POINT('Ctrl Pts',(63.1166098845742,-13.2847992676022,
60.7108683749086));
#138670=CARTESIAN_POINT('Ctrl Pts',(63.9689235685123,-13.5674612430028,
60.7259621828012));
#138671=CARTESIAN_POINT('Ctrl Pts',(65.2661182929138,-13.9277132722346,
60.7309827347046));
#138672=CARTESIAN_POINT('Ctrl Pts',(65.7016502793716,-14.0372001888285,
60.7297935419239));
#138673=CARTESIAN_POINT('Ctrl Pts',(66.3592990316064,-14.1865988501347,
60.7217316183955));
#138674=CARTESIAN_POINT('Ctrl Pts',(66.5792411470865,-14.2339265143736,
60.7180021287601));
#138675=CARTESIAN_POINT('Ctrl Pts',(66.9102057654576,-14.3013405355391,
60.7106327881737));
#138676=CARTESIAN_POINT('Ctrl Pts',(67.0759510003769,-14.3341531242629,
60.7065047068387));
#138677=CARTESIAN_POINT('Ctrl Pts',(67.2697730572207,-14.3708970404124,
60.700870085725));
#138678=CARTESIAN_POINT('Ctrl Pts',(67.3667963501766,-14.3888880475788,
60.6978430990522));
#138679=CARTESIAN_POINT('Ctrl Pts',(67.4084017239288,-14.3965172099711,
60.6965003542154));
#138680=CARTESIAN_POINT('Ctrl Pts',(67.4361439544228,-14.4015852985429,
60.695595029068));
#138681=CARTESIAN_POINT('Ctrl Pts',(67.4484057161541,-14.4038180465247,
60.6951910547581));
#138682=CARTESIAN_POINT('Ctrl Pts',(68.4551540303067,-14.5863595677202,
60.6616105645986));
#138683=CARTESIAN_POINT('Ctrl Pts',(69.4348882544448,-14.7155633134713,
60.6024403511034));
#138684=CARTESIAN_POINT('Ctrl Pts',(71.3683115020908,-14.8862983920642,
60.4149080274217));
#138685=CARTESIAN_POINT('Ctrl Pts',(72.3204976988778,-14.9279095443246,
60.2868765976002));
#138686=CARTESIAN_POINT('Ctrl Pts',(74.2039596689047,-14.9285030083013,
59.9553280722839));
#138687=CARTESIAN_POINT('Ctrl Pts',(75.1453218737733,-14.8873352533871,
59.7498855938032));
#138688=CARTESIAN_POINT('Ctrl Pts',(76.5575153071471,-14.7597504534288,
59.3862081438027));
#138689=CARTESIAN_POINT('Ctrl Pts',(77.028286125825,-14.7061728352285,59.2558131408953));
#138690=CARTESIAN_POINT('Ctrl Pts',(77.7347308696933,-14.6081459868011,
59.0477656063524));
#138691=CARTESIAN_POINT('Ctrl Pts',(77.9702615694473,-14.5725229325366,
58.976346445346));
#138692=CARTESIAN_POINT('Ctrl Pts',(78.3236696704847,-14.5144985780568,
58.8663303577197));
#138693=CARTESIAN_POINT('Ctrl Pts',(78.5004018391417,-14.4843386444595,
58.810601074487));
#138694=CARTESIAN_POINT('Ctrl Pts',(78.7066481109466,-14.4471035306846,
58.744375483863));
#138695=CARTESIAN_POINT('Ctrl Pts',(78.8097872118071,-14.4279686423323,
58.710967921756));
#138696=CARTESIAN_POINT('Ctrl Pts',(78.8539932439514,-14.4196565580471,
58.6965880207475));
#138697=CARTESIAN_POINT('Ctrl Pts',(78.8834647389532,-14.4140903461361,
58.6869876482371));
#138698=CARTESIAN_POINT('Ctrl Pts',(78.8996931502854,-14.4110104881187,
58.6816931073477));
#138699=CARTESIAN_POINT('Ctrl Pts',(79.7605727753105,-14.2469752542833,
58.4004742082687));
#138700=CARTESIAN_POINT('Ctrl Pts',(80.5901085772675,-14.0487671762514,
58.1075295181658));
#138701=CARTESIAN_POINT('Ctrl Pts',(82.2163488264336,-13.5677992372985,
57.508634771837));
#138702=CARTESIAN_POINT('Ctrl Pts',(83.0130461883228,-13.2849117827013,
57.202644532765));
#138703=CARTESIAN_POINT('Ctrl Pts',(83.7957739555191,-12.95454545455,56.90402403487));
#138704=CARTESIAN_POINT('',(90.6495102260261,-12.9546821942561,55.6952426312692));
#138705=CARTESIAN_POINT('',(57.7481818513162,-12.9545454545498,61.4969173053295));
#138706=CARTESIAN_POINT('Ctrl Pts',(90.6495104561691,-12.95468496338,55.69524393652));
#138707=CARTESIAN_POINT('Ctrl Pts',(90.706441946712,-13.6387734581529,56.018118459155));
#138708=CARTESIAN_POINT('Ctrl Pts',(90.780331398439,-14.2760166331061,56.437166363396));
#138709=CARTESIAN_POINT('Ctrl Pts',(90.9562156145685,-15.4055939966706,
57.4346553206896));
#138710=CARTESIAN_POINT('Ctrl Pts',(91.0581912555219,-15.8978053691709,
58.0129879192721));
#138711=CARTESIAN_POINT('Ctrl Pts',(91.2820561979301,-16.6977190109123,
59.2825890972016));
#138712=CARTESIAN_POINT('Ctrl Pts',(91.4039211591117,-17.0053343075513,
59.9737196359998));
#138713=CARTESIAN_POINT('Ctrl Pts',(91.6577724166921,-17.4112866435593,
61.413381658003));
#138714=CARTESIAN_POINT('Ctrl Pts',(91.7897311124809,-17.5095795447499,
62.1617566103703));
#138715=CARTESIAN_POINT('Ctrl Pts',(91.9214475326691,-17.49925970194,62.90875755409));
#138716=CARTESIAN_POINT('Ctrl Pts',(91.6420024106691,-17.49288371527,63.189055042563));
#138717=CARTESIAN_POINT('Ctrl Pts',(91.4789309706691,-17.53604965052,62.18525541893));
#138718=CARTESIAN_POINT('Ctrl Pts',(91.2383497332691,-17.31061722234,60.70610679257));
#138719=CARTESIAN_POINT('Ctrl Pts',(90.9525691954691,-16.49526955095,58.94317170309));
#138720=CARTESIAN_POINT('Ctrl Pts',(90.7669853930691,-15.69349549193,57.79357798409));
#138721=CARTESIAN_POINT('Ctrl Pts',(90.6082909804691,-14.70024762494,56.8029977009));
#138722=CARTESIAN_POINT('Ctrl Pts',(90.5020501967691,-13.74144627108,56.13084913297));
#138723=CARTESIAN_POINT('Ctrl Pts',(90.4359017985691,-12.91166468527,55.70386232151));
#138724=CARTESIAN_POINT('Ctrl Pts',(90.3919674336691,-12.26996490144,55.41701567738));
#138725=CARTESIAN_POINT('Ctrl Pts',(90.3493777569691,-11.625304524,55.14038529704));
#138726=CARTESIAN_POINT('Ctrl Pts',(90.2953449890691,-10.75812458152,54.79028890356));
#138727=CARTESIAN_POINT('Ctrl Pts',(90.2336264398691,-9.65880570576799,
54.39205929397));
#138728=CARTESIAN_POINT('Ctrl Pts',(90.1482830072691,-7.87135436876299,
53.83794898948));
#138729=CARTESIAN_POINT('Ctrl Pts',(90.0307623522691,-4.60885225935899,
53.06845652345));
#138730=CARTESIAN_POINT('Ctrl Pts',(89.9936931463691,-1.72467127219999,
52.8107295824));
#138731=CARTESIAN_POINT('Ctrl Pts',(89.9978563052691,0.222735690736214,
52.82471929149));
#138732=CARTESIAN_POINT('Ctrl Pts',(92.8080572940691,-17.49304845091,62.97994092861));
#138733=CARTESIAN_POINT('Ctrl Pts',(92.5986172762691,-17.53509776596,62.00204648082));
#138734=CARTESIAN_POINT('Ctrl Pts',(92.2903921564691,-17.31889130207,60.55898006565));
#138735=CARTESIAN_POINT('Ctrl Pts',(91.9177634400691,-16.52369843296,58.82356961024));
#138736=CARTESIAN_POINT('Ctrl Pts',(91.6714076250691,-15.73549484237,57.68441568032));
#138737=CARTESIAN_POINT('Ctrl Pts',(91.4546567603691,-14.75116789232,56.69582182932));
#138738=CARTESIAN_POINT('Ctrl Pts',(91.3031505321691,-13.79449439958,56.02158047907));
#138739=CARTESIAN_POINT('Ctrl Pts',(91.2028409584691,-12.96185490683,55.59044131213));
#138740=CARTESIAN_POINT('Ctrl Pts',(91.1354530153691,-12.32146797839,55.30843405595));
#138741=CARTESIAN_POINT('Ctrl Pts',(91.0705758404691,-11.6762140863,55.03376811453));
#138742=CARTESIAN_POINT('Ctrl Pts',(90.9888550571691,-10.80763428019,54.68635453665));
#138743=CARTESIAN_POINT('Ctrl Pts',(90.8964011661691,-9.70473219682899,
54.29014956107));
#138744=CARTESIAN_POINT('Ctrl Pts',(90.7663353867691,-7.91003779904899,
53.73885583036));
#138745=CARTESIAN_POINT('Ctrl Pts',(90.5830035106691,-4.63059815939199,
52.97296234484));
#138746=CARTESIAN_POINT('Ctrl Pts',(90.5158617110691,-1.73018910792199,
52.71855165387));
#138747=CARTESIAN_POINT('Ctrl Pts',(90.5140275158691,0.223471129680114,
52.733710804));
#138748=CARTESIAN_POINT('Ctrl Pts',(95.0332577554691,-17.49342459549,62.57674230611));
#138749=CARTESIAN_POINT('Ctrl Pts',(94.7353286476691,-17.53141586528,61.64843478555));
#138750=CARTESIAN_POINT('Ctrl Pts',(94.2980272562691,-17.32866592076,60.27452483217));
#138751=CARTESIAN_POINT('Ctrl Pts',(93.7599791478691,-16.56684333187,58.59467001798));
#138752=CARTESIAN_POINT('Ctrl Pts',(93.3979525791691,-15.80201717449,57.4785906808));
#138753=CARTESIAN_POINT('Ctrl Pts',(93.0707154216691,-14.83409351927,56.49734889427));
#138754=CARTESIAN_POINT('Ctrl Pts',(92.8329885552691,-13.88266802702,55.82142820773));
#138755=CARTESIAN_POINT('Ctrl Pts',(92.6675763969691,-13.04676841354,55.38372565059));
#138756=CARTESIAN_POINT('Ctrl Pts',(92.5552464286691,-12.40954656296,55.10962258496));
#138757=CARTESIAN_POINT('Ctrl Pts',(92.4477320239691,-11.76404691488,54.83811150331));
#138758=CARTESIAN_POINT('Ctrl Pts',(92.3130280801691,-10.89384905739,54.49495852328));
#138759=CARTESIAN_POINT('Ctrl Pts',(92.1617766247691,-9.78542268762398,
54.10178266879));
#138760=CARTESIAN_POINT('Ctrl Pts',(91.9461684628691,-7.97909093036199,
53.55434070925));
#138761=CARTESIAN_POINT('Ctrl Pts',(91.6370374276691,-4.67110365588999,
52.79259843176));
#138762=CARTESIAN_POINT('Ctrl Pts',(91.5126238322691,-1.74148283807699,
52.5424907566));
#138763=CARTESIAN_POINT('Ctrl Pts',(91.4993304075691,0.224963289364014,
52.55999381651));
#138764=CARTESIAN_POINT('Ctrl Pts',(98.3120694042691,-17.4936941465,61.94984322819));
#138765=CARTESIAN_POINT('Ctrl Pts',(97.8837093615691,-17.5212766318,61.0958639362));
#138766=CARTESIAN_POINT('Ctrl Pts',(97.2562515863691,-17.32774641508,59.82615794485));
#138767=CARTESIAN_POINT('Ctrl Pts',(96.4754412409691,-16.60157660903,58.23885952741));
#138768=CARTESIAN_POINT('Ctrl Pts',(95.9439265902691,-15.8644449042,57.16729227158));
#138769=CARTESIAN_POINT('Ctrl Pts',(95.4548753321691,-14.91906406746,56.20859012133));
#138770=CARTESIAN_POINT('Ctrl Pts',(95.0906828307691,-13.97865602756,55.53812427992));
#138771=CARTESIAN_POINT('Ctrl Pts',(94.8297011904691,-13.1440013253,55.09570191083));
#138772=CARTESIAN_POINT('Ctrl Pts',(94.6507179597691,-12.51318114468,54.83035115667));
#138773=CARTESIAN_POINT('Ctrl Pts',(94.4801736252691,-11.86966475712,54.56265476203));
#138774=CARTESIAN_POINT('Ctrl Pts',(94.2671175844691,-10.99981417036,54.22446202571));
#138775=CARTESIAN_POINT('Ctrl Pts',(94.0289868932691,-9.88660333602599,
53.83473114943));
#138776=CARTESIAN_POINT('Ctrl Pts',(93.6870297939691,-8.06867605678799,
53.29066962107));
#138777=CARTESIAN_POINT('Ctrl Pts',(93.1923470644691,-4.72817180229899,
52.53047480904));
#138778=CARTESIAN_POINT('Ctrl Pts',(92.9840370488691,-1.75997898553199,
52.28237322324));
#138779=CARTESIAN_POINT('Ctrl Pts',(92.9537597297691,0.227376689111014,
52.30357909855));
#138780=CARTESIAN_POINT('Ctrl Pts',(101.475753876769,-17.49353891402,61.29590415825));
#138781=CARTESIAN_POINT('Ctrl Pts',(100.921566523269,-17.50673774598,60.51582742363));
#138782=CARTESIAN_POINT('Ctrl Pts',(100.110769980169,-17.31202591817,59.35038436406));
#138783=CARTESIAN_POINT('Ctrl Pts',(99.0967857761691,-16.60753119682,57.86441562302));
#138784=CARTESIAN_POINT('Ctrl Pts',(98.4027331908691,-15.89075779816,56.84705199828));
#138785=CARTESIAN_POINT('Ctrl Pts',(97.7585857601691,-14.96553329684,55.92243481635));
#138786=CARTESIAN_POINT('Ctrl Pts',(97.2730114467691,-14.03873742039,55.26579785069));
#138787=CARTESIAN_POINT('Ctrl Pts',(96.9202344708691,-13.21083938854,54.82435903563));
#138788=CARTESIAN_POINT('Ctrl Pts',(96.6766080013691,-12.58779566903,54.56550800276));
#138789=CARTESIAN_POINT('Ctrl Pts',(96.4451267608691,-11.9483583019,54.30142844987));
#138790=CARTESIAN_POINT('Ctrl Pts',(96.1563018818691,-11.08137533143,53.96772273336));
#138791=CARTESIAN_POINT('Ctrl Pts',(95.8342360423691,-9.96667796474999,
53.5814680127));
#138792=CARTESIAN_POINT('Ctrl Pts',(95.3702583734691,-8.14278530794399,
53.04015645856));
#138793=CARTESIAN_POINT('Ctrl Pts',(94.6966275852691,-4.78001234482099,
52.27965897447));
#138794=CARTESIAN_POINT('Ctrl Pts',(94.4079254195691,-1.77918545761499,
52.03051149812));
#138795=CARTESIAN_POINT('Ctrl Pts',(94.3611453799691,0.229858466556014,
52.05546690015));
#138796=CARTESIAN_POINT('Ctrl Pts',(104.620667374569,-17.49157325014,60.55329954308));
#138797=CARTESIAN_POINT('Ctrl Pts',(103.941467294069,-17.49090485743,59.85098416646));
#138798=CARTESIAN_POINT('Ctrl Pts',(102.948693194469,-17.29004011696,58.79633328559));
#138799=CARTESIAN_POINT('Ctrl Pts',(101.704261160469,-16.59820570304,57.42793899511));
#138800=CARTESIAN_POINT('Ctrl Pts',(100.849876330569,-15.89691605225,56.47926166912));
#138801=CARTESIAN_POINT('Ctrl Pts',(100.052867821069,-14.99073822913,55.60442015319));
#138802=CARTESIAN_POINT('Ctrl Pts',(99.4475331754691,-14.08024912469,54.97301510726));
#138803=CARTESIAN_POINT('Ctrl Pts',(99.0041424461691,-13.26410825573,54.54036692231));
#138804=CARTESIAN_POINT('Ctrl Pts',(98.6960975395691,-12.64985632218,54.28771822127));
#138805=CARTESIAN_POINT('Ctrl Pts',(98.4040997745691,-12.01595884731,54.02882577639));
#138806=CARTESIAN_POINT('Ctrl Pts',(98.0400351694691,-11.15329344622,53.70144103815));
#138807=CARTESIAN_POINT('Ctrl Pts',(97.6347501637691,-10.03867108199,53.32138367282));
#138808=CARTESIAN_POINT('Ctrl Pts',(97.0498718249691,-8.21126455271099,
52.78612552645));
#138809=CARTESIAN_POINT('Ctrl Pts',(96.1992866781691,-4.83025156960999,
52.02935312355));
#138810=CARTESIAN_POINT('Ctrl Pts',(95.8317280272691,-1.79882607342499,
51.77865552707));
#138811=CARTESIAN_POINT('Ctrl Pts',(95.7685466593691,0.232387251367314,
51.80735245561));
#138812=CARTESIAN_POINT('Ctrl Pts',(107.205895077569,-17.48792573077,59.79663312451));
#138813=CARTESIAN_POINT('Ctrl Pts',(106.424044375869,-17.47674622014,59.16511196524));
#138814=CARTESIAN_POINT('Ctrl Pts',(105.282107586869,-17.26716418147,58.21289119973));
#138815=CARTESIAN_POINT('Ctrl Pts',(103.849819279169,-16.57860703868,56.96285248062));
#138816=CARTESIAN_POINT('Ctrl Pts',(102.865084831869,-15.8861456528,56.08863860426));
#138817=CARTESIAN_POINT('Ctrl Pts',(101.944004472769,-14.9947548764,55.27363787577));
#138818=CARTESIAN_POINT('Ctrl Pts',(101.241437676969,-14.09987468339,54.67719491956));
#138819=CARTESIAN_POINT('Ctrl Pts',(100.724490474169,-13.29748172548,54.26189382541));
#138820=CARTESIAN_POINT('Ctrl Pts',(100.363674930769,-12.69122630203,54.01677538362));
#138821=CARTESIAN_POINT('Ctrl Pts',(100.022315310469,-12.06297792511,53.76608434928));
#138822=CARTESIAN_POINT('Ctrl Pts',(99.5969390137691,-11.20486683145,53.44885422607));
#138823=CARTESIAN_POINT('Ctrl Pts',(99.1240602916691,-10.09129477713,53.08026985688));
#138824=CARTESIAN_POINT('Ctrl Pts',(98.4411431664691,-8.26255458396299,
52.55881082705));
#138825=CARTESIAN_POINT('Ctrl Pts',(97.4476767384691,-4.86917355379199,
51.81765382124));
#138826=CARTESIAN_POINT('Ctrl Pts',(97.0175172127691,-1.81445742157099,
51.56911198349));
#138827=CARTESIAN_POINT('Ctrl Pts',(96.9414794370691,0.234396340647814,
51.60056027643));
#138828=CARTESIAN_POINT('Ctrl Pts',(109.221122985369,-17.48371428409,59.02301436315));
#138829=CARTESIAN_POINT('Ctrl Pts',(108.359464527669,-17.46369969179,58.45552561474));
#138830=CARTESIAN_POINT('Ctrl Pts',(107.101863410569,-17.2437316127,57.59764899938));
#138831=CARTESIAN_POINT('Ctrl Pts',(105.524816585069,-16.55226120142,56.46376307926));
#138832=CARTESIAN_POINT('Ctrl Pts',(104.439982558469,-15.8637820089,55.66640186783));
#138833=CARTESIAN_POINT('Ctrl Pts',(103.423883984169,-14.98313091293,54.9173947312));
#138834=CARTESIAN_POINT('Ctrl Pts',(102.646954741169,-14.10173774314,54.36322879206));
#138835=CARTESIAN_POINT('Ctrl Pts',(102.073834275069,-13.31262966272,53.97252742131));
#138836=CARTESIAN_POINT('Ctrl Pts',(101.672467124869,-12.71315223001,53.73834234543));
#138837=CARTESIAN_POINT('Ctrl Pts',(101.293368480369,-12.09006135913,53.49997643624));
#138838=CARTESIAN_POINT('Ctrl Pts',(100.821239581369,-11.23624367659,53.19828953843));
#138839=CARTESIAN_POINT('Ctrl Pts',(100.297134086169,-10.12429194288,52.84806009283));
#138840=CARTESIAN_POINT('Ctrl Pts',(99.5401819745691,-8.29592164133099,
52.35088649986));
#138841=CARTESIAN_POINT('Ctrl Pts',(98.4397632280691,-4.89564444717199,
51.64188241625));
#138842=CARTESIAN_POINT('Ctrl Pts',(97.9644657491691,-1.82535986943699,
51.40219236142));
#138843=CARTESIAN_POINT('Ctrl Pts',(97.8800499836691,0.235795394943814,
51.4350616318));
#138844=CARTESIAN_POINT('Ctrl Pts',(110.672701851769,-17.47999766231,58.31037897659));
#138845=CARTESIAN_POINT('Ctrl Pts',(109.753831385769,-17.45278452645,57.79676235383));
#138846=CARTESIAN_POINT('Ctrl Pts',(108.413565659369,-17.22287585739,57.01944774531));
#138847=CARTESIAN_POINT('Ctrl Pts',(106.733762387369,-16.52601355492,55.98868535554));
#138848=CARTESIAN_POINT('Ctrl Pts',(105.578169273769,-15.83872897935,55.26157469267));
#138849=CARTESIAN_POINT('Ctrl Pts',(104.495167177069,-14.96539903947,54.57518563264));
#138850=CARTESIAN_POINT('Ctrl Pts',(103.666047098169,-14.0945150779,54.06328095415));
#138851=CARTESIAN_POINT('Ctrl Pts',(103.053623379069,-13.31645894672,53.69908149772));
#138852=CARTESIAN_POINT('Ctrl Pts',(102.623789120869,-12.72222884999,53.4775456014));
#138853=CARTESIAN_POINT('Ctrl Pts',(102.218370147569,-12.10331314131,53.25326699941));
#138854=CARTESIAN_POINT('Ctrl Pts',(101.713794163769,-11.25304338524,52.96950594007));
#138855=CARTESIAN_POINT('Ctrl Pts',(101.154507689069,-10.14273559401,52.64069966665));
#138856=CARTESIAN_POINT('Ctrl Pts',(100.347069733169,-8.31549541333899,
52.17289680127));
#138857=CARTESIAN_POINT('Ctrl Pts',(99.1749906850691,-4.91197363593599,
51.50467268182));
#138858=CARTESIAN_POINT('Ctrl Pts',(98.6719831015691,-1.83222302500599,
51.27786018261));
#138859=CARTESIAN_POINT('Ctrl Pts',(98.5843312103691,0.236674998269714,
51.31085219334));
#138860=CARTESIAN_POINT('Ctrl Pts',(112.025636097869,-17.47582299445,57.414708358));
#138861=CARTESIAN_POINT('Ctrl Pts',(111.053943881869,-17.44061054217,56.96304883204));
#138862=CARTESIAN_POINT('Ctrl Pts',(109.637726867469,-17.19832466102,56.27986640927));
#138863=CARTESIAN_POINT('Ctrl Pts',(107.864525222969,-16.49257767027,55.37376659663));
#138864=CARTESIAN_POINT('Ctrl Pts',(106.645070431869,-15.8045298653,54.73368567427));
#138865=CARTESIAN_POINT('Ctrl Pts',(105.502119542669,-14.93766113307,54.1273069539));
#138866=CARTESIAN_POINT('Ctrl Pts',(104.626551783569,-14.0776072634,53.6717926103));
#138867=CARTESIAN_POINT('Ctrl Pts',(103.979374836369,-13.31165186547,53.34497834332));
#138868=CARTESIAN_POINT('Ctrl Pts',(103.524307770069,-12.72281268686,53.14263950197));
#138869=CARTESIAN_POINT('Ctrl Pts',(103.095833717869,-12.1083681819,52.93935575519));
#138870=CARTESIAN_POINT('Ctrl Pts',(102.563125775069,-11.2619717921,52.68248156474));
#138871=CARTESIAN_POINT('Ctrl Pts',(101.973995647869,-10.15375628522,52.38598466337));
#138872=CARTESIAN_POINT('Ctrl Pts',(101.124401221169,-8.32857766047699,
51.96347806666));
#138873=CARTESIAN_POINT('Ctrl Pts',(99.8948730883691,-4.92400388437899,
51.35987964448));
#138874=CARTESIAN_POINT('Ctrl Pts',(99.3746000680691,-1.83743471054699,
51.15495885151));
#138875=CARTESIAN_POINT('Ctrl Pts',(99.2892527118691,0.237341712479814,
51.18649555293));
#138876=CARTESIAN_POINT('Ctrl Pts',(113.187878522469,-17.47164537042,56.27521036476));
#138877=CARTESIAN_POINT('Ctrl Pts',(112.171887071169,-17.42782008763,55.896203917));
#138878=CARTESIAN_POINT('Ctrl Pts',(110.692580204369,-17.1709192225,55.32523290978));
#138879=CARTESIAN_POINT('Ctrl Pts',(108.843546518669,-16.45293860262,54.57208052895));
#138880=CARTESIAN_POINT('Ctrl Pts',(107.573079972769,-15.7622252762,54.04093228966));
#138881=CARTESIAN_POINT('Ctrl Pts',(106.383104391469,-14.90097081599,53.53723091173));
#138882=CARTESIAN_POINT('Ctrl Pts',(105.471805752069,-14.05204799653,53.15666631614));
#138883=CARTESIAN_POINT('Ctrl Pts',(104.798395092669,-13.29921052309,52.88163095715));
#138884=CARTESIAN_POINT('Ctrl Pts',(104.324299692669,-12.7158750262,52.70763929966));
#138885=CARTESIAN_POINT('Ctrl Pts',(103.878996809469,-12.10616052631,52.53481596519));
#138886=CARTESIAN_POINT('Ctrl Pts',(103.326404821569,-11.26390566317,52.3171231399));
#138887=CARTESIAN_POINT('Ctrl Pts',(102.717650256469,-10.15814664048,52.06780970547));
#138888=CARTESIAN_POINT('Ctrl Pts',(101.841943206069,-8.33580711274199,
51.71237805453));
#138889=CARTESIAN_POINT('Ctrl Pts',(100.582660234469,-4.93206689688699,
51.20591871564));
#138890=CARTESIAN_POINT('Ctrl Pts',(100.066369699469,-1.84107769572599,
51.03478661238));
#138891=CARTESIAN_POINT('Ctrl Pts',(99.9955853506691,0.237806588570414,
51.06184068411));
#138892=CARTESIAN_POINT('Ctrl Pts',(114.125295566369,-17.4681686409,54.80495076776));
#138893=CARTESIAN_POINT('Ctrl Pts',(113.075609260269,-17.41485113758,54.51458434375));
#138894=CARTESIAN_POINT('Ctrl Pts',(111.549286453269,-17.14048950455,54.08233649879));
#138895=CARTESIAN_POINT('Ctrl Pts',(109.646785590869,-16.40654507693,53.5223372395));
#138896=CARTESIAN_POINT('Ctrl Pts',(108.341891044269,-15.7114208792,53.13068024962));
#138897=CARTESIAN_POINT('Ctrl Pts',(107.121834027869,-14.85569373811,52.76062809666));
#138898=CARTESIAN_POINT('Ctrl Pts',(106.189106230169,-14.01930261972,52.47974204073));
#138899=CARTESIAN_POINT('Ctrl Pts',(105.501006553569,-13.28178778393,52.27521181241));
#138900=CARTESIAN_POINT('Ctrl Pts',(105.016385994269,-12.70458531254,52.14111418883));
#138901=CARTESIAN_POINT('Ctrl Pts',(104.562932235469,-12.10030644958,52.0107829688));
#138902=CARTESIAN_POINT('Ctrl Pts',(104.002143959169,-11.26286251636,51.84785983031));
#138903=CARTESIAN_POINT('Ctrl Pts',(103.388634838669,-10.16016220358,51.66454860331));
#138904=CARTESIAN_POINT('Ctrl Pts',(102.510622200469,-8.34157678397199,
51.40350477807));
#138905=CARTESIAN_POINT('Ctrl Pts',(101.264203967269,-4.93999503540199,
51.03437280106));
#138906=CARTESIAN_POINT('Ctrl Pts',(100.787671277369,-1.84502963773899,
50.91043632241));
#138907=CARTESIAN_POINT('Ctrl Pts',(100.754059746769,0.238308208433314,
50.92792952439));
#138908=CARTESIAN_POINT('Ctrl Pts',(114.538941011169,-17.46718763232,53.67900430315));
#138909=CARTESIAN_POINT('Ctrl Pts',(113.476435304769,-17.40728503982,53.4545371021));
#138910=CARTESIAN_POINT('Ctrl Pts',(111.933157162869,-17.11989097826,53.12631997973));
#138911=CARTESIAN_POINT('Ctrl Pts',(110.014547047469,-16.37339715948,52.71350806941));
#138912=CARTESIAN_POINT('Ctrl Pts',(108.700990537169,-15.67453448001,52.42915265115));
#138913=CARTESIAN_POINT('Ctrl Pts',(107.475303053069,-14.82273438004,52.1628920189));
#138914=CARTESIAN_POINT('Ctrl Pts',(106.540338441969,-13.9958275305,51.96016673408));
#138915=CARTESIAN_POINT('Ctrl Pts',(105.852098050869,-13.2701199685,51.81147738317));
#138916=CARTESIAN_POINT('Ctrl Pts',(105.367562667669,-12.69751801236,51.70901280385));
#138917=CARTESIAN_POINT('Ctrl Pts',(104.915851437869,-12.09743795773,51.61240634049));
#138918=CARTESIAN_POINT('Ctrl Pts',(104.359190902469,-11.26379112788,51.49296213066));
#138919=CARTESIAN_POINT('Ctrl Pts',(103.754568792369,-10.16369897044,51.36207880897));
#138920=CARTESIAN_POINT('Ctrl Pts',(102.894237682569,-8.34833379260699,
51.17605601973));
#138921=CARTESIAN_POINT('Ctrl Pts',(101.690547221869,-4.94875211867199,
50.9158704599));
#138922=CARTESIAN_POINT('Ctrl Pts',(101.268979997669,-1.84978703934099,
50.82795858552));
#138923=CARTESIAN_POINT('Ctrl Pts',(101.278306971269,0.238909531620114,
50.8353458769));
#138924=CARTESIAN_POINT('Ctrl Pts',(114.721732415669,-17.46709263224,53.0511844563));
#138925=CARTESIAN_POINT('Ctrl Pts',(113.654169992369,-17.40357906045,52.86327469701));
#138926=CARTESIAN_POINT('Ctrl Pts',(112.104502884069,-17.10880738315,52.59289088903));
#138927=CARTESIAN_POINT('Ctrl Pts',(110.180954315469,-16.35510969368,52.262432252));
#138928=CARTESIAN_POINT('Ctrl Pts',(108.865472379469,-15.65410379572,52.03831580661));
#138929=CARTESIAN_POINT('Ctrl Pts',(107.639522339869,-14.80461369374,51.83047343371));
#138930=CARTESIAN_POINT('Ctrl Pts',(106.705667287469,-13.98326026859,51.67177167508));
#138931=CARTESIAN_POINT('Ctrl Pts',(106.019208150569,-13.26447423575,51.55455277005));
#138932=CARTESIAN_POINT('Ctrl Pts',(105.536071241069,-12.69456042945,51.46969752251));
#138933=CARTESIAN_POINT('Ctrl Pts',(105.086676320869,-12.0969679499,51.39195280225));
#138934=CARTESIAN_POINT('Ctrl Pts',(104.534087620169,-11.26560740794,51.29681409481));
#138935=CARTESIAN_POINT('Ctrl Pts',(103.936593793969,-10.16715557418,51.19525657912));
#138936=CARTESIAN_POINT('Ctrl Pts',(103.089545611369,-8.35379901046899,
51.05114625581));
#138937=CARTESIAN_POINT('Ctrl Pts',(101.915641479169,-4.95541766429799,
50.85167914844));
#138938=CARTESIAN_POINT('Ctrl Pts',(101.529528153669,-1.85347919288199,
50.78336850669));
#138939=CARTESIAN_POINT('Ctrl Pts',(101.565834799469,0.239375795559914,
50.78456512074));
#138940=CARTESIAN_POINT('',(90.1947786764252,-4.3867443600625,53.116590296774));
#138941=CARTESIAN_POINT('Origin',(94.1058924693563,-2.20522353149594,75.3038953413698));
#138942=CARTESIAN_POINT('Ctrl Pts',(90.7329498186947,1.32709932748619E-14,
52.6942605482205));
#138943=CARTESIAN_POINT('Ctrl Pts',(90.7324767382983,-0.227253860817282,
52.6943439650584));
#138944=CARTESIAN_POINT('Ctrl Pts',(90.7281184789287,-0.4477491549907,52.6977472020605));
#138945=CARTESIAN_POINT('Ctrl Pts',(90.720392835498,-0.661516881487571,
52.7039174767894));
#138946=CARTESIAN_POINT('Ctrl Pts',(90.7127053559675,-0.874228616956188,
52.7100572709829));
#138947=CARTESIAN_POINT('Ctrl Pts',(90.7016821327591,-1.08027904536049,
52.7189370153821));
#138948=CARTESIAN_POINT('Ctrl Pts',(90.6878356425394,-1.27973268978521,
52.7300489221175));
#138949=CARTESIAN_POINT('Ctrl Pts',(90.6742009569423,-1.47613536582651,
52.7409908541391));
#138950=CARTESIAN_POINT('Ctrl Pts',(90.6578277551231,-1.66614171826471,
52.7540973949353));
#138951=CARTESIAN_POINT('Ctrl Pts',(90.6392259463126,-1.84984509104067,
52.7689165193269));
#138952=CARTESIAN_POINT('Ctrl Pts',(90.620895075782,-2.03087279521278,52.7835198008339));
#138953=CARTESIAN_POINT('Ctrl Pts',(90.6003995142314,-2.20578003978867,
52.7997863319174));
#138954=CARTESIAN_POINT('Ctrl Pts',(90.5782581940087,-2.37468392683479,
52.8173127062458));
#138955=CARTESIAN_POINT('Ctrl Pts',(90.5706889802761,-2.43242527235826,
52.8233042583265));
#138956=CARTESIAN_POINT('Ctrl Pts',(90.5629277330407,-2.4894652436943,52.829443286268));
#138957=CARTESIAN_POINT('Ctrl Pts',(90.5549961696083,-2.54580919563397,
52.8357144107448));
#138958=CARTESIAN_POINT('Ctrl Pts',(90.5293422811424,-2.72804835580788,
52.8559977671417));
#138959=CARTESIAN_POINT('Ctrl Pts',(90.5019355821923,-2.90298378034419,
52.8776533385827));
#138960=CARTESIAN_POINT('Ctrl Pts',(90.4732449116748,-3.0706739713582,52.9002213305575));
#138961=CARTESIAN_POINT('Ctrl Pts',(90.4457229651428,-3.23153324678687,
52.9218700078892));
#138962=CARTESIAN_POINT('Ctrl Pts',(90.4170197258856,-3.38572597691061,
52.9443585273677));
#138963=CARTESIAN_POINT('Ctrl Pts',(90.3875915344632,-3.53332619020803,
52.9673069738302));
#138964=CARTESIAN_POINT('Ctrl Pts',(90.3562888335583,-3.69032820450255,
52.9917171846222));
#138965=CARTESIAN_POINT('Ctrl Pts',(90.3241654812914,-3.83987120261895,
53.0166475416299));
#138966=CARTESIAN_POINT('Ctrl Pts',(90.2918223241181,-3.982066449326,53.0416713166677));
#138967=CARTESIAN_POINT('Ctrl Pts',(90.2594791669447,-4.12426169603305,
53.0666950917055));
#138968=CARTESIAN_POINT('Ctrl Pts',(90.2269165313409,-4.2591095417022,53.0918123452299));
#138969=CARTESIAN_POINT('Ctrl Pts',(90.1947851173379,-4.38673887645801,
53.1166268251324));
#138970=CARTESIAN_POINT('Ctrl Pts',(114.384013133501,-17.4511087443003,
53.3319432235761));
#138971=CARTESIAN_POINT('Ctrl Pts',(113.233237036033,-17.3623045655773,
53.108253902328));
#138972=CARTESIAN_POINT('Ctrl Pts',(112.09731983445,-17.1143644848258,52.8874528876658));
#138973=CARTESIAN_POINT('Ctrl Pts',(109.922039526642,-16.3121265262524,
52.4646191965448));
#138974=CARTESIAN_POINT('Ctrl Pts',(108.894477527575,-15.7640445013132,
52.2648804337895));
#138975=CARTESIAN_POINT('Ctrl Pts',(106.479013465885,-14.0118510024043,
51.7953596092692));
#138976=CARTESIAN_POINT('Ctrl Pts',(105.376412094549,-12.7334337065386,
51.5810346680078));
#138977=CARTESIAN_POINT('Ctrl Pts',(104.030863071798,-10.5823199299919,
51.3194853359339));
#138978=CARTESIAN_POINT('Ctrl Pts',(103.183629676098,-8.98529837677913,
51.1547991792561));
#138979=CARTESIAN_POINT('Ctrl Pts',(101.788452456429,-4.71138061603123,
50.8836032601707));
#138980=CARTESIAN_POINT('Ctrl Pts',(101.414232739431,-2.35682621946771,
50.8108621807075));
#138981=CARTESIAN_POINT('Ctrl Pts',(101.414232124315,-1.74205094793933E-11,
50.81086228917));
#138982=CARTESIAN_POINT('Origin',(119.365530515369,-0.00786869443873679,
54.30025863205));
#138983=CARTESIAN_POINT('Origin',(115.383008995769,1.4210854715202E-14,
59.12907384506));
#138984=CARTESIAN_POINT('Origin',(114.333554474769,1.4210854715202E-14,
64.528022373109));
#138985=CARTESIAN_POINT('Origin',(127.392589630769,111.0726804259,69.613246531288));
#138986=CARTESIAN_POINT('',(105.588267882983,12.0114366406,65.3748945993009));
#138987=CARTESIAN_POINT('Ctrl Pts',(113.836120912569,9.49997724965368,66.9781228011004));
#138988=CARTESIAN_POINT('Ctrl Pts',(113.620040676569,9.60407357720701,66.93612084843));
#138989=CARTESIAN_POINT('Ctrl Pts',(113.204036263969,9.79597941773501,66.855257378578));
#138990=CARTESIAN_POINT('Ctrl Pts',(112.634681946869,10.03993468234,66.744585558129));
#138991=CARTESIAN_POINT('Ctrl Pts',(112.112598449869,10.24927512774,66.643102300151));
#138992=CARTESIAN_POINT('Ctrl Pts',(111.632740031669,10.43041782041,66.549826807009));
#138993=CARTESIAN_POINT('Ctrl Pts',(111.191763777969,10.58798094238,66.464109278743));
#138994=CARTESIAN_POINT('Ctrl Pts',(110.785976678169,10.72587566292,66.385231863232));
#138995=CARTESIAN_POINT('Ctrl Pts',(110.412223632669,10.84718057429,66.312581268166));
#138996=CARTESIAN_POINT('Ctrl Pts',(110.067718345869,10.95437259849,66.245615889834));
#138997=CARTESIAN_POINT('Ctrl Pts',(109.749884820369,11.04949448021,66.183835002597));
#138998=CARTESIAN_POINT('Ctrl Pts',(109.456458641569,11.13421861423,66.126798446613));
#138999=CARTESIAN_POINT('Ctrl Pts',(109.185588771969,11.20988394979,66.07414641488));
#139000=CARTESIAN_POINT('Ctrl Pts',(108.935411166069,11.27766781735,66.025516571843));
#139001=CARTESIAN_POINT('Ctrl Pts',(108.703758242769,11.33868509469,65.980487580283));
#139002=CARTESIAN_POINT('Ctrl Pts',(108.488694360169,11.39387414376,65.938683187692));
#139003=CARTESIAN_POINT('Ctrl Pts',(108.289535310269,11.44377147107,65.899970396824));
#139004=CARTESIAN_POINT('Ctrl Pts',(108.106685536769,11.48858911862,65.864427823957));
#139005=CARTESIAN_POINT('Ctrl Pts',(107.939918988669,11.52866255842,65.832011529019));
#139006=CARTESIAN_POINT('Ctrl Pts',(107.786401064769,11.56489565973,65.802170518592));
#139007=CARTESIAN_POINT('Ctrl Pts',(107.641419490569,11.59853026744,65.773988814747));
#139008=CARTESIAN_POINT('Ctrl Pts',(107.500358765169,11.63070709409,65.746569250508));
#139009=CARTESIAN_POINT('Ctrl Pts',(107.359302140969,11.66233303899,65.71915048345));
#139010=CARTESIAN_POINT('Ctrl Pts',(107.215797620369,11.69395150831,65.69125589119));
#139011=CARTESIAN_POINT('Ctrl Pts',(107.070978664869,11.72524102839,65.663105797358));
#139012=CARTESIAN_POINT('Ctrl Pts',(106.931199149369,11.75497438103,65.635935276346));
#139013=CARTESIAN_POINT('Ctrl Pts',(106.798191632069,11.78293756265,65.610081104993));
#139014=CARTESIAN_POINT('Ctrl Pts',(106.662552223669,11.81149846886,65.583715343288));
#139015=CARTESIAN_POINT('Ctrl Pts',(106.522208287369,11.84046944262,65.556435109417));
#139016=CARTESIAN_POINT('Ctrl Pts',(106.395784786269,11.86721276223,65.531860747577));
#139017=CARTESIAN_POINT('Ctrl Pts',(106.283189021069,11.88761641784,65.509974238645));
#139018=CARTESIAN_POINT('Ctrl Pts',(106.148953995269,11.91021050843,65.483881462854));
#139019=CARTESIAN_POINT('Ctrl Pts',(106.010964934269,11.93474309679,65.457058971809));
#139020=CARTESIAN_POINT('Ctrl Pts',(105.873653901269,11.95937571227,65.430368280779));
#139021=CARTESIAN_POINT('Ctrl Pts',(105.728095742226,11.9858864817682,65.4020744876716));
#139022=CARTESIAN_POINT('Ctrl Pts',(105.63481165757,12.0031744376127,65.3839418377354));
#139023=CARTESIAN_POINT('Ctrl Pts',(105.588267881069,12.0114366406,65.374894609145));
#139024=CARTESIAN_POINT('',(98.6413355775134,12.9603923092705,64.0245406081078));
#139025=CARTESIAN_POINT('Ctrl Pts',(105.58826788679,12.0114366406,65.3748945797136));
#139026=CARTESIAN_POINT('Ctrl Pts',(105.487707106476,12.02927489928,65.3553474466039));
#139027=CARTESIAN_POINT('Ctrl Pts',(105.382844695789,12.04788335748,65.33496415708));
#139028=CARTESIAN_POINT('Ctrl Pts',(105.273811991669,12.0668309774183,65.313770240584));
#139029=CARTESIAN_POINT('Ctrl Pts',(105.164779287549,12.0857785973567,65.292576324088));
#139030=CARTESIAN_POINT('Ctrl Pts',(105.051576289995,12.1050653790333,65.27057178062));
#139031=CARTESIAN_POINT('Ctrl Pts',(104.933545944418,12.124934015645,65.2476288910684));
#139032=CARTESIAN_POINT('Ctrl Pts',(104.815515598841,12.1448026522567,65.2246860015167));
#139033=CARTESIAN_POINT('Ctrl Pts',(104.692657905241,12.1652531438033,65.2008047658813));
#139034=CARTESIAN_POINT('Ctrl Pts',(104.564552226669,12.18625012801,65.1759034202142));
#139035=CARTESIAN_POINT('Ctrl Pts',(104.436446548096,12.2072471122166,65.151002074547));
#139036=CARTESIAN_POINT('Ctrl Pts',(104.303092884551,12.2287905890833,65.1250806188479));
#139037=CARTESIAN_POINT('Ctrl Pts',(104.164040162969,12.2509033469583,65.0980513729576));
#139038=CARTESIAN_POINT('Ctrl Pts',(104.024987441387,12.2730161048333,65.0710221270673));
#139039=CARTESIAN_POINT('Ctrl Pts',(103.880235661768,12.2956981437167,65.0428850909858));
#139040=CARTESIAN_POINT('Ctrl Pts',(103.72930921272,12.3189383132283,65.0135478147625));
#139041=CARTESIAN_POINT('Ctrl Pts',(103.578382763673,12.34217848274,64.9842105385393));
#139042=CARTESIAN_POINT('Ctrl Pts',(103.421281645198,12.36597678288,64.9536730221743));
#139043=CARTESIAN_POINT('Ctrl Pts',(103.257490308254,12.390312007255,64.9218350525855));
#139044=CARTESIAN_POINT('Ctrl Pts',(103.09369897131,12.41464723163,64.8899970829968));
#139045=CARTESIAN_POINT('Ctrl Pts',(102.923217415897,12.43951938024,64.8568586601843));
#139046=CARTESIAN_POINT('Ctrl Pts',(102.745520526753,12.4648904812933,64.8223177115716));
#139047=CARTESIAN_POINT('Ctrl Pts',(102.567823637608,12.4902615823466,64.7877767629589));
#139048=CARTESIAN_POINT('Ctrl Pts',(102.382911414733,12.5161316358433,64.751833288546));
#139049=CARTESIAN_POINT('Ctrl Pts',(102.190273102186,12.5424417096733,64.7143880069401));
#139050=CARTESIAN_POINT('Ctrl Pts',(101.997634789639,12.5687517835033,64.6769427253342));
#139051=CARTESIAN_POINT('Ctrl Pts',(101.797270387422,12.5955018776666,64.6379956365352));
#139052=CARTESIAN_POINT('Ctrl Pts',(101.588727810885,12.6226092695767,64.5974588637509));
#139053=CARTESIAN_POINT('Ctrl Pts',(101.380185234348,12.6497166614867,64.5569220909665));
#139054=CARTESIAN_POINT('Ctrl Pts',(101.163464483491,12.6771813511433,64.5147956341968));
#139055=CARTESIAN_POINT('Ctrl Pts',(100.937832557286,12.7049367835767,64.4709370117642));
#139056=CARTESIAN_POINT('Ctrl Pts',(100.712200631081,12.73269221601,64.4270783893316));
#139057=CARTESIAN_POINT('Ctrl Pts',(100.477657529529,12.76073839122,64.3814876012362));
#139058=CARTESIAN_POINT('Ctrl Pts',(100.233364830254,12.7889966418833,64.3340016738643));
#139059=CARTESIAN_POINT('Ctrl Pts',(99.9890721309782,12.8172548925466,64.2865157464924));
#139060=CARTESIAN_POINT('Ctrl Pts',(99.7350298339805,12.8457252186633,64.237134679844));
#139061=CARTESIAN_POINT('Ctrl Pts',(99.4698469210946,12.8743478680941,64.1855880860287));
#139062=CARTESIAN_POINT('Ctrl Pts',(99.2046640082087,12.902970517525,64.1340414922134));
#139063=CARTESIAN_POINT('Ctrl Pts',(98.9283404794346,12.93174549027,64.0803293712313));
#139064=CARTESIAN_POINT('Ctrl Pts',(98.6413355057347,12.96039230927,64.0245409773214));
#139065=CARTESIAN_POINT('',(98.6413368503852,-12.9603921337551,64.0245393914519));
#139066=CARTESIAN_POINT('',(98.6413367350691,-12.96039213374,64.024539984441));
#139067=CARTESIAN_POINT('',(105.588202589909,-12.0114482303,65.3748819076663));
#139068=CARTESIAN_POINT('Ctrl Pts',(98.6413365043404,-12.96039213374,64.0245411714316));
#139069=CARTESIAN_POINT('Ctrl Pts',(98.9288825599428,-12.93169130878,64.0804347415339));
#139070=CARTESIAN_POINT('Ctrl Pts',(99.205691626796,-12.902863377555,64.1342412420289));
#139071=CARTESIAN_POINT('Ctrl Pts',(99.4712969064103,-12.8741913427442,
64.1858699360291));
#139072=CARTESIAN_POINT('Ctrl Pts',(99.7369021860247,-12.8455193079333,
64.2374986300293));
#139073=CARTESIAN_POINT('Ctrl Pts',(99.9913036784002,-12.8170031695366,
64.2869495175347));
#139074=CARTESIAN_POINT('Ctrl Pts',(100.235912932002,-12.7887018706566,
64.3344969771415));
#139075=CARTESIAN_POINT('Ctrl Pts',(100.480522185603,-12.7604005717767,
64.3820444367482));
#139076=CARTESIAN_POINT('Ctrl Pts',(100.715339200429,-12.7323141124133,
64.4276884684562));
#139077=CARTESIAN_POINT('Ctrl Pts',(100.941205307535,-12.70452182889,64.4715926112718));
#139078=CARTESIAN_POINT('Ctrl Pts',(101.167071414641,-12.6767295453667,
64.5154967540875));
#139079=CARTESIAN_POINT('Ctrl Pts',(101.383986614025,-12.6492314376833,
64.5576610080107));
#139080=CARTESIAN_POINT('Ctrl Pts',(101.592689687186,-12.62209420599,64.598228978334));
#139081=CARTESIAN_POINT('Ctrl Pts',(101.801392760346,-12.5949569742967,
64.6387969486573));
#139082=CARTESIAN_POINT('Ctrl Pts',(102.001883707283,-12.5681806185933,
64.6777686353807));
#139083=CARTESIAN_POINT('Ctrl Pts',(102.194610984735,-12.5418491480417,
64.7152312100988));
#139084=CARTESIAN_POINT('Ctrl Pts',(102.387338262187,-12.51551767749,64.7526937848169));
#139085=CARTESIAN_POINT('Ctrl Pts',(102.572301870154,-12.48963109209,64.7886472475296));
#139086=CARTESIAN_POINT('Ctrl Pts',(102.75001504787,-12.4642486645433,64.8231913623356));
#139087=CARTESIAN_POINT('Ctrl Pts',(102.927728225585,-12.4388662369967,
64.8577354771415));
#139088=CARTESIAN_POINT('Ctrl Pts',(103.098190973049,-12.4139879673033,
64.8908702440408));
#139089=CARTESIAN_POINT('Ctrl Pts',(103.26192990282,-12.3896522645967,64.9226980266562));
#139090=CARTESIAN_POINT('Ctrl Pts',(103.425668832591,-12.36531656189,64.9545258092716));
#139091=CARTESIAN_POINT('Ctrl Pts',(103.58268394467,-12.34152342617,64.9850466076032));
#139092=CARTESIAN_POINT('Ctrl Pts',(103.733490737885,-12.3182943905,65.0143606249728));
#139093=CARTESIAN_POINT('Ctrl Pts',(103.884297531101,-12.29506535483,65.0436746423425));
#139094=CARTESIAN_POINT('Ctrl Pts',(104.028896005453,-12.27240041921,65.07178187875));
#139095=CARTESIAN_POINT('Ctrl Pts',(104.167764032385,-12.2503109256767,
65.0987752234581));
#139096=CARTESIAN_POINT('Ctrl Pts',(104.306632059317,-12.2282214321433,
65.1257685681661));
#139097=CARTESIAN_POINT('Ctrl Pts',(104.43976963883,-12.2067073806967,65.1516480211745));
#139098=CARTESIAN_POINT('Ctrl Pts',(104.567626845804,-12.18574629921,65.1765010686145));
#139099=CARTESIAN_POINT('Ctrl Pts',(104.695484052777,-12.1647852177233,
65.2013541160545));
#139100=CARTESIAN_POINT('Ctrl Pts',(104.818060887212,-12.1443771061967,
65.2251807579259));
#139101=CARTESIAN_POINT('Ctrl Pts',(104.935782035903,-12.1245571421584,
65.2480635453915));
#139102=CARTESIAN_POINT('Ctrl Pts',(105.053503184595,-12.10473717812,65.270946332857));
#139103=CARTESIAN_POINT('Ctrl Pts',(105.166368647542,-12.08550536157,65.2928852659166));
#139104=CARTESIAN_POINT('Ctrl Pts',(105.275029300469,-12.0666203373025,
65.3140068626255));
#139105=CARTESIAN_POINT('Ctrl Pts',(105.38367608427,-12.0477377234637,65.3351257634363));
#139106=CARTESIAN_POINT('Ctrl Pts',(105.48811913136,-12.0292018133859,65.355427536528));
#139107=CARTESIAN_POINT('Ctrl Pts',(105.588202593739,-12.0114482303,65.3748818879668));
#139108=CARTESIAN_POINT('Ctrl Pts',(105.588202587969,-12.0114482303,65.374881917649));
#139109=CARTESIAN_POINT('Ctrl Pts',(105.632442653569,-12.00359419922,65.383481347831));
#139110=CARTESIAN_POINT('Ctrl Pts',(105.721776657069,-11.98704471645,65.400846175769));
#139111=CARTESIAN_POINT('Ctrl Pts',(105.857335799669,-11.96236204966,65.427196347343));
#139112=CARTESIAN_POINT('Ctrl Pts',(105.999371892069,-11.93673375387,65.454805501442));
#139113=CARTESIAN_POINT('Ctrl Pts',(106.145157650769,-11.91101631839,65.483143524557));
#139114=CARTESIAN_POINT('Ctrl Pts',(106.286567143069,-11.8867305141,65.510630882327));
#139115=CARTESIAN_POINT('Ctrl Pts',(106.385566014869,-11.86929321032,65.529874409723));
#139116=CARTESIAN_POINT('Ctrl Pts',(106.517821024969,-11.84141156517,65.555582307755));
#139117=CARTESIAN_POINT('Ctrl Pts',(106.652849454469,-11.81350628447,65.581829306601));
#139118=CARTESIAN_POINT('Ctrl Pts',(106.786531700769,-11.78539623009,65.607814632638));
#139119=CARTESIAN_POINT('Ctrl Pts',(106.926031207269,-11.7560666564,65.634930725157));
#139120=CARTESIAN_POINT('Ctrl Pts',(107.076045936069,-11.72417565916,65.664090780018));
#139121=CARTESIAN_POINT('Ctrl Pts',(107.238877334269,-11.68894114187,65.69574215549));
#139122=CARTESIAN_POINT('Ctrl Pts',(107.415915338069,-11.64977112412,65.730155029124));
#139123=CARTESIAN_POINT('Ctrl Pts',(107.608289198369,-11.60622911253,65.76754890617));
#139124=CARTESIAN_POINT('Ctrl Pts',(107.816920752269,-11.55785278626,65.808102974495));
#139125=CARTESIAN_POINT('Ctrl Pts',(108.042414036969,-11.50424165311,65.851934647601));
#139126=CARTESIAN_POINT('Ctrl Pts',(108.284998613969,-11.44502211087,65.899088547989));
#139127=CARTESIAN_POINT('Ctrl Pts',(108.546207263869,-11.37939218241,65.949862619481));
#139128=CARTESIAN_POINT('Ctrl Pts',(108.827816386469,-11.30637676569,66.00460216095));
#139129=CARTESIAN_POINT('Ctrl Pts',(109.131558670969,-11.22487329816,66.06364397474));
#139130=CARTESIAN_POINT('Ctrl Pts',(109.459041432369,-11.13368566555,66.127300492802));
#139131=CARTESIAN_POINT('Ctrl Pts',(109.812187865869,-11.03134799395,66.195945548277));
#139132=CARTESIAN_POINT('Ctrl Pts',(110.193003524769,-10.91613450448,66.269968983176));
#139133=CARTESIAN_POINT('Ctrl Pts',(110.603674207869,-10.78597589075,66.349795675867));
#139134=CARTESIAN_POINT('Ctrl Pts',(111.046481677169,-10.63839916197,66.435869158151));
#139135=CARTESIAN_POINT('Ctrl Pts',(111.523670537969,-10.47046824764,66.52862573931));
#139136=CARTESIAN_POINT('Ctrl Pts',(112.038227405869,-10.2783509173,66.628645961495));
#139137=CARTESIAN_POINT('Ctrl Pts',(112.591679391169,-10.05799574284,66.736226666351));
#139138=CARTESIAN_POINT('Ctrl Pts',(113.187817592569,-9.80343559038099,
66.852104772485));
#139139=CARTESIAN_POINT('Ctrl Pts',(113.615465209669,-9.60627779281199,
66.935231463316));
#139140=CARTESIAN_POINT('Ctrl Pts',(113.83612107687,-9.49997725001998,66.9781228330329));
#139141=CARTESIAN_POINT('Origin',(113.570314823169,1.4210854715202E-14,
68.454530393505));
#139142=CARTESIAN_POINT('',(122.781534122803,0.000146553545601451,70.2450189834913));
#139143=CARTESIAN_POINT('Ctrl Pts',(122.781532931853,0.000146553553284748,
70.2450187519928));
#139144=CARTESIAN_POINT('Ctrl Pts',(122.781531239529,-0.0353745236476723,
70.2450184230429));
#139145=CARTESIAN_POINT('Ctrl Pts',(122.78124053361,-0.0707835449077734,
70.2449619152538));
#139146=CARTESIAN_POINT('Ctrl Pts',(122.780675137493,-0.106083713974549,
70.244852012833));
#139147=CARTESIAN_POINT('Ctrl Pts',(122.779055732123,-0.207190321579809,
70.2445372307447));
#139148=CARTESIAN_POINT('Ctrl Pts',(122.775182872892,-0.307404002211838,
70.2437844194156));
#139149=CARTESIAN_POINT('Ctrl Pts',(122.769316063091,-0.406807871668896,
70.242644021423));
#139150=CARTESIAN_POINT('Ctrl Pts',(122.762871839682,-0.515995107010533,
70.2413913850348));
#139151=CARTESIAN_POINT('Ctrl Pts',(122.754021860444,-0.624205283049368,
70.2396711147501));
#139152=CARTESIAN_POINT('Ctrl Pts',(122.743027927957,-0.731526461212833,
70.2375341000902));
#139153=CARTESIAN_POINT('Ctrl Pts',(122.73094004789,-0.849526597371243,
70.2351844425004));
#139154=CARTESIAN_POINT('Ctrl Pts',(122.716260320207,-0.966452014654131,
70.2323309782551));
#139155=CARTESIAN_POINT('Ctrl Pts',(122.699248023636,-1.08240084256692,
70.2290241062858));
#139156=CARTESIAN_POINT('Ctrl Pts',(122.680554797463,-1.20980619642746,
70.2253904930703));
#139157=CARTESIAN_POINT('Ctrl Pts',(122.659045282996,-1.33603243947,70.2212094461342));
#139158=CARTESIAN_POINT('Ctrl Pts',(122.63497587133,-1.4611770396468,70.2165308031054));
#139159=CARTESIAN_POINT('Ctrl Pts',(122.608557608206,-1.59853407279087,
70.2113955873257));
#139160=CARTESIAN_POINT('Ctrl Pts',(122.579055446421,-1.73458805478684,
70.2056609193789));
#139161=CARTESIAN_POINT('Ctrl Pts',(122.546669333643,-1.86950917679617,
70.1993656653502));
#139162=CARTESIAN_POINT('Ctrl Pts',(122.511169293522,-2.01740297551294,
70.1924651221414));
#139163=CARTESIAN_POINT('Ctrl Pts',(122.472204056511,-2.16393559197889,
70.1848910095296));
#139164=CARTESIAN_POINT('Ctrl Pts',(122.429982407261,-2.30908823163419,
70.1766839113411));
#139165=CARTESIAN_POINT('Ctrl Pts',(122.383764360875,-2.46797997442484,
70.1676999883651));
#139166=CARTESIAN_POINT('Ctrl Pts',(122.333644270515,-2.62521813965719,
70.1579575810896));
#139167=CARTESIAN_POINT('Ctrl Pts',(122.279817295125,-2.78082020741005,
70.1474946247605));
#139168=CARTESIAN_POINT('Ctrl Pts',(122.220967597282,-2.95094187232875,
70.1360553452162));
#139169=CARTESIAN_POINT('Ctrl Pts',(122.1576869414,-3.11910785768858,70.1237547703804));
#139170=CARTESIAN_POINT('Ctrl Pts',(122.090160629223,-3.28519814820244,
70.1106289194434));
#139171=CARTESIAN_POINT('Ctrl Pts',(122.016001533456,-3.46760268597425,
70.0962137795481));
#139172=CARTESIAN_POINT('Ctrl Pts',(121.936721757884,-3.64750373124946,
70.0808032753626));
#139173=CARTESIAN_POINT('Ctrl Pts',(121.852816091117,-3.8244629412753,70.0644935845287));
#139174=CARTESIAN_POINT('Ctrl Pts',(121.760024497321,-4.02016280003044,
70.0464566358325));
#139175=CARTESIAN_POINT('Ctrl Pts',(121.661575331438,-4.21226472613055,
70.0273199610365));
#139176=CARTESIAN_POINT('Ctrl Pts',(121.558080406608,-4.40061817325353,
70.0072024851623));
#139177=CARTESIAN_POINT('Ctrl Pts',(121.444803244364,-4.60677460096195,
69.9851835254666));
#139178=CARTESIAN_POINT('Ctrl Pts',(121.325481404919,-4.80844045635922,
69.9619895936845));
#139179=CARTESIAN_POINT('Ctrl Pts',(121.200863122926,-5.00559348100024,
69.9377661326256));
#139180=CARTESIAN_POINT('Ctrl Pts',(121.063713701742,-5.22257146193178,
69.9111068527017));
#139181=CARTESIAN_POINT('Ctrl Pts',(120.920149102657,-5.43408339430728,
69.8832005822919));
#139182=CARTESIAN_POINT('Ctrl Pts',(120.77088450835,-5.64030953171291,69.8541863395183));
#139183=CARTESIAN_POINT('Ctrl Pts',(120.604487294548,-5.87020634573354,
69.8218418362522));
#139184=CARTESIAN_POINT('Ctrl Pts',(120.431006497828,-6.09353431793983,
69.7881204170756));
#139185=CARTESIAN_POINT('Ctrl Pts',(120.251312805852,-6.31035921213186,
69.753191327374));
#139186=CARTESIAN_POINT('Ctrl Pts',(120.049384019086,-6.55401377419899,
69.7139401515053));
#139187=CARTESIAN_POINT('Ctrl Pts',(119.839609656204,-6.78945632053946,
69.673163942518));
#139188=CARTESIAN_POINT('Ctrl Pts',(119.623367581806,-7.01678344073686,
69.6311305314923));
#139189=CARTESIAN_POINT('Ctrl Pts',(119.378320042006,-7.27439265804311,
69.5834978772554));
#139190=CARTESIAN_POINT('Ctrl Pts',(119.124966903649,-7.52158034193558,
69.5342507701456));
#139191=CARTESIAN_POINT('Ctrl Pts',(118.864766581224,-7.75898684155283,
69.4836726986369));
#139192=CARTESIAN_POINT('Ctrl Pts',(118.770447846189,-7.84504315587401,
69.4653389022727));
#139193=CARTESIAN_POINT('Ctrl Pts',(118.67522942243,-7.9298142672405,69.4468302232634));
#139194=CARTESIAN_POINT('Ctrl Pts',(118.579168886261,-8.0133283062913,69.4281578533551));
#139195=CARTESIAN_POINT('Ctrl Pts',(118.579167675758,8.01332909152366,69.4281576180553));
#139196=CARTESIAN_POINT('Ctrl Pts',(118.706407237274,7.90270884529846,69.4528906067866));
#139197=CARTESIAN_POINT('Ctrl Pts',(118.832169568853,7.78988234065932,69.4773364496672));
#139198=CARTESIAN_POINT('Ctrl Pts',(118.956319204754,7.67478356951031,69.501468814699));
#139199=CARTESIAN_POINT('Ctrl Pts',(119.228437971327,7.42250304196803,69.5543636086249));
#139200=CARTESIAN_POINT('Ctrl Pts',(119.492808935974,7.15930596577158,69.6057523749017));
#139201=CARTESIAN_POINT('Ctrl Pts',(119.747642512621,6.88447199855316,69.6552872515001));
#139202=CARTESIAN_POINT('Ctrl Pts',(119.978547509072,6.63544462523624,69.700170860072));
#139203=CARTESIAN_POINT('Ctrl Pts',(120.201622125988,6.37686313990138,69.7435323894544));
#139204=CARTESIAN_POINT('Ctrl Pts',(120.415115575264,6.10870425024106,69.7850315192159));
#139205=CARTESIAN_POINT('Ctrl Pts',(120.608606095043,5.86567008165281,69.822642453955));
#139206=CARTESIAN_POINT('Ctrl Pts',(120.794226723886,5.61476911328383,69.8587236292279));
#139207=CARTESIAN_POINT('Ctrl Pts',(120.970826686337,5.3557943959983,69.8930513558265));
#139208=CARTESIAN_POINT('Ctrl Pts',(121.131776280278,5.11977013523727,69.9243369437748));
#139209=CARTESIAN_POINT('Ctrl Pts',(121.285233194329,4.87703971624811,69.9541660950199));
#139210=CARTESIAN_POINT('Ctrl Pts',(121.429999562862,4.62743401359536,69.9823059669128));
#139211=CARTESIAN_POINT('Ctrl Pts',(121.562804428911,4.39845229469453,70.0081207466524));
#139212=CARTESIAN_POINT('Ctrl Pts',(121.688295552653,4.1636845117424,70.0325138718084));
#139213=CARTESIAN_POINT('Ctrl Pts',(121.805299740365,3.92334839336197,70.0552572954825));
#139214=CARTESIAN_POINT('Ctrl Pts',(121.910633879428,3.70698350411704,70.0757322801725));
#139215=CARTESIAN_POINT('Ctrl Pts',(122.009089634504,3.48610566118503,70.0948702357842));
#139216=CARTESIAN_POINT('Ctrl Pts',(122.099776257765,3.26145942719535,70.1124980176158));
#139217=CARTESIAN_POINT('Ctrl Pts',(122.180315419768,3.06195018556796,70.1281533229478));
#139218=CARTESIAN_POINT('Ctrl Pts',(122.254726843029,2.85946870503029,70.1426175105849));
#139219=CARTESIAN_POINT('Ctrl Pts',(122.322688108602,2.65416502953732,70.1558279083178));
#139220=CARTESIAN_POINT('Ctrl Pts',(122.383730436066,2.4697627220875,70.1676933940108));
#139221=CARTESIAN_POINT('Ctrl Pts',(122.439569095469,2.28308360739369,70.1785473840482));
#139222=CARTESIAN_POINT('Ctrl Pts',(122.489830488269,2.09415146679093,70.1883172578727));
#139223=CARTESIAN_POINT('Ctrl Pts',(122.535556029859,1.92226955163331,70.197205447137));
#139224=CARTESIAN_POINT('Ctrl Pts',(122.576665525928,1.74852291117324,70.2051963635714));
#139225=CARTESIAN_POINT('Ctrl Pts',(122.612786961099,1.57272462037444,70.2122176943462));
#139226=CARTESIAN_POINT('Ctrl Pts',(122.645653698257,1.41276651823369,70.2186063727578));
#139227=CARTESIAN_POINT('Ctrl Pts',(122.674390769341,1.25110983402452,70.2241923213942));
#139228=CARTESIAN_POINT('Ctrl Pts',(122.698498321049,1.08749936217765,70.2288783781316));
#139229=CARTESIAN_POINT('Ctrl Pts',(122.720376484174,0.939019058764628,
70.2331310834647));
#139230=CARTESIAN_POINT('Ctrl Pts',(122.738441782511,0.788929618963829,
70.2366426392626));
#139231=CARTESIAN_POINT('Ctrl Pts',(122.752125116466,0.637035590540334,
70.2393024232196));
#139232=CARTESIAN_POINT('Ctrl Pts',(122.764514347892,0.499506953389438,
70.2417106578718));
#139233=CARTESIAN_POINT('Ctrl Pts',(122.773311270029,0.36049892482727,70.2434206148502));
#139234=CARTESIAN_POINT('Ctrl Pts',(122.777904022792,0.21979855912871,70.2443133600067));
#139235=CARTESIAN_POINT('Ctrl Pts',(122.780278918112,0.147042924934891,
70.2447749951966));
#139236=CARTESIAN_POINT('Ctrl Pts',(122.78152966667,0.0738347930879903,
70.2450181173007));
#139237=CARTESIAN_POINT('Ctrl Pts',(122.781535313754,0.000146553589118155,
70.2450192149898));
#139238=CARTESIAN_POINT('Ctrl Pts',(121.735036999469,-0.251492025179986,
71.3942664706531));
#139239=CARTESIAN_POINT('Ctrl Pts',(121.736666170369,-0.215891144805086,
71.3945831509849));
#139240=CARTESIAN_POINT('Ctrl Pts',(121.741962725169,-0.0671388154477658,
71.395612702069));
#139241=CARTESIAN_POINT('Ctrl Pts',(121.740499271469,0.205652813699514,
71.395328234083));
#139242=CARTESIAN_POINT('Ctrl Pts',(121.717046418369,0.577293639062614,
71.3907694384831));
#139243=CARTESIAN_POINT('Ctrl Pts',(121.668270199469,0.983031965715715,
71.381288254676));
#139244=CARTESIAN_POINT('Ctrl Pts',(121.589935658169,1.42397590041401,71.3660614863309));
#139245=CARTESIAN_POINT('Ctrl Pts',(121.477000594769,1.90145538787401,71.344109024239));
#139246=CARTESIAN_POINT('Ctrl Pts',(121.322206770769,2.41905763331001,71.314020002736));
#139247=CARTESIAN_POINT('Ctrl Pts',(121.115195911069,2.98242360767701,71.273780967021));
#139248=CARTESIAN_POINT('Ctrl Pts',(120.843004798869,3.59315027891601,71.220872110458));
#139249=CARTESIAN_POINT('Ctrl Pts',(120.495342776269,4.24372764292801,71.1532931217909));
#139250=CARTESIAN_POINT('Ctrl Pts',(120.064210631769,4.92582479463801,71.069489104072));
#139251=CARTESIAN_POINT('Ctrl Pts',(119.539917822169,5.63463028088801,70.9675763970829));
#139252=CARTESIAN_POINT('Ctrl Pts',(118.908073927269,6.36718264177401,70.844757772566));
#139253=CARTESIAN_POINT('Ctrl Pts',(118.154101012269,7.11797347893601,70.6981995529159));
#139254=CARTESIAN_POINT('Ctrl Pts',(117.287531488569,7.85964231700502,70.529754660428));
#139255=CARTESIAN_POINT('Ctrl Pts',(116.364458080669,8.54113736259001,70.3503264706501));
#139256=CARTESIAN_POINT('Ctrl Pts',(115.461364070269,9.12444254260202,70.174781901721));
#139257=CARTESIAN_POINT('Ctrl Pts',(114.630345072369,9.60270974752501,70.013247365902));
#139258=CARTESIAN_POINT('Ctrl Pts',(113.875901979669,9.99555594218302,69.866597752494));
#139259=CARTESIAN_POINT('Ctrl Pts',(113.189659887769,10.32266924499,69.733205136871));
#139260=CARTESIAN_POINT('Ctrl Pts',(112.564518764069,10.59800466355,69.6116894056039));
#139261=CARTESIAN_POINT('Ctrl Pts',(111.994010209669,10.83200669423,69.5007932230349));
#139262=CARTESIAN_POINT('Ctrl Pts',(111.472720313369,11.03252162863,69.399464226171));
#139263=CARTESIAN_POINT('Ctrl Pts',(110.995459891769,11.20571011009,69.3066937349319));
#139264=CARTESIAN_POINT('Ctrl Pts',(110.558067988369,11.35623559362,69.221672937274));
#139265=CARTESIAN_POINT('Ctrl Pts',(110.156738142269,11.48782915937,69.14366192843));
#139266=CARTESIAN_POINT('Ctrl Pts',(109.788096674869,11.6034703193,69.072004928438));
#139267=CARTESIAN_POINT('Ctrl Pts',(109.449151069169,11.70555902887,69.006120248052));
#139268=CARTESIAN_POINT('Ctrl Pts',(109.137297799269,11.79604012731,68.945501810536));
#139269=CARTESIAN_POINT('Ctrl Pts',(108.850198007269,11.87652072471,68.889694985726));
#139270=CARTESIAN_POINT('Ctrl Pts',(108.585646974169,11.94836677779,68.838271217513));
#139271=CARTESIAN_POINT('Ctrl Pts',(108.341438482969,12.01277581243,68.790801658613));
#139272=CARTESIAN_POINT('Ctrl Pts',(108.115879319369,12.07068478168,68.7469571798701));
#139273=CARTESIAN_POINT('Ctrl Pts',(107.908033627069,12.12274847362,68.706555868334));
#139274=CARTESIAN_POINT('Ctrl Pts',(107.717523269469,12.16941078817,68.66952422133));
#139275=CARTESIAN_POINT('Ctrl Pts',(107.542993047469,12.21129961914,68.6355988135181));
#139276=CARTESIAN_POINT('Ctrl Pts',(107.381385453769,12.24937353981,68.604185322737));
#139277=CARTESIAN_POINT('Ctrl Pts',(107.228180474569,12.28482690077,68.574405142906));
#139278=CARTESIAN_POINT('Ctrl Pts',(107.078801888769,12.31878946362,68.545368742322));
#139279=CARTESIAN_POINT('Ctrl Pts',(106.929723974469,12.35207976103,68.516390786656));
#139280=CARTESIAN_POINT('Ctrl Pts',(106.779850410769,12.38493913925,68.487258171623));
#139281=CARTESIAN_POINT('Ctrl Pts',(106.631924647569,12.41673973848,68.4585041725629));
#139282=CARTESIAN_POINT('Ctrl Pts',(106.488092805569,12.44721671376,68.430545955138));
#139283=CARTESIAN_POINT('Ctrl Pts',(106.347104704869,12.47683083554,68.403140507774));
#139284=CARTESIAN_POINT('Ctrl Pts',(106.205911688169,12.50644037965,68.375695228581));
#139285=CARTESIAN_POINT('Ctrl Pts',(106.067750102369,12.53503352719,68.3488392027959));
#139286=CARTESIAN_POINT('Ctrl Pts',(105.927289821969,12.56398387632,68.321536353826));
#139287=CARTESIAN_POINT('Ctrl Pts',(105.790462806669,12.58661359322,68.294939743578));
#139288=CARTESIAN_POINT('Ctrl Pts',(105.655382900269,12.6104306869,68.2686827385831));
#139289=CARTESIAN_POINT('Ctrl Pts',(105.514586499069,12.63537735536,68.241314554006));
#139290=CARTESIAN_POINT('Ctrl Pts',(105.372054333269,12.66136914805,68.213608969295));
#139291=CARTESIAN_POINT('Ctrl Pts',(105.224646304969,12.68828209136,68.1849556082059));
#139292=CARTESIAN_POINT('Ctrl Pts',(105.084302374769,12.71309158432,68.1576753755249));
#139293=CARTESIAN_POINT('Ctrl Pts',(104.993587027669,12.72877844949,68.1400420103229));
#139294=CARTESIAN_POINT('Ctrl Pts',(104.951723458469,12.73596373186,68.131904516193));
#139295=CARTESIAN_POINT('Ctrl Pts',(123.952465300269,-0.347324334375986,
70.7269691636091));
#139296=CARTESIAN_POINT('Ctrl Pts',(123.954739795569,-0.297475647665086,
70.727411282907));
#139297=CARTESIAN_POINT('Ctrl Pts',(123.962094199069,-0.0904292661378857,
70.7288408412711));
#139298=CARTESIAN_POINT('Ctrl Pts',(123.959932446069,0.280422996215414,
70.728420636943));
#139299=CARTESIAN_POINT('Ctrl Pts',(123.928784632269,0.770995648308114,
70.722366085071));
#139300=CARTESIAN_POINT('Ctrl Pts',(123.865809617769,1.29342741519301,70.710124921183));
#139301=CARTESIAN_POINT('Ctrl Pts',(123.766849737969,1.84967256667701,70.6908889731791));
#139302=CARTESIAN_POINT('Ctrl Pts',(123.626378368069,2.44310614183101,70.663583968595));
#139303=CARTESIAN_POINT('Ctrl Pts',(123.435749754269,3.08026159298101,70.626529334816));
#139304=CARTESIAN_POINT('Ctrl Pts',(123.182646046169,3.76887936681402,70.57733071228));
#139305=CARTESIAN_POINT('Ctrl Pts',(122.851462108169,4.51172925891301,70.512954754774));
#139306=CARTESIAN_POINT('Ctrl Pts',(122.433221569769,5.29389921289301,70.431656623918));
#139307=CARTESIAN_POINT('Ctrl Pts',(121.921579819569,6.10294846988001,70.3322030460629));
#139308=CARTESIAN_POINT('Ctrl Pts',(121.306988090869,6.93348816094802,70.212737919675));
#139309=CARTESIAN_POINT('Ctrl Pts',(120.573879538169,7.78307150435002,70.07023534144));
#139310=CARTESIAN_POINT('Ctrl Pts',(119.710740143769,8.64212008370501,69.902457201885));
#139311=CARTESIAN_POINT('Ctrl Pts',(118.731411294669,9.47989893856901,69.712094007483));
#139312=CARTESIAN_POINT('Ctrl Pts',(117.700739548969,10.24052756398,69.511750715177));
#139313=CARTESIAN_POINT('Ctrl Pts',(116.702090736569,10.88538371112,69.3176320816061));
#139314=CARTESIAN_POINT('Ctrl Pts',(115.790015237369,11.41020795647,69.1403416793871));
#139315=CARTESIAN_POINT('Ctrl Pts',(114.966933189469,11.83874087279,68.980349938073));
#139316=CARTESIAN_POINT('Ctrl Pts',(114.221954815069,12.19381986534,68.835540088713));
#139317=CARTESIAN_POINT('Ctrl Pts',(113.546053101469,12.49149008357,68.704157449044));
#139318=CARTESIAN_POINT('Ctrl Pts',(112.931611172969,12.74349632572,68.584721441012));
#139319=CARTESIAN_POINT('Ctrl Pts',(112.372113240569,12.95869744806,68.475965517244));
#139320=CARTESIAN_POINT('Ctrl Pts',(111.861422559869,13.1440098487,68.3766968094789));
#139321=CARTESIAN_POINT('Ctrl Pts',(111.394646774969,13.30464238705,68.2859643353231));
#139322=CARTESIAN_POINT('Ctrl Pts',(110.967390651869,13.44473346675,68.2029137436041));
#139323=CARTESIAN_POINT('Ctrl Pts',(110.575721925769,13.56759573733,68.126780675622));
#139324=CARTESIAN_POINT('Ctrl Pts',(110.216251000269,13.67586476001,68.05690625729));
#139325=CARTESIAN_POINT('Ctrl Pts',(109.886051079069,13.77166764477,67.992721574233));
#139326=CARTESIAN_POINT('Ctrl Pts',(109.582506400769,13.85675710051,67.933718171385));
#139327=CARTESIAN_POINT('Ctrl Pts',(109.303181896269,13.93261462941,67.879422716907));
#139328=CARTESIAN_POINT('Ctrl Pts',(109.045629558069,14.00054238633,67.829359363966));
#139329=CARTESIAN_POINT('Ctrl Pts',(108.808137096369,14.06151437864,67.7831952754649));
#139330=CARTESIAN_POINT('Ctrl Pts',(108.589621961869,14.1162502982,67.740720024114));
#139331=CARTESIAN_POINT('Ctrl Pts',(108.389578174769,14.16524723555,67.701835256892));
#139332=CARTESIAN_POINT('Ctrl Pts',(108.206580960669,14.2091681233,67.666264024338));
#139333=CARTESIAN_POINT('Ctrl Pts',(108.037100660769,14.24909690253,67.6333202268571));
#139334=CARTESIAN_POINT('Ctrl Pts',(107.876321113269,14.2863032376,67.6020676927461));
#139335=CARTESIAN_POINT('Ctrl Pts',(107.719480082869,14.32196243997,67.571580732629));
#139336=CARTESIAN_POINT('Ctrl Pts',(107.562912614569,14.35692548367,67.5411469478801));
#139337=CARTESIAN_POINT('Ctrl Pts',(107.405377034369,14.39146426087,67.510524980273));
#139338=CARTESIAN_POINT('Ctrl Pts',(107.250163184169,14.42483253046,67.480354313537));
#139339=CARTESIAN_POINT('Ctrl Pts',(107.101721753269,14.45627778599,67.451500078315));
#139340=CARTESIAN_POINT('Ctrl Pts',(106.959668596669,14.48613647781,67.42388760403));
#139341=CARTESIAN_POINT('Ctrl Pts',(106.812895930169,14.51683767398,67.395357745367));
#139342=CARTESIAN_POINT('Ctrl Pts',(106.685780281469,14.54339449682,67.370648842976));
#139343=CARTESIAN_POINT('Ctrl Pts',(106.475408024369,14.58594290389,67.329756414555));
#139344=CARTESIAN_POINT('Ctrl Pts',(106.330012623469,14.60975916719,67.3014942705451));
#139345=CARTESIAN_POINT('Ctrl Pts',(106.205346414169,14.63184978471,67.277261493309));
#139346=CARTESIAN_POINT('Ctrl Pts',(106.069531214769,14.65588498744,67.250861561116));
#139347=CARTESIAN_POINT('Ctrl Pts',(105.936535264969,14.68014815303,67.2250096382841));
#139348=CARTESIAN_POINT('Ctrl Pts',(105.780150023969,14.70869883296,67.1946112750921));
#139349=CARTESIAN_POINT('Ctrl Pts',(105.630239251269,14.73519937094,67.1654714273339));
#139350=CARTESIAN_POINT('Ctrl Pts',(105.535552987169,14.75157065244,67.1470661902031));
#139351=CARTESIAN_POINT('Ctrl Pts',(105.492059043269,14.75903578704,67.138611781753));
#139352=CARTESIAN_POINT('Ctrl Pts',(123.605514838569,-0.310954453434086,
68.4357418369039));
#139353=CARTESIAN_POINT('Ctrl Pts',(123.607544422969,-0.266513035153486,
68.436136350125));
#139354=CARTESIAN_POINT('Ctrl Pts',(123.614117840269,-0.0815901707869558,
68.4374140993829));
#139355=CARTESIAN_POINT('Ctrl Pts',(123.612221102869,0.252046526328314,
68.43704540915));
#139356=CARTESIAN_POINT('Ctrl Pts',(123.583993648769,0.697482664288614,
68.431558520501));
#139357=CARTESIAN_POINT('Ctrl Pts',(123.526407302269,1.17562742021101,68.420364812818));
#139358=CARTESIAN_POINT('Ctrl Pts',(123.435275065569,1.68811393160701,68.402650412068));
#139359=CARTESIAN_POINT('Ctrl Pts',(123.305254160569,2.23754109181001,68.377376782234));
#139360=CARTESIAN_POINT('Ctrl Pts',(123.128225417769,2.82932420565001,68.342965708767));
#139361=CARTESIAN_POINT('Ctrl Pts',(122.892614676469,3.47040693548102,68.297167391501));
#139362=CARTESIAN_POINT('Ctrl Pts',(122.583819451269,4.16311397020101,68.237143380635));
#139363=CARTESIAN_POINT('Ctrl Pts',(122.192364578769,4.89534244964002,68.161051881783));
#139364=CARTESIAN_POINT('Ctrl Pts',(121.711277500669,5.65621136960901,68.067537560153));
#139365=CARTESIAN_POINT('Ctrl Pts',(121.130955643569,6.44055099962301,67.954733855254));
#139366=CARTESIAN_POINT('Ctrl Pts',(120.436278634169,7.24571922941301,67.8197016495811));
#139367=CARTESIAN_POINT('Ctrl Pts',(119.614569649869,8.06368227897601,67.659976806111));
#139368=CARTESIAN_POINT('Ctrl Pts',(118.678034752669,8.86498585846002,67.477931954842));
#139369=CARTESIAN_POINT('Ctrl Pts',(117.688198282369,9.59558203551501,67.2855262755941));
#139370=CARTESIAN_POINT('Ctrl Pts',(116.725814032569,10.21707861463,67.098456794081));
#139371=CARTESIAN_POINT('Ctrl Pts',(115.844500760869,10.72423372488,66.9271459930001));
#139372=CARTESIAN_POINT('Ctrl Pts',(115.047468284869,11.13922296445,66.7722178007911));
#139373=CARTESIAN_POINT('Ctrl Pts',(114.324781261069,11.4836885343,66.631740972675));
#139374=CARTESIAN_POINT('Ctrl Pts',(113.668143996269,11.77288234189,66.5041029812041));
#139375=CARTESIAN_POINT('Ctrl Pts',(113.070375479869,12.0180557003,66.3879079723501));
#139376=CARTESIAN_POINT('Ctrl Pts',(112.525378103069,12.22768318143,66.28197068511));
#139377=CARTESIAN_POINT('Ctrl Pts',(112.027374735769,12.4083943625,66.1851681535581));
#139378=CARTESIAN_POINT('Ctrl Pts',(111.571750599769,12.56519111328,66.096603351202));
#139379=CARTESIAN_POINT('Ctrl Pts',(111.154333909969,12.70205725169,66.015465361097));
#139380=CARTESIAN_POINT('Ctrl Pts',(110.771404393669,12.82217899627,65.941031031893));
#139381=CARTESIAN_POINT('Ctrl Pts',(110.419723152469,12.92810249213,65.872670782376));
#139382=CARTESIAN_POINT('Ctrl Pts',(110.096486076369,13.02188567459,65.8098395460521));
#139383=CARTESIAN_POINT('Ctrl Pts',(109.799182493169,13.10522599551,65.752049295257));
#139384=CARTESIAN_POINT('Ctrl Pts',(109.525464755369,13.17956110573,65.698843691253));
#139385=CARTESIAN_POINT('Ctrl Pts',(109.272976618669,13.24615345175,65.64976472428));
#139386=CARTESIAN_POINT('Ctrl Pts',(109.040013032869,13.30596297823,65.604480964464));
#139387=CARTESIAN_POINT('Ctrl Pts',(108.825547120869,13.35968474504,65.562792806159));
#139388=CARTESIAN_POINT('Ctrl Pts',(108.629121421369,13.40779565601,65.524611327444));
#139389=CARTESIAN_POINT('Ctrl Pts',(108.449337565069,13.450945346,65.4896647114781));
#139390=CARTESIAN_POINT('Ctrl Pts',(108.282845082069,13.49017017699,65.457301689655));
#139391=CARTESIAN_POINT('Ctrl Pts',(108.124940203269,13.52671123059,65.4266079373401));
#139392=CARTESIAN_POINT('Ctrl Pts',(107.970931288969,13.56172653136,65.396671487568));
#139393=CARTESIAN_POINT('Ctrl Pts',(107.817206225169,13.59605474132,65.36679021304));
#139394=CARTESIAN_POINT('Ctrl Pts',(107.662578501669,13.62995615997,65.336733478351));
#139395=CARTESIAN_POINT('Ctrl Pts',(107.510130596069,13.6627294738,65.307100459463));
#139396=CARTESIAN_POINT('Ctrl Pts',(107.363438577269,13.69380725163,65.2785862772031));
#139397=CARTESIAN_POINT('Ctrl Pts',(107.221789626269,13.72357312524,65.251052372917));
#139398=CARTESIAN_POINT('Ctrl Pts',(107.077134525369,13.75386002214,65.222934129361));
#139399=CARTESIAN_POINT('Ctrl Pts',(106.945826768369,13.7811896625,65.197410359595));
#139400=CARTESIAN_POINT('Ctrl Pts',(106.761987215069,13.81857739095,65.161675392064));
#139401=CARTESIAN_POINT('Ctrl Pts',(106.619843652369,13.84194334108,65.134045344527));
#139402=CARTESIAN_POINT('Ctrl Pts',(106.491225279869,13.86468918368,65.109044340758));
#139403=CARTESIAN_POINT('Ctrl Pts',(106.353519635369,13.88907030211,65.082276941433));
#139404=CARTESIAN_POINT('Ctrl Pts',(106.216904540369,13.91398950909,65.055721524524));
#139405=CARTESIAN_POINT('Ctrl Pts',(106.063926293969,13.941918642,65.0259854173001));
#139406=CARTESIAN_POINT('Ctrl Pts',(105.917646289669,13.96777740158,64.9975513229521));
#139407=CARTESIAN_POINT('Ctrl Pts',(105.824467051569,13.98388893623,64.979439023457));
#139408=CARTESIAN_POINT('Ctrl Pts',(105.781591860669,13.99124786247,64.971104889017));
#139409=CARTESIAN_POINT('Ctrl Pts',(121.290407464969,-0.204882710558486,
68.4579759859419));
#139410=CARTESIAN_POINT('Ctrl Pts',(121.291722773869,-0.176211439766586,
68.458231657368));
#139411=CARTESIAN_POINT('Ctrl Pts',(121.296018466569,-0.0558111958484758,
68.4590666596059));
#139412=CARTESIAN_POINT('Ctrl Pts',(121.294894640169,0.169287343740214,
68.458848208792));
#139413=CARTESIAN_POINT('Ctrl Pts',(121.275184333069,0.483084097755514,
68.455016894092));
#139414=CARTESIAN_POINT('Ctrl Pts',(121.233313886869,0.832067022022413,
68.446878063204));
#139415=CARTESIAN_POINT('Ctrl Pts',(121.165010752469,1.21693268067301,68.43360121256));
#139416=CARTESIAN_POINT('Ctrl Pts',(121.065468336969,1.63801635965901,68.414252030502));
#139417=CARTESIAN_POINT('Ctrl Pts',(120.928103238269,2.09747231783601,68.3875508269161));
#139418=CARTESIAN_POINT('Ctrl Pts',(120.743510246669,2.59992041829301,68.351669405084));
#139419=CARTESIAN_POINT('Ctrl Pts',(120.500011077769,3.14638720868801,68.304337725156));
#139420=CARTESIAN_POINT('Ctrl Pts',(120.186675852369,3.73296277122801,68.243431223252));
#139421=CARTESIAN_POINT('Ctrl Pts',(119.794700622469,4.35331508274601,68.167238576668));
#139422=CARTESIAN_POINT('Ctrl Pts',(119.314325889769,5.00291352389501,68.073862721656));
#139423=CARTESIAN_POINT('Ctrl Pts',(118.731733404269,5.67854631422901,67.960617649101));
#139424=CARTESIAN_POINT('Ctrl Pts',(118.030855054569,6.37668456263001,67.824380018941));
#139425=CARTESIAN_POINT('Ctrl Pts',(117.219127524269,7.07160901930201,67.666595383297));
#139426=CARTESIAN_POINT('Ctrl Pts',(116.348385995069,7.71461639877401,67.4973395310339));
#139427=CARTESIAN_POINT('Ctrl Pts',(115.491766329969,8.26798544955901,67.330828704796));
#139428=CARTESIAN_POINT('Ctrl Pts',(114.700170236569,8.72360902037701,67.176957243574));
#139429=CARTESIAN_POINT('Ctrl Pts',(113.979110609969,9.09909850463502,67.036796751032));
#139430=CARTESIAN_POINT('Ctrl Pts',(113.321435688169,9.41261032332302,66.908957058466));
#139431=CARTESIAN_POINT('Ctrl Pts',(112.720982650669,9.67708291583402,66.792240228967));
#139432=CARTESIAN_POINT('Ctrl Pts',(112.171841675469,9.902328359459,66.6854975037769));
#139433=CARTESIAN_POINT('Ctrl Pts',(111.669134764169,10.09570047157,66.587780691319));
#139434=CARTESIAN_POINT('Ctrl Pts',(111.208133592469,10.26299232414,66.498170693874));
#139435=CARTESIAN_POINT('Ctrl Pts',(110.785032929769,10.4086021075,66.415927845836));
#139436=CARTESIAN_POINT('Ctrl Pts',(110.396312672269,10.53606279464,66.340367904965));
#139437=CARTESIAN_POINT('Ctrl Pts',(110.038870817469,10.64819187163,66.270887900006));
#139438=CARTESIAN_POINT('Ctrl Pts',(109.709907973469,10.74727470395,66.2069436815879));
#139439=CARTESIAN_POINT('Ctrl Pts',(109.406977840669,10.83516748103,66.14805973489));
#139440=CARTESIAN_POINT('Ctrl Pts',(109.127876237269,10.91340649905,66.093807608205));
#139441=CARTESIAN_POINT('Ctrl Pts',(108.870510477969,10.98330151766,66.043780522695));
#139442=CARTESIAN_POINT('Ctrl Pts',(108.632791943669,11.04599917505,65.997572489929));
#139443=CARTESIAN_POINT('Ctrl Pts',(108.413036697869,11.1024184024,65.954856184158));
#139444=CARTESIAN_POINT('Ctrl Pts',(108.210380230269,11.15318242101,65.915463560757));
#139445=CARTESIAN_POINT('Ctrl Pts',(108.024506582569,11.19870926078,65.8793332033499));
#139446=CARTESIAN_POINT('Ctrl Pts',(107.854094394369,11.23960977399,65.8462082642299));
#139447=CARTESIAN_POINT('Ctrl Pts',(107.696315795769,11.2767815596,65.8155390584099));
#139448=CARTESIAN_POINT('Ctrl Pts',(107.546794808369,11.31138233835,65.7864749776119));
#139449=CARTESIAN_POINT('Ctrl Pts',(107.401045681469,11.34451971807,65.7581440758939));
#139450=CARTESIAN_POINT('Ctrl Pts',(107.255610411169,11.37699645313,65.729874182013));
#139451=CARTESIAN_POINT('Ctrl Pts',(107.109463370769,11.40903903339,65.7014659333571));
#139452=CARTESIAN_POINT('Ctrl Pts',(106.965082265369,11.44007717534,65.6734009494109));
#139453=CARTESIAN_POINT('Ctrl Pts',(106.823492358169,11.47008321468,65.645878522126));
#139454=CARTESIAN_POINT('Ctrl Pts',(106.683022261469,11.49957838658,65.618573765051));
#139455=CARTESIAN_POINT('Ctrl Pts',(106.544542981469,11.52865699124,65.591655985468));
#139456=CARTESIAN_POINT('Ctrl Pts',(106.401009057569,11.5582405323,65.563755677742));
#139457=CARTESIAN_POINT('Ctrl Pts',(106.294551394269,11.58057728559,65.5430623009789));
#139458=CARTESIAN_POINT('Ctrl Pts',(106.161891727069,11.60262990991,65.517275745167));
#139459=CARTESIAN_POINT('Ctrl Pts',(106.021746980969,11.62728669818,65.4900342301539));
#139460=CARTESIAN_POINT('Ctrl Pts',(105.878527906069,11.65267667008,65.462195123188));
#139461=CARTESIAN_POINT('Ctrl Pts',(105.731357675069,11.67950920349,65.4335879854359));
#139462=CARTESIAN_POINT('Ctrl Pts',(105.588315833369,11.70562561188,65.405783329264));
#139463=CARTESIAN_POINT('Ctrl Pts',(105.452624863869,11.72961264266,65.379407545042));
#139464=CARTESIAN_POINT('Ctrl Pts',(105.363840824969,11.74496663286,65.3621495899899));
#139465=CARTESIAN_POINT('Ctrl Pts',(105.322770210069,11.75201580539,65.354166231342));
#139466=CARTESIAN_POINT('',(122.019294419317,7.00634560479863E-5,71.2800197814689));
#139467=CARTESIAN_POINT('Origin',(121.309092222769,1.20142455100609E-5,
69.958803843484));
#139468=CARTESIAN_POINT('',(105.406714409596,13.3449720448593,67.5261054277314));
#139469=CARTESIAN_POINT('Ctrl Pts',(122.019295120988,7.90940703660764E-5,
71.2800210882645));
#139470=CARTESIAN_POINT('Ctrl Pts',(122.019289267816,0.0647943413365559,
71.2800206364224));
#139471=CARTESIAN_POINT('Ctrl Pts',(122.018318643201,0.131954861220223,
71.2797688245955));
#139472=CARTESIAN_POINT('Ctrl Pts',(122.016222139614,0.201503059088793,
71.2792342641219));
#139473=CARTESIAN_POINT('Ctrl Pts',(122.013660899416,0.286468160628148,
71.2785812064394));
#139474=CARTESIAN_POINT('Ctrl Pts',(122.009418906529,0.374996384007158,
71.2775060829595));
#139475=CARTESIAN_POINT('Ctrl Pts',(122.003193436169,0.466992869080882,
71.2759496210239));
#139476=CARTESIAN_POINT('Ctrl Pts',(122.000532207089,0.506319009454073,
71.2752842734237));
#139477=CARTESIAN_POINT('Ctrl Pts',(121.997509100327,0.546278850207114,
71.2745310758335));
#139478=CARTESIAN_POINT('Ctrl Pts',(121.994103439403,0.586864690865039,
71.2736859574118));
#139479=CARTESIAN_POINT('Ctrl Pts',(121.993986998336,0.588252338875545,
71.2736570624357));
#139480=CARTESIAN_POINT('Ctrl Pts',(121.99387011027,0.589640718656464,71.2736280600436));
#139481=CARTESIAN_POINT('Ctrl Pts',(121.993752774232,0.591029829879343,
71.2735989500439));
#139482=CARTESIAN_POINT('Ctrl Pts',(121.985566143102,0.687949253089373,
71.2715679216144));
#139483=CARTESIAN_POINT('Ctrl Pts',(121.975194990935,0.78842994343254,71.2690123528165));
#139484=CARTESIAN_POINT('Ctrl Pts',(121.962330547539,0.892356419153909,
71.2658712651658));
#139485=CARTESIAN_POINT('Ctrl Pts',(121.957679506311,0.929930242469154,
71.2647356289231));
#139486=CARTESIAN_POINT('Ctrl Pts',(121.95270301165,0.967954403017347,71.2635235422822));
#139487=CARTESIAN_POINT('Ctrl Pts',(121.947388177942,1.00642321275053,71.2622324436963));
#139488=CARTESIAN_POINT('Ctrl Pts',(121.942961170466,1.03846592897076,71.261157019063));
#139489=CARTESIAN_POINT('Ctrl Pts',(121.938299456839,1.07081714263468,71.2600267821974));
#139490=CARTESIAN_POINT('Ctrl Pts',(121.933394121336,1.10347377448982,71.2588399639624));
#139491=CARTESIAN_POINT('Ctrl Pts',(121.928880251392,1.1335242754022,71.2577478586096));
#139492=CARTESIAN_POINT('Ctrl Pts',(121.924160093542,1.16383339195402,71.2566078426418));
#139493=CARTESIAN_POINT('Ctrl Pts',(121.919226920107,1.19439871366745,71.2554185770162));
#139494=CARTESIAN_POINT('Ctrl Pts',(121.91676033339,1.20968137452416,71.2548239442034));
#139495=CARTESIAN_POINT('Ctrl Pts',(121.914240493777,1.22502808690805,71.2542170008458));
#139496=CARTESIAN_POINT('Ctrl Pts',(121.911666584572,1.240438548423,71.2535975820344));
#139497=CARTESIAN_POINT('Ctrl Pts',(121.91037962997,1.24814377918047,71.2532878726287));
#139498=CARTESIAN_POINT('Ctrl Pts',(121.909079158038,1.25586494723633,71.2529750444866));
#139499=CARTESIAN_POINT('Ctrl Pts',(121.907765067742,1.2636020148263,71.2526590774403));
#139500=CARTESIAN_POINT('Ctrl Pts',(121.906450977447,1.27133908241627,71.252343110394));
#139501=CARTESIAN_POINT('Ctrl Pts',(121.905345477426,1.27780513545291,71.2520773879648));
#139502=CARTESIAN_POINT('Ctrl Pts',(121.903781841349,1.28686087846409,71.2517017397815));
#139503=CARTESIAN_POINT('Ctrl Pts',(121.893675018398,1.34539418595264,71.2492736750057));
#139504=CARTESIAN_POINT('Ctrl Pts',(121.882990116065,1.4036627614239,71.2467149294755));
#139505=CARTESIAN_POINT('Ctrl Pts',(121.871758031279,1.46167228038696,71.2440313578717));
#139506=CARTESIAN_POINT('Ctrl Pts',(121.839585104505,1.62783341977771,71.2363445967452));
#139507=CARTESIAN_POINT('Ctrl Pts',(121.802924103343,1.7918689670011,71.2276340039114));
#139508=CARTESIAN_POINT('Ctrl Pts',(121.762233017693,1.95384294374939,71.2179845293854));
#139509=CARTESIAN_POINT('Ctrl Pts',(121.7171041166,2.13348198408125,71.207282672344));
#139510=CARTESIAN_POINT('Ctrl Pts',(121.667018015079,2.31058496009605,71.1954259703313));
#139511=CARTESIAN_POINT('Ctrl Pts',(121.612456284331,2.48510922069926,71.1825013370691));
#139512=CARTESIAN_POINT('Ctrl Pts',(121.605844188692,2.50625904653242,71.1809350577363));
#139513=CARTESIAN_POINT('Ctrl Pts',(121.599166336251,2.52737100916192,71.1793530879279));
#139514=CARTESIAN_POINT('Ctrl Pts',(121.592423339081,2.54844495564597,71.1777555334907));
#139515=CARTESIAN_POINT('Ctrl Pts',(121.570387141685,2.61731487104202,71.1725347060102));
#139516=CARTESIAN_POINT('Ctrl Pts',(121.547771847224,2.68542579166921,71.1671755693551));
#139517=CARTESIAN_POINT('Ctrl Pts',(121.524426417993,2.75331290177076,71.1616399870936));
#139518=CARTESIAN_POINT('Ctrl Pts',(121.501839088884,2.8189955021176,71.156284162743));
#139519=CARTESIAN_POINT('Ctrl Pts',(121.478567927336,2.8844685952812,71.1507630994509));
#139520=CARTESIAN_POINT('Ctrl Pts',(121.454433664412,2.95020029573306,71.1450338015792));
#139521=CARTESIAN_POINT('Ctrl Pts',(121.44085225073,2.98719042129487,71.1418096730964));
#139522=CARTESIAN_POINT('Ctrl Pts',(121.426677824928,3.02513969909136,71.1384410813606));
#139523=CARTESIAN_POINT('Ctrl Pts',(121.411873730377,3.06403062878303,71.1349206106562));
#139524=CARTESIAN_POINT('Ctrl Pts',(121.379422169101,3.14928213697947,71.1272035043927));
#139525=CARTESIAN_POINT('Ctrl Pts',(121.343945536334,3.23906194266524,71.1187567522501));
#139526=CARTESIAN_POINT('Ctrl Pts',(121.305061550388,3.33313900792745,71.1095025213745));
#139527=CARTESIAN_POINT('Ctrl Pts',(121.267663668914,3.42362054809094,71.1006019773332));
#139528=CARTESIAN_POINT('Ctrl Pts',(121.227113224768,3.51807739288653,71.090954361199));
#139529=CARTESIAN_POINT('Ctrl Pts',(121.18306369568,3.61625626876824,71.0804886127768));
#139530=CARTESIAN_POINT('Ctrl Pts',(121.170900807039,3.64336526990759,71.0775988263196));
#139531=CARTESIAN_POINT('Ctrl Pts',(121.158471137288,3.67075774226389,71.0746466598495));
#139532=CARTESIAN_POINT('Ctrl Pts',(121.145767408056,3.69842763712042,71.071630613055));
#139533=CARTESIAN_POINT('Ctrl Pts',(121.096880958574,3.80490683644929,71.0600242715965));
#139534=CARTESIAN_POINT('Ctrl Pts',(121.04393485288,3.91549749133993,71.047471771854));
#139535=CARTESIAN_POINT('Ctrl Pts',(120.986524703389,4.02987745307783,71.0338891741002));
#139536=CARTESIAN_POINT('Ctrl Pts',(120.930069118973,4.14235560620328,71.0205324157416));
#139537=CARTESIAN_POINT('Ctrl Pts',(120.869295767781,4.25849825442164,71.0061793466359));
#139538=CARTESIAN_POINT('Ctrl Pts',(120.803842983608,4.37795570528577,70.990753891926));
#139539=CARTESIAN_POINT('Ctrl Pts',(120.734846789541,4.50388021051043,70.974493351138));
#139540=CARTESIAN_POINT('Ctrl Pts',(120.660650628725,4.63348670967809,70.9570411482275));
#139541=CARTESIAN_POINT('Ctrl Pts',(120.580836495019,4.76636918385725,70.9383084113126));
#139542=CARTESIAN_POINT('Ctrl Pts',(120.54978599603,4.81806512965831,70.9310207192506));
#139543=CARTESIAN_POINT('Ctrl Pts',(120.517885643202,4.87025653226186,70.9235392920141));
#139544=CARTESIAN_POINT('Ctrl Pts',(120.485112661211,4.92291812442057,70.915859214682));
#139545=CARTESIAN_POINT('Ctrl Pts',(120.468726170215,4.94924892049992,70.912019176016));
#139546=CARTESIAN_POINT('Ctrl Pts',(120.452121524324,4.97569726616381,70.9081294795746));
#139547=CARTESIAN_POINT('Ctrl Pts',(120.435296012009,5.00225991615915,70.9041895297866));
#139548=CARTESIAN_POINT('Ctrl Pts',(120.426883255851,5.01554124115682,70.9022195548926));
#139549=CARTESIAN_POINT('Ctrl Pts',(120.418415283273,5.02885114240544,70.9002370170293));
#139550=CARTESIAN_POINT('Ctrl Pts',(120.409891760874,5.04218921203787,70.8982418433462));
#139551=CARTESIAN_POINT('Ctrl Pts',(120.402622319957,5.05356482702362,70.8965402232263));
#139552=CARTESIAN_POINT('Ctrl Pts',(120.394502748834,5.06621986006523,70.8946399061895));
#139553=CARTESIAN_POINT('Ctrl Pts',(120.387604345069,5.07693276007905,70.8930256645897));
#139554=CARTESIAN_POINT('Ctrl Pts',(120.386414272748,5.07878088701002,70.8927471850585));
#139555=CARTESIAN_POINT('Ctrl Pts',(120.385260645217,5.08057129006946,70.8924772403038));
#139556=CARTESIAN_POINT('Ctrl Pts',(120.384154213863,5.08228751718077,70.892218343275));
#139557=CARTESIAN_POINT('Ctrl Pts',(120.38328842148,5.08363048017059,70.8920157540457));
#139558=CARTESIAN_POINT('Ctrl Pts',(120.382422028954,5.08497378351582,70.8918130272488));
#139559=CARTESIAN_POINT('Ctrl Pts',(120.381555035884,5.08631742674835,70.8916101627974));
#139560=CARTESIAN_POINT('Ctrl Pts',(120.297380541915,5.21676886076607,70.8719144891612));
#139561=CARTESIAN_POINT('Ctrl Pts',(120.207542559621,5.35042682384027,70.8509208255));
#139562=CARTESIAN_POINT('Ctrl Pts',(120.111639563024,5.48684674179412,70.8285420924557));
#139563=CARTESIAN_POINT('Ctrl Pts',(120.033812301504,5.59755432140991,70.810381288613));
#139564=CARTESIAN_POINT('Ctrl Pts',(119.951991106251,5.71008018537599,70.7913083616764));
#139565=CARTESIAN_POINT('Ctrl Pts',(119.865981203322,5.824171158714,70.7712801501997));
#139566=CARTESIAN_POINT('Ctrl Pts',(119.831507080685,5.869900616284,70.7632525278548));
#139567=CARTESIAN_POINT('Ctrl Pts',(119.796360255117,5.91588136703911,70.7550714751542));
#139568=CARTESIAN_POINT('Ctrl Pts',(119.760529634078,5.96209610073101,70.7467344750781));
#139569=CARTESIAN_POINT('Ctrl Pts',(119.72111031052,6.01293958286343,70.7375624625932));
#139570=CARTESIAN_POINT('Ctrl Pts',(119.680863335153,6.06406627492084,70.7282016956236));
#139571=CARTESIAN_POINT('Ctrl Pts',(119.639775001278,6.11545251694759,70.7186490114928));
#139572=CARTESIAN_POINT('Ctrl Pts',(119.61923083434,6.14114563796097,70.7138726694273));
#139573=CARTESIAN_POINT('Ctrl Pts',(119.598476329699,6.16690364875147,70.7090483520244));
#139574=CARTESIAN_POINT('Ctrl Pts',(119.577509905512,6.19272351736988,70.7041756832797));
#139575=CARTESIAN_POINT('Ctrl Pts',(119.567026693418,6.20563345167909,70.7017393489074));
#139576=CARTESIAN_POINT('Ctrl Pts',(119.556490501579,6.21855885061051,70.6992909269887));
#139577=CARTESIAN_POINT('Ctrl Pts',(119.545901136964,6.23149933351409,70.6968303719765));
#139578=CARTESIAN_POINT('Ctrl Pts',(119.540606454656,6.23796957496588,70.6956000944704));
#139579=CARTESIAN_POINT('Ctrl Pts',(119.535298479164,6.24444358742153,70.6943667837094));
#139580=CARTESIAN_POINT('Ctrl Pts',(119.529977186838,6.25092132305579,70.6931304340879));
#139581=CARTESIAN_POINT('Ctrl Pts',(119.525986217594,6.25577962478147,70.6922031718717));
#139582=CARTESIAN_POINT('Ctrl Pts',(119.521987757632,6.26064002079604,70.6912742002981));
#139583=CARTESIAN_POINT('Ctrl Pts',(119.517981797084,6.26550249087177,70.6903435170244));
#139584=CARTESIAN_POINT('Ctrl Pts',(119.516646476901,6.26712331423035,70.6900332892666));
#139585=CARTESIAN_POINT('Ctrl Pts',(119.516325625924,6.26751317211349,70.6899587459064));
#139586=CARTESIAN_POINT('Ctrl Pts',(119.513973335985,6.27036565154658,70.689412263098));
#139587=CARTESIAN_POINT('Ctrl Pts',(119.445940346586,6.3528651341979,70.6736068734286));
#139588=CARTESIAN_POINT('Ctrl Pts',(119.379990061922,6.43080116154606,70.658306683783));
#139589=CARTESIAN_POINT('Ctrl Pts',(119.316404933559,6.50440018602863,70.6435704089504));
#139590=CARTESIAN_POINT('Ctrl Pts',(119.291094816403,6.53369634348217,70.6377046215869));
#139591=CARTESIAN_POINT('Ctrl Pts',(119.266158907851,6.56230510491915,70.6319280753122));
#139592=CARTESIAN_POINT('Ctrl Pts',(119.241612972835,6.59023986855823,70.626244060308));
#139593=CARTESIAN_POINT('Ctrl Pts',(119.177469096201,6.66323949279387,70.6113904905832));
#139594=CARTESIAN_POINT('Ctrl Pts',(119.11599130841,6.73163862511283,70.5971694189702));
#139595=CARTESIAN_POINT('Ctrl Pts',(119.057421138099,6.79566735526086,70.5836315498303));
#139596=CARTESIAN_POINT('Ctrl Pts',(118.996896118557,6.86183312057973,70.5696418381751));
#139597=CARTESIAN_POINT('Ctrl Pts',(118.93947591326,6.92333197083014,70.5563816727075));
#139598=CARTESIAN_POINT('Ctrl Pts',(118.885381777702,6.98038540499861,70.5438977543021));
#139599=CARTESIAN_POINT('Ctrl Pts',(118.830325629018,7.03845348062509,70.531191821195));
#139600=CARTESIAN_POINT('Ctrl Pts',(118.778714658739,7.09191663079638,70.5192899446257));
#139601=CARTESIAN_POINT('Ctrl Pts',(118.730739096332,7.14097469522637,70.5082324977803));
#139602=CARTESIAN_POINT('Ctrl Pts',(118.681463061506,7.19136257543249,70.4968753169885));
#139603=CARTESIAN_POINT('Ctrl Pts',(118.636022019864,7.23710338697868,70.4864089350787));
#139604=CARTESIAN_POINT('Ctrl Pts',(118.594580255186,7.27837773112763,70.4768684059795));
#139605=CARTESIAN_POINT('Ctrl Pts',(118.558239789795,7.3145713847215,70.468502274126));
#139606=CARTESIAN_POINT('Ctrl Pts',(118.524973858968,7.34732992666515,70.4608479323379));
#139607=CARTESIAN_POINT('Ctrl Pts',(118.494869538803,7.37675286197228,70.4539240473464));
#139608=CARTESIAN_POINT('Ctrl Pts',(118.463440223853,7.40747080197225,70.4466954183359));
#139609=CARTESIAN_POINT('Ctrl Pts',(118.435456902054,7.43455317802427,70.4402629544865));
#139610=CARTESIAN_POINT('Ctrl Pts',(118.41099536373,7.45808970851861,70.4346429705706));
#139611=CARTESIAN_POINT('Ctrl Pts',(118.39784091329,7.47074672623445,70.4316207648975));
#139612=CARTESIAN_POINT('Ctrl Pts',(118.385704538703,7.48237792553573,70.4288334372906));
#139613=CARTESIAN_POINT('Ctrl Pts',(118.374595490617,7.49299443529233,70.4262829948165));
#139614=CARTESIAN_POINT('Ctrl Pts',(118.369040966574,7.49830269017064,70.4250077735794));
#139615=CARTESIAN_POINT('Ctrl Pts',(118.363743263503,7.50335725592985,70.4237917504513));
#139616=CARTESIAN_POINT('Ctrl Pts',(118.358703359586,7.50815932475693,70.4226351631851));
#139617=CARTESIAN_POINT('Ctrl Pts',(118.356183407627,7.51056035917047,70.422056869552));
#139618=CARTESIAN_POINT('Ctrl Pts',(118.353727904802,7.51289826832515,70.42149343346));
#139619=CARTESIAN_POINT('Ctrl Pts',(118.351336966545,7.51517319233377,70.4209448794642));
#139620=CARTESIAN_POINT('Ctrl Pts',(118.350141497417,7.51631065433808,70.4206706024662));
#139621=CARTESIAN_POINT('Ctrl Pts',(118.348962169391,7.51743236999189,70.4204000459041));
#139622=CARTESIAN_POINT('Ctrl Pts',(118.347798996254,7.51853835607367,70.4201332127564));
#139623=CARTESIAN_POINT('Ctrl Pts',(118.347217409686,7.51909134911456,70.4199997961826));
#139624=CARTESIAN_POINT('Ctrl Pts',(118.346996942952,7.51930102883103,70.4199491531009));
#139625=CARTESIAN_POINT('Ctrl Pts',(118.346601988741,7.51967648864734,70.4198585474782));
#139626=CARTESIAN_POINT('Ctrl Pts',(118.34620703453,7.52005194846366,70.4197679418556));
#139627=CARTESIAN_POINT('Ctrl Pts',(118.345637604999,7.52059320757401,70.4196374001701));
#139628=CARTESIAN_POINT('Ctrl Pts',(118.344357955025,7.52180914202048,70.4193438863148));
#139629=CARTESIAN_POINT('Ctrl Pts',(118.200158384446,7.65882881815134,70.3862687698805));
#139630=CARTESIAN_POINT('Ctrl Pts',(118.050682131663,7.79545090863632,70.3520656867254));
#139631=CARTESIAN_POINT('Ctrl Pts',(117.895912984387,7.93140957380592,70.3167280067712));
#139632=CARTESIAN_POINT('Ctrl Pts',(117.802236164841,8.01370100957925,70.2953392382312));
#139633=CARTESIAN_POINT('Ctrl Pts',(117.706621202113,8.09574957147887,70.2735349854436));
#139634=CARTESIAN_POINT('Ctrl Pts',(117.609073502286,8.17749823024438,70.251315515606));
#139635=CARTESIAN_POINT('Ctrl Pts',(117.444287644727,8.31559500610868,70.2137805004471));
#139636=CARTESIAN_POINT('Ctrl Pts',(117.273984287767,8.45283498799986,70.1750601865364));
#139637=CARTESIAN_POINT('Ctrl Pts',(117.098159722788,8.58895961478438,70.1351500200475));
#139638=CARTESIAN_POINT('Ctrl Pts',(116.951603325369,8.70242461840276,70.1018833930451));
#139639=CARTESIAN_POINT('Ctrl Pts',(116.80121154568,8.81511488236514,70.0677902031773));
#139640=CARTESIAN_POINT('Ctrl Pts',(116.647007803204,8.92689034648425,70.0328727497835));
#139641=CARTESIAN_POINT('Ctrl Pts',(116.458342625104,9.06364537918784,69.9901519476967));
#139642=CARTESIAN_POINT('Ctrl Pts',(116.263970617385,9.19903062515022,69.9461971697683));
#139643=CARTESIAN_POINT('Ctrl Pts',(116.063915585821,9.33278943972281,69.9010088645471));
#139644=CARTESIAN_POINT('Ctrl Pts',(115.956162455114,9.40483427117338,69.8766696548764));
#139645=CARTESIAN_POINT('Ctrl Pts',(115.846761399342,9.47640759478814,69.8519727368525));
#139646=CARTESIAN_POINT('Ctrl Pts',(115.73572181815,9.54747187918183,69.8269192787979));
#139647=CARTESIAN_POINT('Ctrl Pts',(115.528407371014,9.68015116950339,69.7801436718507));
#139648=CARTESIAN_POINT('Ctrl Pts',(115.315378836785,9.81105470690549,69.732124750275));
#139649=CARTESIAN_POINT('Ctrl Pts',(115.09668957018,9.93994417389922,69.6828685683572));
#139650=CARTESIAN_POINT('Ctrl Pts',(115.033851659791,9.9769791180592,69.6687153563888));
#139651=CARTESIAN_POINT('Ctrl Pts',(114.970546664127,10.013847921227,69.6544600469835));
#139652=CARTESIAN_POINT('Ctrl Pts',(114.906776553754,10.0505453006162,69.6401029203365));
#139653=CARTESIAN_POINT('Ctrl Pts',(114.683663611381,10.1789386849936,69.5898715384005));
#139654=CARTESIAN_POINT('Ctrl Pts',(114.45485392192,10.3052317113346,69.538393175952));
#139655=CARTESIAN_POINT('Ctrl Pts',(114.220422929518,10.4292047081467,69.4856780824899));
#139656=CARTESIAN_POINT('Ctrl Pts',(114.197912463071,10.4411088081827,69.4806162886951));
#139657=CARTESIAN_POINT('Ctrl Pts',(114.175350201025,10.4529915373186,69.4755430985869));
#139658=CARTESIAN_POINT('Ctrl Pts',(114.152736231951,10.4648527141662,69.4704585254692));
#139659=CARTESIAN_POINT('Ctrl Pts',(114.071950519389,10.5072253565056,69.4522944932711));
#139660=CARTESIAN_POINT('Ctrl Pts',(113.990504886149,10.5493229216099,69.4339851843099));
#139661=CARTESIAN_POINT('Ctrl Pts',(113.908402120511,10.5911370811685,69.4155309622082));
#139662=CARTESIAN_POINT('Ctrl Pts',(113.779449253332,10.656811552934,69.3865462522161));
#139663=CARTESIAN_POINT('Ctrl Pts',(113.648875154649,10.721786775683,69.3572040269525));
#139664=CARTESIAN_POINT('Ctrl Pts',(113.516693352567,10.7860324519638,69.3275062031431));
#139665=CARTESIAN_POINT('Ctrl Pts',(113.499773738249,10.7942560655561,69.3237048044859));
#139666=CARTESIAN_POINT('Ctrl Pts',(113.482827787115,10.8024677267741,69.319897582974));
#139667=CARTESIAN_POINT('Ctrl Pts',(113.465855531575,10.8106673757003,69.3160845426478));
#139668=CARTESIAN_POINT('Ctrl Pts',(113.416531260478,10.8344969548387,69.3050031967232));
#139669=CARTESIAN_POINT('Ctrl Pts',(113.366984821204,10.8582250772314,69.2938727050108));
#139670=CARTESIAN_POINT('Ctrl Pts',(113.31721717765,10.8818501694279,69.282693199195));
#139671=CARTESIAN_POINT('Ctrl Pts',(113.283770946889,10.8977273584796,69.2751800379398));
#139672=CARTESIAN_POINT('Ctrl Pts',(113.250224804113,10.9135580175483,69.2676447391799));
#139673=CARTESIAN_POINT('Ctrl Pts',(113.216579071131,10.9293416679507,69.2600873575252));
#139674=CARTESIAN_POINT('Ctrl Pts',(113.19975620464,10.937233493152,69.2563086666978));
#139675=CARTESIAN_POINT('Ctrl Pts',(113.182908440637,10.9451135663309,69.2525244552646));
#139676=CARTESIAN_POINT('Ctrl Pts',(113.16603581926,10.95298182955,69.2487347296099));
#139677=CARTESIAN_POINT('Ctrl Pts',(113.151272275554,10.9598665598666,69.2454187196621));
#139678=CARTESIAN_POINT('Ctrl Pts',(113.136489700425,10.9667422481908,69.2420984878953));
#139679=CARTESIAN_POINT('Ctrl Pts',(113.121688121565,10.9736088558954,69.2387740388456));
#139680=CARTESIAN_POINT('Ctrl Pts',(113.119573610299,10.9745897998531,69.2382991175528));
#139681=CARTESIAN_POINT('Ctrl Pts',(113.116366937548,10.976076666686,69.2375788978328));
#139682=CARTESIAN_POINT('Ctrl Pts',(113.115343424368,10.9765511317019,69.2373490167771));
#139683=CARTESIAN_POINT('Ctrl Pts',(113.022976761086,11.0193690955673,69.2166034646097));
#139684=CARTESIAN_POINT('Ctrl Pts',(112.930834667136,11.0613846056466,69.1959129276571));
#139685=CARTESIAN_POINT('Ctrl Pts',(112.838937704407,11.1026247607013,69.1752819476934));
#139686=CARTESIAN_POINT('Ctrl Pts',(112.647247007684,11.18864886662,69.1322471530072));
#139687=CARTESIAN_POINT('Ctrl Pts',(112.456623792903,11.2713003057167,69.0894716794575));
#139688=CARTESIAN_POINT('Ctrl Pts',(112.267226049986,11.3508294215004,69.0469910784709));
#139689=CARTESIAN_POINT('Ctrl Pts',(112.091732133461,11.4245202469117,69.0076290093744));
#139690=CARTESIAN_POINT('Ctrl Pts',(111.917290107844,11.4955301585317,68.9685200568115));
#139691=CARTESIAN_POINT('Ctrl Pts',(111.744005625658,11.5640455179087,68.9296884945963));
#139692=CARTESIAN_POINT('Ctrl Pts',(111.583303488104,11.627585914419,68.8936765276053));
#139693=CARTESIAN_POINT('Ctrl Pts',(111.423596748605,11.6889807462734,68.857903100716));
#139694=CARTESIAN_POINT('Ctrl Pts',(111.264959024318,11.7483700241455,68.8223854153186));
#139695=CARTESIAN_POINT('Ctrl Pts',(111.117639763161,11.8035220037654,68.7894018409872));
#139696=CARTESIAN_POINT('Ctrl Pts',(110.971242327098,11.8569443146203,68.7566387989538));
#139697=CARTESIAN_POINT('Ctrl Pts',(110.825819706005,11.9087425450732,68.7241088364224));
#139698=CARTESIAN_POINT('Ctrl Pts',(110.822811595885,11.9098140068585,68.7234359444833));
#139699=CARTESIAN_POINT('Ctrl Pts',(110.819803902725,11.9108847735399,68.7227631522441));
#139700=CARTESIAN_POINT('Ctrl Pts',(110.81679662689,11.9119548460335,68.722090459795));
#139701=CARTESIAN_POINT('Ctrl Pts',(110.692917690131,11.9560344217133,68.694380189795));
#139702=CARTESIAN_POINT('Ctrl Pts',(110.569747036027,11.9989362809017,68.6668392805372));
#139703=CARTESIAN_POINT('Ctrl Pts',(110.447309202222,12.040723069193,68.6394738570784));
#139704=CARTESIAN_POINT('Ctrl Pts',(110.439135614158,12.0435126317275,68.6376470222547));
#139705=CARTESIAN_POINT('Ctrl Pts',(110.430965292181,12.0462972237657,68.6358209693533));
#139706=CARTESIAN_POINT('Ctrl Pts',(110.422798243196,12.0490768635367,68.6339957001427));
#139707=CARTESIAN_POINT('Ctrl Pts',(110.36979535197,12.0671162979387,68.6221499838254));
#139708=CARTESIAN_POINT('Ctrl Pts',(110.316930317783,12.0849471593495,68.6103372761136));
#139709=CARTESIAN_POINT('Ctrl Pts',(110.264205167338,12.1025741348408,68.5985580867996));
#139710=CARTESIAN_POINT('Ctrl Pts',(110.233780465725,12.1127456652231,68.5917609830058));
#139711=CARTESIAN_POINT('Ctrl Pts',(110.203402341482,12.1228493053584,68.5849750381828));
#139712=CARTESIAN_POINT('Ctrl Pts',(110.173071187232,12.1328859391197,68.5782003503594));
#139713=CARTESIAN_POINT('Ctrl Pts',(110.157905610107,12.1379042560003,68.5748130064478));
#139714=CARTESIAN_POINT('Ctrl Pts',(110.142751775457,12.1429058211661,68.5714284767039));
#139715=CARTESIAN_POINT('Ctrl Pts',(110.127609731102,12.1478907445677,68.5680467728983));
#139716=CARTESIAN_POINT('Ctrl Pts',(110.116253197836,12.1516294371188,68.5655104950441));
#139717=CARTESIAN_POINT('Ctrl Pts',(110.104903296609,12.1553587686674,68.5629758067734));
#139718=CARTESIAN_POINT('Ctrl Pts',(110.093560047501,12.1590787853552,68.5604427130416));
#139719=CARTESIAN_POINT('Ctrl Pts',(110.089778964465,12.1603187909178,68.5595983484643));
#139720=CARTESIAN_POINT('Ctrl Pts',(110.084399591553,12.1620814929756,68.558397087533));
#139721=CARTESIAN_POINT('Ctrl Pts',(110.0822190165,12.1627956987876,68.5579101510084));
#139722=CARTESIAN_POINT('Ctrl Pts',(110.072323754785,12.1660367032268,68.5557004750138));
#139723=CARTESIAN_POINT('Ctrl Pts',(110.062433616717,12.1692706333837,68.5534919885118));
#139724=CARTESIAN_POINT('Ctrl Pts',(110.052548615494,12.1724975198481,68.5512846947003));
#139725=CARTESIAN_POINT('Ctrl Pts',(109.938374789075,12.2097687317332,68.5257899906722));
#139726=CARTESIAN_POINT('Ctrl Pts',(109.8248863585,12.2461004228557,68.5004544222776));
#139727=CARTESIAN_POINT('Ctrl Pts',(109.712102670886,12.281538637848,68.4752827117343));
#139728=CARTESIAN_POINT('Ctrl Pts',(109.607043021169,12.3145498519027,68.4518348962885));
#139729=CARTESIAN_POINT('Ctrl Pts',(109.502594871715,12.3467857576586,68.4285292596018));
#139730=CARTESIAN_POINT('Ctrl Pts',(109.398772151862,12.3782819466524,68.4053692677365));
#139731=CARTESIAN_POINT('Ctrl Pts',(109.30209569012,12.4076102103943,68.3838034094094));
#139732=CARTESIAN_POINT('Ctrl Pts',(109.205961515276,12.4362970684511,68.3623638344511));
#139733=CARTESIAN_POINT('Ctrl Pts',(109.110380718673,12.4643700095465,68.3410532969063));
#139734=CARTESIAN_POINT('Ctrl Pts',(109.02135376668,12.490518027433,68.3212039938));
#139735=CARTESIAN_POINT('Ctrl Pts',(108.932806884898,12.5161334224034,68.3014666347423));
#139736=CARTESIAN_POINT('Ctrl Pts',(108.844745739944,12.5412378420218,68.2818427936572));
#139737=CARTESIAN_POINT('Ctrl Pts',(108.76259187315,12.5646582182426,68.2635353502629));
#139738=CARTESIAN_POINT('Ctrl Pts',(108.680860819629,12.5876338582503,68.2453267170413));
#139739=CARTESIAN_POINT('Ctrl Pts',(108.599570303343,12.6101796727279,68.2272207144974));
#139740=CARTESIAN_POINT('Ctrl Pts',(108.523569128167,12.6312584956201,68.2102928176904));
#139741=CARTESIAN_POINT('Ctrl Pts',(108.447952977039,12.6519616243288,68.1934546206468));
#139742=CARTESIAN_POINT('Ctrl Pts',(108.372726394293,12.6723051469411,68.176707307025));
#139743=CARTESIAN_POINT('Ctrl Pts',(108.30264726269,12.6912566444887,68.1611059444154));
#139744=CARTESIAN_POINT('Ctrl Pts',(108.232906198054,12.7098960577254,68.1455834507468));
#139745=CARTESIAN_POINT('Ctrl Pts',(108.163504487578,12.7282358457574,68.1301403141801));
#139746=CARTESIAN_POINT('Ctrl Pts',(108.099358819916,12.7451866952396,68.1158667422599));
#139747=CARTESIAN_POINT('Ctrl Pts',(108.035503077865,12.7618815736574,68.1016609676239));
#139748=CARTESIAN_POINT('Ctrl Pts',(107.971945043125,12.7783284770643,68.0875246872087));
#139749=CARTESIAN_POINT('Ctrl Pts',(107.913572073927,12.7934336418153,68.074541644787));
#139750=CARTESIAN_POINT('Ctrl Pts',(107.855450122654,12.8083296560643,68.0616172015617));
#139751=CARTESIAN_POINT('Ctrl Pts',(107.797560039676,12.8230276174717,68.048747775443));
#139752=CARTESIAN_POINT('Ctrl Pts',(107.760781209992,12.8323655522525,68.0405715489289));
#139753=CARTESIAN_POINT('Ctrl Pts',(107.72409599404,12.8416235330491,68.0324175337652));
#139754=CARTESIAN_POINT('Ctrl Pts',(107.687502594336,12.8508023216245,68.024285416003));
#139755=CARTESIAN_POINT('Ctrl Pts',(107.670503421704,12.8550662548149,68.0205077054097));
#139756=CARTESIAN_POINT('Ctrl Pts',(107.65352406376,12.8593130984262,68.0167347204085));
#139757=CARTESIAN_POINT('Ctrl Pts',(107.636564348739,12.8635429281521,68.0129664310072));
#139758=CARTESIAN_POINT('Ctrl Pts',(107.622044777864,12.8671641748781,68.0097403187187));
#139759=CARTESIAN_POINT('Ctrl Pts',(107.607539604355,12.8707729513676,68.0065176480808));
#139760=CARTESIAN_POINT('Ctrl Pts',(107.593048900532,12.8743692770539,68.003298435271));
#139761=CARTESIAN_POINT('Ctrl Pts',(107.577340550319,12.8782678001381,67.9998087136645));
#139762=CARTESIAN_POINT('Ctrl Pts',(107.561649142762,12.8821517050661,67.9963230454734));
#139763=CARTESIAN_POINT('Ctrl Pts',(107.545974860605,12.8860209974835,67.9928414660428));
#139764=CARTESIAN_POINT('Ctrl Pts',(107.530300578449,12.889890289901,67.9893598866122));
#139765=CARTESIAN_POINT('Ctrl Pts',(107.522944596978,12.8916999342926,67.9877262919716));
#139766=CARTESIAN_POINT('Ctrl Pts',(107.513208003348,12.8940940479048,67.985564593278));
#139767=CARTESIAN_POINT('Ctrl Pts',(107.503465179159,12.8964896935383,67.9834015112883));
#139768=CARTESIAN_POINT('Ctrl Pts',(107.493720506002,12.8988815104539,67.9812385969309));
#139769=CARTESIAN_POINT('Ctrl Pts',(107.483974020144,12.9012694810469,67.9790758600759));
#139770=CARTESIAN_POINT('Ctrl Pts',(107.454759494175,12.9084272843738,67.9725931818126));
#139771=CARTESIAN_POINT('Ctrl Pts',(107.425528681299,12.9155505295199,67.9661120982754));
#139772=CARTESIAN_POINT('Ctrl Pts',(107.396282628794,12.9226386763674,67.9596328889247));
#139773=CARTESIAN_POINT('Ctrl Pts',(107.375802408792,12.9276023140007,67.9550956737599));
#139774=CARTESIAN_POINT('Ctrl Pts',(107.355314482445,12.9325488044428,67.9505593124497));
#139775=CARTESIAN_POINT('Ctrl Pts',(107.334819026733,12.9374780121642,67.9460238496044));
#139776=CARTESIAN_POINT('Ctrl Pts',(107.284986691471,12.9494628118774,67.9349963951164));
#139777=CARTESIAN_POINT('Ctrl Pts',(107.235109852007,12.9613454408864,67.9239742535486));
#139778=CARTESIAN_POINT('Ctrl Pts',(107.185183076581,12.9731273009532,67.9129565133477));
#139779=CARTESIAN_POINT('Ctrl Pts',(107.177432063034,12.974956406803,67.9112460352959));
#139780=CARTESIAN_POINT('Ctrl Pts',(107.169679845774,12.9767830839771,67.9095356632865));
#139781=CARTESIAN_POINT('Ctrl Pts',(107.161926525056,12.978607292919,67.9078254173392));
#139782=CARTESIAN_POINT('Ctrl Pts',(107.122808841323,12.9878109401107,67.8991967455085));
#139783=CARTESIAN_POINT('Ctrl Pts',(107.083663058977,12.9969517614264,67.8905712807437));
#139784=CARTESIAN_POINT('Ctrl Pts',(107.044502082751,13.0060246694447,67.8819515950965));
#139785=CARTESIAN_POINT('Ctrl Pts',(107.040777543951,13.0068875794435,67.881131790364));
#139786=CARTESIAN_POINT('Ctrl Pts',(107.037041572928,13.0077523596621,67.8803097895492));
#139787=CARTESIAN_POINT('Ctrl Pts',(107.033299158713,13.0086179012633,67.8794865887452));
#139788=CARTESIAN_POINT('Ctrl Pts',(107.001299623324,13.0160187199605,67.8724478052909));
#139789=CARTESIAN_POINT('Ctrl Pts',(106.968831198066,13.0234723671859,67.8653217039039));
#139790=CARTESIAN_POINT('Ctrl Pts',(106.939044759508,13.030304302297,67.8587372704961));
#139791=CARTESIAN_POINT('Ctrl Pts',(106.935687244491,13.031074395193,67.8579950758895));
#139792=CARTESIAN_POINT('Ctrl Pts',(106.93236376191,13.031836624841,67.8572597550974));
#139793=CARTESIAN_POINT('Ctrl Pts',(106.929078782905,13.0325900521754,67.8565322009618));
#139794=CARTESIAN_POINT('Ctrl Pts',(106.91249838228,13.0363928548811,67.8528599890459));
#139795=CARTESIAN_POINT('Ctrl Pts',(106.896778178434,13.0399979246535,67.8493611719163));
#139796=CARTESIAN_POINT('Ctrl Pts',(106.881919084311,13.043408582267,67.8460359447363));
#139797=CARTESIAN_POINT('Ctrl Pts',(106.864662306634,13.047369588213,67.8421741543944));
#139798=CARTESIAN_POINT('Ctrl Pts',(106.848566718302,13.0510684622532,67.8385464484074));
#139799=CARTESIAN_POINT('Ctrl Pts',(106.833626578492,13.0545108729687,67.8351517377061));
#139800=CARTESIAN_POINT('Ctrl Pts',(106.819724341824,13.0577141367323,67.8319928601997));
#139801=CARTESIAN_POINT('Ctrl Pts',(106.806822543637,13.06069531364,67.8290357206569));
#139802=CARTESIAN_POINT('Ctrl Pts',(106.794915963268,13.0634580977053,67.8262793282536));
#139803=CARTESIAN_POINT('Ctrl Pts',(106.788962673084,13.0648394897379,67.8249011320519));
#139804=CARTESIAN_POINT('Ctrl Pts',(106.783258186263,13.0661662732176,67.8235731169913));
#139805=CARTESIAN_POINT('Ctrl Pts',(106.777801832488,13.0674388372552,67.8222951621539));
#139806=CARTESIAN_POINT('Ctrl Pts',(106.7750736556,13.068075119274,67.8216561847352));
#139807=CARTESIAN_POINT('Ctrl Pts',(106.772407511919,13.0686978459035,67.8210297220832));
#139808=CARTESIAN_POINT('Ctrl Pts',(106.769803319567,13.0693070619732,67.8204157585113));
#139809=CARTESIAN_POINT('Ctrl Pts',(106.767199127215,13.069916278043,67.8198017949394));
#139810=CARTESIAN_POINT('Ctrl Pts',(106.765788256114,13.0702464080975,67.8194689818855));
#139811=CARTESIAN_POINT('Ctrl Pts',(106.762176514847,13.0710942211172,67.8186113489208));
#139812=CARTESIAN_POINT('Ctrl Pts',(106.755061254481,13.0727644432987,67.816921781094));
#139813=CARTESIAN_POINT('Ctrl Pts',(106.747578771434,13.0745366460299,67.8151138078794));
#139814=CARTESIAN_POINT('Ctrl Pts',(106.739731130454,13.0764100827743,67.8131877287666));
#139815=CARTESIAN_POINT('Ctrl Pts',(106.721835157183,13.0806823187216,67.8087954457347));
#139816=CARTESIAN_POINT('Ctrl Pts',(106.702043963982,13.0854801299258,67.8037897445064));
#139817=CARTESIAN_POINT('Ctrl Pts',(106.680330865469,13.0908060953199,67.7981637067688));
#139818=CARTESIAN_POINT('Ctrl Pts',(106.672900165201,13.0926287579148,67.7962383528126));
#139819=CARTESIAN_POINT('Ctrl Pts',(106.665243984317,13.0945133706204,67.7942402645645));
#139820=CARTESIAN_POINT('Ctrl Pts',(106.657359828321,13.0964603835544,67.7921688682916));
#139821=CARTESIAN_POINT('Ctrl Pts',(106.64710361838,13.0989931814114,67.7894742647021));
#139822=CARTESIAN_POINT('Ctrl Pts',(106.637434211784,13.1013940754706,67.7869072339959));
#139823=CARTESIAN_POINT('Ctrl Pts',(106.623515944922,13.1048499015932,67.7832060106365));
#139824=CARTESIAN_POINT('Ctrl Pts',(106.616286187049,13.1066450091568,67.7812834329918));
#139825=CARTESIAN_POINT('Ctrl Pts',(106.609356367751,13.108364189616,67.779441852242));
#139826=CARTESIAN_POINT('Ctrl Pts',(106.602726151841,13.1100077596478,67.7776812720829));
#139827=CARTESIAN_POINT('Ctrl Pts',(106.59659230068,13.1115282853869,67.7760524960676));
#139828=CARTESIAN_POINT('Ctrl Pts',(106.590715050085,13.1129840540664,67.7744930809063));
#139829=CARTESIAN_POINT('Ctrl Pts',(106.585097803888,13.1143743934587,67.7730037378273));
#139830=CARTESIAN_POINT('Ctrl Pts',(106.569098466814,13.1183344314928,67.7687617122677));
#139831=CARTESIAN_POINT('Ctrl Pts',(106.555212866438,13.1217626845447,67.7650890351599));
#139832=CARTESIAN_POINT('Ctrl Pts',(106.543469016872,13.1246550059365,67.7619920879952));
#139833=CARTESIAN_POINT('Ctrl Pts',(106.538052846431,13.1259889216633,67.7605638004819));
#139834=CARTESIAN_POINT('Ctrl Pts',(106.533091358535,13.1272090379781,67.7592577974129));
#139835=CARTESIAN_POINT('Ctrl Pts',(106.528584066935,13.128315652714,67.7580740539427));
#139836=CARTESIAN_POINT('Ctrl Pts',(106.521443854595,13.1300686930967,67.756198830309));
#139837=CARTESIAN_POINT('Ctrl Pts',(106.515443483395,13.1315369037267,67.7546304291683));
#139838=CARTESIAN_POINT('Ctrl Pts',(106.510576637615,13.132722318494,67.7533678281773));
#139839=CARTESIAN_POINT('Ctrl Pts',(106.508143214724,13.1333150258776,67.7527365276818));
#139840=CARTESIAN_POINT('Ctrl Pts',(106.505993172956,13.133837032103,67.7521816760642));
#139841=CARTESIAN_POINT('Ctrl Pts',(106.504125557165,13.1342886081154,67.7517031047385));
#139842=CARTESIAN_POINT('Ctrl Pts',(106.502257941373,13.1347401841277,67.7512245334127));
#139843=CARTESIAN_POINT('Ctrl Pts',(106.49588082428,13.1362765541258,67.7496003744427));
#139844=CARTESIAN_POINT('Ctrl Pts',(106.490817428601,13.1374893006029,67.7483228513659));
#139845=CARTESIAN_POINT('Ctrl Pts',(106.48119359659,13.1397943285143,67.7458947046714));
#139846=CARTESIAN_POINT('Ctrl Pts',(106.471701611211,13.1420471000255,67.7435349913479));
#139847=CARTESIAN_POINT('Ctrl Pts',(106.462350082912,13.1442457702362,67.7412455172647));
#139848=CARTESIAN_POINT('Ctrl Pts',(106.452021098116,13.14667425363,67.7387167388404));
#139849=CARTESIAN_POINT('Ctrl Pts',(106.441862393324,13.1490369570712,67.7362734421338));
#139850=CARTESIAN_POINT('Ctrl Pts',(106.431801048307,13.1513488950868,67.7339015993084));
#139851=CARTESIAN_POINT('Ctrl Pts',(106.416822847289,13.1547906488759,67.730370665963));
#139852=CARTESIAN_POINT('Ctrl Pts',(106.402058175558,13.15812035499,67.7269976603332));
#139853=CARTESIAN_POINT('Ctrl Pts',(106.387310281136,13.1613785817389,67.7237446851911));
#139854=CARTESIAN_POINT('Ctrl Pts',(106.383182383448,13.1622905510192,67.722834185822));
#139855=CARTESIAN_POINT('Ctrl Pts',(106.379056104298,13.1631968581735,67.7219331480982));
#139856=CARTESIAN_POINT('Ctrl Pts',(106.374927825296,13.1640982503239,67.7210408740254));
#139857=CARTESIAN_POINT('Ctrl Pts',(106.372078037868,13.1647204892804,67.7204249293584));
#139858=CARTESIAN_POINT('Ctrl Pts',(106.369600961509,13.1652606190883,67.7198905614545));
#139859=CARTESIAN_POINT('Ctrl Pts',(106.366447297663,13.1659433443158,67.7192190674479));
#139860=CARTESIAN_POINT('Ctrl Pts',(106.364378343724,13.1663912446366,67.7187785353438));
#139861=CARTESIAN_POINT('Ctrl Pts',(106.362017963058,13.1669005568351,67.718278940623));
#139862=CARTESIAN_POINT('Ctrl Pts',(106.359057790106,13.1675369937063,67.7176561793993));
#139863=CARTESIAN_POINT('Ctrl Pts',(106.351585486534,13.1691435381826,67.716084156078));
#139864=CARTESIAN_POINT('Ctrl Pts',(106.344551231825,13.1706374186641,67.714636281189));
#139865=CARTESIAN_POINT('Ctrl Pts',(106.337977136572,13.172014705402,67.7133168711505));
#139866=CARTESIAN_POINT('Ctrl Pts',(106.331084534732,13.1734587199378,67.7119335373667));
#139867=CARTESIAN_POINT('Ctrl Pts',(106.324698195333,13.1747744827679,67.7106915025314));
#139868=CARTESIAN_POINT('Ctrl Pts',(106.318853271182,13.1759554068276,67.7095975998564));
#139869=CARTESIAN_POINT('Ctrl Pts',(106.313548534001,13.1770271900716,67.7086047954943));
#139870=CARTESIAN_POINT('Ctrl Pts',(106.308691606398,13.1779874404298,67.7077343662016));
#139871=CARTESIAN_POINT('Ctrl Pts',(106.304319984305,13.1788283115832,67.7069935851384));
#139872=CARTESIAN_POINT('Ctrl Pts',(106.300005982892,13.1796580995351,67.7062625680274));
#139873=CARTESIAN_POINT('Ctrl Pts',(106.296642203784,13.1802964496147,67.7057071864585));
#139874=CARTESIAN_POINT('Ctrl Pts',(106.293337987742,13.180883497628,67.7052366830344));
#139875=CARTESIAN_POINT('Ctrl Pts',(106.289604539133,13.1815468058258,67.7047050590935));
#139876=CARTESIAN_POINT('Ctrl Pts',(106.285946224121,13.1821450426698,67.7042816525951));
#139877=CARTESIAN_POINT('Ctrl Pts',(106.281022253892,13.1828882466645,67.7038243463946));
#139878=CARTESIAN_POINT('Ctrl Pts',(106.271740419626,13.1842892088927,67.70296231024));
#139879=CARTESIAN_POINT('Ctrl Pts',(106.261586075307,13.1856188361054,67.7023892838068));
#139880=CARTESIAN_POINT('Ctrl Pts',(106.250595879928,13.1868548838305,67.7021085788158));
#139881=CARTESIAN_POINT('Ctrl Pts',(106.24031401124,13.1880112673127,67.7018459654812));
#139882=CARTESIAN_POINT('Ctrl Pts',(106.229300211162,13.1890858286411,67.701839117714));
#139883=CARTESIAN_POINT('Ctrl Pts',(106.217628154117,13.1900446528357,67.7020972302163));
#139884=CARTESIAN_POINT('Ctrl Pts',(106.216824056165,13.1901107070511,67.7021150118065));
#139885=CARTESIAN_POINT('Ctrl Pts',(106.216016853597,13.1901762051296,67.7021340538944));
#139886=CARTESIAN_POINT('Ctrl Pts',(106.215206579378,13.1902411328607,67.7021543608706));
#139887=CARTESIAN_POINT('Ctrl Pts',(106.205123047467,13.1910491319709,67.7024070729002));
#139888=CARTESIAN_POINT('Ctrl Pts',(106.196684534129,13.1916384135438,67.7027328843449));
#139889=CARTESIAN_POINT('Ctrl Pts',(106.188340648465,13.1921930927188,67.7030670039973));
#139890=CARTESIAN_POINT('Ctrl Pts',(106.186281512678,13.1923299785518,67.7031494593138));
#139891=CARTESIAN_POINT('Ctrl Pts',(106.184228288793,13.1924645903933,67.703232430564));
#139892=CARTESIAN_POINT('Ctrl Pts',(106.182158194736,13.1925993098119,67.703315008817));
#139893=CARTESIAN_POINT('Ctrl Pts',(106.175310982203,13.1930449187873,67.7035881514053));
#139894=CARTESIAN_POINT('Ctrl Pts',(106.168503036321,13.1934317655783,67.7039321299558));
#139895=CARTESIAN_POINT('Ctrl Pts',(106.161795839839,13.1937842631555,67.7042881765257));
#139896=CARTESIAN_POINT('Ctrl Pts',(106.148013987272,13.1945085701969,67.7050197759869));
#139897=CARTESIAN_POINT('Ctrl Pts',(106.13465843368,13.1950869560501,67.7058015508074));
#139898=CARTESIAN_POINT('Ctrl Pts',(106.122049394182,13.1958248934581,67.706094333502));
#139899=CARTESIAN_POINT('Ctrl Pts',(106.112676661907,13.1963734276872,67.7063119689382));
#139900=CARTESIAN_POINT('Ctrl Pts',(106.103735822729,13.1970865540103,67.7061195139772));
#139901=CARTESIAN_POINT('Ctrl Pts',(106.095200154032,13.1979828221813,67.7055165398966));
#139902=CARTESIAN_POINT('Ctrl Pts',(106.090932319683,13.1984309562668,67.7052150528563));
#139903=CARTESIAN_POINT('Ctrl Pts',(106.086765773032,13.1989248004721,67.7048108946205));
#139904=CARTESIAN_POINT('Ctrl Pts',(106.082697785093,13.1994661513858,67.7043038387365));
#139905=CARTESIAN_POINT('Ctrl Pts',(106.079433660559,13.1999005275013,67.7038969807084));
#139906=CARTESIAN_POINT('Ctrl Pts',(106.075433665888,13.2004973756032,67.7032766697359));
#139907=CARTESIAN_POINT('Ctrl Pts',(106.072621105963,13.2009398356224,67.7027971657393));
#139908=CARTESIAN_POINT('Ctrl Pts',(106.071928450406,13.201048801262,67.7026790771948));
#139909=CARTESIAN_POINT('Ctrl Pts',(106.071307549541,13.2011484789228,67.702569477134));
#139910=CARTESIAN_POINT('Ctrl Pts',(106.070786735959,13.2012342432933,67.7024735795054));
#139911=CARTESIAN_POINT('Ctrl Pts',(106.062743425631,13.2025587660585,67.7009925613209));
#139912=CARTESIAN_POINT('Ctrl Pts',(106.052634650792,13.2044505865399,67.698700221847));
#139913=CARTESIAN_POINT('Ctrl Pts',(106.040575469081,13.2068972755518,67.6956180730002));
#139914=CARTESIAN_POINT('Ctrl Pts',(106.034052331577,13.2082207558042,67.6939508553383));
#139915=CARTESIAN_POINT('Ctrl Pts',(106.026958761435,13.2097069844791,67.6920525515875));
#139916=CARTESIAN_POINT('Ctrl Pts',(106.019310196946,13.2113605995131,67.6899257675537));
#139917=CARTESIAN_POINT('Ctrl Pts',(106.007982879047,13.2138095588178,67.6867760577111));
#139918=CARTESIAN_POINT('Ctrl Pts',(105.995440848126,13.2166267903083,67.6831257606122));
#139919=CARTESIAN_POINT('Ctrl Pts',(105.981708195429,13.2198130341267,67.6789775432847));
#139920=CARTESIAN_POINT('Ctrl Pts',(105.976918915918,13.2209242405757,67.6775308473918));
#139921=CARTESIAN_POINT('Ctrl Pts',(105.971984418664,13.2220803488126,67.6760235041644));
#139922=CARTESIAN_POINT('Ctrl Pts',(105.966904141517,13.2232814677876,67.6744552939442));
#139923=CARTESIAN_POINT('Ctrl Pts',(105.960175911557,13.2248722086941,67.6723783838305));
#139924=CARTESIAN_POINT('Ctrl Pts',(105.952029538102,13.2268285903403,67.6698157172125));
#139925=CARTESIAN_POINT('Ctrl Pts',(105.945397850862,13.228429470037,67.6677187219855));
#139926=CARTESIAN_POINT('Ctrl Pts',(105.940283703307,13.229664017851,67.666101585558));
#139927=CARTESIAN_POINT('Ctrl Pts',(105.936067560064,13.2306871257169,67.664760947505));
#139928=CARTESIAN_POINT('Ctrl Pts',(105.934085177048,13.231167367077,67.6641321742009));
#139929=CARTESIAN_POINT('Ctrl Pts',(105.929532171261,13.2322703535704,67.6626880493931));
#139930=CARTESIAN_POINT('Ctrl Pts',(105.924436613309,13.2334938104782,67.661093619133));
#139931=CARTESIAN_POINT('Ctrl Pts',(105.918796795571,13.2348382984781,67.6593483847178));
#139932=CARTESIAN_POINT('Ctrl Pts',(105.909551022734,13.23704241769,67.6564872920905));
#139933=CARTESIAN_POINT('Ctrl Pts',(105.898845834699,13.2395716061723,67.6532215584016));
#139934=CARTESIAN_POINT('Ctrl Pts',(105.886639951472,13.2424306572284,67.649542283528));
#139935=CARTESIAN_POINT('Ctrl Pts',(105.872690840467,13.2456980341,67.6453375395795));
#139936=CARTESIAN_POINT('Ctrl Pts',(105.856771681814,13.2493967029723,67.6405907412848));
#139937=CARTESIAN_POINT('Ctrl Pts',(105.838891079168,13.2535316119723,67.6353019750921));
#139938=CARTESIAN_POINT('Ctrl Pts',(105.823539175591,13.2570817565354,67.630761153385));
#139939=CARTESIAN_POINT('Ctrl Pts',(105.806740930001,13.2609535270673,67.6258207238569));
#139940=CARTESIAN_POINT('Ctrl Pts',(105.788540076225,13.2651488956576,67.6204880111972));
#139941=CARTESIAN_POINT('Ctrl Pts',(105.778599083373,13.267440333723,67.6175753753901));
#139942=CARTESIAN_POINT('Ctrl Pts',(105.768240401289,13.269828281464,67.6145458546616));
#139943=CARTESIAN_POINT('Ctrl Pts',(105.757477831466,13.2723128046513,67.6114019202545));
#139944=CARTESIAN_POINT('Ctrl Pts',(105.756521354661,13.2725336058947,67.6111225166934));
#139945=CARTESIAN_POINT('Ctrl Pts',(105.755569399813,13.2727533590239,67.6108445215215));
#139946=CARTESIAN_POINT('Ctrl Pts',(105.754621927495,13.2729720724131,67.610567924591));
#139947=CARTESIAN_POINT('Ctrl Pts',(105.738323688053,13.2767343387243,67.6058099565607));
#139948=CARTESIAN_POINT('Ctrl Pts',(105.723346557623,13.2801893902145,67.6014647422791));
#139949=CARTESIAN_POINT('Ctrl Pts',(105.709403813386,13.2833878795956,67.5974636595106));
#139950=CARTESIAN_POINT('Ctrl Pts',(105.6926733995,13.2872258651633,67.5926626124879));
#139951=CARTESIAN_POINT('Ctrl Pts',(105.677434081816,13.2906942185066,67.5883574104592));
#139952=CARTESIAN_POINT('Ctrl Pts',(105.663267608136,13.293874588328,67.584443733116));
#139953=CARTESIAN_POINT('Ctrl Pts',(105.654765750246,13.295783253312,67.582094981454));
#139954=CARTESIAN_POINT('Ctrl Pts',(105.646651510083,13.2975881134783,67.5798874653339));
#139955=CARTESIAN_POINT('Ctrl Pts',(105.638840450611,13.2993065510575,67.5777996826804));
#139956=CARTESIAN_POINT('Ctrl Pts',(105.630171984851,13.3012136185134,67.5754827277899));
#139957=CARTESIAN_POINT('Ctrl Pts',(105.621973986663,13.302993911731,67.5733372110151));
#139958=CARTESIAN_POINT('Ctrl Pts',(105.614251444181,13.3046459269888,67.5713643636819));
#139959=CARTESIAN_POINT('Ctrl Pts',(105.60758463171,13.3060720992562,67.5696612195124));
#139960=CARTESIAN_POINT('Ctrl Pts',(105.601272756613,13.3074025696676,67.5680868753423));
#139961=CARTESIAN_POINT('Ctrl Pts',(105.595327344932,13.308635035678,67.5666436941515));
#139962=CARTESIAN_POINT('Ctrl Pts',(105.588366685201,13.3100779595644,67.5649540730222));
#139963=CARTESIAN_POINT('Ctrl Pts',(105.579139427266,13.3119575615898,67.5627781036788));
#139964=CARTESIAN_POINT('Ctrl Pts',(105.568996708876,13.3139954644155,67.5604370755091));
#139965=CARTESIAN_POINT('Ctrl Pts',(105.560440831955,13.3157145346964,67.558462304238));
#139966=CARTESIAN_POINT('Ctrl Pts',(105.551234493553,13.3175459511269,67.5563702709175));
#139967=CARTESIAN_POINT('Ctrl Pts',(105.542217628589,13.3193176560284,67.5543595389247));
#139968=CARTESIAN_POINT('Ctrl Pts',(105.52456366563,13.3227864462153,67.5504227617565));
#139969=CARTESIAN_POINT('Ctrl Pts',(105.505715838934,13.3264175887521,67.5463440398532));
#139970=CARTESIAN_POINT('Ctrl Pts',(105.485721490407,13.3301897222825,67.54213280598));
#139971=CARTESIAN_POINT('Ctrl Pts',(105.479197662337,13.3314205076005,67.5407587494202));
#139972=CARTESIAN_POINT('Ctrl Pts',(105.47255214769,13.3326661856339,67.5393706573031));
#139973=CARTESIAN_POINT('Ctrl Pts',(105.465787761714,13.3339256480176,67.5379690826581));
#139974=CARTESIAN_POINT('Ctrl Pts',(105.447000822801,13.3374235919477,67.5340764459385));
#139975=CARTESIAN_POINT('Ctrl Pts',(105.427296437372,13.3410278363802,67.5300797135526));
#139976=CARTESIAN_POINT('Ctrl Pts',(105.406695522736,13.3447315623451,67.5259830318283));
#139977=CARTESIAN_POINT('Ctrl Pts',(105.406714415269,13.34497198119,67.526105385012));
#139978=CARTESIAN_POINT('Ctrl Pts',(105.724920227002,13.896301628367,66.3930340896861));
#139979=CARTESIAN_POINT('Ctrl Pts',(105.782792744022,13.149274277058,65.4129414870055));
#139980=CARTESIAN_POINT('Ctrl Pts',(105.588267881069,12.0114366406,65.374894609145));
#139981=CARTESIAN_POINT('Ctrl Pts',(105.479711788869,13.16446974828,67.8027942772491));
#139982=CARTESIAN_POINT('Ctrl Pts',(105.404457854469,13.17797674511,67.7881663212369));
#139983=CARTESIAN_POINT('Ctrl Pts',(105.217622405069,13.21120999594,67.751849007578));
#139984=CARTESIAN_POINT('Ctrl Pts',(104.909728623269,13.26478499412,67.692000220443));
#139985=CARTESIAN_POINT('Ctrl Pts',(104.545556898969,13.32647740523,67.62121205483));
#139986=CARTESIAN_POINT('Ctrl Pts',(104.149966793169,13.3916066705,67.544316744054));
#139987=CARTESIAN_POINT('Ctrl Pts',(103.719952703269,13.46028345385,67.460730055209));
#139988=CARTESIAN_POINT('Ctrl Pts',(103.252302141369,13.53257321139,67.369827540788));
#139989=CARTESIAN_POINT('Ctrl Pts',(102.743743443769,13.60837809399,67.270973250634));
#139990=CARTESIAN_POINT('Ctrl Pts',(102.190923130269,13.68750427689,67.163515330951));
#139991=CARTESIAN_POINT('Ctrl Pts',(101.590499923169,13.76962735539,67.046804299923));
#139992=CARTESIAN_POINT('Ctrl Pts',(100.939068251569,13.85431465257,66.920178178317));
#139993=CARTESIAN_POINT('Ctrl Pts',(100.232496010669,13.94110230146,66.782833762325));
#139994=CARTESIAN_POINT('Ctrl Pts',(99.4656780020691,14.02948909557,66.633778696936));
#139995=CARTESIAN_POINT('Ctrl Pts',(98.7641160173691,14.10476175395,66.49740818094));
#139996=CARTESIAN_POINT('Ctrl Pts',(98.3174346082691,14.14979091774,66.410581677263));
#139997=CARTESIAN_POINT('Ctrl Pts',(98.147852524169,14.16647603684,66.37761809484));
#139998=CARTESIAN_POINT('Ctrl Pts',(105.898861939469,14.14039115007,66.547598800864));
#139999=CARTESIAN_POINT('Ctrl Pts',(105.822628287069,14.15407399291,66.532780405995));
#140000=CARTESIAN_POINT('Ctrl Pts',(105.633399482669,14.18773289908,66.4959978689441));
#140001=CARTESIAN_POINT('Ctrl Pts',(105.321708482069,14.24196843757,66.4354109735431));
#140002=CARTESIAN_POINT('Ctrl Pts',(104.953242302369,14.30438814198,66.363788046205));
#140003=CARTESIAN_POINT('Ctrl Pts',(104.553186949569,14.37025226255,66.286024775006));
#140004=CARTESIAN_POINT('Ctrl Pts',(104.118570678569,14.43966385608,66.201543508307));
#140005=CARTESIAN_POINT('Ctrl Pts',(103.646007691069,14.51271290559,66.109686110311));
#140006=CARTESIAN_POINT('Ctrl Pts',(103.132149783669,14.5893076241,66.009801752982));
#140007=CARTESIAN_POINT('Ctrl Pts',(102.573627663069,14.66924981062,65.901235508739));
#140008=CARTESIAN_POINT('Ctrl Pts',(101.967092525769,14.7522086941,65.7833364328971));
#140009=CARTESIAN_POINT('Ctrl Pts',(101.309152996869,14.83774177889,65.655445305682));
#140010=CARTESIAN_POINT('Ctrl Pts',(100.595686651869,14.92537590466,65.516760804898));
#140011=CARTESIAN_POINT('Ctrl Pts',(99.8215835246691,15.01460202113,65.366289648841));
#140012=CARTESIAN_POINT('Ctrl Pts',(99.1135435814691,15.09056933134,65.228659939006));
#140013=CARTESIAN_POINT('Ctrl Pts',(98.6628310930692,15.13600478504,65.1410498689811));
#140014=CARTESIAN_POINT('Ctrl Pts',(98.4917311527691,15.15283924478,65.107791243718));
#140015=CARTESIAN_POINT('Ctrl Pts',(106.014802693469,13.27644852387,65.1534015425141));
#140016=CARTESIAN_POINT('Ctrl Pts',(105.939436344769,13.28997569756,65.1387517352451));
#140017=CARTESIAN_POINT('Ctrl Pts',(105.752326277969,13.32325778875,65.102381041112));
#140018=CARTESIAN_POINT('Ctrl Pts',(105.443996797269,13.37690857839,65.04244756226));
#140019=CARTESIAN_POINT('Ctrl Pts',(105.079332320269,13.43868444028,64.971563614758));
#140020=CARTESIAN_POINT('Ctrl Pts',(104.683229864969,13.50389802402,64.89456871282));
#140021=CARTESIAN_POINT('Ctrl Pts',(104.252687713469,13.57265912066,64.810879378689));
#140022=CARTESIAN_POINT('Ctrl Pts',(103.784473491969,13.64503600057,64.719867299405));
#140023=CARTESIAN_POINT('Ctrl Pts',(103.275306754669,13.7209315102,64.6208948177041));
#140024=CARTESIAN_POINT('Ctrl Pts',(102.721832206769,13.80015132265,64.513309727095));
#140025=CARTESIAN_POINT('Ctrl Pts',(102.120707706969,13.88237030275,64.3964623779141));
#140026=CARTESIAN_POINT('Ctrl Pts',(101.468529313469,13.96715464695,64.26969110755));
#140027=CARTESIAN_POINT('Ctrl Pts',(100.761166032169,14.05403942194,64.132192928096));
#140028=CARTESIAN_POINT('Ctrl Pts',(99.9935121174691,14.14252252124,63.9829753782081));
#140029=CARTESIAN_POINT('Ctrl Pts',(99.2912068414691,14.21787488508,63.8464603803061));
#140030=CARTESIAN_POINT('Ctrl Pts',(98.8440628998692,14.26295066722,63.759543968979));
#140031=CARTESIAN_POINT('Ctrl Pts',(98.6743066545691,14.2796529219,63.726546532871));
#140032=CARTESIAN_POINT('Ctrl Pts',(105.677598220969,11.68990176436,65.423193389316));
#140033=CARTESIAN_POINT('Ctrl Pts',(105.603824591269,11.70314306676,65.408853176808));
#140034=CARTESIAN_POINT('Ctrl Pts',(105.420605380269,11.73573317384,65.373238792213));
#140035=CARTESIAN_POINT('Ctrl Pts',(105.118449004669,11.78831012897,65.314505249415));
#140036=CARTESIAN_POINT('Ctrl Pts',(104.760765985569,11.84890363658,65.244978366641));
#140037=CARTESIAN_POINT('Ctrl Pts',(104.371922642669,11.91292257259,65.169394500257));
#140038=CARTESIAN_POINT('Ctrl Pts',(103.948862216169,11.98048909485,65.087159473402));
#140039=CARTESIAN_POINT('Ctrl Pts',(103.488634081469,12.05163160054,64.997699739869));
#140040=CARTESIAN_POINT('Ctrl Pts',(102.988082222469,12.12624308094,64.90040182923));
#140041=CARTESIAN_POINT('Ctrl Pts',(102.443877051669,12.20413632354,64.79461853202));
#140042=CARTESIAN_POINT('Ctrl Pts',(101.852688662669,12.28499654291,64.679702576745));
#140043=CARTESIAN_POINT('Ctrl Pts',(101.211090034869,12.36840589771,64.554987814772));
#140044=CARTESIAN_POINT('Ctrl Pts',(100.514934437469,12.45391456276,64.419668199267));
#140045=CARTESIAN_POINT('Ctrl Pts',(99.7591238753691,12.54103318314,64.272752775408));
#140046=CARTESIAN_POINT('Ctrl Pts',(99.0673497588691,12.61525625766,64.138284837753));
#140047=CARTESIAN_POINT('Ctrl Pts',(98.6267591070691,12.6596715379,64.052642263281));
#140048=CARTESIAN_POINT('Ctrl Pts',(98.4594704271691,12.67613101083,64.0201244757));
#140049=CARTESIAN_POINT('',(98.4192401217934,14.401804164717,65.9071352125797));
#140050=CARTESIAN_POINT('Ctrl Pts',(105.406733283589,13.3452126550092,67.5262279087238));
#140051=CARTESIAN_POINT('Ctrl Pts',(105.381157881525,13.3502102353128,67.5203514165497));
#140052=CARTESIAN_POINT('Ctrl Pts',(105.355581691314,13.3551935844434,67.5144734853879));
#140053=CARTESIAN_POINT('Ctrl Pts',(105.330004713402,13.3601628548922,67.5085941118163));
#140054=CARTESIAN_POINT('Ctrl Pts',(105.219236633267,13.3816836361654,67.4831318806979));
#140055=CARTESIAN_POINT('Ctrl Pts',(105.108453784641,13.4029403629768,67.4576425972809));
#140056=CARTESIAN_POINT('Ctrl Pts',(104.997656804334,13.4239440458079,67.4321261008341));
#140057=CARTESIAN_POINT('Ctrl Pts',(104.8775148326,13.4467192501681,67.4044574569204));
#140058=CARTESIAN_POINT('Ctrl Pts',(104.75735624808,13.4691969250606,67.3767568164943));
#140059=CARTESIAN_POINT('Ctrl Pts',(104.637180377502,13.4913896737591,67.3490236875475));
#140060=CARTESIAN_POINT('Ctrl Pts',(104.506635316763,13.5154972896464,67.3188976482232));
#140061=CARTESIAN_POINT('Ctrl Pts',(104.376069842465,13.5392686921611,67.2887332689063));
#140062=CARTESIAN_POINT('Ctrl Pts',(104.245490553519,13.5627177176572,67.2585313722496));
#140063=CARTESIAN_POINT('Ctrl Pts',(104.199920013792,13.570901134465,67.2479912878111));
#140064=CARTESIAN_POINT('Ctrl Pts',(104.15434779278,13.5790452879071,67.23744663432));
#140065=CARTESIAN_POINT('Ctrl Pts',(104.108773106829,13.587150789758,67.2268972399986));
#140066=CARTESIAN_POINT('Ctrl Pts',(104.012396744216,13.604291418799,67.2045885343815));
#140067=CARTESIAN_POINT('Ctrl Pts',(103.916009401996,13.6212591286287,67.1822587779171));
#140068=CARTESIAN_POINT('Ctrl Pts',(103.819603561869,13.6380596778537,67.1599064253125));
#140069=CARTESIAN_POINT('Ctrl Pts',(103.69951747087,13.6589869606865,67.1320636447776));
#140070=CARTESIAN_POINT('Ctrl Pts',(103.579402664645,13.6796548805289,67.1041858011181));
#140071=CARTESIAN_POINT('Ctrl Pts',(103.459256116394,13.7000647957269,67.0762721529889));
#140072=CARTESIAN_POINT('Ctrl Pts',(103.424986105314,13.7058864196534,67.0683102011509));
#140073=CARTESIAN_POINT('Ctrl Pts',(103.3907135111,13.7116870525938,67.0603453362345));
#140074=CARTESIAN_POINT('Ctrl Pts',(103.356438263105,13.7174667259815,67.0523775410846));
#140075=CARTESIAN_POINT('Ctrl Pts',(103.282396499432,13.7299520393233,67.035165423303));
#140076=CARTESIAN_POINT('Ctrl Pts',(103.208342351437,13.7423395448488,67.0179396313692));
#140077=CARTESIAN_POINT('Ctrl Pts',(103.134276238954,13.7546294882771,67.0007002135295));
#140078=CARTESIAN_POINT('Ctrl Pts',(103.080099922966,13.7636190765831,66.9880902881936));
#140079=CARTESIAN_POINT('Ctrl Pts',(103.025917145159,13.7725564742551,66.9754730625563));
#140080=CARTESIAN_POINT('Ctrl Pts',(102.971728141044,13.7814417670877,66.9628485678601));
#140081=CARTESIAN_POINT('Ctrl Pts',(102.944633638987,13.785884413504,66.956536320512));
#140082=CARTESIAN_POINT('Ctrl Pts',(102.917537580353,13.790314033716,66.9502222559043));
#140083=CARTESIAN_POINT('Ctrl Pts',(102.890439979525,13.7947306404591,66.9439063755002));
#140084=CARTESIAN_POINT('Ctrl Pts',(102.877853347631,13.7967821210921,66.9409726965283));
#140085=CARTESIAN_POINT('Ctrl Pts',(102.865266383003,13.798830794026,66.9380386257926));
#140086=CARTESIAN_POINT('Ctrl Pts',(102.852679087662,13.8008766604567,66.9351041635364));
#140087=CARTESIAN_POINT('Ctrl Pts',(102.851716868426,13.801033054025,66.934879842429));
#140088=CARTESIAN_POINT('Ctrl Pts',(102.850754647258,13.8011894311932,66.9346555190337));
#140089=CARTESIAN_POINT('Ctrl Pts',(102.849792424158,13.8013457919615,66.9344311933506));
#140090=CARTESIAN_POINT('Ctrl Pts',(102.836242855166,13.8035475900876,66.9312723455542));
#140091=CARTESIAN_POINT('Ctrl Pts',(102.821186091383,13.8059902555839,66.9277616759329));
#140092=CARTESIAN_POINT('Ctrl Pts',(102.809142570649,13.8079414318969,66.9249532893378));
#140093=CARTESIAN_POINT('Ctrl Pts',(102.707658542477,13.8243829058051,66.9012885827612));
#140094=CARTESIAN_POINT('Ctrl Pts',(102.590169504002,13.8431985272868,66.8739607615462));
#140095=CARTESIAN_POINT('Ctrl Pts',(102.456651461361,13.8641900914516,66.84295154119));
#140096=CARTESIAN_POINT('Ctrl Pts',(102.40815704942,13.8718143311405,66.8316888393396));
#140097=CARTESIAN_POINT('Ctrl Pts',(102.357548086328,13.8797251196032,66.8199404576736));
#140098=CARTESIAN_POINT('Ctrl Pts',(102.304823305587,13.8879112722829,66.807705396231));
#140099=CARTESIAN_POINT('Ctrl Pts',(102.156756066627,13.9109004816824,66.7733456181368));
#140100=CARTESIAN_POINT('Ctrl Pts',(101.992002262485,13.9360651677371,66.7351478329039));
#140101=CARTESIAN_POINT('Ctrl Pts',(101.810533783638,13.9631224600473,66.693087689397));
#140102=CARTESIAN_POINT('Ctrl Pts',(101.777387409099,13.9680646469805,66.6854051360481));
#140103=CARTESIAN_POINT('Ctrl Pts',(101.743683378144,13.973069837667,66.6775937132222));
#140104=CARTESIAN_POINT('Ctrl Pts',(101.709421523332,13.978136122441,66.6696532620346));
#140105=CARTESIAN_POINT('Ctrl Pts',(101.658173465491,13.9857141492748,66.6577761262525));
#140106=CARTESIAN_POINT('Ctrl Pts',(101.605677362654,13.993428876382,66.645610310142));
#140107=CARTESIAN_POINT('Ctrl Pts',(101.551932634488,14.0012737256221,66.633155264118));
#140108=CARTESIAN_POINT('Ctrl Pts',(101.460383484212,14.0146366973312,66.6119392505836));
#140109=CARTESIAN_POINT('Ctrl Pts',(101.365211319469,14.0283773475413,66.5898840144221));
#140110=CARTESIAN_POINT('Ctrl Pts',(101.266413361469,14.0424614193033,66.5669867527179));
#140111=CARTESIAN_POINT('Ctrl Pts',(101.217014382469,14.0495034551843,66.5555381218657));
#140112=CARTESIAN_POINT('Ctrl Pts',(101.166708953445,14.0566313162386,66.5438789734973));
#140113=CARTESIAN_POINT('Ctrl Pts',(101.115496747552,14.0638405167275,66.5320089592876));
#140114=CARTESIAN_POINT('Ctrl Pts',(101.098208266896,14.0662742358189,66.5280018186564));
#140115=CARTESIAN_POINT('Ctrl Pts',(101.080816446376,14.068717223697,66.5239706465975));
#140116=CARTESIAN_POINT('Ctrl Pts',(101.063321273766,14.0711693046102,66.5199154291647));
#140117=CARTESIAN_POINT('Ctrl Pts',(101.054904210371,14.0723490197782,66.5179644325686));
#140118=CARTESIAN_POINT('Ctrl Pts',(101.046463224621,14.0735308396377,66.5160078703168));
#140119=CARTESIAN_POINT('Ctrl Pts',(101.037998315012,14.0747147445836,66.5140457408203));
#140120=CARTESIAN_POINT('Ctrl Pts',(101.011938782694,14.0783594390487,66.5080052537521));
#140121=CARTESIAN_POINT('Ctrl Pts',(100.987109945946,14.0818214043664,66.5022498544524));
#140122=CARTESIAN_POINT('Ctrl Pts',(100.959139465562,14.0857075368092,66.4957659427328));
#140123=CARTESIAN_POINT('Ctrl Pts',(100.757973610972,14.1136569013962,66.4491331490066));
#140124=CARTESIAN_POINT('Ctrl Pts',(100.559239103292,14.1405560928714,66.4030589659381));
#140125=CARTESIAN_POINT('Ctrl Pts',(100.362947071848,14.1664684645508,66.3575511814201));
#140126=CARTESIAN_POINT('Ctrl Pts',(100.105330190568,14.200476286109,66.2978260186857));
#140127=CARTESIAN_POINT('Ctrl Pts',(99.851920383257,14.2327846518942,66.239076482115));
#140128=CARTESIAN_POINT('Ctrl Pts',(99.6027376068943,14.2635287439544,66.1813184830871));
#140129=CARTESIAN_POINT('Ctrl Pts',(99.321969064362,14.298169877845,66.1162392290418));
#140130=CARTESIAN_POINT('Ctrl Pts',(99.0465670949617,14.3308252092359,66.0524188394242));
#140131=CARTESIAN_POINT('Ctrl Pts',(98.7765544539798,14.3616741416806,65.989877742702));
#140132=CARTESIAN_POINT('Ctrl Pts',(98.6563816132559,14.3754038834872,65.9620429671605));
#140133=CARTESIAN_POINT('Ctrl Pts',(98.5372762547796,14.3887756405978,65.9344615703069));
#140134=CARTESIAN_POINT('Ctrl Pts',(98.4192401229391,14.4018041902007,65.9071352198517));
#140135=CARTESIAN_POINT('Origin',(98.3551330948655,12.9603930090967,65.4969839076243));
#140136=CARTESIAN_POINT('Ctrl Pts',(98.6918699825692,14.27197610448,66.217974461185));
#140137=CARTESIAN_POINT('Ctrl Pts',(98.4405864664691,14.28636537759,66.202563237184));
#140138=CARTESIAN_POINT('Ctrl Pts',(97.8913074767691,14.33180917892,66.112649421504));
#140139=CARTESIAN_POINT('Ctrl Pts',(97.0444533364691,14.44268121769,65.764243077902));
#140140=CARTESIAN_POINT('Ctrl Pts',(96.2125088153692,14.58833219957,65.116820696336));
#140141=CARTESIAN_POINT('Ctrl Pts',(95.5548624757691,14.72994024583,64.167499731003));
#140142=CARTESIAN_POINT('Ctrl Pts',(95.218166978169,14.82374422835,63.013795844258));
#140143=CARTESIAN_POINT('Ctrl Pts',(95.2531311970691,14.84218773752,62.15671974562));
#140144=CARTESIAN_POINT('Ctrl Pts',(95.348322967069,14.83944476018,61.72939797364));
#140145=CARTESIAN_POINT('Ctrl Pts',(95.3600036087691,14.8389630281,61.68154891083));
#140146=CARTESIAN_POINT('Ctrl Pts',(98.8538498000691,14.9154835018,64.9403367841401));
#140147=CARTESIAN_POINT('Ctrl Pts',(98.7129574471692,14.92892963799,64.938434414967));
#140148=CARTESIAN_POINT('Ctrl Pts',(98.3961279961691,14.97159179509,64.9087219556159));
#140149=CARTESIAN_POINT('Ctrl Pts',(97.8612535104691,15.07891262045,64.741238167691));
#140150=CARTESIAN_POINT('Ctrl Pts',(97.2821719387691,15.22467284488,64.362639344877));
#140151=CARTESIAN_POINT('Ctrl Pts',(96.7867641037691,15.37029300066,63.735122492223));
#140152=CARTESIAN_POINT('Ctrl Pts',(96.5173669447691,15.46821211358,62.92168774703));
#140153=CARTESIAN_POINT('Ctrl Pts',(96.536945970469,15.48743521164,62.30909927009));
#140154=CARTESIAN_POINT('Ctrl Pts',(96.6048510481691,15.48457264358,62.0084034354399));
#140155=CARTESIAN_POINT('Ctrl Pts',(96.6132000082691,15.48406241972,61.97480249097));
#140156=CARTESIAN_POINT('Ctrl Pts',(98.8945644152691,14.04213367577,63.796526009201));
#140157=CARTESIAN_POINT('Ctrl Pts',(98.8227012415692,14.0568598104,63.796087997308));
#140158=CARTESIAN_POINT('Ctrl Pts',(98.6604006711691,14.10329713546,63.782568224124));
#140159=CARTESIAN_POINT('Ctrl Pts',(98.3828403562691,14.21543756603,63.699343015961));
#140160=CARTESIAN_POINT('Ctrl Pts',(98.0785794391691,14.36104952961,63.505004006583));
#140161=CARTESIAN_POINT('Ctrl Pts',(97.8158867698691,14.50122456514,63.177410967091));
#140162=CARTESIAN_POINT('Ctrl Pts',(97.6721106794691,14.59355874085,62.7493551232801));
#140163=CARTESIAN_POINT('Ctrl Pts',(97.6820951225691,14.61172380317,62.42647002956));
#140164=CARTESIAN_POINT('Ctrl Pts',(97.7178785373692,14.60902354021,62.26827135895));
#140165=CARTESIAN_POINT('Ctrl Pts',(97.7222791533691,14.60855198458,62.25059797219));
#140166=CARTESIAN_POINT('Ctrl Pts',(98.768177115269,12.63514813157,64.0742499004729));
#140167=CARTESIAN_POINT('Ctrl Pts',(98.6462677492691,12.65193637148,64.061583167723));
#140168=CARTESIAN_POINT('Ctrl Pts',(98.3866060319691,12.70445557414,64.002017605271));
#140169=CARTESIAN_POINT('Ctrl Pts',(98.0220088521691,12.82436049343,63.8115282798));
#140170=CARTESIAN_POINT('Ctrl Pts',(97.705131857869,12.96973360554,63.509444739474));
#140171=CARTESIAN_POINT('Ctrl Pts',(97.4836391437691,13.10113643407,63.122239518025));
#140172=CARTESIAN_POINT('Ctrl Pts',(97.3823820385691,13.18447315457,62.6908108836));
#140173=CARTESIAN_POINT('Ctrl Pts',(97.3993641377692,13.20093369833,62.37669544903));
#140174=CARTESIAN_POINT('Ctrl Pts',(97.4343536442692,13.19849491242,62.21644116502));
#140175=CARTESIAN_POINT('Ctrl Pts',(97.4386343186691,13.19808565216,62.19844345297));
#140176=CARTESIAN_POINT('',(97.4407949555856,13.49843642512,62.3530207360974));
#140177=CARTESIAN_POINT('Ctrl Pts',(98.6413355057991,12.96039230927,64.024540977121));
#140178=CARTESIAN_POINT('Ctrl Pts',(98.605473984333,12.9675617061125,64.0175707852277));
#140179=CARTESIAN_POINT('Ctrl Pts',(98.5683962081428,12.9757376510516,64.0090060419383));
#140180=CARTESIAN_POINT('Ctrl Pts',(98.5302868961479,12.9849201440874,63.9985400265442));
#140181=CARTESIAN_POINT('Ctrl Pts',(98.4921775841531,12.9941026371232,63.98807401115));
#140182=CARTESIAN_POINT('Ctrl Pts',(98.45303623735,13.0042916782556,63.9757060755926));
#140183=CARTESIAN_POINT('Ctrl Pts',(98.4131060346052,13.0154872674846,63.9611280617728));
#140184=CARTESIAN_POINT('Ctrl Pts',(98.376063601498,13.025873186829,63.9476043362559));
#140185=CARTESIAN_POINT('Ctrl Pts',(98.3383426214638,13.0371253307708,63.9321781167114));
#140186=CARTESIAN_POINT('Ctrl Pts',(98.3001875346592,13.0492436993101,63.914610488346));
#140187=CARTESIAN_POINT('Ctrl Pts',(98.297213024295,13.0501884282004,63.9132409437577));
#140188=CARTESIAN_POINT('Ctrl Pts',(98.2942359013327,13.0511384215843,63.9118583908725));
#140189=CARTESIAN_POINT('Ctrl Pts',(98.2912562947423,13.0520936794616,63.9104627199178));
#140190=CARTESIAN_POINT('Ctrl Pts',(98.2730008826755,13.05794634009,63.9019117425944));
#140191=CARTESIAN_POINT('Ctrl Pts',(98.254435686774,13.0640722403333,63.8927621878895));
#140192=CARTESIAN_POINT('Ctrl Pts',(98.2358838421152,13.070370855523,63.8831220800602));
#140193=CARTESIAN_POINT('Ctrl Pts',(98.2175389480234,13.0765992080511,63.8735895100968));
#140194=CARTESIAN_POINT('Ctrl Pts',(98.1992074642894,13.0829964436594,63.8635773538434));
#140195=CARTESIAN_POINT('Ctrl Pts',(98.181180023402,13.0894653644266,63.8532366540782));
#140196=CARTESIAN_POINT('Ctrl Pts',(98.1762937331504,13.0912187483196,63.8504338347112));
#140197=CARTESIAN_POINT('Ctrl Pts',(98.1714296390673,13.0929773986825,63.8476071390264));
#140198=CARTESIAN_POINT('Ctrl Pts',(98.166593201586,13.0947393800183,63.8447601481387));
#140199=CARTESIAN_POINT('Ctrl Pts',(98.1148083545813,13.1136053188947,63.8142767627726));
#140200=CARTESIAN_POINT('Ctrl Pts',(98.0648576610132,13.1327059816041,63.7806779492109));
#140201=CARTESIAN_POINT('Ctrl Pts',(98.0171010756302,13.1520413681468,63.7442058273393));
#140202=CARTESIAN_POINT('Ctrl Pts',(97.9693425234032,13.1713775510129,63.7077322033716));
#140203=CARTESIAN_POINT('Ctrl Pts',(97.9237785922256,13.1909484770466,63.6683852876198));
#140204=CARTESIAN_POINT('Ctrl Pts',(97.8807376519285,13.210754146248,63.6264486452522));
#140205=CARTESIAN_POINT('Ctrl Pts',(97.8652768701684,13.2178685616632,63.6113845395212));
#140206=CARTESIAN_POINT('Ctrl Pts',(97.8501413162752,13.2250132665962,63.5959866436732));
#140207=CARTESIAN_POINT('Ctrl Pts',(97.8353450915221,13.232188261047,63.5802693034007));
#140208=CARTESIAN_POINT('Ctrl Pts',(97.8191490387139,13.2400420609832,63.5630649909962));
#140209=CARTESIAN_POINT('Ctrl Pts',(97.8033595729907,13.2479321527512,63.5454779222972));
#140210=CARTESIAN_POINT('Ctrl Pts',(97.7879943189786,13.2558585363509,63.5275277284681));
#140211=CARTESIAN_POINT('Ctrl Pts',(97.7807787322864,13.2595807987993,63.5190982433705));
#140212=CARTESIAN_POINT('Ctrl Pts',(97.7739289245749,13.2631676096328,63.5109134644787));
#140213=CARTESIAN_POINT('Ctrl Pts',(97.7670570401342,13.266821070005,63.5025229127333));
#140214=CARTESIAN_POINT('Ctrl Pts',(97.7603420894826,13.2703910960028,63.4943239767068));
#140215=CARTESIAN_POINT('Ctrl Pts',(97.7536059018193,13.2740247621372,63.485928455883));
#140216=CARTESIAN_POINT('Ctrl Pts',(97.74652470328,13.2779106371597,63.476885421999));
#140217=CARTESIAN_POINT('Ctrl Pts',(97.7454211026964,13.2785162484723,63.475476070543));
#140218=CARTESIAN_POINT('Ctrl Pts',(97.7443092042379,13.279127985696,63.4740509297644));
#140219=CARTESIAN_POINT('Ctrl Pts',(97.7431878773281,13.279746562645,63.4726082223633));
#140220=CARTESIAN_POINT('Ctrl Pts',(97.7067057287732,13.2998718409635,63.4256700232804));
#140221=CARTESIAN_POINT('Ctrl Pts',(97.6731726327694,13.3186120473381,63.3767606726784));
#140222=CARTESIAN_POINT('Ctrl Pts',(97.6427496914699,13.3359671817688,63.3262726338115));
#140223=CARTESIAN_POINT('Ctrl Pts',(97.6121486921119,13.3534238915703,63.275489100762));
#140224=CARTESIAN_POINT('Ctrl Pts',(97.5846943551583,13.3694792690058,63.2231087895806));
#140225=CARTESIAN_POINT('Ctrl Pts',(97.5604980861838,13.3841333140753,63.1695378143773));
#140226=CARTESIAN_POINT('Ctrl Pts',(97.5360840546123,13.3989192432347,63.1154847088631));
#140227=CARTESIAN_POINT('Ctrl Pts',(97.5149869650521,13.4122785029845,63.0602198511968));
#140228=CARTESIAN_POINT('Ctrl Pts',(97.497268174044,13.4242110933247,63.0041605469673));
#140229=CARTESIAN_POINT('Ctrl Pts',(97.4899793158144,13.4291197216427,62.9810998132641));
#140230=CARTESIAN_POINT('Ctrl Pts',(97.4832615175028,13.4337869294389,62.9579046074509));
#140231=CARTESIAN_POINT('Ctrl Pts',(97.4771165116137,13.4382127167133,62.9346037225659));
#140232=CARTESIAN_POINT('Ctrl Pts',(97.4619819936829,13.4491129758948,62.8772160379222));
#140233=CARTESIAN_POINT('Ctrl Pts',(97.4503255590828,13.4585488113325,62.8191883236414));
#140234=CARTESIAN_POINT('Ctrl Pts',(97.4421362402369,13.4665202230264,62.7609433102217));
#140235=CARTESIAN_POINT('Ctrl Pts',(97.4338962979358,13.4745409111509,62.7023382468543));
#140236=CARTESIAN_POINT('Ctrl Pts',(97.4291662775862,13.4810790144791,62.6435135913618));
#140237=CARTESIAN_POINT('Ctrl Pts',(97.4278843900862,13.4861345330108,62.5848843420891));
#140238=CARTESIAN_POINT('Ctrl Pts',(97.4265906202032,13.4912369133828,62.5257116323384));
#140239=CARTESIAN_POINT('Ctrl Pts',(97.4288089871018,13.4948290961008,62.4667383536048));
#140240=CARTESIAN_POINT('Ctrl Pts',(97.4344276219277,13.4969110811646,62.408369305678));
#140241=CARTESIAN_POINT('Ctrl Pts',(97.4362098135436,13.4975714722454,62.3898550524705));
#140242=CARTESIAN_POINT('Ctrl Pts',(97.4383337629024,13.4980799202305,62.3714014050411));
#140243=CARTESIAN_POINT('Ctrl Pts',(97.4407949555856,13.49843642512,62.3530207360974));
#140244=CARTESIAN_POINT('',(95.9574505237762,14.9983370670242,62.1685354760649));
#140245=CARTESIAN_POINT('Ctrl Pts',(98.4192401195208,14.4018041137337,65.9071351980887));
#140246=CARTESIAN_POINT('Ctrl Pts',(98.3548599127743,14.4089099341238,65.8922317214608));
#140247=CARTESIAN_POINT('Ctrl Pts',(98.2858505689251,14.417160748693,65.873809883599));
#140248=CARTESIAN_POINT('Ctrl Pts',(98.212727410607,14.4267274727341,65.8508614541008));
#140249=CARTESIAN_POINT('Ctrl Pts',(98.1455872512908,14.435511439278,65.8297906846208));
#140250=CARTESIAN_POINT('Ctrl Pts',(98.0749795403419,14.4454051014527,65.8049036302979));
#140251=CARTESIAN_POINT('Ctrl Pts',(98.001322024238,14.4564991321363,65.7754036828193));
#140252=CARTESIAN_POINT('Ctrl Pts',(97.9947582500405,14.4574877442454,65.7727748812477));
#140253=CARTESIAN_POINT('Ctrl Pts',(97.9881702673191,14.458485857057,65.7701094381682));
#140254=CARTESIAN_POINT('Ctrl Pts',(97.9815583771808,14.4594935156246,65.767406783545));
#140255=CARTESIAN_POINT('Ctrl Pts',(97.9116352015369,14.4701498764441,65.7388252145884));
#140256=CARTESIAN_POINT('Ctrl Pts',(97.8390711057577,14.4818801472515,65.7060692153778));
#140257=CARTESIAN_POINT('Ctrl Pts',(97.7644638927116,14.4947164022248,65.6684025466324));
#140258=CARTESIAN_POINT('Ctrl Pts',(97.7528484664463,14.4967148493866,65.6625383091732));
#140259=CARTESIAN_POINT('Ctrl Pts',(97.7411835148542,14.4987400037317,65.6565550210306));
#140260=CARTESIAN_POINT('Ctrl Pts',(97.72947128728,14.5007918709519,65.6504498792864));
#140261=CARTESIAN_POINT('Ctrl Pts',(97.6860006840233,14.5084074936246,65.6277902961367));
#140262=CARTESIAN_POINT('Ctrl Pts',(97.6418829950394,14.5163917403531,65.6034511475642));
#140263=CARTESIAN_POINT('Ctrl Pts',(97.5972596749744,14.5247411162083,65.5772822763999));
#140264=CARTESIAN_POINT('Ctrl Pts',(97.5749480149419,14.5289158041359,65.5641978408177));
#140265=CARTESIAN_POINT('Ctrl Pts',(97.5525102327289,14.5331816709044,65.5506558940559));
#140266=CARTESIAN_POINT('Ctrl Pts',(97.529965780174,14.5375376166696,65.5366371873412));
#140267=CARTESIAN_POINT('Ctrl Pts',(97.5186935538966,14.5397155895522,65.5296278339839));
#140268=CARTESIAN_POINT('Ctrl Pts',(97.5073946597482,14.5419160749039,65.5224992888258));
#140269=CARTESIAN_POINT('Ctrl Pts',(97.4960716716008,14.5441388904471,65.5152491116246));
#140270=CARTESIAN_POINT('Ctrl Pts',(97.4847486834535,14.5463617059903,65.5079989344235));
#140271=CARTESIAN_POINT('Ctrl Pts',(97.4718880028697,14.5489087097035,65.4996291420303));
#140272=CARTESIAN_POINT('Ctrl Pts',(97.462033008452,14.5508741142754,65.4931312351855));
#140273=CARTESIAN_POINT('Ctrl Pts',(97.3831930531109,14.5665973508509,65.4411479804269));
#140274=CARTESIAN_POINT('Ctrl Pts',(97.3062831928474,14.5826460682807,65.3857544981588));
#140275=CARTESIAN_POINT('Ctrl Pts',(97.2315642963389,14.5988726037447,65.3270122750896));
#140276=CARTESIAN_POINT('Ctrl Pts',(97.1942048480847,14.6069858714767,65.297641163555));
#140277=CARTESIAN_POINT('Ctrl Pts',(97.1573958789567,14.6151423536242,65.267437499745));
#140278=CARTESIAN_POINT('Ctrl Pts',(97.1211760870691,14.623321403787,65.2364175858901));
#140279=CARTESIAN_POINT('Ctrl Pts',(97.1030661911253,14.6274109288684,65.2209076289627));
#140280=CARTESIAN_POINT('Ctrl Pts',(97.0851035896286,14.6315060984733,65.2051936103958));
#140281=CARTESIAN_POINT('Ctrl Pts',(97.0672931597619,14.6356043747053,65.1892774460997));
#140282=CARTESIAN_POINT('Ctrl Pts',(97.0583879448286,14.6376535128213,65.1813193639516));
#140283=CARTESIAN_POINT('Ctrl Pts',(97.0495207728092,14.6397034277684,65.173310745412));
#140284=CARTESIAN_POINT('Ctrl Pts',(97.0406922544568,14.6417538041061,65.1652518268546));
#140285=CARTESIAN_POINT('Ctrl Pts',(97.0329673008984,14.6435478834017,65.1582002731169));
#140286=CARTESIAN_POINT('Ctrl Pts',(97.0252719415541,14.6453423159601,65.151110208431));
#140287=CARTESIAN_POINT('Ctrl Pts',(97.0176065863376,14.6471368914392,65.1439817888684));
#140288=CARTESIAN_POINT('Ctrl Pts',(97.0165115355924,14.6473932593647,65.1429634432166));
#140289=CARTESIAN_POINT('Ctrl Pts',(97.0144528815075,14.6478756252705,65.1410452550338));
#140290=CARTESIAN_POINT('Ctrl Pts',(97.0143232723051,14.6479060033694,65.1409244040454));
#140291=CARTESIAN_POINT('Ctrl Pts',(97.0119524859554,14.6484616736518,65.1387138212454));
#140292=CARTESIAN_POINT('Ctrl Pts',(97.0043001237704,14.6502753896007,65.1314987778178));
#140293=CARTESIAN_POINT('Ctrl Pts',(96.991581820615,14.6533604270402,65.1190391432065));
#140294=CARTESIAN_POINT('Ctrl Pts',(96.982050505149,14.6556724072393,65.1097016784032));
#140295=CARTESIAN_POINT('Ctrl Pts',(96.9696745896939,14.6586976140359,65.0974183794051));
#140296=CARTESIAN_POINT('Ctrl Pts',(96.9545534271432,14.6624254448703,65.0820823431156));
#140297=CARTESIAN_POINT('Ctrl Pts',(96.9369042316537,14.6667765134425,65.0641823502017));
#140298=CARTESIAN_POINT('Ctrl Pts',(96.9155414545847,14.6720913792892,65.0420933193525));
#140299=CARTESIAN_POINT('Ctrl Pts',(96.8908164867911,14.6783548011537,65.015465716334));
#140300=CARTESIAN_POINT('Ctrl Pts',(96.8784540028943,14.6814865120859,65.0021519148247));
#140301=CARTESIAN_POINT('Ctrl Pts',(96.865253244134,14.6848551342965,64.9877016437808));
#140302=CARTESIAN_POINT('Ctrl Pts',(96.851272898472,14.6884568977787,64.9720607676581));
#140303=CARTESIAN_POINT('Ctrl Pts',(96.844282725641,14.6902577795197,64.9642403295968));
#140304=CARTESIAN_POINT('Ctrl Pts',(96.8370976548813,14.6921169087872,64.9561222326553));
#140305=CARTESIAN_POINT('Ctrl Pts',(96.8297262224199,14.6940336711822,64.9476989950849));
#140306=CARTESIAN_POINT('Ctrl Pts',(96.8260405061892,14.6949920523797,64.9434873762997));
#140307=CARTESIAN_POINT('Ctrl Pts',(96.8223081994494,14.6959648392636,64.9391994718284));
#140308=CARTESIAN_POINT('Ctrl Pts',(96.818530410879,14.6969519411706,64.9348343262526));
#140309=CARTESIAN_POINT('Ctrl Pts',(96.8147526223086,14.6979390430776,64.9304691806768));
#140310=CARTESIAN_POINT('Ctrl Pts',(96.8098803509342,14.6992159243711,64.9248006981191));
#140311=CARTESIAN_POINT('Ctrl Pts',(96.8070617302252,14.699956091772,64.9215061981443));
#140312=CARTESIAN_POINT('Ctrl Pts',(96.8032885852447,14.7009469164348,64.9170960176601));
#140313=CARTESIAN_POINT('Ctrl Pts',(96.7995557144585,14.7019290499594,64.9127106355594));
#140314=CARTESIAN_POINT('Ctrl Pts',(96.7958627355554,14.702902482579,64.9083506489919));
#140315=CARTESIAN_POINT('Ctrl Pts',(96.7502411896542,14.7149278696991,64.8544891641206));
#140316=CARTESIAN_POINT('Ctrl Pts',(96.7107031946376,14.7256243960024,64.8045047207743));
#140317=CARTESIAN_POINT('Ctrl Pts',(96.676558228223,14.7349808674531,64.7595146643301));
#140318=CARTESIAN_POINT('Ctrl Pts',(96.6473952891325,14.7429721538906,64.7210890217384));
#140319=CARTESIAN_POINT('Ctrl Pts',(96.6221675546253,14.7499867814444,64.6863063983579));
#140320=CARTESIAN_POINT('Ctrl Pts',(96.6004730779209,14.7560178220167,64.6558527121837));
#140321=CARTESIAN_POINT('Ctrl Pts',(96.5629238633939,14.7664564621993,64.6031428906529));
#140322=CARTESIAN_POINT('Ctrl Pts',(96.5242227079699,14.7772898571612,64.5464888620646));
#140323=CARTESIAN_POINT('Ctrl Pts',(96.4851640788121,14.7884057688328,64.4855046878037));
#140324=CARTESIAN_POINT('Ctrl Pts',(96.4484138417273,14.7988647224149,64.4281247205381));
#140325=CARTESIAN_POINT('Ctrl Pts',(96.4113473941561,14.8095737125234,64.366911150988));
#140326=CARTESIAN_POINT('Ctrl Pts',(96.3745927052218,14.8204105290804,64.3015517348863));
#140327=CARTESIAN_POINT('Ctrl Pts',(96.3481442829553,14.8282086280069,64.2545195469866));
#140328=CARTESIAN_POINT('Ctrl Pts',(96.3218566407735,14.8360723462582,64.2053407521427));
#140329=CARTESIAN_POINT('Ctrl Pts',(96.2959506744976,14.8439462867232,64.1539029936064));
#140330=CARTESIAN_POINT('Ctrl Pts',(96.2638834095475,14.8536929115896,64.0902316287224));
#140331=CARTESIAN_POINT('Ctrl Pts',(96.2324644575906,14.8634547627218,64.0230936187831));
#140332=CARTESIAN_POINT('Ctrl Pts',(96.2023566467437,14.8730978451295,63.9523310853555));
#140333=CARTESIAN_POINT('Ctrl Pts',(96.1854403500314,14.8785158824641,63.9125726313894));
#140334=CARTESIAN_POINT('Ctrl Pts',(96.1689371821935,14.8838961256817,63.8716702383139));
#140335=CARTESIAN_POINT('Ctrl Pts',(96.1529581626964,14.8892124571374,63.8295981632268));
#140336=CARTESIAN_POINT('Ctrl Pts',(96.1307488356699,14.8966016554485,63.771121954817));
#140337=CARTESIAN_POINT('Ctrl Pts',(96.1095562915821,14.9038653249061,63.7104017724764));
#140338=CARTESIAN_POINT('Ctrl Pts',(96.0897091813706,14.9109207031831,63.6474492675876));
#140339=CARTESIAN_POINT('Ctrl Pts',(96.0797856262649,14.9144483923216,63.6159730151432));
#140340=CARTESIAN_POINT('Ctrl Pts',(96.0701989423633,14.9179239040919,63.5839392466392));
#140341=CARTESIAN_POINT('Ctrl Pts',(96.0609934095968,14.921336373574,63.5513530352228));
#140342=CARTESIAN_POINT('Ctrl Pts',(96.053607930715,14.9240741533347,63.5252095427864));
#140343=CARTESIAN_POINT('Ctrl Pts',(96.0462305073155,14.9268664675079,63.4977564710501));
#140344=CARTESIAN_POINT('Ctrl Pts',(96.0394561086189,14.9294780313795,63.4712938920148));
#140345=CARTESIAN_POINT('Ctrl Pts',(96.0377866473881,14.9301216168592,63.46477253835));
#140346=CARTESIAN_POINT('Ctrl Pts',(96.0361538646799,14.9307544694931,63.4583113444831));
#140347=CARTESIAN_POINT('Ctrl Pts',(96.0345667776102,14.931373538865,63.4519447433593));
#140348=CARTESIAN_POINT('Ctrl Pts',(96.0131082811534,14.9397437777626,63.3658639666528));
#140349=CARTESIAN_POINT('Ctrl Pts',(95.9957427903507,14.9471044693013,63.2816295298594));
#140350=CARTESIAN_POINT('Ctrl Pts',(95.9818299032794,14.9535676953711,63.1995854857261));
#140351=CARTESIAN_POINT('Ctrl Pts',(95.9675042100614,14.9602226903695,63.1151071311908));
#140352=CARTESIAN_POINT('Ctrl Pts',(95.9568390643428,14.965926347952,63.0329510722339));
#140353=CARTESIAN_POINT('Ctrl Pts',(95.9491875207717,14.9708082268386,62.9534723392464));
#140354=CARTESIAN_POINT('Ctrl Pts',(95.942031555446,14.9753739142338,62.8791413167404));
#140355=CARTESIAN_POINT('Ctrl Pts',(95.9375121760969,14.9792210400244,62.8071517437967));
#140356=CARTESIAN_POINT('Ctrl Pts',(95.9351384484719,14.9824588177391,62.7377790576165));
#140357=CARTESIAN_POINT('Ctrl Pts',(95.9323603880237,14.9862481076789,62.6565896601325));
#140358=CARTESIAN_POINT('Ctrl Pts',(95.9323866516514,14.9892056743569,62.5789843422128));
#140359=CARTESIAN_POINT('Ctrl Pts',(95.9344117700746,14.9915124506985,62.5050586921308));
#140360=CARTESIAN_POINT('Ctrl Pts',(95.9365700339944,14.9939708907046,62.4262726510363));
#140361=CARTESIAN_POINT('Ctrl Pts',(95.9409989357065,14.9956903942518,62.3516658234036));
#140362=CARTESIAN_POINT('Ctrl Pts',(95.9467749196894,14.99686525085,62.281333677442));
#140363=CARTESIAN_POINT('Ctrl Pts',(95.9499705646574,14.9975152569073,62.2424214212794));
#140364=CARTESIAN_POINT('Ctrl Pts',(95.9535794175851,14.9979980947992,62.2048173203955));
#140365=CARTESIAN_POINT('Ctrl Pts',(95.9574505343397,14.99834334873,62.1685355389868));
#140366=CARTESIAN_POINT('Ctrl Pts',(95.9574504676803,14.9983112794787,62.1685352218286));
#140367=CARTESIAN_POINT('Ctrl Pts',(96.0005011109051,14.9981619617962,62.1743324282915));
#140368=CARTESIAN_POINT('Ctrl Pts',(96.0441829211307,14.9961208430062,62.180187222598));
#140369=CARTESIAN_POINT('Ctrl Pts',(96.0882590761874,14.992038585098,62.1860688983633));
#140370=CARTESIAN_POINT('Ctrl Pts',(96.1314805172245,14.9880354893368,62.1918365181106));
#140371=CARTESIAN_POINT('Ctrl Pts',(96.1750806514507,14.9820691038472,62.1976299162011));
#140372=CARTESIAN_POINT('Ctrl Pts',(96.2188022886828,14.9740352308408,62.2034157554569));
#140373=CARTESIAN_POINT('Ctrl Pts',(96.2620787520592,14.966083158756,62.2091426832782));
#140374=CARTESIAN_POINT('Ctrl Pts',(96.3054736560346,14.956105021506,62.2148621223634));
#140375=CARTESIAN_POINT('Ctrl Pts',(96.3487121925896,14.9440435852066,62.2205385368215));
#140376=CARTESIAN_POINT('Ctrl Pts',(96.3914593744506,14.9321192128278,62.2261504455607));
#140377=CARTESIAN_POINT('Ctrl Pts',(96.4340530118707,14.9181583406398,62.2317202050112));
#140378=CARTESIAN_POINT('Ctrl Pts',(96.4762123767249,14.9021542371481,62.2372116669386));
#140379=CARTESIAN_POINT('Ctrl Pts',(96.4929937416756,14.8957838683741,62.2393975211857));
#140380=CARTESIAN_POINT('Ctrl Pts',(96.5097061892548,14.889090334833,62.2415709577068));
#140381=CARTESIAN_POINT('Ctrl Pts',(96.526331738287,14.8820755052874,62.2437296705194));
#140382=CARTESIAN_POINT('Ctrl Pts',(96.5677011654777,14.8646204739027,62.2491012051589));
#140383=CARTESIAN_POINT('Ctrl Pts',(96.6085321883246,14.8451724086258,62.2543818537009));
#140384=CARTESIAN_POINT('Ctrl Pts',(96.6485498202056,14.8237961698842,62.2595354128814));
#140385=CARTESIAN_POINT('Ctrl Pts',(96.6887339095709,14.8023310144636,62.2647104088251));
#140386=CARTESIAN_POINT('Ctrl Pts',(96.7280970216981,14.7789217013327,62.2697571489435));
#140387=CARTESIAN_POINT('Ctrl Pts',(96.7663731273024,14.7536856636138,62.2746411252101));
#140388=CARTESIAN_POINT('Ctrl Pts',(96.8042656201698,14.7287025477986,62.2794761530409));
#140389=CARTESIAN_POINT('Ctrl Pts',(96.8410921005653,14.7019295529653,62.2841515753469));
#140390=CARTESIAN_POINT('Ctrl Pts',(96.8766177138151,14.6735272668377,62.2886374649293));
#140391=CARTESIAN_POINT('Ctrl Pts',(96.9121727657077,14.6451014448811,62.2931270717874));
#140392=CARTESIAN_POINT('Ctrl Pts',(96.9464241864178,14.6150441406749,62.2974267552004));
#140393=CARTESIAN_POINT('Ctrl Pts',(96.9791697210766,14.5835564888875,62.3015113349985));
#140394=CARTESIAN_POINT('Ctrl Pts',(97.0120092150943,14.5519784870843,62.3056076350053));
#140395=CARTESIAN_POINT('Ctrl Pts',(97.043333705804,14.5189625652565,62.3094875393312));
#140396=CARTESIAN_POINT('Ctrl Pts',(97.0729806653625,14.484743219441,62.3131315012315));
#140397=CARTESIAN_POINT('Ctrl Pts',(97.1030081825707,14.4500846233949,62.316822238167));
#140398=CARTESIAN_POINT('Ctrl Pts',(97.1313144664109,14.4141922439907,62.3202708953771));
#140399=CARTESIAN_POINT('Ctrl Pts',(97.1577795236448,14.3773316661675,62.3234639139798));
#140400=CARTESIAN_POINT('Ctrl Pts',(97.1843342351965,14.3403462176542,62.3266677494081));
#140401=CARTESIAN_POINT('Ctrl Pts',(97.2090351572593,14.3023868126045,62.3296142099809));
#140402=CARTESIAN_POINT('Ctrl Pts',(97.2318130930835,14.2637318774777,62.3322966586155));
#140403=CARTESIAN_POINT('Ctrl Pts',(97.2549393663752,14.2244858017705,62.3350201292886));
#140404=CARTESIAN_POINT('Ctrl Pts',(97.276083437397,14.1845235730453,62.3374714655972));
#140405=CARTESIAN_POINT('Ctrl Pts',(97.2952267179217,14.1441346156089,62.3396509096967));
#140406=CARTESIAN_POINT('Ctrl Pts',(97.3136023357209,14.1053652916048,62.3417429561323));
#140407=CARTESIAN_POINT('Ctrl Pts',(97.3301350398945,14.0662033083041,62.3435845683744));
#140408=CARTESIAN_POINT('Ctrl Pts',(97.3448517592675,14.0268930901495,62.3451816578265));
#140409=CARTESIAN_POINT('Ctrl Pts',(97.3605291573088,13.9850167778082,62.3468830021556));
#140410=CARTESIAN_POINT('Ctrl Pts',(97.3741457445416,13.9429731857398,62.3483068521509));
#140411=CARTESIAN_POINT('Ctrl Pts',(97.3857801232169,13.9010337028441,62.3494664591817));
#140412=CARTESIAN_POINT('Ctrl Pts',(97.3977004858437,13.8580633080815,62.350654570442));
#140413=CARTESIAN_POINT('Ctrl Pts',(97.4075405333139,13.8152027833417,62.3515653653733));
#140414=CARTESIAN_POINT('Ctrl Pts',(97.415426538954,13.7727089150853,62.3522183319137));
#140415=CARTESIAN_POINT('Ctrl Pts',(97.423434730561,13.7295566457809,62.352881415534));
#140416=CARTESIAN_POINT('Ctrl Pts',(97.4294285686737,13.6867828301511,62.3532787166675));
#140417=CARTESIAN_POINT('Ctrl Pts',(97.4335730705108,13.6446135218585,62.3534346198244));
#140418=CARTESIAN_POINT('Ctrl Pts',(97.4378188709953,13.6014135242178,62.3535943335186));
#140419=CARTESIAN_POINT('Ctrl Pts',(97.4401245654739,13.5588481660462,62.3535008046023));
#140420=CARTESIAN_POINT('Ctrl Pts',(97.4406905904248,13.5171113558476,62.3531828726247));
#140421=CARTESIAN_POINT('Ctrl Pts',(97.4407752648613,13.510867742592,62.3531353116276));
#140422=CARTESIAN_POINT('Ctrl Pts',(97.4408210370043,13.5046425807729,62.3530827318652));
#140423=CARTESIAN_POINT('Ctrl Pts',(97.440828605087,13.4984364247508,62.3530252326599));
#140424=CARTESIAN_POINT('Ctrl Pts',(95.6383694486691,14.96466568086,62.13083612273));
#140425=CARTESIAN_POINT('Ctrl Pts',(95.6497349713691,14.96550769017,62.04287213666));
#140426=CARTESIAN_POINT('Ctrl Pts',(95.6643822846691,14.96457285862,61.95567204144));
#140427=CARTESIAN_POINT('Ctrl Pts',(95.6821735052692,14.96198967028,61.8696850735));
#140428=CARTESIAN_POINT('Ctrl Pts',(96.8005714632691,15.21737516854,62.287692685));
#140429=CARTESIAN_POINT('Ctrl Pts',(96.8092255620691,15.21825422082,62.21975234547));
#140430=CARTESIAN_POINT('Ctrl Pts',(96.8206378887691,15.21727770737,62.15269641207));
#140431=CARTESIAN_POINT('Ctrl Pts',(96.8346416864691,15.21458604043,62.08693395755));
#140432=CARTESIAN_POINT('Ctrl Pts',(97.6471925791692,14.37376668098,62.39128093599));
#140433=CARTESIAN_POINT('Ctrl Pts',(97.6521322186691,14.37452207443,62.35267039112));
#140434=CARTESIAN_POINT('Ctrl Pts',(97.6586006697691,14.37368470574,62.31451148597));
#140435=CARTESIAN_POINT('Ctrl Pts',(97.6665135970691,14.37135516796,62.2770259460699));
#140436=CARTESIAN_POINT('Ctrl Pts',(97.4109254415691,13.19841717584,62.34771705287));
#140437=CARTESIAN_POINT('Ctrl Pts',(97.414514065169,13.1990002828,62.32116035078));
#140438=CARTESIAN_POINT('Ctrl Pts',(97.4188104715692,13.19835677621,62.294461464));
#140439=CARTESIAN_POINT('Ctrl Pts',(97.4238493419691,13.19653177145,62.26767738332));
#140440=CARTESIAN_POINT('',(95.9754884183226,14.9956963974856,61.9308509078933));
#140441=CARTESIAN_POINT('',(97.4550857102592,13.496508878909,62.2658809045985));
#140442=CARTESIAN_POINT('Ctrl Pts',(95.9754884244307,14.9956951278022,61.9308509489964));
#140443=CARTESIAN_POINT('Ctrl Pts',(96.0191083210387,14.9961786137454,61.9393038707493));
#140444=CARTESIAN_POINT('Ctrl Pts',(96.0635504718247,14.9946955776386,61.9479826282064));
#140445=CARTESIAN_POINT('Ctrl Pts',(96.1085757343769,14.9910370652072,61.9568462597379));
#140446=CARTESIAN_POINT('Ctrl Pts',(96.1505747912088,14.9876244460949,61.9651141552109));
#140447=CARTESIAN_POINT('Ctrl Pts',(96.193080514892,14.9823184951072,61.9735427871285));
#140448=CARTESIAN_POINT('Ctrl Pts',(96.2358578027182,14.9749781871825,61.9820900878307));
#140449=CARTESIAN_POINT('Ctrl Pts',(96.278072462214,14.9677344226667,61.99052497015));
#140450=CARTESIAN_POINT('Ctrl Pts',(96.3205511352868,14.9585088652372,61.9990753497081));
#140451=CARTESIAN_POINT('Ctrl Pts',(96.3630342769716,14.9472028291044,62.0076931693938));
#140452=CARTESIAN_POINT('Ctrl Pts',(96.4048605947515,14.9360715934809,62.0161777505818));
#140453=CARTESIAN_POINT('Ctrl Pts',(96.4466906368304,14.9229232703164,62.0247275977974));
#140454=CARTESIAN_POINT('Ctrl Pts',(96.4882518102421,14.9077073157761,62.0332907098102));
#140455=CARTESIAN_POINT('Ctrl Pts',(96.4992763656077,14.9036711175772,62.0355621688364));
#140456=CARTESIAN_POINT('Ctrl Pts',(96.510281893819,14.8994896941963,62.0378345323532));
#140457=CARTESIAN_POINT('Ctrl Pts',(96.521263097106,14.8951626834577,62.0401067716795));
#140458=CARTESIAN_POINT('Ctrl Pts',(96.5620779388225,14.8790800872441,62.0485522112201));
#140459=CARTESIAN_POINT('Ctrl Pts',(96.6025573539562,14.8609822885599,62.0569960680615));
#140460=CARTESIAN_POINT('Ctrl Pts',(96.6424231041339,14.8408826368191,62.0653838282803));
#140461=CARTESIAN_POINT('Ctrl Pts',(96.6820560401633,14.8209003661205,62.073722604365));
#140462=CARTESIAN_POINT('Ctrl Pts',(96.7210816886419,14.7989394613249,62.0820057905489));
#140463=CARTESIAN_POINT('Ctrl Pts',(96.759225816053,14.7750648426393,62.0901780232053));
#140464=CARTESIAN_POINT('Ctrl Pts',(96.7969762923547,14.7514366123435,62.0982659176249));
#140465=CARTESIAN_POINT('Ctrl Pts',(96.8338625952804,14.7259341211053,62.106244985407));
#140466=CARTESIAN_POINT('Ctrl Pts',(96.8696294257684,14.6986706484175,62.1140620170905));
#140467=CARTESIAN_POINT('Ctrl Pts',(96.9052869047156,14.671490529572,62.1218551494111));
#140468=CARTESIAN_POINT('Ctrl Pts',(96.939831034534,14.642560483646,62.1294870870391));
#140469=CARTESIAN_POINT('Ctrl Pts',(96.9730303594275,14.6120396990625,62.1369078063701));
#140470=CARTESIAN_POINT('Ctrl Pts',(97.0061957622891,14.5815500996622,62.1443209434421));
#140471=CARTESIAN_POINT('Ctrl Pts',(97.0380184890529,14.5494734876474,62.1515231584376));
#140472=CARTESIAN_POINT('Ctrl Pts',(97.068299307024,14.5160096404253,62.1584694107072));
#140473=CARTESIAN_POINT('Ctrl Pts',(97.09931311718,14.4817357510665,62.1655838073326));
#140474=CARTESIAN_POINT('Ctrl Pts',(97.1287087824755,14.4460071930328,62.1724295492829));
#140475=CARTESIAN_POINT('Ctrl Pts',(97.1563155440183,14.4090742021617,62.1789655383446));
#140476=CARTESIAN_POINT('Ctrl Pts',(97.1834562895665,14.3727646587185,62.1853911966296));
#140477=CARTESIAN_POINT('Ctrl Pts',(97.2088678516148,14.335291837961,62.1915174128252));
#140478=CARTESIAN_POINT('Ctrl Pts',(97.2324352222714,14.2969167745708,62.1973135863302));
#140479=CARTESIAN_POINT('Ctrl Pts',(97.2566095827945,14.2575533415002,62.2032590432931));
#140480=CARTESIAN_POINT('Ctrl Pts',(97.2788432203137,14.2172413970997,62.2088571516982));
#140481=CARTESIAN_POINT('Ctrl Pts',(97.299066299966,14.1762750641382,62.2140850483323));
#140482=CARTESIAN_POINT('Ctrl Pts',(97.3192893796184,14.1353087311766,62.2193129449663));
#140483=CARTESIAN_POINT('Ctrl Pts',(97.3375020484776,14.0936888593738,62.2241706315931));
#140484=CARTESIAN_POINT('Ctrl Pts',(97.3536889863142,14.0517091014271,62.2286458580523));
#140485=CARTESIAN_POINT('Ctrl Pts',(97.3698918780564,14.0096879680761,62.2331254953113));
#140486=CARTESIAN_POINT('Ctrl Pts',(97.3840653445013,13.967306988715,62.2372221744852));
#140487=CARTESIAN_POINT('Ctrl Pts',(97.396245092228,13.9248481617357,62.2409331441791));
#140488=CARTESIAN_POINT('Ctrl Pts',(97.4086654939252,13.8815504105422,62.2447174371971));
#140489=CARTESIAN_POINT('Ctrl Pts',(97.4190129936999,13.8381724103773,62.2481006829844));
#140490=CARTESIAN_POINT('Ctrl Pts',(97.4273730516207,13.7949890382272,62.2510901819957));
#140491=CARTESIAN_POINT('Ctrl Pts',(97.4358374764906,13.7512665649319,62.2541170019076));
#140492=CARTESIAN_POINT('Ctrl Pts',(97.442265119551,13.7077441406454,62.2567402848846));
#140493=CARTESIAN_POINT('Ctrl Pts',(97.4467854389199,13.6646730669697,62.2589767561171));
#140494=CARTESIAN_POINT('Ctrl Pts',(97.4514017019649,13.6206878107326,62.2612606964008));
#140495=CARTESIAN_POINT('Ctrl Pts',(97.4540294770364,13.577173683171,62.2631413499673));
#140496=CARTESIAN_POINT('Ctrl Pts',(97.4548393150145,13.534355713319,62.2646443224215));
#140497=CARTESIAN_POINT('Ctrl Pts',(97.4550791011521,13.5216776766181,62.2650893397822));
#140498=CARTESIAN_POINT('Ctrl Pts',(97.4551596851296,13.5090603723168,62.2655012899924));
#140499=CARTESIAN_POINT('Ctrl Pts',(97.4550858933237,13.4965088789097,62.2658809401734));
#140500=CARTESIAN_POINT('Origin',(98.1267616152515,12.5716410462426,62.320869231712));
#140501=CARTESIAN_POINT('Origin',(98.8206098656912,12.3624040386408,62.2958872923182));
#140502=CARTESIAN_POINT('Ctrl Pts',(100.169335608469,14.99405726692,61.51611510888));
#140503=CARTESIAN_POINT('Ctrl Pts',(99.7148652716691,15.00734885163,60.98676941964));
#140504=CARTESIAN_POINT('Ctrl Pts',(98.8332753637691,14.83573834731,59.9502829098));
#140505=CARTESIAN_POINT('Ctrl Pts',(97.5676198956691,13.94788897315,58.43673095921));
#140506=CARTESIAN_POINT('Ctrl Pts',(96.8532769472691,12.93890086152,57.61785572376));
#140507=CARTESIAN_POINT('Ctrl Pts',(96.5377967531691,12.32169782044,57.28766800809));
#140508=CARTESIAN_POINT('Ctrl Pts',(99.1305766688691,14.99446242178,61.72461748813));
#140509=CARTESIAN_POINT('Ctrl Pts',(98.7164568384691,15.01076845648,61.17415228594));
#140510=CARTESIAN_POINT('Ctrl Pts',(97.9131284468691,14.83848819158,60.09687442266));
#140511=CARTESIAN_POINT('Ctrl Pts',(96.7645667377691,13.93938484243,58.54312551318));
#140512=CARTESIAN_POINT('Ctrl Pts',(96.1205077616691,12.92500300104,57.71449926823));
#140513=CARTESIAN_POINT('Ctrl Pts',(95.8379926099691,12.30969319204,57.38425138438));
#140514=CARTESIAN_POINT('Ctrl Pts',(96.3176189348691,14.99514161892,62.26071968093));
#140515=CARTESIAN_POINT('Ctrl Pts',(96.0154143699691,15.01926889724,61.65498469172));
#140516=CARTESIAN_POINT('Ctrl Pts',(95.4288082679691,14.84230328349,60.47059453057));
#140517=CARTESIAN_POINT('Ctrl Pts',(94.6024390106691,13.90781835228,58.81819612913));
#140518=CARTESIAN_POINT('Ctrl Pts',(94.1494817780691,12.87788125739,57.96906759383));
#140519=CARTESIAN_POINT('Ctrl Pts',(93.9560138780691,12.26890002092,57.6409827674));
#140520=CARTESIAN_POINT('Ctrl Pts',(93.4953850345691,14.99506638051,62.7559974319));
#140521=CARTESIAN_POINT('Ctrl Pts',(93.3103671812691,15.0242959982,62.09949931116));
#140522=CARTESIAN_POINT('Ctrl Pts',(92.9497536882691,14.83329013866,60.81498722494));
#140523=CARTESIAN_POINT('Ctrl Pts',(92.4556410153691,13.85106768651,59.08485218125));
#140524=CARTESIAN_POINT('Ctrl Pts',(92.1957994607691,12.80282306576,58.22524694262));
#140525=CARTESIAN_POINT('Ctrl Pts',(92.0912558337691,12.20332775014,57.90308798197));
#140526=CARTESIAN_POINT('Ctrl Pts',(91.7184465780691,14.9948609804,63.073805056447));
#140527=CARTESIAN_POINT('Ctrl Pts',(91.6074520331691,15.02536787074,62.38713311363));
#140528=CARTESIAN_POINT('Ctrl Pts',(91.3893306495691,14.82127594063,61.04190429299));
#140529=CARTESIAN_POINT('Ctrl Pts',(91.1046486454691,13.80536352591,59.26795531069));
#140530=CARTESIAN_POINT('Ctrl Pts',(90.9665687706691,12.7445626307,58.40207411475));
#140531=CARTESIAN_POINT('Ctrl Pts',(90.9180991174691,12.15223092569,58.08340275416));
#140532=CARTESIAN_POINT('Ctrl Pts',(95.9574506170498,14.9983799452468,62.1685358987961));
#140533=CARTESIAN_POINT('Ctrl Pts',(94.6103064012642,14.9990728434965,62.4078600669976));
#140534=CARTESIAN_POINT('Ctrl Pts',(93.2623353470216,14.9994593482969,62.640153612899));
#140535=CARTESIAN_POINT('Ctrl Pts',(91.9155436377164,14.9994907910626,62.8752831531645));
#140536=CARTESIAN_POINT('',(91.0790838175691,12.28284151812,58.13147659972));
#140537=CARTESIAN_POINT('Ctrl Pts',(91.9155428607298,14.9991665213478,62.8752787466432));
#140538=CARTESIAN_POINT('Ctrl Pts',(91.8320338374965,15.0060364948596,62.4015881812362));
#140539=CARTESIAN_POINT('Ctrl Pts',(91.7477460466049,14.9479895031152,61.9239636529671));
#140540=CARTESIAN_POINT('Ctrl Pts',(91.5847899897675,14.709291500823,61.0000296041516));
#140541=CARTESIAN_POINT('Ctrl Pts',(91.5063590297402,14.5281607691405,60.5547834032252));
#140542=CARTESIAN_POINT('Ctrl Pts',(91.360391355721,14.0537134211762,59.726275526801));
#140543=CARTESIAN_POINT('Ctrl Pts',(91.2926247379441,13.7595734546084,59.342158909907));
#140544=CARTESIAN_POINT('Ctrl Pts',(91.1722735521674,13.077960345171,58.6612811253686));
#140545=CARTESIAN_POINT('Ctrl Pts',(91.1199115659794,12.6926154932127,58.3651666009541));
#140546=CARTESIAN_POINT('Ctrl Pts',(91.0790838175691,12.28284151812,58.13147659972));
#140547=CARTESIAN_POINT('',(96.4484017897691,12.44788635501,57.38025496851));
#140548=CARTESIAN_POINT('Ctrl Pts',(96.4484001507624,12.4478935028557,57.3802439116704));
#140549=CARTESIAN_POINT('Ctrl Pts',(95.7943735804126,12.4360471853169,57.4695350918061));
#140550=CARTESIAN_POINT('Ctrl Pts',(95.1433169455258,12.4214640739689,57.5574467728654));
#140551=CARTESIAN_POINT('Ctrl Pts',(94.4942820323385,12.403912404117,57.645899157917));
#140552=CARTESIAN_POINT('Ctrl Pts',(93.3510410917193,12.3729960587199,57.8017033925302));
#140553=CARTESIAN_POINT('Ctrl Pts',(92.2140755027029,12.3328695466178,57.9591853627902));
#140554=CARTESIAN_POINT('Ctrl Pts',(91.0788501393933,12.2836266462612,58.1301510978283));
#140555=CARTESIAN_POINT('Ctrl Pts',(95.9754884061691,14.99569893684,61.9308508253));
#140556=CARTESIAN_POINT('Ctrl Pts',(96.0318216593838,14.9774616413474,61.3605505558174));
#140557=CARTESIAN_POINT('Ctrl Pts',(96.0870995927844,14.8752077739731,60.8239709384119));
#140558=CARTESIAN_POINT('Ctrl Pts',(96.1885970738804,14.5572749510219,59.8513640078858));
#140559=CARTESIAN_POINT('Ctrl Pts',(96.2348131316939,14.3415143833096,59.4152840448726));
#140560=CARTESIAN_POINT('Ctrl Pts',(96.3152663723759,13.8490496175605,58.6542136864889));
#140561=CARTESIAN_POINT('Ctrl Pts',(96.3494921073714,13.5735114454258,58.3292420428182));
#140562=CARTESIAN_POINT('Ctrl Pts',(96.4064692538042,13.0105709490317,57.7832918174657));
#140563=CARTESIAN_POINT('Ctrl Pts',(96.4293880105424,12.7235448882221,57.561431885349));
#140564=CARTESIAN_POINT('Ctrl Pts',(96.4484017897691,12.44788635501,57.38025496851));
#140565=CARTESIAN_POINT('Ctrl Pts',(95.2659401102691,14.82531735257,61.99879853622));
#140566=CARTESIAN_POINT('Ctrl Pts',(95.3458225527691,14.82663418575,61.58784104641));
#140567=CARTESIAN_POINT('Ctrl Pts',(95.5189963877691,14.73079097291,60.6969433442));
#140568=CARTESIAN_POINT('Ctrl Pts',(95.7720667392691,14.25687316564,59.39501574815));
#140569=CARTESIAN_POINT('Ctrl Pts',(96.0056186731692,13.40283085562,58.19350120435));
#140570=CARTESIAN_POINT('Ctrl Pts',(96.1266411507691,12.63732789559,57.57089763824));
#140571=CARTESIAN_POINT('Ctrl Pts',(96.176798873169,12.21892969183,57.31285981381));
#140572=CARTESIAN_POINT('Ctrl Pts',(96.5343893935691,15.50721522815,62.24751894428));
#140573=CARTESIAN_POINT('Ctrl Pts',(96.6237567750691,15.50871098773,61.78776591757));
#140574=CARTESIAN_POINT('Ctrl Pts',(96.8172823823691,15.40154840317,60.7921679457));
#140575=CARTESIAN_POINT('Ctrl Pts',(97.1010190211691,14.87088436705,59.33247676506));
#140576=CARTESIAN_POINT('Ctrl Pts',(97.3638686534691,13.90970119862,57.9802393816401));
#140577=CARTESIAN_POINT('Ctrl Pts',(97.4995976301692,13.05070844107,57.2819778141701));
#140578=CARTESIAN_POINT('Ctrl Pts',(97.5558445876691,12.5815240184,56.99261374721));
#140579=CARTESIAN_POINT('Ctrl Pts',(97.6826966252692,14.63050777912,62.4679543560901));
#140580=CARTESIAN_POINT('Ctrl Pts',(97.7598693410691,14.63177349529,62.07093713223));
#140581=CARTESIAN_POINT('Ctrl Pts',(97.9272289328691,14.53916408337,61.20995096898));
#140582=CARTESIAN_POINT('Ctrl Pts',(98.1715383149691,14.08145795388,59.9530944278801));
#140583=CARTESIAN_POINT('Ctrl Pts',(98.3967202681692,13.25802442806,58.7946394875));
#140584=CARTESIAN_POINT('Ctrl Pts',(98.5135412854691,12.51923031731,58.1936504526901));
#140585=CARTESIAN_POINT('Ctrl Pts',(98.5619593906691,12.11534109209,57.9445621383801));
#140586=CARTESIAN_POINT('Ctrl Pts',(97.3966210806691,13.19858904608,62.40781584814));
#140587=CARTESIAN_POINT('Ctrl Pts',(97.453876354069,13.19947903431,62.11326447128));
#140588=CARTESIAN_POINT('Ctrl Pts',(97.5784992177692,13.13063919407,61.47213861681));
#140589=CARTESIAN_POINT('Ctrl Pts',(97.7584124008692,12.7920945857,60.5465701472));
#140590=CARTESIAN_POINT('Ctrl Pts',(97.922072057769,12.19364636594,59.70461840367));
#140591=CARTESIAN_POINT('Ctrl Pts',(98.0080108677692,11.65117167077,59.26250375952));
#140592=CARTESIAN_POINT('Ctrl Pts',(98.043642175869,11.35392852974,59.07919748546));
#140593=CARTESIAN_POINT('',(98.1061411588691,11.63978271644,58.91650643966));
#140594=CARTESIAN_POINT('Origin',(96.6336399486667,11.6397563224413,58.6303566427588));
#140595=CARTESIAN_POINT('Ctrl Pts',(97.4550854747306,13.4965088789073,62.265880858822));
#140596=CARTESIAN_POINT('Ctrl Pts',(97.4710316674903,13.4939105765947,62.1838452181956));
#140597=CARTESIAN_POINT('Ctrl Pts',(97.4868368133731,13.4890042223143,62.1025351947875));
#140598=CARTESIAN_POINT('Ctrl Pts',(97.5025133966026,13.4818673165301,62.0218865595026));
#140599=CARTESIAN_POINT('Ctrl Pts',(97.5183414772651,13.4746614401742,61.9404585412976));
#140600=CARTESIAN_POINT('Ctrl Pts',(97.5340386156073,13.4651816199485,61.859704152008));
#140601=CARTESIAN_POINT('Ctrl Pts',(97.5496185369051,13.4534544942426,61.7795527920009));
#140602=CARTESIAN_POINT('Ctrl Pts',(97.5652427832381,13.4416940047444,61.6991734005564));
#140603=CARTESIAN_POINT('Ctrl Pts',(97.5807492628728,13.4276733183867,61.6193998689467));
#140604=CARTESIAN_POINT('Ctrl Pts',(97.5961509203515,13.4113674093164,61.540165617543));
#140605=CARTESIAN_POINT('Ctrl Pts',(97.6005894255313,13.4066683136528,61.5173316053105));
#140606=CARTESIAN_POINT('Ctrl Pts',(97.6050192133311,13.4017791063397,61.4945424413528));
#140607=CARTESIAN_POINT('Ctrl Pts',(97.6094405582086,13.3966984044635,61.4717967133184));
#140608=CARTESIAN_POINT('Ctrl Pts',(97.6217225074074,13.3825848430778,61.4086118942317));
#140609=CARTESIAN_POINT('Ctrl Pts',(97.6339394170431,13.3669950677195,61.3457616858146));
#140610=CARTESIAN_POINT('Ctrl Pts',(97.6460994865771,13.3499001745025,61.2832038634467));
#140611=CARTESIAN_POINT('Ctrl Pts',(97.6654943689363,13.322634422283,61.183426341445));
#140612=CARTESIAN_POINT('Ctrl Pts',(97.6847450916549,13.2916668606854,61.0843903797846));
#140613=CARTESIAN_POINT('Ctrl Pts',(97.7037650545336,13.2570607508129,60.986541612079));
#140614=CARTESIAN_POINT('Ctrl Pts',(97.7226733142535,13.2226578806529,60.8892675046138));
#140615=CARTESIAN_POINT('Ctrl Pts',(97.7413534008831,13.1846592194458,60.793167275849));
#140616=CARTESIAN_POINT('Ctrl Pts',(97.7597222786598,13.1431769134627,60.698668092815));
#140617=CARTESIAN_POINT('Ctrl Pts',(97.7770207196428,13.1041119672744,60.6096758004973));
#140618=CARTESIAN_POINT('Ctrl Pts',(97.7940431028222,13.0619580618998,60.5221037113969));
#140619=CARTESIAN_POINT('Ctrl Pts',(97.810723134052,13.0168479924667,60.4362928354362));
#140620=CARTESIAN_POINT('Ctrl Pts',(97.8153555595118,13.0043198963704,60.4124611962112));
#140621=CARTESIAN_POINT('Ctrl Pts',(97.8199616014906,12.9915640125088,60.3887652855272));
#140622=CARTESIAN_POINT('Ctrl Pts',(97.824540077791,12.9785846860467,60.3652111844326));
#140623=CARTESIAN_POINT('Ctrl Pts',(97.84505639357,12.920423860736,60.2596644164161));
#140624=CARTESIAN_POINT('Ctrl Pts',(97.8650117626206,12.8576748931493,60.1570034319238));
#140625=CARTESIAN_POINT('Ctrl Pts',(97.8843730926296,12.7905931363591,60.0573985277848));
#140626=CARTESIAN_POINT('Ctrl Pts',(97.9037787186106,12.7233579060411,59.9575657417781));
#140627=CARTESIAN_POINT('Ctrl Pts',(97.9225876941704,12.6517700260684,59.860802443492));
#140628=CARTESIAN_POINT('Ctrl Pts',(97.9407669328909,12.5760343521528,59.7672788340814));
#140629=CARTESIAN_POINT('Ctrl Pts',(97.9541162592562,12.5204203496004,59.6986028458245));
#140630=CARTESIAN_POINT('Ctrl Pts',(97.9671260345575,12.4625686736672,59.6316736884987));
#140631=CARTESIAN_POINT('Ctrl Pts',(97.9797826669382,12.4025427161283,59.5665612844729));
#140632=CARTESIAN_POINT('Ctrl Pts',(97.9812479553316,12.3955933684475,59.5590230668007));
#140633=CARTESIAN_POINT('Ctrl Pts',(97.9827083599984,12.3886146548968,59.5515099735276));
#140634=CARTESIAN_POINT('Ctrl Pts',(97.9841638984601,12.3816064428523,59.5440219145336));
#140635=CARTESIAN_POINT('Ctrl Pts',(97.9960965004404,12.3241526502376,59.4826343044275));
#140636=CARTESIAN_POINT('Ctrl Pts',(98.007702617975,12.2647194408385,59.4229263001133));
#140637=CARTESIAN_POINT('Ctrl Pts',(98.0189889056623,12.2032956677188,59.3648636713558));
#140638=CARTESIAN_POINT('Ctrl Pts',(98.0302418362812,12.1420534349835,59.3069726489878));
#140639=CARTESIAN_POINT('Ctrl Pts',(98.0411768994689,12.0788318970064,59.2507169060417));
#140640=CARTESIAN_POINT('Ctrl Pts',(98.0517931981222,12.0135865599172,59.1961010571825));
#140641=CARTESIAN_POINT('Ctrl Pts',(98.062222148816,11.9494926204258,59.1424490252025));
#140642=CARTESIAN_POINT('Ctrl Pts',(98.0723435436394,11.8834451697451,59.0903792238159));
#140643=CARTESIAN_POINT('Ctrl Pts',(98.082148346113,11.8153772009759,59.0399381404546));
#140644=CARTESIAN_POINT('Ctrl Pts',(98.0903722575035,11.7582842666511,58.9976299959384));
#140645=CARTESIAN_POINT('Ctrl Pts',(98.0983733254029,11.6997692909013,58.9564682759002));
#140646=CARTESIAN_POINT('Ctrl Pts',(98.106141158279,11.63978271644,58.9165064395453));
#140647=CARTESIAN_POINT('Origin',(97.1688706058691,111.0726804259,63.738321366581));
#140648=CARTESIAN_POINT('',(98.1858652500691,10.88568327564,58.50636359317));
#140649=CARTESIAN_POINT('Ctrl Pts',(98.1061411591776,11.63978271644,58.91650643972));
#140650=CARTESIAN_POINT('Ctrl Pts',(98.108957693088,11.6180159291794,58.9020167011815));
#140651=CARTESIAN_POINT('Ctrl Pts',(98.111757780675,11.5959177554122,58.887611571194));
#140652=CARTESIAN_POINT('Ctrl Pts',(98.1145737776585,11.5732403953004,58.8731245948671));
#140653=CARTESIAN_POINT('Ctrl Pts',(98.1157390292683,11.5638565676433,58.8671299249208));
#140654=CARTESIAN_POINT('Ctrl Pts',(98.1169069832582,11.5543731003895,58.8611213525139));
#140655=CARTESIAN_POINT('Ctrl Pts',(98.1180781549355,11.5447817294967,58.8550962266101));
#140656=CARTESIAN_POINT('Ctrl Pts',(98.121010950369,11.5207634499409,58.8400083773408));
#140657=CARTESIAN_POINT('Ctrl Pts',(98.1239728709995,11.4960136689371,58.8247706926541));
#140658=CARTESIAN_POINT('Ctrl Pts',(98.1268620657231,11.4713264099956,58.8099071485045));
#140659=CARTESIAN_POINT('Ctrl Pts',(98.1270884423703,11.469392092844,58.8087425474262));
#140660=CARTESIAN_POINT('Ctrl Pts',(98.1273143750141,11.4674581802752,58.8075802305365));
#140661=CARTESIAN_POINT('Ctrl Pts',(98.1275398164358,11.4655250607335,58.8064204407522));
#140662=CARTESIAN_POINT('Ctrl Pts',(98.1283628179086,11.4584679715023,58.8021864863481));
#140663=CARTESIAN_POINT('Ctrl Pts',(98.1291792664275,11.4514214597892,58.7979862438015));
#140664=CARTESIAN_POINT('Ctrl Pts',(98.1299883415914,11.4443905815583,58.7938239336896));
#140665=CARTESIAN_POINT('Ctrl Pts',(98.1333240402532,11.4154032981102,58.7766633373815));
#140666=CARTESIAN_POINT('Ctrl Pts',(98.1365184813657,11.3868197450042,58.7602294445414));
#140667=CARTESIAN_POINT('Ctrl Pts',(98.1396491641854,11.3578775779917,58.7441235580485));
#140668=CARTESIAN_POINT('Ctrl Pts',(98.1401405593415,11.3533347860531,58.7415955617414));
#140669=CARTESIAN_POINT('Ctrl Pts',(98.1406303646256,11.3487831606216,58.7390757445758));
#140670=CARTESIAN_POINT('Ctrl Pts',(98.141119084895,11.3442187888434,58.7365615092952));
#140671=CARTESIAN_POINT('Ctrl Pts',(98.1434235917695,11.3226959939062,58.7247059083503));
#140672=CARTESIAN_POINT('Ctrl Pts',(98.1457009550164,11.3009021167795,58.7129899485201));
#140673=CARTESIAN_POINT('Ctrl Pts',(98.148004722259,11.2783989497205,58.7011381526501));
#140674=CARTESIAN_POINT('Ctrl Pts',(98.1490995696116,11.267704495687,58.6955056794158));
#140675=CARTESIAN_POINT('Ctrl Pts',(98.1502004020906,11.2568493114865,58.6898424155362));
#140676=CARTESIAN_POINT('Ctrl Pts',(98.1513132659929,11.2457821220828,58.6841172556582));
#140677=CARTESIAN_POINT('Ctrl Pts',(98.1515191903653,11.2437342489988,58.6830578718898));
#140678=CARTESIAN_POINT('Ctrl Pts',(98.1517255276039,11.2416791064181,58.6819963641191));
#140679=CARTESIAN_POINT('Ctrl Pts',(98.1519322820927,11.2396167148383,58.680932709793));
#140680=CARTESIAN_POINT('Ctrl Pts',(98.1541341104614,11.2176533112195,58.6696053413607));
#140681=CARTESIAN_POINT('Ctrl Pts',(98.156385810195,11.1948478916945,58.6580214082935));
#140682=CARTESIAN_POINT('Ctrl Pts',(98.1586590821498,11.171568427522,58.6463264963344));
#140683=CARTESIAN_POINT('Ctrl Pts',(98.1601802832843,11.1559905521009,58.6385006340118));
#140684=CARTESIAN_POINT('Ctrl Pts',(98.161711085333,11.1402017840564,58.6306253795112));
#140685=CARTESIAN_POINT('Ctrl Pts',(98.1632426453179,11.1243220713734,58.6227462257746));
#140686=CARTESIAN_POINT('Ctrl Pts',(98.1633263038242,11.1234546727363,58.6223158422186));
#140687=CARTESIAN_POINT('Ctrl Pts',(98.1634099653807,11.122586987239,58.6218854429707));
#140688=CARTESIAN_POINT('Ctrl Pts',(98.1634936289301,11.1217190315489,58.6214550334704));
#140689=CARTESIAN_POINT('Ctrl Pts',(98.1672305078062,11.0829513088304,58.6022305542108));
#140690=CARTESIAN_POINT('Ctrl Pts',(98.1709714100823,11.0436418556078,58.5829853763942));
#140691=CARTESIAN_POINT('Ctrl Pts',(98.174663363706,11.00463610201,58.5639920163024));
#140692=CARTESIAN_POINT('Ctrl Pts',(98.175041887474,11.0006369713794,58.5620446900463));
#140693=CARTESIAN_POINT('Ctrl Pts',(98.1754199002714,10.996640893791,58.5600999924886));
#140694=CARTESIAN_POINT('Ctrl Pts',(98.1757974296572,10.9926477485928,58.5581577818497));
#140695=CARTESIAN_POINT('Ctrl Pts',(98.1791845957236,10.9568215416152,58.5407324098953));
#140696=CARTESIAN_POINT('Ctrl Pts',(98.1825328300625,10.9212333134944,58.52350732206));
#140697=CARTESIAN_POINT('Ctrl Pts',(98.1858652500111,10.88568327564,58.5063635931587));
#140698=CARTESIAN_POINT('',(98.2872556700151,9.75862481052195,57.9847577051873));
#140699=CARTESIAN_POINT('Ctrl Pts',(98.1858652500691,10.88568327564,58.50636359317));
#140700=CARTESIAN_POINT('Ctrl Pts',(98.1966659246691,10.77045641959,58.45079921683));
#140701=CARTESIAN_POINT('Ctrl Pts',(98.2187284794691,10.53376517775,58.33729777984));
#140702=CARTESIAN_POINT('Ctrl Pts',(98.2525318077691,10.1617048254,58.1633955988));
#140703=CARTESIAN_POINT('Ctrl Pts',(98.2756771376691,9.89580942135701,58.044323793));
#140704=CARTESIAN_POINT('Ctrl Pts',(98.2872556111691,9.75862550816901,57.98475800809));
#140705=CARTESIAN_POINT('',(98.6928295681274,5.40399176655855E-8,55.8982712910719));
#140706=CARTESIAN_POINT('Ctrl Pts',(98.2872556700071,9.75862481052194,57.9847577051857));
#140707=CARTESIAN_POINT('Ctrl Pts',(98.2938324661056,9.68069541295108,57.9509231912672));
#140708=CARTESIAN_POINT('Ctrl Pts',(98.3005315104572,9.60020361132716,57.9164597677727));
#140709=CARTESIAN_POINT('Ctrl Pts',(98.3073332358664,9.51720250231419,57.8814680986399));
#140710=CARTESIAN_POINT('Ctrl Pts',(98.3114852418091,9.46653578510105,57.8601079863974));
#140711=CARTESIAN_POINT('Ctrl Pts',(98.315675509981,9.41493407546324,57.8385510330277));
#140712=CARTESIAN_POINT('Ctrl Pts',(98.3198995954507,9.36240953697897,57.8168201056097));
#140713=CARTESIAN_POINT('Ctrl Pts',(98.3272912721984,9.27049747398018,57.7787934150857));
#140714=CARTESIAN_POINT('Ctrl Pts',(98.3347860684279,9.17575904375019,57.740236223455));
#140715=CARTESIAN_POINT('Ctrl Pts',(98.3423907023324,9.07784748703031,57.7011139687803));
#140716=CARTESIAN_POINT('Ctrl Pts',(98.3462510395746,9.02814468297722,57.6812543544166));
#140717=CARTESIAN_POINT('Ctrl Pts',(98.3501396227374,8.97762411472197,57.6612494281096));
#140718=CARTESIAN_POINT('Ctrl Pts',(98.3540569257759,8.92624000370595,57.6410967515864));
#140719=CARTESIAN_POINT('Ctrl Pts',(98.3622776065608,8.81840755624538,57.5988052262606));
#140720=CARTESIAN_POINT('Ctrl Pts',(98.3706251328623,8.70677272130092,57.555861140571));
#140721=CARTESIAN_POINT('Ctrl Pts',(98.3790873026441,8.59108494554968,57.5123272682698));
#140722=CARTESIAN_POINT('Ctrl Pts',(98.3826010515574,8.54304788096543,57.4942506873886));
#140723=CARTESIAN_POINT('Ctrl Pts',(98.3861345253723,8.49431200908934,57.4760726311964));
#140724=CARTESIAN_POINT('Ctrl Pts',(98.3896865688376,8.44485924296572,57.4577990429139));
#140725=CARTESIAN_POINT('Ctrl Pts',(98.3987630183157,8.31849380356387,57.4111049913216));
#140726=CARTESIAN_POINT('Ctrl Pts',(98.4079611173156,8.18744778524474,57.3637851103391));
#140727=CARTESIAN_POINT('Ctrl Pts',(98.4172610042855,8.05137118275037,57.3159415782706));
#140728=CARTESIAN_POINT('Ctrl Pts',(98.4203655829907,8.00594476802641,57.2999699851403));
#140729=CARTESIAN_POINT('Ctrl Pts',(98.4234814533572,7.95995772525002,57.2839403017396));
#140730=CARTESIAN_POINT('Ctrl Pts',(98.4266076415366,7.91339695145371,57.2678575380585));
#140731=CARTESIAN_POINT('Ctrl Pts',(98.4365115964214,7.76588957933778,57.216906361488));
#140732=CARTESIAN_POINT('Ctrl Pts',(98.4465198842675,7.61262391526305,57.1654184410462));
#140733=CARTESIAN_POINT('Ctrl Pts',(98.4565927279828,7.45322050326538,57.1135984110812));
#140734=CARTESIAN_POINT('Ctrl Pts',(98.4592236929996,7.4115853094341,57.100063336989));
#140735=CARTESIAN_POINT('Ctrl Pts',(98.4618590112775,7.36953140210051,57.0865058674196));
#140736=CARTESIAN_POINT('Ctrl Pts',(98.4644977943282,7.32705180073446,57.0729305732268));
#140737=CARTESIAN_POINT('Ctrl Pts',(98.4737471702992,7.17815369256111,57.0253468963982));
#140738=CARTESIAN_POINT('Ctrl Pts',(98.4830399243306,7.02402682490015,56.9775400598888));
#140739=CARTESIAN_POINT('Ctrl Pts',(98.4923349328763,6.86431827542829,56.9297216249575));
#140740=CARTESIAN_POINT('Ctrl Pts',(98.4937450242413,6.84008982578176,56.9224673699615));
#140741=CARTESIAN_POINT('Ctrl Pts',(98.495155148829,6.81573291735723,56.9152129440496));
#140742=CARTESIAN_POINT('Ctrl Pts',(98.4965651426352,6.79124631741037,56.907959190947));
#140743=CARTESIAN_POINT('Ctrl Pts',(98.4986643177188,6.75479107890955,56.8971599252279));
#140744=CARTESIAN_POINT('Ctrl Pts',(98.5007632042589,6.71804838275074,56.8863621439284));
#140745=CARTESIAN_POINT('Ctrl Pts',(98.5028612343922,6.68101408690589,56.8755687684378));
#140746=CARTESIAN_POINT('Ctrl Pts',(98.5117937371179,6.52333811108084,56.8296152549685));
#140747=CARTESIAN_POINT('Ctrl Pts',(98.5207113052586,6.36037729196436,56.783738572884));
#140748=CARTESIAN_POINT('Ctrl Pts',(98.5295639120642,6.19183044120843,56.7381960862364));
#140749=CARTESIAN_POINT('Ctrl Pts',(98.5318613063152,6.14808981492023,56.7263770763899));
#140750=CARTESIAN_POINT('Ctrl Pts',(98.5341542738737,6.10397297544074,56.7145808397893));
#140751=CARTESIAN_POINT('Ctrl Pts',(98.536441828956,6.05947465891517,56.7028124478262));
#140752=CARTESIAN_POINT('Ctrl Pts',(98.5379673597325,6.02979950403509,56.6949643115041));
#140753=CARTESIAN_POINT('Ctrl Pts',(98.5394904824751,5.99995469400219,56.687128563381));
#140754=CARTESIAN_POINT('Ctrl Pts',(98.541010884844,5.96993866215367,56.6793068102967));
#140755=CARTESIAN_POINT('Ctrl Pts',(98.5490671310346,5.81089093427212,56.6378612234056));
#140756=CARTESIAN_POINT('Ctrl Pts',(98.557047457191,5.64703601870898,56.5968062092273));
#140757=CARTESIAN_POINT('Ctrl Pts',(98.5649017095693,5.47807690593747,56.5563997852451));
#140758=CARTESIAN_POINT('Ctrl Pts',(98.5683654825653,5.40356491115158,56.5385803068891));
#140759=CARTESIAN_POINT('Ctrl Pts',(98.5718046102653,5.32806022579709,56.5208876169778));
#140760=CARTESIAN_POINT('Ctrl Pts',(98.5752141681515,5.25153744002567,56.5033470498056));
#140761=CARTESIAN_POINT('Ctrl Pts',(98.5761510227838,5.23051104049898,56.4985273745994));
#140762=CARTESIAN_POINT('Ctrl Pts',(98.5770856425293,5.2094077745652,56.4937191968305));
#140763=CARTESIAN_POINT('Ctrl Pts',(98.5780179284323,5.18822710561756,56.4889230255777));
#140764=CARTESIAN_POINT('Ctrl Pts',(98.5896228921777,4.92457311873915,56.4292209606589));
#140765=CARTESIAN_POINT('Ctrl Pts',(98.6008697818594,4.64892682249802,56.3713610178423));
#140766=CARTESIAN_POINT('Ctrl Pts',(98.6114959693711,4.3619790174758,56.3166942950998));
#140767=CARTESIAN_POINT('Ctrl Pts',(98.6118749303484,4.35174561810061,56.3147447196141));
#140768=CARTESIAN_POINT('Ctrl Pts',(98.6122531015984,4.34149785024426,56.3127992069021));
#140769=CARTESIAN_POINT('Ctrl Pts',(98.6126304712299,4.33123575067178,56.3108578181371));
#140770=CARTESIAN_POINT('Ctrl Pts',(98.6185074083927,4.17141972598951,56.2806237483352));
#140771=CARTESIAN_POINT('Ctrl Pts',(98.624187943365,4.00812585773189,56.2514000749912));
#140772=CARTESIAN_POINT('Ctrl Pts',(98.6296439055601,3.84092052918692,56.2233317228906));
#140773=CARTESIAN_POINT('Ctrl Pts',(98.6343618715543,3.69633209072024,56.1990600131557));
#140774=CARTESIAN_POINT('Ctrl Pts',(98.6389117954758,3.54881871977499,56.1756528006555));
#140775=CARTESIAN_POINT('Ctrl Pts',(98.6432694545152,3.39810126942076,56.1532347002108));
#140776=CARTESIAN_POINT('Ctrl Pts',(98.6433517135133,3.39525619449609,56.1528115164634));
#140777=CARTESIAN_POINT('Ctrl Pts',(98.6434339037304,3.39240997828525,56.1523886865624));
#140778=CARTESIAN_POINT('Ctrl Pts',(98.6435160249773,3.38956261908564,56.1519662114799));
#140779=CARTESIAN_POINT('Ctrl Pts',(98.6483479194062,3.22202815546134,56.1271083936297));
#140780=CARTESIAN_POINT('Ctrl Pts',(98.6529418144172,3.05053624630029,56.1034749704414));
#140781=CARTESIAN_POINT('Ctrl Pts',(98.6572541559725,2.87474284373071,56.0812900070522));
#140782=CARTESIAN_POINT('Ctrl Pts',(98.6612410191838,2.71221762616855,56.0607794762317));
#140783=CARTESIAN_POINT('Ctrl Pts',(98.6649871771304,2.54601565953765,56.04150726062));
#140784=CARTESIAN_POINT('Ctrl Pts',(98.6684507060235,2.37587034056348,56.0236890380562));
#140785=CARTESIAN_POINT('Ctrl Pts',(98.6688289428818,2.35728951364044,56.0217431878175));
#140786=CARTESIAN_POINT('Ctrl Pts',(98.669203783092,2.33866168424419,56.0198148117289));
#140787=CARTESIAN_POINT('Ctrl Pts',(98.6695751687599,2.31998634897416,56.0179042076281));
#140788=CARTESIAN_POINT('Ctrl Pts',(98.6729603432827,2.14976096168309,56.000489081296));
#140789=CARTESIAN_POINT('Ctrl Pts',(98.6760593868739,1.97558797111138,55.9845459635106));
#140790=CARTESIAN_POINT('Ctrl Pts',(98.6788217101339,1.79709173088618,55.9703351132181));
#140791=CARTESIAN_POINT('Ctrl Pts',(98.6814391775938,1.62795580560928,55.9568694776945));
#140792=CARTESIAN_POINT('Ctrl Pts',(98.6837542976694,1.45493804794544,55.9449592770681));
#140793=CARTESIAN_POINT('Ctrl Pts',(98.6857145488864,1.27772726544477,55.9348747091783));
#140794=CARTESIAN_POINT('Ctrl Pts',(98.6858230330464,1.26792007200714,55.9343166093458));
#140795=CARTESIAN_POINT('Ctrl Pts',(98.6859304278319,1.25810003896687,55.9337641138303));
#140796=CARTESIAN_POINT('Ctrl Pts',(98.6860367234487,1.24826711449324,55.9332172730186));
#140797=CARTESIAN_POINT('Ctrl Pts',(98.6864430693246,1.21067790404311,55.9311268151483));
#140798=CARTESIAN_POINT('Ctrl Pts',(98.6868334406238,1.17290063339673,55.9291185389282));
#140799=CARTESIAN_POINT('Ctrl Pts',(98.6872072395185,1.13493594641422,55.9271955199121));
#140800=CARTESIAN_POINT('Ctrl Pts',(98.6892422221279,0.928254014288536,
55.9167264941582));
#140801=CARTESIAN_POINT('Ctrl Pts',(98.6907866121855,0.716014733679109,
55.9087813358087));
#140802=CARTESIAN_POINT('Ctrl Pts',(98.6917376176423,0.498367644923183,
55.9038888613311));
#140803=CARTESIAN_POINT('Ctrl Pts',(98.692450329743,0.335256368631961,55.900222293766));
#140804=CARTESIAN_POINT('Ctrl Pts',(98.6928296276282,0.1691084573483,55.898270985022));
#140805=CARTESIAN_POINT('Ctrl Pts',(98.6928295681199,5.40399167993425E-8,
55.8982712910703));
#140806=CARTESIAN_POINT('',(98.2872554315585,-9.75846368330451,57.9847589320145));
#140807=CARTESIAN_POINT('Ctrl Pts',(98.6928295681281,6.6572433925823E-14,
55.898271291072));
#140808=CARTESIAN_POINT('Ctrl Pts',(98.6928296474929,-0.233002523781841,
55.8982708828174));
#140809=CARTESIAN_POINT('Ctrl Pts',(98.6921101359835,-0.460828478822231,
55.901972430164));
#140810=CARTESIAN_POINT('Ctrl Pts',(98.6907814689873,-0.683286144820053,
55.9088077951516));
#140811=CARTESIAN_POINT('Ctrl Pts',(98.6895584056879,-0.888062667241723,
55.9150998789302));
#140812=CARTESIAN_POINT('Ctrl Pts',(98.6878190826087,-1.08829092549095,
55.924047875812));
#140813=CARTESIAN_POINT('Ctrl Pts',(98.6856443363506,-1.2838487345319,55.9352359196192));
#140814=CARTESIAN_POINT('Ctrl Pts',(98.6852103789473,-1.3228711072297,55.9374684257888));
#140815=CARTESIAN_POINT('Ctrl Pts',(98.6847590680062,-1.3617075926073,55.9397902077243));
#140816=CARTESIAN_POINT('Ctrl Pts',(98.6842910076255,-1.40035752210753,
55.9421981576195));
#140817=CARTESIAN_POINT('Ctrl Pts',(98.6821032008459,-1.58101493574617,
55.9534533916101));
#140818=CARTESIAN_POINT('Ctrl Pts',(98.6795477347256,-1.75758682047222,
55.966600059531));
#140819=CARTESIAN_POINT('Ctrl Pts',(98.67667745122,-1.93039577447675,55.9813663143511));
#140820=CARTESIAN_POINT('Ctrl Pts',(98.6737209928796,-2.10839299056471,
55.9965758980511));
#140821=CARTESIAN_POINT('Ctrl Pts',(98.670430508282,-2.28239809007581,56.0135038891433));
#140822=CARTESIAN_POINT('Ctrl Pts',(98.6668533640194,-2.4527727677904,56.0319066092901));
#140823=CARTESIAN_POINT('Ctrl Pts',(98.6658545410567,-2.50034539217089,
56.0370450823593));
#140824=CARTESIAN_POINT('Ctrl Pts',(98.6648333089686,-2.54763501352004,
56.042298839829));
#140825=CARTESIAN_POINT('Ctrl Pts',(98.6637905639107,-2.59464960347772,
56.0476632713666));
#140826=CARTESIAN_POINT('Ctrl Pts',(98.6633077144648,-2.61641999551992,
56.0501473040416));
#140827=CARTESIAN_POINT('Ctrl Pts',(98.662820251386,-2.6381314155892,56.0526550716774));
#140828=CARTESIAN_POINT('Ctrl Pts',(98.6623282582051,-2.65978465620982,
56.0551861445406));
#140829=CARTESIAN_POINT('Ctrl Pts',(98.6585713879635,-2.82512925543108,
56.0745134699746));
#140830=CARTESIAN_POINT('Ctrl Pts',(98.6545512559065,-2.9870775460763,56.0951951515127));
#140831=CARTESIAN_POINT('Ctrl Pts',(98.6502908550547,-3.14611017159622,
56.1171129019404));
#140832=CARTESIAN_POINT('Ctrl Pts',(98.6459153901131,-3.30943791979361,
56.1396226027721));
#140833=CARTESIAN_POINT('Ctrl Pts',(98.6412864794858,-3.46969054367775,
56.1634361641968));
#140834=CARTESIAN_POINT('Ctrl Pts',(98.6364185581575,-3.6273878627602,56.1884793274269));
#140835=CARTESIAN_POINT('Ctrl Pts',(98.6348423095874,-3.67845076147005,
56.1965883841619));
#140836=CARTESIAN_POINT('Ctrl Pts',(98.6332409224524,-3.72924572385145,
56.2048267671867));
#140837=CARTESIAN_POINT('Ctrl Pts',(98.6316146662119,-3.77979033808198,
56.2131930889267));
#140838=CARTESIAN_POINT('Ctrl Pts',(98.631368185853,-3.7874510340703,56.2144611141826));
#140839=CARTESIAN_POINT('Ctrl Pts',(98.6311211340222,-3.79510597914968,
56.2157320793639));
#140840=CARTESIAN_POINT('Ctrl Pts',(98.6308735113466,-3.80275523505594,
56.2170059812372));
#140841=CARTESIAN_POINT('Ctrl Pts',(98.6255167623133,-3.96822935443883,
56.2445639284743));
#140842=CARTESIAN_POINT('Ctrl Pts',(98.6199010201482,-4.13104773944181,
56.2734542528777));
#140843=CARTESIAN_POINT('Ctrl Pts',(98.614091333514,-4.29051457498224,56.3033423413468));
#140844=CARTESIAN_POINT('Ctrl Pts',(98.6080973471629,-4.45504015026177,
56.3341785646449));
#140845=CARTESIAN_POINT('Ctrl Pts',(98.60189696042,-4.61599801174581,56.3660766493794));
#140846=CARTESIAN_POINT('Ctrl Pts',(98.5955713922438,-4.77264457106099,
56.3986187291727));
#140847=CARTESIAN_POINT('Ctrl Pts',(98.5944765483748,-4.79975731734657,
56.4042511870888));
#140848=CARTESIAN_POINT('Ctrl Pts',(98.5933779763023,-4.82674095913177,
56.4099028241245));
#140849=CARTESIAN_POINT('Ctrl Pts',(98.5922761238409,-4.85359170514252,
56.4155713353442));
#140850=CARTESIAN_POINT('Ctrl Pts',(98.5921063773628,-4.85772821137103,
56.4164446009122));
#140851=CARTESIAN_POINT('Ctrl Pts',(98.5919365365544,-4.86186154246186,
56.4173183517196));
#140852=CARTESIAN_POINT('Ctrl Pts',(98.5917665996274,-4.8659917644681,56.4181925969701));
#140853=CARTESIAN_POINT('Ctrl Pts',(98.5875838950192,-4.9676500615998,56.439710637237));
#140854=CARTESIAN_POINT('Ctrl Pts',(98.5833437983902,-5.06742568600838,
56.4615239092009));
#140855=CARTESIAN_POINT('Ctrl Pts',(98.5790151557521,-5.16630175587408,
56.4837927191261));
#140856=CARTESIAN_POINT('Ctrl Pts',(98.5746405785477,-5.26622707599619,
56.5062978405731));
#140857=CARTESIAN_POINT('Ctrl Pts',(98.5701755389641,-5.36523370042368,
56.5292683593524));
#140858=CARTESIAN_POINT('Ctrl Pts',(98.5655779015931,-5.4643255132017,56.5529210461131));
#140859=CARTESIAN_POINT('Ctrl Pts',(98.5609687180466,-5.56366617802217,
56.5766331325279));
#140860=CARTESIAN_POINT('Ctrl Pts',(98.5562262616802,-5.66309253484219,
56.6010308600264));
#140861=CARTESIAN_POINT('Ctrl Pts',(98.5512983893228,-5.76360426017417,
56.6263824488875));
#140862=CARTESIAN_POINT('Ctrl Pts',(98.5503261219759,-5.78343518545595,
56.6313843077533));
#140863=CARTESIAN_POINT('Ctrl Pts',(98.5493466068255,-5.80330832208338,
56.6364234523898));
#140864=CARTESIAN_POINT('Ctrl Pts',(98.5483593988895,-5.82323128918212,
56.6415021715976));
#140865=CARTESIAN_POINT('Ctrl Pts',(98.5476218816008,-5.83811521802843,
56.6452963501927));
#140866=CARTESIAN_POINT('Ctrl Pts',(98.5468803236845,-5.85302723303626,
56.6491113152531));
#140867=CARTESIAN_POINT('Ctrl Pts',(98.5461347475265,-5.86796609953466,
56.6529469518745));
#140868=CARTESIAN_POINT('Ctrl Pts',(98.539662373568,-5.99765094721716,56.6862442539868));
#140869=CARTESIAN_POINT('Ctrl Pts',(98.5328863818807,-6.12935871916372,
56.7211035119263));
#140870=CARTESIAN_POINT('Ctrl Pts',(98.5258273229773,-6.26228133553224,
56.7574190434097));
#140871=CARTESIAN_POINT('Ctrl Pts',(98.5187946772217,-6.39470659031704,
56.7935986916948));
#140872=CARTESIAN_POINT('Ctrl Pts',(98.5114810749149,-6.52833747013118,
56.8312237430612));
#140873=CARTESIAN_POINT('Ctrl Pts',(98.5039165891754,-6.66238366461827,
56.8701394614732));
#140874=CARTESIAN_POINT('Ctrl Pts',(98.500829836016,-6.71708236174012,56.8860193534973));
#140875=CARTESIAN_POINT('Ctrl Pts',(98.4977014210483,-6.77185032717012,
56.9021135744207));
#140876=CARTESIAN_POINT('Ctrl Pts',(98.4945338538751,-6.82663436643004,
56.9184092135179));
#140877=CARTESIAN_POINT('Ctrl Pts',(98.493003329194,-6.85310525706257,56.9262830411173));
#140878=CARTESIAN_POINT('Ctrl Pts',(98.4914635315537,-6.87957978561574,
56.93420457341));
#140879=CARTESIAN_POINT('Ctrl Pts',(98.4899146152936,-6.90605554898886,
56.9421730165938));
#140880=CARTESIAN_POINT('Ctrl Pts',(98.4799287769744,-7.0767443713754,56.9935454421638));
#140881=CARTESIAN_POINT('Ctrl Pts',(98.4695631611305,-7.24748321033599,
57.046871644524));
#140882=CARTESIAN_POINT('Ctrl Pts',(98.4588614968984,-7.41761929184993,
57.1019266614792));
#140883=CARTESIAN_POINT('Ctrl Pts',(98.4499447236189,-7.55937900628529,
57.1477992560068));
#140884=CARTESIAN_POINT('Ctrl Pts',(98.4407948299866,-7.70072045197103,
57.1948711448736));
#140885=CARTESIAN_POINT('Ctrl Pts',(98.4314420591005,-7.84127558167099,
57.242986739758));
#140886=CARTESIAN_POINT('Ctrl Pts',(98.4289556404352,-7.87864193034442,
57.2557781910477));
#140887=CARTESIAN_POINT('Ctrl Pts',(98.4264548838178,-7.91595286969873,
57.2686434042667));
#140888=CARTESIAN_POINT('Ctrl Pts',(98.4239404978578,-7.95319956841815,
57.2815787339915));
#140889=CARTESIAN_POINT('Ctrl Pts',(98.4133514625485,-8.11005957883956,
57.3360543257941));
#140890=CARTESIAN_POINT('Ctrl Pts',(98.4025199853583,-8.26577859095142,
57.3917771663333));
#140891=CARTESIAN_POINT('Ctrl Pts',(98.3914982332011,-8.41970398105144,
57.4484788828979));
#140892=CARTESIAN_POINT('Ctrl Pts',(98.381644947558,-8.55731103433506,57.4991693903411));
#140893=CARTESIAN_POINT('Ctrl Pts',(98.3716397225239,-8.6934847827116,57.5506415552392));
#140894=CARTESIAN_POINT('Ctrl Pts',(98.3615259095763,-8.82777412625757,
57.6026723526391));
#140895=CARTESIAN_POINT('Ctrl Pts',(98.3580260822914,-8.87424418765305,
57.6206773133141));
#140896=CARTESIAN_POINT('Ctrl Pts',(98.3545128408008,-8.92048773989161,
57.6387512835947));
#140897=CARTESIAN_POINT('Ctrl Pts',(98.3509861898095,-8.96651232671047,
57.656894239467));
#140898=CARTESIAN_POINT('Ctrl Pts',(98.3363782376875,-9.15715352210037,
57.7320452627451));
#140899=CARTESIAN_POINT('Ctrl Pts',(98.3215409859264,-9.34403834396314,
57.8083759256478));
#140900=CARTESIAN_POINT('Ctrl Pts',(98.3064659623698,-9.52768824794068,
57.8859298118043));
#140901=CARTESIAN_POINT('Ctrl Pts',(98.3001053609739,-9.60517561180472,
57.9186521060475));
#140902=CARTESIAN_POINT('Ctrl Pts',(98.293702309927,-9.68208699449254,57.9515927836448));
#140903=CARTESIAN_POINT('Ctrl Pts',(98.2872556496088,-9.75846110048999,
57.9847578103677));
#140904=CARTESIAN_POINT('',(98.1858622879398,-10.8854244761627,58.5063788330415));
#140905=CARTESIAN_POINT('Ctrl Pts',(98.287255431523,-9.75846368326178,57.9847589321044));
#140906=CARTESIAN_POINT('Ctrl Pts',(98.2752326904077,-9.90087388729895,
58.0466102646848));
#140907=CARTESIAN_POINT('Ctrl Pts',(98.2514522368865,-10.1736221482937,
58.1689494817128));
#140908=CARTESIAN_POINT('Ctrl Pts',(98.2176663389691,-10.54488259149,58.34276199094));
#140909=CARTESIAN_POINT('Ctrl Pts',(98.1962080794691,-10.77506402066,58.45315461531));
#140910=CARTESIAN_POINT('Ctrl Pts',(98.1858622898691,-10.88542445529,58.50637882297));
#140911=CARTESIAN_POINT('',(98.1061703786691,-11.63926799201,58.91635611737));
#140912=CARTESIAN_POINT('Ctrl Pts',(98.1858622879714,-10.8854244761627,
58.5063788330476));
#140913=CARTESIAN_POINT('Ctrl Pts',(98.1822193745813,-10.9242853208731,
58.5251199041985));
#140914=CARTESIAN_POINT('Ctrl Pts',(98.1785918743415,-10.9628736870434,
58.5437816819218));
#140915=CARTESIAN_POINT('Ctrl Pts',(98.1749505020994,-11.0013736886429,
58.5625148246342));
#140916=CARTESIAN_POINT('Ctrl Pts',(98.1749372589513,-11.0015137076219,
58.5625829543851));
#140917=CARTESIAN_POINT('Ctrl Pts',(98.1749240156201,-11.0016537254113,
58.5626510850778));
#140918=CARTESIAN_POINT('Ctrl Pts',(98.1749107721045,-11.0017937420141,
58.5627192167188));
#140919=CARTESIAN_POINT('Ctrl Pts',(98.1712560546698,-11.0404331137333,
58.5815210141535));
#140920=CARTESIAN_POINT('Ctrl Pts',(98.1675872573881,-11.0789841252467,
58.6003952458404));
#140921=CARTESIAN_POINT('Ctrl Pts',(98.1639481760854,-11.116772737625,58.6191166027382));
#140922=CARTESIAN_POINT('Ctrl Pts',(98.1639103076985,-11.1171659670351,
58.6193114177278));
#140923=CARTESIAN_POINT('Ctrl Pts',(98.1638724425624,-11.1175591133193,
58.6195062159939));
#140924=CARTESIAN_POINT('Ctrl Pts',(98.1638345806645,-11.1179521764361,
58.6197009976006));
#140925=CARTESIAN_POINT('Ctrl Pts',(98.1602339848412,-11.1553317452324,
58.6382243648567));
#140926=CARTESIAN_POINT('Ctrl Pts',(98.1566627809925,-11.1919582746467,
58.6565965241752));
#140927=CARTESIAN_POINT('Ctrl Pts',(98.1531490508319,-11.2272122368966,
58.6746730085577));
#140928=CARTESIAN_POINT('Ctrl Pts',(98.153061326564,-11.2280923921411,58.6751243085397));
#140929=CARTESIAN_POINT('Ctrl Pts',(98.1529736355007,-11.2289717013682,
58.6755754376997));
#140930=CARTESIAN_POINT('Ctrl Pts',(98.1528859765534,-11.2298501688127,
58.6760264016383));
#140931=CARTESIAN_POINT('Ctrl Pts',(98.1503402480423,-11.2553619926082,
58.6891229740981));
#140932=CARTESIAN_POINT('Ctrl Pts',(98.1478217144922,-11.2801692510307,
58.702079641213));
#140933=CARTESIAN_POINT('Ctrl Pts',(98.1452503468445,-11.3048609610118,
58.7153081150659));
#140934=CARTESIAN_POINT('Ctrl Pts',(98.1443264877432,-11.3137323726955,
58.7200609344367));
#140935=CARTESIAN_POINT('Ctrl Pts',(98.1433957829007,-11.3225883365942,
58.7248489719439));
#140936=CARTESIAN_POINT('Ctrl Pts',(98.1424543184985,-11.3314550087017,
58.7296923622527));
#140937=CARTESIAN_POINT('Ctrl Pts',(98.1423123309019,-11.3327922419092,
58.7304228214688));
#140938=CARTESIAN_POINT('Ctrl Pts',(98.1421701018987,-11.3341298086781,
58.731154522607));
#140939=CARTESIAN_POINT('Ctrl Pts',(98.1420276323736,-11.3354676606157,
58.7318874611152));
#140940=CARTESIAN_POINT('Ctrl Pts',(98.1397828557107,-11.3565471076515,
58.7434357782575));
#140941=CARTESIAN_POINT('Ctrl Pts',(98.1374784063472,-11.3776920623505,
58.7552910832167));
#140942=CARTESIAN_POINT('Ctrl Pts',(98.135115269475,-11.3988808424873,58.7674483078894));
#140943=CARTESIAN_POINT('Ctrl Pts',(98.1337707147605,-11.4109366292514,
58.7743654077578));
#140944=CARTESIAN_POINT('Ctrl Pts',(98.1324071370899,-11.4230079261992,
58.7813803717716));
#140945=CARTESIAN_POINT('Ctrl Pts',(98.1310252011188,-11.435094523445,58.7884897805351));
#140946=CARTESIAN_POINT('Ctrl Pts',(98.1308171645218,-11.4369140394091,
58.7895600307038));
#140947=CARTESIAN_POINT('Ctrl Pts',(98.1306087354596,-11.438733601095,58.7906322999199));
#140948=CARTESIAN_POINT('Ctrl Pts',(98.1303998967675,-11.4405534015101,
58.7917066764878));
#140949=CARTESIAN_POINT('Ctrl Pts',(98.1271948586614,-11.4684817974332,
58.8081950858267));
#140950=CARTESIAN_POINT('Ctrl Pts',(98.1238938833199,-11.496462789953,58.8251770470384));
#140951=CARTESIAN_POINT('Ctrl Pts',(98.1205589506922,-11.5240776285944,
58.8423337024545));
#140952=CARTESIAN_POINT('Ctrl Pts',(98.1199696640494,-11.5289572040972,
58.8453653042888));
#140953=CARTESIAN_POINT('Ctrl Pts',(98.1193793015924,-11.5338254501362,
58.8484024406795));
#140954=CARTESIAN_POINT('Ctrl Pts',(98.1187881861463,-11.538680182265,58.8514434508447));
#140955=CARTESIAN_POINT('Ctrl Pts',(98.1185110438627,-11.5409563054102,
58.852869217177));
#140956=CARTESIAN_POINT('Ctrl Pts',(98.1182337152748,-11.5432295396573,
58.8542959419573));
#140957=CARTESIAN_POINT('Ctrl Pts',(98.1179562112343,-11.5454998274262,
58.8557235693581));
#140958=CARTESIAN_POINT('Ctrl Pts',(98.1145024686386,-11.5737552342998,
58.8734914460235));
#140959=CARTESIAN_POINT('Ctrl Pts',(98.1110218674615,-11.6015576167855,
58.8913974974267));
#140960=CARTESIAN_POINT('Ctrl Pts',(98.1074882690966,-11.6290487900927,
58.9095761943874));
#140961=CARTESIAN_POINT('Ctrl Pts',(98.1070498095344,-11.6324599779435,
58.9118318620347));
#140962=CARTESIAN_POINT('Ctrl Pts',(98.106610530279,-11.6358663095293,58.9140917466174));
#140963=CARTESIAN_POINT('Ctrl Pts',(98.1061703789843,-11.63926799201,58.9163561174312));
#140964=CARTESIAN_POINT('',(97.4550855056363,-13.496463426129,62.2658808648332));
#140965=CARTESIAN_POINT('Ctrl Pts',(98.1061703781116,-11.63926799201,58.9163561172616));
#140966=CARTESIAN_POINT('Ctrl Pts',(98.0966576593874,-11.7127292568203,
58.9652945684228));
#140967=CARTESIAN_POINT('Ctrl Pts',(98.0867888698576,-11.7839934899085,
59.016064839334));
#140968=CARTESIAN_POINT('Ctrl Pts',(98.0765879384257,-11.8531333041328,
59.068543821195));
#140969=CARTESIAN_POINT('Ctrl Pts',(98.0662437675195,-11.9232439660403,
59.1217597026055));
#140970=CARTESIAN_POINT('Ctrl Pts',(98.0555579974791,-11.9911706438039,
59.176732947));
#140971=CARTESIAN_POINT('Ctrl Pts',(98.0445455451492,-12.0569745023016,
59.2333868161265));
#140972=CARTESIAN_POINT('Ctrl Pts',(98.0334164928612,-12.1234750927278,
59.2906405370001));
#140973=CARTESIAN_POINT('Ctrl Pts',(98.021953738878,-12.1878082086981,59.3496109954792));
#140974=CARTESIAN_POINT('Ctrl Pts',(98.0101634916104,-12.2500142572324,
59.4102662590643));
#140975=CARTESIAN_POINT('Ctrl Pts',(98.0003308970524,-12.301891613187,59.4608503224098));
#140976=CARTESIAN_POINT('Ctrl Pts',(97.9902703516646,-12.3522893588823,
59.5126070912772));
#140977=CARTESIAN_POINT('Ctrl Pts',(97.9799811312989,-12.4012149719552,
59.5655402787358));
#140978=CARTESIAN_POINT('Ctrl Pts',(97.9791397502712,-12.405215769017,59.5698687874157));
#140979=CARTESIAN_POINT('Ctrl Pts',(97.9782968381121,-12.4092067130191,
59.5742051729851));
#140980=CARTESIAN_POINT('Ctrl Pts',(97.9774523937125,-12.4131878324592,
59.5785494411326));
#140981=CARTESIAN_POINT('Ctrl Pts',(97.9642635778662,-12.4753662910788,
59.6463996780582));
#140982=CARTESIAN_POINT('Ctrl Pts',(97.9507110349178,-12.5351261696814,
59.7161210881153));
#140983=CARTESIAN_POINT('Ctrl Pts',(97.9367891102262,-12.5924643940136,
59.7877427208916));
#140984=CARTESIAN_POINT('Ctrl Pts',(97.9228467908142,-12.6498866151409,
59.8594692747337));
#140985=CARTESIAN_POINT('Ctrl Pts',(97.9085339122914,-12.7048802027885,
59.9331021117221));
#140986=CARTESIAN_POINT('Ctrl Pts',(97.8938417282283,-12.7573923544939,
60.0086863934301));
#140987=CARTESIAN_POINT('Ctrl Pts',(97.87921585619,-12.8096674967059,60.0839295313886));
#140988=CARTESIAN_POINT('Ctrl Pts',(97.8642140129851,-12.8594836321143,
60.1611070065553));
#140989=CARTESIAN_POINT('Ctrl Pts',(97.8488258520106,-12.9067380051098,
60.2402720326482));
#140990=CARTESIAN_POINT('Ctrl Pts',(97.8390598470948,-12.9367277121149,
60.2905136460074));
#140991=CARTESIAN_POINT('Ctrl Pts',(97.8291382141621,-12.965684591652,60.3415559413888));
#140992=CARTESIAN_POINT('Ctrl Pts',(97.8190581603176,-12.993571479285,60.3934130640865));
#140993=CARTESIAN_POINT('Ctrl Pts',(97.813338575709,-13.009394947666,60.4228376292132));
#140994=CARTESIAN_POINT('Ctrl Pts',(97.8075699015489,-13.0249019223777,
60.4525146740103));
#140995=CARTESIAN_POINT('Ctrl Pts',(97.8017575137646,-13.0400726694135,
60.4824165743383));
#140996=CARTESIAN_POINT('Ctrl Pts',(97.7893783643013,-13.0723831332008,
60.5461012607575));
#140997=CARTESIAN_POINT('Ctrl Pts',(97.7768006366382,-13.1031654309393,
60.6108074090894));
#140998=CARTESIAN_POINT('Ctrl Pts',(97.7640835268832,-13.1322806911523,
60.6762307023581));
#140999=CARTESIAN_POINT('Ctrl Pts',(97.7512575615967,-13.1616451712891,
60.7422140039539));
#141000=CARTESIAN_POINT('Ctrl Pts',(97.7382898944951,-13.1893137939528,
60.8089263874268));
#141001=CARTESIAN_POINT('Ctrl Pts',(97.7252453091653,-13.2151926323364,
60.8760346476848));
#141002=CARTESIAN_POINT('Ctrl Pts',(97.7121335901379,-13.2412046556442,
60.9434882792618));
#141003=CARTESIAN_POINT('Ctrl Pts',(97.6989442439426,-13.2654083480943,
61.011341438086));
#141004=CARTESIAN_POINT('Ctrl Pts',(97.6857459106975,-13.287758912407,61.0792409073627));
#141005=CARTESIAN_POINT('Ctrl Pts',(97.6724397736567,-13.3102920358071,
61.1476949785263));
#141006=CARTESIAN_POINT('Ctrl Pts',(97.6591245885233,-13.3309415965499,
61.2161956772425));
#141007=CARTESIAN_POINT('Ctrl Pts',(97.6458722845238,-13.3497138986142,
61.2843726625986));
#141008=CARTESIAN_POINT('Ctrl Pts',(97.6428236518917,-13.3540323818497,
61.3000564699068));
#141009=CARTESIAN_POINT('Ctrl Pts',(97.6397783505005,-13.3582517361044,
61.3157231270329));
#141010=CARTESIAN_POINT('Ctrl Pts',(97.6367372604432,-13.3623724257183,
61.3313681010267));
#141011=CARTESIAN_POINT('Ctrl Pts',(97.62311532789,-13.3808302007058,61.4014465191353));
#141012=CARTESIAN_POINT('Ctrl Pts',(97.6095678838933,-13.3971449365558,
61.4711414460592));
#141013=CARTESIAN_POINT('Ctrl Pts',(97.5960759980443,-13.4115039866449,
61.540550717809));
#141014=CARTESIAN_POINT('Ctrl Pts',(97.5826014167824,-13.4258446199289,
61.6098709657708));
#141015=CARTESIAN_POINT('Ctrl Pts',(97.5691821716715,-13.43823474134,61.6789066596063));
#141016=CARTESIAN_POINT('Ctrl Pts',(97.5557971529493,-13.4488343816429,
61.7477663459257));
#141017=CARTESIAN_POINT('Ctrl Pts',(97.5422439188024,-13.4595672322934,
61.8174914222474));
#141018=CARTESIAN_POINT('Ctrl Pts',(97.5287256767822,-13.4684643880439,
61.8870365323244));
#141019=CARTESIAN_POINT('Ctrl Pts',(97.515216014868,-13.4756434557848,61.9565374549115));
#141020=CARTESIAN_POINT('Ctrl Pts',(97.5015833205085,-13.4828879032713,
62.0266713221648));
#141021=CARTESIAN_POINT('Ctrl Pts',(97.4879592676874,-13.4883829249004,
62.0967606847404));
#141022=CARTESIAN_POINT('Ctrl Pts',(97.4743136522677,-13.4921990177858,
62.1669609501112));
#141023=CARTESIAN_POINT('Ctrl Pts',(97.4679101303506,-13.4939898079903,
62.1999040548421));
#141024=CARTESIAN_POINT('Ctrl Pts',(97.4615018253202,-13.4954101432466,
62.2328717624063));
#141025=CARTESIAN_POINT('Ctrl Pts',(97.4550854749278,-13.4964634261277,
62.2658808588604));
#141026=CARTESIAN_POINT('',(97.4550855974691,-13.49646342613,62.26588088268));
#141027=CARTESIAN_POINT('Origin',(98.9275259828691,-15.39012394141,62.55209572828));
#141028=CARTESIAN_POINT('',(97.4408144041081,-13.4984402470751,62.3529940555964));
#141029=CARTESIAN_POINT('Origin',(98.6415803004823,-11.8684041259695,62.3485284784612));
#141030=CARTESIAN_POINT('Ctrl Pts',(97.4408111863691,-13.49844024719,62.35299362778));
#141031=CARTESIAN_POINT('Ctrl Pts',(97.4173636613705,-13.4950477422291,
62.527984492391));
#141032=CARTESIAN_POINT('Ctrl Pts',(97.4236570627935,-13.4751288891508,
62.7187077839406));
#141033=CARTESIAN_POINT('Ctrl Pts',(97.4949557198421,-13.420461087357,63.0077137348997));
#141034=CARTESIAN_POINT('Ctrl Pts',(97.5289803287109,-13.3981068997297,
63.1043922603008));
#141035=CARTESIAN_POINT('Ctrl Pts',(97.5966941058591,-13.3583782377447,
63.2460891480223));
#141036=CARTESIAN_POINT('Ctrl Pts',(97.6220365677761,-13.3441024536591,
63.2927595285971));
#141037=CARTESIAN_POINT('Ctrl Pts',(97.664279676,-13.3211394323945,63.3613732688597));
#141038=CARTESIAN_POINT('Ctrl Pts',(97.6864575470268,-13.3092705854783,
63.3953315107788));
#141039=CARTESIAN_POINT('Ctrl Pts',(97.7102234673853,-13.296820734136,63.4286582671533));
#141040=CARTESIAN_POINT('Ctrl Pts',(97.7264199637094,-13.2883917211465,
63.4507233650114));
#141041=CARTESIAN_POINT('Ctrl Pts',(97.7358935390684,-13.2834963577579,
63.4632223753341));
#141042=CARTESIAN_POINT('Ctrl Pts',(97.8011573536291,-13.249950498071,63.547199335367));
#141043=CARTESIAN_POINT('Ctrl Pts',(97.8662462666935,-13.2196202737384,
63.616343275454));
#141044=CARTESIAN_POINT('Ctrl Pts',(97.9727587025035,-13.1733574136564,
63.7099617869203));
#141045=CARTESIAN_POINT('Ctrl Pts',(98.009738986224,-13.1578085396986,63.7394884174016));
#141046=CARTESIAN_POINT('Ctrl Pts',(98.0671760684826,-13.1342933478661,
63.7810613979237));
#141047=CARTESIAN_POINT('Ctrl Pts',(98.0963859781652,-13.1224877817258,
63.8011690100459));
#141048=CARTESIAN_POINT('Ctrl Pts',(98.1262839966426,-13.1106102602497,
63.8202246363938));
#141049=CARTESIAN_POINT('Ctrl Pts',(98.1463633209196,-13.1026759225243,
63.8326911146773));
#141050=CARTESIAN_POINT('Ctrl Pts',(98.1579299503343,-13.0981323525652,
63.8396610984129));
#141051=CARTESIAN_POINT('Ctrl Pts',(98.3063545768017,-13.0400815536355,
63.927021476433));
#141052=CARTESIAN_POINT('Ctrl Pts',(98.466686355582,-12.9953063983198,63.9905955773411));
#141053=CARTESIAN_POINT('Ctrl Pts',(98.6413367350691,-12.96039213374,64.024539984441));
#141054=CARTESIAN_POINT('Ctrl Pts',(95.3600739029692,-14.83896505265,61.68126243292));
#141055=CARTESIAN_POINT('Ctrl Pts',(95.3488967629692,-14.83942460114,61.7270366935901));
#141056=CARTESIAN_POINT('Ctrl Pts',(95.2537938103691,-14.84221155252,62.15207107076));
#141057=CARTESIAN_POINT('Ctrl Pts',(95.2173222593691,-14.82409468882,63.006826791351));
#141058=CARTESIAN_POINT('Ctrl Pts',(95.5518922378691,-14.73065279882,64.161325047946));
#141059=CARTESIAN_POINT('Ctrl Pts',(96.2081398692692,-14.58918963245,65.112261313913));
#141060=CARTESIAN_POINT('Ctrl Pts',(97.039871915969,-14.44338212505,65.761701368215));
#141061=CARTESIAN_POINT('Ctrl Pts',(97.8878639618691,-14.33215462512,66.111820330221));
#141062=CARTESIAN_POINT('Ctrl Pts',(98.4384132164691,-14.28651698832,66.202335719855));
#141063=CARTESIAN_POINT('Ctrl Pts',(98.6904498008691,-14.27205827794,66.217885926039));
#141064=CARTESIAN_POINT('Ctrl Pts',(96.6132510546691,-15.48406398727,61.9746008524));
#141065=CARTESIAN_POINT('Ctrl Pts',(96.605261792769,-15.48455020164,62.00674475245));
#141066=CARTESIAN_POINT('Ctrl Pts',(96.5374119126691,-15.48745755549,62.30580352411));
#141067=CARTESIAN_POINT('Ctrl Pts',(96.5166513377691,-15.46857722262,62.91670103595));
#141068=CARTESIAN_POINT('Ctrl Pts',(96.7844491779691,-15.3710316785,63.73087440493));
#141069=CARTESIAN_POINT('Ctrl Pts',(97.2789917563691,-15.22554231463,64.359787283689));
#141070=CARTESIAN_POINT('Ctrl Pts',(97.8582212558691,-15.079599962,64.7398975319179));
#141071=CARTESIAN_POINT('Ctrl Pts',(98.3940856313691,-14.97191574057,64.908401892465));
#141072=CARTESIAN_POINT('Ctrl Pts',(98.7117257326691,-14.92907221933,64.938374720735));
#141073=CARTESIAN_POINT('Ctrl Pts',(98.8530540086691,-14.91555874585,64.9403245206161));
#141074=CARTESIAN_POINT('Ctrl Pts',(97.7223056686691,-14.60855129545,62.25049179));
#141075=CARTESIAN_POINT('Ctrl Pts',(97.7180946320691,-14.60900131952,62.26739880163));
#141076=CARTESIAN_POINT('Ctrl Pts',(97.6823397918691,-14.61174526606,62.4247344993));
#141077=CARTESIAN_POINT('Ctrl Pts',(97.6717261099691,-14.5939010951,62.74672635053));
#141078=CARTESIAN_POINT('Ctrl Pts',(97.8146542530691,-14.50192493123,63.1751821767));
#141079=CARTESIAN_POINT('Ctrl Pts',(98.076899205869,-14.36189982535,63.503526109119));
#141080=CARTESIAN_POINT('Ctrl Pts',(98.3812567346691,-14.21614048141,63.698666180833));
#141081=CARTESIAN_POINT('Ctrl Pts',(98.6593498648691,-14.10364740799,63.782416805214));
#141082=CARTESIAN_POINT('Ctrl Pts',(98.8220717947691,-14.05701178061,63.7960633438949));
#141083=CARTESIAN_POINT('Ctrl Pts',(98.8941584479691,-14.04221545444,63.7965231491));
#141084=CARTESIAN_POINT('Ctrl Pts',(97.438659219569,-13.19808298716,62.19833602395));
#141085=CARTESIAN_POINT('Ctrl Pts',(97.4345632129691,-13.19847470795,62.21555337483));
#141086=CARTESIAN_POINT('Ctrl Pts',(97.3996126441691,-13.20095540206,62.37497098533));
#141087=CARTESIAN_POINT('Ctrl Pts',(97.3821583556691,-13.1847805085,62.68826097786));
#141088=CARTESIAN_POINT('Ctrl Pts',(97.4826980927691,-13.10177672665,63.119849099336));
#141089=CARTESIAN_POINT('Ctrl Pts',(97.7035745284691,-12.97055464874,63.507460358022));
#141090=CARTESIAN_POINT('Ctrl Pts',(98.0201427273691,-12.82509013543,63.810230114874));
#141091=CARTESIAN_POINT('Ctrl Pts',(98.3850210303692,-12.7048499061,64.001503994499));
#141092=CARTESIAN_POINT('Ctrl Pts',(98.6452233244691,-12.65210512052,64.06142072345));
#141093=CARTESIAN_POINT('Ctrl Pts',(98.7674875616692,-12.63524209323,64.074178388114));
#141094=CARTESIAN_POINT('',(98.4192415713824,-14.4018367539862,65.9071444853374));
#141095=CARTESIAN_POINT('Origin',(98.3551473045331,-12.9603609055107,65.4970333128763));
#141096=CARTESIAN_POINT('',(95.9574099869533,-14.9983144997034,62.1685143007228));
#141097=CARTESIAN_POINT('Ctrl Pts',(95.9574099809601,-14.998310267243,62.1685142604261));
#141098=CARTESIAN_POINT('Ctrl Pts',(96.0012696150027,-14.9981600557221,
62.1743656086402));
#141099=CARTESIAN_POINT('Ctrl Pts',(96.045922325758,-14.9960467811955,62.1803077696328));
#141100=CARTESIAN_POINT('Ctrl Pts',(96.0911271820895,-14.9917723025715,
62.1863059731721));
#141101=CARTESIAN_POINT('Ctrl Pts',(96.1336142904867,-14.9877548086256,
62.1919435604722));
#141102=CARTESIAN_POINT('Ctrl Pts',(96.1765884876485,-14.9818276967302,
62.1976305608909));
#141103=CARTESIAN_POINT('Ctrl Pts',(96.2198092128224,-14.9738563958951,
62.203332991161));
#141104=CARTESIAN_POINT('Ctrl Pts',(96.262472893195,-14.9659878321537,62.2089619263863));
#141105=CARTESIAN_POINT('Ctrl Pts',(96.3053763103589,-14.9561268512073,
62.2146058264365));
#141106=CARTESIAN_POINT('Ctrl Pts',(96.3482551438108,-14.944182080057,62.2202279883614));
#141107=CARTESIAN_POINT('Ctrl Pts',(96.3904901203016,-14.9324166683583,
62.2257657294241));
#141108=CARTESIAN_POINT('Ctrl Pts',(96.432700618763,-14.9186291541119,62.2312822920534));
#141109=CARTESIAN_POINT('Ctrl Pts',(96.4746100837264,-14.9027767896463,
62.2367398532758));
#141110=CARTESIAN_POINT('Ctrl Pts',(96.4846316619751,-14.8989861015271,
62.2380448896651));
#141111=CARTESIAN_POINT('Ctrl Pts',(96.4946359428567,-14.895077562312,62.2393465433086));
#141112=CARTESIAN_POINT('Ctrl Pts',(96.5046190037531,-14.8910510095824,
62.2406442824845));
#141113=CARTESIAN_POINT('Ctrl Pts',(96.5457967195746,-14.8744424517706,
62.2459971432502));
#141114=CARTESIAN_POINT('Ctrl Pts',(96.5866136873752,-14.8558221045463,
62.2512833241223));
#141115=CARTESIAN_POINT('Ctrl Pts',(96.6267891696673,-14.8352101723846,
62.256465459109));
#141116=CARTESIAN_POINT('Ctrl Pts',(96.6665575653341,-14.8148070950125,
62.26159508501));
#141117=CARTESIAN_POINT('Ctrl Pts',(96.7056966429397,-14.7924525602942,
62.2666226596332));
#141118=CARTESIAN_POINT('Ctrl Pts',(96.7439344194183,-14.768217200915,62.2715124359294));
#141119=CARTESIAN_POINT('Ctrl Pts',(96.7819897340631,-14.7440974870707,
62.2763788793431));
#141120=CARTESIAN_POINT('Ctrl Pts',(96.8191515649532,-14.7181149926537,
62.2811087349992));
#141121=CARTESIAN_POINT('Ctrl Pts',(96.8551635552591,-14.6903894065228,
62.2856687884924));
#141122=CARTESIAN_POINT('Ctrl Pts',(96.8910568242675,-14.6627552237698,
62.2902138087853));
#141123=CARTESIAN_POINT('Ctrl Pts',(96.9258071117811,-14.633389754186,62.2945900522334));
#141124=CARTESIAN_POINT('Ctrl Pts',(96.9591833549712,-14.6024578646699,
62.2987681021177));
#141125=CARTESIAN_POINT('Ctrl Pts',(96.9755304033134,-14.5873080142103,
62.3008144313898));
#141126=CARTESIAN_POINT('Ctrl Pts',(96.9915482527109,-14.5717830782717,
62.3028132785694));
#141127=CARTESIAN_POINT('Ctrl Pts',(97.00721250667,-14.555906054082,62.3047615892805));
#141128=CARTESIAN_POINT('Ctrl Pts',(97.0391864667746,-14.5234977862291,
62.3087384916667));
#141129=CARTESIAN_POINT('Ctrl Pts',(97.0696845088655,-14.4896205716953,
62.3125045103739));
#141130=CARTESIAN_POINT('Ctrl Pts',(97.0985277703137,-14.4544960363077,
62.3160376868357));
#141131=CARTESIAN_POINT('Ctrl Pts',(97.127520425927,-14.4191895727894,62.3195891634454));
#141132=CARTESIAN_POINT('Ctrl Pts',(97.1548406995405,-14.3826235179928,
62.3229053300049));
#141133=CARTESIAN_POINT('Ctrl Pts',(97.1803516998964,-14.3450501607815,
62.3259701517649));
#141134=CARTESIAN_POINT('Ctrl Pts',(97.2059642027226,-14.3073273077244,
62.3290471677539));
#141135=CARTESIAN_POINT('Ctrl Pts',(97.2297527999203,-14.2685898948594,
62.3318708142175));
#141136=CARTESIAN_POINT('Ctrl Pts',(97.251628667622,-14.2291095152601,62.3344316956302));
#141137=CARTESIAN_POINT('Ctrl Pts',(97.2737184624237,-14.1892430516328,
62.3370176202522));
#141138=CARTESIAN_POINT('Ctrl Pts',(97.2938578932226,-14.1486198206857,
62.3393356171633));
#141139=CARTESIAN_POINT('Ctrl Pts',(97.3120080591549,-14.1075240544886,
62.3413831196368));
#141140=CARTESIAN_POINT('Ctrl Pts',(97.3206890515527,-14.0878684747397,
62.3423624139018));
#141141=CARTESIAN_POINT('Ctrl Pts',(97.3289157554256,-14.0681047891605,
62.3432799340599));
#141142=CARTESIAN_POINT('Ctrl Pts',(97.3366880569937,-14.0482636570666,
62.344135952151));
#141143=CARTESIAN_POINT('Ctrl Pts',(97.3531769291343,-14.0061708628855,
62.3459519873024));
#141144=CARTESIAN_POINT('Ctrl Pts',(97.3676175655061,-13.963730686189,62.3474907783583));
#141145=CARTESIAN_POINT('Ctrl Pts',(97.3800460797385,-13.9212249218851,
62.3487600116083));
#141146=CARTESIAN_POINT('Ctrl Pts',(97.3927201547522,-13.8778793348564,
62.3500543221848));
#141147=CARTESIAN_POINT('Ctrl Pts',(97.4033021998725,-13.8344662432008,
62.3510683756366));
#141148=CARTESIAN_POINT('Ctrl Pts',(97.4118785175442,-13.7912598252116,
62.3518165265851));
#141149=CARTESIAN_POINT('Ctrl Pts',(97.420562430531,-13.7475113554538,62.3525740635592));
#141150=CARTESIAN_POINT('Ctrl Pts',(97.4271905740984,-13.7039753017101,
62.3530590688327));
#141151=CARTESIAN_POINT('Ctrl Pts',(97.4318936058219,-13.6609018927404,
62.3532916397747));
#141152=CARTESIAN_POINT('Ctrl Pts',(97.4366956008386,-13.6169221138694,
62.3535291045783));
#141153=CARTESIAN_POINT('Ctrl Pts',(97.4394912825679,-13.5734250601916,
62.3535034923263));
#141154=CARTESIAN_POINT('Ctrl Pts',(97.4404525837326,-13.5306342066661,
62.3532402240524));
#141155=CARTESIAN_POINT('Ctrl Pts',(97.4406946885919,-13.5198572785274,
62.3531739196196));
#141156=CARTESIAN_POINT('Ctrl Pts',(97.4408205713521,-13.5091249202389,
62.3530925565016));
#141157=CARTESIAN_POINT('Ctrl Pts',(97.4408332182749,-13.4984402468452,
62.3529965689936));
#141158=CARTESIAN_POINT('Ctrl Pts',(95.9574099789773,-14.9983102672498,
62.1685142601616));
#141159=CARTESIAN_POINT('Ctrl Pts',(95.9514096344211,-14.9977629302669,
62.2247096010251));
#141160=CARTESIAN_POINT('Ctrl Pts',(95.9470290608532,-14.9969313978935,
62.2791925737174));
#141161=CARTESIAN_POINT('Ctrl Pts',(95.9439607817034,-14.9958717399714,
62.3318365274954));
#141162=CARTESIAN_POINT('Ctrl Pts',(95.94075500107,-14.9947645946698,62.3868396609303));
#141163=CARTESIAN_POINT('Ctrl Pts',(95.9389816069068,-14.9934084729966,
62.439835565818));
#141164=CARTESIAN_POINT('Ctrl Pts',(95.9383155634341,-14.9918643947086,
62.4907304568309));
#141165=CARTESIAN_POINT('Ctrl Pts',(95.9381103916246,-14.9913887480739,
62.5064084077641));
#141166=CARTESIAN_POINT('Ctrl Pts',(95.9380104850422,-14.990895242425,62.521887319159));
#141167=CARTESIAN_POINT('Ctrl Pts',(95.9380068387977,-14.9903855965846,
62.5371652841353));
#141168=CARTESIAN_POINT('Ctrl Pts',(95.9379943682758,-14.9886425566529,
62.5894174579373));
#141169=CARTESIAN_POINT('Ctrl Pts',(95.9391054646362,-14.9867110841805,
62.6393159758539));
#141170=CARTESIAN_POINT('Ctrl Pts',(95.9410004067022,-14.9846569562105,
62.6868137064653));
#141171=CARTESIAN_POINT('Ctrl Pts',(95.9411425522047,-14.9845028696779,
62.6903766590784));
#141172=CARTESIAN_POINT('Ctrl Pts',(95.9412891231093,-14.9843480907103,
62.6939261214091));
#141173=CARTESIAN_POINT('Ctrl Pts',(95.9414399831782,-14.984192645958,62.6974620824213));
#141174=CARTESIAN_POINT('Ctrl Pts',(95.9425209711992,-14.983078806382,62.722799015682));
#141175=CARTESIAN_POINT('Ctrl Pts',(95.943821969844,-14.9819308181225,62.7474425085392));
#141176=CARTESIAN_POINT('Ctrl Pts',(95.9452943492417,-14.9807582395695,
62.771390098375));
#141177=CARTESIAN_POINT('Ctrl Pts',(95.9462186984745,-14.9800221031582,
62.7864242236333));
#141178=CARTESIAN_POINT('Ctrl Pts',(95.9472415248629,-14.9792519192772,
62.8016628127833));
#141179=CARTESIAN_POINT('Ctrl Pts',(95.9482960543119,-14.9784952260472,
62.8162039813757));
#141180=CARTESIAN_POINT('Ctrl Pts',(95.9489212660038,-14.9780465961345,
62.824825180743));
#141181=CARTESIAN_POINT('Ctrl Pts',(95.9495565466789,-14.9776029280011,
62.8332013115559));
#141182=CARTESIAN_POINT('Ctrl Pts',(95.9501796139764,-14.9771758460696,
62.8411452441104));
#141183=CARTESIAN_POINT('Ctrl Pts',(95.9524166031059,-14.9756425002467,
62.8696662254577));
#141184=CARTESIAN_POINT('Ctrl Pts',(95.9550153969764,-14.9739649344671,
62.8993025836247));
#141185=CARTESIAN_POINT('Ctrl Pts',(95.9580817994832,-14.972120655243,62.9300357303402));
#141186=CARTESIAN_POINT('Ctrl Pts',(95.9627412086753,-14.9693182665968,
62.976734852844));
#141187=CARTESIAN_POINT('Ctrl Pts',(95.968479815432,-14.9661307753707,63.0259682427745));
#141188=CARTESIAN_POINT('Ctrl Pts',(95.9756655139945,-14.9624862295701,
63.077650834127));
#141189=CARTESIAN_POINT('Ctrl Pts',(95.977905960307,-14.9613498878312,63.0937650741281));
#141190=CARTESIAN_POINT('Ctrl Pts',(95.9802872866223,-14.9601690919896,
63.1101170981702));
#141191=CARTESIAN_POINT('Ctrl Pts',(95.9828211744858,-14.9589416115939,
63.1267034101123));
#141192=CARTESIAN_POINT('Ctrl Pts',(95.990825716738,-14.95506400563,63.1790995072962));
#141193=CARTESIAN_POINT('Ctrl Pts',(96.0003510877725,-14.9507205586402,
63.2338378254576));
#141194=CARTESIAN_POINT('Ctrl Pts',(96.0117803923567,-14.945840314384,63.2907734730001));
#141195=CARTESIAN_POINT('Ctrl Pts',(96.0174950446489,-14.9434001922559,
63.3192412967713));
#141196=CARTESIAN_POINT('Ctrl Pts',(96.0236860222231,-14.9408258612085,
63.3482575912512));
#141197=CARTESIAN_POINT('Ctrl Pts',(96.0304031093579,-14.9381084849442,
63.3777984390504));
#141198=CARTESIAN_POINT('Ctrl Pts',(96.0337616529253,-14.936749796812,63.39256886295));
#141199=CARTESIAN_POINT('Ctrl Pts',(96.0372517238174,-14.935355342873,63.4074704247759));
#141200=CARTESIAN_POINT('Ctrl Pts',(96.0408796711626,-14.9339240340903,
63.4224996477211));
#141201=CARTESIAN_POINT('Ctrl Pts',(96.0426936448352,-14.9332083796989,
63.4300142591937));
#141202=CARTESIAN_POINT('Ctrl Pts',(96.0445420876175,-14.9324835113438,
63.4375607859244));
#141203=CARTESIAN_POINT('Ctrl Pts',(96.0464257961909,-14.9317492929014,
63.4451387756133));
#141204=CARTESIAN_POINT('Ctrl Pts',(96.0478696280205,-14.9311865264672,
63.450947180837));
#141205=CARTESIAN_POINT('Ctrl Pts',(96.0495783943475,-14.9305236394949,
63.4577406841441));
#141206=CARTESIAN_POINT('Ctrl Pts',(96.0509917948209,-14.9299779874319,
63.4632961350523));
#141207=CARTESIAN_POINT('Ctrl Pts',(96.0514224003701,-14.9298117494756,
63.4649886546417));
#141208=CARTESIAN_POINT('Ctrl Pts',(96.0518252088932,-14.9296564667047,
63.4665663717365));
#141209=CARTESIAN_POINT('Ctrl Pts',(96.0521835178952,-14.929518450927,63.4679666720874));
#141210=CARTESIAN_POINT('Ctrl Pts',(96.0691237899622,-14.922993287423,63.5341706155741));
#141211=CARTESIAN_POINT('Ctrl Pts',(96.0881777231867,-14.9159073862417,
63.601199258289));
#141212=CARTESIAN_POINT('Ctrl Pts',(96.109570791596,-14.9082293103102,63.668841239143));
#141213=CARTESIAN_POINT('Ctrl Pts',(96.1302222508339,-14.9008174015045,
63.7341383523783));
#141214=CARTESIAN_POINT('Ctrl Pts',(96.1530535583824,-14.8928536236557,
63.8000071753183));
#141215=CARTESIAN_POINT('Ctrl Pts',(96.1782714395541,-14.8843122721267,
63.8662087137561));
#141216=CARTESIAN_POINT('Ctrl Pts',(96.1830084378664,-14.8827078404338,
63.8786441984709));
#141217=CARTESIAN_POINT('Ctrl Pts',(96.1878296557326,-14.8810830375917,
63.8910912759394));
#141218=CARTESIAN_POINT('Ctrl Pts',(96.1927364758324,-14.8794377055759,
63.9035481533974));
#141219=CARTESIAN_POINT('Ctrl Pts',(96.2200589510483,-14.8702760607002,
63.9729113496606));
#141220=CARTESIAN_POINT('Ctrl Pts',(96.2500368149232,-14.8604768525931,
64.0425820309446));
#141221=CARTESIAN_POINT('Ctrl Pts',(96.2828300686085,-14.8500536955576,
64.1123257811251));
#141222=CARTESIAN_POINT('Ctrl Pts',(96.3142549584493,-14.8400654655157,
64.1791593343775));
#141223=CARTESIAN_POINT('Ctrl Pts',(96.3482652772853,-14.8295042523752,
64.2460600637489));
#141224=CARTESIAN_POINT('Ctrl Pts',(96.3849873652349,-14.8183938641851,
64.3127789400618));
#141225=CARTESIAN_POINT('Ctrl Pts',(96.4209821229657,-14.807503532139,64.378176359518));
#141226=CARTESIAN_POINT('Ctrl Pts',(96.4595824246679,-14.7960855115134,
64.4433992698679));
#141227=CARTESIAN_POINT('Ctrl Pts',(96.5008913544073,-14.7841744147628,
64.5081688476521));
#141228=CARTESIAN_POINT('Ctrl Pts',(96.5166722132981,-14.7796241313678,
64.5329121555488));
#141229=CARTESIAN_POINT('Ctrl Pts',(96.5328481906253,-14.7750020211855,
64.5575888206246));
#141230=CARTESIAN_POINT('Ctrl Pts',(96.5494243368809,-14.7703105239057,
64.5821814293567));
#141231=CARTESIAN_POINT('Ctrl Pts',(96.5577124100088,-14.7679647752658,
64.5944777337228));
#141232=CARTESIAN_POINT('Ctrl Pts',(96.566100525408,-14.7656016812886,64.6067530242521));
#141233=CARTESIAN_POINT('Ctrl Pts',(96.5745892679672,-14.7632215783835,
64.6190050019048));
#141234=CARTESIAN_POINT('Ctrl Pts',(96.5788336392468,-14.7620315269309,
64.6251309907311));
#141235=CARTESIAN_POINT('Ctrl Pts',(96.583103167319,-14.7608372233412,64.6312511513545));
#141236=CARTESIAN_POINT('Ctrl Pts',(96.5873979238826,-14.7596387109044,
64.6373651927919));
#141237=CARTESIAN_POINT('Ctrl Pts',(96.5895453021644,-14.759039454686,64.6404222135105));
#141238=CARTESIAN_POINT('Ctrl Pts',(96.5916989875691,-14.7584391462613,
64.6434777044337));
#141239=CARTESIAN_POINT('Ctrl Pts',(96.5938589888889,-14.7578377911593,
64.6465316287433));
#141240=CARTESIAN_POINT('Ctrl Pts',(96.5958381016573,-14.757286796329,64.6493298032349));
#141241=CARTESIAN_POINT('Ctrl Pts',(96.5987682376394,-14.7564721479833,
64.6534559247871));
#141242=CARTESIAN_POINT('Ctrl Pts',(96.6000499109288,-14.756116149547,64.6552560745118));
#141243=CARTESIAN_POINT('Ctrl Pts',(96.6001670543419,-14.7560836117137,
64.655420606054));
#141244=CARTESIAN_POINT('Ctrl Pts',(96.6002703991504,-14.7560549081226,
64.6555657297191));
#141245=CARTESIAN_POINT('Ctrl Pts',(96.6003579493328,-14.7560305913982,
64.6556886648793));
#141246=CARTESIAN_POINT('Ctrl Pts',(96.6173725778219,-14.751304844188,64.6795800608916));
#141247=CARTESIAN_POINT('Ctrl Pts',(96.6362979304481,-14.7460791896076,
64.7055873977613));
#141248=CARTESIAN_POINT('Ctrl Pts',(96.657330736075,-14.7403386778775,64.7335281250405));
#141249=CARTESIAN_POINT('Ctrl Pts',(96.663756580762,-14.7385848635051,64.742064445735));
#141250=CARTESIAN_POINT('Ctrl Pts',(96.6703793071634,-14.7367830111207,
64.7507809081317));
#141251=CARTESIAN_POINT('Ctrl Pts',(96.6772049534311,-14.7349327574401,
64.7596714255857));
#141252=CARTESIAN_POINT('Ctrl Pts',(96.7003374256768,-14.7286621509313,
64.7898018542933));
#141253=CARTESIAN_POINT('Ctrl Pts',(96.7257991469457,-14.7218349641208,
64.8219349205996));
#141254=CARTESIAN_POINT('Ctrl Pts',(96.7538385481015,-14.714442632941,64.8558164648191));
#141255=CARTESIAN_POINT('Ctrl Pts',(96.781397335869,-14.7071770110771,64.889117257557));
#141256=CARTESIAN_POINT('Ctrl Pts',(96.8114468393952,-14.6993651700304,
64.9241073165543));
#141257=CARTESIAN_POINT('Ctrl Pts',(96.8442357055063,-14.6910095669947,
64.9604980558787));
#141258=CARTESIAN_POINT('Ctrl Pts',(96.875624641371,-14.6830107088789,64.9953350819245));
#141259=CARTESIAN_POINT('Ctrl Pts',(96.9095246271991,-14.6745133307496,
65.03145575547));
#141260=CARTESIAN_POINT('Ctrl Pts',(96.9461565118213,-14.6655327595853,
65.0685618480512));
#141261=CARTESIAN_POINT('Ctrl Pts',(96.9817089216784,-14.6568168294584,
65.1045744918245));
#141262=CARTESIAN_POINT('Ctrl Pts',(97.0198351312783,-14.6476455649945,
65.1415154605205));
#141263=CARTESIAN_POINT('Ctrl Pts',(97.0607314266875,-14.6380485623792,
65.1790675346859));
#141264=CARTESIAN_POINT('Ctrl Pts',(97.0996415206312,-14.6289176552982,
65.2147958254501));
#141265=CARTESIAN_POINT('Ctrl Pts',(97.1410595728877,-14.6194012540219,
65.2510772824833));
#141266=CARTESIAN_POINT('Ctrl Pts',(97.1851428296347,-14.6095412396628,
65.287597215422));
#141267=CARTESIAN_POINT('Ctrl Pts',(97.2196328613478,-14.6018269228671,
65.3161698241211));
#141268=CARTESIAN_POINT('Ctrl Pts',(97.2557541868158,-14.5939025487894,
65.3448876692596));
#141269=CARTESIAN_POINT('Ctrl Pts',(97.2935742074652,-14.5857964285298,
65.3735807790044));
#141270=CARTESIAN_POINT('Ctrl Pts',(97.3062872473112,-14.5830715905185,
65.3832258463848));
#141271=CARTESIAN_POINT('Ctrl Pts',(97.319192159892,-14.5803262824039,65.3928679693906));
#141272=CARTESIAN_POINT('Ctrl Pts',(97.33229128162,-14.5775617856489,65.4025002359996));
#141273=CARTESIAN_POINT('Ctrl Pts',(97.3464079637588,-14.5745825384311,
65.4128807522524));
#141274=CARTESIAN_POINT('Ctrl Pts',(97.360750198253,-14.5715810050985,65.4232498158811));
#141275=CARTESIAN_POINT('Ctrl Pts',(97.3753212746219,-14.568558755652,65.4335994685519));
#141276=CARTESIAN_POINT('Ctrl Pts',(97.3893671939351,-14.5656454312828,
65.443576108757));
#141277=CARTESIAN_POINT('Ctrl Pts',(97.4036256790824,-14.5627128946341,
65.4535345687424));
#141278=CARTESIAN_POINT('Ctrl Pts',(97.4180996460052,-14.5597626309598,
65.4634676907597));
#141279=CARTESIAN_POINT('Ctrl Pts',(97.4253366294665,-14.5582874991226,
65.4684342517683));
#141280=CARTESIAN_POINT('Ctrl Pts',(97.4326274834083,-14.5568079365226,
65.473394478516));
#141281=CARTESIAN_POINT('Ctrl Pts',(97.4399725384888,-14.5553241507323,
65.4783474185003));
#141282=CARTESIAN_POINT('Ctrl Pts',(97.443645066029,-14.5545822578372,65.4808238884924));
#141283=CARTESIAN_POINT('Ctrl Pts',(97.4473311438567,-14.5538393092137,
65.4832985368107));
#141284=CARTESIAN_POINT('Ctrl Pts',(97.4510308137269,-14.5530953309797,
65.4857712454299));
#141285=CARTESIAN_POINT('Ctrl Pts',(97.454730483597,-14.5523513527457,65.4882439540491));
#141286=CARTESIAN_POINT('Ctrl Pts',(97.4594831837347,-14.551398281015,65.491403251175));
#141287=CARTESIAN_POINT('Ctrl Pts',(97.4621706409605,-14.5508603339509,
65.4931834338171));
#141288=CARTESIAN_POINT('Ctrl Pts',(97.5231372774435,-14.5386566706569,
65.5335679828131));
#141289=CARTESIAN_POINT('Ctrl Pts',(97.5838904468826,-14.5270214011671,
65.5705895517535));
#141290=CARTESIAN_POINT('Ctrl Pts',(97.6440811651151,-14.5159906565726,
65.6045419319516));
#141291=CARTESIAN_POINT('Ctrl Pts',(97.7050374390766,-14.5048196137732,
65.6389261468234));
#141292=CARTESIAN_POINT('Ctrl Pts',(97.7654169391016,-14.4942684085919,
65.6701626512717));
#141293=CARTESIAN_POINT('Ctrl Pts',(97.824906488088,-14.484354276746,65.6985487188738));
#141294=CARTESIAN_POINT('Ctrl Pts',(97.8856406114176,-14.4742327324329,
65.7275286482894));
#141295=CARTESIAN_POINT('Ctrl Pts',(97.9454472157503,-14.4647750504268,
65.7535377111398));
#141296=CARTESIAN_POINT('Ctrl Pts',(98.004043176135,-14.4559808830376,65.7768830527672));
#141297=CARTESIAN_POINT('Ctrl Pts',(98.0200331420063,-14.4535810855858,
65.7832536491944));
#141298=CARTESIAN_POINT('Ctrl Pts',(98.0359332350288,-14.4512305993524,
65.789425832096));
#141299=CARTESIAN_POINT('Ctrl Pts',(98.0517383197579,-14.4489292049126,
65.7954057135219));
#141300=CARTESIAN_POINT('Ctrl Pts',(98.1165405888195,-14.4394932806982,
65.8199237652603));
#141301=CARTESIAN_POINT('Ctrl Pts',(98.17974232874,-14.4308834625626,65.8412111725943));
#141302=CARTESIAN_POINT('Ctrl Pts',(98.2410749986541,-14.423052262834,65.8596960227291));
#141303=CARTESIAN_POINT('Ctrl Pts',(98.3024076685682,-14.4152210631054,
65.878180872864));
#141304=CARTESIAN_POINT('Ctrl Pts',(98.3618713705022,-14.4081682887106,
65.8938632586274));
#141305=CARTESIAN_POINT('Ctrl Pts',(98.4192415713824,-14.4018367539862,
65.9071444853374));
#141306=CARTESIAN_POINT('Ctrl Pts',(91.7279224053691,-15.00086655583,62.66821414647));
#141307=CARTESIAN_POINT('Ctrl Pts',(92.8206547514691,-15.00091548588,62.47811409076));
#141308=CARTESIAN_POINT('Ctrl Pts',(94.9571365614691,-15.00012240043,62.10622675894));
#141309=CARTESIAN_POINT('Ctrl Pts',(97.3520603458691,-14.99728767361,61.67409908363));
#141310=CARTESIAN_POINT('Ctrl Pts',(98.9140829208691,-14.9946683359,61.38022674646));
#141311=CARTESIAN_POINT('Ctrl Pts',(99.7424919119691,-14.99311894757,61.22079195603));
#141312=CARTESIAN_POINT('Ctrl Pts',(100.309755217069,-14.99193659845,61.10860712166));
#141313=CARTESIAN_POINT('Ctrl Pts',(100.617471098369,-14.99125877485,61.04648221514));
#141314=CARTESIAN_POINT('Ctrl Pts',(91.9040967972691,-15.00296392531,63.719058961888));
#141315=CARTESIAN_POINT('Ctrl Pts',(93.0606464640691,-15.0026956181,63.506039291405));
#141316=CARTESIAN_POINT('Ctrl Pts',(95.3224996923691,-15.0032813732,63.093090511071));
#141317=CARTESIAN_POINT('Ctrl Pts',(97.8588287799691,-15.00640433575,62.62496746378));
#141318=CARTESIAN_POINT('Ctrl Pts',(99.5138086795691,-15.00944466321,62.31213308663));
#141319=CARTESIAN_POINT('Ctrl Pts',(100.390785755669,-15.01129179849,62.14422141575));
#141320=CARTESIAN_POINT('Ctrl Pts',(100.993297194369,-15.01272721411,62.02642432059));
#141321=CARTESIAN_POINT('Ctrl Pts',(101.318242921569,-15.01358278139,61.96242696786));
#141322=CARTESIAN_POINT('Ctrl Pts',(92.2448361102691,-14.79056277436,65.751541377466));
#141323=CARTESIAN_POINT('Ctrl Pts',(93.5247227957691,-14.79469787263,65.492534702806));
#141324=CARTESIAN_POINT('Ctrl Pts',(96.0287721259691,-14.80601079336,64.996333659406));
#141325=CARTESIAN_POINT('Ctrl Pts',(98.8382499265691,-14.82557675296,64.452349667076));
#141326=CARTESIAN_POINT('Ctrl Pts',(100.673211451469,-14.84109633199,64.097462534948));
#141327=CARTESIAN_POINT('Ctrl Pts',(101.644481448969,-14.84982392585,63.909951340424));
#141328=CARTESIAN_POINT('Ctrl Pts',(102.315435468069,-14.8565128255,63.778640063626));
#141329=CARTESIAN_POINT('Ctrl Pts',(102.672968839569,-14.85993777441,63.710281289207));
#141330=CARTESIAN_POINT('Ctrl Pts',(92.8846953387691,-13.59339522536,69.569112430703));
#141331=CARTESIAN_POINT('Ctrl Pts',(94.3995479103691,-13.62144836123,69.235119209287));
#141332=CARTESIAN_POINT('Ctrl Pts',(97.3641245099691,-13.67740135474,68.599574225623));
#141333=CARTESIAN_POINT('Ctrl Pts',(100.691605655469,-13.74147687523,67.919598525714));
#141334=CARTESIAN_POINT('Ctrl Pts',(102.867637731469,-13.78402627843,67.484518318603));
#141335=CARTESIAN_POINT('Ctrl Pts',(104.018563150869,-13.80621016489,67.257624542188));
#141336=CARTESIAN_POINT('Ctrl Pts',(104.818068817069,-13.82296220245,67.099320059727));
#141337=CARTESIAN_POINT('Ctrl Pts',(105.237162052669,-13.82954337409,67.020632065286));
#141338=CARTESIAN_POINT('Ctrl Pts',(93.4372496265691,-11.36012668785,72.8749686356714));
#141339=CARTESIAN_POINT('Ctrl Pts',(95.1718643785691,-11.41712605373,72.5027022658309));
#141340=CARTESIAN_POINT('Ctrl Pts',(98.5659480545691,-11.5258471646,71.79092364103));
#141341=CARTESIAN_POINT('Ctrl Pts',(102.374754293569,-11.63978355673,71.024735995695));
#141342=CARTESIAN_POINT('Ctrl Pts',(104.865797163869,-11.71128588736,70.534131296002));
#141343=CARTESIAN_POINT('Ctrl Pts',(106.185002256269,-11.74808512595,70.277403513677));
#141344=CARTESIAN_POINT('Ctrl Pts',(107.098214269869,-11.77444776282,70.101421471233));
#141345=CARTESIAN_POINT('Ctrl Pts',(107.578337843769,-11.78460067693,70.010906079548));
#141346=CARTESIAN_POINT('Ctrl Pts',(93.8521515924691,-8.31376415398099,
75.380290328567));
#141347=CARTESIAN_POINT('Ctrl Pts',(95.7842091872691,-8.37610151927799,
74.996687936449));
#141348=CARTESIAN_POINT('Ctrl Pts',(99.5633456799691,-8.49649192700699,
74.256622113144));
#141349=CARTESIAN_POINT('Ctrl Pts',(103.803511293669,-8.62652182891199,
73.4457843508907));
#141350=CARTESIAN_POINT('Ctrl Pts',(106.574368779969,-8.70918767776199,
72.9222235420443));
#141351=CARTESIAN_POINT('Ctrl Pts',(108.046575455569,-8.75337472261899,
72.645850034118));
#141352=CARTESIAN_POINT('Ctrl Pts',(109.052811928669,-8.78167412688299,
72.4603562024988));
#141353=CARTESIAN_POINT('Ctrl Pts',(109.595630317769,-8.79651115761099,
72.3582991883668));
#141354=CARTESIAN_POINT('Ctrl Pts',(94.0472766649691,-6.14488949293299,
76.567167410547));
#141355=CARTESIAN_POINT('Ctrl Pts',(96.0854968862691,-6.19932125750799,
76.182430497497));
#141356=CARTESIAN_POINT('Ctrl Pts',(100.071511458569,-6.30590151645599,
75.436192057807));
#141357=CARTESIAN_POINT('Ctrl Pts',(104.544032724869,-6.42467485066199,
74.609669612437));
#141358=CARTESIAN_POINT('Ctrl Pts',(107.464659287669,-6.50123978999499,
74.073144793283));
#141359=CARTESIAN_POINT('Ctrl Pts',(109.020613207169,-6.54339816253699,
73.7885097201805));
#141360=CARTESIAN_POINT('Ctrl Pts',(110.072680416569,-6.56809626639499,
73.5995632553892));
#141361=CARTESIAN_POINT('Ctrl Pts',(110.653470670069,-6.58429622250299,
73.4915052896967));
#141362=CARTESIAN_POINT('Ctrl Pts',(94.1596433973691,-4.29694974983499,
77.257573104574));
#141363=CARTESIAN_POINT('Ctrl Pts',(96.2671293792691,-4.33699728402899,
76.872950615596));
#141364=CARTESIAN_POINT('Ctrl Pts',(100.388073242369,-4.41679216450099,
76.124486128563));
#141365=CARTESIAN_POINT('Ctrl Pts',(105.012816858869,-4.50905954903699,
75.289931616852));
#141366=CARTESIAN_POINT('Ctrl Pts',(108.030893246069,-4.56946366778099,
74.746434477664));
#141367=CARTESIAN_POINT('Ctrl Pts',(109.642849121469,-4.60376584696699,
74.45726477928));
#141368=CARTESIAN_POINT('Ctrl Pts',(110.721584350869,-4.62195018599999,
74.266525935187));
#141369=CARTESIAN_POINT('Ctrl Pts',(111.330637583069,-4.63685072441499,
74.154803592336));
#141370=CARTESIAN_POINT('Ctrl Pts',(94.2215314633691,-2.87401142301499,
77.640260609653));
#141371=CARTESIAN_POINT('Ctrl Pts',(96.3708143948691,-2.90124327492399,
77.25556064955));
#141372=CARTESIAN_POINT('Ctrl Pts',(100.573127343269,-2.95640194059799,
76.505561208076));
#141373=CARTESIAN_POINT('Ctrl Pts',(105.290085863569,-3.02238747552899,
75.666090425013));
#141374=CARTESIAN_POINT('Ctrl Pts',(108.366745098769,-3.06612832963899,
75.11841156241));
#141375=CARTESIAN_POINT('Ctrl Pts',(110.013387788769,-3.09171881003499,
74.826511058606));
#141376=CARTESIAN_POINT('Ctrl Pts',(111.106033315769,-3.10383313136499,
74.634769909069));
#141377=CARTESIAN_POINT('Ctrl Pts',(111.734449639069,-3.11622061397699,
74.520727967092));
#141378=CARTESIAN_POINT('Ctrl Pts',(94.2650345463691,-1.31031824892799,
77.910754859622));
#141379=CARTESIAN_POINT('Ctrl Pts',(96.4453247786691,-1.32158371898399,
77.525392447647));
#141380=CARTESIAN_POINT('Ctrl Pts',(100.707884176569,-1.34593412180199,
76.773013051733));
#141381=CARTESIAN_POINT('Ctrl Pts',(105.493651081669,-1.37849110683099,
75.928270717931));
#141382=CARTESIAN_POINT('Ctrl Pts',(108.613311575269,-1.40102659958799,
75.376389135756));
#141383=CARTESIAN_POINT('Ctrl Pts',(110.286981216069,-1.41501268170799,
75.081756321705));
#141384=CARTESIAN_POINT('Ctrl Pts',(111.386572784969,-1.42033729508099,
74.88908018054));
#141385=CARTESIAN_POINT('Ctrl Pts',(112.032792121069,-1.42836747710599,
74.772757830664));
#141386=CARTESIAN_POINT('Ctrl Pts',(94.2748040922691,-0.278275671875586,
77.974281587457));
#141387=CARTESIAN_POINT('Ctrl Pts',(96.4657713563691,-0.279825571159086,
77.588107109206));
#141388=CARTESIAN_POINT('Ctrl Pts',(100.748949641169,-0.283983060529886,
76.833828722269));
#141389=CARTESIAN_POINT('Ctrl Pts',(105.558826386669,-0.291328739675386,
75.986054822495));
#141390=CARTESIAN_POINT('Ctrl Pts',(108.692803760269,-0.296740586015386,
75.432041328266));
#141391=CARTESIAN_POINT('Ctrl Pts',(110.377140334169,-0.300757700117286,
75.135908202226));
#141392=CARTESIAN_POINT('Ctrl Pts',(111.475574778769,-0.300917836469986,
74.943110155442));
#141393=CARTESIAN_POINT('Ctrl Pts',(112.131539947869,-0.304306622775186,
74.825323634026));
#141394=CARTESIAN_POINT('Ctrl Pts',(94.2720112807691,0.226163356373814,
77.96047019643));
#141395=CARTESIAN_POINT('Ctrl Pts',(96.4654988279691,0.227634972375714,
77.573615266263));
#141396=CARTESIAN_POINT('Ctrl Pts',(100.753485332469,0.231339974406114,
76.818101757373));
#141397=CARTESIAN_POINT('Ctrl Pts',(105.569346130169,0.237025460465514,
75.969015910907));
#141398=CARTESIAN_POINT('Ctrl Pts',(108.706464376969,0.241496016631014,
75.414309396842));
#141399=CARTESIAN_POINT('Ctrl Pts',(110.394133361669,0.243542056646714,
75.117607997261));
#141400=CARTESIAN_POINT('Ctrl Pts',(111.490264022669,0.246460875082214,
74.925066840918));
#141401=CARTESIAN_POINT('Ctrl Pts',(112.150634911769,0.246228592821014,
74.806547696003));
#141402=CARTESIAN_POINT('',(91.9155434736732,-14.9991665202076,62.8752787211534));
#141403=CARTESIAN_POINT('Ctrl Pts',(95.9574100500792,-14.998343644201,62.1685145911545));
#141404=CARTESIAN_POINT('Ctrl Pts',(95.9452997971755,-14.9983495824529,
62.1707000739723));
#141405=CARTESIAN_POINT('Ctrl Pts',(95.8963891825556,-14.9983766962934,
62.1792257798343));
#141406=CARTESIAN_POINT('Ctrl Pts',(95.8106852915384,-14.9984234747686,
62.194055653576));
#141407=CARTESIAN_POINT('Ctrl Pts',(95.7734726089319,-14.9984437860115,
62.2004947939475));
#141408=CARTESIAN_POINT('Ctrl Pts',(95.7293234569771,-14.9984677764014,
62.2081217736258));
#141409=CARTESIAN_POINT('Ctrl Pts',(95.6782392676023,-14.9984951851695,
62.2169307774249));
#141410=CARTESIAN_POINT('Ctrl Pts',(95.5938716127534,-14.9985404518853,
62.2314792121007));
#141411=CARTESIAN_POINT('Ctrl Pts',(95.4905877629147,-14.9985950833701,
62.2492520642195));
#141412=CARTESIAN_POINT('Ctrl Pts',(95.368397778593,-14.9986573431981,62.2702154651726));
#141413=CARTESIAN_POINT('Ctrl Pts',(95.3073027864321,-14.9986884731122,
62.2806971656492));
#141414=CARTESIAN_POINT('Ctrl Pts',(95.241481260621,-14.9987214974988,62.2919765031988));
#141415=CARTESIAN_POINT('Ctrl Pts',(95.1709350275728,-14.9987561261751,
62.3040485648304));
#141416=CARTESIAN_POINT('Ctrl Pts',(95.1442556676702,-14.9987692221389,
62.3086140088394));
#141417=CARTESIAN_POINT('Ctrl Pts',(95.1169005706544,-14.9987825469947,
62.3132928296912));
#141418=CARTESIAN_POINT('Ctrl Pts',(95.0888698437195,-14.9987960828689,
62.3180847692762));
#141419=CARTESIAN_POINT('Ctrl Pts',(95.0798407948187,-14.9988004429438,
62.3196283131502));
#141420=CARTESIAN_POINT('Ctrl Pts',(95.0707416449853,-14.9988048249041,
62.321183593822));
#141421=CARTESIAN_POINT('Ctrl Pts',(95.0615723979527,-14.9988092281285,
62.3227506025527));
#141422=CARTESIAN_POINT('Ctrl Pts',(95.0427547880724,-14.9988182646565,
62.3259665000923));
#141423=CARTESIAN_POINT('Ctrl Pts',(95.0236419465857,-14.9988273907554,
62.3292317934443));
#141424=CARTESIAN_POINT('Ctrl Pts',(95.0042339067701,-14.9988366008968,
62.3325464059602));
#141425=CARTESIAN_POINT('Ctrl Pts',(94.9872518719314,-14.9988446597705,
62.3354466919116));
#141426=CARTESIAN_POINT('Ctrl Pts',(94.9700438258722,-14.9988527829859,
62.3383847378479));
#141427=CARTESIAN_POINT('Ctrl Pts',(94.9526097917505,-14.9988609666919,
62.3413604926689));
#141428=CARTESIAN_POINT('Ctrl Pts',(94.9501192154474,-14.9988621357928,
62.3417856005005));
#141429=CARTESIAN_POINT('Ctrl Pts',(94.946312537638,-14.9988639207714,62.3424353129184));
#141430=CARTESIAN_POINT('Ctrl Pts',(94.9451242269272,-14.9988644776858,
62.3426381247191));
#141431=CARTESIAN_POINT('Ctrl Pts',(94.7930204559396,-14.9989357627347,
62.3685980352097));
#141432=CARTESIAN_POINT('Ctrl Pts',(94.6327281907657,-14.99900408532,62.3961886287692));
#141433=CARTESIAN_POINT('Ctrl Pts',(94.4642319885938,-14.9990675132126,
62.4254070205069));
#141434=CARTESIAN_POINT('Ctrl Pts',(94.3799838875078,-14.9990992271589,
62.4400162163758));
#141435=CARTESIAN_POINT('Ctrl Pts',(94.2936848021655,-14.9991297146013,
62.4550323617557));
#141436=CARTESIAN_POINT('Ctrl Pts',(94.2053324757767,-14.9991587135592,
62.4704557980971));
#141437=CARTESIAN_POINT('Ctrl Pts',(94.1611563125823,-14.9991732130382,
62.4781675162678));
#141438=CARTESIAN_POINT('Ctrl Pts',(94.1164668391261,-14.9991873402925,
62.4859810571776));
#141439=CARTESIAN_POINT('Ctrl Pts',(94.0712637660084,-14.9992010617574,
62.493896493564));
#141440=CARTESIAN_POINT('Ctrl Pts',(94.0486622294495,-14.9992079224898,
62.4978542117572));
#141441=CARTESIAN_POINT('Ctrl Pts',(94.0259322929752,-14.9992146817712,
62.5018374038195));
#141442=CARTESIAN_POINT('Ctrl Pts',(94.0030739193293,-14.9992213353548,
62.5058460818041));
#141443=CARTESIAN_POINT('Ctrl Pts',(93.9802155456834,-14.9992279889383,
62.5098547597888));
#141444=CARTESIAN_POINT('Ctrl Pts',(93.9551481387037,-14.9992351163016,
62.5142543317982));
#141445=CARTESIAN_POINT('Ctrl Pts',(93.9341134493102,-14.9992409747461,
62.5179485865606));
#141446=CARTESIAN_POINT('Ctrl Pts',(93.2610033887235,-14.9994284449695,
62.6361647389558));
#141447=CARTESIAN_POINT('Ctrl Pts',(92.5882566618296,-14.9995133827134,
62.7549799849729));
#141448=CARTESIAN_POINT('Ctrl Pts',(91.9155442365578,-14.9994907910654,
62.8752830475864));
#141449=CARTESIAN_POINT('Ctrl Pts',(91.9155434736732,-14.9991665202076,
62.8752787211533));
#141450=CARTESIAN_POINT('Ctrl Pts',(92.086693919164,-14.9860768545361,63.846009912322));
#141451=CARTESIAN_POINT('Ctrl Pts',(92.4297074936291,-14.7677508465704,
65.7913694335692));
#141452=CARTESIAN_POINT('Ctrl Pts',(93.087950234184,-13.5971624559109,69.5243543489225));
#141453=CARTESIAN_POINT('Ctrl Pts',(93.6699893115637,-11.3677658456745,
72.8250712227319));
#141454=CARTESIAN_POINT('Ctrl Pts',(94.1113790316493,-8.32212329542681,
75.3288531905138));
#141455=CARTESIAN_POINT('Ctrl Pts',(94.3207457772408,-6.1521930131437,76.5155659174532));
#141456=CARTESIAN_POINT('Ctrl Pts',(94.4424043515144,-4.3023274699128,77.2059794423346));
#141457=CARTESIAN_POINT('Ctrl Pts',(94.5098992359463,-2.87767097403913,
77.5886523041447));
#141458=CARTESIAN_POINT('Ctrl Pts',(94.5463398268069,-1.68049722662779,
77.795390819026));
#141459=CARTESIAN_POINT('Ctrl Pts',(94.5585266384417,-0.993628204659395,
77.8644736013413));
#141460=CARTESIAN_POINT('Ctrl Pts',(94.5611174495922,-0.79195163185674,
77.8790704031872));
#141461=CARTESIAN_POINT('',(111.837855320939,-3.16944077116514E-5,74.8658931845202));
#141462=CARTESIAN_POINT('Ctrl Pts',(94.5668566070111,2.94209101525666E-14,
77.9116179430022));
#141463=CARTESIAN_POINT('Ctrl Pts',(96.6609425362034,-9.94245023112965E-6,
77.5423740937652));
#141464=CARTESIAN_POINT('Ctrl Pts',(98.7546944933837,-8.73790753213637E-7,
77.1735054108323));
#141465=CARTESIAN_POINT('Ctrl Pts',(100.849271657605,-2.47060687980083E-5,
76.8043622416323));
#141466=CARTESIAN_POINT('Ctrl Pts',(102.94384882182,-4.85383468428085E-5,
76.4352190724334));
#141467=CARTESIAN_POINT('Ctrl Pts',(105.039251179636,-0.000105274089662958,
76.0658014187793));
#141468=CARTESIAN_POINT('Ctrl Pts',(107.130561787693,-4.76672842314452E-5,
75.6962533003417));
#141469=CARTESIAN_POINT('Ctrl Pts',(107.653389439708,-3.32655828735113E-5,
75.6038662707323));
#141470=CARTESIAN_POINT('Ctrl Pts',(108.175961359368,-1.17169284003341E-5,
75.5114710868269));
#141471=CARTESIAN_POINT('Ctrl Pts',(108.702045166413,-9.48554258586864E-5,
75.4187174262545));
#141472=CARTESIAN_POINT('Ctrl Pts',(109.228128973458,-0.000177993923317082,
75.3259637656821));
#141473=CARTESIAN_POINT('Ctrl Pts',(109.757724660669,-0.000365821513508409,
75.2328516293625));
#141474=CARTESIAN_POINT('Ctrl Pts',(110.274862201896,-0.000138237845730693,
75.1419811030903));
#141475=CARTESIAN_POINT('Ctrl Pts',(110.792000729337,8.93462560637043E-5,
75.0511104035223));
#141476=CARTESIAN_POINT('Ctrl Pts',(111.296681089265,0.000732349520133465,
74.9624813188668));
#141477=CARTESIAN_POINT('Ctrl Pts',(111.837855320796,-3.1694407687799E-5,
74.8658931837171));
#141478=CARTESIAN_POINT('',(105.406754466169,-13.34496396307,67.526113924257));
#141479=CARTESIAN_POINT('Ctrl Pts',(105.406754466169,-13.34496396307,67.526113924257));
#141480=CARTESIAN_POINT('Ctrl Pts',(105.667201640758,-13.1524845173195,
67.8633312808299));
#141481=CARTESIAN_POINT('Ctrl Pts',(106.505311711911,-12.4720154542567,
68.9441574710452));
#141482=CARTESIAN_POINT('Ctrl Pts',(107.85098938429,-11.0326717788794,70.6411848672459));
#141483=CARTESIAN_POINT('Ctrl Pts',(109.342844894738,-8.78940909978976,
72.4057715996434));
#141484=CARTESIAN_POINT('Ctrl Pts',(110.383862574518,-6.57696435517895,
73.5414086564304));
#141485=CARTESIAN_POINT('Ctrl Pts',(111.048812787947,-4.63025152828649,
74.2062402037403));
#141486=CARTESIAN_POINT('Ctrl Pts',(111.444414280311,-3.11083529273396,
74.5731246015333));
#141487=CARTESIAN_POINT('Ctrl Pts',(111.719571250065,-1.51676729084888,
74.8123187261577));
#141488=CARTESIAN_POINT('Ctrl Pts',(111.814574930745,-0.48158953538163,
74.8700323543884));
#141489=CARTESIAN_POINT('Ctrl Pts',(111.837855321069,-3.16944077378891E-5,
74.865893185247));
#141490=CARTESIAN_POINT('Ctrl Pts',(98.4192401226558,-14.4018041922808,
65.9071352203558));
#141491=CARTESIAN_POINT('Ctrl Pts',(98.5394222325127,-14.3885387757991,
65.9349583803957));
#141492=CARTESIAN_POINT('Ctrl Pts',(98.6603383966166,-14.374958657731,65.9629600008797));
#141493=CARTESIAN_POINT('Ctrl Pts',(98.7819870929894,-14.3610525428478,
65.991138645606));
#141494=CARTESIAN_POINT('Ctrl Pts',(99.055167133486,-14.3298243164859,66.0544179370163));
#141495=CARTESIAN_POINT('Ctrl Pts',(99.3320414430944,-14.29695261602,66.1185900405074));
#141496=CARTESIAN_POINT('Ctrl Pts',(99.6125904245059,-14.2623012850507,
66.1836375765257));
#141497=CARTESIAN_POINT('Ctrl Pts',(99.864228609599,-14.231220801378,66.2419819120712));
#141498=CARTESIAN_POINT('Ctrl Pts',(100.1188231284,-14.1987084989489,66.3010305345064));
#141499=CARTESIAN_POINT('Ctrl Pts',(100.376356493531,-14.1646597066291,
66.3607696469528));
#141500=CARTESIAN_POINT('Ctrl Pts',(100.608382744196,-14.1339832402317,
66.4145919634202));
#141501=CARTESIAN_POINT('Ctrl Pts',(100.842794518842,-14.1020595156083,
66.4689747570966));
#141502=CARTESIAN_POINT('Ctrl Pts',(101.079575550411,-14.06880806769,66.5239068806237));
#141503=CARTESIAN_POINT('Ctrl Pts',(101.29374443798,-14.0387320706242,66.5735930894793));
#141504=CARTESIAN_POINT('Ctrl Pts',(101.509851670884,-14.0075697765779,
66.6237287128978));
#141505=CARTESIAN_POINT('Ctrl Pts',(101.727881568406,-13.9752609413613,
66.6743045521247));
#141506=CARTESIAN_POINT('Ctrl Pts',(101.73469078124,-13.9742519158197,66.6758840678586));
#141507=CARTESIAN_POINT('Ctrl Pts',(101.74150186925,-13.9732417718155,66.6774640129205));
#141508=CARTESIAN_POINT('Ctrl Pts',(101.748314831864,-13.9722305075756,
66.6790443870086));
#141509=CARTESIAN_POINT('Ctrl Pts',(101.939045528263,-13.9439198968092,
66.7232873790084));
#141510=CARTESIAN_POINT('Ctrl Pts',(102.131245435303,-13.914731514922,66.7678663795309));
#141511=CARTESIAN_POINT('Ctrl Pts',(102.324901610156,-13.8846258365114,
66.8127747496898));
#141512=CARTESIAN_POINT('Ctrl Pts',(102.506628542656,-13.8563746713085,
66.854916759149));
#141513=CARTESIAN_POINT('Ctrl Pts',(102.68963784033,-13.8273157158036,66.8973488050202));
#141514=CARTESIAN_POINT('Ctrl Pts',(102.873920096121,-13.7974174109149,
66.9400655525872));
#141515=CARTESIAN_POINT('Ctrl Pts',(103.041030899371,-13.7703050352588,
66.9788019462107));
#141516=CARTESIAN_POINT('Ctrl Pts',(103.209188482724,-13.7425024380409,
67.0177724546423));
#141517=CARTESIAN_POINT('Ctrl Pts',(103.378384309845,-13.7139852922797,
67.0569727401741));
#141518=CARTESIAN_POINT('Ctrl Pts',(103.531978313377,-13.6880977591102,
67.0925583033458));
#141519=CARTESIAN_POINT('Ctrl Pts',(103.686427861312,-13.6616213783368,
67.1283332103164));
#141520=CARTESIAN_POINT('Ctrl Pts',(103.841739997656,-13.6345361019978,
67.1642967862645));
#141521=CARTESIAN_POINT('Ctrl Pts',(103.982895043955,-13.609919716404,67.1969821922314));
#141522=CARTESIAN_POINT('Ctrl Pts',(104.124762558038,-13.5848004539271,
67.2298234324098));
#141523=CARTESIAN_POINT('Ctrl Pts',(104.267363231029,-13.5591467521705,
67.2628229687538));
#141524=CARTESIAN_POINT('Ctrl Pts',(104.397096995614,-13.5358077928613,
67.2928449454364));
#141525=CARTESIAN_POINT('Ctrl Pts',(104.527437651834,-13.5120264782336,
67.3229979540809));
#141526=CARTESIAN_POINT('Ctrl Pts',(104.658378047142,-13.4877790297983,
67.3532794135337));
#141527=CARTESIAN_POINT('Ctrl Pts',(104.777697437958,-13.4656835506351,
67.3808733831903));
#141528=CARTESIAN_POINT('Ctrl Pts',(104.8975148222,-13.4432010017889,67.4085740120716));
#141529=CARTESIAN_POINT('Ctrl Pts',(105.017830159682,-13.4203108238425,
67.4363803810496));
#141530=CARTESIAN_POINT('Ctrl Pts',(105.127759789782,-13.3993965426938,
67.4617864840467));
#141531=CARTESIAN_POINT('Ctrl Pts',(105.238105118067,-13.3781419657311,
67.4872808601476));
#141532=CARTESIAN_POINT('Ctrl Pts',(105.348864990805,-13.3565297908362,
67.5128625834291));
#141533=CARTESIAN_POINT('Ctrl Pts',(105.368155212552,-13.3527657593702,
67.5173179615599));
#141534=CARTESIAN_POINT('Ctrl Pts',(105.387458008218,-13.3489908797117,
67.5217759890865));
#141535=CARTESIAN_POINT('Ctrl Pts',(105.406773374803,-13.3452050513228,
67.5262366617009));
#141536=CARTESIAN_POINT('Ctrl Pts',(98.147874059069,-14.16647195032,66.377624860735));
#141537=CARTESIAN_POINT('Ctrl Pts',(98.3192707537691,-14.14960825726,66.410941169501));
#141538=CARTESIAN_POINT('Ctrl Pts',(98.7692528742691,-14.10423461334,66.49840926967));
#141539=CARTESIAN_POINT('Ctrl Pts',(99.475313200169,-14.0284261438,66.63565417898));
#141540=CARTESIAN_POINT('Ctrl Pts',(100.245778761469,-13.93952753982,66.785418260323));
#141541=CARTESIAN_POINT('Ctrl Pts',(100.955266880469,-13.85227099363,66.923329468429));
#141542=CARTESIAN_POINT('Ctrl Pts',(101.608963576769,-13.76716640219,67.050395868438));
#141543=CARTESIAN_POINT('Ctrl Pts',(102.211049942569,-13.68468735089,67.167430186381));
#141544=CARTESIAN_POINT('Ctrl Pts',(102.764974645969,-13.60527459453,67.275102778783));
#141545=CARTESIAN_POINT('Ctrl Pts',(103.274134623369,-13.52925563303,67.374073946483));
#141546=CARTESIAN_POINT('Ctrl Pts',(103.741928092369,-13.45682638993,67.465004239355));
#141547=CARTESIAN_POINT('Ctrl Pts',(104.171681279769,-13.38808134065,67.548540213642));
#141548=CARTESIAN_POINT('Ctrl Pts',(104.566639668869,-13.32295149178,67.625312730527));
#141549=CARTESIAN_POINT('Ctrl Pts',(104.929858598669,-13.26132355552,67.695915690707));
#141550=CARTESIAN_POINT('Ctrl Pts',(105.230722483069,-13.20889210549,67.7543979974229));
#141551=CARTESIAN_POINT('Ctrl Pts',(105.410854685069,-13.1768266842,67.7894123252601));
#141552=CARTESIAN_POINT('Ctrl Pts',(105.479818269769,-13.16444861054,67.8028175550729));
#141553=CARTESIAN_POINT('Ctrl Pts',(98.4917532848691,-15.15283943808,65.107798179803));
#141554=CARTESIAN_POINT('Ctrl Pts',(98.6646840855691,-15.13582480531,65.141412690049));
#141555=CARTESIAN_POINT('Ctrl Pts',(99.118727448469,-15.09004172714,65.229670219725));
#141556=CARTESIAN_POINT('Ctrl Pts',(99.8313090557691,-15.01353347332,65.368182744046));
#141557=CARTESIAN_POINT('Ctrl Pts',(100.609097474869,-14.92379033494,65.519370251844));
#141558=CARTESIAN_POINT('Ctrl Pts',(101.325512002269,-14.83568226642,65.658627824088));
#141559=CARTESIAN_POINT('Ctrl Pts',(101.985742908669,-14.74972723616,65.7869643522));
#141560=CARTESIAN_POINT('Ctrl Pts',(102.593961489469,-14.66640829463,65.905190657944));
#141561=CARTESIAN_POINT('Ctrl Pts',(103.153601372269,-14.58617629943,66.013974174222));
#141562=CARTESIAN_POINT('Ctrl Pts',(103.668070041369,-14.50936478303,66.113977252218));
#141563=CARTESIAN_POINT('Ctrl Pts',(104.140776933769,-14.43617487359,66.205862622613));
#141564=CARTESIAN_POINT('Ctrl Pts',(104.575141584369,-14.36669236077,66.29029497901));
#141565=CARTESIAN_POINT('Ctrl Pts',(104.974569077469,-14.30082583635,66.36793620605));
#141566=CARTESIAN_POINT('Ctrl Pts',(105.342082261369,-14.23846949589,66.439373888846));
#141567=CARTESIAN_POINT('Ctrl Pts',(105.646666250369,-14.18538993416,66.498579314229));
#141568=CARTESIAN_POINT('Ctrl Pts',(105.829109116169,-14.15291324103,66.53404279186));
#141569=CARTESIAN_POINT('Ctrl Pts',(105.898970538669,-14.14037401648,66.547622544524));
#141570=CARTESIAN_POINT('Ctrl Pts',(98.6743292104692,-14.27965323873,63.726550398401));
#141571=CARTESIAN_POINT('Ctrl Pts',(98.8459019370691,-14.26277222601,63.7599009244629));
#141572=CARTESIAN_POINT('Ctrl Pts',(99.2963500670691,-14.21735160134,63.847459608161));
#141573=CARTESIAN_POINT('Ctrl Pts',(100.003158681069,-14.14146283465,63.984849970664));
#141574=CARTESIAN_POINT('Ctrl Pts',(100.774464507769,-14.0524673241,64.134777383871));
#141575=CARTESIAN_POINT('Ctrl Pts',(101.484747401269,-13.96511306951,64.272843081282));
#141576=CARTESIAN_POINT('Ctrl Pts',(102.139193869169,-13.87991089399,64.400055222849));
#141577=CARTESIAN_POINT('Ctrl Pts',(102.741983879469,-13.79733546902,64.517226316099));
#141578=CARTESIAN_POINT('Ctrl Pts',(103.296564374369,-13.71782870864,64.625026382081));
#141579=CARTESIAN_POINT('Ctrl Pts',(103.806333500569,-13.64171880499,64.724115956905));
#141580=CARTESIAN_POINT('Ctrl Pts',(104.274690762969,-13.5692022788,64.815155840681));
#141581=CARTESIAN_POINT('Ctrl Pts',(104.704973095269,-13.50037260886,64.898794670833));
#141582=CARTESIAN_POINT('Ctrl Pts',(105.100444294269,-13.43515822974,64.97566686835));
#141583=CARTESIAN_POINT('Ctrl Pts',(105.464155970669,-13.37344671233,65.0463656092431));
#141584=CARTESIAN_POINT('Ctrl Pts',(105.765446720569,-13.32094089436,65.104930890615));
#141585=CARTESIAN_POINT('Ctrl Pts',(105.945844060969,-13.28882828145,65.1399967563969));
#141586=CARTESIAN_POINT('Ctrl Pts',(106.014910668569,-13.27643171644,65.153422011931));
#141587=CARTESIAN_POINT('Ctrl Pts',(98.4594923245691,-12.67612886135,64.020128731373));
#141588=CARTESIAN_POINT('Ctrl Pts',(98.6285710756692,-12.65949322928,64.052994475293));
#141589=CARTESIAN_POINT('Ctrl Pts',(99.0724168983691,-12.61473821638,64.139269794044));
#141590=CARTESIAN_POINT('Ctrl Pts',(99.7686239528691,-12.53998707959,64.274599411849));
#141591=CARTESIAN_POINT('Ctrl Pts',(100.528025108069,-12.45236451727,64.422212779784));
#141592=CARTESIAN_POINT('Ctrl Pts',(101.227047832369,-12.3663945711,64.558089711098));
#141593=CARTESIAN_POINT('Ctrl Pts',(101.870871722769,-12.28257494254,64.683237022467));
#141594=CARTESIAN_POINT('Ctrl Pts',(102.463692673469,-12.20136491585,64.798470317158));
#141595=CARTESIAN_POINT('Ctrl Pts',(103.008982077969,-12.12318998103,64.904464369116));
#141596=CARTESIAN_POINT('Ctrl Pts',(103.510120935269,-12.04836852325,65.00187638123));
#141597=CARTESIAN_POINT('Ctrl Pts',(103.970490511369,-11.97708860212,65.091363608305));
#141598=CARTESIAN_POINT('Ctrl Pts',(104.393276049869,-11.90945781675,65.173545202099));
#141599=CARTESIAN_POINT('Ctrl Pts',(104.781481886469,-11.84544104117,65.249005149184));
#141600=CARTESIAN_POINT('Ctrl Pts',(105.138212451569,-11.78491368068,65.318346892732));
#141601=CARTESIAN_POINT('Ctrl Pts',(105.433455477569,-11.7334614892,65.375736609798));
#141602=CARTESIAN_POINT('Ctrl Pts',(105.610096402769,-11.7020174754,65.410072298793));
#141603=CARTESIAN_POINT('Ctrl Pts',(105.677703407669,-11.68988289124,65.423213834872));
#141604=CARTESIAN_POINT('Ctrl Pts',(105.406773374803,-13.3452050513228,
67.5262366617009));
#141605=CARTESIAN_POINT('Ctrl Pts',(105.416734125676,-13.3624674052046,
67.4907943810988));
#141606=CARTESIAN_POINT('Ctrl Pts',(105.426800824707,-13.3786476915153,
67.4538067765956));
#141607=CARTESIAN_POINT('Ctrl Pts',(105.436918323535,-13.3934812987196,
67.4153185213962));
#141608=CARTESIAN_POINT('Ctrl Pts',(105.44680434208,-13.4079755248515,67.3777108467017));
#141609=CARTESIAN_POINT('Ctrl Pts',(105.45673880432,-13.4211833350787,67.3386701059155));
#141610=CARTESIAN_POINT('Ctrl Pts',(105.466659412237,-13.4328491135877,
67.2982858097589));
#141611=CARTESIAN_POINT('Ctrl Pts',(105.476285818735,-13.444168936625,67.2590991334795));
#141612=CARTESIAN_POINT('Ctrl Pts',(105.485899070319,-13.4540361373327,
67.2186473412336));
#141613=CARTESIAN_POINT('Ctrl Pts',(105.495433165373,-13.4622186730866,
67.1770603204156));
#141614=CARTESIAN_POINT('Ctrl Pts',(105.504813767443,-13.4702694751185,
67.1361428246943));
#141615=CARTESIAN_POINT('Ctrl Pts',(105.514117612121,-13.4766886950509,
67.0941263620656));
#141616=CARTESIAN_POINT('Ctrl Pts',(105.52327463302,-13.4812672146046,67.0511825584069));
#141617=CARTESIAN_POINT('Ctrl Pts',(105.532244290811,-13.4857520524174,
67.0091174340333));
#141618=CARTESIAN_POINT('Ctrl Pts',(105.541072907105,-13.4884700626533,
66.96616275373));
#141619=CARTESIAN_POINT('Ctrl Pts',(105.549689835139,-13.4892465523338,
66.9225244285964));
#141620=CARTESIAN_POINT('Ctrl Pts',(105.553743287625,-13.4896118175436,
66.9019967095727));
#141621=CARTESIAN_POINT('Ctrl Pts',(105.557749842784,-13.4895478405243,
66.8813183408023));
#141622=CARTESIAN_POINT('Ctrl Pts',(105.561701940056,-13.4890388168851,
66.8605139917143));
#141623=CARTESIAN_POINT('Ctrl Pts',(105.569908612252,-13.4879818109819,
66.8173130122237));
#141624=CARTESIAN_POINT('Ctrl Pts',(105.577880147696,-13.4850031947318,
66.7735680660603));
#141625=CARTESIAN_POINT('Ctrl Pts',(105.585548195281,-13.4799888463478,
66.7295266454243));
#141626=CARTESIAN_POINT('Ctrl Pts',(105.593127183416,-13.4750327364015,
66.685996737618));
#141627=CARTESIAN_POINT('Ctrl Pts',(105.600409498371,-13.4680874471808,
66.6421777804316));
#141628=CARTESIAN_POINT('Ctrl Pts',(105.60733124381,-13.4590851280279,66.5983365748304));
#141629=CARTESIAN_POINT('Ctrl Pts',(105.614188221935,-13.4501670442791,
66.5549055948175));
#141630=CARTESIAN_POINT('Ctrl Pts',(105.620691159308,-13.4392299403628,
66.511453466019));
#141631=CARTESIAN_POINT('Ctrl Pts',(105.626782851463,-13.4262553715034,
66.4682576499431));
#141632=CARTESIAN_POINT('Ctrl Pts',(105.632831399466,-13.4133726944771,
66.4253677664004));
#141633=CARTESIAN_POINT('Ctrl Pts',(105.638474338109,-13.3984811831692,
66.3827313295392));
#141634=CARTESIAN_POINT('Ctrl Pts',(105.643663200714,-13.3816131129061,
66.3406271353247));
#141635=CARTESIAN_POINT('Ctrl Pts',(105.648825111233,-13.3648326590884,
66.2987416395013));
#141636=CARTESIAN_POINT('Ctrl Pts',(105.653537512519,-13.3460961921019,
66.2573836419157));
#141637=CARTESIAN_POINT('Ctrl Pts',(105.657762469329,-13.3254859593339,
66.2168233627578));
#141638=CARTESIAN_POINT('Ctrl Pts',(105.661980909241,-13.3049075173765,
66.1763256468989));
#141639=CARTESIAN_POINT('Ctrl Pts',(105.665713305536,-13.2824613297786,
66.1366239365531));
#141640=CARTESIAN_POINT('Ctrl Pts',(105.668933485206,-13.2582774310437,
66.0979715501854));
#141641=CARTESIAN_POINT('Ctrl Pts',(105.67215525787,-13.2340815687411,66.059300042813));
#141642=CARTESIAN_POINT('Ctrl Pts',(105.674864251458,-13.2081466988365,
66.0216795698616));
#141643=CARTESIAN_POINT('Ctrl Pts',(105.677047053913,-13.1806462961128,
65.9853374431438));
#141644=CARTESIAN_POINT('Ctrl Pts',(105.679235389074,-13.1530761886772,
65.948903200776));
#141645=CARTESIAN_POINT('Ctrl Pts',(105.680894856989,-13.1239331775076,
65.9137543455201));
#141646=CARTESIAN_POINT('Ctrl Pts',(105.682025272019,-13.0934279909319,
65.8800841419623));
#141647=CARTESIAN_POINT('Ctrl Pts',(105.683166173587,-13.0626398164298,
65.8461015895171));
#141648=CARTESIAN_POINT('Ctrl Pts',(105.683768196746,-13.0304647557896,
65.8136256862783));
#141649=CARTESIAN_POINT('Ctrl Pts',(105.683844504273,-12.9971465327891,
65.7828111360314));
#141650=CARTESIAN_POINT('Ctrl Pts',(105.683921267299,-12.9636294248799,
65.7518126459323));
#141651=CARTESIAN_POINT('Ctrl Pts',(105.683466115453,-12.9289562400225,
65.7224956156532));
#141652=CARTESIAN_POINT('Ctrl Pts',(105.68250488943,-12.8933912866128,65.6949683115688));
#141653=CARTESIAN_POINT('Ctrl Pts',(105.681529725943,-12.8573106529629,
65.6670418705413));
#141654=CARTESIAN_POINT('Ctrl Pts',(105.680033833554,-12.8203130016877,
65.6409575062467));
#141655=CARTESIAN_POINT('Ctrl Pts',(105.678055280779,-12.7826789266197,
65.6167754398037));
#141656=CARTESIAN_POINT('Ctrl Pts',(105.676291466558,-12.7491293960437,
65.5952179290623));
#141657=CARTESIAN_POINT('Ctrl Pts',(105.674144315099,-12.7150744959912,
65.5751713377354));
#141658=CARTESIAN_POINT('Ctrl Pts',(105.671646638611,-12.6807085185017,
65.5566441699934));
#141659=CARTESIAN_POINT('Ctrl Pts',(105.668775916753,-12.6412097430363,
65.5353498407728));
#141660=CARTESIAN_POINT('Ctrl Pts',(105.665442179767,-12.6013009501918,
65.5160633596856));
#141661=CARTESIAN_POINT('Ctrl Pts',(105.661701496265,-12.561260204733,65.4987500365353));
#141662=CARTESIAN_POINT('Ctrl Pts',(105.657902192529,-12.5205919809412,
65.4811653963796));
#141663=CARTESIAN_POINT('Ctrl Pts',(105.653683288102,-12.4797882328283,
65.4656157553205));
#141664=CARTESIAN_POINT('Ctrl Pts',(105.64910744664,-12.4391121897216,65.4520189555552));
#141665=CARTESIAN_POINT('Ctrl Pts',(105.644402469273,-12.3972882183761,
65.4380384372859));
#141666=CARTESIAN_POINT('Ctrl Pts',(105.639320327356,-12.3555997906835,
65.4261219763008));
#141667=CARTESIAN_POINT('Ctrl Pts',(105.633930130516,-12.3142947246995,
65.4161401886094));
#141668=CARTESIAN_POINT('Ctrl Pts',(105.628448069826,-12.2722857062425,
65.4059882836706));
#141669=CARTESIAN_POINT('Ctrl Pts',(105.622647554534,-12.2306734997387,
65.3978368288397));
#141670=CARTESIAN_POINT('Ctrl Pts',(105.616599251241,-12.189673606019,65.3915189375991));
#141671=CARTESIAN_POINT('Ctrl Pts',(105.610377006754,-12.1474946096516,
65.3850193521732));
#141672=CARTESIAN_POINT('Ctrl Pts',(105.603892691435,-12.1059638194751,
65.3804595659265));
#141673=CARTESIAN_POINT('Ctrl Pts',(105.597218269814,-12.0652648663608,
65.3776369306512));
#141674=CARTESIAN_POINT('Ctrl Pts',(105.594248782885,-12.047157678023,65.3763811246751));
#141675=CARTESIAN_POINT('Ctrl Pts',(105.591241585468,-12.029214467156,65.3754689690382));
#141676=CARTESIAN_POINT('Ctrl Pts',(105.588202588019,-12.0114482303019,
65.3748819173935));
#141677=CARTESIAN_POINT('Ctrl Pts',(104.952232036869,-12.73587741823,68.1320028366331));
#141678=CARTESIAN_POINT('Ctrl Pts',(104.959822185469,-12.73457436689,68.133478219418));
#141679=CARTESIAN_POINT('Ctrl Pts',(105.015863075569,-12.7249411692,68.144371519325));
#141680=CARTESIAN_POINT('Ctrl Pts',(105.118775843869,-12.70706879104,68.1643758348569));
#141681=CARTESIAN_POINT('Ctrl Pts',(105.261221405869,-12.68166925282,68.192064585411));
#141682=CARTESIAN_POINT('Ctrl Pts',(105.402364938369,-12.65578816422,68.219500245804));
#141683=CARTESIAN_POINT('Ctrl Pts',(105.543618402569,-12.6301955777,68.246957274863));
#141684=CARTESIAN_POINT('Ctrl Pts',(105.687431557269,-12.60472429698,68.274911859823));
#141685=CARTESIAN_POINT('Ctrl Pts',(105.823449722569,-12.58115097953,68.30135124478));
#141686=CARTESIAN_POINT('Ctrl Pts',(105.963723330769,-12.55697430171,68.3286178081799));
#141687=CARTESIAN_POINT('Ctrl Pts',(106.097164283069,-12.52886481947,68.35455623118));
#141688=CARTESIAN_POINT('Ctrl Pts',(106.234154640669,-12.5005565727,68.381184592121));
#141689=CARTESIAN_POINT('Ctrl Pts',(106.374425007569,-12.47109589523,68.408450525463));
#141690=CARTESIAN_POINT('Ctrl Pts',(106.520440250569,-12.44039854804,68.436833155168));
#141691=CARTESIAN_POINT('Ctrl Pts',(106.676875480469,-12.40715650872,68.467241235266));
#141692=CARTESIAN_POINT('Ctrl Pts',(106.847058876369,-12.37032464115,68.500321701448));
#141693=CARTESIAN_POINT('Ctrl Pts',(107.032307995569,-12.32930601219,68.536330662197));
#141694=CARTESIAN_POINT('Ctrl Pts',(107.233857295369,-12.28362359072,68.575508072906));
#141695=CARTESIAN_POINT('Ctrl Pts',(107.452609118669,-12.23279531428,68.6180293321429));
#141696=CARTESIAN_POINT('Ctrl Pts',(107.689333475969,-12.17635893667,68.664044115523));
#141697=CARTESIAN_POINT('Ctrl Pts',(107.945108470469,-12.1136901956,68.713761986126));
#141698=CARTESIAN_POINT('Ctrl Pts',(108.221352645369,-12.04394693307,68.767458682204));
#141699=CARTESIAN_POINT('Ctrl Pts',(108.519904230369,-11.96606158696,68.825491521187));
#141700=CARTESIAN_POINT('Ctrl Pts',(108.842656572169,-11.87879604663,68.888228534223));
#141701=CARTESIAN_POINT('Ctrl Pts',(109.191603713569,-11.78073386166,68.956057325939));
#141702=CARTESIAN_POINT('Ctrl Pts',(109.568887864469,-11.67018852649,69.029394301794));
#141703=CARTESIAN_POINT('Ctrl Pts',(109.976855656869,-11.54513335067,69.1086956031249));
#141704=CARTESIAN_POINT('Ctrl Pts',(110.418012265769,-11.40313753581,69.1944481890609));
#141705=CARTESIAN_POINT('Ctrl Pts',(110.895045258669,-11.2412511075,69.28717447242));
#141706=CARTESIAN_POINT('Ctrl Pts',(111.410817072669,-11.05585348146,69.387430857371));
#141707=CARTESIAN_POINT('Ctrl Pts',(111.968193872269,-10.84255144708,69.495774472649));
#141708=CARTESIAN_POINT('Ctrl Pts',(112.570412941369,-10.59580176849,69.612834585628));
#141709=CARTESIAN_POINT('Ctrl Pts',(113.220235519769,-10.3088878416,69.7391479296449));
#141710=CARTESIAN_POINT('Ctrl Pts',(113.920526429469,-9.97338727422198,
69.8752713724391));
#141711=CARTESIAN_POINT('Ctrl Pts',(114.673362321169,-9.57892440546198,
70.021608576066));
#141712=CARTESIAN_POINT('Ctrl Pts',(115.480641495669,-9.11187730365798,
70.178528534627));
#141713=CARTESIAN_POINT('Ctrl Pts',(116.342765158169,-8.55458391315699,
70.346109234944));
#141714=CARTESIAN_POINT('Ctrl Pts',(117.226756584969,-7.90619100724499,
70.517940619224));
#141715=CARTESIAN_POINT('Ctrl Pts',(118.060477130769,-7.20202699572299,
70.680000285382));
#141716=CARTESIAN_POINT('Ctrl Pts',(118.784806129869,-6.495187570145,70.8207962827541));
#141717=CARTESIAN_POINT('Ctrl Pts',(119.382258340369,-5.82452362446499,
70.9369298076469));
#141718=CARTESIAN_POINT('Ctrl Pts',(119.873935776169,-5.19148602277899,
71.032502696561));
#141719=CARTESIAN_POINT('Ctrl Pts',(120.279478642169,-4.59391006016099,
71.11133263759));
#141720=CARTESIAN_POINT('Ctrl Pts',(120.613855905469,-4.02868582297099,
71.176329317749));
#141721=CARTESIAN_POINT('Ctrl Pts',(120.887058111969,-3.49549879784399,
71.229434712121));
#141722=CARTESIAN_POINT('Ctrl Pts',(121.107492496269,-2.99524221621799,
71.272283029704));
#141723=CARTESIAN_POINT('Ctrl Pts',(121.282922740269,-2.52901011200199,
71.30638338495));
#141724=CARTESIAN_POINT('Ctrl Pts',(121.421275086969,-2.09491375878399,
71.333276491063));
#141725=CARTESIAN_POINT('Ctrl Pts',(121.528476941569,-1.69170413216199,
71.3541145246909));
#141726=CARTESIAN_POINT('Ctrl Pts',(121.609328944569,-1.31874211906699,
71.369830640449));
#141727=CARTESIAN_POINT('Ctrl Pts',(121.667923195969,-0.974734023751388,
71.381220265999));
#141728=CARTESIAN_POINT('Ctrl Pts',(121.707625940769,-0.658282511519486,
71.388937736322));
#141729=CARTESIAN_POINT('Ctrl Pts',(121.731363094969,-0.367700522520886,
71.393551794715));
#141730=CARTESIAN_POINT('Ctrl Pts',(121.741634599469,-0.101175225261786,
71.395548382888));
#141731=CARTESIAN_POINT('Ctrl Pts',(121.740745608969,0.102180689578914,
71.395375579788));
#141732=CARTESIAN_POINT('Ctrl Pts',(121.736614525769,0.216805681933914,
71.3945725745509));
#141733=CARTESIAN_POINT('Ctrl Pts',(121.735103526269,0.249988879730614,
71.394278864527));
#141734=CARTESIAN_POINT('Ctrl Pts',(105.492580541969,-14.75894581259,67.138711581365));
#141735=CARTESIAN_POINT('Ctrl Pts',(105.500469740069,-14.75759123539,67.140245093777));
#141736=CARTESIAN_POINT('Ctrl Pts',(105.558768713869,-14.7475691159,67.15157732288));
#141737=CARTESIAN_POINT('Ctrl Pts',(105.666629227569,-14.72884244559,67.172543387499));
#141738=CARTESIAN_POINT('Ctrl Pts',(105.819635636069,-14.70155594623,67.202284968906));
#141739=CARTESIAN_POINT('Ctrl Pts',(105.965965642769,-14.67472441123,67.2307287827801));
#141740=CARTESIAN_POINT('Ctrl Pts',(106.095643432669,-14.65123731042,67.2559357174571));
#141741=CARTESIAN_POINT('Ctrl Pts',(106.240626942769,-14.62551395671,67.284117797616));
#141742=CARTESIAN_POINT('Ctrl Pts',(106.346379463669,-14.6074213232,67.304674107888));
#141743=CARTESIAN_POINT('Ctrl Pts',(106.565377381869,-14.5688173883,67.347243203358));
#141744=CARTESIAN_POINT('Ctrl Pts',(106.702418711469,-14.53959176337,67.37388147231));
#141745=CARTESIAN_POINT('Ctrl Pts',(106.845617522769,-14.51009959534,67.401716640428));
#141746=CARTESIAN_POINT('Ctrl Pts',(106.986141518569,-14.48055441258,67.429031874481));
#141747=CARTESIAN_POINT('Ctrl Pts',(107.135114434969,-14.44924442858,67.4579894205271));
#141748=CARTESIAN_POINT('Ctrl Pts',(107.296863943769,-14.41487311883,67.4894304969489));
#141749=CARTESIAN_POINT('Ctrl Pts',(107.476158454069,-14.37607194618,67.524281993211));
#141750=CARTESIAN_POINT('Ctrl Pts',(107.670628850969,-14.33300989809,67.562083397709));
#141751=CARTESIAN_POINT('Ctrl Pts',(107.882299752669,-14.2850339185,67.603228258333));
#141752=CARTESIAN_POINT('Ctrl Pts',(108.111834366569,-14.23169947047,67.647845490204));
#141753=CARTESIAN_POINT('Ctrl Pts',(108.359969891769,-14.17254283898,67.696078390983));
#141754=CARTESIAN_POINT('Ctrl Pts',(108.628544882169,-14.1067388206,67.748284341169));
#141755=CARTESIAN_POINT('Ctrl Pts',(108.919099624169,-14.03338368093,67.804762743585));
#141756=CARTESIAN_POINT('Ctrl Pts',(109.233784324169,-13.95129086149,67.8659315580971));
#141757=CARTESIAN_POINT('Ctrl Pts',(109.574509226469,-13.85916720993,67.932162100438));
#141758=CARTESIAN_POINT('Ctrl Pts',(109.943480085769,-13.75547965436,68.003883128056));
#141759=CARTESIAN_POINT('Ctrl Pts',(110.343130829169,-13.63838326156,68.0815677507689));
#141760=CARTESIAN_POINT('Ctrl Pts',(110.776141189469,-13.50565488543,68.165736858487));
#141761=CARTESIAN_POINT('Ctrl Pts',(111.245388189769,-13.354622112,68.256949690632));
#141762=CARTESIAN_POINT('Ctrl Pts',(111.754109128869,-13.18198856946,68.3558355175029));
#141763=CARTESIAN_POINT('Ctrl Pts',(112.305743248969,-12.9837090819,68.463062863392));
#141764=CARTESIAN_POINT('Ctrl Pts',(112.903812062269,-12.75484751004,68.579316244352));
#141765=CARTESIAN_POINT('Ctrl Pts',(113.552372588269,-12.48912859477,68.705384268995));
#141766=CARTESIAN_POINT('Ctrl Pts',(114.255050788269,-12.17890247091,68.841971756345));
#141767=CARTESIAN_POINT('Ctrl Pts',(115.015487040869,-11.81462198028,68.989786327825));
#141768=CARTESIAN_POINT('Ctrl Pts',(115.837112874269,-11.38417047417,69.149495008306));
#141769=CARTESIAN_POINT('Ctrl Pts',(116.723420541269,-10.87148884659,69.32177662635));
#141770=CARTESIAN_POINT('Ctrl Pts',(117.676819254069,-10.25533692963,69.507099487684));
#141771=CARTESIAN_POINT('Ctrl Pts',(118.663346228469,-9.53199294674199,
69.69886186288));
#141772=CARTESIAN_POINT('Ctrl Pts',(119.604511054069,-8.73743036268499,
69.881806685573));
#141773=CARTESIAN_POINT('Ctrl Pts',(120.432208031169,-7.93008953233,70.042695482718));
#141774=CARTESIAN_POINT('Ctrl Pts',(121.123557856069,-7.15431205073399,
70.1770809460259));
#141775=CARTESIAN_POINT('Ctrl Pts',(121.698017157269,-6.41492080923599,
70.2887450798039));
#141776=CARTESIAN_POINT('Ctrl Pts',(122.176477179669,-5.71015914524499,
70.381748750991));
#141777=CARTESIAN_POINT('Ctrl Pts',(122.575512542569,-5.03589455575199,
70.459313755258));
#141778=CARTESIAN_POINT('Ctrl Pts',(122.905036512669,-4.39304561090499,
70.523367046078));
#141779=CARTESIAN_POINT('Ctrl Pts',(123.173320684769,-3.78433296845899,
70.575516466625));
#141780=CARTESIAN_POINT('Ctrl Pts',(123.387691659769,-3.21470112064199,
70.617186170945));
#141781=CARTESIAN_POINT('Ctrl Pts',(123.557630545669,-2.68164729664499,
70.650219108973));
#141782=CARTESIAN_POINT('Ctrl Pts',(123.690314882669,-2.18277829981599,
70.6760104601161));
#141783=CARTESIAN_POINT('Ctrl Pts',(123.791288846669,-1.71727622468999,
70.695637908411));
#141784=CARTESIAN_POINT('Ctrl Pts',(123.865481191169,-1.28212654844499,
70.710059511236));
#141785=CARTESIAN_POINT('Ctrl Pts',(123.916585892469,-0.875408245070486,
70.719993308449));
#141786=CARTESIAN_POINT('Ctrl Pts',(123.947740644269,-0.495009380945386,
70.726049208952));
#141787=CARTESIAN_POINT('Ctrl Pts',(123.961550139369,-0.138830407839186,
70.728733516261));
#141788=CARTESIAN_POINT('Ctrl Pts',(123.960405633669,0.139179398717814,
70.7285110457929));
#141789=CARTESIAN_POINT('Ctrl Pts',(123.954664204369,0.298769253595514,
70.727395019413));
#141790=CARTESIAN_POINT('Ctrl Pts',(123.952552482969,0.345228639253714,
70.7269845403021));
#141791=CARTESIAN_POINT('Ctrl Pts',(105.782108038469,-13.99115798116,64.971205130231));
#141792=CARTESIAN_POINT('Ctrl Pts',(105.789883742369,-13.98982295888,64.972716581491));
#141793=CARTESIAN_POINT('Ctrl Pts',(105.847325736169,-13.97994844163,64.983882229722));
#141794=CARTESIAN_POINT('Ctrl Pts',(105.953308498869,-13.96154598928,65.004483294697));
#141795=CARTESIAN_POINT('Ctrl Pts',(106.102306891869,-13.93497562281,65.033445792928));
#141796=CARTESIAN_POINT('Ctrl Pts',(106.246668546069,-13.9085047979,65.061506995923));
#141797=CARTESIAN_POINT('Ctrl Pts',(106.380739495269,-13.88421863053,65.0875678785401));
#141798=CARTESIAN_POINT('Ctrl Pts',(106.525278836269,-13.85859094267,65.115663620517));
#141799=CARTESIAN_POINT('Ctrl Pts',(106.642517668469,-13.83841829919,65.138452654689));
#141800=CARTESIAN_POINT('Ctrl Pts',(106.831638412269,-13.80528974637,65.175214186783));
#141801=CARTESIAN_POINT('Ctrl Pts',(106.967313339269,-13.776487716,65.2015868526511));
#141802=CARTESIAN_POINT('Ctrl Pts',(107.108155939969,-13.74744486562,65.228964017536));
#141803=CARTESIAN_POINT('Ctrl Pts',(107.248583679469,-13.71793175401,65.256260541156));
#141804=CARTESIAN_POINT('Ctrl Pts',(107.396434109969,-13.68685427579,65.284999896966));
#141805=CARTESIAN_POINT('Ctrl Pts',(107.556166762269,-13.6529115428,65.316048934241));
#141806=CARTESIAN_POINT('Ctrl Pts',(107.732003454369,-13.61485775391,65.3502282953701));
#141807=CARTESIAN_POINT('Ctrl Pts',(107.922974224169,-13.57257121709,65.387349437894));
#141808=CARTESIAN_POINT('Ctrl Pts',(108.130803810969,-13.52546568065,65.427747618817));
#141809=CARTESIAN_POINT('Ctrl Pts',(108.356246177969,-13.47308236608,65.471569394495));
#141810=CARTESIAN_POINT('Ctrl Pts',(108.600050976669,-13.41495811582,65.518960483128));
#141811=CARTESIAN_POINT('Ctrl Pts',(108.863768157469,-13.3503439869,65.570222166064));
#141812=CARTESIAN_POINT('Ctrl Pts',(109.148891803169,-13.2783596142,65.625644865033));
#141813=CARTESIAN_POINT('Ctrl Pts',(109.457453719869,-13.19786360029,65.685623525096));
#141814=CARTESIAN_POINT('Ctrl Pts',(109.791357738969,-13.1075836821,65.750528215431));
#141815=CARTESIAN_POINT('Ctrl Pts',(110.152729267069,-13.00603104747,65.820772075312));
#141816=CARTESIAN_POINT('Ctrl Pts',(110.543891519569,-12.89142088912,65.896806694317));
#141817=CARTESIAN_POINT('Ctrl Pts',(110.967397812269,-12.7616046191,65.9791283892041));
#141818=CARTESIAN_POINT('Ctrl Pts',(111.425984045469,-12.61400152053,66.0682689678321));
#141819=CARTESIAN_POINT('Ctrl Pts',(111.922678886269,-12.44544668515,66.164817146322));
#141820=CARTESIAN_POINT('Ctrl Pts',(112.460702669569,-12.25205607655,66.269398897531));
#141821=CARTESIAN_POINT('Ctrl Pts',(113.043328192369,-12.02909960586,66.382650391923));
#141822=CARTESIAN_POINT('Ctrl Pts',(113.674301370969,-11.77057982886,66.50529976548));
#141823=CARTESIAN_POINT('Ctrl Pts',(114.356919990569,-11.46920106834,66.637988045937));
#141824=CARTESIAN_POINT('Ctrl Pts',(115.094530093269,-11.11584303338,66.7813656412041));
#141825=CARTESIAN_POINT('Ctrl Pts',(115.890049008869,-10.69904980887,66.9359996256221));
#141826=CARTESIAN_POINT('Ctrl Pts',(116.746364059269,-10.20368723669,67.102451240462));
#141827=CARTESIAN_POINT('Ctrl Pts',(117.665122384669,-9.60987310153999,
67.281040658987));
#141828=CARTESIAN_POINT('Ctrl Pts',(118.612735427169,-8.91497428887999,
67.4652388943169));
#141829=CARTESIAN_POINT('Ctrl Pts',(119.513123375969,-8.15471945445799,
67.64025745555));
#141830=CARTESIAN_POINT('Ctrl Pts',(120.301590500069,-7.38552056524799,
67.7935207036991));
#141831=CARTESIAN_POINT('Ctrl Pts',(120.957304631269,-6.64963540465299,
67.920979255265));
#141832=CARTESIAN_POINT('Ctrl Pts',(121.500346848769,-5.95060712404298,
68.02653649615));
#141833=CARTESIAN_POINT('Ctrl Pts',(121.951133607369,-5.28652420202899,
68.114161002909));
#141834=CARTESIAN_POINT('Ctrl Pts',(122.325630154769,-4.65364222513899,
68.186956120831));
#141835=CARTESIAN_POINT('Ctrl Pts',(122.633779086469,-4.05241178798398,
68.246854504334));
#141836=CARTESIAN_POINT('Ctrl Pts',(122.883903474669,-3.48486000988298,
68.29547400286));
#141837=CARTESIAN_POINT('Ctrl Pts',(123.083495799869,-2.95447007060999,
68.3342710143309));
#141838=CARTESIAN_POINT('Ctrl Pts',(123.241447072969,-2.45897223933399,
68.364973784855));
#141839=CARTESIAN_POINT('Ctrl Pts',(123.364460387569,-1.99640755164799,
68.388885270283));
#141840=CARTESIAN_POINT('Ctrl Pts',(123.457797735369,-1.56602595675199,
68.407028303353));
#141841=CARTESIAN_POINT('Ctrl Pts',(123.526070346269,-1.16546601408599,
68.420299220781));
#141842=CARTESIAN_POINT('Ctrl Pts',(123.572847816969,-0.793005447135286,
68.429391885375));
#141843=CARTESIAN_POINT('Ctrl Pts',(123.601187468069,-0.446693568883186,
68.434900583011));
#141844=CARTESIAN_POINT('Ctrl Pts',(123.613654237269,-0.124539644830986,
68.437323889562));
#141845=CARTESIAN_POINT('Ctrl Pts',(123.612606703869,0.125137778209914,
68.43712026868));
#141846=CARTESIAN_POINT('Ctrl Pts',(123.607476427469,0.267662725948114,
68.436123038987));
#141847=CARTESIAN_POINT('Ctrl Pts',(123.605592689969,0.309083579287614,
68.4357568756719));
#141848=CARTESIAN_POINT('Ctrl Pts',(105.323272139269,-11.75192916108,65.354263847219));
#141849=CARTESIAN_POINT('Ctrl Pts',(105.330716840869,-11.75065117009,65.355710957828));
#141850=CARTESIAN_POINT('Ctrl Pts',(105.385659479669,-11.74120713008,65.36639077824));
#141851=CARTESIAN_POINT('Ctrl Pts',(105.486165841169,-11.72375024912,65.385927333345));
#141852=CARTESIAN_POINT('Ctrl Pts',(105.623474984369,-11.69926846146,65.412617660244));
#141853=CARTESIAN_POINT('Ctrl Pts',(105.762096000969,-11.67384963606,65.439562990768));
#141854=CARTESIAN_POINT('Ctrl Pts',(105.908979459969,-11.64723301644,65.468114385421));
#141855=CARTESIAN_POINT('Ctrl Pts',(106.052223395469,-11.62188433502,65.4959583248361));
#141856=CARTESIAN_POINT('Ctrl Pts',(106.202961689969,-11.59564540853,65.5252590273339));
#141857=CARTESIAN_POINT('Ctrl Pts',(106.304946603769,-11.5784856336,65.545082985332));
#141858=CARTESIAN_POINT('Ctrl Pts',(106.436636461069,-11.55091900332,65.570681028241));
#141859=CARTESIAN_POINT('Ctrl Pts',(106.570607248369,-11.5231865736,65.596722441247));
#141860=CARTESIAN_POINT('Ctrl Pts',(106.710754259169,-11.49376699648,65.623964396482));
#141861=CARTESIAN_POINT('Ctrl Pts',(106.855330995369,-11.46336761397,65.6520674073999));
#141862=CARTESIAN_POINT('Ctrl Pts',(107.009181549769,-11.43067481148,65.681973074956));
#141863=CARTESIAN_POINT('Ctrl Pts',(107.174933624769,-11.3948007436,65.714192175322));
#141864=CARTESIAN_POINT('Ctrl Pts',(107.355697843669,-11.35477596077,65.7493293554091));
#141865=CARTESIAN_POINT('Ctrl Pts',(107.552324357569,-11.31020904411,65.787549868703));
#141866=CARTESIAN_POINT('Ctrl Pts',(107.765831816469,-11.26059968008,65.829051721663));
#141867=CARTESIAN_POINT('Ctrl Pts',(107.997006189069,-11.20548633686,65.873987691913));
#141868=CARTESIAN_POINT('Ctrl Pts',(108.246555722369,-11.14434248276,65.922495449414));
#141869=CARTESIAN_POINT('Ctrl Pts',(108.515839748269,-11.07635590836,65.9748392228171));
#141870=CARTESIAN_POINT('Ctrl Pts',(108.806544761969,-11.0005169271,66.031346835236));
#141871=CARTESIAN_POINT('Ctrl Pts',(109.120555891769,-10.91561419867,66.092384720314));
#141872=CARTESIAN_POINT('Ctrl Pts',(109.459764211569,-10.82028799318,66.158320467413));
#141873=CARTESIAN_POINT('Ctrl Pts',(109.826170050169,-10.71292885861,66.229542903018));
#141874=CARTESIAN_POINT('Ctrl Pts',(110.221958031369,-10.59160565353,66.306476677071));
#141875=CARTESIAN_POINT('Ctrl Pts',(110.649452476469,-10.45400509277,66.389573594144));
#141876=CARTESIAN_POINT('Ctrl Pts',(111.111073583469,-10.29734567721,66.479304095394));
#141877=CARTESIAN_POINT('Ctrl Pts',(111.609403251769,-10.11821332882,66.57617005376));
#141878=CARTESIAN_POINT('Ctrl Pts',(112.146988908369,-9.91247889809999,
66.6806666413349));
#141879=CARTESIAN_POINT('Ctrl Pts',(112.726669146869,-9.674955179165,66.7933456276021));
#141880=CARTESIAN_POINT('Ctrl Pts',(113.350784637569,-9.399379472793,66.91466199502));
#141881=CARTESIAN_POINT('Ctrl Pts',(114.021822999269,-9.07787643283398,
67.045099290116));
#141882=CARTESIAN_POINT('Ctrl Pts',(114.741201918669,-8.70091715272899,
67.1849330846709));
#141883=CARTESIAN_POINT('Ctrl Pts',(115.510044455069,-8.25606505541699,
67.334381680369));
#141884=CARTESIAN_POINT('Ctrl Pts',(116.327775191169,-7.727398351337,67.493333226842));
#141885=CARTESIAN_POINT('Ctrl Pts',(117.161896987269,-7.11545897401699,
67.655470888542));
#141886=CARTESIAN_POINT('Ctrl Pts',(117.943360470569,-6.45526160155699,
67.807372760021));
#141887=CARTESIAN_POINT('Ctrl Pts',(118.617414974669,-5.79730247204099,
67.938396336759));
#141888=CARTESIAN_POINT('Ctrl Pts',(119.169198736969,-5.17776199838799,
68.0456527702781));
#141889=CARTESIAN_POINT('Ctrl Pts',(119.620614028269,-4.59645101100099,
68.133399452039));
#141890=CARTESIAN_POINT('Ctrl Pts',(119.990692591969,-4.05100634772499,
68.205335796626));
#141891=CARTESIAN_POINT('Ctrl Pts',(120.293622463469,-3.53881544589199,
68.2642196925429));
#141892=CARTESIAN_POINT('Ctrl Pts',(120.539431774469,-3.05896406432699,
68.3120004208479));
#141893=CARTESIAN_POINT('Ctrl Pts',(120.736593729869,-2.61145663953499,
68.350325013936));
#141894=CARTESIAN_POINT('Ctrl Pts',(120.893084592369,-2.19551447993599,
68.3807439079669));
#141895=CARTESIAN_POINT('Ctrl Pts',(121.016074373769,-1.80954750839099,
68.404650818987));
#141896=CARTESIAN_POINT('Ctrl Pts',(121.110882458469,-1.45286318504499,
68.423079735776));
#141897=CARTESIAN_POINT('Ctrl Pts',(121.181947857769,-1.12490935506699,
68.4368935189959));
#141898=CARTESIAN_POINT('Ctrl Pts',(121.232955753569,-0.825229271576386,
68.44680849902));
#141899=CARTESIAN_POINT('Ctrl Pts',(121.267112993769,-0.552680304641586,
68.453448027053));
#141900=CARTESIAN_POINT('Ctrl Pts',(121.287242493169,-0.305782037849186,
68.457360824907));
#141901=CARTESIAN_POINT('Ctrl Pts',(121.295793245269,-0.0828610884916358,
68.459022931039));
#141902=CARTESIAN_POINT('Ctrl Pts',(121.295028528269,0.0841858380577142,
68.458874284375));
#141903=CARTESIAN_POINT('Ctrl Pts',(121.291680659969,0.176941526223414,
68.458223521449));
#141904=CARTESIAN_POINT('Ctrl Pts',(121.290461830169,0.203667660114414,
68.457986603741));
#141905=CARTESIAN_POINT('Ctrl Pts',(105.406735574489,-13.3447234534956,
67.5259914523896));
#141906=CARTESIAN_POINT('Ctrl Pts',(105.419348855129,-13.3424555725803,
67.5284994651872));
#141907=CARTESIAN_POINT('Ctrl Pts',(105.432007480475,-13.340144416473,67.5310693565358));
#141908=CARTESIAN_POINT('Ctrl Pts',(105.44466272379,-13.3377895139349,67.5337091593829));
#141909=CARTESIAN_POINT('Ctrl Pts',(105.4595503261,-13.3350192114135,67.5368146180442));
#141910=CARTESIAN_POINT('Ctrl Pts',(105.474434021802,-13.3321885390212,
67.5400163316475));
#141911=CARTESIAN_POINT('Ctrl Pts',(105.489300427801,-13.3293085895235,
67.5432963615387));
#141912=CARTESIAN_POINT('Ctrl Pts',(105.505021656339,-13.3262630421172,
67.5467649940739));
#141913=CARTESIAN_POINT('Ctrl Pts',(105.52072783756,-13.3231632268862,67.5503189569254));
#141914=CARTESIAN_POINT('Ctrl Pts',(105.536428766284,-13.3200260560355,
67.5539280211083));
#141915=CARTESIAN_POINT('Ctrl Pts',(105.550053300076,-13.3173037654616,
67.557059798711));
#141916=CARTESIAN_POINT('Ctrl Pts',(105.563676092547,-13.3145537563832,
67.5602320101648));
#141917=CARTESIAN_POINT('Ctrl Pts',(105.577277511334,-13.3117813163253,
67.5634408239287));
#141918=CARTESIAN_POINT('Ctrl Pts',(105.579350383511,-13.3113587932084,
67.5639298509103));
#141919=CARTESIAN_POINT('Ctrl Pts',(105.581422673761,-13.310935731282,67.5644197761276));
#141920=CARTESIAN_POINT('Ctrl Pts',(105.583494211195,-13.3105121282584,
67.564910642499));
#141921=CARTESIAN_POINT('Ctrl Pts',(105.595509025827,-13.3080552516775,
67.5677576431688));
#141922=CARTESIAN_POINT('Ctrl Pts',(105.607502181302,-13.3055808108532,
67.5706348249016));
#141923=CARTESIAN_POINT('Ctrl Pts',(105.619424338444,-13.3030823900979,
67.5735715360503));
#141924=CARTESIAN_POINT('Ctrl Pts',(105.624099925604,-13.3021025687565,
67.574723244485));
#141925=CARTESIAN_POINT('Ctrl Pts',(105.628764089798,-13.3011189716412,
67.5758843118018));
#141926=CARTESIAN_POINT('Ctrl Pts',(105.633411799757,-13.3001308573854,
67.5770573205464));
#141927=CARTESIAN_POINT('Ctrl Pts',(105.650114324641,-13.2965798606385,
67.5812727745909));
#141928=CARTESIAN_POINT('Ctrl Pts',(105.666708531094,-13.2929881960317,
67.585592200278));
#141929=CARTESIAN_POINT('Ctrl Pts',(105.683281251363,-13.2893570357737,
67.5900082142077));
#141930=CARTESIAN_POINT('Ctrl Pts',(105.710542028484,-13.2833840724412,
67.5972721980045));
#141931=CARTESIAN_POINT('Ctrl Pts',(105.737741142737,-13.2773032862321,
67.6048004028214));
#141932=CARTESIAN_POINT('Ctrl Pts',(105.765107084503,-13.2711032057106,
67.6125810102969));
#141933=CARTESIAN_POINT('Ctrl Pts',(105.780782298461,-13.2675517990181,
67.6170377429738));
#141934=CARTESIAN_POINT('Ctrl Pts',(105.796510488709,-13.2639611441589,
67.6215771922203));
#141935=CARTESIAN_POINT('Ctrl Pts',(105.81234015007,-13.2603311242177,67.6261905806811));
#141936=CARTESIAN_POINT('Ctrl Pts',(105.825404534772,-13.2573352308815,
67.6299980583176));
#141937=CARTESIAN_POINT('Ctrl Pts',(105.838534840569,-13.2543118163068,
67.633857648385));
#141938=CARTESIAN_POINT('Ctrl Pts',(105.851663194163,-13.2512384347092,
67.6378180818378));
#141939=CARTESIAN_POINT('Ctrl Pts',(105.853208076029,-13.2508767738607,
67.6382841267064));
#141940=CARTESIAN_POINT('Ctrl Pts',(105.854752981239,-13.2505144320582,
67.6387515407154));
#141941=CARTESIAN_POINT('Ctrl Pts',(105.856297837123,-13.2501513809293,
67.6392203828757));
#141942=CARTESIAN_POINT('Ctrl Pts',(105.871928249551,-13.2464781328706,
67.6439639944989));
#141943=CARTESIAN_POINT('Ctrl Pts',(105.887507214198,-13.2427762158654,
67.6487775733898));
#141944=CARTESIAN_POINT('Ctrl Pts',(105.902910700177,-13.2390652774627,
67.6536389990103));
#141945=CARTESIAN_POINT('Ctrl Pts',(105.906042369124,-13.2383108098976,
67.6546273711018));
#141946=CARTESIAN_POINT('Ctrl Pts',(105.909166936774,-13.2375560028952,
67.6556176432816));
#141947=CARTESIAN_POINT('Ctrl Pts',(105.912283569683,-13.2368010670366,
67.6566095252591));
#141948=CARTESIAN_POINT('Ctrl Pts',(105.914589339976,-13.2362425448344,
67.6573433466827));
#141949=CARTESIAN_POINT('Ctrl Pts',(105.916890635439,-13.2356839325614,
67.6580781031648));
#141950=CARTESIAN_POINT('Ctrl Pts',(105.919187076455,-13.2351252969899,
67.6588137177562));
#141951=CARTESIAN_POINT('Ctrl Pts',(105.921483517471,-13.2345666614184,
67.6595493323476));
#141952=CARTESIAN_POINT('Ctrl Pts',(105.926365493087,-13.233377729542,67.6611160596461));
#141953=CARTESIAN_POINT('Ctrl Pts',(105.930102670479,-13.2324674516722,
67.6623162717565));
#141954=CARTESIAN_POINT('Ctrl Pts',(105.937577025265,-13.2306468959328,
67.6647166959771));
#141955=CARTESIAN_POINT('Ctrl Pts',(105.944480659722,-13.2289649159458,
67.6669365825435));
#141956=CARTESIAN_POINT('Ctrl Pts',(105.950857804366,-13.2274131285108,
67.6689851561453));
#141957=CARTESIAN_POINT('Ctrl Pts',(105.958938076775,-13.2254469091608,
67.6715808370775));
#141958=CARTESIAN_POINT('Ctrl Pts',(105.966180881029,-13.2236889322356,
67.6739019442468));
#141959=CARTESIAN_POINT('Ctrl Pts',(105.972589215247,-13.222136306475,67.675952322906));
#141960=CARTESIAN_POINT('Ctrl Pts',(105.976296102932,-13.2212381933123,
67.6771383602045));
#141961=CARTESIAN_POINT('Ctrl Pts',(105.979724062723,-13.220408854815,67.6782336403411));
#141962=CARTESIAN_POINT('Ctrl Pts',(105.982875322055,-13.2196480918367,
67.6792378960421));
#141963=CARTESIAN_POINT('Ctrl Pts',(105.991474365275,-13.2175721491608,
67.6819782729092));
#141964=CARTESIAN_POINT('Ctrl Pts',(105.997989368553,-13.216008835081,67.6840398857284));
#141965=CARTESIAN_POINT('Ctrl Pts',(106.002298346939,-13.2149771010983,
67.6853994996504));
#141966=CARTESIAN_POINT('Ctrl Pts',(106.004452836132,-13.214461234107,67.6860793066115));
#141967=CARTESIAN_POINT('Ctrl Pts',(106.006055362552,-13.214078368262,67.6865835393359));
#141968=CARTESIAN_POINT('Ctrl Pts',(106.00704938813,-13.213845890555,67.6868871294661));
#141969=CARTESIAN_POINT('Ctrl Pts',(106.0079275809,-13.213640503243,67.6871553425417));
#141970=CARTESIAN_POINT('Ctrl Pts',(106.008771662554,-13.2134477302784,
67.6874045785535));
#141971=CARTESIAN_POINT('Ctrl Pts',(106.011353112438,-13.2128765343337,
67.6881335578442));
#141972=CARTESIAN_POINT('Ctrl Pts',(106.01169360327,-13.2128011941214,67.6882297095327));
#141973=CARTESIAN_POINT('Ctrl Pts',(106.012064263459,-13.2127192510605,
67.6883342516613));
#141974=CARTESIAN_POINT('Ctrl Pts',(106.01246908579,-13.2126297834597,67.6884483843945));
#141975=CARTESIAN_POINT('Ctrl Pts',(106.018706785095,-13.2112512231658,
67.6902069970421));
#141976=CARTESIAN_POINT('Ctrl Pts',(106.025629390392,-13.2098534637644,
67.6919178460703));
#141977=CARTESIAN_POINT('Ctrl Pts',(106.033070473643,-13.2084838648189,
67.693516276775));
#141978=CARTESIAN_POINT('Ctrl Pts',(106.039796379662,-13.2072459007375,
67.6949610791423));
#141979=CARTESIAN_POINT('Ctrl Pts',(106.046946255791,-13.2060309835752,
67.6963139902179));
#141980=CARTESIAN_POINT('Ctrl Pts',(106.054358327978,-13.2048662938512,
67.6975448752181));
#141981=CARTESIAN_POINT('Ctrl Pts',(106.057014045171,-13.2044489899657,
67.6979858966186));
#141982=CARTESIAN_POINT('Ctrl Pts',(106.059703006123,-13.2040380529815,
67.698411432947));
#141983=CARTESIAN_POINT('Ctrl Pts',(106.062416233874,-13.2036344373729,
67.6988207497283));
#141984=CARTESIAN_POINT('Ctrl Pts',(106.067640753954,-13.2028572457602,
67.6996089193695));
#141985=CARTESIAN_POINT('Ctrl Pts',(106.072917428486,-13.20210323266,67.7003487886868));
#141986=CARTESIAN_POINT('Ctrl Pts',(106.078291363442,-13.2013858193255,
67.7010093557201));
#141987=CARTESIAN_POINT('Ctrl Pts',(106.082994471742,-13.2007579604781,
67.7015874643728));
#141988=CARTESIAN_POINT('Ctrl Pts',(106.08777242606,-13.200158185367,67.7021047405022));
#141989=CARTESIAN_POINT('Ctrl Pts',(106.092620378955,-13.1995878076451,
67.7025577171331));
#141990=CARTESIAN_POINT('Ctrl Pts',(106.094961596148,-13.1993123556846,
67.7027764726986));
#141991=CARTESIAN_POINT('Ctrl Pts',(106.097318554236,-13.1990436338865,
67.7029805142864));
#141992=CARTESIAN_POINT('Ctrl Pts',(106.099686672438,-13.1987809372948,
67.7031713487706));
#141993=CARTESIAN_POINT('Ctrl Pts',(106.106306020717,-13.1980466495254,
67.7037047680541));
#141994=CARTESIAN_POINT('Ctrl Pts',(106.113015286185,-13.1973595556006,
67.7041346722277));
#141995=CARTESIAN_POINT('Ctrl Pts',(106.119760232682,-13.1967182146413,
67.7044643428826));
#141996=CARTESIAN_POINT('Ctrl Pts',(106.120291884984,-13.1966676626618,
67.7044903282871));
#141997=CARTESIAN_POINT('Ctrl Pts',(106.120823733892,-13.196617393249,67.7045156950284));
#141998=CARTESIAN_POINT('Ctrl Pts',(106.121355741848,-13.1965674055061,
67.7045404452821));
#141999=CARTESIAN_POINT('Ctrl Pts',(106.126806388336,-13.1960552599398,
67.704794022098));
#142000=CARTESIAN_POINT('Ctrl Pts',(106.132300873379,-13.1955789258494,
67.7049683496596));
#142001=CARTESIAN_POINT('Ctrl Pts',(106.137816755595,-13.1951304042744,
67.7050744113511));
#142002=CARTESIAN_POINT('Ctrl Pts',(106.142627707291,-13.1947392038194,
67.7051669183437));
#142003=CARTESIAN_POINT('Ctrl Pts',(106.147452442908,-13.1943684627235,
67.7052090760339));
#142004=CARTESIAN_POINT('Ctrl Pts',(106.15229430885,-13.1940239170325,67.705183407132));
#142005=CARTESIAN_POINT('Ctrl Pts',(106.154293195483,-13.1938816768746,
67.7051728101379));
#142006=CARTESIAN_POINT('Ctrl Pts',(106.156057216663,-13.1937568448576,
67.7051595416078));
#142007=CARTESIAN_POINT('Ctrl Pts',(106.157935224526,-13.1936307172706,
67.7051301165763));
#142008=CARTESIAN_POINT('Ctrl Pts',(106.159344479978,-13.1935360712399,
67.7051080360584));
#142009=CARTESIAN_POINT('Ctrl Pts',(106.160816586509,-13.1934404193615,
67.7050774867419));
#142010=CARTESIAN_POINT('Ctrl Pts',(106.162480765056,-13.1933340722082,
67.7050369249592));
#142011=CARTESIAN_POINT('Ctrl Pts',(106.164364380857,-13.1932137022041,
67.7049910147323));
#142012=CARTESIAN_POINT('Ctrl Pts',(106.166494087513,-13.1930794657017,
67.7049328065703));
#142013=CARTESIAN_POINT('Ctrl Pts',(106.169036390997,-13.192916817047,67.7048600150695));
#142014=CARTESIAN_POINT('Ctrl Pts',(106.173988369297,-13.1926000049064,
67.7047182295057));
#142015=CARTESIAN_POINT('Ctrl Pts',(106.1787882912,-13.1922750737932,67.7045866164252));
#142016=CARTESIAN_POINT('Ctrl Pts',(106.183439168815,-13.1919492595683,
67.7044538112829));
#142017=CARTESIAN_POINT('Ctrl Pts',(106.18609681466,-13.1917630799065,67.7043779225876));
#142018=CARTESIAN_POINT('Ctrl Pts',(106.188706333932,-13.191576536862,67.7043018744545));
#142019=CARTESIAN_POINT('Ctrl Pts',(106.191262452227,-13.1913884722509,
67.7042303695505));
#142020=CARTESIAN_POINT('Ctrl Pts',(106.19531464786,-13.191090334799,67.7041170133492));
#142021=CARTESIAN_POINT('Ctrl Pts',(106.199200076115,-13.1907929689485,
67.7040122321995));
#142022=CARTESIAN_POINT('Ctrl Pts',(106.202979797795,-13.1905041748381,
67.7038985058269));
#142023=CARTESIAN_POINT('Ctrl Pts',(106.204080645818,-13.1904200632415,
67.703865382898));
#142024=CARTESIAN_POINT('Ctrl Pts',(106.205172202955,-13.1903366268841,
67.703831634868));
#142025=CARTESIAN_POINT('Ctrl Pts',(106.206255281634,-13.1902539498646,
67.7037971082059));
#142026=CARTESIAN_POINT('Ctrl Pts',(106.210961647814,-13.189894688496,67.7036470774486));
#142027=CARTESIAN_POINT('Ctrl Pts',(106.21550436911,-13.1895485333888,67.7034855994441));
#142028=CARTESIAN_POINT('Ctrl Pts',(106.219845269805,-13.1892023369266,
67.7033519059895));
#142029=CARTESIAN_POINT('Ctrl Pts',(106.224742564287,-13.1888117668255,
67.7032010764121));
#142030=CARTESIAN_POINT('Ctrl Pts',(106.229383204607,-13.1884212700987,
67.7030852992312));
#142031=CARTESIAN_POINT('Ctrl Pts',(106.233759144139,-13.1880288718173,
67.7030159462491));
#142032=CARTESIAN_POINT('Ctrl Pts',(106.2387553242,-13.1875808554644,67.7029367632569));
#142033=CARTESIAN_POINT('Ctrl Pts',(106.243406787408,-13.1871305335341,
67.7029176584391));
#142034=CARTESIAN_POINT('Ctrl Pts',(106.247754302878,-13.1866931537782,
67.7029267676943));
#142035=CARTESIAN_POINT('Ctrl Pts',(106.251285121241,-13.186337937452,67.7029341657417));
#142036=CARTESIAN_POINT('Ctrl Pts',(106.254616705439,-13.1859916872872,
67.7029590202608));
#142037=CARTESIAN_POINT('Ctrl Pts',(106.257788816691,-13.1856684565596,
67.7029683476007));
#142038=CARTESIAN_POINT('Ctrl Pts',(106.263348662761,-13.1851019212311,
67.7029846958843));
#142039=CARTESIAN_POINT('Ctrl Pts',(106.268332466383,-13.1845596796241,
67.7030583307742));
#142040=CARTESIAN_POINT('Ctrl Pts',(106.272752463344,-13.1840366895586,
67.7032011751615));
#142041=CARTESIAN_POINT('Ctrl Pts',(106.274940771102,-13.1837777610508,
67.7032718963597));
#142042=CARTESIAN_POINT('Ctrl Pts',(106.276991551938,-13.1835237709647,
67.7033589856214));
#142043=CARTESIAN_POINT('Ctrl Pts',(106.278909589549,-13.1832751579372,
67.7034610233969));
#142044=CARTESIAN_POINT('Ctrl Pts',(106.281805657742,-13.1828997741193,
67.7036150914685));
#142045=CARTESIAN_POINT('Ctrl Pts',(106.28439497079,-13.1825356113142,67.7038060310672));
#142046=CARTESIAN_POINT('Ctrl Pts',(106.28668290027,-13.182182080024,67.7040347302797));
#142047=CARTESIAN_POINT('Ctrl Pts',(106.28838368379,-13.1819192746371,67.7042047389513));
#142048=CARTESIAN_POINT('Ctrl Pts',(106.289172451088,-13.1818103688079,
67.7042586550601));
#142049=CARTESIAN_POINT('Ctrl Pts',(106.290712328531,-13.1815248738751,
67.7045027578366));
#142050=CARTESIAN_POINT('Ctrl Pts',(106.291243926355,-13.181426315067,67.7045870272085));
#142051=CARTESIAN_POINT('Ctrl Pts',(106.291865315224,-13.1813067816776,
67.7046937549635));
#142052=CARTESIAN_POINT('Ctrl Pts',(106.29264608939,-13.1811529706491,67.7048346699659));
#142053=CARTESIAN_POINT('Ctrl Pts',(106.308230747469,-13.1780828225921,
67.7076474066395));
#142054=CARTESIAN_POINT('Ctrl Pts',(106.325794339231,-13.174397015322,67.7112173579816));
#142055=CARTESIAN_POINT('Ctrl Pts',(106.34552537209,-13.1700711157576,67.7155433191232));
#142056=CARTESIAN_POINT('Ctrl Pts',(106.356609505867,-13.1676409921134,
67.7179734773591));
#142057=CARTESIAN_POINT('Ctrl Pts',(106.368378129295,-13.1650086066466,
67.7206425875831));
#142058=CARTESIAN_POINT('Ctrl Pts',(106.380848846052,-13.1621681033657,
67.7235563945947));
#142059=CARTESIAN_POINT('Ctrl Pts',(106.390746763908,-13.1599136164191,
67.7258690621831));
#142060=CARTESIAN_POINT('Ctrl Pts',(106.401669238631,-13.1573934798774,
67.728475184187));
#142061=CARTESIAN_POINT('Ctrl Pts',(106.412902229041,-13.1547957200748,
67.7311586306529));
#142062=CARTESIAN_POINT('Ctrl Pts',(106.421342471128,-13.1528438158342,
67.7331749181213));
#142063=CARTESIAN_POINT('Ctrl Pts',(106.429956610801,-13.1508478008114,
67.7352358032063));
#142064=CARTESIAN_POINT('Ctrl Pts',(106.43842557944,-13.1488848065073,67.7372594300533));
#142065=CARTESIAN_POINT('Ctrl Pts',(106.458165770223,-13.1443092928029,
67.7419762712338));
#142066=CARTESIAN_POINT('Ctrl Pts',(106.47783830857,-13.1397336851529,67.7466869839844));
#142067=CARTESIAN_POINT('Ctrl Pts',(106.497415498927,-13.1351634667802,
67.7513934960968));
#142068=CARTESIAN_POINT('Ctrl Pts',(106.517010927316,-13.1305889908104,
67.7561043927769));
#142069=CARTESIAN_POINT('Ctrl Pts',(106.536598800992,-13.1260326377809,
67.7607696183555));
#142070=CARTESIAN_POINT('Ctrl Pts',(106.556115761675,-13.1214660922766,
67.7654617021941));
#142071=CARTESIAN_POINT('Ctrl Pts',(106.614593983727,-13.1077834566277,
67.7795204854777));
#142072=CARTESIAN_POINT('Ctrl Pts',(106.672439179494,-13.0940112378979,
67.7938147099477));
#142073=CARTESIAN_POINT('Ctrl Pts',(106.730750213752,-13.0801193452713,
67.8080999015867));
#142074=CARTESIAN_POINT('Ctrl Pts',(106.769636311969,-13.0708552067089,
67.8176263209374));
#142075=CARTESIAN_POINT('Ctrl Pts',(106.808539671188,-13.0615329788697,
67.8271947355138));
#142076=CARTESIAN_POINT('Ctrl Pts',(106.847463012598,-13.0521360046979,
67.8368067246768));
#142077=CARTESIAN_POINT('Ctrl Pts',(106.866924683304,-13.0474375176119,
67.8416127192583));
#142078=CARTESIAN_POINT('Ctrl Pts',(106.886392130002,-13.0427202088031,
67.8464296643369));
#142079=CARTESIAN_POINT('Ctrl Pts',(106.905867009676,-13.0379817218561,
67.8512578091657));
#142080=CARTESIAN_POINT('Ctrl Pts',(106.910735729595,-13.0367971001194,
67.8524648453729));
#142081=CARTESIAN_POINT('Ctrl Pts',(106.915604914056,-13.0356111545458,
67.8536725814496));
#142082=CARTESIAN_POINT('Ctrl Pts',(106.920474588092,-13.0344238482103,
67.8548810207559));
#142083=CARTESIAN_POINT('Ctrl Pts',(106.925344262128,-13.0332365418749,
67.8560894600622));
#142084=CARTESIAN_POINT('Ctrl Pts',(106.930697157267,-13.031927921499,67.8574217098111));
#142085=CARTESIAN_POINT('Ctrl Pts',(106.931726432134,-13.0316795015703,
67.8576719813984));
#142086=CARTESIAN_POINT('Ctrl Pts',(106.933784981867,-13.0311826617128,
67.8581725245729));
#142087=CARTESIAN_POINT('Ctrl Pts',(106.936923967831,-13.0304423944958,
67.8589040957394));
#142088=CARTESIAN_POINT('Ctrl Pts',(106.94114463868,-13.0294576651308,67.8598669197149));
#142089=CARTESIAN_POINT('Ctrl Pts',(106.950441317851,-13.0272886466725,
67.8619876881709));
#142090=CARTESIAN_POINT('Ctrl Pts',(106.9649906445,-13.0239350581153,67.8652288807271));
#142091=CARTESIAN_POINT('Ctrl Pts',(106.984801432774,-13.0193731607089,
67.8695970565263));
#142092=CARTESIAN_POINT('Ctrl Pts',(107.000966852782,-13.0156506946166,
67.8731614475788));
#142093=CARTESIAN_POINT('Ctrl Pts',(107.020635638888,-13.0111238244378,
67.8774751049033));
#142094=CARTESIAN_POINT('Ctrl Pts',(107.043812218085,-13.0057758568377,
67.8825361178667));
#142095=CARTESIAN_POINT('Ctrl Pts',(107.069602003937,-12.9998248949646,
67.8881677703815));
#142096=CARTESIAN_POINT('Ctrl Pts',(107.099727177575,-12.9928579994466,
67.8947252155551));
#142097=CARTESIAN_POINT('Ctrl Pts',(107.134152385793,-12.98485017791,67.9022020853204));
#142098=CARTESIAN_POINT('Ctrl Pts',(107.151364989902,-12.9808462671417,
67.9059405202031));
#142099=CARTESIAN_POINT('Ctrl Pts',(107.169653865867,-12.9765817338447,
67.9099090152389));
#142100=CARTESIAN_POINT('Ctrl Pts',(107.1890184561,-12.9720518542785,67.9141073841192));
#142101=CARTESIAN_POINT('Ctrl Pts',(107.198700751216,-12.9697869144955,
67.9162065685594));
#142102=CARTESIAN_POINT('Ctrl Pts',(107.208651974163,-12.9674556316093,
67.9183632178064));
#142103=CARTESIAN_POINT('Ctrl Pts',(107.218872157659,-12.9650573413603,
67.9205773271656));
#142104=CARTESIAN_POINT('Ctrl Pts',(107.223982249406,-12.9638581962358,
67.9216843818451));
#142105=CARTESIAN_POINT('Ctrl Pts',(107.229159581246,-12.9626422988637,
67.9228058013249));
#142106=CARTESIAN_POINT('Ctrl Pts',(107.234404161833,-12.9614095624508,
67.9239415850425));
#142107=CARTESIAN_POINT('Ctrl Pts',(107.237026452127,-12.9607931942444,
67.9245094769013));
#142108=CARTESIAN_POINT('Ctrl Pts',(107.239665554605,-12.9601726162525,
67.9250809598053));
#142109=CARTESIAN_POINT('Ctrl Pts',(107.242321470771,-12.9595478173416,
67.9256560337469));
#142110=CARTESIAN_POINT('Ctrl Pts',(107.243649428854,-12.9592354178861,
67.9259435707177));
#142111=CARTESIAN_POINT('Ctrl Pts',(107.24498159036,-12.9589219631993,67.9262320054471));
#142112=CARTESIAN_POINT('Ctrl Pts',(107.246317955505,-12.9586074518708,
67.9265213379387));
#142113=CARTESIAN_POINT('Ctrl Pts',(107.247654320651,-12.9582929405424,
67.9268106704303));
#142114=CARTESIAN_POINT('Ctrl Pts',(107.250177381402,-12.9576989554457,
67.9273568967762));
#142115=CARTESIAN_POINT('Ctrl Pts',(107.25033966209,-12.9576607465408,67.9273920287038));
#142116=CARTESIAN_POINT('Ctrl Pts',(107.263428087531,-12.9545790834838,
67.9302255242923));
#142117=CARTESIAN_POINT('Ctrl Pts',(107.286145037413,-12.9491868368947,
67.9352153777412));
#142118=CARTESIAN_POINT('Ctrl Pts',(107.318469490553,-12.9414271973423,
67.942368949705));
#142119=CARTESIAN_POINT('Ctrl Pts',(107.337445418838,-12.9368719350143,
67.9465684227163));
#142120=CARTESIAN_POINT('Ctrl Pts',(107.359732422305,-12.931500312654,67.9515128573504));
#142121=CARTESIAN_POINT('Ctrl Pts',(107.385329787984,-12.9252967084814,
67.957197178429));
#142122=CARTESIAN_POINT('Ctrl Pts',(107.393979922269,-12.9232003205242,
67.9591180847155));
#142123=CARTESIAN_POINT('Ctrl Pts',(107.403007784403,-12.9210087677287,
67.9611237406437));
#142124=CARTESIAN_POINT('Ctrl Pts',(107.412413111063,-12.9187212637526,
67.9632140784353));
#142125=CARTESIAN_POINT('Ctrl Pts',(107.413588776895,-12.9184353257555,
67.9634753706593));
#142126=CARTESIAN_POINT('Ctrl Pts',(107.414770340603,-12.9181478884549,
67.9637379859997));
#142127=CARTESIAN_POINT('Ctrl Pts',(107.415957801536,-12.9178589502324,
67.9640019243639));
#142128=CARTESIAN_POINT('Ctrl Pts',(107.417145262469,-12.9175700120099,
67.9642658627281));
#142129=CARTESIAN_POINT('Ctrl Pts',(107.421399590165,-12.9165345440671,
67.9652114953958));
#142130=CARTESIAN_POINT('Ctrl Pts',(107.424537922514,-12.9157701484059,
67.9659090759425));
#142131=CARTESIAN_POINT('Ctrl Pts',(107.430814587213,-12.9142413570834,
67.9673042370359));
#142132=CARTESIAN_POINT('Ctrl Pts',(107.43708970593,-12.9127112789761,67.9686990791321));
#142133=CARTESIAN_POINT('Ctrl Pts',(107.443363264349,-12.9111799206928,
67.970093600068));
#142134=CARTESIAN_POINT('Ctrl Pts',(107.455910381186,-12.9081172041261,
67.9728826419399));
#142135=CARTESIAN_POINT('Ctrl Pts',(107.468451256819,-12.9050493668033,
67.9756703991361));
#142136=CARTESIAN_POINT('Ctrl Pts',(107.480985748233,-12.901976467266,67.9784568517438));
#142137=CARTESIAN_POINT('Ctrl Pts',(107.531123713887,-12.8896848691169,
67.9896026621746));
#142138=CARTESIAN_POINT('Ctrl Pts',(107.581159531596,-12.877312267325,68.0007275954188));
#142139=CARTESIAN_POINT('Ctrl Pts',(107.631093001679,-12.8648609057211,
68.0118313415621));
#142140=CARTESIAN_POINT('Ctrl Pts',(107.695290512925,-12.8488526766662,
68.02610699408));
#142141=CARTESIAN_POINT('Ctrl Pts',(107.75930625601,-12.832715850264,68.0403476199207));
#142142=CARTESIAN_POINT('Ctrl Pts',(107.823178038429,-12.816449128691,68.0545552102772));
#142143=CARTESIAN_POINT('Ctrl Pts',(107.858666485858,-12.8074110108942,
68.0624492333398));
#142144=CARTESIAN_POINT('Ctrl Pts',(107.894110420149,-12.7983327871238,
68.0703330675227));
#142145=CARTESIAN_POINT('Ctrl Pts',(107.929507029907,-12.7892133079803,
68.0782085743562));
#142146=CARTESIAN_POINT('Ctrl Pts',(107.983521817539,-12.7752970958739,
68.0902265001408));
#142147=CARTESIAN_POINT('Ctrl Pts',(108.037442841,-12.7612838820349,68.1022230318144));
#142148=CARTESIAN_POINT('Ctrl Pts',(108.091265807375,-12.7471725434948,
68.1141982544549));
#142149=CARTESIAN_POINT('Ctrl Pts',(108.294350377707,-12.6939277055151,
68.1593831097012));
#142150=CARTESIAN_POINT('Ctrl Pts',(108.496034079401,-12.6392855691849,
68.2042656174757));
#142151=CARTESIAN_POINT('Ctrl Pts',(108.696127954478,-12.5831843055722,
68.248843918316));
#142152=CARTESIAN_POINT('Ctrl Pts',(108.832191396481,-12.5450355565164,
68.2791570753214));
#142153=CARTESIAN_POINT('Ctrl Pts',(108.967522039852,-12.5062122247552,
68.3093291886953));
#142154=CARTESIAN_POINT('Ctrl Pts',(109.102170552872,-12.4667056364051,
68.3393417122603));
#142155=CARTESIAN_POINT('Ctrl Pts',(109.453424423852,-12.363645886424,68.4176345566715));
#142156=CARTESIAN_POINT('Ctrl Pts',(109.799724391402,-12.2559464931104,
68.4948956137196));
#142157=CARTESIAN_POINT('Ctrl Pts',(110.140821024858,-12.1434889766497,
68.5710707710017));
#142158=CARTESIAN_POINT('Ctrl Pts',(110.173727741523,-12.1326398293169,
68.5784196395386));
#142159=CARTESIAN_POINT('Ctrl Pts',(110.206586003916,-12.1217464208938,
68.5857584201245));
#142160=CARTESIAN_POINT('Ctrl Pts',(110.239395571674,-12.1108086599221,
68.5930870754831));
#142161=CARTESIAN_POINT('Ctrl Pts',(110.345808727803,-12.0753335913508,
68.6168565244638));
#142162=CARTESIAN_POINT('Ctrl Pts',(110.451708902476,-12.0393922845856,
68.6405191617746));
#142163=CARTESIAN_POINT('Ctrl Pts',(110.557091482789,-12.0029811494992,
68.6640737449812));
#142164=CARTESIAN_POINT('Ctrl Pts',(110.636352799546,-11.9755952712735,
68.681789835013));
#142165=CARTESIAN_POINT('Ctrl Pts',(110.715321294688,-11.9479436164212,
68.6994447990933));
#142166=CARTESIAN_POINT('Ctrl Pts',(110.793993320436,-11.9200246667457,
68.7170379770568));
#142167=CARTESIAN_POINT('Ctrl Pts',(110.885628874946,-11.887505249449,68.7375301482316));
#142168=CARTESIAN_POINT('Ctrl Pts',(110.976862459063,-11.8546231658946,
68.7579384497065));
#142169=CARTESIAN_POINT('Ctrl Pts',(111.067688403721,-11.821376277975,68.7782617217179));
#142170=CARTESIAN_POINT('Ctrl Pts',(111.11310137605,-11.8047528340152,68.7884233577236));
#142171=CARTESIAN_POINT('Ctrl Pts',(111.158412439001,-11.7880381911324,
68.7985637379712));
#142172=CARTESIAN_POINT('Ctrl Pts',(111.203620891663,-11.7712321070967,
68.8086827088724));
#142173=CARTESIAN_POINT('Ctrl Pts',(111.226225117994,-11.7628290650789,
68.813742194323));
#142174=CARTESIAN_POINT('Ctrl Pts',(111.248803691776,-11.754403162908,68.8187963275252));
#142175=CARTESIAN_POINT('Ctrl Pts',(111.271356510201,-11.7459543749221,
68.8238450891866));
#142176=CARTESIAN_POINT('Ctrl Pts',(111.282632919414,-11.7417299809291,
68.8263694700173));
#142177=CARTESIAN_POINT('Ctrl Pts',(111.293902889791,-11.737499865492,68.8288925079705));
#142178=CARTESIAN_POINT('Ctrl Pts',(111.305166409589,-11.7332640252594,
68.8314142006312));
#142179=CARTESIAN_POINT('Ctrl Pts',(111.315021989413,-11.7295576650559,
68.8336206817094));
#142180=CARTESIAN_POINT('Ctrl Pts',(111.324872630526,-11.7258469218158,
68.8358261327756));
#142181=CARTESIAN_POINT('Ctrl Pts',(111.334718215831,-11.7221317721431,
68.8380306137598));
#142182=CARTESIAN_POINT('Ctrl Pts',(111.336124728018,-11.7216010364755,
68.8383455396147));
#142183=CARTESIAN_POINT('Ctrl Pts',(111.337531120636,-11.7210703090457,
68.8386605681555));
#142184=CARTESIAN_POINT('Ctrl Pts',(111.340784955608,-11.7198418175818,
68.8393889026379));
#142185=CARTESIAN_POINT('Ctrl Pts',(111.676598330681,-11.5930548513553,
68.9145569621135));
#142186=CARTESIAN_POINT('Ctrl Pts',(112.010698132989,-11.4596490571931,
68.9894187938631));
#142187=CARTESIAN_POINT('Ctrl Pts',(112.342633408572,-11.3190643094168,
69.0638575505441));
#142188=CARTESIAN_POINT('Ctrl Pts',(112.566856914298,-11.2240987925921,
69.114141205861));
#142189=CARTESIAN_POINT('Ctrl Pts',(112.790091959944,-11.1258569855089,
69.1642315263753));
#142190=CARTESIAN_POINT('Ctrl Pts',(113.012189026206,-11.0241600292873,
69.2140865598598));
#142191=CARTESIAN_POINT('Ctrl Pts',(113.289691953154,-10.8970930513742,
69.2763787726652));
#142192=CARTESIAN_POINT('Ctrl Pts',(113.565421268222,-10.7646317480393,
69.3383038963364));
#142193=CARTESIAN_POINT('Ctrl Pts',(113.838972335797,-10.6264708943272,
69.3997865989108));
#142194=CARTESIAN_POINT('Ctrl Pts',(114.104544539504,-10.4923398791873,
69.4594759905747));
#142195=CARTESIAN_POINT('Ctrl Pts',(114.368063772043,-10.3528368900573,
69.5187486148448));
#142196=CARTESIAN_POINT('Ctrl Pts',(114.629112607753,-10.2076787365451,
69.5775221736678));
#142197=CARTESIAN_POINT('Ctrl Pts',(114.721749901965,-10.1561670776727,
69.5983788974519));
#142198=CARTESIAN_POINT('Ctrl Pts',(114.81407565261,-10.1039432332318,69.6191726327996));
#142199=CARTESIAN_POINT('Ctrl Pts',(114.906069691261,-10.0509944466622,
69.6398991964471));
#142200=CARTESIAN_POINT('Ctrl Pts',(115.158260743509,-9.90584145201093,
69.6967186814093));
#142201=CARTESIAN_POINT('Ctrl Pts',(115.407962187416,-9.75524064263987,
69.7530347717736));
#142202=CARTESIAN_POINT('Ctrl Pts',(115.654720644459,-9.59893015320212,
69.8087507530049));
#142203=CARTESIAN_POINT('Ctrl Pts',(115.820069278053,-9.49418916010859,
69.8460850817907));
#142204=CARTESIAN_POINT('Ctrl Pts',(115.984095575379,-9.38688437968712,
69.8831495949633));
#142205=CARTESIAN_POINT('Ctrl Pts',(116.146651119149,-9.27693621160278,
69.9199097730351));
#142206=CARTESIAN_POINT('Ctrl Pts',(116.370838736652,-9.1253017777346,69.9706073779878));
#142207=CARTESIAN_POINT('Ctrl Pts',(116.59227521728,-8.96861412888962,70.0207329109146));
#142208=CARTESIAN_POINT('Ctrl Pts',(116.810505003658,-8.80664115597571,
70.0702052203824));
#142209=CARTESIAN_POINT('Ctrl Pts',(117.023958781536,-8.64821299840652,
70.1185948171075));
#142210=CARTESIAN_POINT('Ctrl Pts',(117.234345143066,-8.48472837853567,
70.1663595531027));
#142211=CARTESIAN_POINT('Ctrl Pts',(117.441174068438,-8.31595777817756,
70.2134049767224));
#142212=CARTESIAN_POINT('Ctrl Pts',(117.642407602492,-8.15175296836516,
70.2591776694877));
#142213=CARTESIAN_POINT('Ctrl Pts',(117.840273614692,-7.98254426435186,
70.3042696055394));
#142214=CARTESIAN_POINT('Ctrl Pts',(118.0342763988,-7.80811648244908,70.3485728169649));
#142215=CARTESIAN_POINT('Ctrl Pts',(118.123449679351,-7.72794084165549,
70.3689367654512));
#142216=CARTESIAN_POINT('Ctrl Pts',(118.211806116165,-7.64666247736764,
70.3891337632917));
#142217=CARTESIAN_POINT('Ctrl Pts',(118.299294254877,-7.56426025759235,
70.4091516254367));
#142218=CARTESIAN_POINT('Ctrl Pts',(118.489293739946,-7.38530594954026,
70.4526247585464));
#142219=CARTESIAN_POINT('Ctrl Pts',(118.67518421981,-7.20105610757558,70.4952581234905));
#142220=CARTESIAN_POINT('Ctrl Pts',(118.856312446238,-7.01133104918698,
70.5369285437103));
#142221=CARTESIAN_POINT('Ctrl Pts',(118.99619198796,-6.86481244883354,70.569109277761));
#142222=CARTESIAN_POINT('Ctrl Pts',(119.133230427345,-6.71502846719137,
70.6007154059949));
#142223=CARTESIAN_POINT('Ctrl Pts',(119.267107529061,-6.56189725353795,
70.6316812677236));
#142224=CARTESIAN_POINT('Ctrl Pts',(119.383489889386,-6.42877686285118,
70.6586005842556));
#142225=CARTESIAN_POINT('Ctrl Pts',(119.497465439713,-6.29314640495762,
70.6850316807826));
#142226=CARTESIAN_POINT('Ctrl Pts',(119.6087870881,-6.15498623441501,70.7109234456726));
#142227=CARTESIAN_POINT('Ctrl Pts',(119.6444020833,-6.11078482451875,70.7192069655057));
#142228=CARTESIAN_POINT('Ctrl Pts',(119.67974539263,-6.06632450162849,70.7274352643774));
#142229=CARTESIAN_POINT('Ctrl Pts',(119.714807140622,-6.02160798752607,
70.7356067925721));
#142230=CARTESIAN_POINT('Ctrl Pts',(119.787134197516,-5.92936461562263,
70.7524634132056));
#142231=CARTESIAN_POINT('Ctrl Pts',(119.858268463629,-5.83602393539941,
70.7690801116031));
#142232=CARTESIAN_POINT('Ctrl Pts',(119.928141526215,-5.74158973693852,
70.7854436423368));
#142233=CARTESIAN_POINT('Ctrl Pts',(119.963078057509,-5.69437263770807,
70.7936254077037));
#142234=CARTESIAN_POINT('Ctrl Pts',(119.99769927408,-5.64688214208205,70.8017438526601));
#142235=CARTESIAN_POINT('Ctrl Pts',(120.03199650483,-5.59911866729075,70.8097971234142));
#142236=CARTESIAN_POINT('Ctrl Pts',(120.049145120205,-5.5752369298951,70.8138237587912));
#142237=CARTESIAN_POINT('Ctrl Pts',(120.066212738068,-5.55128694670323,
70.8178340985175));
#142238=CARTESIAN_POINT('Ctrl Pts',(120.083198268887,-5.52726876482581,
70.8218278966712));
#142239=CARTESIAN_POINT('Ctrl Pts',(120.098060608353,-5.50625285568306,
70.8253224700557));
#142240=CARTESIAN_POINT('Ctrl Pts',(120.112860099865,-5.48518473185981,
70.8288043786772));
#142241=CARTESIAN_POINT('Ctrl Pts',(120.127596010453,-5.46406442325504,
70.8322734515337));
#142242=CARTESIAN_POINT('Ctrl Pts',(120.129701140537,-5.4610472363115,70.8327690333704));
#142243=CARTESIAN_POINT('Ctrl Pts',(120.132551182633,-5.4569573991032,70.8334400539826));
#142244=CARTESIAN_POINT('Ctrl Pts',(120.133907505838,-5.45500966753072,
70.8337594106343));
#142245=CARTESIAN_POINT('Ctrl Pts',(120.250042395984,-5.28823555987381,
70.8611042570002));
#142246=CARTESIAN_POINT('Ctrl Pts',(120.360277472768,-5.12122346206651,
70.8870716294798));
#142247=CARTESIAN_POINT('Ctrl Pts',(120.464639371518,-4.95442575006959,
70.9116486720203));
#142248=CARTESIAN_POINT('Ctrl Pts',(120.520202986649,-4.86562050615205,
70.9247338050923));
#142249=CARTESIAN_POINT('Ctrl Pts',(120.574102616812,-4.77687589085944,
70.9374249284167));
#142250=CARTESIAN_POINT('Ctrl Pts',(120.626348178696,-4.68825898388539,
70.9497208309657));
#142251=CARTESIAN_POINT('Ctrl Pts',(120.723100044827,-4.5241522002407,70.9724912151761));
#142252=CARTESIAN_POINT('Ctrl Pts',(120.814176502228,-4.36048177456388,
70.9939065657032));
#142253=CARTESIAN_POINT('Ctrl Pts',(120.899680756234,-4.19745355593584,
71.0140330377286));
#142254=CARTESIAN_POINT('Ctrl Pts',(120.94056301105,-4.11950467194616,71.0236561327133));
#142255=CARTESIAN_POINT('Ctrl Pts',(120.980172134073,-4.04170283677841,
71.0329845449487));
#142256=CARTESIAN_POINT('Ctrl Pts',(121.018523425566,-3.96407181115534,
71.0420253267797));
#142257=CARTESIAN_POINT('Ctrl Pts',(121.099100190346,-3.80096760664018,
71.0610201747404));
#142258=CARTESIAN_POINT('Ctrl Pts',(121.1740756497,-3.63888509553889,71.0786695045519));
#142259=CARTESIAN_POINT('Ctrl Pts',(121.243628132454,-3.47805224050065,
71.0950745582767));
#142260=CARTESIAN_POINT('Ctrl Pts',(121.290992880891,-3.36852620465547,
71.1062462837421));
#142261=CARTESIAN_POINT('Ctrl Pts',(121.335843774898,-3.25958000608234,
71.1168408835626));
#142262=CARTESIAN_POINT('Ctrl Pts',(121.378250394056,-3.15128934077509,
71.1268891787873));
#142263=CARTESIAN_POINT('Ctrl Pts',(121.43227088005,-3.01334119766261,71.1396893925801));
#142264=CARTESIAN_POINT('Ctrl Pts',(121.482324676729,-2.87646114422512,
71.1516021824958));
#142265=CARTESIAN_POINT('Ctrl Pts',(121.528620957139,-2.7410992539322,71.162625975379));
#142266=CARTESIAN_POINT('Ctrl Pts',(121.553709517772,-2.6677448729351,71.1685999131058));
#142267=CARTESIAN_POINT('Ctrl Pts',(121.577694962148,-2.59483551362207,
71.1743129425307));
#142268=CARTESIAN_POINT('Ctrl Pts',(121.600612981877,-2.52243699463433,
71.1797659749776));
#142269=CARTESIAN_POINT('Ctrl Pts',(121.64447704994,-2.3838694568596,71.1902028359817));
#142270=CARTESIAN_POINT('Ctrl Pts',(121.684455689974,-2.24700129479839,
71.1997183239856));
#142271=CARTESIAN_POINT('Ctrl Pts',(121.72077379674,-2.11198800006035,71.2083759721307));
#142272=CARTESIAN_POINT('Ctrl Pts',(121.758884318929,-1.97031136482238,
71.2174609030676));
#142273=CARTESIAN_POINT('Ctrl Pts',(121.792964243599,-1.83067690477613,
71.2256013439609));
#142274=CARTESIAN_POINT('Ctrl Pts',(121.823259728927,-1.69320953569154,
71.2328601754872));
#142275=CARTESIAN_POINT('Ctrl Pts',(121.833105683649,-1.64853299471043,
71.2352192770422));
#142276=CARTESIAN_POINT('Ctrl Pts',(121.842551798816,-1.60408495489313,
71.2374851732322));
#142277=CARTESIAN_POINT('Ctrl Pts',(121.851606188792,-1.55986862758669,
71.2396597694634));
#142278=CARTESIAN_POINT('Ctrl Pts',(121.877212802925,-1.4348209507498,71.2458097195688));
#142279=CARTESIAN_POINT('Ctrl Pts',(121.899687221721,-1.31162984135314,
71.251229551335));
#142280=CARTESIAN_POINT('Ctrl Pts',(121.919209628913,-1.19044907925386,
71.2559200140058));
#142281=CARTESIAN_POINT('Ctrl Pts',(121.941356854127,-1.05297537514837,
71.2612411166804));
#142282=CARTESIAN_POINT('Ctrl Pts',(121.959684929351,-0.917991321981767,
71.2656471422445));
#142283=CARTESIAN_POINT('Ctrl Pts',(121.974343097486,-0.785644001935815,
71.2691750218849));
#142284=CARTESIAN_POINT('Ctrl Pts',(121.990228746996,-0.642213859750984,
71.2729983277007));
#142285=CARTESIAN_POINT('Ctrl Pts',(122.001804504546,-0.501879910786403,
71.2757906643818));
#142286=CARTESIAN_POINT('Ctrl Pts',(122.00923088834,-0.364773384560142,
71.2775855021344));
#142287=CARTESIAN_POINT('Ctrl Pts',(122.015963003551,-0.24048450366651,
71.2792125463153));
#142288=CARTESIAN_POINT('Ctrl Pts',(122.019284931663,-0.118846386916853,
71.2800198326534));
#142289=CARTESIAN_POINT('Ctrl Pts',(122.019294419317,7.00634560479863E-5,
71.2800197814689));
#142290=CARTESIAN_POINT('Ctrl Pts',(105.189140139769,-13.40679170556,67.435700227319));
#142291=CARTESIAN_POINT('Ctrl Pts',(105.299653563669,-13.41337593904,67.406356677722));
#142292=CARTESIAN_POINT('Ctrl Pts',(105.401917646169,-13.41098220979,67.394906186081));
#142293=CARTESIAN_POINT('Ctrl Pts',(105.556077554169,-13.41563420522,67.36049564276));
#142294=CARTESIAN_POINT('Ctrl Pts',(105.693195182669,-13.42587977367,67.321725313285));
#142295=CARTESIAN_POINT('Ctrl Pts',(105.787908303369,-13.42998293955,67.302642707235));
#142296=CARTESIAN_POINT('Ctrl Pts',(105.843699474669,-13.42556821351,67.304299111144));
#142297=CARTESIAN_POINT('Ctrl Pts',(105.901721494369,-13.41833028344,67.309756553462));
#142298=CARTESIAN_POINT('Ctrl Pts',(105.999937763269,-13.41754327638,67.292509415534));
#142299=CARTESIAN_POINT('Ctrl Pts',(106.191477591769,-13.42342170879,67.242225690654));
#142300=CARTESIAN_POINT('Ctrl Pts',(106.517706045669,-13.42874124418,67.170350527559));
#142301=CARTESIAN_POINT('Ctrl Pts',(106.972945214669,-13.43533245482,67.064406479912));
#142302=CARTESIAN_POINT('Ctrl Pts',(107.704900537069,-13.44597315009,66.883611271943));
#142303=CARTESIAN_POINT('Ctrl Pts',(108.977104518069,-13.46320029547,66.539642935235));
#142304=CARTESIAN_POINT('Ctrl Pts',(110.926077218569,-13.48513863723,65.918375229425));
#142305=CARTESIAN_POINT('Ctrl Pts',(112.473091744269,-13.49504460676,65.294246012061));
#142306=CARTESIAN_POINT('Ctrl Pts',(113.297333561069,-13.49824966426,64.913239003008));
#142307=CARTESIAN_POINT('Ctrl Pts',(105.478427326569,-13.19592113931,67.814696830677));
#142308=CARTESIAN_POINT('Ctrl Pts',(105.591643512169,-13.20306212524,67.784735120544));
#142309=CARTESIAN_POINT('Ctrl Pts',(105.695005130969,-13.2003702312,67.773227229612));
#142310=CARTESIAN_POINT('Ctrl Pts',(105.852272395169,-13.20541340111,67.738120811063));
#142311=CARTESIAN_POINT('Ctrl Pts',(105.993070604769,-13.21654104784,67.698517329733));
#142312=CARTESIAN_POINT('Ctrl Pts',(106.089820788269,-13.22091338784,67.679141475208));
#142313=CARTESIAN_POINT('Ctrl Pts',(106.145526268469,-13.21592737404,67.681167947591));
#142314=CARTESIAN_POINT('Ctrl Pts',(106.202588490469,-13.20778342815,67.687361817172));
#142315=CARTESIAN_POINT('Ctrl Pts',(106.301625528069,-13.20677245091,67.670083535681));
#142316=CARTESIAN_POINT('Ctrl Pts',(106.497013492869,-13.21312249052,67.618572997914));
#142317=CARTESIAN_POINT('Ctrl Pts',(106.828733086469,-13.21866923959,67.545296939605));
#142318=CARTESIAN_POINT('Ctrl Pts',(107.291294977669,-13.22548051179,67.437274779936));
#142319=CARTESIAN_POINT('Ctrl Pts',(108.035171310469,-13.23648940418,67.252647434483));
#142320=CARTESIAN_POINT('Ctrl Pts',(109.327875563169,-13.2542371189,66.900862712001));
#142321=CARTESIAN_POINT('Ctrl Pts',(111.307648267369,-13.27658471517,66.264026081233));
#142322=CARTESIAN_POINT('Ctrl Pts',(112.877927795969,-13.28622829001,65.622947147765));
#142323=CARTESIAN_POINT('Ctrl Pts',(113.714069025669,-13.2891351954,65.231473861432));
#142324=CARTESIAN_POINT('Ctrl Pts',(106.340768199269,-12.49617988855,68.938679513356));
#142325=CARTESIAN_POINT('Ctrl Pts',(106.461348540569,-12.50489810892,68.907399560009));
#142326=CARTESIAN_POINT('Ctrl Pts',(106.568694932869,-12.50140712085,68.895202904603));
#142327=CARTESIAN_POINT('Ctrl Pts',(106.735211577569,-12.50762735198,68.8582212536));
#142328=CARTESIAN_POINT('Ctrl Pts',(106.886027864869,-12.52127083058,68.816883431501));
#142329=CARTESIAN_POINT('Ctrl Pts',(106.988265476969,-12.52637208736,68.7968524246));
#142330=CARTESIAN_POINT('Ctrl Pts',(107.043686493669,-12.51965320266,68.799585472983));
#142331=CARTESIAN_POINT('Ctrl Pts',(107.098110445069,-12.50876138298,68.807353899232));
#142332=CARTESIAN_POINT('Ctrl Pts',(107.199726651269,-12.50704598615,68.789813299972));
#142333=CARTESIAN_POINT('Ctrl Pts',(107.406494709669,-12.51480155187,68.734910758024));
#142334=CARTESIAN_POINT('Ctrl Pts',(107.754339071769,-12.52098631199,68.657515777145));
#142335=CARTESIAN_POINT('Ctrl Pts',(108.238521910769,-12.5283887722,68.543365540915));
#142336=CARTESIAN_POINT('Ctrl Pts',(109.017525905269,-12.54039893825,68.347482153695));
#142337=CARTESIAN_POINT('Ctrl Pts',(110.370669954069,-12.55953474246,67.972787846649));
#142338=CARTESIAN_POINT('Ctrl Pts',(112.441188500469,-12.58287697068,67.290442003463));
#142339=CARTESIAN_POINT('Ctrl Pts',(114.080031548069,-12.59161918337,66.599933992995));
#142340=CARTESIAN_POINT('Ctrl Pts',(114.951331881769,-12.59359707781,66.177945211323));
#142341=CARTESIAN_POINT('Ctrl Pts',(107.705305680269,-11.02502719391,70.672420612353));
#142342=CARTESIAN_POINT('Ctrl Pts',(107.833381308469,-11.03528783259,70.641686343356));
#142343=CARTESIAN_POINT('Ctrl Pts',(107.951392073669,-11.03147444739,70.625804113145));
#142344=CARTESIAN_POINT('Ctrl Pts',(108.132218771569,-11.03935848219,70.586956173343));
#142345=CARTESIAN_POINT('Ctrl Pts',(108.293216363269,-11.05563644096,70.546564593204));
#142346=CARTESIAN_POINT('Ctrl Pts',(108.400946594669,-11.06130905076,70.526510377485));
#142347=CARTESIAN_POINT('Ctrl Pts',(108.456184132269,-11.05215576087,70.528338166625));
#142348=CARTESIAN_POINT('Ctrl Pts',(108.508445485069,-11.03741701809,70.535283131199));
#142349=CARTESIAN_POINT('Ctrl Pts',(108.615264948969,-11.0346333001,70.516278570094));
#142350=CARTESIAN_POINT('Ctrl Pts',(108.839308569169,-11.04433520867,70.457395905042));
#142351=CARTESIAN_POINT('Ctrl Pts',(109.211536657569,-11.05132191043,70.373703522875));
#142352=CARTESIAN_POINT('Ctrl Pts',(109.729138867969,-11.05938103001,70.250016451));
#142353=CARTESIAN_POINT('Ctrl Pts',(110.561966036269,-11.072549911,70.03691849479));
#142354=CARTESIAN_POINT('Ctrl Pts',(112.007824449569,-11.09321823243,69.627472483783));
#142355=CARTESIAN_POINT('Ctrl Pts',(114.216996636269,-11.11743227536,68.876876679782));
#142356=CARTESIAN_POINT('Ctrl Pts',(115.960380806369,-11.12475694542,68.113039813493));
#142357=CARTESIAN_POINT('Ctrl Pts',(116.885619574069,-11.12546079243,67.64590027152));
#142358=CARTESIAN_POINT('Ctrl Pts',(109.191315175669,-8.78258410338099,
72.435524489286));
#142359=CARTESIAN_POINT('Ctrl Pts',(109.318496917169,-8.79074914635699,
72.409211353215));
#142360=CARTESIAN_POINT('Ctrl Pts',(109.457842018369,-8.79007298746399,
72.3857653537551));
#142361=CARTESIAN_POINT('Ctrl Pts',(109.652915194969,-8.79836367012399,
72.3469077691189));
#142362=CARTESIAN_POINT('Ctrl Pts',(109.812649879569,-8.81202888418299,
72.3129069755914));
#142363=CARTESIAN_POINT('Ctrl Pts',(109.920220140069,-8.81641528675999,
72.2941525170867));
#142364=CARTESIAN_POINT('Ctrl Pts',(109.977236747169,-8.80705067009099,
72.2917242776799));
#142365=CARTESIAN_POINT('Ctrl Pts',(110.033657601769,-8.79212768276199,
72.2920076171935));
#142366=CARTESIAN_POINT('Ctrl Pts',(110.149585959269,-8.78926868864499,
72.269245222296));
#142367=CARTESIAN_POINT('Ctrl Pts',(110.390312409269,-8.79939079703399,
72.208516320971));
#142368=CARTESIAN_POINT('Ctrl Pts',(110.787643550469,-8.80677737047199,
72.1183221609802));
#142369=CARTESIAN_POINT('Ctrl Pts',(111.341319341869,-8.81519511236299,
71.984258610211));
#142370=CARTESIAN_POINT('Ctrl Pts',(112.231076887069,-8.82897614512199,
71.753069698651));
#142371=CARTESIAN_POINT('Ctrl Pts',(113.775050360169,-8.85050085119999,
71.307507313673));
#142372=CARTESIAN_POINT('Ctrl Pts',(116.129334143269,-8.87550178253899,
70.487298823422));
#142373=CARTESIAN_POINT('Ctrl Pts',(117.980858361269,-8.88284629712299,
69.650145847141));
#142374=CARTESIAN_POINT('Ctrl Pts',(118.962042593769,-8.88349197063399,
69.138257608636));
#142375=CARTESIAN_POINT('Ctrl Pts',(110.232926505569,-6.57248630373099,
73.5692045140896));
#142376=CARTESIAN_POINT('Ctrl Pts',(110.350595026869,-6.57646225464799,
73.5475367647887));
#142377=CARTESIAN_POINT('Ctrl Pts',(110.514246826669,-6.57982144133399,
73.5174352873947));
#142378=CARTESIAN_POINT('Ctrl Pts',(110.718524840469,-6.58683805357799,
73.4794333787347));
#142379=CARTESIAN_POINT('Ctrl Pts',(110.863485607269,-6.59434132275299,
73.4525971677378));
#142380=CARTESIAN_POINT('Ctrl Pts',(110.963557032969,-6.59638291515199,
73.4355706395166));
#142381=CARTESIAN_POINT('Ctrl Pts',(111.025104038669,-6.58935878847399,
73.4281786648391));
#142382=CARTESIAN_POINT('Ctrl Pts',(111.092548007969,-6.57825182407899,
73.420294394042));
#142383=CARTESIAN_POINT('Ctrl Pts',(111.218265532969,-6.57629110243299,
73.393596872829));
#142384=CARTESIAN_POINT('Ctrl Pts',(111.468139343069,-6.58471600587499,
73.3330060922452));
#142385=CARTESIAN_POINT('Ctrl Pts',(111.881580646269,-6.59151971225099,
73.2383699264408));
#142386=CARTESIAN_POINT('Ctrl Pts',(112.460108658969,-6.59931301435299,
73.0968990798939));
#142387=CARTESIAN_POINT('Ctrl Pts',(113.387924113269,-6.61202441850599,
72.8532330466304));
#142388=CARTESIAN_POINT('Ctrl Pts',(114.997470218769,-6.63187069013699,
72.3831353278457));
#142389=CARTESIAN_POINT('Ctrl Pts',(117.446904114169,-6.65506062627299,
71.516844779856));
#142390=CARTESIAN_POINT('Ctrl Pts',(119.367596957269,-6.66229891622699,
70.632566385416));
#142391=CARTESIAN_POINT('Ctrl Pts',(120.384430332969,-6.66327650304099,
70.092315923963));
#142392=CARTESIAN_POINT('Ctrl Pts',(110.901961917469,-4.62825007550899,
74.232635396243));
#142393=CARTESIAN_POINT('Ctrl Pts',(111.006547711069,-4.62839570152099,
74.214148267874));
#142394=CARTESIAN_POINT('Ctrl Pts',(111.193027963169,-4.63438875271899,
74.179690962165));
#142395=CARTESIAN_POINT('Ctrl Pts',(111.402994344069,-4.63938360278399,
74.142365011593));
#142396=CARTESIAN_POINT('Ctrl Pts',(111.526432862869,-4.64076307547399,
74.121036795092));
#142397=CARTESIAN_POINT('Ctrl Pts',(111.614963911669,-4.64062253314799,
74.105572716154));
#142398=CARTESIAN_POINT('Ctrl Pts',(111.682764776369,-4.63679325639199,
74.094106144587));
#142399=CARTESIAN_POINT('Ctrl Pts',(111.764602035069,-4.63067007736599,
74.079412733284));
#142400=CARTESIAN_POINT('Ctrl Pts',(111.899222872569,-4.62973342336699,
74.049659910301));
#142401=CARTESIAN_POINT('Ctrl Pts',(112.152730704169,-4.63547879755899,
73.989765470765));
#142402=CARTESIAN_POINT('Ctrl Pts',(112.575258310169,-4.64094937026599,
73.8923029904515));
#142403=CARTESIAN_POINT('Ctrl Pts',(113.169259174669,-4.64722823235099,
73.7460063308676));
#142404=CARTESIAN_POINT('Ctrl Pts',(114.119837515269,-4.65744614110199,
73.4944221208521));
#142405=CARTESIAN_POINT('Ctrl Pts',(115.768577097969,-4.67339593125899,
73.0090005205452));
#142406=CARTESIAN_POINT('Ctrl Pts',(118.273335469269,-4.69224475007099,
72.1147099921028));
#142407=CARTESIAN_POINT('Ctrl Pts',(120.232682197569,-4.69862092546799,
71.202748992289));
#142408=CARTESIAN_POINT('Ctrl Pts',(121.269225159869,-4.69980354156199,
70.646094772409));
#142409=CARTESIAN_POINT('Ctrl Pts',(111.302429095369,-3.11051865222899,
74.598597220957));
#142410=CARTESIAN_POINT('Ctrl Pts',(111.394664964469,-3.10840859475799,
74.582176303359));
#142411=CARTESIAN_POINT('Ctrl Pts',(111.599388335569,-3.11523302300199,
74.54494440117));
#142412=CARTESIAN_POINT('Ctrl Pts',(111.812891893969,-3.11842203978399,
74.507953556329));
#142413=CARTESIAN_POINT('Ctrl Pts',(111.914920967869,-3.11592395483799,
74.490718133494));
#142414=CARTESIAN_POINT('Ctrl Pts',(111.991551157469,-3.11454821759999,
74.476683595707));
#142415=CARTESIAN_POINT('Ctrl Pts',(112.065694454869,-3.11329885156799,
74.462165162077));
#142416=CARTESIAN_POINT('Ctrl Pts',(112.161368620869,-3.11103482700299,
74.44237079032));
#142417=CARTESIAN_POINT('Ctrl Pts',(112.302906402769,-3.11077709479499,
74.410512416406));
#142418=CARTESIAN_POINT('Ctrl Pts',(112.557032270969,-3.11418756663799,
74.35133796726));
#142419=CARTESIAN_POINT('Ctrl Pts',(112.984043669169,-3.11832910238899,
74.252142747192));
#142420=CARTESIAN_POINT('Ctrl Pts',(113.586802782869,-3.12303242315999,
74.102855342059));
#142421=CARTESIAN_POINT('Ctrl Pts',(114.549613779969,-3.13070244834699,
73.8464836526737));
#142422=CARTESIAN_POINT('Ctrl Pts',(116.219395574769,-3.14265309403299,
73.351981889596));
#142423=CARTESIAN_POINT('Ctrl Pts',(118.752714943269,-3.15700449747199,
72.4416801021735));
#142424=CARTESIAN_POINT('Ctrl Pts',(120.730863957769,-3.16240049109099,
71.514613718839));
#142425=CARTESIAN_POINT('Ctrl Pts',(121.776847155169,-3.16372012641999,
70.949175311126));
#142426=CARTESIAN_POINT('Ctrl Pts',(111.595468274169,-1.45466988121399,
74.846425761956));
#142427=CARTESIAN_POINT('Ctrl Pts',(111.672253123969,-1.45163639103699,
74.831834122798));
#142428=CARTESIAN_POINT('Ctrl Pts',(111.896696929169,-1.45746867042799,
74.792127065424));
#142429=CARTESIAN_POINT('Ctrl Pts',(112.113181296169,-1.45871739800999,
74.755147828598));
#142430=CARTESIAN_POINT('Ctrl Pts',(112.186881942369,-1.45424709587499,
74.742277395159));
#142431=CARTESIAN_POINT('Ctrl Pts',(112.247193366669,-1.45261550698799,
74.730167292197));
#142432=CARTESIAN_POINT('Ctrl Pts',(112.329914138269,-1.45373145173099,
74.712493047907));
#142433=CARTESIAN_POINT('Ctrl Pts',(112.443345128069,-1.45470158497499,
74.687471532958));
#142434=CARTESIAN_POINT('Ctrl Pts',(112.592014534569,-1.45484197653799,
74.653711867639));
#142435=CARTESIAN_POINT('Ctrl Pts',(112.844283022569,-1.45592779359099,
74.595400592069));
#142436=CARTESIAN_POINT('Ctrl Pts',(113.273006027669,-1.45860301392999,
74.494769001152));
#142437=CARTESIAN_POINT('Ctrl Pts',(113.881141937569,-1.46150941159199,
74.343021342311));
#142438=CARTESIAN_POINT('Ctrl Pts',(114.850437750669,-1.46639764963599,
74.082853248785));
#142439=CARTESIAN_POINT('Ctrl Pts',(116.531353108869,-1.47415976484399,
73.5814438142693));
#142440=CARTESIAN_POINT('Ctrl Pts',(119.077925826669,-1.48453718184899,
72.659858147644));
#142441=CARTESIAN_POINT('Ctrl Pts',(121.062922877469,-1.49054042270799,
71.723311212546));
#142442=CARTESIAN_POINT('Ctrl Pts',(122.112156142069,-1.49316944729799,
71.152601994141));
#142443=CARTESIAN_POINT('Ctrl Pts',(111.696491028569,-0.360124565212986,
74.900584192463));
#142444=CARTESIAN_POINT('Ctrl Pts',(111.761426133369,-0.357775193352486,
74.887267715531));
#142445=CARTESIAN_POINT('Ctrl Pts',(111.999128447469,-0.361200807995286,
74.845983993127));
#142446=CARTESIAN_POINT('Ctrl Pts',(112.217455760169,-0.361051136160086,
74.808705222488));
#142447=CARTESIAN_POINT('Ctrl Pts',(112.267551186169,-0.357445487552886,
74.799599156875));
#142448=CARTESIAN_POINT('Ctrl Pts',(112.313688292569,-0.356642658628786,
74.789619793948));
#142449=CARTESIAN_POINT('Ctrl Pts',(112.404015928469,-0.358478224453286,
74.769559885122));
#142450=CARTESIAN_POINT('Ctrl Pts',(112.532089053369,-0.360155784921286,
74.740675828192));
#142451=CARTESIAN_POINT('Ctrl Pts',(112.685292843269,-0.360040770149286,
74.705871242989));
#142452=CARTESIAN_POINT('Ctrl Pts',(112.934525079669,-0.359694178076486,
74.648368228787));
#142453=CARTESIAN_POINT('Ctrl Pts',(113.362220200769,-0.360955145893786,
74.54721473497));
#142454=CARTESIAN_POINT('Ctrl Pts',(113.971187372169,-0.361918458962486,
74.394502753305));
#142455=CARTESIAN_POINT('Ctrl Pts',(114.940214773769,-0.363780597524286,
74.13302532246));
#142456=CARTESIAN_POINT('Ctrl Pts',(116.620643502969,-0.366578249264186,
73.6295086638907));
#142457=CARTESIAN_POINT('Ctrl Pts',(119.163972296969,-0.370652417349286,
72.7054355250659));
#142458=CARTESIAN_POINT('Ctrl Pts',(121.144272815269,-0.373784456041386,
71.768179001727));
#142459=CARTESIAN_POINT('Ctrl Pts',(122.190927037569,-0.375416645258886,
71.197391893318));
#142460=CARTESIAN_POINT('Ctrl Pts',(111.719449830669,0.168542024809114,
74.886725365525));
#142461=CARTESIAN_POINT('Ctrl Pts',(111.777956490669,0.170096013221014,
74.874161149833));
#142462=CARTESIAN_POINT('Ctrl Pts',(112.022380833669,0.168541949368414,
74.832039678843));
#142463=CARTESIAN_POINT('Ctrl Pts',(112.241742962669,0.169476862651314,
74.794498014263));
#142464=CARTESIAN_POINT('Ctrl Pts',(112.278226804169,0.171833202524114,
74.787818476474));
#142465=CARTESIAN_POINT('Ctrl Pts',(112.315978018769,0.171867884708614,
74.779355268586));
#142466=CARTESIAN_POINT('Ctrl Pts',(112.410919825469,0.170092732407714,
74.75789040944));
#142467=CARTESIAN_POINT('Ctrl Pts',(112.547469632369,0.168715079612914,
74.726766261338));
#142468=CARTESIAN_POINT('Ctrl Pts',(112.702898853469,0.169203428043914,
74.69149379952));
#142469=CARTESIAN_POINT('Ctrl Pts',(112.950064158069,0.170274286069014,
74.634528449429));
#142470=CARTESIAN_POINT('Ctrl Pts',(113.376613512969,0.170027200701914,
74.533302102221));
#142471=CARTESIAN_POINT('Ctrl Pts',(113.985227807269,0.170539620258414,
74.380372401485));
#142472=CARTESIAN_POINT('Ctrl Pts',(114.952812262469,0.171032612972814,
74.118724642226));
#142473=CARTESIAN_POINT('Ctrl Pts',(116.630740742369,0.172350907441314,
73.6151214271312));
#142474=CARTESIAN_POINT('Ctrl Pts',(119.168949242269,0.174425178655114,
72.6917147397916));
#142475=CARTESIAN_POINT('Ctrl Pts',(121.144176338569,0.175723369492814,
71.756197744828));
#142476=CARTESIAN_POINT('Ctrl Pts',(122.188142213169,0.176373882112714,
71.186651895743));
#142477=CARTESIAN_POINT('Ctrl Pts',(111.837855321069,-3.16944077378891E-5,
74.865893185247));
#142478=CARTESIAN_POINT('Ctrl Pts',(111.905501829069,-0.000126979998721889,
74.853819715785));
#142479=CARTESIAN_POINT('Ctrl Pts',(112.067033374169,-0.00145620723710179,
74.825979590322));
#142480=CARTESIAN_POINT('Ctrl Pts',(112.232987931369,-0.000804753782924589,
74.797596316915));
#142481=CARTESIAN_POINT('Ctrl Pts',(112.273760035969,0.00190512480894021,
74.790159935677));
#142482=CARTESIAN_POINT('Ctrl Pts',(112.314147583869,0.00217643220178221,
74.781227585595));
#142483=CARTESIAN_POINT('Ctrl Pts',(112.407642187069,0.000395759237193011,
74.760204664648));
#142484=CARTESIAN_POINT('Ctrl Pts',(112.541521774169,-0.00105456873310479,
74.729786169022));
#142485=CARTESIAN_POINT('Ctrl Pts',(112.696237777969,-0.000677150123564289,
74.694665286851));
#142486=CARTESIAN_POINT('Ctrl Pts',(112.944044643669,0.000162384145561411,
74.637532653636));
#142487=CARTESIAN_POINT('Ctrl Pts',(113.370937985569,-0.000398344211388589,
74.536336212313));
#142488=CARTESIAN_POINT('Ctrl Pts',(113.979637815569,-0.000339910781080989,
74.38348544604));
#142489=CARTESIAN_POINT('Ctrl Pts',(114.947637210069,-0.000572835564488789,
74.121909214046));
#142490=CARTESIAN_POINT('Ctrl Pts',(116.626285365669,-0.000492304917713389,
73.618367621019));
#142491=CARTESIAN_POINT('Ctrl Pts',(119.105257840569,-0.000471121657127989,
72.7169063002584));
#142492=CARTESIAN_POINT('Ctrl Pts',(121.026723756869,8.56223467947709E-5,
71.813563678684));
#142493=CARTESIAN_POINT('Ctrl Pts',(122.019294640269,7.00634385962609E-5,
71.280020192514));
#142494=CARTESIAN_POINT('Ctrl Pts',(111.719593813469,-0.171868557479286,
74.886637782194));
#142495=CARTESIAN_POINT('Ctrl Pts',(111.778059621769,-0.173417549884886,
74.874078349544));
#142496=CARTESIAN_POINT('Ctrl Pts',(112.022526849069,-0.171875263124186,
74.831951508582));
#142497=CARTESIAN_POINT('Ctrl Pts',(112.241895554969,-0.172815126157786,
74.794408177235));
#142498=CARTESIAN_POINT('Ctrl Pts',(112.278293639269,-0.175163590064086,
74.78774392618));
#142499=CARTESIAN_POINT('Ctrl Pts',(112.315992195369,-0.175193426080186,
74.779290235468));
#142500=CARTESIAN_POINT('Ctrl Pts',(112.410963116769,-0.173418660436886,
74.757816516147));
#142501=CARTESIAN_POINT('Ctrl Pts',(112.547566271969,-0.172042908902086,
74.726678270653));
#142502=CARTESIAN_POINT('Ctrl Pts',(112.703009488169,-0.172533610923386,
74.691402866405));
#142503=CARTESIAN_POINT('Ctrl Pts',(112.950161776769,-0.173609024219986,
74.634440900189));
#142504=CARTESIAN_POINT('Ctrl Pts',(113.376703920169,-0.173368321007886,
74.533214092014));
#142505=CARTESIAN_POINT('Ctrl Pts',(113.985315989269,-0.173890031129486,
74.380283018442));
#142506=CARTESIAN_POINT('Ctrl Pts',(114.952891357869,-0.174397850254086,
74.118634182427));
#142507=CARTESIAN_POINT('Ctrl Pts',(116.630804091769,-0.175742056888286,
73.615030414165));
#142508=CARTESIAN_POINT('Ctrl Pts',(119.169069409069,-0.177855112533286,
72.6915955064676));
#142509=CARTESIAN_POINT('Ctrl Pts',(121.144345474869,-0.179181240266986,
71.756041340767));
#142510=CARTESIAN_POINT('Ctrl Pts',(122.188370590769,-0.179846170816786,
71.186449512022));
#142511=CARTESIAN_POINT('Ctrl Pts',(111.696720868469,0.357553932207514,
74.900699702834));
#142512=CARTESIAN_POINT('Ctrl Pts',(111.761627617569,0.355206270543514,
74.88738629695));
#142513=CARTESIAN_POINT('Ctrl Pts',(111.999361718969,0.358626044628914,
74.846098758947));
#142514=CARTESIAN_POINT('Ctrl Pts',(112.217693493969,0.358473043628614,
74.808819236382));
#142515=CARTESIAN_POINT('Ctrl Pts',(112.267732763269,0.354869659983714,
74.799722194961));
#142516=CARTESIAN_POINT('Ctrl Pts',(112.313836230769,0.354068889305514,
74.789747953326));
#142517=CARTESIAN_POINT('Ctrl Pts',(112.404182058769,0.355906032159314,
74.769682354654));
#142518=CARTESIAN_POINT('Ctrl Pts',(112.532289985869,0.357585071714214,
74.740789115781));
#142519=CARTESIAN_POINT('Ctrl Pts',(112.685504442769,0.357469385220414,
74.705982084654));
#142520=CARTESIAN_POINT('Ctrl Pts',(112.934729378669,0.357119416652214,
74.648481010021));
#142521=CARTESIAN_POINT('Ctrl Pts',(113.362421902569,0.358376964644214,
74.547326339107));
#142522=CARTESIAN_POINT('Ctrl Pts',(113.971390825869,0.359335555158114,
74.394612156851));
#142523=CARTESIAN_POINT('Ctrl Pts',(114.940417238669,0.361190320974714,
74.133131773532));
#142524=CARTESIAN_POINT('Ctrl Pts',(116.620844208169,0.363975801124614,
73.6296104139194));
#142525=CARTESIAN_POINT('Ctrl Pts',(119.164253646169,0.368034378933414,
72.705499511873));
#142526=CARTESIAN_POINT('Ctrl Pts',(121.144623526169,0.371158886658614,
71.768193655697));
#142527=CARTESIAN_POINT('Ctrl Pts',(122.191347654569,0.372788308176714,
71.197352785866));
#142528=CARTESIAN_POINT('Ctrl Pts',(111.595710961569,1.45325035480701,74.846630855493));
#142529=CARTESIAN_POINT('Ctrl Pts',(111.672482312469,1.45021612247701,74.832040780653));
#142530=CARTESIAN_POINT('Ctrl Pts',(111.896943450769,1.45604747320501,74.792331548089));
#142531=CARTESIAN_POINT('Ctrl Pts',(112.113430453969,1.45729453350601,74.755352280744));
#142532=CARTESIAN_POINT('Ctrl Pts',(112.187106546769,1.45282267665201,74.742485580224));
#142533=CARTESIAN_POINT('Ctrl Pts',(112.247403885269,1.45119094433001,74.730377126641));
#142534=CARTESIAN_POINT('Ctrl Pts',(112.330132104869,1.45230888561001,74.712700186003));
#142535=CARTESIAN_POINT('Ctrl Pts',(112.443578434869,1.45328172180801,74.687674215795));
#142536=CARTESIAN_POINT('Ctrl Pts',(112.592253937869,1.45342243526401,74.653912939217));
#142537=CARTESIAN_POINT('Ctrl Pts',(112.844520708369,1.45450628572401,74.595602400977));
#142538=CARTESIAN_POINT('Ctrl Pts',(113.273244987869,1.45718026009701,74.49496960171));
#142539=CARTESIAN_POINT('Ctrl Pts',(113.881385280069,1.46008513257001,74.343219868355));
#142540=CARTESIAN_POINT('Ctrl Pts',(114.850686264869,1.46497102099801,74.083048585761));
#142541=CARTESIAN_POINT('Ctrl Pts',(116.531610508469,1.47272962768101,73.5816333668206));
#142542=CARTESIAN_POINT('Ctrl Pts',(119.078282948369,1.48310419649501,72.6600059770705));
#142543=CARTESIAN_POINT('Ctrl Pts',(121.063366585069,1.48910835453501,71.72340298214));
#142544=CARTESIAN_POINT('Ctrl Pts',(122.112678824069,1.49173876143601,71.152635474748));
#142545=CARTESIAN_POINT('Ctrl Pts',(111.302470472569,3.11036131899101,74.598635134671));
#142546=CARTESIAN_POINT('Ctrl Pts',(111.394705080869,3.10825098976601,74.582214427328));
#142547=CARTESIAN_POINT('Ctrl Pts',(111.599430723269,3.11507552701201,74.544982169353));
#142548=CARTESIAN_POINT('Ctrl Pts',(111.812934849969,3.11826434695701,74.50799132848));
#142549=CARTESIAN_POINT('Ctrl Pts',(111.914961677469,3.11576585252101,74.49075633246));
#142550=CARTESIAN_POINT('Ctrl Pts',(111.991590635469,3.11438998720401,74.476721939464));
#142551=CARTESIAN_POINT('Ctrl Pts',(112.065734580169,3.11314088897001,74.462203188155));
#142552=CARTESIAN_POINT('Ctrl Pts',(112.161410197369,3.11087726918001,74.442408279252));
#142553=CARTESIAN_POINT('Ctrl Pts',(112.302948742769,3.11061961324801,74.410549673625));
#142554=CARTESIAN_POINT('Ctrl Pts',(112.557074701769,3.11402984287401,74.351375293478));
#142555=CARTESIAN_POINT('Ctrl Pts',(112.984086541969,3.11817123287701,74.252179898395));
#142556=CARTESIAN_POINT('Ctrl Pts',(113.586846597569,3.12287438806101,74.102892171601));
#142557=CARTESIAN_POINT('Ctrl Pts',(114.549658879369,3.13054413896501,73.8465199768088));
#142558=CARTESIAN_POINT('Ctrl Pts',(116.219442899969,3.14249435186701,73.3520172503437));
#142559=CARTESIAN_POINT('Ctrl Pts',(118.752854170869,3.15684575437601,72.4416818256266));
#142560=CARTESIAN_POINT('Ctrl Pts',(120.731086507869,3.16224156635401,71.514566000912));
#142561=CARTESIAN_POINT('Ctrl Pts',(121.777147093869,3.16356103770801,70.949073117786));
#142562=CARTESIAN_POINT('Ctrl Pts',(110.901961451069,4.62824984549301,74.232635559883));
#142563=CARTESIAN_POINT('Ctrl Pts',(111.006547427469,4.62839545723401,74.214148401757));
#142564=CARTESIAN_POINT('Ctrl Pts',(111.193027966069,4.63438852139201,74.179691041673));
#142565=CARTESIAN_POINT('Ctrl Pts',(111.402994594569,4.63938337439001,74.142365049295));
#142566=CARTESIAN_POINT('Ctrl Pts',(111.526433112769,4.64076284552401,74.121036832436));
#142567=CARTESIAN_POINT('Ctrl Pts',(111.614964129869,4.64062229704501,74.105572759132));
#142568=CARTESIAN_POINT('Ctrl Pts',(111.682764955069,4.63679301361201,74.09410619405));
#142569=CARTESIAN_POINT('Ctrl Pts',(111.764602222569,4.63066983700401,74.079412776184));
#142570=CARTESIAN_POINT('Ctrl Pts',(111.899223119269,4.62973319388701,74.049659934194));
#142571=CARTESIAN_POINT('Ctrl Pts',(112.152730985569,4.63547857422301,73.98976548501));
#142572=CARTESIAN_POINT('Ctrl Pts',(112.575258551469,4.64094913902301,73.8923030139087));
#142573=CARTESIAN_POINT('Ctrl Pts',(113.169259448369,4.64722800682301,73.7460063403004));
#142574=CARTESIAN_POINT('Ctrl Pts',(114.119837790469,4.65744591559201,73.4944221223189));
#142575=CARTESIAN_POINT('Ctrl Pts',(115.768577398569,4.67339571091001,73.0090004995231));
#142576=CARTESIAN_POINT('Ctrl Pts',(118.273423680269,4.69224519885701,72.114678555699));
#142577=CARTESIAN_POINT('Ctrl Pts',(120.232851148669,4.69862127106701,71.202670417722));
#142578=CARTESIAN_POINT('Ctrl Pts',(121.269469905269,4.69980362325801,70.645963403317));
#142579=CARTESIAN_POINT('Ctrl Pts',(110.232925928169,6.57248641407201,73.5692045744232));
#142580=CARTESIAN_POINT('Ctrl Pts',(110.350594809869,6.57646238792501,73.547536757197));
#142581=CARTESIAN_POINT('Ctrl Pts',(110.514246798369,6.57982157032801,73.517435246692));
#142582=CARTESIAN_POINT('Ctrl Pts',(110.718525112169,6.58683820167901,73.4794332803124));
#142583=CARTESIAN_POINT('Ctrl Pts',(110.863485898169,6.59434146833501,73.4525970688935));
#142584=CARTESIAN_POINT('Ctrl Pts',(110.963557254469,6.59638304026101,73.4355705602877));
#142585=CARTESIAN_POINT('Ctrl Pts',(111.025104194869,6.58935890101301,73.4281785994106));
#142586=CARTESIAN_POINT('Ctrl Pts',(111.092548167869,6.57825194271401,73.4202943209154));
#142587=CARTESIAN_POINT('Ctrl Pts',(111.218265769069,6.57629123923301,73.3935967718485));
#142588=CARTESIAN_POINT('Ctrl Pts',(111.468139625369,6.58471615098001,73.3330059774607));
#142589=CARTESIAN_POINT('Ctrl Pts',(111.881580876669,6.59151984344101,73.2383698280508));
#142590=CARTESIAN_POINT('Ctrl Pts',(112.460108929569,6.59931315242701,73.0968989644948));
#142591=CARTESIAN_POINT('Ctrl Pts',(113.387924384169,6.61202455237501,72.8532329259722));
#142592=CARTESIAN_POINT('Ctrl Pts',(114.997470519269,6.63187082303001,72.3831351861819));
#142593=CARTESIAN_POINT('Ctrl Pts',(117.446990386569,6.65506156567701,71.516814210058));
#142594=CARTESIAN_POINT('Ctrl Pts',(119.367762586869,6.66229965768501,70.632490081439));
#142595=CARTESIAN_POINT('Ctrl Pts',(120.384670436869,6.66327684772201,70.092188313576));
#142596=CARTESIAN_POINT('Ctrl Pts',(109.191314516269,8.78258400348901,72.4355246472895));
#142597=CARTESIAN_POINT('Ctrl Pts',(109.318496766669,8.79074911336402,72.4092113893872));
#142598=CARTESIAN_POINT('Ctrl Pts',(109.457841968569,8.79007292918101,72.3857653855102));
#142599=CARTESIAN_POINT('Ctrl Pts',(109.652915483569,8.79836364817301,72.346907721148));
#142600=CARTESIAN_POINT('Ctrl Pts',(109.812650199469,8.81202886086001,72.3129069288903));
#142601=CARTESIAN_POINT('Ctrl Pts',(109.920220362869,8.81641523097701,72.294152507876));
#142602=CARTESIAN_POINT('Ctrl Pts',(109.977236887169,8.80705059642201,72.2917242903443));
#142603=CARTESIAN_POINT('Ctrl Pts',(110.033657738369,8.79212761653301,72.2920076209844));
#142604=CARTESIAN_POINT('Ctrl Pts',(110.149586182069,8.78926864593201,72.2692451879473));
#142605=CARTESIAN_POINT('Ctrl Pts',(110.390312685769,8.79939076523601,72.2085162678206));
#142606=CARTESIAN_POINT('Ctrl Pts',(110.787643766769,8.80677732173501,72.1183221319088));
#142607=CARTESIAN_POINT('Ctrl Pts',(111.341319601969,8.81519507323601,71.98425856008));
#142608=CARTESIAN_POINT('Ctrl Pts',(112.231077144669,8.82897610251101,71.753069645188));
#142609=CARTESIAN_POINT('Ctrl Pts',(113.775050646669,8.85050081128701,71.307507238708));
#142610=CARTESIAN_POINT('Ctrl Pts',(116.129417060569,8.87550261923901,70.48726993864));
#142611=CARTESIAN_POINT('Ctrl Pts',(117.981018021169,8.88284688927401,69.650073667281));
#142612=CARTESIAN_POINT('Ctrl Pts',(118.962274274669,8.88349208348702,69.138136754579));
#142613=CARTESIAN_POINT('Ctrl Pts',(107.705304995269,11.02502713784,70.67242078014));
#142614=CARTESIAN_POINT('Ctrl Pts',(107.833381203869,11.0352878678,70.641686335191));
#142615=CARTESIAN_POINT('Ctrl Pts',(107.951392012169,11.03147444484,70.625804130375));
#142616=CARTESIAN_POINT('Ctrl Pts',(108.132219055569,11.03935852329,70.586956090092));
#142617=CARTESIAN_POINT('Ctrl Pts',(108.293216685169,11.0556364815,70.546564513235));
#142618=CARTESIAN_POINT('Ctrl Pts',(108.400946813269,11.06130905511,70.526510351234));
#142619=CARTESIAN_POINT('Ctrl Pts',(108.456184265469,11.05215574674,70.528338167977));
#142620=CARTESIAN_POINT('Ctrl Pts',(108.508445607669,11.03741701131,70.535283122245));
#142621=CARTESIAN_POINT('Ctrl Pts',(108.615265154269,11.03463331631,70.516278516022));
#142622=CARTESIAN_POINT('Ctrl Pts',(108.839308828169,11.04433523527,70.457395828984));
#142623=CARTESIAN_POINT('Ctrl Pts',(109.211536858369,11.05132192073,70.373703475901));
#142624=CARTESIAN_POINT('Ctrl Pts',(109.729139110969,11.05938104937,70.250016380467));
#142625=CARTESIAN_POINT('Ctrl Pts',(110.561966276769,11.0725499267,70.036918422342));
#142626=CARTESIAN_POINT('Ctrl Pts',(112.007824717869,11.09321824995,69.627472389874));
#142627=CARTESIAN_POINT('Ctrl Pts',(114.217074442569,11.11743314014,68.876850220292));
#142628=CARTESIAN_POINT('Ctrl Pts',(115.960531140069,11.12475758935,68.112973926865));
#142629=CARTESIAN_POINT('Ctrl Pts',(116.885838043069,11.12546097109,67.645789953276));
#142630=CARTESIAN_POINT('Ctrl Pts',(106.340746064769,12.49620299268,68.938652400208));
#142631=CARTESIAN_POINT('Ctrl Pts',(106.461326845869,12.50492126694,68.907372247313));
#142632=CARTESIAN_POINT('Ctrl Pts',(106.568673101969,12.50143025146,68.895175686918));
#142633=CARTESIAN_POINT('Ctrl Pts',(106.735189843669,12.50765049241,68.858193961533));
#142634=CARTESIAN_POINT('Ctrl Pts',(106.886006010469,12.52129392982,68.816856127653));
#142635=CARTESIAN_POINT('Ctrl Pts',(106.988243444669,12.52639514863,68.796825178415));
#142636=CARTESIAN_POINT('Ctrl Pts',(107.043664387869,12.5196762878,68.799558268862));
#142637=CARTESIAN_POINT('Ctrl Pts',(107.098088360869,12.50878453451,68.807326697118));
#142638=CARTESIAN_POINT('Ctrl Pts',(107.199704553969,12.50706917166,68.789786078134));
#142639=CARTESIAN_POINT('Ctrl Pts',(107.406472387069,12.51482471433,68.734883578961));
#142640=CARTESIAN_POINT('Ctrl Pts',(107.754316317369,12.52100944962,68.657488725541));
#142641=CARTESIAN_POINT('Ctrl Pts',(108.238498666269,12.528411906,68.543338618884));
#142642=CARTESIAN_POINT('Ctrl Pts',(109.017501812769,12.54042205079,68.347455503471));
#142643=CARTESIAN_POINT('Ctrl Pts',(110.370644427969,12.5595578317,67.972761728283));
#142644=CARTESIAN_POINT('Ctrl Pts',(112.441233465469,12.58290086265,67.290392999253));
#142645=CARTESIAN_POINT('Ctrl Pts',(114.080143265369,12.59164302917,66.599850642037));
#142646=CARTESIAN_POINT('Ctrl Pts',(114.951507165569,12.59362065671,66.177822481062));
#142647=CARTESIAN_POINT('Ctrl Pts',(105.478381382169,13.19595788191,67.814637903535));
#142648=CARTESIAN_POINT('Ctrl Pts',(105.591597695769,13.20309884871,67.784676078824));
#142649=CARTESIAN_POINT('Ctrl Pts',(105.694959142869,13.20040697058,67.773168259565));
#142650=CARTESIAN_POINT('Ctrl Pts',(105.852226219569,13.20545010774,67.738061839862));
#142651=CARTESIAN_POINT('Ctrl Pts',(105.993023940669,13.21657762319,67.698458452134));
#142652=CARTESIAN_POINT('Ctrl Pts',(106.089773756169,13.22094990211,67.679082686242));
#142653=CARTESIAN_POINT('Ctrl Pts',(106.145479184669,13.21596396795,67.681109146461));
#142654=CARTESIAN_POINT('Ctrl Pts',(106.202541533469,13.20782017102,67.68730292165));
#142655=CARTESIAN_POINT('Ctrl Pts',(106.301578493169,13.20680924394,67.67002461521));
#142656=CARTESIAN_POINT('Ctrl Pts',(106.496965899669,13.21315921563,67.618514237609));
#142657=CARTESIAN_POINT('Ctrl Pts',(106.828684605869,13.21870592217,67.545238419545));
#142658=CARTESIAN_POINT('Ctrl Pts',(107.291245390969,13.22551716859,67.437216561838));
#142659=CARTESIAN_POINT('Ctrl Pts',(108.035119877169,13.23652600666,67.252589805463));
#142660=CARTESIAN_POINT('Ctrl Pts',(109.327820975069,13.2542736501,66.90080626753));
#142661=CARTESIAN_POINT('Ctrl Pts',(111.307658395069,13.27662197795,66.26394965669));
#142662=CARTESIAN_POINT('Ctrl Pts',(112.877999996569,13.28626564592,65.62284046902));
#142663=CARTESIAN_POINT('Ctrl Pts',(113.714201400569,13.28917245567,65.231331633562));
#142664=CARTESIAN_POINT('Ctrl Pts',(105.189070557869,13.40684195318,67.435610002882));
#142665=CARTESIAN_POINT('Ctrl Pts',(105.299583835569,13.4134261125,67.40626642105));
#142666=CARTESIAN_POINT('Ctrl Pts',(105.401847697369,13.41103243054,67.3948159773));
#142667=CARTESIAN_POINT('Ctrl Pts',(105.556007154469,13.41568435939,67.360405502425));
#142668=CARTESIAN_POINT('Ctrl Pts',(105.693123942669,13.42592971861,67.321635373775));
#142669=CARTESIAN_POINT('Ctrl Pts',(105.787836502669,13.43003279964,67.302552890253));
#142670=CARTESIAN_POINT('Ctrl Pts',(105.843627630969,13.42561819941,67.304209229825));
#142671=CARTESIAN_POINT('Ctrl Pts',(105.901649868169,13.41838048947,67.309666484894));
#142672=CARTESIAN_POINT('Ctrl Pts',(105.999865994969,13.4175935476,67.29241931739));
#142673=CARTESIAN_POINT('Ctrl Pts',(106.191404943369,13.42347187295,67.242135867778));
#142674=CARTESIAN_POINT('Ctrl Pts',(106.517632051069,13.42879134615,67.170261061005));
#142675=CARTESIAN_POINT('Ctrl Pts',(106.972869502569,13.43538250913,67.064317489389));
#142676=CARTESIAN_POINT('Ctrl Pts',(107.704821982669,13.44602311522,66.883523192121));
#142677=CARTESIAN_POINT('Ctrl Pts',(108.977021096569,13.4632501382,66.539556699398));
#142678=CARTESIAN_POINT('Ctrl Pts',(110.926054857169,13.48518915223,65.918270879432));
#142679=CARTESIAN_POINT('Ctrl Pts',(112.473128590069,13.49509526728,65.294113763225));
#142680=CARTESIAN_POINT('Ctrl Pts',(113.297428787769,13.49830029927,64.91307310569));
#142681=CARTESIAN_POINT('Ctrl Pts',(111.837855321069,-3.16944077378891E-5,
74.865893185247));
#142682=CARTESIAN_POINT('Ctrl Pts',(111.814564406692,0.481394395961152,
74.8700371574733));
#142683=CARTESIAN_POINT('Ctrl Pts',(111.719575962393,1.51657032727011,74.8123455490061));
#142684=CARTESIAN_POINT('Ctrl Pts',(111.444434225665,3.11067739388218,74.5731663746096));
#142685=CARTESIAN_POINT('Ctrl Pts',(111.048792048017,4.63025083099635,74.2062440518196));
#142686=CARTESIAN_POINT('Ctrl Pts',(110.383842672146,6.57696395825753,73.5414122769946));
#142687=CARTESIAN_POINT('Ctrl Pts',(109.342826174747,8.7894085376038,72.4057751166405));
#142688=CARTESIAN_POINT('Ctrl Pts',(107.850972194421,11.0326713699803,70.6411881108118));
#142689=CARTESIAN_POINT('Ctrl Pts',(106.505291772843,12.472019416551,68.9441554245893));
#142690=CARTESIAN_POINT('Ctrl Pts',(105.66717799772,13.1524911207421,67.8633232117159));
#142691=CARTESIAN_POINT('Ctrl Pts',(105.406714415269,13.34497198119,67.526105385012));
#142692=CARTESIAN_POINT('Ctrl Pts',(94.2719755564691,-0.232535619158986,
77.960293090095));
#142693=CARTESIAN_POINT('Ctrl Pts',(96.4654948137691,-0.234045302815186,
77.573429542034));
#142694=CARTESIAN_POINT('Ctrl Pts',(100.753541807869,-0.237849509244786,
76.817900401937));
#142695=CARTESIAN_POINT('Ctrl Pts',(105.569477935369,-0.243699651693586,
75.968797979103));
#142696=CARTESIAN_POINT('Ctrl Pts',(108.706635670869,-0.248295135150586,
75.414082723585));
#142697=CARTESIAN_POINT('Ctrl Pts',(110.394346681069,-0.250417836874586,
75.117374150089));
#142698=CARTESIAN_POINT('Ctrl Pts',(111.490448059869,-0.253375583460886,
74.924836266052));
#142699=CARTESIAN_POINT('Ctrl Pts',(112.150874686469,-0.253183225873986,
74.806307851534));
#142700=CARTESIAN_POINT('Ctrl Pts',(94.2748484062691,0.273581135887814,
77.974569798547));
#142701=CARTESIAN_POINT('Ctrl Pts',(96.4658642089691,0.275086851522514,
77.588391617785));
#142702=CARTESIAN_POINT('Ctrl Pts',(100.749136226669,0.279152495519414,
76.834104579055));
#142703=CARTESIAN_POINT('Ctrl Pts',(105.559122588369,0.286383475540014,
75.986316878894));
#142704=CARTESIAN_POINT('Ctrl Pts',(108.693165039069,0.291717408504714,
75.43229368399));
#142705=CARTESIAN_POINT('Ctrl Pts',(110.377550127869,0.295689160759514,
75.136153730842));
#142706=CARTESIAN_POINT('Ctrl Pts',(111.475979202669,0.295825796724414,
74.943355140899));
#142707=CARTESIAN_POINT('Ctrl Pts',(112.131988786069,0.299193462052214,
74.825561946835));
#142708=CARTESIAN_POINT('Ctrl Pts',(94.2651023215691,1.30788160650201,77.911176272393));
#142709=CARTESIAN_POINT('Ctrl Pts',(96.4454408924691,1.31912219392701,77.525812822656));
#142710=CARTESIAN_POINT('Ctrl Pts',(100.708094210469,1.34342458471501,76.773429707576));
#142711=CARTESIAN_POINT('Ctrl Pts',(105.493968389769,1.37592947659601,75.928679146587));
#142712=CARTESIAN_POINT('Ctrl Pts',(108.613695916869,1.39843192417101,75.376791007982));
#142713=CARTESIAN_POINT('Ctrl Pts',(110.287407697569,1.41239992444901,75.082153932159));
#142714=CARTESIAN_POINT('Ctrl Pts',(111.387010027669,1.41771395267601,74.889476340583));
#142715=CARTESIAN_POINT('Ctrl Pts',(112.033257179669,1.42573735113301,74.77315042647));
#142716=CARTESIAN_POINT('Ctrl Pts',(94.2215315361691,2.87400974300901,77.640261060409));
#142717=CARTESIAN_POINT('Ctrl Pts',(96.3708145483691,2.90124158064901,77.255561094568));
#142718=CARTESIAN_POINT('Ctrl Pts',(100.573127653869,2.95640021853601,76.505561640338));
#142719=CARTESIAN_POINT('Ctrl Pts',(105.290086356369,3.02238572421201,75.666090838628));
#142720=CARTESIAN_POINT('Ctrl Pts',(108.366745704269,3.06612655879001,75.118411963246));
#142721=CARTESIAN_POINT('Ctrl Pts',(110.013388461769,3.09171703117801,74.826511452526));
#142722=CARTESIAN_POINT('Ctrl Pts',(111.106033966669,3.10383133871601,74.634770306963));
#142723=CARTESIAN_POINT('Ctrl Pts',(111.734450365969,3.11621882693801,74.520728353414));
#142724=CARTESIAN_POINT('Ctrl Pts',(94.1596433975691,4.29694974764301,77.25757310543));
#142725=CARTESIAN_POINT('Ctrl Pts',(96.2671294098691,4.33699728228101,76.872950610942));
#142726=CARTESIAN_POINT('Ctrl Pts',(100.388073332769,4.41679216356601,76.124486113148));
#142727=CARTESIAN_POINT('Ctrl Pts',(105.012817018869,4.50905954978901,75.289931588994));
#142728=CARTESIAN_POINT('Ctrl Pts',(108.030893450169,4.56946366906201,74.746434441845));
#142729=CARTESIAN_POINT('Ctrl Pts',(109.642849346369,4.60376585045201,74.457264740274));
#142730=CARTESIAN_POINT('Ctrl Pts',(110.721584552469,4.62195018338701,74.266525899993));
#142731=CARTESIAN_POINT('Ctrl Pts',(111.330637817569,4.63685072964401,74.154803550323));
#142732=CARTESIAN_POINT('Ctrl Pts',(94.0472766649691,6.14488949419901,76.567167410036));
#142733=CARTESIAN_POINT('Ctrl Pts',(96.0854969155691,6.19932125964201,76.182430491435));
#142734=CARTESIAN_POINT('Ctrl Pts',(100.071511546369,6.30590152019101,75.436192040905));
#142735=CARTESIAN_POINT('Ctrl Pts',(104.544032878269,6.42467485629401,74.609669583592));
#142736=CARTESIAN_POINT('Ctrl Pts',(107.464659485969,6.50123979669401,74.073144756336));
#142737=CARTESIAN_POINT('Ctrl Pts',(109.020613419869,6.54339817072601,73.7885096808893));
#142738=CARTESIAN_POINT('Ctrl Pts',(110.072680623769,6.56809627052501,73.5995632178325));
#142739=CARTESIAN_POINT('Ctrl Pts',(110.653470886869,6.58429623151501,73.4915052484874));
#142740=CARTESIAN_POINT('Ctrl Pts',(93.8521515925691,8.31376415356201,75.380290328722));
#142741=CARTESIAN_POINT('Ctrl Pts',(95.7842092150691,8.37610151972701,74.996687931097));
#142742=CARTESIAN_POINT('Ctrl Pts',(99.5633457638691,8.49649192920001,74.256622096991));
#142743=CARTESIAN_POINT('Ctrl Pts',(103.803511437969,8.62652183262401,73.4457843236508));
#142744=CARTESIAN_POINT('Ctrl Pts',(106.574368969069,8.70918768300001,72.9222235065084));
#142745=CARTESIAN_POINT('Ctrl Pts',(108.046575652369,8.75337472812401,72.6458499975918));
#142746=CARTESIAN_POINT('Ctrl Pts',(109.052812137369,8.78167413182101,72.4603561642308));
#142747=CARTESIAN_POINT('Ctrl Pts',(109.595630513669,8.79651116265801,72.3582991515531));
#142748=CARTESIAN_POINT('Ctrl Pts',(93.4372496266691,11.3601266881,72.8749686355627));
#142749=CARTESIAN_POINT('Ctrl Pts',(95.1718644035691,11.41712605481,72.5027022603797));
#142750=CARTESIAN_POINT('Ctrl Pts',(98.5659481303691,11.52584716743,71.790923625058));
#142751=CARTESIAN_POINT('Ctrl Pts',(102.374754422069,11.63978356045,71.024735970194));
#142752=CARTESIAN_POINT('Ctrl Pts',(104.865797334769,11.71128589282,70.534131262146));
#142753=CARTESIAN_POINT('Ctrl Pts',(106.185002428269,11.74808513017,70.277403481005));
#142754=CARTESIAN_POINT('Ctrl Pts',(107.098214469969,11.77444777076,70.10142143118));
#142755=CARTESIAN_POINT('Ctrl Pts',(107.578338009969,11.78460067935,70.010906049077));
#142756=CARTESIAN_POINT('Ctrl Pts',(92.8846953388691,13.59339522532,69.569112430708));
#142757=CARTESIAN_POINT('Ctrl Pts',(94.3995479321691,13.62144836159,69.235119204506));
#142758=CARTESIAN_POINT('Ctrl Pts',(97.3641245763691,13.67740135604,68.599574211411));
#142759=CARTESIAN_POINT('Ctrl Pts',(100.691605767869,13.74147687714,67.919598503328));
#142760=CARTESIAN_POINT('Ctrl Pts',(102.867637880669,13.78402628147,67.4845182886));
#142761=CARTESIAN_POINT('Ctrl Pts',(104.018563300369,13.80621016716,67.257624514061));
#142762=CARTESIAN_POINT('Ctrl Pts',(104.818068993669,13.82296220744,67.099320022254));
#142763=CARTESIAN_POINT('Ctrl Pts',(105.237162196869,13.82954337535,67.020632040054));
#142764=CARTESIAN_POINT('Ctrl Pts',(92.2448326917691,14.79056917055,65.751520981076));
#142765=CARTESIAN_POINT('Ctrl Pts',(93.5247181401691,14.79470414109,65.492514703334));
#142766=CARTESIAN_POINT('Ctrl Pts',(96.0287650471691,14.80601682355,64.996314397124));
#142767=CARTESIAN_POINT('Ctrl Pts',(98.8382401202691,14.82558254573,64.452331124048));
#142768=CARTESIAN_POINT('Ctrl Pts',(100.673199852269,14.84110198079,64.097444414381));
#142769=CARTESIAN_POINT('Ctrl Pts',(101.644468893269,14.84982950274,63.909933430294));
#142770=CARTESIAN_POINT('Ctrl Pts',(102.315422239769,14.85651834918,63.778622292892));
#142771=CARTESIAN_POINT('Ctrl Pts',(102.672955266469,14.85994328065,63.710263579365));
#142772=CARTESIAN_POINT('Ctrl Pts',(91.9040896551691,15.00296837733,63.719016359691));
#142773=CARTESIAN_POINT('Ctrl Pts',(93.0606367533691,15.00269997783,63.505997650065));
#142774=CARTESIAN_POINT('Ctrl Pts',(95.3224849385691,15.0032855081,63.09305060872));
#142775=CARTESIAN_POINT('Ctrl Pts',(97.8588083377691,15.00640812609,62.62492914454));
#142776=CARTESIAN_POINT('Ctrl Pts',(99.5137844899691,15.00944819208,62.31209564356));
#142777=CARTESIAN_POINT('Ctrl Pts',(100.390759595169,15.01129518319,62.1441843822));
#142778=CARTESIAN_POINT('Ctrl Pts',(100.993269605169,15.01273048873,62.02638756854));
#142779=CARTESIAN_POINT('Ctrl Pts',(101.318214643569,15.01358600216,61.96239030853));
#142780=CARTESIAN_POINT('Ctrl Pts',(91.7279117369691,15.00086642868,62.66815051123));
#142781=CARTESIAN_POINT('Ctrl Pts',(92.8206402341691,15.00091537795,62.47805184071));
#142782=CARTESIAN_POINT('Ctrl Pts',(94.9571144835691,15.00012220898,62.10616698998));
#142783=CARTESIAN_POINT('Ctrl Pts',(97.3520297403691,14.99728712131,61.67404148758));
#142784=CARTESIAN_POINT('Ctrl Pts',(98.9140467094691,14.99466744079,61.3801702936));
#142785=CARTESIAN_POINT('Ctrl Pts',(99.7424527660691,14.99311784675,61.22073601459));
#142786=CARTESIAN_POINT('Ctrl Pts',(100.309713938069,14.99193533907,61.10855151957));
#142787=CARTESIAN_POINT('Ctrl Pts',(100.617428775669,14.99125742262,61.04642672594));
#142788=CARTESIAN_POINT('Origin',(57.8121127436691,0.499074165591614,68.674471503788));
#142789=CARTESIAN_POINT('',(88.0907987596691,-14.9986801145128,63.5496776718788));
#142790=CARTESIAN_POINT('Ctrl Pts',(88.0907987596691,-14.99868011451,63.549677671879));
#142791=CARTESIAN_POINT('Ctrl Pts',(89.3657116351038,-14.997869438043,63.3248649301893));
#142792=CARTESIAN_POINT('Ctrl Pts',(90.6406264262481,-14.9978694380615,
63.1000630530281));
#142793=CARTESIAN_POINT('Ctrl Pts',(91.9155434702571,-14.9991665204688,
62.8752787017783));
#142794=CARTESIAN_POINT('',(88.2224712981462,-14.9706103812352,64.2964297435509));
#142795=CARTESIAN_POINT('Origin',(88.0541760202691,0.499074165591714,63.341979795825));
#142796=CARTESIAN_POINT('',(86.2245100263342,-14.5670381546171,67.3623544040121));
#142797=CARTESIAN_POINT('Ctrl Pts',(86.2245100263343,-14.5670381546171,
67.3623544040121));
#142798=CARTESIAN_POINT('Ctrl Pts',(86.2554419271589,-14.5670466650294,
67.3569163665417));
#142799=CARTESIAN_POINT('Ctrl Pts',(86.2870207042859,-14.5672200014156,
67.3506752471842));
#142800=CARTESIAN_POINT('Ctrl Pts',(86.3191954228747,-14.5675775833023,
67.343555076842));
#142801=CARTESIAN_POINT('Ctrl Pts',(86.3720903212892,-14.5681654441572,
67.3318495918071));
#142802=CARTESIAN_POINT('Ctrl Pts',(86.4265983686621,-14.5692515099211,
67.3177684420538));
#142803=CARTESIAN_POINT('Ctrl Pts',(86.4824665885848,-14.570911942245,67.3009764873743));
#142804=CARTESIAN_POINT('Ctrl Pts',(86.5377339405401,-14.5725545164628,
67.284365131749));
#142805=CARTESIAN_POINT('Ctrl Pts',(86.5943325024795,-14.5747592405898,
67.2651006452783));
#142806=CARTESIAN_POINT('Ctrl Pts',(86.6519673512887,-14.5775977677942,
67.2428541575597));
#142807=CARTESIAN_POINT('Ctrl Pts',(86.708850881912,-14.5803992924359,67.2208976713098));
#142808=CARTESIAN_POINT('Ctrl Pts',(86.7667439050915,-14.5838182728098,
67.1960361291941));
#142809=CARTESIAN_POINT('Ctrl Pts',(86.8253125521276,-14.5879205216877,
67.1679535725664));
#142810=CARTESIAN_POINT('Ctrl Pts',(86.8831432720715,-14.5919710848816,
67.1402248379989));
#142811=CARTESIAN_POINT('Ctrl Pts',(86.9416326729376,-14.5966878749362,
67.1093554830591));
#142812=CARTESIAN_POINT('Ctrl Pts',(87.0004097878607,-14.602130222003,67.0750456413716));
#142813=CARTESIAN_POINT('Ctrl Pts',(87.004855976204,-14.6025419077436,67.0724502772002));
#142814=CARTESIAN_POINT('Ctrl Pts',(87.0093037872775,-14.6029577430099,
67.0698352291958));
#142815=CARTESIAN_POINT('Ctrl Pts',(87.0137530489033,-14.6033777523591,
67.0672003692174));
#142816=CARTESIAN_POINT('Ctrl Pts',(87.0673706317975,-14.6084392407573,
67.0354479493357));
#142817=CARTESIAN_POINT('Ctrl Pts',(87.1212027637474,-14.6141080608135,
67.000817354719));
#142818=CARTESIAN_POINT('Ctrl Pts',(87.1748912039063,-14.6203899220705,
66.9631099249675));
#142819=CARTESIAN_POINT('Ctrl Pts',(87.228031685852,-14.6266076690142,66.9257873470718));
#142820=CARTESIAN_POINT('Ctrl Pts',(87.2810314455855,-14.6334261169198,
66.8854503046114));
#142821=CARTESIAN_POINT('Ctrl Pts',(87.3334965537328,-14.6408362228309,
66.8419190364476));
#142822=CARTESIAN_POINT('Ctrl Pts',(87.3853068214865,-14.648153839908,66.7989311014396));
#142823=CARTESIAN_POINT('Ctrl Pts',(87.4365956948904,-14.656048538499,66.75282810209));
#142824=CARTESIAN_POINT('Ctrl Pts',(87.4869378782774,-14.6644957728132,
66.7034509629592));
#142825=CARTESIAN_POINT('Ctrl Pts',(87.529302299325,-14.6716043677747,66.6618986549041));
#142826=CARTESIAN_POINT('Ctrl Pts',(87.5709955263894,-14.6791040253077,
66.6180279110203));
#142827=CARTESIAN_POINT('Ctrl Pts',(87.6117384985287,-14.6869704165268,
66.5717523386305));
#142828=CARTESIAN_POINT('Ctrl Pts',(87.6121077818064,-14.6870417153688,
66.5713329093609));
#142829=CARTESIAN_POINT('Ctrl Pts',(87.6124769868582,-14.6871130442736,
66.5709132825869));
#142830=CARTESIAN_POINT('Ctrl Pts',(87.6128461134674,-14.6871844032196,
66.5704934582473));
#142831=CARTESIAN_POINT('Ctrl Pts',(87.6444349017475,-14.6932910955579,
66.5345661047386));
#142832=CARTESIAN_POINT('Ctrl Pts',(87.6754500449891,-14.6996181921391,
66.4971912644075));
#142833=CARTESIAN_POINT('Ctrl Pts',(87.7057467458941,-14.7061432798311,
66.4583601287152));
#142834=CARTESIAN_POINT('Ctrl Pts',(87.721072110393,-14.7094439477019,66.4387176828179));
#142835=CARTESIAN_POINT('Ctrl Pts',(87.7362136452609,-14.7127952215432,
66.4187025888031));
#142836=CARTESIAN_POINT('Ctrl Pts',(87.7511514388679,-14.7161936925683,
66.3983146178697));
#142837=CARTESIAN_POINT('Ctrl Pts',(87.7586203356714,-14.7178929280808,
66.3881206324029));
#142838=CARTESIAN_POINT('Ctrl Pts',(87.766038297027,-14.7196039590666,66.3778334269534));
#142839=CARTESIAN_POINT('Ctrl Pts',(87.7734027995865,-14.7213263313501,
66.367452998191));
#142840=CARTESIAN_POINT('Ctrl Pts',(87.7770850508662,-14.7221875174919,
66.3622627838098));
#142841=CARTESIAN_POINT('Ctrl Pts',(87.7807539374385,-14.723051538708,66.357049263553));
#142842=CARTESIAN_POINT('Ctrl Pts',(87.7844091396446,-14.7239183361676,
66.3518124403372));
#142843=CARTESIAN_POINT('Ctrl Pts',(87.7870489286653,-14.7245443377642,
66.3480304037633));
#142844=CARTESIAN_POINT('Ctrl Pts',(87.7890837516772,-14.7250289729097,
66.345100062789));
#142845=CARTESIAN_POINT('Ctrl Pts',(87.7918098054448,-14.7256815781967,
66.3411505749329));
#142846=CARTESIAN_POINT('Ctrl Pts',(87.7928584009643,-14.725932607354,66.339631376992));
#142847=CARTESIAN_POINT('Ctrl Pts',(87.7940089138699,-14.7262085113202,
66.3379611222576));
#142848=CARTESIAN_POINT('Ctrl Pts',(87.7953333722025,-14.7265269972584,
66.3360320656442));
#142849=CARTESIAN_POINT('Ctrl Pts',(87.8270421704474,-14.7341518549904,
66.289848606751));
#142850=CARTESIAN_POINT('Ctrl Pts',(87.8561396361996,-14.7415770020337,
66.244320185919));
#142851=CARTESIAN_POINT('Ctrl Pts',(87.8828760026715,-14.748749880654,66.1997346079998));
#142852=CARTESIAN_POINT('Ctrl Pts',(87.910460227642,-14.7561502242182,66.1537351408298));
#142853=CARTESIAN_POINT('Ctrl Pts',(87.9355316640307,-14.763282194667,66.1087389913815));
#142854=CARTESIAN_POINT('Ctrl Pts',(87.9583700286187,-14.7701074924571,
66.0650087511747));
#142855=CARTESIAN_POINT('Ctrl Pts',(87.9822638228765,-14.7772482078318,
66.0192576047507));
#142856=CARTESIAN_POINT('Ctrl Pts',(88.0037139084123,-14.7840533931963,
65.9748918859642));
#142857=CARTESIAN_POINT('Ctrl Pts',(88.0230383633048,-14.7904978943206,
65.9321581299024));
#142858=CARTESIAN_POINT('Ctrl Pts',(88.0318926560556,-14.7934507072152,
65.9125779042962));
#142859=CARTESIAN_POINT('Ctrl Pts',(88.0403006154473,-14.7963280359603,
65.8933395819523));
#142860=CARTESIAN_POINT('Ctrl Pts',(88.0482922250197,-14.7991285520152,
65.8744635085759));
#142861=CARTESIAN_POINT('Ctrl Pts',(88.065125839151,-14.805027589776,65.8347027404038));
#142862=CARTESIAN_POINT('Ctrl Pts',(88.0801135053758,-14.8105852644645,
65.7965526375944));
#142863=CARTESIAN_POINT('Ctrl Pts',(88.0935327480613,-14.815798128202,65.76019469969));
#142864=CARTESIAN_POINT('Ctrl Pts',(88.1075745036794,-14.8212528144604,
65.722150132586));
#142865=CARTESIAN_POINT('Ctrl Pts',(88.1198994082141,-14.8263301020729,
65.6860675199005));
#142866=CARTESIAN_POINT('Ctrl Pts',(88.1308005801532,-14.831034908916,65.6521039125264));
#142867=CARTESIAN_POINT('Ctrl Pts',(88.1419307746528,-14.8358385589768,
65.6174267642257));
#142868=CARTESIAN_POINT('Ctrl Pts',(88.1515771757746,-14.8402541052123,
65.5849580331557));
#142869=CARTESIAN_POINT('Ctrl Pts',(88.1600199398178,-14.8442931348452,
65.5548203474047));
#142870=CARTESIAN_POINT('Ctrl Pts',(88.168631899223,-14.848413107766,65.5240786939688));
#142871=CARTESIAN_POINT('Ctrl Pts',(88.1759918859795,-14.8521415135935,
65.495761910864));
#142872=CARTESIAN_POINT('Ctrl Pts',(88.1823584667009,-14.8554942316909,
65.4699627854301));
#142873=CARTESIAN_POINT('Ctrl Pts',(88.1847937175939,-14.8567766641453,
65.4600944831181));
#142874=CARTESIAN_POINT('Ctrl Pts',(88.1870831946187,-14.8580041512027,
65.4505941995436));
#142875=CARTESIAN_POINT('Ctrl Pts',(88.1892397344708,-14.8591776291228,
65.4414659667121));
#142876=CARTESIAN_POINT('Ctrl Pts',(88.192226482607,-14.8608028636333,65.4288236163428));
#142877=CARTESIAN_POINT('Ctrl Pts',(88.1949583819352,-14.8623245059375,
65.4168949795531));
#142878=CARTESIAN_POINT('Ctrl Pts',(88.1974665021121,-14.8637450227631,
65.405689057559));
#142879=CARTESIAN_POINT('Ctrl Pts',(88.1987205622005,-14.8644552811758,
65.400086096562));
#142880=CARTESIAN_POINT('Ctrl Pts',(88.1999186773672,-14.8651402523145,
65.3946638134873));
#142881=CARTESIAN_POINT('Ctrl Pts',(88.2010643297083,-14.8658002411051,
65.3894231368125));
#142882=CARTESIAN_POINT('Ctrl Pts',(88.2016371558788,-14.8661302355004,
65.3868027984751));
#142883=CARTESIAN_POINT('Ctrl Pts',(88.2021968663335,-14.8664539838941,
65.3842278616828));
#142884=CARTESIAN_POINT('Ctrl Pts',(88.2027438845188,-14.8667715226077,
65.3816984385093));
#142885=CARTESIAN_POINT('Ctrl Pts',(88.2030173936114,-14.8669302919645,
65.3804337269225));
#142886=CARTESIAN_POINT('Ctrl Pts',(88.203287729636,-14.8670875088745,65.379180393737));
#142887=CARTESIAN_POINT('Ctrl Pts',(88.2035549440709,-14.8672431778277,
65.3779384523255));
#142888=CARTESIAN_POINT('Ctrl Pts',(88.2036885512884,-14.8673210123043,
65.3773174816197));
#142889=CARTESIAN_POINT('Ctrl Pts',(88.2037365216033,-14.8673487925349,
65.3770956790665));
#142890=CARTESIAN_POINT('Ctrl Pts',(88.2038261467464,-14.8674010463921,
65.3766785694427));
#142891=CARTESIAN_POINT('Ctrl Pts',(88.2039157718895,-14.8674533002492,
65.3762614598189));
#142892=CARTESIAN_POINT('Ctrl Pts',(88.2040470524583,-14.8675300544217,
65.3756490465892));
#142893=CARTESIAN_POINT('Ctrl Pts',(88.2043472736409,-14.8677055452291,
65.3742468165999));
#142894=CARTESIAN_POINT('Ctrl Pts',(88.227475833264,-14.8812250762862,65.2662212614667));
#142895=CARTESIAN_POINT('Ctrl Pts',(88.2436194410596,-14.8941054177045,
65.1564485646021));
#142896=CARTESIAN_POINT('Ctrl Pts',(88.2523597375445,-14.9060423907878,
65.045853643057));
#142897=CARTESIAN_POINT('Ctrl Pts',(88.2545110024111,-14.9089804594049,
65.0186327164501));
#142898=CARTESIAN_POINT('Ctrl Pts',(88.2562138322223,-14.9118613774451,
64.9913618680356));
#142899=CARTESIAN_POINT('Ctrl Pts',(88.2574686769471,-14.9146825923509,
64.9640590854486));
#142900=CARTESIAN_POINT('Ctrl Pts',(88.2585275283017,-14.9170631635605,
64.9410207064748));
#142901=CARTESIAN_POINT('Ctrl Pts',(88.259267407385,-14.9194012251429,64.9179595883371));
#142902=CARTESIAN_POINT('Ctrl Pts',(88.2596886006513,-14.9216952433542,
64.8948864854724));
#142903=CARTESIAN_POINT('Ctrl Pts',(88.2598991972844,-14.9228422524599,
64.88334993404));
#142904=CARTESIAN_POINT('Ctrl Pts',(88.2600301224623,-14.9239782506498,
64.8718103864186));
#142905=CARTESIAN_POINT('Ctrl Pts',(88.2600814136634,-14.9251030462851,
64.8602691814297));
#142906=CARTESIAN_POINT('Ctrl Pts',(88.2601262934643,-14.9260872424659,
64.8501706270644));
#142907=CARTESIAN_POINT('Ctrl Pts',(88.2601102035016,-14.927062861686,64.8400708037766));
#142908=CARTESIAN_POINT('Ctrl Pts',(88.2600331691618,-14.9280297754665,
64.829970607531));
#142909=CARTESIAN_POINT('Ctrl Pts',(88.2600221642561,-14.9281679060066,
64.8285277223531));
#142910=CARTESIAN_POINT('Ctrl Pts',(88.2599973832409,-14.92843383089,64.825744595575));
#142911=CARTESIAN_POINT('Ctrl Pts',(88.2599964232447,-14.9284436337292,
64.8256419317284));
#142912=CARTESIAN_POINT('Ctrl Pts',(88.2599806488439,-14.9286047113654,
64.8239549868249));
#142913=CARTESIAN_POINT('Ctrl Pts',(88.2600688441228,-14.9290215173409,
64.8195787139235));
#142914=CARTESIAN_POINT('Ctrl Pts',(88.2602191362165,-14.9296883818484,
64.812510127624));
#142915=CARTESIAN_POINT('Ctrl Pts',(88.2603693339231,-14.9303548275483,
64.8054459805742));
#142916=CARTESIAN_POINT('Ctrl Pts',(88.260581556943,-14.931271041923,64.7956927273991));
#142917=CARTESIAN_POINT('Ctrl Pts',(88.2607625743269,-14.9324242352605,
64.7832444165503));
#142918=CARTESIAN_POINT('Ctrl Pts',(88.2609427967042,-14.9335723639107,
64.7708507771936));
#142919=CARTESIAN_POINT('Ctrl Pts',(88.2610920711133,-14.9349554320682,
64.7557854023437));
#142920=CARTESIAN_POINT('Ctrl Pts',(88.2610675057493,-14.9365532924553,
64.7380430085675));
#142921=CARTESIAN_POINT('Ctrl Pts',(88.2610452719137,-14.9379994979787,
64.7219845668633));
#142922=CARTESIAN_POINT('Ctrl Pts',(88.2608800214993,-14.9396215991874,
64.7037329239017));
#142923=CARTESIAN_POINT('Ctrl Pts',(88.2604296824915,-14.9413988229924,
64.6832882670058));
#142924=CARTESIAN_POINT('Ctrl Pts',(88.2599427492754,-14.9433204626641,
64.661182292702));
#142925=CARTESIAN_POINT('Ctrl Pts',(88.2591231165921,-14.9454236237161,
64.6365118554533));
#142926=CARTESIAN_POINT('Ctrl Pts',(88.2577455814398,-14.9476738742103,
64.6092883924997));
#142927=CARTESIAN_POINT('Ctrl Pts',(88.2563947050679,-14.9498805766806,
64.5825917722334));
#142928=CARTESIAN_POINT('Ctrl Pts',(88.2545072049435,-14.9522287813219,
64.5534394929417));
#142929=CARTESIAN_POINT('Ctrl Pts',(88.2518258964013,-14.9546770210727,
64.5218605477094));
#142930=CARTESIAN_POINT('Ctrl Pts',(88.2490652167,-14.9571977327618,64.4893468135673));
#142931=CARTESIAN_POINT('Ctrl Pts',(88.2454633288124,-14.9598246464015,
64.4542597760387));
#142932=CARTESIAN_POINT('Ctrl Pts',(88.2406896430595,-14.9625011974931,
64.4166609082583));
#142933=CARTESIAN_POINT('Ctrl Pts',(88.2362931783414,-14.9649662450579,
64.3820331375601));
#142934=CARTESIAN_POINT('Ctrl Pts',(88.2309022872888,-14.9674733471412,
64.345274641701));
#142935=CARTESIAN_POINT('Ctrl Pts',(88.2242201005126,-14.9699684545082,
64.3064647140518));
#142936=CARTESIAN_POINT('Ctrl Pts',(88.2236467622574,-14.9701825371959,
64.3031347837538));
#142937=CARTESIAN_POINT('Ctrl Pts',(88.2230638949306,-14.9703965253424,
64.2997897727192));
#142938=CARTESIAN_POINT('Ctrl Pts',(88.2224712981462,-14.9706103812352,
64.2964297435509));
#142939=CARTESIAN_POINT('',(69.482779745793,-14.5670748341037,70.3143821603081));
#142940=CARTESIAN_POINT('',(68.9413550361439,-14.5670748341037,70.4098499446415));
#142941=CARTESIAN_POINT('',(69.0831878262454,-14.4277621758119,70.9275690132791));
#142942=CARTESIAN_POINT('Ctrl Pts',(69.0831878262454,-14.4277621758119,
70.9275690132791));
#142943=CARTESIAN_POINT('Ctrl Pts',(69.0731820518308,-14.4438343998325,
70.8709989238709));
#142944=CARTESIAN_POINT('Ctrl Pts',(69.071801460729,-14.458723937518,70.8159229870168));
#142945=CARTESIAN_POINT('Ctrl Pts',(69.0785459095066,-14.4728469146059,
70.7612092128021));
#142946=CARTESIAN_POINT('Ctrl Pts',(69.0838687136473,-14.4839929464615,
70.7180284112939));
#142947=CARTESIAN_POINT('Ctrl Pts',(69.094251884068,-14.4946539059933,70.6750710969902));
#142948=CARTESIAN_POINT('Ctrl Pts',(69.1093808572375,-14.5044009701503,
70.634246903647));
#142949=CARTESIAN_POINT('Ctrl Pts',(69.1134215889724,-14.5070042711821,
70.6233433471565));
#142950=CARTESIAN_POINT('Ctrl Pts',(69.1178008736704,-14.5095426677788,
70.6125920261805));
#142951=CARTESIAN_POINT('Ctrl Pts',(69.1225127424941,-14.5120085718611,
70.6020294622628));
#142952=CARTESIAN_POINT('Ctrl Pts',(69.1448664004014,-14.5237071098194,
70.5519194211572));
#142953=CARTESIAN_POINT('Ctrl Pts',(69.1747054265118,-14.5337740168253,
70.5060577501982));
#142954=CARTESIAN_POINT('Ctrl Pts',(69.2107935956292,-14.5419633333216,
70.4662869693077));
#142955=CARTESIAN_POINT('Ctrl Pts',(69.2468817647466,-14.550152649818,70.4265161884173));
#142956=CARTESIAN_POINT('Ctrl Pts',(69.2892192207947,-14.5564675938574,
70.3928371138276));
#142957=CARTESIAN_POINT('Ctrl Pts',(69.3348500498842,-14.560698920749,70.3671498835826));
#142958=CARTESIAN_POINT('Ctrl Pts',(69.3747126952468,-14.5643953664779,
70.3447097708335));
#142959=CARTESIAN_POINT('Ctrl Pts',(69.4170887498322,-14.5665026120276,
70.3283689348563));
#142960=CARTESIAN_POINT('Ctrl Pts',(69.4627495397367,-14.5669736346079,
70.3183391465774));
#142961=CARTESIAN_POINT('Ctrl Pts',(69.4693567235523,-14.5670417922717,
70.3168878213829));
#142962=CARTESIAN_POINT('Ctrl Pts',(69.4760326811777,-14.5670756030821,
70.3155686193061));
#142963=CARTESIAN_POINT('Ctrl Pts',(69.4827797457826,-14.5670748341036,
70.3143821603099));
#142964=CARTESIAN_POINT('',(69.9613703778984,-11.9506558356043,75.9079897530419));
#142965=CARTESIAN_POINT('Origin',(68.3580209600691,0.499074165591714,66.814943349163));
#142966=CARTESIAN_POINT('',(70.5465863733413,-11.5358762249694,76.3475293475958));
#142967=CARTESIAN_POINT('Ctrl Pts',(70.5465865011915,-11.5358771324844,
76.3475300730731));
#142968=CARTESIAN_POINT('Ctrl Pts',(70.5313040392169,-11.5358611953978,
76.3502432234202));
#142969=CARTESIAN_POINT('Ctrl Pts',(70.5161018493598,-11.5364564485583,
76.352177065221));
#142970=CARTESIAN_POINT('Ctrl Pts',(70.5009632632138,-11.5376480599897,
76.3533544936938));
#142971=CARTESIAN_POINT('Ctrl Pts',(70.4995823522497,-11.537756756355,76.3534618963186));
#142972=CARTESIAN_POINT('Ctrl Pts',(70.4982019647776,-11.5378704373222,
76.3535629778345));
#142973=CARTESIAN_POINT('Ctrl Pts',(70.4968220853222,-11.5379891051123,
76.3536577391986));
#142974=CARTESIAN_POINT('Ctrl Pts',(70.4816890378852,-11.5392905269794,
76.3546969808609));
#142975=CARTESIAN_POINT('Ctrl Pts',(70.466616928596,-11.5411889943885,76.3549795204622));
#142976=CARTESIAN_POINT('Ctrl Pts',(70.4515726992923,-11.5436640619456,
76.354532064538));
#142977=CARTESIAN_POINT('Ctrl Pts',(70.4361732910351,-11.5461975633306,
76.3540740446344));
#142978=CARTESIAN_POINT('Ctrl Pts',(70.4208024273472,-11.5493354437837,
76.3528510340008));
#142979=CARTESIAN_POINT('Ctrl Pts',(70.4054325685759,-11.5530882736582,
76.3508492610654));
#142980=CARTESIAN_POINT('Ctrl Pts',(70.4013883728073,-11.554075737429,76.3503225443431));
#142981=CARTESIAN_POINT('Ctrl Pts',(70.3973443191322,-11.5551059379066,
76.3497416918571));
#142982=CARTESIAN_POINT('Ctrl Pts',(70.3933000862645,-11.5561794006954,
76.3491059929155));
#142983=CARTESIAN_POINT('Ctrl Pts',(70.372629786894,-11.5616659287797,76.3458569002287));
#142984=CARTESIAN_POINT('Ctrl Pts',(70.3519362330081,-11.5682204805058,
76.3412564835926));
#142985=CARTESIAN_POINT('Ctrl Pts',(70.3314707729455,-11.5758188287446,
76.3352764690793));
#142986=CARTESIAN_POINT('Ctrl Pts',(70.3270314425513,-11.5774670486321,
76.3339792952017));
#142987=CARTESIAN_POINT('Ctrl Pts',(70.3226029447382,-11.5791642675993,
76.3326173286124));
#142988=CARTESIAN_POINT('Ctrl Pts',(70.3181880005322,-11.5809100473327,
76.3311904857735));
#142989=CARTESIAN_POINT('Ctrl Pts',(70.297673760895,-11.5890218924964,76.3245605954383));
#142990=CARTESIAN_POINT('Ctrl Pts',(70.2774513760942,-11.5981849144579,
76.3165268005299));
#142991=CARTESIAN_POINT('Ctrl Pts',(70.2577328684847,-11.6082908082475,
76.3071659887023));
#142992=CARTESIAN_POINT('Ctrl Pts',(70.2531703837878,-11.6106291183609,
76.3050000762733));
#142993=CARTESIAN_POINT('Ctrl Pts',(70.2486349115508,-11.6130177658129,
76.302763286082));
#142994=CARTESIAN_POINT('Ctrl Pts',(70.2441291287376,-11.6154551612671,
76.3004568668291));
#142995=CARTESIAN_POINT('Ctrl Pts',(70.2195057584611,-11.6287751310191,
76.2878526607157));
#142996=CARTESIAN_POINT('Ctrl Pts',(70.1957811556634,-11.64359859179,76.2731068200489));
#142997=CARTESIAN_POINT('Ctrl Pts',(70.1732440005013,-11.6597303060056,
76.2563626943157));
#142998=CARTESIAN_POINT('Ctrl Pts',(70.1671237010594,-11.6641111127578,
76.2518155781139));
#142999=CARTESIAN_POINT('Ctrl Pts',(70.1610912386706,-11.6685884171355,
76.2471209830158));
#143000=CARTESIAN_POINT('Ctrl Pts',(70.1551530632265,-11.6731583054232,
76.2422815649606));
#143001=CARTESIAN_POINT('Ctrl Pts',(70.1407842417427,-11.6842162321592,
76.2305714471351));
#143002=CARTESIAN_POINT('Ctrl Pts',(70.1269668641474,-11.6958163819125,
76.2180134052578));
#143003=CARTESIAN_POINT('Ctrl Pts',(70.1137575779468,-11.7079088255401,
76.2046488610965));
#143004=CARTESIAN_POINT('Ctrl Pts',(70.0987377197503,-11.7216587576543,
76.1894524640228));
#143005=CARTESIAN_POINT('Ctrl Pts',(70.0845018742824,-11.7360358510045,
76.1732255334069));
#143006=CARTESIAN_POINT('Ctrl Pts',(70.0712089922545,-11.750870538935,76.1561403878423));
#143007=CARTESIAN_POINT('Ctrl Pts',(70.0574121206845,-11.7662676728092,
76.1384074719393));
#143008=CARTESIAN_POINT('Ctrl Pts',(70.0446317261883,-11.7821570931785,
76.1197506601893));
#143009=CARTESIAN_POINT('Ctrl Pts',(70.0330087939373,-11.7983289080146,
76.1003981507878));
#143010=CARTESIAN_POINT('Ctrl Pts',(70.0320519553556,-11.7996602257954,
76.0988049876128));
#143011=CARTESIAN_POINT('Ctrl Pts',(70.03110293782,-11.8009934499662,76.0972071254132));
#143012=CARTESIAN_POINT('Ctrl Pts',(70.0301618072275,-11.8023284599218,
76.0956046994724));
#143013=CARTESIAN_POINT('Ctrl Pts',(70.025118225905,-11.8094828668982,76.0870171924787));
#143014=CARTESIAN_POINT('Ctrl Pts',(70.0203012914773,-11.8166885762045,
76.0782985593257));
#143015=CARTESIAN_POINT('Ctrl Pts',(70.0157173732272,-11.8239292805152,
76.0694689672843));
#143016=CARTESIAN_POINT('Ctrl Pts',(70.0071740977884,-11.8374241396995,
76.0530128193545));
#143017=CARTESIAN_POINT('Ctrl Pts',(69.9994952539932,-11.8510449978951,
76.0361560556408));
#143018=CARTESIAN_POINT('Ctrl Pts',(69.9926445641082,-11.8648198974923,
76.0188632102975));
#143019=CARTESIAN_POINT('Ctrl Pts',(69.9858613355384,-11.8784591504816,
76.0017406540947));
#143020=CARTESIAN_POINT('Ctrl Pts',(69.9798896952674,-11.8922500478019,
75.9841898344588));
#143021=CARTESIAN_POINT('Ctrl Pts',(69.9747409884352,-11.9062242291212,
75.9661574739964));
#143022=CARTESIAN_POINT('Ctrl Pts',(69.969592281603,-11.9201984104406,75.948125113534));
#143023=CARTESIAN_POINT('Ctrl Pts',(69.9652659732438,-11.9343565179746,
75.9296105175509));
#143024=CARTESIAN_POINT('Ctrl Pts',(69.9618267835144,-11.9487252623603,
75.9105519754272));
#143025=CARTESIAN_POINT('Ctrl Pts',(69.9616728578679,-11.9493683551943,
75.9096989842725));
#143026=CARTESIAN_POINT('Ctrl Pts',(69.961520718983,-11.9500118681541,75.9088449031724));
#143027=CARTESIAN_POINT('Ctrl Pts',(69.961370373637,-11.9506558025134,75.9079897288741));
#143028=CARTESIAN_POINT('',(80.8778403488691,-11.53587675694,74.525850965447));
#143029=CARTESIAN_POINT('Ctrl Pts',(63.5269668554091,-14.97035104563,67.431942152481));
#143030=CARTESIAN_POINT('Ctrl Pts',(63.4204723176291,-14.97157761715,67.728904162768));
#143031=CARTESIAN_POINT('Ctrl Pts',(63.2791491661791,-14.96118285201,68.415759542565));
#143032=CARTESIAN_POINT('Ctrl Pts',(63.3636705257291,-14.90657053402,69.163225313652));
#143033=CARTESIAN_POINT('Ctrl Pts',(63.4869154152091,-14.86162731758,69.560641054351));
#143034=CARTESIAN_POINT('Ctrl Pts',(63.5016556949791,-14.85641574646,69.604876045245));
#143035=CARTESIAN_POINT('Ctrl Pts',(64.6260804730591,-15.20847950524,67.822908934237));
#143036=CARTESIAN_POINT('Ctrl Pts',(64.5533052413691,-15.20970453555,68.02494034063));
#143037=CARTESIAN_POINT('Ctrl Pts',(64.4577204629591,-15.19922013264,68.498512102653));
#143038=CARTESIAN_POINT('Ctrl Pts',(64.5278151508691,-15.14370900441,69.017398832301));
#143039=CARTESIAN_POINT('Ctrl Pts',(64.6218784967391,-15.09809367435,69.289035305194));
#143040=CARTESIAN_POINT('Ctrl Pts',(64.6330779166991,-15.09280488929,69.319208806332));
#143041=CARTESIAN_POINT('Ctrl Pts',(65.4174681368491,-14.3663713944,68.109543058174));
#143042=CARTESIAN_POINT('Ctrl Pts',(65.374277542859,-14.367601875,68.229634464589));
#143043=CARTESIAN_POINT('Ctrl Pts',(65.3173415915791,-14.35743446355,68.509807748111));
#143044=CARTESIAN_POINT('Ctrl Pts',(65.3563485675191,-14.30510185249,68.8160557029299));
#143045=CARTESIAN_POINT('Ctrl Pts',(65.4101046346091,-14.2618633586,68.977254924068));
#143046=CARTESIAN_POINT('Ctrl Pts',(65.4165145100791,-14.25684762985,68.995173914932));
#143047=CARTESIAN_POINT('Ctrl Pts',(65.1907448967991,-13.19994060407,68.034548919224));
#143048=CARTESIAN_POINT('Ctrl Pts',(65.1464477785891,-13.20117863405,68.159243937098));
#143049=CARTESIAN_POINT('Ctrl Pts',(65.0863781932991,-13.19145029757,68.439507002547));
#143050=CARTESIAN_POINT('Ctrl Pts',(65.1055421371491,-13.14352035198,68.739930520519));
#143051=CARTESIAN_POINT('Ctrl Pts',(65.1440468058491,-13.10357408963,68.905167920781));
#143052=CARTESIAN_POINT('Ctrl Pts',(65.148717761429,-13.0989365799,68.923639577176));
#143053=CARTESIAN_POINT('',(65.1554522360012,-13.4300820896322,68.8079743462767));
#143054=CARTESIAN_POINT('Origin',(63.6782406040291,-13.4300822103766,69.0684425118754));
#143055=CARTESIAN_POINT('',(65.176702388046,-13.4988189934219,68.1867892363913));
#143056=CARTESIAN_POINT('Ctrl Pts',(65.1766881521841,-13.49881898955,68.1867857093006));
#143057=CARTESIAN_POINT('Ctrl Pts',(65.1631764280226,-13.4974095391694,
68.2413218051627));
#143058=CARTESIAN_POINT('Ctrl Pts',(65.1528655627841,-13.4948284037889,
68.2960765161634));
#143059=CARTESIAN_POINT('Ctrl Pts',(65.1456380345049,-13.4910755834085,
68.3506775411135));
#143060=CARTESIAN_POINT('Ctrl Pts',(65.1383292863499,-13.4872805904355,
68.4058921490608));
#143061=CARTESIAN_POINT('Ctrl Pts',(65.1341731466497,-13.4822874307076,
68.4609493248272));
#143062=CARTESIAN_POINT('Ctrl Pts',(65.1330085931394,-13.4760961042247,
68.5155010552506));
#143063=CARTESIAN_POINT('Ctrl Pts',(65.1318220968064,-13.469788119144,68.5710806636891));
#143064=CARTESIAN_POINT('Ctrl Pts',(65.1337405720278,-13.4622363895776,
68.6261353347979));
#143065=CARTESIAN_POINT('Ctrl Pts',(65.1385592353595,-13.4534409155254,
68.680339376681));
#143066=CARTESIAN_POINT('Ctrl Pts',(65.1423934985484,-13.4464422604907,
68.7234701264704));
#143067=CARTESIAN_POINT('Ctrl Pts',(65.1480632663611,-13.4386561212723,
68.7660631216691));
#143068=CARTESIAN_POINT('Ctrl Pts',(65.1554529407002,-13.43008249787,68.8079742555258));
#143069=CARTESIAN_POINT('Origin',(63.7199392236019,-13.4984347767573,67.8257809705908));
#143070=CARTESIAN_POINT('Ctrl Pts',(66.3247580495291,-14.30756367035,64.653048442206));
#143071=CARTESIAN_POINT('Ctrl Pts',(66.2370201501591,-14.30418007722,64.660179387221));
#143072=CARTESIAN_POINT('Ctrl Pts',(65.8957020926591,-14.29548166727,64.699341304182));
#143073=CARTESIAN_POINT('Ctrl Pts',(65.2897313547191,-14.31367841804,64.848477924246));
#143074=CARTESIAN_POINT('Ctrl Pts',(64.4888593299491,-14.40595071535,65.229365043181));
#143075=CARTESIAN_POINT('Ctrl Pts',(63.6868754779191,-14.55587601027,65.891174774896));
#143076=CARTESIAN_POINT('Ctrl Pts',(63.0361776061691,-14.69164668395,66.864705767423));
#143077=CARTESIAN_POINT('Ctrl Pts',(62.8000900869391,-14.70223108065,67.6910995312599));
#143078=CARTESIAN_POINT('Ctrl Pts',(62.7500345788591,-14.67447645787,68.1072094165649));
#143079=CARTESIAN_POINT('Ctrl Pts',(62.7478962467391,-14.67314451722,68.126114759757));
#143080=CARTESIAN_POINT('Ctrl Pts',(66.3548790151891,-15.30077409373,65.9656697779481));
#143081=CARTESIAN_POINT('Ctrl Pts',(66.3133354429391,-15.29804521015,65.97128019847));
#143082=CARTESIAN_POINT('Ctrl Pts',(66.1545084345491,-15.29119071457,65.99560282881));
#143083=CARTESIAN_POINT('Ctrl Pts',(65.8756710738591,-15.30514064789,66.049701459109));
#143084=CARTESIAN_POINT('Ctrl Pts',(65.4157972527891,-15.38496723526,66.200633846256));
#143085=CARTESIAN_POINT('Ctrl Pts',(64.8331603453191,-15.53410391348,66.579998802577));
#143086=CARTESIAN_POINT('Ctrl Pts',(64.2808612154091,-15.68485087802,67.30171533471));
#143087=CARTESIAN_POINT('Ctrl Pts',(64.0735921049591,-15.69860285338,68.005645199803));
#143088=CARTESIAN_POINT('Ctrl Pts',(64.0381426791891,-15.66572474596,68.369480153518));
#143089=CARTESIAN_POINT('Ctrl Pts',(64.0366658453191,-15.66414383633,68.3860269579031));
#143090=CARTESIAN_POINT('Ctrl Pts',(66.4883687499992,-14.4250384257,67.353342695188));
#143091=CARTESIAN_POINT('Ctrl Pts',(66.4727224083191,-14.42173227018,67.35612722381));
#143092=CARTESIAN_POINT('Ctrl Pts',(66.4137416085591,-14.41325195438,67.367025031932));
#143093=CARTESIAN_POINT('Ctrl Pts',(66.3111555793591,-14.43094640088,67.38243504645));
#143094=CARTESIAN_POINT('Ctrl Pts',(66.1137087919391,-14.52174664686,67.430437654035));
#143095=CARTESIAN_POINT('Ctrl Pts',(65.8332830717091,-14.67157866592,67.593155113558));
#143096=CARTESIAN_POINT('Ctrl Pts',(65.5518702100291,-14.8091207025,67.943351706207));
#143097=CARTESIAN_POINT('Ctrl Pts',(65.4451062657591,-14.82007975348,68.3024447707801));
#143098=CARTESIAN_POINT('Ctrl Pts',(65.4282236829991,-14.79171913615,68.489615271462));
#143099=CARTESIAN_POINT('Ctrl Pts',(65.4275278935291,-14.790357748,68.4981302604861));
#143100=CARTESIAN_POINT('Ctrl Pts',(66.5523790655891,-12.81429647004,67.019249257931));
#143101=CARTESIAN_POINT('Ctrl Pts',(66.5088000219191,-12.80992853736,67.021561612314));
#143102=CARTESIAN_POINT('Ctrl Pts',(66.3377354711091,-12.79845784797,67.0378320936299));
#143103=CARTESIAN_POINT('Ctrl Pts',(66.0323010044891,-12.82303958328,67.120998532188));
#143104=CARTESIAN_POINT('Ctrl Pts',(65.6789083917491,-12.93402369634,67.326374170474));
#143105=CARTESIAN_POINT('Ctrl Pts',(65.3922421976991,-13.0851346569,67.618765808573));
#143106=CARTESIAN_POINT('Ctrl Pts',(65.2034480648691,-13.19838884926,67.958796807735));
#143107=CARTESIAN_POINT('Ctrl Pts',(65.1387376786991,-13.20421087014,68.1971895314531));
#143108=CARTESIAN_POINT('Ctrl Pts',(65.1203415613491,-13.18415927923,68.3120587081699));
#143109=CARTESIAN_POINT('Ctrl Pts',(65.1195350329091,-13.18320165728,68.3172685415469));
#143110=CARTESIAN_POINT('',(66.3723478475728,-13.1050046819904,67.0702812784609));
#143111=CARTESIAN_POINT('Ctrl Pts',(66.3723470578469,-13.10500468188,67.0702768035153));
#143112=CARTESIAN_POINT('Ctrl Pts',(66.3391116532978,-13.1050449423269,
67.0761335665632));
#143113=CARTESIAN_POINT('Ctrl Pts',(66.3045689466359,-13.1065804249721,
67.083375400249));
#143114=CARTESIAN_POINT('Ctrl Pts',(66.2688718737599,-13.1096111298157,
67.0922994496814));
#143115=CARTESIAN_POINT('Ctrl Pts',(66.2340002184672,-13.1125717561663,
67.101017149777));
#143116=CARTESIAN_POINT('Ctrl Pts',(66.1980266690957,-13.116959256602,67.1113407048153));
#143117=CARTESIAN_POINT('Ctrl Pts',(66.1611425862324,-13.1227736311227,
67.1235543419997));
#143118=CARTESIAN_POINT('Ctrl Pts',(66.1254109251342,-13.1284063388857,
67.1353863711779));
#143119=CARTESIAN_POINT('Ctrl Pts',(66.0888246147659,-13.1353781499622,
67.1489927704856));
#143120=CARTESIAN_POINT('Ctrl Pts',(66.0516068828885,-13.1436890643524,
67.1646309082111));
#143121=CARTESIAN_POINT('Ctrl Pts',(66.0440858281265,-13.1453685552589,
67.1677911032115));
#143122=CARTESIAN_POINT('Ctrl Pts',(66.0365391564341,-13.1471027316143,
67.171034249684));
#143123=CARTESIAN_POINT('Ctrl Pts',(66.0289689707891,-13.1488915934185,
67.1743624337803));
#143124=CARTESIAN_POINT('Ctrl Pts',(65.9928233038006,-13.1574329431415,
67.190253646977));
#143125=CARTESIAN_POINT('Ctrl Pts',(65.9561376823215,-13.1672210194115,
67.2080846714309));
#143126=CARTESIAN_POINT('Ctrl Pts',(65.9191702216006,-13.1782558222285,
67.2280750892431));
#143127=CARTESIAN_POINT('Ctrl Pts',(65.8833564575203,-13.1889462461054,
67.2474416373758));
#143128=CARTESIAN_POINT('Ctrl Pts',(65.84727825624,-13.2008067940272,67.2688354021097));
#143129=CARTESIAN_POINT('Ctrl Pts',(65.8112155646009,-13.2138374659941,
67.2924385375834));
#143130=CARTESIAN_POINT('Ctrl Pts',(65.7892798381047,-13.2217635869611,
67.3067955337108));
#143131=CARTESIAN_POINT('Ctrl Pts',(65.7673507305799,-13.2301226399125,
67.321969602589));
#143132=CARTESIAN_POINT('Ctrl Pts',(65.7454995863913,-13.2389146248483,
67.3379971598794));
#143133=CARTESIAN_POINT('Ctrl Pts',(65.7296903107005,-13.2452756150335,
67.3495930776797));
#143134=CARTESIAN_POINT('Ctrl Pts',(65.7139219774182,-13.2518632236623,
67.3616356827555));
#143135=CARTESIAN_POINT('Ctrl Pts',(65.6982237003632,-13.2586774507346,
67.3741373222992));
#143136=CARTESIAN_POINT('Ctrl Pts',(65.6903745618356,-13.2620845642708,
67.3803881420711));
#143137=CARTESIAN_POINT('Ctrl Pts',(65.6825429382797,-13.2655483324178,
67.3867537216006));
#143138=CARTESIAN_POINT('Ctrl Pts',(65.6747326640873,-13.2690687551758,
67.3932354506086));
#143139=CARTESIAN_POINT('Ctrl Pts',(65.6708275269912,-13.2708289665547,
67.3964763151126));
#143140=CARTESIAN_POINT('Ctrl Pts',(65.6669277271924,-13.2726033415864,
67.3997462169384));
#143141=CARTESIAN_POINT('Ctrl Pts',(65.6630337500704,-13.2743918802709,
67.4030453243454));
#143142=CARTESIAN_POINT('Ctrl Pts',(65.660251867848,-13.2756696237743,67.4054022278293));
#143143=CARTESIAN_POINT('Ctrl Pts',(65.6580604087891,-13.2766808889237,
67.4072712987835));
#143144=CARTESIAN_POINT('Ctrl Pts',(65.6551995973018,-13.2780122901473,
67.4097290096595));
#143145=CARTESIAN_POINT('Ctrl Pts',(65.6540559493652,-13.2785445357248,
67.4107115126957));
#143146=CARTESIAN_POINT('Ctrl Pts',(65.6528056389096,-13.2791279425155,
67.4117884475048));
#143147=CARTESIAN_POINT('Ctrl Pts',(65.6513697753868,-13.2797999872823,
67.4130304286083));
#143148=CARTESIAN_POINT('Ctrl Pts',(65.618531420134,-13.2951697243408,67.4414346718029));
#143149=CARTESIAN_POINT('Ctrl Pts',(65.5878590939958,-13.3097312798685,
67.4704571260051));
#143150=CARTESIAN_POINT('Ctrl Pts',(65.5592488544451,-13.3234846538655,
67.499768352367));
#143151=CARTESIAN_POINT('Ctrl Pts',(65.5295341230282,-13.3377689737737,
67.5302111320333));
#143152=CARTESIAN_POINT('Ctrl Pts',(65.5020432606503,-13.3511815083625,
67.5609651215252));
#143153=CARTESIAN_POINT('Ctrl Pts',(65.4766259981956,-13.3637222576317,
67.5917070571682));
#143154=CARTESIAN_POINT('Ctrl Pts',(65.4506520266231,-13.3765376843756,
67.6231223271604));
#143155=CARTESIAN_POINT('Ctrl Pts',(65.4268428557283,-13.3884427185039,
67.6545249450618));
#143156=CARTESIAN_POINT('Ctrl Pts',(65.4050124114097,-13.3994373600167,
67.6856194723999));
#143157=CARTESIAN_POINT('Ctrl Pts',(65.3824046098077,-13.4108235082041,
67.7178212404772));
#143158=CARTESIAN_POINT('Ctrl Pts',(65.3619183401328,-13.4212332733158,
67.749692514182));
#143159=CARTESIAN_POINT('Ctrl Pts',(65.3433293485563,-13.4306666553519,
67.7809589504468));
#143160=CARTESIAN_POINT('Ctrl Pts',(65.331487643871,-13.4366759820976,67.8008765400204));
#143161=CARTESIAN_POINT('Ctrl Pts',(65.3204155466602,-13.4422890882589,
67.8205497791698));
#143162=CARTESIAN_POINT('Ctrl Pts',(65.3100532853308,-13.447505973836,67.8399185337666));
#143163=CARTESIAN_POINT('Ctrl Pts',(65.2930999158816,-13.4560411560468,
67.8716071432325));
#143164=CARTESIAN_POINT('Ctrl Pts',(65.278046340807,-13.4635157666288,67.9024779678514));
#143165=CARTESIAN_POINT('Ctrl Pts',(65.264630059606,-13.4699298055819,67.9323119524872));
#143166=CARTESIAN_POINT('Ctrl Pts',(65.2506946713848,-13.4765920185706,
67.9633002831475));
#143167=CARTESIAN_POINT('Ctrl Pts',(65.2385250554639,-13.4821100002037,
67.9931701882726));
#143168=CARTESIAN_POINT('Ctrl Pts',(65.227835380454,-13.4864837504812,68.0217317365142));
#143169=CARTESIAN_POINT('Ctrl Pts',(65.2169231989982,-13.4909485407229,
68.0508877956813));
#143170=CARTESIAN_POINT('Ctrl Pts',(65.2075526093426,-13.494220969315,68.0786809186596));
#143171=CARTESIAN_POINT('Ctrl Pts',(65.1994379493454,-13.4963010362577,
68.104960526297));
#143172=CARTESIAN_POINT('Ctrl Pts',(65.1911190497657,-13.4984334568423,
68.1319015709006));
#143173=CARTESIAN_POINT('Ctrl Pts',(65.1841195422163,-13.4993127388276,
68.1572524438131));
#143174=CARTESIAN_POINT('Ctrl Pts',(65.1781597320144,-13.4989388822135,
68.1808971743649));
#143175=CARTESIAN_POINT('Ctrl Pts',(65.1776619856803,-13.4989076587763,
68.18287191476));
#143176=CARTESIAN_POINT('Ctrl Pts',(65.1771715099249,-13.4988676945552,
68.1848347781111));
#143177=CARTESIAN_POINT('Ctrl Pts',(65.1766881521841,-13.49881898955,68.1867857093006));
#143178=CARTESIAN_POINT('Ctrl Pts',(65.9990563614061,-14.4574811117313,
64.9541310528021));
#143179=CARTESIAN_POINT('Ctrl Pts',(66.0069547419919,-14.4793092068606,
64.9989444984957));
#143180=CARTESIAN_POINT('Ctrl Pts',(66.0150536595875,-14.4988596768414,
65.044891079552));
#143181=CARTESIAN_POINT('Ctrl Pts',(66.0233037502849,-14.516005350927,65.0916919095426));
#143182=CARTESIAN_POINT('Ctrl Pts',(66.0320127944002,-14.5341048406751,
65.1410962746547));
#143183=CARTESIAN_POINT('Ctrl Pts',(66.0408901082891,-14.5495248096361,
65.1914514973418));
#143184=CARTESIAN_POINT('Ctrl Pts',(66.049879846746,-14.5621739529066,65.2424419490977));
#143185=CARTESIAN_POINT('Ctrl Pts',(66.0592376012889,-14.5753409186053,
65.2955198149165));
#143186=CARTESIAN_POINT('Ctrl Pts',(66.0687170259418,-14.5855064940319,
65.3492851484083));
#143187=CARTESIAN_POINT('Ctrl Pts',(66.0782602192334,-14.5926194563088,
65.4034105789931));
#143188=CARTESIAN_POINT('Ctrl Pts',(66.0887744064903,-14.6004561431542,
65.4630431249489));
#143189=CARTESIAN_POINT('Ctrl Pts',(66.0993658663221,-14.6045887182656,
65.523112024764));
#143190=CARTESIAN_POINT('Ctrl Pts',(66.1099657432096,-14.6049928480227,
65.5832278089851));
#143191=CARTESIAN_POINT('Ctrl Pts',(66.1155120833583,-14.6052043071859,
65.6146831354134));
#143192=CARTESIAN_POINT('Ctrl Pts',(66.1210608803727,-14.6043955326921,
65.6461521569814));
#143193=CARTESIAN_POINT('Ctrl Pts',(66.1266031485341,-14.6025651695425,
65.6775840264054));
#143194=CARTESIAN_POINT('Ctrl Pts',(66.1363407838677,-14.5993492643643,
65.7328090847001));
#143195=CARTESIAN_POINT('Ctrl Pts',(66.1460503077678,-14.5929783595983,
65.7878746692027));
#143196=CARTESIAN_POINT('Ctrl Pts',(66.155666603048,-14.5834926139621,65.8424115397955));
#143197=CARTESIAN_POINT('Ctrl Pts',(66.1657629405947,-14.5735333430542,
65.8996708728552));
#143198=CARTESIAN_POINT('Ctrl Pts',(66.1757564492557,-14.5601408008186,
65.956347045915));
#143199=CARTESIAN_POINT('Ctrl Pts',(66.1855765340643,-14.5434124527068,
66.0120397024279));
#143200=CARTESIAN_POINT('Ctrl Pts',(66.1956851946349,-14.5261925206731,
66.0693689589401));
#143201=CARTESIAN_POINT('Ctrl Pts',(66.2056100906302,-14.5054382282124,
66.1256560523008));
#143202=CARTESIAN_POINT('Ctrl Pts',(66.2152795913734,-14.481302712779,66.1804947231858));
#143203=CARTESIAN_POINT('Ctrl Pts',(66.2252319917202,-14.456461067016,66.2369378035087));
#143204=CARTESIAN_POINT('Ctrl Pts',(66.2349138675465,-14.4280375351101,
66.291846655123));
#143205=CARTESIAN_POINT('Ctrl Pts',(66.2442524298549,-14.3962441949578,
66.3448084647408));
#143206=CARTESIAN_POINT('Ctrl Pts',(66.2463349419034,-14.3891542370238,
66.356619020049));
#143207=CARTESIAN_POINT('Ctrl Pts',(66.2484004002693,-14.3818968727244,
66.3683328586023));
#143208=CARTESIAN_POINT('Ctrl Pts',(66.2504480296382,-14.3744747519765,
66.37994558372));
#143209=CARTESIAN_POINT('Ctrl Pts',(66.2597159703859,-14.3408808915069,
66.4325068772548));
#143210=CARTESIAN_POINT('Ctrl Pts',(66.2686129326532,-14.3039273404708,
66.4829645574844));
#143211=CARTESIAN_POINT('Ctrl Pts',(66.2770714108995,-14.263898617603,66.5309354107161));
#143212=CARTESIAN_POINT('Ctrl Pts',(66.2851736588896,-14.2255557112358,
66.5768859632702));
#143213=CARTESIAN_POINT('Ctrl Pts',(66.2928736045143,-14.1843911377398,
66.6205548920699));
#143214=CARTESIAN_POINT('Ctrl Pts',(66.3001161560663,-14.1406963638839,
66.6616296477246));
#143215=CARTESIAN_POINT('Ctrl Pts',(66.307148361561,-14.0982706211612,66.7015114656637));
#143216=CARTESIAN_POINT('Ctrl Pts',(66.3137493144063,-14.0534593449539,
66.7389473766632));
#143217=CARTESIAN_POINT('Ctrl Pts',(66.3198728148747,-14.0065712294518,
66.7736754547477));
#143218=CARTESIAN_POINT('Ctrl Pts',(66.3257509833222,-13.9615616401617,
66.8070121865545));
#143219=CARTESIAN_POINT('Ctrl Pts',(66.3311891229665,-13.9146383488563,
66.8378533321756));
#143220=CARTESIAN_POINT('Ctrl Pts',(66.3361511159024,-13.8661143232919,
66.8659942805906));
#143221=CARTESIAN_POINT('Ctrl Pts',(66.3373696432826,-13.8541981729645,
66.8729049144006));
#143222=CARTESIAN_POINT('Ctrl Pts',(66.3385594824833,-13.8421856810548,
66.8796528600556));
#143223=CARTESIAN_POINT('Ctrl Pts',(66.3397201532679,-13.8300818586723,
66.886235398542));
#143224=CARTESIAN_POINT('Ctrl Pts',(66.3450140367401,-13.7748756571299,
66.9162587196766));
#143225=CARTESIAN_POINT('Ctrl Pts',(66.3496974087145,-13.7178145654519,
66.942815204432));
#143226=CARTESIAN_POINT('Ctrl Pts',(66.3537436587053,-13.6592730960824,
66.9657431428049));
#143227=CARTESIAN_POINT('Ctrl Pts',(66.3573093551042,-13.6076843146192,
66.9859480405442));
#143228=CARTESIAN_POINT('Ctrl Pts',(66.3603800645005,-13.5549457672634,
67.0033339489328));
#143229=CARTESIAN_POINT('Ctrl Pts',(66.3629385113433,-13.5013556708403,
67.0177941584979));
#143230=CARTESIAN_POINT('Ctrl Pts',(66.3653860939825,-13.4500877736746,
67.0316277693041));
#143231=CARTESIAN_POINT('Ctrl Pts',(66.3673646518407,-13.3980405699007,
67.0427826803886));
#143232=CARTESIAN_POINT('Ctrl Pts',(66.3688628389521,-13.3455170266702,
67.0511848303657));
#143233=CARTESIAN_POINT('Ctrl Pts',(66.3702937991307,-13.2953503297189,
67.0592099574937));
#143234=CARTESIAN_POINT('Ctrl Pts',(66.371286385483,-13.2447495890845,67.0647230188068));
#143235=CARTESIAN_POINT('Ctrl Pts',(66.3718366772028,-13.1940136326873,
67.0676908984141));
#143236=CARTESIAN_POINT('Ctrl Pts',(66.3721582180026,-13.1643681202944,
67.0694250593116));
#143237=CARTESIAN_POINT('Ctrl Pts',(66.3723288762056,-13.1346770820982,
67.0702909089734));
#143238=CARTESIAN_POINT('Ctrl Pts',(66.3723491609777,-13.1050046822981,
67.0702887165938));
#143239=CARTESIAN_POINT('Origin',(58.0356083261291,-9.5,68.77323523472));
#143240=CARTESIAN_POINT('',(91.0790815025691,-12.28281717502,58.13146250234));
#143241=CARTESIAN_POINT('Ctrl Pts',(91.0790815025691,-12.28281717502,58.13146250234));
#143242=CARTESIAN_POINT('Ctrl Pts',(91.1199088515142,-12.6925940776003,
58.3651513297703));
#143243=CARTESIAN_POINT('Ctrl Pts',(91.1722707753266,-13.0779420821198,
58.6612655335377));
#143244=CARTESIAN_POINT('Ctrl Pts',(91.2926220959915,-13.7595612344036,
59.3421440579158));
#143245=CARTESIAN_POINT('Ctrl Pts',(91.3603889077048,-14.0537040594648,
59.7262617256362));
#143246=CARTESIAN_POINT('Ctrl Pts',(91.506357098809,-14.5281559853725,60.5547725075601));
#143247=CARTESIAN_POINT('Ctrl Pts',(91.5847883885152,-14.709288519388,61.000020579335));
#143248=CARTESIAN_POINT('Ctrl Pts',(91.7477452037583,-14.9479889262476,
61.9239589072862));
#143249=CARTESIAN_POINT('Ctrl Pts',(91.8320334198305,-15.0060365273816,
62.4015858279761));
#143250=CARTESIAN_POINT('Ctrl Pts',(91.9155434595542,-14.9991665213493,
62.8752786410684));
#143251=CARTESIAN_POINT('',(91.0413458950691,-11.874941516,57.91633991463));
#143252=CARTESIAN_POINT('Ctrl Pts',(91.0413458950691,-11.874941516,57.91633991463));
#143253=CARTESIAN_POINT('Ctrl Pts',(91.0543131272762,-12.024294137281,57.9879089911249));
#143254=CARTESIAN_POINT('Ctrl Pts',(91.0660084826674,-12.16018136282,58.0593039544405));
#143255=CARTESIAN_POINT('Ctrl Pts',(91.07908074693,-12.2828100865246,58.1314583314809));
#143256=CARTESIAN_POINT('',(87.2166270801612,-11.8742918211854,58.592003722724));
#143257=CARTESIAN_POINT('Ctrl Pts',(87.2164851556291,-11.87468271151,58.59119882454));
#143258=CARTESIAN_POINT('Ctrl Pts',(88.491322681793,-11.8750882864112,58.365587681618));
#143259=CARTESIAN_POINT('Ctrl Pts',(89.7663021731098,-11.8751032627281,
58.1407816630862));
#143260=CARTESIAN_POINT('Ctrl Pts',(91.0413458950691,-11.874941516,57.91633991463));
#143261=CARTESIAN_POINT('Origin',(88.0778048294691,-9.5,63.475985431442));
#143262=CARTESIAN_POINT('Origin',(88.0778048294691,-9.5,63.475985431442));
#143263=CARTESIAN_POINT('',(86.3881929029811,-11.4435878621033,59.6524812960673));
#143264=CARTESIAN_POINT('Ctrl Pts',(87.2166270533076,-11.8742914943215,
58.5920035689655));
#143265=CARTESIAN_POINT('Ctrl Pts',(87.1733550876063,-11.8742658138293,
58.5996210997768));
#143266=CARTESIAN_POINT('Ctrl Pts',(87.1305249711706,-11.8729960713397,
58.6098208361203));
#143267=CARTESIAN_POINT('Ctrl Pts',(87.0885121797564,-11.8704898997059,
58.6225169055592));
#143268=CARTESIAN_POINT('Ctrl Pts',(87.0465172644131,-11.8679847944259,
58.6352075729329));
#143269=CARTESIAN_POINT('Ctrl Pts',(87.0053394416954,-11.8642443312419,
58.6503923191013));
#143270=CARTESIAN_POINT('Ctrl Pts',(86.9653398723854,-11.859298361522,58.6679403817511));
#143271=CARTESIAN_POINT('Ctrl Pts',(86.9253413449803,-11.8543525206343,
58.6854879873107));
#143272=CARTESIAN_POINT('Ctrl Pts',(86.8865214517456,-11.8482012828593,
58.7053986005361));
#143273=CARTESIAN_POINT('Ctrl Pts',(86.8492206895109,-11.8408962348827,
58.7274988317037));
#143274=CARTESIAN_POINT('Ctrl Pts',(86.8119302495413,-11.833593208437,58.7495929470594));
#143275=CARTESIAN_POINT('Ctrl Pts',(86.77615850976,-11.8251370862027,58.7738752269925));
#143276=CARTESIAN_POINT('Ctrl Pts',(86.7422186640335,-11.8156002149462,
58.8001330226941));
#143277=CARTESIAN_POINT('Ctrl Pts',(86.7082697178207,-11.8060607865134,
58.8263978590496));
#143278=CARTESIAN_POINT('Ctrl Pts',(86.6761540216081,-11.7954401303729,
58.8546389828117));
#143279=CARTESIAN_POINT('Ctrl Pts',(86.6461520958714,-11.7838301429435,
58.8846081166276));
#143280=CARTESIAN_POINT('Ctrl Pts',(86.6176861844754,-11.7728145542652,
58.9130429149572));
#143281=CARTESIAN_POINT('Ctrl Pts',(86.5911231320854,-11.7609085815675,
58.943032806359));
#143282=CARTESIAN_POINT('Ctrl Pts',(86.5666708390468,-11.7482055380309,
58.9743400397999));
#143283=CARTESIAN_POINT('Ctrl Pts',(86.5406752356164,-11.7347007398667,
59.007623234294));
#143284=CARTESIAN_POINT('Ctrl Pts',(86.5170617786849,-11.7202932043829,
59.0424004060605));
#143285=CARTESIAN_POINT('Ctrl Pts',(86.4960387773943,-11.7051095247828,
59.0783644560062));
#143286=CARTESIAN_POINT('Ctrl Pts',(86.4750173510482,-11.6899269826728,
59.1143258116941));
#143287=CARTESIAN_POINT('Ctrl Pts',(86.4565862107747,-11.6739685704833,
59.1514734922184));
#143288=CARTESIAN_POINT('Ctrl Pts',(86.4409079191863,-11.6573746042409,
59.1894795581048));
#143289=CARTESIAN_POINT('Ctrl Pts',(86.425225638195,-11.6407764155988,59.2274952947838));
#143290=CARTESIAN_POINT('Ctrl Pts',(86.4122977726285,-11.6235425217402,
59.2663694576407));
#143291=CARTESIAN_POINT('Ctrl Pts',(86.4022383956474,-11.6058246270749,
59.3057587287828));
#143292=CARTESIAN_POINT('Ctrl Pts',(86.3921809072349,-11.5881100588044,
59.3451406049005));
#143293=CARTESIAN_POINT('Ctrl Pts',(86.3849909337562,-11.5699118565233,
59.3850369848708));
#143294=CARTESIAN_POINT('Ctrl Pts',(86.3807318812011,-11.5513902301268,
59.4250956854601));
#143295=CARTESIAN_POINT('Ctrl Pts',(86.37647211738,-11.5328655106001,59.4651610758927));
#143296=CARTESIAN_POINT('Ctrl Pts',(86.3751442993911,-11.5140174524455,
59.5053884234905));
#143297=CARTESIAN_POINT('Ctrl Pts',(86.3767601154266,-11.4950120983375,
59.5454225279031));
#143298=CARTESIAN_POINT('Ctrl Pts',(86.3782101629784,-11.4779565260503,
59.5813494860583));
#143299=CARTESIAN_POINT('Ctrl Pts',(86.3820301552334,-11.4607744513163,
59.6171205724333));
#143300=CARTESIAN_POINT('Ctrl Pts',(86.3881929029811,-11.4435878621033,
59.6524812960673));
#143301=CARTESIAN_POINT('',(87.1036278102967,-13.9987735363373,63.7099253475457));
#143302=CARTESIAN_POINT('Origin',(87.0929970764191,-9.5,63.649633609109));
#143303=CARTESIAN_POINT('Ctrl Pts',(88.0907987596691,-14.99868011451,63.549677671879));
#143304=CARTESIAN_POINT('Ctrl Pts',(87.8327127247742,-14.9994907916134,
63.5951963601042));
#143305=CARTESIAN_POINT('Ctrl Pts',(87.5759653099965,-14.8914956855539,
63.6389755291981));
#143306=CARTESIAN_POINT('Ctrl Pts',(87.2105814416028,-14.5207989635053,
63.6982800998973));
#143307=CARTESIAN_POINT('Ctrl Pts',(87.1040483163665,-14.2605452795666,
63.7134684546579));
#143308=CARTESIAN_POINT('Ctrl Pts',(87.1036271773116,-13.9987735308997,
63.7099254590822));
#143309=CARTESIAN_POINT('Origin',(88.0541760202691,0.499074165591714,63.341979795825));
#143310=CARTESIAN_POINT('',(87.2268050854822,-13.9725532728231,64.4084965381912));
#143311=CARTESIAN_POINT('Origin',(87.0693682672991,0.499074165591714,63.515627973491));
#143312=CARTESIAN_POINT('Origin',(88.2115792922668,-13.9725914352474,64.234869837276));
#143313=CARTESIAN_POINT('Ctrl Pts',(85.9869779804892,-14.45602459315,67.672990289305));
#143314=CARTESIAN_POINT('Ctrl Pts',(86.1188182448091,-14.45335775601,67.662512009987));
#143315=CARTESIAN_POINT('Ctrl Pts',(86.5288714744991,-14.45079478986,67.60303640583));
#143316=CARTESIAN_POINT('Ctrl Pts',(87.1981096901091,-14.47737661549,67.359429353844));
#143317=CARTESIAN_POINT('Ctrl Pts',(87.9232293938691,-14.55613194807,66.826118621937));
#143318=CARTESIAN_POINT('Ctrl Pts',(88.4877746877692,-14.66433129533,66.054781967478));
#143319=CARTESIAN_POINT('Ctrl Pts',(88.7930035000691,-14.7713702607,65.092548915634));
#143320=CARTESIAN_POINT('Ctrl Pts',(88.7694653550692,-14.8243760301,64.337245624157));
#143321=CARTESIAN_POINT('Ctrl Pts',(88.6750970702691,-14.84113316934,63.942676946827));
#143322=CARTESIAN_POINT('Ctrl Pts',(88.6595111695691,-14.84334740449,63.885082644327));
#143323=CARTESIAN_POINT('Ctrl Pts',(85.9335802203091,-15.01572702015,66.7387418852801));
#143324=CARTESIAN_POINT('Ctrl Pts',(86.0152075191491,-15.01321673433,66.731223622732));
#143325=CARTESIAN_POINT('Ctrl Pts',(86.2682166275592,-15.0109676354,66.693423484771));
#143326=CARTESIAN_POINT('Ctrl Pts',(86.6862036438991,-15.03579852014,66.553203088848));
#143327=CARTESIAN_POINT('Ctrl Pts',(87.1727929355791,-15.11147478167,66.234254228036));
#143328=CARTESIAN_POINT('Ctrl Pts',(87.5896609990691,-15.21882727978,65.731333854876));
#143329=CARTESIAN_POINT('Ctrl Pts',(87.8421542441691,-15.32805298848,65.053945148687));
#143330=CARTESIAN_POINT('Ctrl Pts',(87.8414001753692,-15.38310788666,64.498042625236));
#143331=CARTESIAN_POINT('Ctrl Pts',(87.7768598826691,-15.40041417173,64.2066844999171));
#143332=CARTESIAN_POINT('Ctrl Pts',(87.766043127269,-15.40269862144,64.164158809273));
#143333=CARTESIAN_POINT('Ctrl Pts',(85.8554993785191,-14.34158763438,65.885303472011));
#143334=CARTESIAN_POINT('Ctrl Pts',(85.9044684357291,-14.33888878869,65.880917669075));
#143335=CARTESIAN_POINT('Ctrl Pts',(86.0563563157591,-14.33626164914,65.858358908938));
#143336=CARTESIAN_POINT('Ctrl Pts',(86.3066718932891,-14.36320147278,65.772958420671));
#143337=CARTESIAN_POINT('Ctrl Pts',(86.5940361948891,-14.44258635333,65.580259831417));
#143338=CARTESIAN_POINT('Ctrl Pts',(86.8359877173291,-14.55095884767,65.281614918033));
#143339=CARTESIAN_POINT('Ctrl Pts',(86.9797906777992,-14.65755071071,64.885100969035));
#143340=CARTESIAN_POINT('Ctrl Pts',(86.9776694167192,-14.71013751451,64.562268729993));
#143341=CARTESIAN_POINT('Ctrl Pts',(86.9396893054491,-14.7267823752,64.393163885495));
#143342=CARTESIAN_POINT('Ctrl Pts',(86.9333411474091,-14.72898225425,64.368481564751));
#143343=CARTESIAN_POINT('Ctrl Pts',(85.8531929635192,-13.30094292267,66.210694673787));
#143344=CARTESIAN_POINT('Ctrl Pts',(85.9290760517791,-13.2979530039,66.205583603029));
#143345=CARTESIAN_POINT('Ctrl Pts',(86.1658664817091,-13.29474229664,66.172222829911));
#143346=CARTESIAN_POINT('Ctrl Pts',(86.5478136567391,-13.32493761335,66.022545122284));
#143347=CARTESIAN_POINT('Ctrl Pts',(86.9315779387592,-13.41004735564,65.705553711945));
#143348=CARTESIAN_POINT('Ctrl Pts',(87.1964183130791,-13.51999438146,65.284226038267));
#143349=CARTESIAN_POINT('Ctrl Pts',(87.3154153783191,-13.62252047174,64.803248481328));
#143350=CARTESIAN_POINT('Ctrl Pts',(87.2895346633291,-13.67129736704,64.447291703555));
#143351=CARTESIAN_POINT('Ctrl Pts',(87.2406750363991,-13.68692121071,64.26219383718));
#143352=CARTESIAN_POINT('Ctrl Pts',(87.2327457050291,-13.68899054109,64.235172662353));
#143353=CARTESIAN_POINT('',(86.0102737124181,-13.5950714519424,66.1461371018416));
#143354=CARTESIAN_POINT('Ctrl Pts',(86.0102754056894,-13.5950714520587,
66.1461466969166));
#143355=CARTESIAN_POINT('Ctrl Pts',(86.0492876851558,-13.5950562057199,
66.1392620846122));
#143356=CARTESIAN_POINT('Ctrl Pts',(86.0892387535854,-13.5958711067968,
66.1306186693381));
#143357=CARTESIAN_POINT('Ctrl Pts',(86.1299313365959,-13.5975161552896,
66.1199521500868));
#143358=CARTESIAN_POINT('Ctrl Pts',(86.1697969025363,-13.5991277705844,
66.1095024121958));
#143359=CARTESIAN_POINT('Ctrl Pts',(86.2103742594308,-13.6015361331266,
66.0971104528392));
#143360=CARTESIAN_POINT('Ctrl Pts',(86.2514298118022,-13.6047412429161,
66.0825351254452));
#143361=CARTESIAN_POINT('Ctrl Pts',(86.2911847028321,-13.6078448131536,
66.0684215520355));
#143362=CARTESIAN_POINT('Ctrl Pts',(86.3313879017758,-13.6116954475604,
66.0522602815009));
#143363=CARTESIAN_POINT('Ctrl Pts',(86.3717816078402,-13.6162931461365,
66.0338465287676));
#143364=CARTESIAN_POINT('Ctrl Pts',(86.4121185431954,-13.6208843829483,
66.0154586553582));
#143365=CARTESIAN_POINT('Ctrl Pts',(86.4526455344907,-13.6262205855055,
65.9948240255609));
#143366=CARTESIAN_POINT('Ctrl Pts',(86.493059073377,-13.632301753808,65.9717611584834));
#143367=CARTESIAN_POINT('Ctrl Pts',(86.5317954639478,-13.6381305556647,
65.949655392658));
#143368=CARTESIAN_POINT('Ctrl Pts',(86.5704272936403,-13.6446437746059,
65.9253183810991));
#143369=CARTESIAN_POINT('Ctrl Pts',(86.6086463440478,-13.6518414106316,
65.8986178782715));
#143370=CARTESIAN_POINT('Ctrl Pts',(86.6462018383928,-13.6589140818826,
65.8723809474148));
#143371=CARTESIAN_POINT('Ctrl Pts',(86.6833585620957,-13.6666476109382,
65.8438614184352));
#143372=CARTESIAN_POINT('Ctrl Pts',(86.7197870729016,-13.6750419977982,
65.8129673352123));
#143373=CARTESIAN_POINT('Ctrl Pts',(86.7553577534027,-13.683238710933,65.782800755811));
#143374=CARTESIAN_POINT('Ctrl Pts',(86.7902338105182,-13.6920655241485,
65.7503697580506));
#143375=CARTESIAN_POINT('Ctrl Pts',(86.8240766932061,-13.7015224374449,
65.7156270904934));
#143376=CARTESIAN_POINT('Ctrl Pts',(86.8332160850262,-13.7040763107902,
65.7062447085431));
#143377=CARTESIAN_POINT('Ctrl Pts',(86.8422799602235,-13.7066761366659,
65.6966939774646));
#143378=CARTESIAN_POINT('Ctrl Pts',(86.8512612876911,-13.7093219150721,
65.6869745180572));
#143379=CARTESIAN_POINT('Ctrl Pts',(86.8697546103514,-13.7147697994666,
65.6669613184994));
#143380=CARTESIAN_POINT('Ctrl Pts',(86.8878980994665,-13.7204125149521,
65.6462324301027));
#143381=CARTESIAN_POINT('Ctrl Pts',(86.9056284488882,-13.7262500615288,
65.6247880383187));
#143382=CARTESIAN_POINT('Ctrl Pts',(86.914493623599,-13.7291688348171,65.6140658424267));
#143383=CARTESIAN_POINT('Ctrl Pts',(86.923255526305,-13.7321363158782,65.6031647811458));
#143384=CARTESIAN_POINT('Ctrl Pts',(86.931905959028,-13.7351525047121,65.5920854172301));
#143385=CARTESIAN_POINT('Ctrl Pts',(86.9362311753895,-13.7366605991291,
65.5865457352722));
#143386=CARTESIAN_POINT('Ctrl Pts',(86.9405285254553,-13.7381808704892,
65.5809614786555));
#143387=CARTESIAN_POINT('Ctrl Pts',(86.94479697978,-13.7397133187925,65.5753327385516));
#143388=CARTESIAN_POINT('Ctrl Pts',(86.9473884578402,-13.740643703858,65.5719153993049));
#143389=CARTESIAN_POINT('Ctrl Pts',(86.9495048194128,-13.7414089232411,
65.5691004992296));
#143390=CARTESIAN_POINT('Ctrl Pts',(86.9519942293893,-13.7423179797889,
65.5657627451645));
#143391=CARTESIAN_POINT('Ctrl Pts',(86.9536051561832,-13.7429062410893,
65.5636028448244));
#143392=CARTESIAN_POINT('Ctrl Pts',(86.9553717945738,-13.7435547347487,
65.5612236041841));
#143393=CARTESIAN_POINT('Ctrl Pts',(86.957514624389,-13.744347194532,65.5583131708614));
#143394=CARTESIAN_POINT('Ctrl Pts',(86.9847172363177,-13.7544072449398,
65.5213660518397));
#143395=CARTESIAN_POINT('Ctrl Pts',(87.0095589313433,-13.764145285636,65.4840751543646));
#143396=CARTESIAN_POINT('Ctrl Pts',(87.0321894775652,-13.7735613166208,
65.4467565493519));
#143397=CARTESIAN_POINT('Ctrl Pts',(87.0553307906926,-13.7831898655431,
65.4085956708822));
#143398=CARTESIAN_POINT('Ctrl Pts',(87.0761605696567,-13.7924817053338,
65.3704059473313));
#143399=CARTESIAN_POINT('Ctrl Pts',(87.0948671719668,-13.8014368359929,
65.3324778916709));
#143400=CARTESIAN_POINT('Ctrl Pts',(87.114960647704,-13.8110558837302,65.2917379190378));
#143401=CARTESIAN_POINT('Ctrl Pts',(87.1326049450955,-13.8202864456207,
65.251300355813));
#143402=CARTESIAN_POINT('Ctrl Pts',(87.1480577281618,-13.8291285216646,
65.211465491273));
#143403=CARTESIAN_POINT('Ctrl Pts',(87.1633255765337,-13.8378647781534,
65.1721073595302));
#143404=CARTESIAN_POINT('Ctrl Pts',(87.1764547697631,-13.8462217917393,
65.1333371825646));
#143405=CARTESIAN_POINT('Ctrl Pts',(87.1877068794637,-13.8541995624225,
65.0953888662222));
#143406=CARTESIAN_POINT('Ctrl Pts',(87.1993786382646,-13.8624748652468,
65.0560252617927));
#143407=CARTESIAN_POINT('Ctrl Pts',(87.2090313008149,-13.870342109828,65.0175459071096));
#143408=CARTESIAN_POINT('Ctrl Pts',(87.2169608558396,-13.8778012961662,
64.9801544525308));
#143409=CARTESIAN_POINT('Ctrl Pts',(87.2245979934478,-13.8849854108275,
64.9441418789246));
#143410=CARTESIAN_POINT('Ctrl Pts',(87.2306372077812,-13.8917910081719,
64.9091377462617));
#143411=CARTESIAN_POINT('Ctrl Pts',(87.2353388130221,-13.8982180881996,
64.8752784912196));
#143412=CARTESIAN_POINT('Ctrl Pts',(87.2404731788812,-13.9052367506725,
64.8383026512263));
#143413=CARTESIAN_POINT('Ctrl Pts',(87.2440130153083,-13.9118040074304,
64.8026923280386));
#143414=CARTESIAN_POINT('Ctrl Pts',(87.2462835806719,-13.9179198584735,
64.7685728342865));
#143415=CARTESIAN_POINT('Ctrl Pts',(87.2486150854234,-13.9241998519917,
64.7335376121884));
#143416=CARTESIAN_POINT('Ctrl Pts',(87.2496087866808,-13.9300038842062,
64.700073851738));
#143417=CARTESIAN_POINT('Ctrl Pts',(87.2495938463983,-13.9353319551167,
64.6682673708162));
#143418=CARTESIAN_POINT('Ctrl Pts',(87.2495783399401,-13.940861938145,64.6352555542241));
#143419=CARTESIAN_POINT('Ctrl Pts',(87.2484768178698,-13.9458792023638,
64.6040285120549));
#143420=CARTESIAN_POINT('Ctrl Pts',(87.2466246838941,-13.9503837477732,
64.5746365608777));
#143421=CARTESIAN_POINT('Ctrl Pts',(87.2447359087654,-13.9549774075446,
64.5446631425953));
#143422=CARTESIAN_POINT('Ctrl Pts',(87.2420668685604,-13.9590378613946,
64.5165974609744));
#143423=CARTESIAN_POINT('Ctrl Pts',(87.2389334330773,-13.9625651093231,
64.4904556039545));
#143424=CARTESIAN_POINT('Ctrl Pts',(87.2357270569359,-13.9661744651449,
64.4637052122221));
#143425=CARTESIAN_POINT('Ctrl Pts',(87.2320346909611,-13.969225501994,64.4389685682266));
#143426=CARTESIAN_POINT('Ctrl Pts',(87.2281486846861,-13.9717182198705,
64.4162347826597));
#143427=CARTESIAN_POINT('Ctrl Pts',(87.2277032801709,-13.9720039290842,
64.4136290918749));
#143428=CARTESIAN_POINT('Ctrl Pts',(87.2272552806075,-13.9722823035597,
64.4110496898349));
#143429=CARTESIAN_POINT('Ctrl Pts',(87.2268050864046,-13.9725533432969,
64.4084965434475));
#143430=CARTESIAN_POINT('Ctrl Pts',(86.2245100214957,-14.5670381546648,
67.3623544046571));
#143431=CARTESIAN_POINT('Ctrl Pts',(86.21790608955,-14.5762309095507,67.3249068234169));
#143432=CARTESIAN_POINT('Ctrl Pts',(86.2112032324775,-14.5831956362181,
67.2868968861811));
#143433=CARTESIAN_POINT('Ctrl Pts',(86.2044540605054,-14.5878733629712,
67.248623365796));
#143434=CARTESIAN_POINT('Ctrl Pts',(86.197437632731,-14.5927363197972,67.2088342786954));
#143435=CARTESIAN_POINT('Ctrl Pts',(86.1903713000755,-14.595128429718,67.168761175206));
#143436=CARTESIAN_POINT('Ctrl Pts',(86.1833095869423,-14.5950365325702,
67.1287136717026));
#143437=CARTESIAN_POINT('Ctrl Pts',(86.1755325592852,-14.5949353267232,
67.0846095660177));
#143438=CARTESIAN_POINT('Ctrl Pts',(86.1677612647959,-14.5918224815627,
67.0405372500604));
#143439=CARTESIAN_POINT('Ctrl Pts',(86.1600605535813,-14.5857283801364,
66.996864939702));
#143440=CARTESIAN_POINT('Ctrl Pts',(86.1555769842231,-14.5821802239129,
66.9714376996629));
#143441=CARTESIAN_POINT('Ctrl Pts',(86.1511171770846,-14.5776222205114,
66.9461451210373));
#143442=CARTESIAN_POINT('Ctrl Pts',(86.146692761572,-14.5720643646981,66.9210532283303));
#143443=CARTESIAN_POINT('Ctrl Pts',(86.1394556395654,-14.5629732473513,
66.8800098208153));
#143444=CARTESIAN_POINT('Ctrl Pts',(86.1323177597175,-14.5512087224418,
66.8395292495397));
#143445=CARTESIAN_POINT('Ctrl Pts',(86.1253401741445,-14.5368699810008,
66.7999577493598));
#143446=CARTESIAN_POINT('Ctrl Pts',(86.1181504314958,-14.5220952627563,
66.7591830573775));
#143447=CARTESIAN_POINT('Ctrl Pts',(86.1111308966058,-14.5045878930689,
66.7193736581523));
#143448=CARTESIAN_POINT('Ctrl Pts',(86.1043425244012,-14.4845020933198,
66.6808752405993));
#143449=CARTESIAN_POINT('Ctrl Pts',(86.0973159958783,-14.4637116238834,
66.6410261838784));
#143450=CARTESIAN_POINT('Ctrl Pts',(86.0905371172554,-14.4401588108996,
66.6025816115021));
#143451=CARTESIAN_POINT('Ctrl Pts',(86.0840673353281,-14.4140575196726,
66.5658900139963));
#143452=CARTESIAN_POINT('Ctrl Pts',(86.0814287747804,-14.4034126728985,
66.5509261399891));
#143453=CARTESIAN_POINT('Ctrl Pts',(86.0788415569041,-14.392344423101,66.5362534449891));
#143454=CARTESIAN_POINT('Ctrl Pts',(86.076309583227,-14.3808692039259,66.521894057092));
#143455=CARTESIAN_POINT('Ctrl Pts',(86.0701221752456,-14.3528271024801,
66.486803885308));
#143456=CARTESIAN_POINT('Ctrl Pts',(86.0642677470609,-14.3223642102344,
66.4536021666565));
#143457=CARTESIAN_POINT('Ctrl Pts',(86.0587985898109,-14.2897543905021,
66.4225854143852));
#143458=CARTESIAN_POINT('Ctrl Pts',(86.0534543531146,-14.2578894088772,
66.3922771131036));
#143459=CARTESIAN_POINT('Ctrl Pts',(86.0484779941468,-14.2239742656419,
66.3640551372869));
#143460=CARTESIAN_POINT('Ctrl Pts',(86.0439131969578,-14.1883035423802,
66.3381672267215));
#143461=CARTESIAN_POINT('Ctrl Pts',(86.0395484851462,-14.1541963475362,
66.3134140417839));
#143462=CARTESIAN_POINT('Ctrl Pts',(86.0355600908499,-14.1184841072631,
66.2907950438382));
#143463=CARTESIAN_POINT('Ctrl Pts',(86.0319811186901,-14.0814617480119,
66.2704980036799));
#143464=CARTESIAN_POINT('Ctrl Pts',(86.030405635642,-14.0651643037178,66.2615631359944));
#143465=CARTESIAN_POINT('Ctrl Pts',(86.0289094185842,-14.0486134846307,
66.2530778102736));
#143466=CARTESIAN_POINT('Ctrl Pts',(86.0274949090129,-14.0318368536377,
66.2450558766909));
#143467=CARTESIAN_POINT('Ctrl Pts',(86.0241177110331,-13.991781978473,66.2259031905307));
#143468=CARTESIAN_POINT('Ctrl Pts',(86.0212088028127,-13.9504617089997,
66.2094036096931));
#143469=CARTESIAN_POINT('Ctrl Pts',(86.0187949238061,-13.9081978233312,
66.1956794901586));
#143470=CARTESIAN_POINT('Ctrl Pts',(86.0165451824516,-13.8688077747309,
66.1828885759558));
#143471=CARTESIAN_POINT('Ctrl Pts',(86.0147255938159,-13.8285977890043,
66.1725095723019));
#143472=CARTESIAN_POINT('Ctrl Pts',(86.0133551556414,-13.7878683714231,
66.1646254052992));
#143473=CARTESIAN_POINT('Ctrl Pts',(86.0120724941042,-13.7497476751854,
66.1572462196087));
#143474=CARTESIAN_POINT('Ctrl Pts',(86.0111834231525,-13.7111723372268,
66.152053375483));
#143475=CARTESIAN_POINT('Ctrl Pts',(86.0106990615863,-13.6724238593391,
66.1490866930459));
#143476=CARTESIAN_POINT('Ctrl Pts',(86.0103773263657,-13.6466853388875,
66.1471160861796));
#143477=CARTESIAN_POINT('Ctrl Pts',(86.0102340649736,-13.6208711820731,
66.1461271215101));
#143478=CARTESIAN_POINT('Ctrl Pts',(86.0102709048271,-13.5950714516843,
66.1461211485216));
#143479=CARTESIAN_POINT('Origin',(68.9005579452291,-13.59506522122,70.178478144643));
#143480=CARTESIAN_POINT('',(69.2684768035491,-13.5950670495485,69.0981773024547));
#143481=CARTESIAN_POINT('',(69.2686191785991,-13.59506704669,69.098152274888));
#143482=CARTESIAN_POINT('Origin',(69.4419826548991,-13.59506522122,70.083010360306));
#143483=CARTESIAN_POINT('Ctrl Pts',(69.3960064164891,-14.36360211489,70.934760808954));
#143484=CARTESIAN_POINT('Ctrl Pts',(69.3948941469191,-14.36432617912,70.932322575951));
#143485=CARTESIAN_POINT('Ctrl Pts',(69.381319711449,-14.37348187874,70.9013962234701));
#143486=CARTESIAN_POINT('Ctrl Pts',(69.365369560429,-14.39219596977,70.83622702643));
#143487=CARTESIAN_POINT('Ctrl Pts',(69.3732349764891,-14.41738726414,70.7437279326));
#143488=CARTESIAN_POINT('Ctrl Pts',(69.4081799305892,-14.43748604032,70.665615251245));
#143489=CARTESIAN_POINT('Ctrl Pts',(69.4631712916492,-14.45027727949,70.610789156178));
#143490=CARTESIAN_POINT('Ctrl Pts',(69.5265616814791,-14.45439606951,70.5852234897169));
#143491=CARTESIAN_POINT('Ctrl Pts',(69.5705096728792,-14.45215669278,70.585314755206));
#143492=CARTESIAN_POINT('Ctrl Pts',(69.5901759596291,-14.45019796276,70.5887204004031));
#143493=CARTESIAN_POINT('Ctrl Pts',(68.4737857702591,-14.59510829149,71.468546571735));
#143494=CARTESIAN_POINT('Ctrl Pts',(68.4681080885491,-14.59879574582,71.456943752246));
#143495=CARTESIAN_POINT('Ctrl Pts',(68.398951202899,-14.64525476894,71.309844593959));
#143496=CARTESIAN_POINT('Ctrl Pts',(68.3208252767391,-14.73575279283,71.000643124038));
#143497=CARTESIAN_POINT('Ctrl Pts',(68.3692877416891,-14.85190586561,70.541515055448));
#143498=CARTESIAN_POINT('Ctrl Pts',(68.5773966848091,-14.94278494479,70.12318452394));
#143499=CARTESIAN_POINT('Ctrl Pts',(68.9244124274791,-15.00011120262,69.805528015821));
#143500=CARTESIAN_POINT('Ctrl Pts',(69.3392401939591,-15.01849094173,69.647259299348));
#143501=CARTESIAN_POINT('Ctrl Pts',(69.6249372840391,-15.00849600097,69.643102053229));
#143502=CARTESIAN_POINT('Ctrl Pts',(69.7505968801491,-14.99973699477,69.6606970664251));
#143503=CARTESIAN_POINT('Ctrl Pts',(67.8246108602491,-13.72054945886,71.520893278361));
#143504=CARTESIAN_POINT('Ctrl Pts',(67.8160399692091,-13.72604884949,71.503718416127));
#143505=CARTESIAN_POINT('Ctrl Pts',(67.7116892300791,-13.79531380705,71.2859739195089));
#143506=CARTESIAN_POINT('Ctrl Pts',(67.5949376413891,-13.92962281055,70.828058226473));
#143507=CARTESIAN_POINT('Ctrl Pts',(67.6719744253092,-14.10119003487,70.144322017472));
#143508=CARTESIAN_POINT('Ctrl Pts',(67.9941451974891,-14.23515457677,69.5162707493999));
#143509=CARTESIAN_POINT('Ctrl Pts',(68.5315781770691,-14.31958028328,69.035370936371));
#143510=CARTESIAN_POINT('Ctrl Pts',(69.1744797319091,-14.34663621025,68.793437652579));
#143511=CARTESIAN_POINT('Ctrl Pts',(69.6165656972991,-14.33192284069,68.785276381127));
#143512=CARTESIAN_POINT('Ctrl Pts',(69.8106988187391,-14.31902626561,68.810980738384));
#143513=CARTESIAN_POINT('Ctrl Pts',(68.283664590389,-12.8650716666,71.0244553278579));
#143514=CARTESIAN_POINT('Ctrl Pts',(68.2775948930291,-12.8689004296,71.0124695659739));
#143515=CARTESIAN_POINT('Ctrl Pts',(68.203716840389,-12.91713341696,70.8604945354981));
#143516=CARTESIAN_POINT('Ctrl Pts',(68.121582769839,-13.01091631349,70.5405079572659));
#143517=CARTESIAN_POINT('Ctrl Pts',(68.178409428339,-13.13105810204,70.063149520895));
#143518=CARTESIAN_POINT('Ctrl Pts',(68.4087959210191,-13.22498253222,69.6256866190019));
#143519=CARTESIAN_POINT('Ctrl Pts',(68.7900615322991,-13.28420786759,69.291147994876));
#143520=CARTESIAN_POINT('Ctrl Pts',(69.2442495489591,-13.30319304647,69.122225590261));
#143521=CARTESIAN_POINT('Ctrl Pts',(69.5561652089491,-13.29286878287,69.115456077889));
#143522=CARTESIAN_POINT('Ctrl Pts',(69.6931588369591,-13.28382045211,69.132756842017));
#143523=CARTESIAN_POINT('',(68.0516610740254,-13.4647404820174,70.8358748491249));
#143524=CARTESIAN_POINT('Ctrl Pts',(68.0516610740254,-13.4647404820174,
70.835874849125));
#143525=CARTESIAN_POINT('Ctrl Pts',(68.0421205335876,-13.46988128998,70.7818800903522));
#143526=CARTESIAN_POINT('Ctrl Pts',(68.0356143114983,-13.4748971670155,
70.7278391604887));
#143527=CARTESIAN_POINT('Ctrl Pts',(68.0320569230294,-13.4797508904263,
70.6741055266695));
#143528=CARTESIAN_POINT('Ctrl Pts',(68.028342778009,-13.484818493471,70.6180041168247));
#143529=CARTESIAN_POINT('Ctrl Pts',(68.02784208004,-13.4897095996712,70.5622381436379));
#143530=CARTESIAN_POINT('Ctrl Pts',(68.0303533192616,-13.4944247707082,
70.5071605870412));
#143531=CARTESIAN_POINT('Ctrl Pts',(68.0329792081805,-13.4993552111341,
70.4495684849789));
#143532=CARTESIAN_POINT('Ctrl Pts',(68.0388979933081,-13.5040932318593,
70.3927295676384));
#143533=CARTESIAN_POINT('Ctrl Pts',(68.0478686063493,-13.5086485211404,
70.3369881668536));
#143534=CARTESIAN_POINT('Ctrl Pts',(68.0568392193905,-13.5132038104215,
70.2812467660689));
#143535=CARTESIAN_POINT('Ctrl Pts',(68.0688612106036,-13.5175763912568,
70.2266027815759));
#143536=CARTESIAN_POINT('Ctrl Pts',(68.0836892332499,-13.5217849262162,
70.1733404031047));
#143537=CARTESIAN_POINT('Ctrl Pts',(68.0876485063194,-13.5229086592671,
70.1591186618967));
#143538=CARTESIAN_POINT('Ctrl Pts',(68.0918074778127,-13.5240202220121,
70.1449963682538));
#143539=CARTESIAN_POINT('Ctrl Pts',(68.0961615044139,-13.5251191716146,
70.130977824729));
#143540=CARTESIAN_POINT('Ctrl Pts',(68.1118919831629,-13.5290895202027,
70.0803308211147));
#143541=CARTESIAN_POINT('Ctrl Pts',(68.1301665305715,-13.532894769871,70.0310417949526));
#143542=CARTESIAN_POINT('Ctrl Pts',(68.1506864552881,-13.5365283692355,
69.9833257802005));
#143543=CARTESIAN_POINT('Ctrl Pts',(68.1715708548488,-13.5402265085816,
69.9347622337311));
#143544=CARTESIAN_POINT('Ctrl Pts',(68.1947809799418,-13.5437468823172,
69.8878278111564));
#143545=CARTESIAN_POINT('Ctrl Pts',(68.220028013724,-13.5470886456198,69.8427012760628));
#143546=CARTESIAN_POINT('Ctrl Pts',(68.2460472991032,-13.5505326261599,
69.796194418865));
#143547=CARTESIAN_POINT('Ctrl Pts',(68.2742298660689,-13.5537869291663,
69.7516075202316));
#143548=CARTESIAN_POINT('Ctrl Pts',(68.304289181768,-13.5568565394829,69.7090893843644));
#143549=CARTESIAN_POINT('Ctrl Pts',(68.3191133708432,-13.5583703624912,
69.688120946775));
#143550=CARTESIAN_POINT('Ctrl Pts',(68.3343944672205,-13.5598393527349,
69.6676549694699));
#143551=CARTESIAN_POINT('Ctrl Pts',(68.3501007657274,-13.5612645825095,
69.6477055627966));
#143552=CARTESIAN_POINT('Ctrl Pts',(68.35475770232,-13.5616871648695,69.6417905394767));
#143553=CARTESIAN_POINT('Ctrl Pts',(68.3594520305785,-13.5621059021736,
69.6359209138541));
#143554=CARTESIAN_POINT('Ctrl Pts',(68.364182573376,-13.5625208751211,69.6300969152317));
#143555=CARTESIAN_POINT('Ctrl Pts',(68.3968043587475,-13.5653825252549,
69.5899346672198));
#143556=CARTESIAN_POINT('Ctrl Pts',(68.4311388118727,-13.5680575385359,
69.5519512465469));
#143557=CARTESIAN_POINT('Ctrl Pts',(68.4668297458609,-13.5705432646287,
69.5161993167051));
#143558=CARTESIAN_POINT('Ctrl Pts',(68.5034294369521,-13.5730922818991,
69.4795370766932));
#143559=CARTESIAN_POINT('Ctrl Pts',(68.5414557353341,-13.5754422829169,
69.4452211726811));
#143560=CARTESIAN_POINT('Ctrl Pts',(68.5805740405099,-13.5775926222074,
69.4132822919613));
#143561=CARTESIAN_POINT('Ctrl Pts',(68.6212598754391,-13.5798291288511,
69.3800635719029));
#143562=CARTESIAN_POINT('Ctrl Pts',(68.66312708886,-13.5818496788251,69.3494160245309));
#143563=CARTESIAN_POINT('Ctrl Pts',(68.7058501301954,-13.5836554461766,
69.3213494005411));
#143564=CARTESIAN_POINT('Ctrl Pts',(68.723546776751,-13.5844034272561,69.3097237037455));
#143565=CARTESIAN_POINT('Ctrl Pts',(68.7413908401205,-13.5851145762207,
69.2985405620008));
#143566=CARTESIAN_POINT('Ctrl Pts',(68.7593615209816,-13.5857890505673,
69.2877995937322));
#143567=CARTESIAN_POINT('Ctrl Pts',(68.7699968921183,-13.5861882165785,
69.281442896132));
#143568=CARTESIAN_POINT('Ctrl Pts',(68.7806766317356,-13.5865745387272,
69.2752410529925));
#143569=CARTESIAN_POINT('Ctrl Pts',(68.7913955230437,-13.5869482277688,
69.2691925544764));
#143570=CARTESIAN_POINT('Ctrl Pts',(68.8361426982761,-13.5885082332348,
69.2439424408949));
#143571=CARTESIAN_POINT('Ctrl Pts',(68.8815567060986,-13.5898425649172,
69.2213712387007));
#143572=CARTESIAN_POINT('Ctrl Pts',(68.9272883543862,-13.5909523521958,
69.2013656174685));
#143573=CARTESIAN_POINT('Ctrl Pts',(68.9742558909504,-13.5920921312446,
69.1808193484865));
#143574=CARTESIAN_POINT('Ctrl Pts',(69.0215587529483,-13.5929950826377,
69.1629791935471));
#143575=CARTESIAN_POINT('Ctrl Pts',(69.0688746875484,-13.593661482091,69.1477194858201));
#143576=CARTESIAN_POINT('Ctrl Pts',(69.1180508388671,-13.5943540809085,
69.1318598456671));
#143577=CARTESIAN_POINT('Ctrl Pts',(69.1672412886183,-13.5947911796269,
69.1187875750068));
#143578=CARTESIAN_POINT('Ctrl Pts',(69.216140495377,-13.594971802996,69.1083583062007));
#143579=CARTESIAN_POINT('Ctrl Pts',(69.2336267898101,-13.5950363936842,
69.1046288128786));
#143580=CARTESIAN_POINT('Ctrl Pts',(69.2510763346266,-13.595068174289,69.1012372658518));
#143581=CARTESIAN_POINT('Ctrl Pts',(69.2684767416407,-13.5950670565703,
69.0981769504524));
#143582=CARTESIAN_POINT('Origin',(69.0364672392459,-13.4647383323567,70.6622289425537));
#143583=CARTESIAN_POINT('Origin',(68.3580209600691,0.499074165591714,66.814943349163));
#143584=CARTESIAN_POINT('',(68.8731212986265,-11.1474493393501,75.4949909016172));
#143585=CARTESIAN_POINT('Origin',(67.3732132070591,0.499074165591714,66.988591526828));
#143586=CARTESIAN_POINT('Origin',(69.8579284813091,-11.14744746673,75.321341605509));
#143587=CARTESIAN_POINT('Ctrl Pts',(70.5727142903791,-11.62540260925,76.212415349127));
#143588=CARTESIAN_POINT('Ctrl Pts',(70.5474025662891,-11.62160041199,76.221790216259));
#143589=CARTESIAN_POINT('Ctrl Pts',(70.4849770218291,-11.61987597393,76.2350078033179));
#143590=CARTESIAN_POINT('Ctrl Pts',(70.3779197843791,-11.64555877,76.220765968497));
#143591=CARTESIAN_POINT('Ctrl Pts',(70.2560676070191,-11.71486549074,76.152463833801));
#143592=CARTESIAN_POINT('Ctrl Pts',(70.1558432364391,-11.81914313621,76.032792395521));
#143593=CARTESIAN_POINT('Ctrl Pts',(70.1050930198391,-11.92846628364,75.894132175066));
#143594=CARTESIAN_POINT('Ctrl Pts',(70.0998645202791,-11.99631186027,75.801284231172));
#143595=CARTESIAN_POINT('Ctrl Pts',(70.1022592401991,-12.02298947846,75.763694284642));
#143596=CARTESIAN_POINT('Ctrl Pts',(70.8569680292191,-11.22017028,76.869673584669));
#143597=CARTESIAN_POINT('Ctrl Pts',(70.7478285345391,-11.20473814975,76.9076141171011));
#143598=CARTESIAN_POINT('Ctrl Pts',(70.4658852850292,-11.19636485193,76.967431120053));
#143599=CARTESIAN_POINT('Ctrl Pts',(70.0286683689591,-11.30538170868,76.912662413182));
#143600=CARTESIAN_POINT('Ctrl Pts',(69.6654256755191,-11.51820751993,76.714360538357));
#143601=CARTESIAN_POINT('Ctrl Pts',(69.4246643242891,-11.77129992332,76.433832422159));
#143602=CARTESIAN_POINT('Ctrl Pts',(69.3125109709092,-12.01186619021,76.132469357613));
#143603=CARTESIAN_POINT('Ctrl Pts',(69.3008812463991,-12.16248052272,75.924831943563));
#143604=CARTESIAN_POINT('Ctrl Pts',(69.3072602647691,-12.22316470436,75.8378355297749));
#143605=CARTESIAN_POINT('Ctrl Pts',(70.9671564453892,-10.40460940052,76.8651302226241));
#143606=CARTESIAN_POINT('Ctrl Pts',(70.8026967635191,-10.38178139262,76.921572843059));
#143607=CARTESIAN_POINT('Ctrl Pts',(70.3760114274691,-10.36915940562,77.0119477511941));
#143608=CARTESIAN_POINT('Ctrl Pts',(69.7215419928391,-10.53124236333,76.9327305518971));
#143609=CARTESIAN_POINT('Ctrl Pts',(69.2001137835892,-10.83431808305,76.65410085986));
#143610=CARTESIAN_POINT('Ctrl Pts',(68.8680419533291,-11.17951523624,76.2751089113451));
#143611=CARTESIAN_POINT('Ctrl Pts',(68.7168083006591,-11.50052073533,75.874419214426));
#143612=CARTESIAN_POINT('Ctrl Pts',(68.7018554092492,-11.70191427611,75.5961943394401));
#143613=CARTESIAN_POINT('Ctrl Pts',(68.7112204234791,-11.78351622729,75.478665827774));
#143614=CARTESIAN_POINT('Ctrl Pts',(70.7997299180591,-9.94514372726199,
76.203054889814));
#143615=CARTESIAN_POINT('Ctrl Pts',(70.6604448068091,-9.92610417687498,
76.250548674226));
#143616=CARTESIAN_POINT('Ctrl Pts',(70.2998144530591,-9.91562637911499,
76.326723169705));
#143617=CARTESIAN_POINT('Ctrl Pts',(69.7451628261291,-10.05063858235,76.26211134095));
#143618=CARTESIAN_POINT('Ctrl Pts',(69.2974090212691,-10.30588263055,76.028313862207));
#143619=CARTESIAN_POINT('Ctrl Pts',(69.0090622832791,-10.59991903937,75.705782364097));
#143620=CARTESIAN_POINT('Ctrl Pts',(68.8777969001991,-10.87496707353,75.362484500442));
#143621=CARTESIAN_POINT('Ctrl Pts',(68.8657218477491,-11.04743048786,75.124208776502));
#143622=CARTESIAN_POINT('Ctrl Pts',(68.8742684640891,-11.11720392997,75.023715091041));
#143623=CARTESIAN_POINT('Ctrl Pts',(70.6107884237591,-10.75942680297,76.71163854688));
#143624=CARTESIAN_POINT('Ctrl Pts',(70.4329281245592,-10.7588937036665,
76.7430935490508));
#143625=CARTESIAN_POINT('Ctrl Pts',(70.2423398126716,-10.768156222049,76.7431479729786));
#143626=CARTESIAN_POINT('Ctrl Pts',(69.9571737741532,-10.7967434261519,
76.6853219130463));
#143627=CARTESIAN_POINT('Ctrl Pts',(69.8623280976091,-10.8087213986076,
76.6564591267567));
#143628=CARTESIAN_POINT('Ctrl Pts',(69.7235605112814,-10.8303617139236,
76.5982160113568));
#143629=CARTESIAN_POINT('Ctrl Pts',(69.677892530448,-10.8381873784676,76.5763169357272));
#143630=CARTESIAN_POINT('Ctrl Pts',(69.6107045260779,-10.8508442144416,
76.5397381599502));
#143631=CARTESIAN_POINT('Ctrl Pts',(69.5774393211989,-10.8574022172182,
76.5205169934371));
#143632=CARTESIAN_POINT('Ctrl Pts',(69.5393026779042,-10.8654549938392,
76.4964694047508));
#143633=CARTESIAN_POINT('Ctrl Pts',(69.5204148930439,-10.8695818254951,
76.4840415082369));
#143634=CARTESIAN_POINT('Ctrl Pts',(69.5123601399464,-10.8713719912073,
76.4786288640684));
#143635=CARTESIAN_POINT('Ctrl Pts',(69.5069993437469,-10.872570218032,76.4750012569881));
#143636=CARTESIAN_POINT('Ctrl Pts',(69.5033202961855,-10.8733985090141,
76.4724895148948));
#143637=CARTESIAN_POINT('Ctrl Pts',(69.3948927597608,-10.8979106828788,
76.398089236559));
#143638=CARTESIAN_POINT('Ctrl Pts',(69.2671450458483,-10.9327842016567,
76.2910185912873));
#143639=CARTESIAN_POINT('Ctrl Pts',(69.0294099549965,-11.0240081109645,
75.972523756007));
#143640=CARTESIAN_POINT('Ctrl Pts',(68.9196520979315,-11.080358483221,75.7588815978788));
#143641=CARTESIAN_POINT('Ctrl Pts',(68.8731215714991,-11.1474472924843,
75.4949903331303));
#143642=CARTESIAN_POINT('Ctrl Pts',(70.5465863094391,-11.53587577121,76.347528984853));
#143643=CARTESIAN_POINT('Ctrl Pts',(70.5665960457121,-11.4425022179353,
76.4608199972518));
#143644=CARTESIAN_POINT('Ctrl Pts',(70.5828633060719,-11.3232077539368,
76.5532835146138));
#143645=CARTESIAN_POINT('Ctrl Pts',(70.604920056824,-11.0556680213945,76.6787881629939));
#143646=CARTESIAN_POINT('Ctrl Pts',(70.6106952853454,-10.9075952019447,
76.7117484109232));
#143647=CARTESIAN_POINT('Ctrl Pts',(70.6107884237367,-10.759426838634,76.7116385469064));
#143648=CARTESIAN_POINT('Origin',(93.9117403164691,-10.75942675157,71.587718899901));
#143649=CARTESIAN_POINT('Ctrl Pts',(79.7232095658691,-10.75961935955,75.104974613695));
#143650=CARTESIAN_POINT('Ctrl Pts',(79.8754552241483,-10.8828544446583,
75.0780971616129));
#143651=CARTESIAN_POINT('Ctrl Pts',(80.0491425096114,-11.019491411425,75.0240272782727));
#143652=CARTESIAN_POINT('Ctrl Pts',(80.4350484926432,-11.2915328846245,
74.8368221251738));
#143653=CARTESIAN_POINT('Ctrl Pts',(80.6471382934547,-11.4268302101939,
74.7029558455787));
#143654=CARTESIAN_POINT('Ctrl Pts',(80.8778403488691,-11.53587675694,74.525850965447));
#143655=CARTESIAN_POINT('Ctrl Pts',(79.3965414347691,-10.75937454605,75.186662823148));
#143656=CARTESIAN_POINT('Ctrl Pts',(79.3992528435091,-10.7645545324,75.1866956812119));
#143657=CARTESIAN_POINT('Ctrl Pts',(79.4725942355591,-10.90537889734,75.186841976488));
#143658=CARTESIAN_POINT('Ctrl Pts',(79.6130654149191,-11.21423607471,75.144851871569));
#143659=CARTESIAN_POINT('Ctrl Pts',(79.8139675630191,-11.69507199961,74.9338518091059));
#143660=CARTESIAN_POINT('Ctrl Pts',(79.9721744722591,-12.03339183741,74.641026175075));
#143661=CARTESIAN_POINT('Ctrl Pts',(80.0647903183391,-12.1995563218,74.42412393955));
#143662=CARTESIAN_POINT('Ctrl Pts',(80.0853956808191,-12.23499347946,74.373394440298));
#143663=CARTESIAN_POINT('Ctrl Pts',(79.7916100122891,-10.5653046013,75.021875684663));
#143664=CARTESIAN_POINT('Ctrl Pts',(79.7941034949391,-10.57001050956,75.021940607005));
#143665=CARTESIAN_POINT('Ctrl Pts',(79.8614679630191,-10.6979216525,75.022938558934));
#143666=CARTESIAN_POINT('Ctrl Pts',(79.9858550612891,-10.97673091235,74.981925321278));
#143667=CARTESIAN_POINT('Ctrl Pts',(80.1528636967791,-11.40236933979,74.784369362516));
#143668=CARTESIAN_POINT('Ctrl Pts',(80.278150309989,-11.69585236607,74.521057735256));
#143669=CARTESIAN_POINT('Ctrl Pts',(80.3509919691591,-11.83827309688,74.3307566055));
#143670=CARTESIAN_POINT('Ctrl Pts',(80.3672219688891,-11.86855566293,74.286462610011));
#143671=CARTESIAN_POINT('Ctrl Pts',(80.2102524607391,-10.35643022745,75.066664900866));
#143672=CARTESIAN_POINT('Ctrl Pts',(80.2128494848392,-10.36134940962,75.066774703059));
#143673=CARTESIAN_POINT('Ctrl Pts',(80.2829816961191,-10.49495458286,75.0688538343589));
#143674=CARTESIAN_POINT('Ctrl Pts',(80.4106556196692,-10.77987219022,75.0227015441689));
#143675=CARTESIAN_POINT('Ctrl Pts',(80.5737969977991,-11.19462437857,74.8135437512119));
#143676=CARTESIAN_POINT('Ctrl Pts',(80.6877425938991,-11.46754862033,74.5509908140901));
#143677=CARTESIAN_POINT('Ctrl Pts',(80.7524414512091,-11.59633911287,74.368633104737));
#143678=CARTESIAN_POINT('Ctrl Pts',(80.7668633987791,-11.6235324656,74.326529759673));
#143679=CARTESIAN_POINT('Ctrl Pts',(80.5677595186891,-10.17501563828,75.311967698886));
#143680=CARTESIAN_POINT('Ctrl Pts',(80.570760600919,-10.18079229193,75.312126115391));
#143681=CARTESIAN_POINT('Ctrl Pts',(80.6518451898191,-10.33754660207,75.31529717998));
#143682=CARTESIAN_POINT('Ctrl Pts',(80.8015117797791,-10.66349284216,75.258929767445));
#143683=CARTESIAN_POINT('Ctrl Pts',(80.9915946672691,-11.11387280127,75.015471749357));
#143684=CARTESIAN_POINT('Ctrl Pts',(81.1180732976791,-11.39467620639,74.724768670296));
#143685=CARTESIAN_POINT('Ctrl Pts',(81.1879083750491,-11.52270795576,74.530089402506));
#143686=CARTESIAN_POINT('Ctrl Pts',(81.2034554272791,-11.54950255337,74.48548859231));
#143687=CARTESIAN_POINT('Origin',(70.3503323584791,15.19124921296,75.234517520424));
#143688=CARTESIAN_POINT('',(68.8731215366466,11.1474497637427,75.4949903427175));
#143689=CARTESIAN_POINT('',(68.8731214546391,11.14744746373,75.494989659206));
#143690=CARTESIAN_POINT('Ctrl Pts',(68.873121472862,11.1474474374557,75.494989762555));
#143691=CARTESIAN_POINT('Ctrl Pts',(68.9196357623451,11.0803819298226,75.7587895431469));
#143692=CARTESIAN_POINT('Ctrl Pts',(69.0293411064219,11.0240431945441,75.9724005246367));
#143693=CARTESIAN_POINT('Ctrl Pts',(69.2076201138475,10.9556252471803,76.2112882368804));
#143694=CARTESIAN_POINT('Ctrl Pts',(69.2696540133536,10.9355009565293,76.2780069134329));
#143695=CARTESIAN_POINT('Ctrl Pts',(69.3598779034547,10.9093370612364,76.3617636879751));
#143696=CARTESIAN_POINT('Ctrl Pts',(69.3895069124018,10.9012861862527,76.386976797235));
#143697=CARTESIAN_POINT('Ctrl Pts',(69.432655939315,10.890215508948,76.4211964872657));
#143698=CARTESIAN_POINT('Ctrl Pts',(69.4539089655518,10.8849315790885,76.4374067439443));
#143699=CARTESIAN_POINT('Ctrl Pts',(69.4780260298471,10.8792069596395,76.4548468328527));
#143700=CARTESIAN_POINT('Ctrl Pts',(69.4899020813184,10.8764546412619,76.46321167396));
#143701=CARTESIAN_POINT('Ctrl Pts',(69.4949513584603,10.8752986458172,76.4667218509199));
#143702=CARTESIAN_POINT('Ctrl Pts',(69.4983084054692,10.8745332198706,76.4690455074634));
#143703=CARTESIAN_POINT('Ctrl Pts',(69.498981060932,10.8743795455877,76.4695120379923));
#143704=CARTESIAN_POINT('Ctrl Pts',(69.6725708456909,10.8351263615574,76.58862513492));
#143705=CARTESIAN_POINT('Ctrl Pts',(69.8620431857368,10.8062726507668,76.6660209055238));
#143706=CARTESIAN_POINT('Ctrl Pts',(70.2422605680285,10.768156393542,76.7431422960647));
#143707=CARTESIAN_POINT('Ctrl Pts',(70.4328762301428,10.7588938387249,76.7431026435897));
#143708=CARTESIAN_POINT('Ctrl Pts',(70.6107879836103,10.7594268536258,76.7116386626372));
#143709=CARTESIAN_POINT('Ctrl Pts',(70.102712361999,12.02753207592,75.757282539526));
#143710=CARTESIAN_POINT('Ctrl Pts',(70.0996331790591,11.99950461932,75.796911436068));
#143711=CARTESIAN_POINT('Ctrl Pts',(70.1043339346791,11.93010065,75.892059102544));
#143712=CARTESIAN_POINT('Ctrl Pts',(70.1558442152191,11.81914181107,76.032794052158));
#143713=CARTESIAN_POINT('Ctrl Pts',(70.256068577559,11.71486478129,76.152464588268));
#143714=CARTESIAN_POINT('Ctrl Pts',(70.3779204807191,11.64555844469,76.220766236192));
#143715=CARTESIAN_POINT('Ctrl Pts',(70.4854323625891,11.61976697429,76.235068208024));
#143716=CARTESIAN_POINT('Ctrl Pts',(70.5482524904191,11.62162458361,76.221609172899));
#143717=CARTESIAN_POINT('Ctrl Pts',(70.5739515098291,11.62559101398,76.211953819954));
#143718=CARTESIAN_POINT('Ctrl Pts',(69.3084586152291,12.23351299725,75.822967076824));
#143719=CARTESIAN_POINT('Ctrl Pts',(69.3003664827991,12.16956777349,75.915049294702));
#143720=CARTESIAN_POINT('Ctrl Pts',(69.3108335232591,12.01546339144,76.127964138853));
#143721=CARTESIAN_POINT('Ctrl Pts',(69.4246666664091,11.77129665272,76.433835944702));
#143722=CARTESIAN_POINT('Ctrl Pts',(69.6654281435891,11.51820560131,76.714362465994));
#143723=CARTESIAN_POINT('Ctrl Pts',(70.0286715861291,11.30538064205,76.912663256773));
#143724=CARTESIAN_POINT('Ctrl Pts',(70.4677430073291,11.19590164666,76.96766322359));
#143725=CARTESIAN_POINT('Ctrl Pts',(70.7516719479191,11.20485608161,76.906794945282));
#143726=CARTESIAN_POINT('Ctrl Pts',(70.8623006925891,11.22093455699,76.867807281098));
#143727=CARTESIAN_POINT('Ctrl Pts',(68.7129713268991,11.79743625123,75.458569937586));
#143728=CARTESIAN_POINT('Ctrl Pts',(68.7011960208591,11.71139085457,75.583084770824));
#143729=CARTESIAN_POINT('Ctrl Pts',(68.7145463530291,11.50532104132,75.868429277325));
#143730=CARTESIAN_POINT('Ctrl Pts',(68.8680451809691,11.17951080797,76.275113604241));
#143731=CARTESIAN_POINT('Ctrl Pts',(69.2001172342691,10.83431545673,76.654103547953));
#143732=CARTESIAN_POINT('Ctrl Pts',(69.7215468729191,10.53124087494,76.93273179034));
#143733=CARTESIAN_POINT('Ctrl Pts',(70.3787919557391,10.36847068451,77.012283454108));
#143734=CARTESIAN_POINT('Ctrl Pts',(70.8085139955891,10.38195929028,76.920335313241));
#143735=CARTESIAN_POINT('Ctrl Pts',(70.9751918492591,10.40573993406,76.8623542019151));
#143736=CARTESIAN_POINT('Ctrl Pts',(68.8758599429291,11.12910515526,75.006533496628));
#143737=CARTESIAN_POINT('Ctrl Pts',(68.8651925032291,11.05554582734,75.112981674439));
#143738=CARTESIAN_POINT('Ctrl Pts',(68.8758335592991,10.87908010167,75.35735252033));
#143739=CARTESIAN_POINT('Ctrl Pts',(69.0090650491591,10.59991528949,75.705786421317));
#143740=CARTESIAN_POINT('Ctrl Pts',(69.2974119850591,10.30588041722,76.028316179364));
#143741=CARTESIAN_POINT('Ctrl Pts',(69.7451669278891,10.05063733625,76.262112423484));
#143742=CARTESIAN_POINT('Ctrl Pts',(70.3021709983891,9.91505270512101,76.326997017962));
#143743=CARTESIAN_POINT('Ctrl Pts',(70.6653612936691,9.92625183784202,76.24950570992));
#143744=CARTESIAN_POINT('Ctrl Pts',(70.8065354647891,9.94608665721,76.20071911601));
#143745=CARTESIAN_POINT('Origin',(70.4377543611373,10.7600784829335,75.7271941746767));
#143746=CARTESIAN_POINT('Origin',(69.8579298464391,11.14744710765,75.321341757772));
#143747=CARTESIAN_POINT('Origin',(68.3580209600691,-0.499074165591386,66.814943349163));
#143748=CARTESIAN_POINT('',(68.0516611136485,13.4647404820328,70.8358748421131));
#143749=CARTESIAN_POINT('Origin',(67.3732132070591,-0.499074165591386,66.988591526828));
#143750=CARTESIAN_POINT('Origin',(69.0364886624041,13.4646700573952,70.6621973310861));
#143751=CARTESIAN_POINT('Ctrl Pts',(69.5909480384691,14.4501205633,70.5888558711801));
#143752=CARTESIAN_POINT('Ctrl Pts',(69.5710297789591,14.45212989413,70.5853163357091));
#143753=CARTESIAN_POINT('Ctrl Pts',(69.526803187669,14.45441189054,70.5851259273609));
#143754=CARTESIAN_POINT('Ctrl Pts',(69.463170177939,14.45027710795,70.610789854498));
#143755=CARTESIAN_POINT('Ctrl Pts',(69.408179216219,14.43748579055,70.665616301966));
#143756=CARTESIAN_POINT('Ctrl Pts',(69.3732345852692,14.41738679729,70.7437295812081));
#143757=CARTESIAN_POINT('Ctrl Pts',(69.3653696994291,14.39219576725,70.836228061593));
#143758=CARTESIAN_POINT('Ctrl Pts',(69.3811532223691,14.37367712896,70.900715547079));
#143759=CARTESIAN_POINT('Ctrl Pts',(69.3943519653192,14.36469356993,70.931081264837));
#143760=CARTESIAN_POINT('Ctrl Pts',(69.3951714436091,14.36415051983,70.9329126925041));
#143761=CARTESIAN_POINT('Ctrl Pts',(69.7555290321091,14.99939089597,69.6613979532501));
#143762=CARTESIAN_POINT('Ctrl Pts',(69.6283184250891,15.0083774287,69.643055967434));
#143763=CARTESIAN_POINT('Ctrl Pts',(69.3408205475991,15.0185610031,69.646655229886));
#143764=CARTESIAN_POINT('Ctrl Pts',(68.9244052019191,15.00011063687,69.805532218907));
#143765=CARTESIAN_POINT('Ctrl Pts',(68.5773922830591,14.94278376454,70.12319038474));
#143766=CARTESIAN_POINT('Ctrl Pts',(68.3692854484991,14.85190392646,70.541523557376));
#143767=CARTESIAN_POINT('Ctrl Pts',(68.3208257724191,14.73575126236,71.000647874436));
#143768=CARTESIAN_POINT('Ctrl Pts',(68.3981360480691,14.64620032309,71.306615498519));
#143769=CARTESIAN_POINT('Ctrl Pts',(68.4653464484391,14.60065890237,71.45103966638));
#143770=CARTESIAN_POINT('Ctrl Pts',(68.4695255391492,14.59789853672,71.459752952336));
#143771=CARTESIAN_POINT('Ctrl Pts',(69.8183183999891,14.31851666367,68.8120051244791));
#143772=CARTESIAN_POINT('Ctrl Pts',(69.6217976430991,14.33174843893,68.785184513493));
#143773=CARTESIAN_POINT('Ctrl Pts',(69.1769289671191,14.34673924446,68.7925142553861));
#143774=CARTESIAN_POINT('Ctrl Pts',(68.5315669763691,14.319579466,69.035377325048));
#143775=CARTESIAN_POINT('Ctrl Pts',(67.9941383798391,14.23515281344,69.516279580646));
#143776=CARTESIAN_POINT('Ctrl Pts',(67.6719708568691,14.10118718706,70.144334725471));
#143777=CARTESIAN_POINT('Ctrl Pts',(67.5949383401392,13.92962044387,70.828065237159));
#143778=CARTESIAN_POINT('Ctrl Pts',(67.7104711173591,13.79671729307,71.2811918084051));
#143779=CARTESIAN_POINT('Ctrl Pts',(67.8118731588091,13.7288264298,71.494978799744));
#143780=CARTESIAN_POINT('Ctrl Pts',(67.8181804147791,13.7247103957,71.507876616965));
#143781=CARTESIAN_POINT('Ctrl Pts',(69.6985357447892,13.28346290429,69.1334466308519));
#143782=CARTESIAN_POINT('Ctrl Pts',(69.559856613789,13.29274633139,69.1153792244139));
#143783=CARTESIAN_POINT('Ctrl Pts',(69.245979860049,13.30326537476,69.121580881155));
#143784=CARTESIAN_POINT('Ctrl Pts',(68.7900536127391,13.28420727445,69.291152448768));
#143785=CARTESIAN_POINT('Ctrl Pts',(68.4087910751191,13.2249812931,69.6256927678659));
#143786=CARTESIAN_POINT('Ctrl Pts',(68.178406861629,13.13105608861,70.0631583819599));
#143787=CARTESIAN_POINT('Ctrl Pts',(68.1215832668291,13.01091468929,70.5405128677461));
#143788=CARTESIAN_POINT('Ctrl Pts',(68.2028599044891,12.91811333149,70.8571528134859));
#143789=CARTESIAN_POINT('Ctrl Pts',(68.2746450030891,12.87083467023,71.0063696573741));
#143790=CARTESIAN_POINT('Ctrl Pts',(68.2791110289791,12.86796872275,71.015371154369));
#143791=CARTESIAN_POINT('',(69.2684762522038,13.5950670419766,69.0981773334213));
#143792=CARTESIAN_POINT('Ctrl Pts',(69.2684762020613,13.5950670489771,69.0981770483176));
#143793=CARTESIAN_POINT('Ctrl Pts',(69.220057547122,13.5950701709265,69.1066927282233));
#143794=CARTESIAN_POINT('Ctrl Pts',(69.1712548530349,13.5948186616202,69.117773390592));
#143795=CARTESIAN_POINT('Ctrl Pts',(69.122350723928,13.5943139780203,69.1315625395245));
#143796=CARTESIAN_POINT('Ctrl Pts',(69.0747459064741,13.5938227031304,69.1449853308053));
#143797=CARTESIAN_POINT('Ctrl Pts',(69.0270447253686,13.5930915155534,69.1609745635876));
#143798=CARTESIAN_POINT('Ctrl Pts',(68.9795563737709,13.5921205463393,69.1796595201576));
#143799=CARTESIAN_POINT('Ctrl Pts',(68.9339098572451,13.5911872361529,69.1976197809407));
#143800=CARTESIAN_POINT('Ctrl Pts',(68.8884598373705,13.590032367056,69.2180707031689));
#143801=CARTESIAN_POINT('Ctrl Pts',(68.843528998897,13.5886551324547,69.2411245525615));
#143802=CARTESIAN_POINT('Ctrl Pts',(68.8260648327327,13.5881198151817,69.2500853525421));
#143803=CARTESIAN_POINT('Ctrl Pts',(68.8086796450837,13.587550894111,69.2594393750054));
#143804=CARTESIAN_POINT('Ctrl Pts',(68.7913945439412,13.5869482908414,69.2691931008479));
#143805=CARTESIAN_POINT('Ctrl Pts',(68.7806744900466,13.586574562075,69.2752422680377));
#143806=CARTESIAN_POINT('Ctrl Pts',(68.7699935966165,13.5861881975767,69.2814448130544));
#143807=CARTESIAN_POINT('Ctrl Pts',(68.7593570820778,13.5857889863606,69.2878022461852));
#143808=CARTESIAN_POINT('Ctrl Pts',(68.7161705873195,13.5841681045361,69.3136147669676));
#143809=CARTESIAN_POINT('Ctrl Pts',(68.6737122633642,13.5823353232669,69.3419823375415));
#143810=CARTESIAN_POINT('Ctrl Pts',(68.6322838040265,13.5802888544023,69.372904327941));
#143811=CARTESIAN_POINT('Ctrl Pts',(68.5919679036079,13.5782973433426,69.4029959100473));
#143812=CARTESIAN_POINT('Ctrl Pts',(68.5526271061992,13.5761034412783,69.4355067406709));
#143813=CARTESIAN_POINT('Ctrl Pts',(68.5145832966752,13.5737070098349,69.4704155296987));
#143814=CARTESIAN_POINT('Ctrl Pts',(68.4779560546146,13.5713998099078,69.5040244842636));
#143815=CARTESIAN_POINT('Ctrl Pts',(68.4425309391481,13.5689048579052,69.5398563008427));
#143816=CARTESIAN_POINT('Ctrl Pts',(68.408638167092,13.5662238098117,69.5778701295916));
#143817=CARTESIAN_POINT('Ctrl Pts',(68.3935024629306,13.5650265176363,69.5948461994463));
#143818=CARTESIAN_POINT('Ctrl Pts',(68.3786729461382,13.5637921386554,69.6122571171597));
#143819=CARTESIAN_POINT('Ctrl Pts',(68.3641820136269,13.5625209630308,69.630097615198));
#143820=CARTESIAN_POINT('Ctrl Pts',(68.3594486557417,13.5621057427432,69.6359250843411));
#143821=CARTESIAN_POINT('Ctrl Pts',(68.3547515554537,13.561686753605,69.6417982348309));
#143822=CARTESIAN_POINT('Ctrl Pts',(68.3500918920114,13.5612639147922,69.6477168369388));
#143823=CARTESIAN_POINT('Ctrl Pts',(68.3183422079409,13.5583828056981,69.6880445879435));
#143824=CARTESIAN_POINT('Ctrl Pts',(68.2883282544299,13.5553225520827,69.7304857583872));
#143825=CARTESIAN_POINT('Ctrl Pts',(68.2603193199432,13.5520755798442,69.7749137039889));
#143826=CARTESIAN_POINT('Ctrl Pts',(68.2328820724945,13.5488948811708,69.8184348360651));
#143827=CARTESIAN_POINT('Ctrl Pts',(68.2073688978383,13.5455349757244,69.8638627496069));
#143828=CARTESIAN_POINT('Ctrl Pts',(68.1840604240437,13.5419938709497,69.9110378480984));
#143829=CARTESIAN_POINT('Ctrl Pts',(68.1613768188838,13.5385476984011,69.95694824605));
#143830=CARTESIAN_POINT('Ctrl Pts',(68.1407814228562,13.5349298863568,70.0045135978539));
#143831=CARTESIAN_POINT('Ctrl Pts',(68.1225576898816,13.5311439178348,70.0535446151893));
#143832=CARTESIAN_POINT('Ctrl Pts',(68.1131060521354,13.5291803463185,70.0789742796179));
#143833=CARTESIAN_POINT('Ctrl Pts',(68.1042927727855,13.5271716324888,70.104797479399));
#143834=CARTESIAN_POINT('Ctrl Pts',(68.0961599336273,13.5251188862045,70.1309828875299));
#143835=CARTESIAN_POINT('Ctrl Pts',(68.091806425645,13.5240200513253,70.1449999338651));
#143836=CARTESIAN_POINT('Ctrl Pts',(68.0876479307248,13.5229086059803,70.1591207069769));
#143837=CARTESIAN_POINT('Ctrl Pts',(68.0836890907593,13.5217849930833,70.1733409057962));
#143838=CARTESIAN_POINT('Ctrl Pts',(68.0693978664713,13.5177288038804,70.2246751482821));
#143839=CARTESIAN_POINT('Ctrl Pts',(68.057713180962,13.5135202722556,70.2772924424713));
#143840=CARTESIAN_POINT('Ctrl Pts',(68.0488547159004,13.5091425519104,70.3309393260326));
#143841=CARTESIAN_POINT('Ctrl Pts',(68.0396975073969,13.5046171970444,70.3863954005243));
#143842=CARTESIAN_POINT('Ctrl Pts',(68.033560798574,13.4999109806522,70.4429520930334));
#143843=CARTESIAN_POINT('Ctrl Pts',(68.0306832804395,13.4950139845556,70.5002711676494));
#143844=CARTESIAN_POINT('Ctrl Pts',(68.0278057623051,13.4901169884591,70.5575902422654));
#143845=CARTESIAN_POINT('Ctrl Pts',(68.028187870028,13.4850291992576,70.6156716572521));
#143846=CARTESIAN_POINT('Ctrl Pts',(68.0320577126148,13.4797498060016,70.6741175007522));
#143847=CARTESIAN_POINT('Ctrl Pts',(68.0356152869072,13.4748964215795,70.7278471875989));
#143848=CARTESIAN_POINT('Ctrl Pts',(68.0421212736795,13.469880918388,70.7818841101077));
#143849=CARTESIAN_POINT('Ctrl Pts',(68.0516611136484,13.4647404820328,70.8358748421131));
#143850=CARTESIAN_POINT('Origin',(69.4419825833591,13.59506528922,70.083010104271));
#143851=CARTESIAN_POINT('Origin',(86.5648503253491,13.59506522122,67.063786802906));
#143852=CARTESIAN_POINT('',(86.010255170479,13.5950708837,66.1461463384425));
#143853=CARTESIAN_POINT('',(86.0102549463391,13.5950708837,66.146145068228));
#143854=CARTESIAN_POINT('Origin',(86.1839250991447,13.5950984680028,67.1309524517065));
#143855=CARTESIAN_POINT('Ctrl Pts',(88.6593324780691,14.84336710374,63.884495094759));
#143856=CARTESIAN_POINT('Ctrl Pts',(88.6758192267691,14.84102992348,63.945364550575));
#143857=CARTESIAN_POINT('Ctrl Pts',(88.7703803079691,14.82406732012,64.343280741328));
#143858=CARTESIAN_POINT('Ctrl Pts',(88.7916617756691,14.77049785957,65.102043024085));
#143859=CARTESIAN_POINT('Ctrl Pts',(88.4834074127691,14.66322007682,66.063510160615));
#143860=CARTESIAN_POINT('Ctrl Pts',(87.9165820708691,14.55516355775,66.832622048277));
#143861=CARTESIAN_POINT('Ctrl Pts',(87.1896027922191,14.47674597442,67.36402324018));
#143862=CARTESIAN_POINT('Ctrl Pts',(86.523410283589,14.45075628501,67.604169553547));
#143863=CARTESIAN_POINT('Ctrl Pts',(86.1167247268192,14.45343250308,67.662585942143));
#143864=CARTESIAN_POINT('Ctrl Pts',(85.9893418468191,14.4559869198,67.672805629135));
#143865=CARTESIAN_POINT('Ctrl Pts',(87.7659216997691,15.40269777024,64.163723845293));
#143866=CARTESIAN_POINT('Ctrl Pts',(87.7773647030691,15.4002869873,64.20866780167));
#143867=CARTESIAN_POINT('Ctrl Pts',(87.8419823874691,15.38277416046,64.50249998336));
#143868=CARTESIAN_POINT('Ctrl Pts',(87.840895988169,15.32713368737,65.060818615117));
#143869=CARTESIAN_POINT('Ctrl Pts',(87.5862445180691,15.21768960789,65.737276187674));
#143870=CARTESIAN_POINT('Ctrl Pts',(87.1681234221592,15.11051345271,66.238286033849));
#143871=CARTESIAN_POINT('Ctrl Pts',(86.6807204492591,15.0351865187,66.555863273335));
#143872=CARTESIAN_POINT('Ctrl Pts',(86.2648695496191,15.01090882485,66.69410425116));
#143873=CARTESIAN_POINT('Ctrl Pts',(86.0139094660691,15.01327826998,66.731297190963));
#143874=CARTESIAN_POINT('Ctrl Pts',(85.9350444544391,15.01568051436,66.738612051129));
#143875=CARTESIAN_POINT('Ctrl Pts',(86.9332803389491,14.72899156245,64.368226172776));
#143876=CARTESIAN_POINT('Ctrl Pts',(86.9399959780591,14.72666943294,64.394312291263));
#143877=CARTESIAN_POINT('Ctrl Pts',(86.9780279391791,14.70981934282,64.564854256711));
#143878=CARTESIAN_POINT('Ctrl Pts',(86.9790987592991,14.65667337628,64.889105458825));
#143879=CARTESIAN_POINT('Ctrl Pts',(86.8340345043091,14.54983857184,65.285119497221));
#143880=CARTESIAN_POINT('Ctrl Pts',(86.5913101296991,14.44160203029,65.5826856115101));
#143881=CARTESIAN_POINT('Ctrl Pts',(86.3034141674891,14.36255245106,65.774586384496));
#143882=CARTESIAN_POINT('Ctrl Pts',(86.0543471845591,14.33621268175,65.858780684233));
#143883=CARTESIAN_POINT('Ctrl Pts',(85.9036912609991,14.33895163073,65.880969539341));
#143884=CARTESIAN_POINT('Ctrl Pts',(85.8563785120091,14.34153716464,65.885238584742));
#143885=CARTESIAN_POINT('Ctrl Pts',(87.2326575734091,13.68901688165,64.234896062448));
#143886=CARTESIAN_POINT('Ctrl Pts',(87.241044301839,13.68683160307,64.263453882858));
#143887=CARTESIAN_POINT('Ctrl Pts',(87.2900525363391,13.67100455445,64.450120590002));
#143888=CARTESIAN_POINT('Ctrl Pts',(87.315030254419,13.62170926292,64.807824093329));
#143889=CARTESIAN_POINT('Ctrl Pts',(87.1945462053492,13.51890229723,65.288770118133));
#143890=CARTESIAN_POINT('Ctrl Pts',(86.9282513347491,13.40902887753,65.70929487038));
#143891=CARTESIAN_POINT('Ctrl Pts',(86.543113884849,13.32423279229,66.025357899537));
#143892=CARTESIAN_POINT('Ctrl Pts',(86.162694386879,13.29470987542,66.17289886931));
#143893=CARTESIAN_POINT('Ctrl Pts',(85.9278732541291,13.29801921346,66.205606769103));
#143894=CARTESIAN_POINT('Ctrl Pts',(85.8545530515491,13.30088768445,66.210607657589));
#143895=CARTESIAN_POINT('',(87.2268072287975,13.97255211819,64.4085086937024));
#143896=CARTESIAN_POINT('Ctrl Pts',(87.2268072287975,13.97255211819,64.4085086937024));
#143897=CARTESIAN_POINT('Ctrl Pts',(87.2312812396292,13.9698592700985,64.4338829742751));
#143898=CARTESIAN_POINT('Ctrl Pts',(87.2354272871341,13.9665880921402,64.4612020199036));
#143899=CARTESIAN_POINT('Ctrl Pts',(87.2389350555738,13.9627385843149,64.4904691407583));
#143900=CARTESIAN_POINT('Ctrl Pts',(87.2423151679509,13.9590291692638,64.5186711612585));
#143901=CARTESIAN_POINT('Ctrl Pts',(87.2451022399931,13.9547827520096,64.5486825826784));
#143902=CARTESIAN_POINT('Ctrl Pts',(87.2469812637975,13.9499993325526,64.5804766593118));
#143903=CARTESIAN_POINT('Ctrl Pts',(87.2488177885167,13.9453241027575,64.6115516289473));
#143904=CARTESIAN_POINT('Ctrl Pts',(87.2497865220104,13.9401358874976,64.644330080219));
#143905=CARTESIAN_POINT('Ctrl Pts',(87.2495621407118,13.9344346867727,64.6787501211913));
#143906=CARTESIAN_POINT('Ctrl Pts',(87.2493461835623,13.9289475313605,64.7118778995703));
#143907=CARTESIAN_POINT('Ctrl Pts',(87.2480245505996,13.9229851863581,64.7465266782797));
#143908=CARTESIAN_POINT('Ctrl Pts',(87.2452840225134,13.9165476517654,64.7826002641726));
#143909=CARTESIAN_POINT('Ctrl Pts',(87.2426391201109,13.9103347430945,64.8174151286769));
#143910=CARTESIAN_POINT('Ctrl Pts',(87.238672141117,13.9036792280069,64.8535573775341));
#143911=CARTESIAN_POINT('Ctrl Pts',(87.2330862628216,13.8965811065027,64.8908970380363));
#143912=CARTESIAN_POINT('Ctrl Pts',(87.227475282113,13.8894510867063,64.9284044994698));
#143913=CARTESIAN_POINT('Ctrl Pts',(87.2202303287225,13.8818744734913,64.9671207126452));
#143914=CARTESIAN_POINT('Ctrl Pts',(87.2110418621861,13.8738512668577,65.0068627398523));
#143915=CARTESIAN_POINT('Ctrl Pts',(87.2023231880501,13.8662382746477,65.0445728173009));
#143916=CARTESIAN_POINT('Ctrl Pts',(87.1918541218471,13.8582231888616,65.0832064522933));
#143917=CARTESIAN_POINT('Ctrl Pts',(87.1793699426723,13.8498060094996,65.1225585398391));
#143918=CARTESIAN_POINT('Ctrl Pts',(87.1671491162136,13.8415663898326,65.1610804983878));
#143919=CARTESIAN_POINT('Ctrl Pts',(87.152996760082,13.8329414619205,65.200291035028));
#143920=CARTESIAN_POINT('Ctrl Pts',(87.1366720319832,13.8239312257634,65.2399488099957));
#143921=CARTESIAN_POINT('Ctrl Pts',(87.1208093365176,13.8151760029279,65.2784841658893));
#143922=CARTESIAN_POINT('Ctrl Pts',(87.1028949803302,13.806056973669,65.3174417675221));
#143923=CARTESIAN_POINT('Ctrl Pts',(87.0827227812748,13.7965741379866,65.3565529957343));
#143924=CARTESIAN_POINT('Ctrl Pts',(87.0778123620077,13.7942657779058,65.3660736497813));
#143925=CARTESIAN_POINT('Ctrl Pts',(87.0727682435476,13.7919358601946,65.3756031840621));
#143926=CARTESIAN_POINT('Ctrl Pts',(87.0675876448807,13.7895843848528,65.3851372898738));
#143927=CARTESIAN_POINT('Ctrl Pts',(87.0518679418159,13.782449206756,65.4140670182677));
#143928=CARTESIAN_POINT('Ctrl Pts',(87.0348909798187,13.7751155426953,65.4430399321384));
#143929=CARTESIAN_POINT('Ctrl Pts',(87.0165845281435,13.7675833926708,65.4719258986537));
#143930=CARTESIAN_POINT('Ctrl Pts',(87.0074313023059,13.7638173176586,65.4863688819112));
#143931=CARTESIAN_POINT('Ctrl Pts',(86.9979458392243,13.7600016211554,65.5007898979865));
#143932=CARTESIAN_POINT('Ctrl Pts',(86.9881200266237,13.7561363031612,65.5151712902311));
#143933=CARTESIAN_POINT('Ctrl Pts',(86.9832071203233,13.7542036441641,65.5223619863535));
#143934=CARTESIAN_POINT('Ctrl Pts',(86.9782091268413,13.7522585797943,65.529542776657));
#143935=CARTESIAN_POINT('Ctrl Pts',(86.9731251124026,13.7503011100517,65.5367113457746));
#143936=CARTESIAN_POINT('Ctrl Pts',(86.9700355107765,13.7491115379582,65.5410677501612));
#143937=CARTESIAN_POINT('Ctrl Pts',(86.9665039298293,13.747760364286,65.5459898821353));
#143938=CARTESIAN_POINT('Ctrl Pts',(86.9632751770817,13.7465338567315,65.5504355297153));
#143939=CARTESIAN_POINT('Ctrl Pts',(86.9611909388439,13.7457421163464,65.5533053030929));
#143940=CARTESIAN_POINT('Ctrl Pts',(86.9592340192321,13.7450023245288,65.5559773238831));
#143941=CARTESIAN_POINT('Ctrl Pts',(86.9576140827913,13.7443914847058,65.5581780686928));
#143942=CARTESIAN_POINT('Ctrl Pts',(86.9276120553036,13.7330784277883,65.5989369556538));
#143943=CARTESIAN_POINT('Ctrl Pts',(86.8960454693322,13.7224082080239,65.6374984887618));
#143944=CARTESIAN_POINT('Ctrl Pts',(86.86326398763,13.7123808254125,65.6738297509258));
#143945=CARTESIAN_POINT('Ctrl Pts',(86.8296033654357,13.7020845264,65.7111353523215));
#143946=CARTESIAN_POINT('Ctrl Pts',(86.7946622475351,13.6924660063563,65.7460897243064));
#143947=CARTESIAN_POINT('Ctrl Pts',(86.7587956819623,13.6835252652814,65.7787070560654));
#143948=CARTESIAN_POINT('Ctrl Pts',(86.7223633854806,13.6744435000105,65.8118388678826));
#143949=CARTESIAN_POINT('Ctrl Pts',(86.6849765503329,13.6660610638373,65.842559747867));
#143950=CARTESIAN_POINT('Ctrl Pts',(86.6469774815292,13.6583779567619,65.8709299052986));
#143951=CARTESIAN_POINT('Ctrl Pts',(86.6080887922948,13.6505149755675,65.8999642545766));
#143952=CARTESIAN_POINT('Ctrl Pts',(86.5685591778603,13.6433844516553,65.9265369400317));
#143953=CARTESIAN_POINT('Ctrl Pts',(86.5287195432174,13.6369863850254,65.9507532985586));
#143954=CARTESIAN_POINT('Ctrl Pts',(86.5187484575909,13.6353850733974,65.9568141820632));
#143955=CARTESIAN_POINT('Ctrl Pts',(86.5087577674021,13.6338296431522,65.9627276422958));
#143956=CARTESIAN_POINT('Ctrl Pts',(86.4987522872098,13.6323200942899,65.9684956696234));
#143957=CARTESIAN_POINT('Ctrl Pts',(86.457246068366,13.6260579595165,65.9924234571914));
#143958=CARTESIAN_POINT('Ctrl Pts',(86.4154889093146,13.620585388071,66.0138460386652));
#143959=CARTESIAN_POINT('Ctrl Pts',(86.3737965186916,13.6159023799535,66.0329262200579));
#143960=CARTESIAN_POINT('Ctrl Pts',(86.3313585325839,13.6111356244266,66.0523476171228));
#143961=CARTESIAN_POINT('Ctrl Pts',(86.2889877557992,13.6071869246566,66.0693426394481));
#143962=CARTESIAN_POINT('Ctrl Pts',(86.2469691935481,13.6040562806436,66.0841107946872));
#143963=CARTESIAN_POINT('Ctrl Pts',(86.2036516610332,13.6008288552735,66.0993354956402));
#143964=CARTESIAN_POINT('Ctrl Pts',(86.1607085767477,13.5984708465459,66.1121940545044));
#143965=CARTESIAN_POINT('Ctrl Pts',(86.1183997985764,13.5969822544608,66.1229259772511));
#143966=CARTESIAN_POINT('Ctrl Pts',(86.0818331447479,13.5956956932831,66.1322013692844));
#143967=CARTESIAN_POINT('Ctrl Pts',(86.0457393733944,13.5950585696962,66.1398887501012));
#143968=CARTESIAN_POINT('Ctrl Pts',(86.0102558429037,13.5950708837,66.1461501490856));
#143969=CARTESIAN_POINT('Origin',(88.2116008665994,13.9725941882181,64.234862063316));
#143970=CARTESIAN_POINT('Origin',(88.0541760202691,-0.499074165591386,63.341979795825));
#143971=CARTESIAN_POINT('',(87.1036300406178,13.9995834170875,63.709936145709));
#143972=CARTESIAN_POINT('Origin',(87.0693682672991,-0.499074165591386,63.515627973492));
#143973=CARTESIAN_POINT('Origin',(88.088437795226,13.9995833743814,63.5362879772457));
#143974=CARTESIAN_POINT('Origin',(88.0778048294691,9.5,63.475985431442));
#143975=CARTESIAN_POINT('',(86.3873398105787,11.4325417365447,59.6476527159751));
#143976=CARTESIAN_POINT('Ctrl Pts',(86.3873923039748,11.4323977449269,59.6479500913008));
#143977=CARTESIAN_POINT('Ctrl Pts',(86.4137108606564,11.7502480376137,59.7972100433247));
#143978=CARTESIAN_POINT('Ctrl Pts',(86.4760319983401,12.3203221675509,60.1506507663566));
#143979=CARTESIAN_POINT('Ctrl Pts',(86.6035424971191,13.05672232746,60.87379879423));
#143980=CARTESIAN_POINT('Ctrl Pts',(86.7559255690891,13.60185460728,61.7380059407));
#143981=CARTESIAN_POINT('Ctrl Pts',(86.9268053206991,13.93453843381,62.70711391189));
#143982=CARTESIAN_POINT('Ctrl Pts',(87.0436770949691,14.00347098775,63.369924833184));
#143983=CARTESIAN_POINT('Ctrl Pts',(87.1036300406291,13.99958341709,63.709936145707));
#143984=CARTESIAN_POINT('',(87.2158423658651,11.8669336587046,58.5875534023177));
#143985=CARTESIAN_POINT('Ctrl Pts',(87.2158423505991,11.86693347431,58.58755331574));
#143986=CARTESIAN_POINT('Ctrl Pts',(86.9577709596166,11.8673938453636,58.6322628228547));
#143987=CARTESIAN_POINT('Ctrl Pts',(86.7183367978951,11.8209912942895,58.7733653215963));
#143988=CARTESIAN_POINT('Ctrl Pts',(86.4118284068604,11.6615314736288,59.1669451161913));
#143989=CARTESIAN_POINT('Ctrl Pts',(86.3465703878581,11.5494863410242,59.4169490701672));
#143990=CARTESIAN_POINT('Ctrl Pts',(86.3873396949891,11.4325417044808,59.6476527211807));
#143991=CARTESIAN_POINT('Origin',(88.0778048294691,9.5,63.475985431442));
#143992=CARTESIAN_POINT('Origin',(58.0359414686091,9.5,68.773176492713));
#143993=CARTESIAN_POINT('',(91.0401366110177,11.8600632412174,57.9099602235744));
#143994=CARTESIAN_POINT('Ctrl Pts',(91.0790830817097,12.2828346383176,58.1314725547239));
#143995=CARTESIAN_POINT('Ctrl Pts',(91.0655561192021,12.1563659248288,58.0571151382804));
#143996=CARTESIAN_POINT('Ctrl Pts',(91.0534674480175,12.0155874078506,57.9833514930887));
#143997=CARTESIAN_POINT('Ctrl Pts',(91.0401366110177,11.8600632412174,57.9099602235744));
#143998=CARTESIAN_POINT('Ctrl Pts',(87.2158423505991,11.86693347431,58.58755331574));
#143999=CARTESIAN_POINT('Ctrl Pts',(88.4907931887827,11.8652382567572,58.3629426652979));
#144000=CARTESIAN_POINT('Ctrl Pts',(89.7656022238009,11.8639324281498,58.1375278091412));
#144001=CARTESIAN_POINT('Ctrl Pts',(91.0401366110177,11.8600632412174,57.9099602235744));
#144002=CARTESIAN_POINT('Origin',(91.9465816191691,-0.0433423696914158,
83.0870666032));
#144003=CARTESIAN_POINT('',(90.9047766966899,10.0691253898985,57.142294634787));
#144004=CARTESIAN_POINT('',(90.6242545431152,4.0210988023396,55.5521021866124));
#144005=CARTESIAN_POINT('Ctrl Pts',(90.904778401325,10.0691210019042,57.1423041413024));
#144006=CARTESIAN_POINT('Ctrl Pts',(90.8376715128848,9.09973890145265,56.7649981889273));
#144007=CARTESIAN_POINT('Ctrl Pts',(90.7811184881318,8.10415089350686,56.4431269592421));
#144008=CARTESIAN_POINT('Ctrl Pts',(90.6876392936001,6.08161709929453,55.9116332521325));
#144009=CARTESIAN_POINT('Ctrl Pts',(90.6508535215351,5.05587121367757,55.7027270401013));
#144010=CARTESIAN_POINT('Ctrl Pts',(90.6242545431152,4.0210988023396,55.5521021866125));
#144011=CARTESIAN_POINT('',(90.9921937685691,11.26993034099,57.63983708294));
#144012=CARTESIAN_POINT('Ctrl Pts',(90.9921937685691,11.26993034099,57.63983708294));
#144013=CARTESIAN_POINT('Ctrl Pts',(90.9607404151601,10.8632738684627,57.4621582006354));
#144014=CARTESIAN_POINT('Ctrl Pts',(90.9324253490825,10.4675402739369,57.2966575608245));
#144015=CARTESIAN_POINT('Ctrl Pts',(90.9047784163434,10.0691212184121,57.1423042252401));
#144016=CARTESIAN_POINT('Ctrl Pts',(91.0401366110177,11.8600632412174,57.9099602235744));
#144017=CARTESIAN_POINT('Ctrl Pts',(91.0254325534448,11.6817810703298,57.8215495147345));
#144018=CARTESIAN_POINT('Ctrl Pts',(91.008241628779,11.4857992440152,57.7340837415959));
#144019=CARTESIAN_POINT('Ctrl Pts',(90.9921937685691,11.26993034099,57.63983708294));
#144020=CARTESIAN_POINT('',(87.0625519269491,9.81028963511501,57.71791233337));
#144021=CARTESIAN_POINT('Origin',(91.5481551204691,-0.0433423696914658,
83.15731994474));
#144022=CARTESIAN_POINT('Ctrl Pts',(87.0625519269491,9.81028963511501,57.71791233337));
#144023=CARTESIAN_POINT('Ctrl Pts',(87.9398460791424,9.01004234588953,57.2538665845636));
#144024=CARTESIAN_POINT('Ctrl Pts',(88.6726439433507,8.12875357581062,56.8262866069459));
#144025=CARTESIAN_POINT('Ctrl Pts',(89.8570639140029,6.19929588766557,56.0883896079714));
#144026=CARTESIAN_POINT('Ctrl Pts',(90.3086910869141,5.15099973035466,55.778101303947));
#144027=CARTESIAN_POINT('Ctrl Pts',(90.6242545337037,4.02109881283824,55.5521021898692));
#144028=CARTESIAN_POINT('Ctrl Pts',(83.5527963632191,7.79551024574101,56.39696245495));
#144029=CARTESIAN_POINT('Ctrl Pts',(84.6832114812291,8.33549466069001,57.18456946643));
#144030=CARTESIAN_POINT('Ctrl Pts',(85.9062799740191,9.11477790243301,57.67842771583));
#144031=CARTESIAN_POINT('Ctrl Pts',(87.0598604213891,10.03501468075,57.80394780523));
#144032=CARTESIAN_POINT('Ctrl Pts',(83.9461301143991,7.49859304613501,56.27865761436));
#144033=CARTESIAN_POINT('Ctrl Pts',(85.1013709827991,8.01223740062101,57.02294274994));
#144034=CARTESIAN_POINT('Ctrl Pts',(86.3505790285991,8.74968408384501,57.47095990997));
#144035=CARTESIAN_POINT('Ctrl Pts',(87.5310943091691,9.61958516366902,57.5556017672));
#144036=CARTESIAN_POINT('Ctrl Pts',(84.6734906132591,6.86959461361001,56.04876303691));
#144037=CARTESIAN_POINT('Ctrl Pts',(85.8693472222591,7.32712499929101,56.71036553051));
#144038=CARTESIAN_POINT('Ctrl Pts',(87.1601981332091,7.97782666496401,57.07216083468));
#144039=CARTESIAN_POINT('Ctrl Pts',(88.3840197380691,8.74413048764801,57.08058953316));
#144040=CARTESIAN_POINT('Ctrl Pts',(85.6006910643591,5.80441907889401,55.7287923738));
#144041=CARTESIAN_POINT('Ctrl Pts',(86.8339936590691,6.17114924616401,56.28135323536));
#144042=CARTESIAN_POINT('Ctrl Pts',(88.1602935371691,6.68693631322101,56.53299296536));
#144043=CARTESIAN_POINT('Ctrl Pts',(89.4222061602691,7.29363942440101,56.44631864302));
#144044=CARTESIAN_POINT('Ctrl Pts',(86.3890436286191,4.56793334804501,55.43379604209));
#144045=CARTESIAN_POINT('Ctrl Pts',(87.6400403009691,4.83930736953001,55.89394630833));
#144046=CARTESIAN_POINT('Ctrl Pts',(88.9796858299691,5.21750983688301,56.05603070301));
#144047=CARTESIAN_POINT('Ctrl Pts',(90.2577115618691,5.66224725175901,55.89495734691));
#144048=CARTESIAN_POINT('Ctrl Pts',(86.7846654732391,3.65544465457401,55.27474745921));
#144049=CARTESIAN_POINT('Ctrl Pts',(88.0375966273691,3.86480378841501,55.68903466726));
#144050=CARTESIAN_POINT('Ctrl Pts',(89.3757879463691,4.15550040108601,55.80860463891));
#144051=CARTESIAN_POINT('Ctrl Pts',(90.6540092174691,4.49744425651901,55.61381970811));
#144052=CARTESIAN_POINT('Ctrl Pts',(86.9516944429091,3.16130406753901,55.20620234028));
#144053=CARTESIAN_POINT('Ctrl Pts',(88.2044408468691,3.33962332755001,55.60142198926));
#144054=CARTESIAN_POINT('Ctrl Pts',(89.5408894909691,3.58684077310001,55.70363976371));
#144055=CARTESIAN_POINT('Ctrl Pts',(90.8181034903691,3.87767846552801,55.49540382885));
#144056=CARTESIAN_POINT('',(87.0452063053445,3.32468194401047,55.2706145694237));
#144057=CARTESIAN_POINT('Ctrl Pts',(87.045203902867,3.32467973942797,55.2706236824706));
#144058=CARTESIAN_POINT('Ctrl Pts',(87.0470012523809,3.86784541765893,55.4025787775118));
#144059=CARTESIAN_POINT('Ctrl Pts',(87.0490460696036,4.40136020801294,55.5629627912764));
#144060=CARTESIAN_POINT('Ctrl Pts',(87.0510069518472,4.9241759395484,55.741622912552));
#144061=CARTESIAN_POINT('Ctrl Pts',(87.0511357651415,4.9585204887604,55.7533593637665));
#144062=CARTESIAN_POINT('Ctrl Pts',(87.0512642162768,4.99281886767013,55.7651746825583));
#144063=CARTESIAN_POINT('Ctrl Pts',(87.0513922869735,5.02707185220943,55.7770659468569));
#144064=CARTESIAN_POINT('Ctrl Pts',(87.0531964624245,5.50960529212154,55.9445822303015));
#144065=CARTESIAN_POINT('Ctrl Pts',(87.0549245412221,5.98313101850152,56.1271703607983));
#144066=CARTESIAN_POINT('Ctrl Pts',(87.0565238510531,6.44982066766169,56.3166620251401));
#144067=CARTESIAN_POINT('Ctrl Pts',(87.0567662711181,6.5205605161276,56.3453847783557));
#144068=CARTESIAN_POINT('Ctrl Pts',(87.0570057326289,6.59114329985223,56.3742661462039));
#144069=CARTESIAN_POINT('Ctrl Pts',(87.0572418456943,6.66157985193077,56.403277172837));
#144070=CARTESIAN_POINT('Ctrl Pts',(87.058513573033,7.04095779438498,56.5595333107053));
#144071=CARTESIAN_POINT('Ctrl Pts',(87.0596934926687,7.41609585314038,56.7195520426998));
#144072=CARTESIAN_POINT('Ctrl Pts',(87.0607150048372,7.78868443971465,56.8788072211256));
#144073=CARTESIAN_POINT('Ctrl Pts',(87.061816906091,8.19059431738695,57.0505951705856));
#144074=CARTESIAN_POINT('Ctrl Pts',(87.0627344512309,8.58953771072732,57.2214945859138));
#144075=CARTESIAN_POINT('Ctrl Pts',(87.0630038488618,8.98798817633719,57.3865187845672));
#144076=CARTESIAN_POINT('Ctrl Pts',(87.0631892513137,9.26220622729475,57.50009027719));
#144077=CARTESIAN_POINT('Ctrl Pts',(87.0630676703773,9.53619078362226,57.6108791136097));
#144078=CARTESIAN_POINT('Ctrl Pts',(87.0624604019528,9.81049105390748,57.7173931076103));
#144079=CARTESIAN_POINT('Origin',(88.9840679110593,4.82687630561811,49.4062655211528));
#144080=CARTESIAN_POINT('Ctrl Pts',(86.2777587182191,3.35797480132401,55.0378852179));
#144081=CARTESIAN_POINT('Ctrl Pts',(87.6910580236691,3.55694831838901,55.61191127816));
#144082=CARTESIAN_POINT('Ctrl Pts',(89.2470251821691,3.86322784531101,55.79788947715));
#144083=CARTESIAN_POINT('Ctrl Pts',(90.7231331745691,4.23364950808901,55.56595754335));
#144084=CARTESIAN_POINT('Ctrl Pts',(86.7049180588991,2.24396285722701,54.88675785712));
#144085=CARTESIAN_POINT('Ctrl Pts',(88.1203558938691,2.36828606915101,55.40277505789));
#144086=CARTESIAN_POINT('Ctrl Pts',(89.6721739084691,2.55739749999101,55.53501604492));
#144087=CARTESIAN_POINT('Ctrl Pts',(91.1466488631691,2.78622655700001,55.26249917316));
#144088=CARTESIAN_POINT('Ctrl Pts',(86.9126052467991,1.05468974025801,54.80544650431));
#144089=CARTESIAN_POINT('Ctrl Pts',(88.3228401741691,1.11258841309801,55.294362315));
#144090=CARTESIAN_POINT('Ctrl Pts',(89.8650971183691,1.20112353795701,55.40385472609));
#144091=CARTESIAN_POINT('Ctrl Pts',(91.3314350643691,1.30850424140801,55.11623041902));
#144092=CARTESIAN_POINT('Ctrl Pts',(86.8937434252391,-0.150524780926486,
54.8128006371));
#144093=CARTESIAN_POINT('Ctrl Pts',(88.3044266143691,-0.158795700165486,
55.30418203856));
#144094=CARTESIAN_POINT('Ctrl Pts',(89.8475225660691,-0.171437606626586,
55.41575356859));
#144095=CARTESIAN_POINT('Ctrl Pts',(91.3145709684691,-0.186767340196186,
55.1295192676));
#144096=CARTESIAN_POINT('',(91.1670701462358,2.74307740674274E-14,55.1562792695813));
#144097=CARTESIAN_POINT('Ctrl Pts',(90.6242676274951,4.02108764649613,55.5521764045675));
#144098=CARTESIAN_POINT('Ctrl Pts',(90.6813389532947,3.8179674433382,55.5116429418745));
#144099=CARTESIAN_POINT('Ctrl Pts',(90.7332711723362,3.61452700426379,55.4743452737089));
#144100=CARTESIAN_POINT('Ctrl Pts',(90.7804179111772,3.41093104822288,55.440220608944));
#144101=CARTESIAN_POINT('Ctrl Pts',(90.8278289816426,3.20619361662901,55.4059046217613));
#144102=CARTESIAN_POINT('Ctrl Pts',(90.8704007345699,3.00129904715451,55.374797431572));
#144103=CARTESIAN_POINT('Ctrl Pts',(90.9084408089441,2.79640895953868,55.346841452405));
#144104=CARTESIAN_POINT('Ctrl Pts',(90.9217531255787,2.72470663596276,55.3370581159467));
#144105=CARTESIAN_POINT('Ctrl Pts',(90.9345099925611,2.65300480010805,55.3276607516866));
#144106=CARTESIAN_POINT('Ctrl Pts',(90.9467231118361,2.58131016892631,55.3186470337802));
#144107=CARTESIAN_POINT('Ctrl Pts',(90.9795215444716,2.38877364502865,55.2944406199317));
#144108=CARTESIAN_POINT('Ctrl Pts',(91.0084013120712,2.19628946790016,55.2730008323369));
#144109=CARTESIAN_POINT('Ctrl Pts',(91.0335604077023,2.0039904930509,55.254286091841));
#144110=CARTESIAN_POINT('Ctrl Pts',(91.0605575797341,1.79764251529882,55.2342040874594));
#144111=CARTESIAN_POINT('Ctrl Pts',(91.0832710805389,1.59150787532994,55.2172598837242));
#144112=CARTESIAN_POINT('Ctrl Pts',(91.1018956986807,1.38574194395299,55.2034051674291));
#144113=CARTESIAN_POINT('Ctrl Pts',(91.1205387383242,1.17977249068807,55.1895367475145));
#144114=CARTESIAN_POINT('Ctrl Pts',(91.1350847496725,0.974172664288115,
55.1787639986015));
#144115=CARTESIAN_POINT('Ctrl Pts',(91.1456782134625,0.769086615773664,
55.1710404532243));
#144116=CARTESIAN_POINT('Ctrl Pts',(91.1562761152521,0.563914649017109,
55.1633136721642));
#144117=CARTESIAN_POINT('Ctrl Pts',(91.1629180943347,0.359257095879952,
55.1586386921846));
#144118=CARTESIAN_POINT('Ctrl Pts',(91.165698781784,0.155243665858008,55.1569701398367));
#144119=CARTESIAN_POINT('Ctrl Pts',(91.1664046750334,0.103453701808425,
55.1565465683781));
#144120=CARTESIAN_POINT('Ctrl Pts',(91.1668614876952,0.0517051643952373,
55.1563167434454));
#144121=CARTESIAN_POINT('Ctrl Pts',(91.1670702628135,2.73247007625336E-14,
55.156279930759));
#144122=CARTESIAN_POINT('',(87.0379664172709,2.17389847372088E-10,54.8607146728376));
#144123=CARTESIAN_POINT('Ctrl Pts',(87.0379678287862,4.10407994795547E-10,
54.8607103703767));
#144124=CARTESIAN_POINT('Ctrl Pts',(87.0379693004997,0.20239753568915,54.8607199332154));
#144125=CARTESIAN_POINT('Ctrl Pts',(87.0380265697462,0.407113829529953,
54.865362440369));
#144126=CARTESIAN_POINT('Ctrl Pts',(87.0381782738253,0.613853290402161,
54.8748935232933));
#144127=CARTESIAN_POINT('Ctrl Pts',(87.0382727664481,0.742626056552804,
54.8808301930873));
#144128=CARTESIAN_POINT('Ctrl Pts',(87.0384036832572,0.872182872546045,
54.8886637295171));
#144129=CARTESIAN_POINT('Ctrl Pts',(87.0385782393398,1.00244245311521,54.8984581722552));
#144130=CARTESIAN_POINT('Ctrl Pts',(87.038856657565,1.21020743434017,54.9140803798709));
#144131=CARTESIAN_POINT('Ctrl Pts',(87.0392469253613,1.41976219000755,54.9346923733824));
#144132=CARTESIAN_POINT('Ctrl Pts',(87.03974221153,1.63084475620316,54.9604067657937));
#144133=CARTESIAN_POINT('Ctrl Pts',(87.0402076100815,1.82918972676854,54.9845694453454));
#144134=CARTESIAN_POINT('Ctrl Pts',(87.0407656988976,2.02888353522731,55.0132373241063));
#144135=CARTESIAN_POINT('Ctrl Pts',(87.0413993099936,2.22967027819263,55.0464953442303));
#144136=CARTESIAN_POINT('Ctrl Pts',(87.0420220231652,2.42700354829937,55.0791813362008));
#144137=CARTESIAN_POINT('Ctrl Pts',(87.0427179229967,2.62539230935319,55.1163025646978));
#144138=CARTESIAN_POINT('Ctrl Pts',(87.0434324375699,2.82460332828506,55.1577725266321));
#144139=CARTESIAN_POINT('Ctrl Pts',(87.0440284707663,2.9907810170511,55.1923659063779));
#144140=CARTESIAN_POINT('Ctrl Pts',(87.044637213594,3.15753036322419,55.2299849453235));
#144141=CARTESIAN_POINT('Ctrl Pts',(87.0452197681563,3.32469429787419,55.2705635024578));
#144142=CARTESIAN_POINT('Origin',(89.5099641414739,-2.03747057816781E-10,
48.9689653069594));
#144143=CARTESIAN_POINT('Ctrl Pts',(86.8937713403091,0.150278927427014,
54.81280807796));
#144144=CARTESIAN_POINT('Ctrl Pts',(88.3043999218691,0.158534897272514,
55.3042706166));
#144145=CARTESIAN_POINT('Ctrl Pts',(89.8475194425691,0.171158442280014,
55.41552889153));
#144146=CARTESIAN_POINT('Ctrl Pts',(91.3145776951691,0.186460507929914,
55.12953401502));
#144147=CARTESIAN_POINT('Ctrl Pts',(86.9126943758391,-1.06234500207499,
54.80543698782));
#144148=CARTESIAN_POINT('Ctrl Pts',(88.3228790529691,-1.12065140134899,
55.29442473537));
#144149=CARTESIAN_POINT('Ctrl Pts',(89.8651634112691,-1.20984047105699,
55.40359516778));
#144150=CARTESIAN_POINT('Ctrl Pts',(91.3315154389691,-1.31797588386699,
55.11620079281));
#144151=CARTESIAN_POINT('Ctrl Pts',(86.7024783203091,-2.25075885387899,
54.88765019828));
#144152=CARTESIAN_POINT('Ctrl Pts',(88.1178555459691,-2.37550823105599,
55.40408429379));
#144153=CARTESIAN_POINT('Ctrl Pts',(89.6697334134691,-2.56535408039399,
55.53630712185));
#144154=CARTESIAN_POINT('Ctrl Pts',(91.1442381655691,-2.79499085550699,
55.26426627484));
#144155=CARTESIAN_POINT('Ctrl Pts',(86.2773845990691,-3.35901852522699,
55.03803802306));
#144156=CARTESIAN_POINT('Ctrl Pts',(87.6906204733691,-3.55803150344899,
55.61220513576));
#144157=CARTESIAN_POINT('Ctrl Pts',(89.2466200909691,-3.86449453312799,
55.79788968037));
#144158=CARTESIAN_POINT('Ctrl Pts',(90.7227405050691,-4.23499951536299,
55.56626117546));
#144159=CARTESIAN_POINT('',(90.6242675720478,-4.0209956755633,55.5521118754408));
#144160=CARTESIAN_POINT('Ctrl Pts',(91.1670701073691,2.7354895961722E-14,
55.15627904919));
#144161=CARTESIAN_POINT('Ctrl Pts',(91.165849317076,-0.34243594626333,55.1564952164306));
#144162=CARTESIAN_POINT('Ctrl Pts',(91.1540382483519,-0.685319034794855,
55.1651207635041));
#144163=CARTESIAN_POINT('Ctrl Pts',(91.1196950287164,-1.19945881862615,
55.1907739782479));
#144164=CARTESIAN_POINT('Ctrl Pts',(91.105470345645,-1.37080633281857,55.2014442692401));
#144165=CARTESIAN_POINT('Ctrl Pts',(91.0798226281247,-1.62765967198077,
55.220642109171));
#144166=CARTESIAN_POINT('Ctrl Pts',(91.0659205480108,-1.75604424626546,
55.2310391461268));
#144167=CARTESIAN_POINT('Ctrl Pts',(91.0503689410442,-1.88434237146833,
55.2426360874994));
#144168=CARTESIAN_POINT('Ctrl Pts',(91.0396307218966,-1.96985259603912,
55.250634346356));
#144169=CARTESIAN_POINT('Ctrl Pts',(91.0337889985745,-2.01473568195959,
55.2549805002222));
#144170=CARTESIAN_POINT('Ctrl Pts',(90.9410678105965,-2.7048171237868,55.3238766186337));
#144171=CARTESIAN_POINT('Ctrl Pts',(90.8097152049346,-3.3619013328331,55.4205634794744));
#144172=CARTESIAN_POINT('Ctrl Pts',(90.6242620411691,-4.02100037299999,
55.55208048089));
#144173=CARTESIAN_POINT('',(87.0451990682794,-3.32463143800401,55.2706077778965));
#144174=CARTESIAN_POINT('Ctrl Pts',(87.0452086535362,-3.32464023403444,
55.2705714208367));
#144175=CARTESIAN_POINT('Ctrl Pts',(87.044512655429,-3.12434940334929,55.2219520465534));
#144176=CARTESIAN_POINT('Ctrl Pts',(87.0437782589915,-2.92464886642339,
55.1775771565754));
#144177=CARTESIAN_POINT('Ctrl Pts',(87.0430717007898,-2.72580575381143,
55.1375605048055));
#144178=CARTESIAN_POINT('Ctrl Pts',(87.0424604951936,-2.55379724423082,
55.1029442460931));
#144179=CARTESIAN_POINT('Ctrl Pts',(87.0418699116625,-2.38242948815377,
55.071588697763));
#144180=CARTESIAN_POINT('Ctrl Pts',(87.0413346239677,-2.21185108387118,
55.0435494536918));
#144181=CARTESIAN_POINT('Ctrl Pts',(87.0407234368002,-2.01708603929369,
55.0115344712302));
#144182=CARTESIAN_POINT('Ctrl Pts',(87.0401843291019,-1.82335088020513,
54.9838418574831));
#144183=CARTESIAN_POINT('Ctrl Pts',(87.039732739701,-1.63088300680562,54.9603934382341));
#144184=CARTESIAN_POINT('Ctrl Pts',(87.0392228290388,-1.41355855107868,
54.9339167340397));
#144185=CARTESIAN_POINT('Ctrl Pts',(87.0388247135594,-1.1978503828135,54.9128513309689));
#144186=CARTESIAN_POINT('Ctrl Pts',(87.0385455377253,-0.984048864472286,
54.8970736810246));
#144187=CARTESIAN_POINT('Ctrl Pts',(87.0382733538861,-0.775602032849812,
54.8816911843666));
#144188=CARTESIAN_POINT('Ctrl Pts',(87.0381138462719,-0.568968001308234,
54.8713330126585));
#144189=CARTESIAN_POINT('Ctrl Pts',(87.0380333744037,-0.364473437435225,
54.865729131077));
#144190=CARTESIAN_POINT('Ctrl Pts',(87.0379852570288,-0.242197891955986,
54.8623783443167));
#144191=CARTESIAN_POINT('Ctrl Pts',(87.0379651969979,-0.120686245134875,
54.8607276135635));
#144192=CARTESIAN_POINT('Ctrl Pts',(87.0379642136838,4.26840621093993E-10,
54.8607213896952));
#144193=CARTESIAN_POINT('Origin',(88.9855508168953,-4.82568011021053,49.4111666499231));
#144194=CARTESIAN_POINT('Ctrl Pts',(86.9516806969691,-3.16128829937699,
55.20619343277));
#144195=CARTESIAN_POINT('Ctrl Pts',(88.2046044567691,-3.33963640945299,
55.60147925581));
#144196=CARTESIAN_POINT('Ctrl Pts',(89.5412550807691,-3.58690525771299,
55.70367918435));
#144197=CARTESIAN_POINT('Ctrl Pts',(90.8186331109691,-3.87780431688299,
55.49533239395));
#144198=CARTESIAN_POINT('Ctrl Pts',(86.3310017513891,-4.99858829213699,
55.46112141282));
#144199=CARTESIAN_POINT('Ctrl Pts',(87.5848676480691,-5.29218632210199,
55.92705497751));
#144200=CARTESIAN_POINT('Ctrl Pts',(88.9282678155691,-5.70086660722399,
56.09343319582));
#144201=CARTESIAN_POINT('Ctrl Pts',(90.2096509505691,-6.18149989797999,
55.93471566337));
#144202=CARTESIAN_POINT('Ctrl Pts',(85.1490259917191,-6.59074061544199,
55.91688020941));
#144203=CARTESIAN_POINT('Ctrl Pts',(86.3803940981591,-7.02390396003999,
56.52876345794));
#144204=CARTESIAN_POINT('Ctrl Pts',(87.7097804104691,-7.63353048324999,
56.8365779079));
#144205=CARTESIAN_POINT('Ctrl Pts',(88.9728619095691,-8.34964142880199,
56.79608157395));
#144206=CARTESIAN_POINT('Ctrl Pts',(83.5523400802591,-7.79584216569499,
56.39708965395));
#144207=CARTESIAN_POINT('Ctrl Pts',(84.6828934797891,-8.33593481762399,
57.18486396867));
#144208=CARTESIAN_POINT('Ctrl Pts',(85.9061266288191,-9.11541493494999,
57.67880573437));
#144209=CARTESIAN_POINT('Ctrl Pts',(87.0598268116091,-10.03588562153,57.80428409672));
#144210=CARTESIAN_POINT('',(87.0625766316463,-9.81041847342618,57.7173854406919));
#144211=CARTESIAN_POINT('Ctrl Pts',(87.0625766316463,-9.81041847342618,
57.7173854406918));
#144212=CARTESIAN_POINT('Ctrl Pts',(87.0628390720482,-9.72800334949134,
57.6853973399913));
#144213=CARTESIAN_POINT('Ctrl Pts',(87.0630165460847,-9.64183968033886,
57.6515805060854));
#144214=CARTESIAN_POINT('Ctrl Pts',(87.0631680142214,-9.5518831048575,57.6158526863386));
#144215=CARTESIAN_POINT('Ctrl Pts',(87.0633173044982,-9.46321995533027,
57.580638573223));
#144216=CARTESIAN_POINT('Ctrl Pts',(87.0634412649436,-9.37087237149314,
57.543567861564));
#144217=CARTESIAN_POINT('Ctrl Pts',(87.0635591572122,-9.27480601330731,
57.5045950508041));
#144218=CARTESIAN_POINT('Ctrl Pts',(87.063676277597,-9.17936863662741,57.4658774092592));
#144219=CARTESIAN_POINT('Ctrl Pts',(87.0637873718588,-9.08026122963494,
57.4252823285718));
#144220=CARTESIAN_POINT('Ctrl Pts',(87.0638750591467,-8.9774553211851,57.3828008206487));
#144221=CARTESIAN_POINT('Ctrl Pts',(87.0639619897901,-8.87553651420938,
57.3406858812318));
#144222=CARTESIAN_POINT('Ctrl Pts',(87.0640258614301,-8.76998300272115,
57.2967168269121));
#144223=CARTESIAN_POINT('Ctrl Pts',(87.0640146935108,-8.66076881904943,
57.2509220047819));
#144224=CARTESIAN_POINT('Ctrl Pts',(87.0640067257105,-8.58284948796222,
57.218249491124));
#144225=CARTESIAN_POINT('Ctrl Pts',(87.0639598370757,-8.50306686636715,
57.184648402424));
#144226=CARTESIAN_POINT('Ctrl Pts',(87.063844289737,-8.42141094988714,57.1501411036244));
#144227=CARTESIAN_POINT('Ctrl Pts',(87.0636971541048,-8.31743196586373,
57.1062002108483));
#144228=CARTESIAN_POINT('Ctrl Pts',(87.0634755557133,-8.21039512883709,
57.0607768776444));
#144229=CARTESIAN_POINT('Ctrl Pts',(87.0632118349515,-8.10023332471427,
57.0139242727969));
#144230=CARTESIAN_POINT('Ctrl Pts',(87.0629538134131,-7.99245220816343,
56.9680841914367));
#144231=CARTESIAN_POINT('Ctrl Pts',(87.0626555217958,-7.88168000204142,
56.9208760258635));
#144232=CARTESIAN_POINT('Ctrl Pts',(87.0623152977027,-7.76783902226488,
56.8723843235867));
#144233=CARTESIAN_POINT('Ctrl Pts',(87.0620908174656,-7.69272661651815,
56.8403894442039));
#144234=CARTESIAN_POINT('Ctrl Pts',(87.0618474375089,-7.61627795303887,
56.8078365028245));
#144235=CARTESIAN_POINT('Ctrl Pts',(87.0615765299235,-7.53846614864338,
56.7747580743624));
#144236=CARTESIAN_POINT('Ctrl Pts',(87.0611942931426,-7.42867766273656,
56.728086099522));
#144237=CARTESIAN_POINT('Ctrl Pts',(87.0607724680966,-7.31617500558751,
56.6803657943976));
#144238=CARTESIAN_POINT('Ctrl Pts',(87.0603299026845,-7.20087200964981,
56.6317176985142));
#144239=CARTESIAN_POINT('Ctrl Pts',(87.0601349919148,-7.15009127741691,
56.6102925316257));
#144240=CARTESIAN_POINT('Ctrl Pts',(87.0599356548905,-7.09876703602993,
56.5886877983236));
#144241=CARTESIAN_POINT('Ctrl Pts',(87.0597314860299,-7.04689015678793,
56.5669156204394));
#144242=CARTESIAN_POINT('Ctrl Pts',(87.0593976081587,-6.96205576063497,
56.5313115210655));
#144243=CARTESIAN_POINT('Ctrl Pts',(87.0590537502245,-6.87574472053487,
56.4952595532075));
#144244=CARTESIAN_POINT('Ctrl Pts',(87.0587059254545,-6.78791548485091,
56.4588226097982));
#144245=CARTESIAN_POINT('Ctrl Pts',(87.0585320130695,-6.74400086700893,
56.4406041380935));
#144246=CARTESIAN_POINT('Ctrl Pts',(87.0583570948179,-6.699706629326,56.4222895954189));
#144247=CARTESIAN_POINT('Ctrl Pts',(87.0581820490815,-6.65502710214539,
56.4038879243479));
#144248=CARTESIAN_POINT('Ctrl Pts',(87.0580945262132,-6.63268733855508,
56.3946870888124));
#144249=CARTESIAN_POINT('Ctrl Pts',(87.0580069704471,-6.61025124788037,
56.3854644828236));
#144250=CARTESIAN_POINT('Ctrl Pts',(87.057919492524,-6.58771809232852,56.3762212956712));
#144251=CARTESIAN_POINT('Ctrl Pts',(87.0578487179328,-6.56948749407615,
56.3687430340865));
#144252=CARTESIAN_POINT('Ctrl Pts',(87.0577762649015,-6.55023610058555,
56.3608598848097));
#144253=CARTESIAN_POINT('Ctrl Pts',(87.0577058929201,-6.53228718790687,
56.3535227476336));
#144254=CARTESIAN_POINT('Ctrl Pts',(87.0576892846071,-6.52805111050587,
56.3517911284801));
#144255=CARTESIAN_POINT('Ctrl Pts',(87.0576729901796,-6.52388748793224,
56.3500898405514));
#144256=CARTESIAN_POINT('Ctrl Pts',(87.0576574112025,-6.51982669637165,
56.3484312386392));
#144257=CARTESIAN_POINT('Ctrl Pts',(87.0571374689694,-6.38429937495421,
56.2930760520697));
#144258=CARTESIAN_POINT('Ctrl Pts',(87.0566006156764,-6.2515905165016,56.2396059531338));
#144259=CARTESIAN_POINT('Ctrl Pts',(87.05604921051,-6.12167918640636,56.1881084907986));
#144260=CARTESIAN_POINT('Ctrl Pts',(87.0554872516434,-5.98928139932232,
56.1356253852171));
#144261=CARTESIAN_POINT('Ctrl Pts',(87.0549099356614,-5.85978891486309,
56.0851907730958));
#144262=CARTESIAN_POINT('Ctrl Pts',(87.0543251722186,-5.73321454309557,
56.0368560060033));
#144263=CARTESIAN_POINT('Ctrl Pts',(87.0537357786718,-5.6056379669076,55.9881385285993));
#144264=CARTESIAN_POINT('Ctrl Pts',(87.0531385664979,-5.48102569214467,
55.9415538436113));
#144265=CARTESIAN_POINT('Ctrl Pts',(87.052550870209,-5.35943007569011,55.8971192626733));
#144266=CARTESIAN_POINT('Ctrl Pts',(87.0519558777,-5.23632485570613,55.8521330286235));
#144267=CARTESIAN_POINT('Ctrl Pts',(87.0513703909122,-5.11631150324506,
55.8093502210095));
#144268=CARTESIAN_POINT('Ctrl Pts',(87.0508256785423,-4.99948723236905,
55.7687590932993));
#144269=CARTESIAN_POINT('Ctrl Pts',(87.0503358700086,-4.89443816795456,
55.7322593149784));
#144270=CARTESIAN_POINT('Ctrl Pts',(87.0498791272192,-4.79196827286971,
55.6975310760738));
#144271=CARTESIAN_POINT('Ctrl Pts',(87.0494893659084,-4.6921783257891,55.6645495917059));
#144272=CARTESIAN_POINT('Ctrl Pts',(87.0490528360166,-4.58041429584728,
55.6276105641358));
#144273=CARTESIAN_POINT('Ctrl Pts',(87.0486704434854,-4.47206232451012,
55.5928728915689));
#144274=CARTESIAN_POINT('Ctrl Pts',(87.0483243200076,-4.36712983835204,
55.5602093885637));
#144275=CARTESIAN_POINT('Ctrl Pts',(87.0479620947937,-4.25731587116184,
55.5260263726202));
#144276=CARTESIAN_POINT('Ctrl Pts',(87.047639371313,-4.15124699665592,55.4941147704494));
#144277=CARTESIAN_POINT('Ctrl Pts',(87.0473383877036,-4.0489891864447,55.4643215436082));
#144278=CARTESIAN_POINT('Ctrl Pts',(87.0470281082852,-3.94357316747328,
55.4336081598636));
#144279=CARTESIAN_POINT('Ctrl Pts',(87.0467408565464,-3.84220755551895,
55.4051457763424));
#144280=CARTESIAN_POINT('Ctrl Pts',(87.0464623874826,-3.74502133901434,
55.3787629182717));
#144281=CARTESIAN_POINT('Ctrl Pts',(87.0461680367163,-3.64229237903069,
55.3508753878329));
#144282=CARTESIAN_POINT('Ctrl Pts',(87.0458836085151,-3.5442333332799,55.3253110722094));
#144283=CARTESIAN_POINT('Ctrl Pts',(87.0455979336287,-3.45105532541971,
55.3018673545319));
#144284=CARTESIAN_POINT('Ctrl Pts',(87.0454654881388,-3.40785584417653,
55.2909983043629));
#144285=CARTESIAN_POINT('Ctrl Pts',(87.0453328410789,-3.36570630287924,
55.2805850943015));
#144286=CARTESIAN_POINT('Ctrl Pts',(87.0451990682794,-3.32463143800401,
55.2706077778965));
#144287=CARTESIAN_POINT('Ctrl Pts',(90.6242675720478,-4.0209956755633,55.5521118754408));
#144288=CARTESIAN_POINT('Ctrl Pts',(90.5688797519172,-4.21918219490549,
55.5916472433144));
#144289=CARTESIAN_POINT('Ctrl Pts',(90.5092334210679,-4.4148115362535,55.6339688670712));
#144290=CARTESIAN_POINT('Ctrl Pts',(90.4453817395859,-4.60789992207962,
55.6788299742543));
#144291=CARTESIAN_POINT('Ctrl Pts',(90.3803286655751,-4.80462133586623,
55.7245351594281));
#144292=CARTESIAN_POINT('Ctrl Pts',(90.3109105403745,-4.99870563338229,
55.7728765859279));
#144293=CARTESIAN_POINT('Ctrl Pts',(90.2371438374155,-5.19016628571155,
55.8236299825407));
#144294=CARTESIAN_POINT('Ctrl Pts',(90.1616401667213,-5.38613521836696,
55.8755784578114));
#144295=CARTESIAN_POINT('Ctrl Pts',(90.0815807831541,-5.57935587985819,
55.9300541196797));
#144296=CARTESIAN_POINT('Ctrl Pts',(89.9969412499602,-5.76983317571853,
55.9868500877407));
#144297=CARTESIAN_POINT('Ctrl Pts',(89.9114467241532,-5.96223459231502,
56.0442197845465));
#144298=CARTESIAN_POINT('Ctrl Pts',(89.8212790150361,-6.15183730756892,
56.1039572727477));
#144299=CARTESIAN_POINT('Ctrl Pts',(89.7263703623101,-6.33863102978564,
56.1658780736405));
#144300=CARTESIAN_POINT('Ctrl Pts',(89.6305117548475,-6.52729439798418,
56.228418648984));
#144301=CARTESIAN_POINT('Ctrl Pts',(89.5298167828039,-6.71309263142337,
56.2931868387061));
#144302=CARTESIAN_POINT('Ctrl Pts',(89.424172972098,-6.89599393591638,56.3600160628481));
#144303=CARTESIAN_POINT('Ctrl Pts',(89.372389864718,-6.98564611551143,56.3927735416511));
#144304=CARTESIAN_POINT('Ctrl Pts',(89.3194170895394,-7.07460191252195,
56.4260265319146));
#144305=CARTESIAN_POINT('Ctrl Pts',(89.265237764927,-7.16285534378127,56.4597570269004));
#144306=CARTESIAN_POINT('Ctrl Pts',(89.1514748157839,-7.3481653431933,56.5305825791401));
#144307=CARTESIAN_POINT('Ctrl Pts',(89.0324076176265,-7.53045736360164,
56.6035308814627));
#144308=CARTESIAN_POINT('Ctrl Pts',(88.9081095276437,-7.70971421697662,
56.6784254559144));
#144309=CARTESIAN_POINT('Ctrl Pts',(88.7848087492422,-7.88753279454283,
56.7527191102194));
#144310=CARTESIAN_POINT('Ctrl Pts',(88.6563608772338,-8.06236500249708,
56.8289279758922));
#144311=CARTESIAN_POINT('Ctrl Pts',(88.5227985537957,-8.23420622355589,
56.9069108044424));
#144312=CARTESIAN_POINT('Ctrl Pts',(88.3916483918356,-8.40294395881794,
56.983485247977));
#144313=CARTESIAN_POINT('Ctrl Pts',(88.2555670078433,-8.56879807427274,
57.0617702627864));
#144314=CARTESIAN_POINT('Ctrl Pts',(88.1145450617424,-8.73177155843689,
57.141660937297));
#144315=CARTESIAN_POINT('Ctrl Pts',(87.9754900721468,-8.89247190878235,
57.2204373066495));
#144316=CARTESIAN_POINT('Ctrl Pts',(87.8316316013172,-9.05037172662669,
57.3007749486453));
#144317=CARTESIAN_POINT('Ctrl Pts',(87.6829183415991,-9.20547662654759,
57.3826001342298));
#144318=CARTESIAN_POINT('Ctrl Pts',(87.537851788522,-9.35677808574178,57.4624188245747));
#144319=CARTESIAN_POINT('Ctrl Pts',(87.3881657871141,-9.50542030776213,
57.5436531350847));
#144320=CARTESIAN_POINT('Ctrl Pts',(87.2337694243479,-9.65140681675671,
57.6262586182279));
#144321=CARTESIAN_POINT('Ctrl Pts',(87.1773368748085,-9.70476552776076,
57.6564512855692));
#144322=CARTESIAN_POINT('Ctrl Pts',(87.1202746136925,-9.75776941491483,
57.6868273584235));
#144323=CARTESIAN_POINT('Ctrl Pts',(87.0625766316463,-9.81041847342618,
57.7173854406918));
#144324=CARTESIAN_POINT('Origin',(91.9461506873691,0.0433429899084442,83.08714534325));
#144325=CARTESIAN_POINT('Origin',(91.5481555916691,0.0433429899084342,83.15732261681));
#144326=CARTESIAN_POINT('',(90.9924243507979,-11.2698537367303,57.6400054152702));
#144327=CARTESIAN_POINT('Ctrl Pts',(90.9924243507979,-11.2698537367303,
57.6400054152702));
#144328=CARTESIAN_POINT('Ctrl Pts',(91.0087196669506,-11.4929559013193,
57.7372219051933));
#144329=CARTESIAN_POINT('Ctrl Pts',(91.0264213003634,-11.6946801922847,
57.8273475410391));
#144330=CARTESIAN_POINT('Ctrl Pts',(91.0413458950691,-11.874941516,57.91633991463));
#144331=CARTESIAN_POINT('',(90.9047353709724,-10.0689627465674,57.1426963510668));
#144332=CARTESIAN_POINT('Ctrl Pts',(90.9045946917496,-10.0692831548029,
57.1418989990502));
#144333=CARTESIAN_POINT('Ctrl Pts',(90.9324261720231,-10.4675541238281,
57.2966628248043));
#144334=CARTESIAN_POINT('Ctrl Pts',(90.9607405811956,-10.8632766047505,
57.4621592417098));
#144335=CARTESIAN_POINT('Ctrl Pts',(90.9923722612255,-11.2699867077158,
57.6397093617342));
#144336=CARTESIAN_POINT('Ctrl Pts',(90.6242620415567,-4.02100038809876,
55.5520804830879));
#144337=CARTESIAN_POINT('Ctrl Pts',(90.6508298361238,-5.05591292129145,
55.7027332878991));
#144338=CARTESIAN_POINT('Ctrl Pts',(90.6876273743442,-6.08235086745013,
55.9118120415735));
#144339=CARTESIAN_POINT('Ctrl Pts',(90.7811137180524,-8.10404684266629,
56.4431103566449));
#144340=CARTESIAN_POINT('Ctrl Pts',(90.8376673001883,-9.09977064310684,
56.7650116874898));
#144341=CARTESIAN_POINT('Ctrl Pts',(90.9047434407505,-10.0689443669993,
57.1427420895467));
#144342=CARTESIAN_POINT('Ctrl Pts',(90.7138133970691,-10.19657068826,57.22715772731));
#144343=CARTESIAN_POINT('Ctrl Pts',(90.6626401866691,-9.35597025367699,
56.89396444657));
#144344=CARTESIAN_POINT('Ctrl Pts',(90.5763427137691,-7.68274033475999,
56.32754975961));
#144345=CARTESIAN_POINT('Ctrl Pts',(90.4541100393691,-4.24096410950499,
55.51544965917));
#144346=CARTESIAN_POINT('Ctrl Pts',(90.4199971140691,-1.61565261237899,
55.278532208));
#144347=CARTESIAN_POINT('Ctrl Pts',(90.4235408013691,0.151366721048514,
55.2878082705));
#144348=CARTESIAN_POINT('Ctrl Pts',(92.7962304970691,-10.33573356652,56.91274505515));
#144349=CARTESIAN_POINT('Ctrl Pts',(92.6626615303691,-9.48934028449099,
56.58708866282));
#144350=CARTESIAN_POINT('Ctrl Pts',(92.4384562628691,-7.79709517031399,
56.02944513539));
#144351=CARTESIAN_POINT('Ctrl Pts',(92.1038555437691,-4.30231560357699,
55.22999031531));
#144352=CARTESIAN_POINT('Ctrl Pts',(91.9893535601691,-1.63094673070299,
55.00159014612));
#144353=CARTESIAN_POINT('Ctrl Pts',(91.9738408428691,0.152837241252914,
55.0144585082));
#144354=CARTESIAN_POINT('Ctrl Pts',(95.7917187514691,-10.46442002935,56.51480537428));
#144355=CARTESIAN_POINT('Ctrl Pts',(95.5385368179691,-9.61788303082499,
56.19345931582));
#144356=CARTESIAN_POINT('Ctrl Pts',(95.1142808849691,-7.90799621978299,
55.63550595397));
#144357=CARTESIAN_POINT('Ctrl Pts',(94.4716188046691,-4.36724739891599,
54.83183905851));
#144358=CARTESIAN_POINT('Ctrl Pts',(94.2410150211691,-1.65095915302099,
54.60377902895));
#144359=CARTESIAN_POINT('Ctrl Pts',(94.1980369484691,0.154734101969314,
54.62230769129));
#144360=CARTESIAN_POINT('Ctrl Pts',(98.8683031516691,-10.53264157621,56.06075913389));
#144361=CARTESIAN_POINT('Ctrl Pts',(98.4877770766691,-9.70318322055799,
55.75728931457));
#144362=CARTESIAN_POINT('Ctrl Pts',(97.8443279361691,-7.98735677313499,
55.21668635057));
#144363=CARTESIAN_POINT('Ctrl Pts',(96.8545601533691,-4.42828578380799,
54.43258140482));
#144364=CARTESIAN_POINT('Ctrl Pts',(96.4917933988691,-1.67262404030799,
54.20606631111));
#144365=CARTESIAN_POINT('Ctrl Pts',(96.4222845185691,0.156770965735314,
54.23015027228));
#144366=CARTESIAN_POINT('Ctrl Pts',(99.8158998763691,-10.54389419866,55.88918321301));
#144367=CARTESIAN_POINT('Ctrl Pts',(99.3961224694691,-9.72294815639999,
55.59736775867));
#144368=CARTESIAN_POINT('Ctrl Pts',(98.6828965672691,-8.00820666453199,
55.07186546666));
#144369=CARTESIAN_POINT('Ctrl Pts',(97.5798863617691,-4.44890047093699,
54.30829590648));
#144370=CARTESIAN_POINT('Ctrl Pts',(97.1727004419691,-1.68039152780799,
54.0858613594));
#144371=CARTESIAN_POINT('Ctrl Pts',(97.0962919792691,0.157498942840914,
54.11131090037));
#144372=CARTESIAN_POINT('',(96.9599167740691,3.35717732455102E-13,54.13484467945));
#144373=CARTESIAN_POINT('',(91.1670701073691,2.7354895961722E-14,55.15627904919));
#144374=CARTESIAN_POINT('',(96.602194994137,-10.3347552344798,56.3300847780142));
#144375=CARTESIAN_POINT('Ctrl Pts',(90.9045946917494,-10.0692831548015,
57.1418989990485));
#144376=CARTESIAN_POINT('Ctrl Pts',(92.790213969345,-10.1923684393204,56.8585600051375));
#144377=CARTESIAN_POINT('Ctrl Pts',(94.6808936658549,-10.2756779228702,
56.6037222733635));
#144378=CARTESIAN_POINT('Ctrl Pts',(96.602194994137,-10.3347552344798,56.3300847780142));
#144379=CARTESIAN_POINT('Ctrl Pts',(96.9599167578601,6.36803545775495E-13,
54.134844587524));
#144380=CARTESIAN_POINT('Ctrl Pts',(96.9599171426822,-0.277060945827445,
54.134843612205));
#144381=CARTESIAN_POINT('Ctrl Pts',(96.9591759725721,-0.56015552509148,
54.1397203553601));
#144382=CARTESIAN_POINT('Ctrl Pts',(96.9575927400265,-0.849076263937013,
54.1499931425902));
#144383=CARTESIAN_POINT('Ctrl Pts',(96.9566606021444,-1.01918012288742,
54.1560413091462));
#144384=CARTESIAN_POINT('Ctrl Pts',(96.9554366094299,-1.19130261050792,
54.1639598075232));
#144385=CARTESIAN_POINT('Ctrl Pts',(96.9539006071702,-1.36539298195192,
54.1738529901787));
#144386=CARTESIAN_POINT('Ctrl Pts',(96.9511742972054,-1.67439273208784,
54.1914127836539));
#144387=CARTESIAN_POINT('Ctrl Pts',(96.9474649896664,-1.98959457399915,
54.2151936749478));
#144388=CARTESIAN_POINT('Ctrl Pts',(96.9426532817427,-2.31074252617866,
54.24581600169));
#144389=CARTESIAN_POINT('Ctrl Pts',(96.9404448505482,-2.45813990916418,
54.2598707412332));
#144390=CARTESIAN_POINT('Ctrl Pts',(96.9380042152572,-2.60678916580932,
54.2753665899201));
#144391=CARTESIAN_POINT('Ctrl Pts',(96.9353199592136,-2.75666185664168,
54.2923630781649));
#144392=CARTESIAN_POINT('Ctrl Pts',(96.9296516014349,-3.07314881581515,
54.3282546528831));
#144393=CARTESIAN_POINT('Ctrl Pts',(96.9228968211612,-3.39509477480875,
54.3708380894919));
#144394=CARTESIAN_POINT('Ctrl Pts',(96.9149435292017,-3.72219497430077,
54.4206994698898));
#144395=CARTESIAN_POINT('Ctrl Pts',(96.9125976699976,-3.81867464807259,
54.4354063081065));
#144396=CARTESIAN_POINT('Ctrl Pts',(96.9101475494493,-3.91560238986618,
54.4507462954679));
#144397=CARTESIAN_POINT('Ctrl Pts',(96.9075903110946,-4.01296950428391,
54.4667344125127));
#144398=CARTESIAN_POINT('Ctrl Pts',(96.8994999337026,-4.32101145890927,
54.5173162835551));
#144399=CARTESIAN_POINT('Ctrl Pts',(96.8903373787788,-4.6334550620318,54.574385330324));
#144400=CARTESIAN_POINT('Ctrl Pts',(96.8800083495169,-4.94995790029281,
54.6384369908349));
#144401=CARTESIAN_POINT('Ctrl Pts',(96.8776910512548,-5.02096471598414,
54.6528068602415));
#144402=CARTESIAN_POINT('Ctrl Pts',(96.8753150437641,-5.09217563446697,
54.6675281773576));
#144403=CARTESIAN_POINT('Ctrl Pts',(96.8728792659521,-5.16358642425807,
54.6826065310305));
#144404=CARTESIAN_POINT('Ctrl Pts',(96.8630108022917,-5.45290459628258,
54.7436959229071));
#144405=CARTESIAN_POINT('Ctrl Pts',(96.8521608407434,-5.74550708452013,
54.8106478289228));
#144406=CARTESIAN_POINT('Ctrl Pts',(96.8402839376195,-6.04105560289267,
54.8837055006886));
#144407=CARTESIAN_POINT('Ctrl Pts',(96.8378379451746,-6.10192243286345,
54.8987513852354));
#144408=CARTESIAN_POINT('Ctrl Pts',(96.8353484135449,-6.16291405982723,
54.9140561536033));
#144409=CARTESIAN_POINT('Ctrl Pts',(96.8328149727655,-6.22402728514366,
54.9296217986156));
#144410=CARTESIAN_POINT('Ctrl Pts',(96.81901609602,-6.55689232407346,55.0144031042355));
#144411=CARTESIAN_POINT('Ctrl Pts',(96.8039139414176,-6.89336720567203,
55.1069268719829));
#144412=CARTESIAN_POINT('Ctrl Pts',(96.7874496467217,-7.23312623612149,
55.2075115883376));
#144413=CARTESIAN_POINT('Ctrl Pts',(96.786035072685,-7.26231754446941,55.2161535940153));
#144414=CARTESIAN_POINT('Ctrl Pts',(96.784610448577,-7.29153307619233,55.2248550796922));
#144415=CARTESIAN_POINT('Ctrl Pts',(96.7831757399513,-7.32077261352518,
55.2336162332069));
#144416=CARTESIAN_POINT('Ctrl Pts',(96.7803261873095,-7.37884684501412,
55.2510172355393));
#144417=CARTESIAN_POINT('Ctrl Pts',(96.7774368533627,-7.43701577347718,
55.2686536150049));
#144418=CARTESIAN_POINT('Ctrl Pts',(96.7745072371656,-7.49527846640879,
55.2865280332663));
#144419=CARTESIAN_POINT('Ctrl Pts',(96.7590394015428,-7.8028947876485,55.3809016798179));
#144420=CARTESIAN_POINT('Ctrl Pts',(96.742448658216,-8.11312489114606,55.4819107935465));
#144421=CARTESIAN_POINT('Ctrl Pts',(96.7246611171326,-8.42583162785647,
55.5899487265824));
#144422=CARTESIAN_POINT('Ctrl Pts',(96.7067169276187,-8.74129225951466,
55.6989381105564));
#144423=CARTESIAN_POINT('Ctrl Pts',(96.6875554159446,-9.05927574423186,
55.8150773272328));
#144424=CARTESIAN_POINT('Ctrl Pts',(96.6670513754222,-9.37946266624096,
55.9390253826691));
#144425=CARTESIAN_POINT('Ctrl Pts',(96.6645609067954,-9.41835331723715,
55.9540804028285));
#144426=CARTESIAN_POINT('Ctrl Pts',(96.662050621889,-9.45727644122763,55.9692506796209));
#144427=CARTESIAN_POINT('Ctrl Pts',(96.6595202881283,-9.49623143702847,
55.9845374374691));
#144428=CARTESIAN_POINT('Ctrl Pts',(96.6414623973248,-9.7742362881439,56.0936323751597));
#144429=CARTESIAN_POINT('Ctrl Pts',(96.6223838211085,-10.0538674463473,
56.2086575718103));
#144430=CARTESIAN_POINT('Ctrl Pts',(96.6021951000051,-10.3347534605419,
56.3300838067384));
#144431=CARTESIAN_POINT('Ctrl Pts',(96.6696289028691,0.160268731304714,
54.21733794602));
#144432=CARTESIAN_POINT('Ctrl Pts',(96.670308400869,-0.346230314545186,
54.21384224945));
#144433=CARTESIAN_POINT('Ctrl Pts',(96.6654264806691,-1.31612458106799,
54.23895742649));
#144434=CARTESIAN_POINT('Ctrl Pts',(96.6422624601691,-2.70059882064599,
54.35812538629));
#144435=CARTESIAN_POINT('Ctrl Pts',(96.608028791469,-3.95977777602399,54.53424146526));
#144436=CARTESIAN_POINT('Ctrl Pts',(96.5658452623691,-5.10903817364999,
54.75125582648));
#144437=CARTESIAN_POINT('Ctrl Pts',(96.5158510367691,-6.20578639454099,
55.00845253674));
#144438=CARTESIAN_POINT('Ctrl Pts',(96.4572022184691,-7.28729934218798,
55.31017304474));
#144439=CARTESIAN_POINT('Ctrl Pts',(96.3889045551691,-8.37105043441599,
55.6615323096));
#144440=CARTESIAN_POINT('Ctrl Pts',(96.3136363712691,-9.41723706373098,
56.04875161508));
#144441=CARTESIAN_POINT('Ctrl Pts',(96.258897993869,-10.09227685666,56.33035474907));
#144442=CARTESIAN_POINT('Ctrl Pts',(96.2311574648692,-10.41546419882,56.47306668683));
#144443=CARTESIAN_POINT('Ctrl Pts',(98.1128935683692,0.166136603669114,
53.6477629649701));
#144444=CARTESIAN_POINT('Ctrl Pts',(98.1135980223691,-0.358956357238386,
53.64413888123));
#144445=CARTESIAN_POINT('Ctrl Pts',(98.108536711269,-1.36355315035499,53.67017693973));
#144446=CARTESIAN_POINT('Ctrl Pts',(98.0845692883691,-2.79580825471999,
53.7934780261801));
#144447=CARTESIAN_POINT('Ctrl Pts',(98.0491810976691,-4.09738494468499,
53.97553357625));
#144448=CARTESIAN_POINT('Ctrl Pts',(98.0055962418691,-5.284787566009,54.1997571019299));
#144449=CARTESIAN_POINT('Ctrl Pts',(97.9539701807691,-6.41729306682898,
54.4653488368801));
#144450=CARTESIAN_POINT('Ctrl Pts',(97.893484104969,-7.53261697524899,54.7765211682));
#144451=CARTESIAN_POINT('Ctrl Pts',(97.8231219679691,-8.64911747269499,
55.1385011759801));
#144452=CARTESIAN_POINT('Ctrl Pts',(97.7455474807691,-9.72739355825898,
55.53758532437));
#144453=CARTESIAN_POINT('Ctrl Pts',(97.6890592547692,-10.42404175222,55.82819060393));
#144454=CARTESIAN_POINT('Ctrl Pts',(97.660409458769,-10.75782222324,55.97558029138));
#144455=CARTESIAN_POINT('Ctrl Pts',(99.2004280885691,0.159957130493114,
54.75442165969));
#144456=CARTESIAN_POINT('Ctrl Pts',(99.2011062613691,-0.345554525266686,
54.75093278085));
#144457=CARTESIAN_POINT('Ctrl Pts',(99.1962338672691,-1.31360598833699,
54.7759989502401));
#144458=CARTESIAN_POINT('Ctrl Pts',(99.1731125097691,-2.69554292728499,
54.89494742919));
#144459=CARTESIAN_POINT('Ctrl Pts',(99.1389401494691,-3.95247044164899,
55.0707481052501));
#144460=CARTESIAN_POINT('Ctrl Pts',(99.0968310347691,-5.09970537806498,
55.28737963921));
#144461=CARTESIAN_POINT('Ctrl Pts',(99.0469234643691,-6.19455478508299,
55.54413054964));
#144462=CARTESIAN_POINT('Ctrl Pts',(98.9883722097691,-7.27427227397399,
55.8453491387801));
#144463=CARTESIAN_POINT('Ctrl Pts',(98.9201841758691,-8.35628427908298,
56.1961444118));
#144464=CARTESIAN_POINT('Ctrl Pts',(98.8450384632691,-9.40076686645699,
56.58273366018));
#144465=CARTESIAN_POINT('Ctrl Pts',(98.7903930078691,-10.07465919146,56.8638587544801));
#144466=CARTESIAN_POINT('Ctrl Pts',(98.7627007634691,-10.39728400817,57.00632229035));
#144467=CARTESIAN_POINT('Ctrl Pts',(98.6057368794691,0.149267584137414,
56.18749216758));
#144468=CARTESIAN_POINT('Ctrl Pts',(98.6063695895691,-0.322371399450786,
56.18423717261));
#144469=CARTESIAN_POINT('Ctrl Pts',(98.6018239931692,-1.22720501392999,
56.20762212203));
#144470=CARTESIAN_POINT('Ctrl Pts',(98.5801661998691,-2.52209919915899,
56.31904125369));
#144471=CARTESIAN_POINT('Ctrl Pts',(98.5480970407691,-3.70179044778499,
56.48402195143));
#144472=CARTESIAN_POINT('Ctrl Pts',(98.5085407331691,-4.77954141403098,
56.68752049734));
#144473=CARTESIAN_POINT('Ctrl Pts',(98.461605889769,-5.80925152052899,56.9289781294));
#144474=CARTESIAN_POINT('Ctrl Pts',(98.4064015806692,-6.82737533285799,
57.21297826229));
#144475=CARTESIAN_POINT('Ctrl Pts',(98.3419744134691,-7.84972750498899,
57.54442564961));
#144476=CARTESIAN_POINT('Ctrl Pts',(98.2710301106691,-8.835752493285,57.90940062617));
#144477=CARTESIAN_POINT('Ctrl Pts',(98.2195723673692,-9.47028063478298,
58.17412644551));
#144478=CARTESIAN_POINT('Ctrl Pts',(98.1935365413691,-9.77360787053599,
58.30806849027));
#144479=CARTESIAN_POINT('Origin',(96.8148132210691,-9.75846282474099,57.69855282308));
#144480=CARTESIAN_POINT('Origin',(97.2203890703691,1.08526369006055E-7,
55.61205637088));
#144481=CARTESIAN_POINT('Ctrl Pts',(96.2311597944691,10.41560961071,56.47305462378));
#144482=CARTESIAN_POINT('Ctrl Pts',(96.2425456644691,10.28294688966,56.41447969266));
#144483=CARTESIAN_POINT('Ctrl Pts',(96.2665237450691,9.99701257139901,56.29112377728));
#144484=CARTESIAN_POINT('Ctrl Pts',(96.3029830043691,9.53999273052302,56.10355808445));
#144485=CARTESIAN_POINT('Ctrl Pts',(96.341615819269,9.02742880050502,55.90481047335));
#144486=CARTESIAN_POINT('Ctrl Pts',(96.3817550230691,8.45983449326603,55.69831320138));
#144487=CARTESIAN_POINT('Ctrl Pts',(96.4230873061691,7.83124748153802,55.48567809967));
#144488=CARTESIAN_POINT('Ctrl Pts',(96.465123940069,7.13529453258901,55.26941944543));
#144489=CARTESIAN_POINT('Ctrl Pts',(96.5071095016691,6.36519388110002,55.05342353344));
#144490=CARTESIAN_POINT('Ctrl Pts',(96.5479785345691,5.51425300235401,54.84317163521));
#144491=CARTESIAN_POINT('Ctrl Pts',(96.5862074329692,4.57747980015701,54.64650198403));
#144492=CARTESIAN_POINT('Ctrl Pts',(96.6201253331691,3.54799753503601,54.47201038533));
#144493=CARTESIAN_POINT('Ctrl Pts',(96.6478026904691,2.41338163155501,54.32962343617));
#144494=CARTESIAN_POINT('Ctrl Pts',(96.6664221526691,1.16626940880601,54.23383508485));
#144495=CARTESIAN_POINT('Ctrl Pts',(96.6702378408692,0.293677663957814,
54.21420516889));
#144496=CARTESIAN_POINT('Ctrl Pts',(96.6696289293692,-0.160237368166786,
54.21733773116));
#144497=CARTESIAN_POINT('Ctrl Pts',(97.6604144928692,10.75793837742,55.97555520529));
#144498=CARTESIAN_POINT('Ctrl Pts',(97.6721750711691,10.62090973503,55.9150525767801));
#144499=CARTESIAN_POINT('Ctrl Pts',(97.6969333406691,10.32566953004,55.78768295773));
#144500=CARTESIAN_POINT('Ctrl Pts',(97.7345529493691,9.854100032395,55.59414781434));
#144501=CARTESIAN_POINT('Ctrl Pts',(97.7743875562691,9.32558631739701,55.38921755005));
#144502=CARTESIAN_POINT('Ctrl Pts',(97.815752058769,8.74066062569102,55.17641669437));
#144503=CARTESIAN_POINT('Ctrl Pts',(97.8583357654691,8.09304235429201,54.95734360863));
#144504=CARTESIAN_POINT('Ctrl Pts',(97.9016574024691,7.37582286052101,54.7344742188501));
#144505=CARTESIAN_POINT('Ctrl Pts',(97.9449558647691,6.58165855423801,54.5117240523701));
#144506=CARTESIAN_POINT('Ctrl Pts',(97.9871389566692,5.70338735783601,54.2947119403101));
#144507=CARTESIAN_POINT('Ctrl Pts',(98.0266336670691,4.73562596871401,54.09153028349));
#144508=CARTESIAN_POINT('Ctrl Pts',(98.0616832237691,3.67181175629301,53.91121684539));
#144509=CARTESIAN_POINT('Ctrl Pts',(98.0903010919691,2.49871342897601,53.76399141175));
#144510=CARTESIAN_POINT('Ctrl Pts',(98.109568905869,1.20836539597901,53.66486759685));
#144511=CARTESIAN_POINT('Ctrl Pts',(98.1135250776691,0.304474695687914,
53.64451495891));
#144512=CARTESIAN_POINT('Ctrl Pts',(98.1128937887691,-0.166104368673886,
53.64776264251));
#144513=CARTESIAN_POINT('Ctrl Pts',(98.7627032108691,10.39743093721,57.0063110524));
#144514=CARTESIAN_POINT('Ctrl Pts',(98.7740691828691,10.26500005954,56.9478384877199));
#144515=CARTESIAN_POINT('Ctrl Pts',(98.7980058330692,9.97955991148701,56.82469571192));
#144516=CARTESIAN_POINT('Ctrl Pts',(98.8344034743691,9.52331270056701,56.63744701464));
#144517=CARTESIAN_POINT('Ctrl Pts',(98.8729724705691,9.01159575146801,56.43902772077));
#144518=CARTESIAN_POINT('Ctrl Pts',(98.9130466074691,8.44492179218101,56.2328651878));
#144519=CARTESIAN_POINT('Ctrl Pts',(98.9543124361691,7.81734539682401,56.02057196215));
#144520=CARTESIAN_POINT('Ctrl Pts',(98.9962808325691,7.12252176452102,55.80466435759));
#144521=CARTESIAN_POINT('Ctrl Pts',(99.0381966752691,6.35369896451901,55.58902711656));
#144522=CARTESIAN_POINT('Ctrl Pts',(99.0789959277691,5.50420940675301,55.3791342057501));
#144523=CARTESIAN_POINT('Ctrl Pts',(99.1171576077691,4.56908176925101,55.1828103613901));
#144524=CARTESIAN_POINT('Ctrl Pts',(99.1510154135691,3.54142263242401,55.00862791964));
#144525=CARTESIAN_POINT('Ctrl Pts',(99.1786428269691,2.40885025985901,54.86649790837));
#144526=CARTESIAN_POINT('Ctrl Pts',(99.1972278598691,1.16403398695201,54.77088668006));
#144527=CARTESIAN_POINT('Ctrl Pts',(99.2010360879692,0.293104309528914,
54.75129514278));
#144528=CARTESIAN_POINT('Ctrl Pts',(99.2004283647692,-0.159925813027386,
54.75442159177));
#144529=CARTESIAN_POINT('Ctrl Pts',(98.1935340747691,9.77380813262502,58.30808090183));
#144530=CARTESIAN_POINT('Ctrl Pts',(98.2042174378691,9.64933068563601,58.25312003751));
#144531=CARTESIAN_POINT('Ctrl Pts',(98.2267328124692,9.38084313911702,58.13728905489));
#144532=CARTESIAN_POINT('Ctrl Pts',(98.261016636769,8.95110114377703,57.96091494911));
#144533=CARTESIAN_POINT('Ctrl Pts',(98.297396319569,8.468440034004,57.77375863954));
#144534=CARTESIAN_POINT('Ctrl Pts',(98.335238320969,7.93333878387603,57.57907939087));
#144535=CARTESIAN_POINT('Ctrl Pts',(98.3742244223691,7.34043177270501,57.37851428755));
#144536=CARTESIAN_POINT('Ctrl Pts',(98.4138519189691,6.68434955980702,57.17464950802));
#144537=CARTESIAN_POINT('Ctrl Pts',(98.453376041069,5.95936369479301,56.97131654153));
#144538=CARTESIAN_POINT('Ctrl Pts',(98.4917814626692,5.15966197551602,56.77373876143));
#144539=CARTESIAN_POINT('Ctrl Pts',(98.5276372037691,4.28098574355801,56.58927788512));
#144540=CARTESIAN_POINT('Ctrl Pts',(98.5594334625691,3.31586936487401,56.42570113055));
#144541=CARTESIAN_POINT('Ctrl Pts',(98.585347540569,2.25340070375301,56.29238542167));
#144542=CARTESIAN_POINT('Ctrl Pts',(98.6027514664691,1.08734742089201,56.2028504316));
#144543=CARTESIAN_POINT('Ctrl Pts',(98.6063037745691,0.273435278283314,
56.18457548221));
#144544=CARTESIAN_POINT('Ctrl Pts',(98.605736816469,-0.149237855524086,
56.18749221385));
#144545=CARTESIAN_POINT('',(96.6024042671263,10.3348601566812,56.3300319325398));
#144546=CARTESIAN_POINT('Origin',(96.8148145050691,9.75862245206801,57.69854621723));
#144547=CARTESIAN_POINT('Ctrl Pts',(96.6024043659547,10.3348592664372,56.3300312921791));
#144548=CARTESIAN_POINT('Ctrl Pts',(96.6084219835484,10.2511412529389,56.2938461676181));
#144549=CARTESIAN_POINT('Ctrl Pts',(96.6144624575879,10.1658560418771,56.2575059362147));
#144550=CARTESIAN_POINT('Ctrl Pts',(96.6205180308355,10.0789934768286,56.221050733991));
#144551=CARTESIAN_POINT('Ctrl Pts',(96.6309956957853,9.9286993897054,56.157974064127));
#144552=CARTESIAN_POINT('Ctrl Pts',(96.6415186109792,9.77368272111521,56.0945529558029));
#144553=CARTESIAN_POINT('Ctrl Pts',(96.6520454633506,9.61389022100475,56.0310011592772));
#144554=CARTESIAN_POINT('Ctrl Pts',(96.6630026090245,9.44756607780156,55.9648516334932));
#144555=CARTESIAN_POINT('Ctrl Pts',(96.6739640081778,9.27606786512193,55.8985605793858));
#144556=CARTESIAN_POINT('Ctrl Pts',(96.6848822592359,9.09932968087413,55.8323732675094));
#144557=CARTESIAN_POINT('Ctrl Pts',(96.6930210020023,8.96758453131361,55.783035557386));
#144558=CARTESIAN_POINT('Ctrl Pts',(96.7011357766724,8.83292802143723,55.7337554546973));
#144559=CARTESIAN_POINT('Ctrl Pts',(96.7092052910968,8.69532473815957,55.6846430982255));
#144560=CARTESIAN_POINT('Ctrl Pts',(96.7124201954733,8.64050342248117,55.6650766755812));
#144561=CARTESIAN_POINT('Ctrl Pts',(96.7156279109387,8.58521438368289,55.6455369040242));
#144562=CARTESIAN_POINT('Ctrl Pts',(96.7188270717432,8.52945538252802,55.6260308482034));
#144563=CARTESIAN_POINT('Ctrl Pts',(96.7305350870968,8.32539335454058,55.554644251844));
#144564=CARTESIAN_POINT('Ctrl Pts',(96.7421288191065,8.11503747979796,55.4837077123816));
#144565=CARTESIAN_POINT('Ctrl Pts',(96.7535336198707,7.89825013892825,55.413607184542));
#144566=CARTESIAN_POINT('Ctrl Pts',(96.7646799253056,7.68637638806486,55.3450955190947));
#144567=CARTESIAN_POINT('Ctrl Pts',(96.7756460513596,7.46835904462709,55.2773809341928));
#144568=CARTESIAN_POINT('Ctrl Pts',(96.7863456394669,7.24407857810092,55.210909559299));
#144569=CARTESIAN_POINT('Ctrl Pts',(96.7870529629367,7.22925194775016,55.2065153000944));
#144570=CARTESIAN_POINT('Ctrl Pts',(96.7877591190464,7.21439794543156,55.2021264870342));
#144571=CARTESIAN_POINT('Ctrl Pts',(96.7884640817421,7.19951653632829,55.1977432546116));
#144572=CARTESIAN_POINT('Ctrl Pts',(96.7918518676576,7.12800207396804,55.1766790860286));
#144573=CARTESIAN_POINT('Ctrl Pts',(96.7952120997352,7.05585467210436,55.1557437612974));
#144574=CARTESIAN_POINT('Ctrl Pts',(96.7985416990093,6.98307159402205,55.1349531713329));
#144575=CARTESIAN_POINT('Ctrl Pts',(96.8005529259795,6.93910735762018,55.122394724559));
#144576=CARTESIAN_POINT('Ctrl Pts',(96.8025529812833,6.89491116477672,55.1098890893669));
#144577=CARTESIAN_POINT('Ctrl Pts',(96.8045411626626,6.85048244849461,55.0974398546943));
#144578=CARTESIAN_POINT('Ctrl Pts',(96.8055352533523,6.82826809035355,55.091215237358));
#144579=CARTESIAN_POINT('Ctrl Pts',(96.8065263756882,6.80599560113382,55.0850047209203));
#144580=CARTESIAN_POINT('Ctrl Pts',(96.8075144421586,6.78366490678631,55.078808758257));
#144581=CARTESIAN_POINT('Ctrl Pts',(96.8083790003203,6.76412554923223,55.0733872909267));
#144582=CARTESIAN_POINT('Ctrl Pts',(96.8092412188429,6.74454162836447,55.0679769663772));
#144583=CARTESIAN_POINT('Ctrl Pts',(96.8101010386112,6.72491309569946,55.06257809058));
#144584=CARTESIAN_POINT('Ctrl Pts',(96.8102238700067,6.72210901960446,55.0618068226089));
#144585=CARTESIAN_POINT('Ctrl Pts',(96.8102881861003,6.72064067545679,55.0614029734022));
#144586=CARTESIAN_POINT('Ctrl Pts',(96.8104693857455,6.71649813595896,55.0602649885249));
#144587=CARTESIAN_POINT('Ctrl Pts',(96.8146869362856,6.62007758461498,55.0337775816222));
#144588=CARTESIAN_POINT('Ctrl Pts',(96.8188309109694,6.52337416078276,55.0077816168893));
#144589=CARTESIAN_POINT('Ctrl Pts',(96.8228991985691,6.42639016931002,54.9822874190042));
#144590=CARTESIAN_POINT('Ctrl Pts',(96.8347505673355,6.14386514638222,54.9080200194814));
#144591=CARTESIAN_POINT('Ctrl Pts',(96.8459597618218,5.85895886716469,54.8380099622278));
#144592=CARTESIAN_POINT('Ctrl Pts',(96.8564654327478,5.57175606730921,54.772560755726));
#144593=CARTESIAN_POINT('Ctrl Pts',(96.8678570598177,5.26033310228057,54.7015921371824));
#144594=CARTESIAN_POINT('Ctrl Pts',(96.8784214633711,4.9462092729796,54.6359862154016));
#144595=CARTESIAN_POINT('Ctrl Pts',(96.8880960192383,4.62968227709694,54.5760520609986));
#144596=CARTESIAN_POINT('Ctrl Pts',(96.8985101039455,4.2889597682312,54.5115365039669));
#144597=CARTESIAN_POINT('Ctrl Pts',(96.9078930631961,3.9454530461053,54.453593113036));
#144598=CARTESIAN_POINT('Ctrl Pts',(96.916182680695,3.59934808772723,54.4025288115359));
#144599=CARTESIAN_POINT('Ctrl Pts',(96.9251664910279,3.224259454056,54.3471882605979));
#144600=CARTESIAN_POINT('Ctrl Pts',(96.9328662348363,2.84611874664824,54.2999268110739));
#144601=CARTESIAN_POINT('Ctrl Pts',(96.9391924031706,2.465241900983,54.2611926479285));
#144602=CARTESIAN_POINT('Ctrl Pts',(96.9461055728112,2.04902372481488,54.2188643653793));
#144603=CARTESIAN_POINT('Ctrl Pts',(96.9513785461808,1.62953797927088,54.1867186023368));
#144604=CARTESIAN_POINT('Ctrl Pts',(96.9548785263097,1.20715853147687,54.1654288564663));
#144605=CARTESIAN_POINT('Ctrl Pts',(96.9581927427499,0.807197143619323,
54.1452690775045));
#144606=CARTESIAN_POINT('Ctrl Pts',(96.9599172393264,0.40464045421033,54.134843246294));
#144607=CARTESIAN_POINT('Ctrl Pts',(96.9599167505116,-6.53612581251083E-14,
54.134844545849));
#144608=CARTESIAN_POINT('Ctrl Pts',(99.8229747619691,10.54405187355,55.88748381909));
#144609=CARTESIAN_POINT('Ctrl Pts',(99.6011503882691,10.11099294518,55.73360189522));
#144610=CARTESIAN_POINT('Ctrl Pts',(99.2102368780691,9.25605213789501,55.45271235202));
#144611=CARTESIAN_POINT('Ctrl Pts',(98.7021511514691,7.94604321926101,55.08505245608));
#144612=CARTESIAN_POINT('Ctrl Pts',(98.2701917582691,6.66238207832301,54.78216749588));
#144613=CARTESIAN_POINT('Ctrl Pts',(97.7799388929691,4.91797092981301,54.44745221876));
#144614=CARTESIAN_POINT('Ctrl Pts',(97.3195994411691,2.63983322288901,54.16192812077));
#144615=CARTESIAN_POINT('Ctrl Pts',(97.1410285879691,0.789227954741114,
54.0973421985));
#144616=CARTESIAN_POINT('Ctrl Pts',(97.1017087564691,-0.155244189994386,
54.11034113544));
#144617=CARTESIAN_POINT('Ctrl Pts',(99.4111077309691,10.53918164393,55.96185987267));
#144618=CARTESIAN_POINT('Ctrl Pts',(99.1983162588691,10.10413395607,55.80530734332));
#144619=CARTESIAN_POINT('Ctrl Pts',(98.8236902496691,9.24752851307401,55.52032811987));
#144620=CARTESIAN_POINT('Ctrl Pts',(98.3374458072691,7.93709116282101,55.14813869173));
#144621=CARTESIAN_POINT('Ctrl Pts',(97.9244713730691,6.65312626074601,54.84160399721));
#144622=CARTESIAN_POINT('Ctrl Pts',(97.4562446747691,4.90972638740901,54.50320205192));
#144623=CARTESIAN_POINT('Ctrl Pts',(97.0170970717691,2.63464759459801,54.21479821838));
#144624=CARTESIAN_POINT('Ctrl Pts',(96.8467105044691,0.787641994762214,
54.14926657865));
#144625=CARTESIAN_POINT('Ctrl Pts',(96.8089517314691,-0.154932922945286,
54.1619595982));
#144626=CARTESIAN_POINT('Ctrl Pts',(98.4777090344691,10.52329010473,56.11845317377));
#144627=CARTESIAN_POINT('Ctrl Pts',(98.2852261383691,10.08453122649,55.95714161523));
#144628=CARTESIAN_POINT('Ctrl Pts',(97.9470076983691,9.22517756954501,55.6650077805));
#144629=CARTESIAN_POINT('Ctrl Pts',(97.5092800778691,7.91480618950201,55.28511132683));
#144630=CARTESIAN_POINT('Ctrl Pts',(97.1383378946691,6.63111996167601,54.97247109813));
#144631=CARTESIAN_POINT('Ctrl Pts',(96.7186546373691,4.89091160154701,54.62808485806));
#144632=CARTESIAN_POINT('Ctrl Pts',(96.3258627810691,2.62326937253201,54.33521804603));
#144633=CARTESIAN_POINT('Ctrl Pts',(96.1735151682691,0.784230533506414,
54.26805760886));
#144634=CARTESIAN_POINT('Ctrl Pts',(96.1394690336691,-0.154262148337386,
54.27999958306));
#144635=CARTESIAN_POINT('Ctrl Pts',(95.4083885479691,10.44883596239,56.56563465392));
#144636=CARTESIAN_POINT('Ctrl Pts',(95.2828062625691,10.00197988592,56.3957398526));
#144637=CARTESIAN_POINT('Ctrl Pts',(95.0630081160691,9.13858690468502,56.09214344177));
#144638=CARTESIAN_POINT('Ctrl Pts',(94.7806758719691,7.83336858220501,55.70203084944));
#144639=CARTESIAN_POINT('Ctrl Pts',(94.5431290615691,6.55548841998301,55.38187058097));
#144640=CARTESIAN_POINT('Ctrl Pts',(94.2760893890691,4.83002811735801,55.03105620878));
#144641=CARTESIAN_POINT('Ctrl Pts',(94.0284201829691,2.58855410828601,54.73379249893));
#144642=CARTESIAN_POINT('Ctrl Pts',(93.9343732761691,0.774119276983114,
54.66327669956));
#144643=CARTESIAN_POINT('Ctrl Pts',(93.9140860931691,-0.152268583664686,
54.67235913534));
#144644=CARTESIAN_POINT('Ctrl Pts',(92.8064875484691,10.33635977521,56.9112474595));
#144645=CARTESIAN_POINT('Ctrl Pts',(92.7357330084691,9.88956369225401,56.7393789277));
#144646=CARTESIAN_POINT('Ctrl Pts',(92.6117114470691,9.03084370884002,56.43423816251));
#144647=CARTESIAN_POINT('Ctrl Pts',(92.4529045945691,7.73795351776001,56.04452333574));
#144648=CARTESIAN_POINT('Ctrl Pts',(92.3202486007691,6.47365310299701,55.7253050736));
#144649=CARTESIAN_POINT('Ctrl Pts',(92.1720133995691,4.76915259221901,55.37615663976));
#144650=CARTESIAN_POINT('Ctrl Pts',(92.0369115993691,2.55748337778701,55.07951654561));
#144651=CARTESIAN_POINT('Ctrl Pts',(91.9894945383691,0.765968439024214,
55.00654446214));
#144652=CARTESIAN_POINT('Ctrl Pts',(91.9814512487691,-0.150644741938386,
55.01310502597));
#144653=CARTESIAN_POINT('Ctrl Pts',(90.7164576703691,10.19678286554,57.22677077382));
#144654=CARTESIAN_POINT('Ctrl Pts',(90.6893899738691,9.75304619127001,57.05089591696));
#144655=CARTESIAN_POINT('Ctrl Pts',(90.6417223165691,8.90227290514001,56.73991954444));
#144656=CARTESIAN_POINT('Ctrl Pts',(90.5814051064691,7.62527961729201,56.34394113065));
#144657=CARTESIAN_POINT('Ctrl Pts',(90.5323570494691,6.37927852091801,56.01957703094));
#144658=CARTESIAN_POINT('Ctrl Pts',(90.4788919205691,4.70104472127001,55.66451641314));
#144659=CARTESIAN_POINT('Ctrl Pts',(90.4337583071691,2.52566132230601,55.3604051064));
#144660=CARTESIAN_POINT('Ctrl Pts',(90.4237131106691,0.758799367497314,
55.28274489739));
#144661=CARTESIAN_POINT('Ctrl Pts',(90.4255048500691,-0.149192139117986,
55.28745041171));
#144662=CARTESIAN_POINT('Ctrl Pts',(96.6024042105574,10.3348592504771,56.3300313412501));
#144663=CARTESIAN_POINT('Ctrl Pts',(94.6805165943852,10.2762753587676,56.6036838964873));
#144664=CARTESIAN_POINT('Ctrl Pts',(92.790310713495,10.192372964693,56.8585465176481));
#144665=CARTESIAN_POINT('Ctrl Pts',(90.9047040108584,10.0692900874229,57.1418824909803));
#144666=CARTESIAN_POINT('Ctrl Pts',(97.4033426433691,11.67390399386,56.81447980514));
#144667=CARTESIAN_POINT('Ctrl Pts',(97.2044197352691,11.15857038581,56.59946163497));
#144668=CARTESIAN_POINT('Ctrl Pts',(97.0199546676691,10.69792038896,56.41485272246));
#144669=CARTESIAN_POINT('Ctrl Pts',(96.8505358648691,10.20340241203,56.23655459461));
#144670=CARTESIAN_POINT('Ctrl Pts',(95.1818404305691,11.63097278493,57.12775727934));
#144671=CARTESIAN_POINT('Ctrl Pts',(95.0391297258691,11.10781492551,56.90710660012));
#144672=CARTESIAN_POINT('Ctrl Pts',(94.9074321944691,10.63959524128,56.71574595965));
#144673=CARTESIAN_POINT('Ctrl Pts',(94.7862029432691,10.14192491651,56.53272828161));
#144674=CARTESIAN_POINT('Ctrl Pts',(93.0043471674691,11.54190049326,57.40548638152));
#144675=CARTESIAN_POINT('Ctrl Pts',(92.9159773486691,11.02450742992,57.18494785266));
#144676=CARTESIAN_POINT('Ctrl Pts',(92.8351915464691,10.54867530012,56.98933837901));
#144677=CARTESIAN_POINT('Ctrl Pts',(92.7597699884691,10.05314564258,56.80529830028));
#144678=CARTESIAN_POINT('Ctrl Pts',(90.8330907240691,11.394827307,57.7243208529));
#144679=CARTESIAN_POINT('Ctrl Pts',(90.7978936089691,10.8933807422,57.50281317575));
#144680=CARTESIAN_POINT('Ctrl Pts',(90.7679564434691,10.40883217466,57.29914644491));
#144681=CARTESIAN_POINT('Ctrl Pts',(90.7377901915691,9.91924603277401,57.11183124642));
#144682=CARTESIAN_POINT('',(96.5107425399285,11.5157870618668,56.8740840772352));
#144683=CARTESIAN_POINT('Ctrl Pts',(96.5107425395691,11.51578706178,56.87408407794));
#144684=CARTESIAN_POINT('Ctrl Pts',(94.6510436680464,11.468268482461,57.1317517447984));
#144685=CARTESIAN_POINT('Ctrl Pts',(92.819127139777,11.3889026395626,57.3718290827166));
#144686=CARTESIAN_POINT('Ctrl Pts',(90.9921937685691,11.26993034099,57.63983708294));
#144687=CARTESIAN_POINT('Ctrl Pts',(96.5107387539899,11.5157988299523,56.8740589380757));
#144688=CARTESIAN_POINT('Ctrl Pts',(96.5207205591766,11.392698487589,56.8149316120969));
#144689=CARTESIAN_POINT('Ctrl Pts',(96.5307034778743,11.2688057038616,56.7558085326091));
#144690=CARTESIAN_POINT('Ctrl Pts',(96.5406385265741,11.1438449346926,56.6969417202444));
#144691=CARTESIAN_POINT('Ctrl Pts',(96.5530657379208,10.9875383140187,56.6233084305987));
#144692=CARTESIAN_POINT('Ctrl Pts',(96.5654180277,10.8295608937585,56.5500762210146));
#144693=CARTESIAN_POINT('Ctrl Pts',(96.5775455007843,10.6697694503403,56.4780162762873));
#144694=CARTESIAN_POINT('Ctrl Pts',(96.58595630413,10.5589488038983,56.4280403233424));
#144695=CARTESIAN_POINT('Ctrl Pts',(96.5942589709957,10.4472556926979,56.3786282277779));
#144696=CARTESIAN_POINT('Ctrl Pts',(96.6024044181752,10.3348599160687,56.3300325143648));
#144697=CARTESIAN_POINT('Ctrl Pts',(96.1920310780691,11.59801716752,56.99776218657));
#144698=CARTESIAN_POINT('Ctrl Pts',(96.1943841679691,11.57301298649,56.98565664926));
#144699=CARTESIAN_POINT('Ctrl Pts',(96.2102167272692,11.40463464678,56.90420559885));
#144700=CARTESIAN_POINT('Ctrl Pts',(96.2404380922691,11.08085053798,56.7487309300401));
#144701=CARTESIAN_POINT('Ctrl Pts',(96.2821887412691,10.61938261741,56.53394353332));
#144702=CARTESIAN_POINT('Ctrl Pts',(96.309676275269,10.29835023287,56.39253313524));
#144703=CARTESIAN_POINT('Ctrl Pts',(96.3230502473691,10.13650208273,56.32373035667));
#144704=CARTESIAN_POINT('Ctrl Pts',(97.5959005388692,11.92723780495,56.59071945719));
#144705=CARTESIAN_POINT('Ctrl Pts',(97.5982687932691,11.90207219424,56.57853590535));
#144706=CARTESIAN_POINT('Ctrl Pts',(97.6142156663691,11.73247787192,56.49649676485));
#144707=CARTESIAN_POINT('Ctrl Pts',(97.6448186696691,11.40462228168,56.33905874716));
#144708=CARTESIAN_POINT('Ctrl Pts',(97.6875832150691,10.93200877884,56.11905533097));
#144709=CARTESIAN_POINT('Ctrl Pts',(97.7160179626691,10.59995097196,55.97277196594));
#144710=CARTESIAN_POINT('Ctrl Pts',(97.7298770894691,10.43223240023,55.90147329555));
#144711=CARTESIAN_POINT('Ctrl Pts',(98.6373592863691,11.5387915904,57.5954048691));
#144712=CARTESIAN_POINT('Ctrl Pts',(98.6397096481691,11.51381644996,57.58331336632));
#144713=CARTESIAN_POINT('Ctrl Pts',(98.6555216428691,11.34565686104,57.50196811114));
#144714=CARTESIAN_POINT('Ctrl Pts',(98.6856743525691,11.02260519672,57.34684664155));
#144715=CARTESIAN_POINT('Ctrl Pts',(98.7272426052691,10.56314232525,57.13299758747));
#144716=CARTESIAN_POINT('Ctrl Pts',(98.7545597390691,10.24409337348,56.99246381815));
#144717=CARTESIAN_POINT('Ctrl Pts',(98.7678464336691,10.08330129051,56.92411004131));
#144718=CARTESIAN_POINT('Ctrl Pts',(98.0919591842691,10.88937663559,58.83060487635));
#144719=CARTESIAN_POINT('Ctrl Pts',(98.0942796327691,10.86471992855,58.81866726368));
#144720=CARTESIAN_POINT('Ctrl Pts',(98.109866134269,10.69895896597,58.73848206487));
#144721=CARTESIAN_POINT('Ctrl Pts',(98.139266030869,10.38393863577,58.58723346345));
#144722=CARTESIAN_POINT('Ctrl Pts',(98.1788342886691,9.94646134776901,58.38367343947));
#144723=CARTESIAN_POINT('Ctrl Pts',(98.204282965369,9.64916095408402,58.25275200076));
#144724=CARTESIAN_POINT('Ctrl Pts',(98.2166126522691,9.49994876354401,58.1893215771));
#144725=CARTESIAN_POINT('Origin',(96.7134309613668,10.8856837889288,58.2201165235725));
#144726=CARTESIAN_POINT('Ctrl Pts',(96.095757050069,12.56332359615,57.55926050678));
#144727=CARTESIAN_POINT('Ctrl Pts',(96.102715496369,12.51478413356,57.5234625825));
#144728=CARTESIAN_POINT('Ctrl Pts',(96.1154032364691,12.42239695131,57.45819014398));
#144729=CARTESIAN_POINT('Ctrl Pts',(96.1329310601691,12.28520907105,57.36801775808));
#144730=CARTESIAN_POINT('Ctrl Pts',(96.1492921242691,12.14940768661,57.28384780045));
#144731=CARTESIAN_POINT('Ctrl Pts',(96.1657574770691,12.0034808127,57.19914132621));
#144732=CARTESIAN_POINT('Ctrl Pts',(96.1813456845691,11.8528395076,57.11894735106));
#144733=CARTESIAN_POINT('Ctrl Pts',(96.195164363669,11.71115093,57.04785676469));
#144734=CARTESIAN_POINT('Ctrl Pts',(96.2081771592692,11.57434490033,56.98091206873));
#144735=CARTESIAN_POINT('Ctrl Pts',(96.2204772585692,11.44332796521,56.91763385951));
#144736=CARTESIAN_POINT('Ctrl Pts',(96.228403107169,11.35848918082,56.8768591065301));
#144737=CARTESIAN_POINT('Ctrl Pts',(96.232252508769,11.31727201741,56.85705575105));
#144738=CARTESIAN_POINT('Ctrl Pts',(97.4808568854692,13.00157661483,57.2381820055001));
#144739=CARTESIAN_POINT('Ctrl Pts',(97.4891197811691,12.94386767406,57.19567330404));
#144740=CARTESIAN_POINT('Ctrl Pts',(97.5038887926691,12.83627687729,57.11969370597));
#144741=CARTESIAN_POINT('Ctrl Pts',(97.5237380737692,12.68084622952,57.01757851685));
#144742=CARTESIAN_POINT('Ctrl Pts',(97.5420178020692,12.52915975172,56.92353793651));
#144743=CARTESIAN_POINT('Ctrl Pts',(97.5609169829691,12.36171395817,56.82631056443));
#144744=CARTESIAN_POINT('Ctrl Pts',(97.5787431504691,12.18934898555,56.73460334054));
#144745=CARTESIAN_POINT('Ctrl Pts',(97.5935031851692,12.03787995816,56.6586699236201));
#144746=CARTESIAN_POINT('Ctrl Pts',(97.6069668917692,11.89634010197,56.58940550347));
#144747=CARTESIAN_POINT('Ctrl Pts',(97.6194660408691,11.76319375133,56.52510327666));
#144748=CARTESIAN_POINT('Ctrl Pts',(97.6274325288691,11.67792065658,56.4841194534901));
#144749=CARTESIAN_POINT('Ctrl Pts',(97.6312875136692,11.63664378591,56.4642873747));
#144750=CARTESIAN_POINT('Ctrl Pts',(98.5264853577691,12.47205724986,58.15468209609));
#144751=CARTESIAN_POINT('Ctrl Pts',(98.5331721520691,12.42542733435,58.1202816935401));
#144752=CARTESIAN_POINT('Ctrl Pts',(98.545426466569,12.33620631021,58.05723902479));
#144753=CARTESIAN_POINT('Ctrl Pts',(98.5624708459691,12.20281749274,57.96955373189));
#144754=CARTESIAN_POINT('Ctrl Pts',(98.5784323475691,12.07032418462,57.88743933493));
#144755=CARTESIAN_POINT('Ctrl Pts',(98.5943908547691,11.92887863335,57.80534034209));
#144756=CARTESIAN_POINT('Ctrl Pts',(98.6095130062692,11.7827612897,57.72754400507));
#144757=CARTESIAN_POINT('Ctrl Pts',(98.6231356477691,11.64310949422,57.65746193988));
#144758=CARTESIAN_POINT('Ctrl Pts',(98.6360545410691,11.5072892856,57.5910003273));
#144759=CARTESIAN_POINT('Ctrl Pts',(98.6483131880692,11.37671580202,57.52793537011));
#144760=CARTESIAN_POINT('Ctrl Pts',(98.6562305735691,11.29196746291,57.48720415607));
#144761=CARTESIAN_POINT('Ctrl Pts',(98.6600788123691,11.25076273356,57.4674067822201));
#144762=CARTESIAN_POINT('Ctrl Pts',(98.0125191480691,11.59265124379,59.23931483098));
#144763=CARTESIAN_POINT('Ctrl Pts',(98.0165884117691,11.56442096011,59.21838038874));
#144764=CARTESIAN_POINT('Ctrl Pts',(98.0246664116691,11.50570776901,59.17682288956));
#144765=CARTESIAN_POINT('Ctrl Pts',(98.0370525149691,11.40892520096,59.11310222996));
#144766=CARTESIAN_POINT('Ctrl Pts',(98.0491639918691,11.30830719299,59.05079439342));
#144767=CARTESIAN_POINT('Ctrl Pts',(98.0602387379691,11.21004187408,58.99382004842));
#144768=CARTESIAN_POINT('Ctrl Pts',(98.0708701605691,11.10751561337,58.9391263933));
#144769=CARTESIAN_POINT('Ctrl Pts',(98.0826038618691,10.98748943577,58.87876203478));
#144770=CARTESIAN_POINT('Ctrl Pts',(98.0946179494691,10.86116820446,58.81695522043));
#144771=CARTESIAN_POINT('Ctrl Pts',(98.1064771796691,10.7348676425,58.75594507446));
#144772=CARTESIAN_POINT('Ctrl Pts',(98.1143130175691,10.65099079798,58.71563338423));
#144773=CARTESIAN_POINT('Ctrl Pts',(98.1181500529691,10.60990587824,58.69589364708));
#144774=CARTESIAN_POINT('Ctrl Pts',(96.4483997728069,12.4478951511663,57.3802413623125));
#144775=CARTESIAN_POINT('Ctrl Pts',(96.4503965593856,12.4174690215184,57.360275428893));
#144776=CARTESIAN_POINT('Ctrl Pts',(96.4523301450555,12.3874581010196,57.341020297604));
#144777=CARTESIAN_POINT('Ctrl Pts',(96.4542318291937,12.3577640171988,57.3223117132754));
#144778=CARTESIAN_POINT('Ctrl Pts',(96.4561788230357,12.3273624393641,57.3031573764695));
#144779=CARTESIAN_POINT('Ctrl Pts',(96.4580925317787,12.2972901160016,57.2845751437417));
#144780=CARTESIAN_POINT('Ctrl Pts',(96.4600178933175,12.267172905776,57.2663306183736));
#144781=CARTESIAN_POINT('Ctrl Pts',(96.4611390891504,12.2496347499947,57.2557062834612));
#144782=CARTESIAN_POINT('Ctrl Pts',(96.4622641396932,12.2320822382948,57.2451969710702));
#144783=CARTESIAN_POINT('Ctrl Pts',(96.4634011392841,12.2144484575392,57.2347604468922));
#144784=CARTESIAN_POINT('Ctrl Pts',(96.4638851130955,12.2069424846703,57.2303180491777));
#144785=CARTESIAN_POINT('Ctrl Pts',(96.4643712419676,12.1994218714392,57.2258888910985));
#144786=CARTESIAN_POINT('Ctrl Pts',(96.4648589255827,12.1918906230061,57.2214760169925));
#144787=CARTESIAN_POINT('Ctrl Pts',(96.4670040447873,12.1587637654514,57.2020656027413));
#144788=CARTESIAN_POINT('Ctrl Pts',(96.4691787247034,12.1254343605685,57.1829729329922));
#144789=CARTESIAN_POINT('Ctrl Pts',(96.4713360069344,12.0922182879089,57.1644361287263));
#144790=CARTESIAN_POINT('Ctrl Pts',(96.4719225310154,12.083187468384,57.1593963235811));
#144791=CARTESIAN_POINT('Ctrl Pts',(96.4725078065675,12.0741647991286,57.1543974169163));
#144792=CARTESIAN_POINT('Ctrl Pts',(96.4730909725966,12.0651561275595,57.1494437735876));
#144793=CARTESIAN_POINT('Ctrl Pts',(96.4749397057767,12.0365971422826,57.1337399014011));
#144794=CARTESIAN_POINT('Ctrl Pts',(96.4767669938174,12.0081829116634,57.1184921654224));
#144795=CARTESIAN_POINT('Ctrl Pts',(96.4785488707318,11.9803414777681,57.103821944266));
#144796=CARTESIAN_POINT('Ctrl Pts',(96.4800041754786,11.9576026619836,57.0918403969921));
#144797=CARTESIAN_POINT('Ctrl Pts',(96.4814292548088,11.9352449100542,57.0802437418831));
#144798=CARTESIAN_POINT('Ctrl Pts',(96.482812617572,11.913476986101,57.0690901595441));
#144799=CARTESIAN_POINT('Ctrl Pts',(96.4847631184953,11.8827848517605,57.0533639355705));
#144800=CARTESIAN_POINT('Ctrl Pts',(96.4866314864273,11.8532585032914,57.0385144148399));
#144801=CARTESIAN_POINT('Ctrl Pts',(96.4884731621611,11.8245853546652,57.0242540861522));
#144802=CARTESIAN_POINT('Ctrl Pts',(96.489733386178,11.8049648591179,57.014496011824));
#144803=CARTESIAN_POINT('Ctrl Pts',(96.4909809648059,11.7857447070329,57.0050145855083));
#144804=CARTESIAN_POINT('Ctrl Pts',(96.4922318608456,11.7668349910155,56.9957270555952));
#144805=CARTESIAN_POINT('Ctrl Pts',(96.4934096768903,11.7490300206445,56.9869821228436));
#144806=CARTESIAN_POINT('Ctrl Pts',(96.4945903601356,11.7315006612338,56.9784094735593));
#144807=CARTESIAN_POINT('Ctrl Pts',(96.495778605489,11.7142162265952,56.9699844976127));
#144808=CARTESIAN_POINT('Ctrl Pts',(96.4978222701042,11.6844887066305,56.955494371329));
#144809=CARTESIAN_POINT('Ctrl Pts',(96.499888464771,11.6554845981431,56.9414402003286));
#144810=CARTESIAN_POINT('Ctrl Pts',(96.5019986356943,11.6270641292994,56.9277098101259));
#144811=CARTESIAN_POINT('Ctrl Pts',(96.5048277488586,11.588960712341,56.9093014303847));
#144812=CARTESIAN_POINT('Ctrl Pts',(96.5077358157164,11.5519073988749,56.891475448813));
#144813=CARTESIAN_POINT('Ctrl Pts',(96.5107462434937,11.5157755464754,56.8741086777739));
#144814=CARTESIAN_POINT('Ctrl Pts',(97.3598553272691,12.59304662146,57.34302211945));
#144815=CARTESIAN_POINT('Ctrl Pts',(97.2905909335691,12.48457249915,57.27739215867));
#144816=CARTESIAN_POINT('Ctrl Pts',(97.1823916103691,12.29078220396,57.16980269553));
#144817=CARTESIAN_POINT('Ctrl Pts',(97.0407277756691,12.03891918979,57.04853971653));
#144818=CARTESIAN_POINT('Ctrl Pts',(96.9065972293691,11.77555579319,56.93603687571));
#144819=CARTESIAN_POINT('Ctrl Pts',(96.8118741496691,11.52347507691,56.83220141859));
#144820=CARTESIAN_POINT('Ctrl Pts',(96.7553526290691,11.35053149358,56.75991005414));
#144821=CARTESIAN_POINT('Ctrl Pts',(96.4155772962691,12.57897283386,57.47256425052));
#144822=CARTESIAN_POINT('Ctrl Pts',(96.3548004162691,12.47093811279,57.4066316253));
#144823=CARTESIAN_POINT('Ctrl Pts',(96.2601630177691,12.27776084815,57.2986569495));
#144824=CARTESIAN_POINT('Ctrl Pts',(96.1360036193691,12.02333015192,57.17498429364));
#144825=CARTESIAN_POINT('Ctrl Pts',(96.0179323943691,11.75617400365,57.05956940227));
#144826=CARTESIAN_POINT('Ctrl Pts',(95.9345062497691,11.50262773359,56.95458058277));
#144827=CARTESIAN_POINT('Ctrl Pts',(95.8848951356691,11.3292765712,56.88185866928));
#144828=CARTESIAN_POINT('Ctrl Pts',(94.2594273773691,12.53398823169,57.75933364546));
#144829=CARTESIAN_POINT('Ctrl Pts',(94.2182042994691,12.4271741912,57.6935704398));
#144830=CARTESIAN_POINT('Ctrl Pts',(94.1547707708691,12.23637559016,57.58613155241));
#144831=CARTESIAN_POINT('Ctrl Pts',(94.0707455882691,11.97320006148,57.45632676081));
#144832=CARTESIAN_POINT('Ctrl Pts',(93.9893028835691,11.69394466693,57.33289395567));
#144833=CARTESIAN_POINT('Ctrl Pts',(93.9314988904691,11.4384415765,57.2258100722));
#144834=CARTESIAN_POINT('Ctrl Pts',(93.8975579673691,11.26636189084,57.15304096365));
#144835=CARTESIAN_POINT('Ctrl Pts',(92.1249207086691,12.45611361649,58.0505002254));
#144836=CARTESIAN_POINT('Ctrl Pts',(92.1032618890691,12.35145474945,57.98614284192));
#144837=CARTESIAN_POINT('Ctrl Pts',(92.0710528306691,12.16481527354,57.88111746708));
#144838=CARTESIAN_POINT('Ctrl Pts',(92.0271469727691,11.8851148392,57.74207150913));
#144839=CARTESIAN_POINT('Ctrl Pts',(91.9820262412691,11.58554660934,57.60607342512));
#144840=CARTESIAN_POINT('Ctrl Pts',(91.9492978565691,11.33112885221,57.49706203015));
#144841=CARTESIAN_POINT('Ctrl Pts',(91.9306629864691,11.16481243865,57.42570847496));
#144842=CARTESIAN_POINT('Ctrl Pts',(90.9201693766691,12.4015395951,58.23050592227));
#144843=CARTESIAN_POINT('Ctrl Pts',(90.9095559520691,12.29862098453,58.16703117139));
#144844=CARTESIAN_POINT('Ctrl Pts',(90.8950120714691,12.11470097399,58.0633845424));
#144845=CARTESIAN_POINT('Ctrl Pts',(90.8739785056691,11.82255160128,57.91735245787));
#144846=CARTESIAN_POINT('Ctrl Pts',(90.8494994559691,11.50865392223,57.77212231743));
#144847=CARTESIAN_POINT('Ctrl Pts',(90.8307945255691,11.25577205409,57.6615810195));
#144848=CARTESIAN_POINT('Ctrl Pts',(90.8206727756691,11.09390799359,57.59118585437));
#144849=CARTESIAN_POINT('Ctrl Pts',(96.3228725566692,-10.13609008452,56.32369383094));
#144850=CARTESIAN_POINT('Ctrl Pts',(96.3073991073691,-10.32332545426,56.40329742928));
#144851=CARTESIAN_POINT('Ctrl Pts',(96.2766341738692,-10.6804967028,56.56156850188));
#144852=CARTESIAN_POINT('Ctrl Pts',(96.2323525649691,-11.16575807496,56.7893764936));
#144853=CARTESIAN_POINT('Ctrl Pts',(96.2043598232691,-11.46454615057,56.93338594698));
#144854=CARTESIAN_POINT('Ctrl Pts',(96.1917988812692,-11.59798170647,56.99800606902));
#144855=CARTESIAN_POINT('Ctrl Pts',(97.7297501322691,-10.43195556948,55.90123229366));
#144856=CARTESIAN_POINT('Ctrl Pts',(97.7137150971691,-10.6259862983,55.98372498668));
#144857=CARTESIAN_POINT('Ctrl Pts',(97.6818999404691,-10.99529135564,56.14739896205));
#144858=CARTESIAN_POINT('Ctrl Pts',(97.6366458245691,-11.49114086689,56.3802100435801));
#144859=CARTESIAN_POINT('Ctrl Pts',(97.6083601074691,-11.79304779847,56.52572671727));
#144860=CARTESIAN_POINT('Ctrl Pts',(97.5957180332691,-11.92734449924,56.59076422634));
#144861=CARTESIAN_POINT('Ctrl Pts',(98.7678990136691,-10.08298790648,56.92386767886));
#144862=CARTESIAN_POINT('Ctrl Pts',(98.7525263582691,-10.26900363965,57.00295274013));
#144863=CARTESIAN_POINT('Ctrl Pts',(98.7219499196691,-10.62399710232,57.16025409535));
#144864=CARTESIAN_POINT('Ctrl Pts',(98.6778428571691,-11.10735810665,57.38716412844));
#144865=CARTESIAN_POINT('Ctrl Pts',(98.6499026988691,-11.40558640745,57.53090306468));
#144866=CARTESIAN_POINT('Ctrl Pts',(98.6373563185692,-11.53886740437,57.59544827376));
#144867=CARTESIAN_POINT('Ctrl Pts',(98.2166477117691,-9.49950866349698,
58.18916950595));
#144868=CARTESIAN_POINT('Ctrl Pts',(98.2023825655691,-9.67212320196098,
58.2625569551));
#144869=CARTESIAN_POINT('Ctrl Pts',(98.1738772823691,-10.00318746055,58.40920319245));
#144870=CARTESIAN_POINT('Ctrl Pts',(98.1316881104691,-10.46566749127,58.62624658273));
#144871=CARTESIAN_POINT('Ctrl Pts',(98.1043257318692,-10.75774506542,58.76701311493));
#144872=CARTESIAN_POINT('Ctrl Pts',(98.0919393532691,-10.88932779005,58.83073519093));
#144873=CARTESIAN_POINT('',(96.5106393256908,-11.5155612869847,56.8741302054996));
#144874=CARTESIAN_POINT('Ctrl Pts',(96.6021949941369,-10.33475523448,56.3300847780136));
#144875=CARTESIAN_POINT('Ctrl Pts',(96.5948822022228,-10.435748834368,56.3737520728817));
#144876=CARTESIAN_POINT('Ctrl Pts',(96.5874571230913,-10.5359169900225,
56.4179778623221));
#144877=CARTESIAN_POINT('Ctrl Pts',(96.5799409457604,-10.635428958833,56.4626894439106));
#144878=CARTESIAN_POINT('Ctrl Pts',(96.5741108888598,-10.7126171909511,
56.4973707790231));
#144879=CARTESIAN_POINT('Ctrl Pts',(96.5682259870746,-10.7894129763387,
56.5323441573885));
#144880=CARTESIAN_POINT('Ctrl Pts',(96.5622983146813,-10.8658798203598,
56.567554048647));
#144881=CARTESIAN_POINT('Ctrl Pts',(96.556828481434,-10.9364405494262,56.600044412665));
#144882=CARTESIAN_POINT('Ctrl Pts',(96.5513222058239,-11.0067221225276,
56.6327362197256));
#144883=CARTESIAN_POINT('Ctrl Pts',(96.5457914507374,-11.0767403757038,
56.6655656323231));
#144884=CARTESIAN_POINT('Ctrl Pts',(96.5405297524791,-11.1433524232494,
56.6967979795132));
#144885=CARTESIAN_POINT('Ctrl Pts',(96.5352458876006,-11.2097266735917,
56.7281548929787));
#144886=CARTESIAN_POINT('Ctrl Pts',(96.5299527321305,-11.2758345850683,
56.7595617552571));
#144887=CARTESIAN_POINT('Ctrl Pts',(96.5248807987823,-11.3391795827159,
56.7896559992396));
#144888=CARTESIAN_POINT('Ctrl Pts',(96.519800335829,-11.4022802633477,56.8197960704493));
#144889=CARTESIAN_POINT('Ctrl Pts',(96.5147251649627,-11.4650665900728,
56.8498979075562));
#144890=CARTESIAN_POINT('Ctrl Pts',(96.5133627229575,-11.4819217327144,
56.8579788191922));
#144891=CARTESIAN_POINT('Ctrl Pts',(96.5120006766485,-11.4987539524958,
56.8660568709375));
#144892=CARTESIAN_POINT('Ctrl Pts',(96.5106393253565,-11.5155612875649,
56.8741302042353));
#144893=CARTESIAN_POINT('Origin',(96.7134217792691,-10.8854245001,58.22016396893));
#144894=CARTESIAN_POINT('Ctrl Pts',(96.2319806560691,-11.31915553447,56.85809517453));
#144895=CARTESIAN_POINT('Ctrl Pts',(96.2313075516691,-11.32636229438,56.8615579791));
#144896=CARTESIAN_POINT('Ctrl Pts',(96.2269271353691,-11.3732593077,56.88409315519));
#144897=CARTESIAN_POINT('Ctrl Pts',(96.2187625258692,-11.46060590276,56.92609622013));
#144898=CARTESIAN_POINT('Ctrl Pts',(96.2073028932692,-11.58253166397,56.98505062475));
#144899=CARTESIAN_POINT('Ctrl Pts',(96.1954645381691,-11.70692018984,57.04595337828));
#144900=CARTESIAN_POINT('Ctrl Pts',(96.1829463911691,-11.83547271731,57.11035333984));
#144901=CARTESIAN_POINT('Ctrl Pts',(96.1687179031691,-11.97470333685,57.18355220011));
#144902=CARTESIAN_POINT('Ctrl Pts',(96.1529902214692,-12.11658703733,57.2644637043));
#144903=CARTESIAN_POINT('Ctrl Pts',(96.1369908001691,-12.25127581358,57.34677318043));
#144904=CARTESIAN_POINT('Ctrl Pts',(96.1203673447691,-12.38344363953,57.43229301775));
#144905=CARTESIAN_POINT('Ctrl Pts',(96.1071896113692,-12.48167452487,57.50008624114));
#144906=CARTESIAN_POINT('Ctrl Pts',(96.0993554236692,-12.53698100232,57.5403894418501));
#144907=CARTESIAN_POINT('Ctrl Pts',(96.0978863429691,-12.54724815652,57.54794716878));
#144908=CARTESIAN_POINT('Ctrl Pts',(97.6310403542691,-11.63858287431,56.46525177409));
#144909=CARTESIAN_POINT('Ctrl Pts',(97.6303662018692,-11.64580085354,56.46871997001));
#144910=CARTESIAN_POINT('Ctrl Pts',(97.6259760867691,-11.69280167865,56.4913050417201));
#144911=CARTESIAN_POINT('Ctrl Pts',(97.6177567136691,-11.78073412854,56.53358983964));
#144912=CARTESIAN_POINT('Ctrl Pts',(97.6060926281691,-11.90484126191,56.5935960578001));
#144913=CARTESIAN_POINT('Ctrl Pts',(97.5938327508691,-12.03366062773,56.6566673441101));
#144914=CARTESIAN_POINT('Ctrl Pts',(97.5804970871691,-12.17067970326,56.7252730443601));
#144915=CARTESIAN_POINT('Ctrl Pts',(97.5643968403691,-12.32833263289,56.8081012202001));
#144916=CARTESIAN_POINT('Ctrl Pts',(97.5462329964691,-12.49217228257,56.9015456297601));
#144917=CARTESIAN_POINT('Ctrl Pts',(97.5283143898692,-12.6429610529,56.99372840947));
#144918=CARTESIAN_POINT('Ctrl Pts',(97.5095746503691,-12.79199140804,57.09013553031));
#144919=CARTESIAN_POINT('Ctrl Pts',(97.4944008867691,-12.90518115369,57.16819738757));
#144920=CARTESIAN_POINT('Ctrl Pts',(97.4850324848691,-12.9713358854,57.21639339649));
#144921=CARTESIAN_POINT('Ctrl Pts',(97.4832630223691,-12.98370914531,57.2254964466401));
#144922=CARTESIAN_POINT('Ctrl Pts',(98.6598999117692,-11.25268497975,57.4683762086));
#144923=CARTESIAN_POINT('Ctrl Pts',(98.6592270254691,-11.259889405,57.47183789127));
#144924=CARTESIAN_POINT('Ctrl Pts',(98.6548486273692,-11.30676481583,57.49436268444));
#144925=CARTESIAN_POINT('Ctrl Pts',(98.6466954137691,-11.39398949866,57.5363071227601));
#144926=CARTESIAN_POINT('Ctrl Pts',(98.6352783263692,-11.51546133186,57.59504265246));
#144927=CARTESIAN_POINT('Ctrl Pts',(98.6235276870692,-11.63892783149,57.65549414976));
#144928=CARTESIAN_POINT('Ctrl Pts',(98.6111796595691,-11.7657185306,57.71901892705));
#144929=CARTESIAN_POINT('Ctrl Pts',(98.5973406711692,-11.9011155986,57.79021399533));
#144930=CARTESIAN_POINT('Ctrl Pts',(98.5821199374691,-12.03843042241,57.86851749115));
#144931=CARTESIAN_POINT('Ctrl Pts',(98.5665198849691,-12.16976890454,57.94877240313));
#144932=CARTESIAN_POINT('Ctrl Pts',(98.5503368132692,-12.29842775824,58.03202667427));
#144933=CARTESIAN_POINT('Ctrl Pts',(98.5375744394691,-12.39354581128,58.0976830680801));
#144934=CARTESIAN_POINT('Ctrl Pts',(98.5300595107692,-12.44659484427,58.1363438316));
#144935=CARTESIAN_POINT('Ctrl Pts',(98.5286529374691,-12.45642373287,58.14357998778));
#144936=CARTESIAN_POINT('Ctrl Pts',(98.1179556775691,-10.61177639351,58.6968958282));
#144937=CARTESIAN_POINT('Ctrl Pts',(98.117284893969,-10.61895830798,58.70034669351));
#144938=CARTESIAN_POINT('Ctrl Pts',(98.1129259557691,-10.66562542773,58.72277137462));
#144939=CARTESIAN_POINT('Ctrl Pts',(98.1048826215691,-10.75167463385,58.76415053543));
#144940=CARTESIAN_POINT('Ctrl Pts',(98.093875754469,-10.86876969659,58.82077567492));
#144941=CARTESIAN_POINT('Ctrl Pts',(98.082970869869,-10.98334602619,58.87687616307));
#144942=CARTESIAN_POINT('Ctrl Pts',(98.072263132669,-11.09314918956,58.93196242022));
#144943=CARTESIAN_POINT('Ctrl Pts',(98.062179696969,-11.19158318259,58.98383694122));
#144944=CARTESIAN_POINT('Ctrl Pts',(98.0518469520691,-11.28484493202,59.03699404015));
#144945=CARTESIAN_POINT('Ctrl Pts',(98.0400976106691,-11.38387990358,59.09743885998));
#144946=CARTESIAN_POINT('Ctrl Pts',(98.028160714769,-11.47870527343,59.15884855924));
#144947=CARTESIAN_POINT('Ctrl Pts',(98.0194032357691,-11.5438094209,59.20390165835));
#144948=CARTESIAN_POINT('Ctrl Pts',(98.014966600369,-11.57509219147,59.22672605496));
#144949=CARTESIAN_POINT('Ctrl Pts',(98.0141627222692,-11.58069532646,59.23086162834));
#144950=CARTESIAN_POINT('',(96.4484068068018,-12.4473571364169,57.3800828637172));
#144951=CARTESIAN_POINT('Ctrl Pts',(96.4484069697816,-12.447356425455,57.3800839617248));
#144952=CARTESIAN_POINT('Ctrl Pts',(96.4893190913068,-12.4538771542219,
57.378233981164));
#144953=CARTESIAN_POINT('Ctrl Pts',(96.5312830311879,-12.4596052833508,
57.3777807178534));
#144954=CARTESIAN_POINT('Ctrl Pts',(96.5741400434367,-12.4644013848093,
57.3789024988894));
#144955=CARTESIAN_POINT('Ctrl Pts',(96.6157010964277,-12.4690524562772,
57.3799903582299));
#144956=CARTESIAN_POINT('Ctrl Pts',(96.6581018844681,-12.4728266228935,
57.3825600077121));
#144957=CARTESIAN_POINT('Ctrl Pts',(96.7011513468475,-12.4756001614079,
57.3867599081895));
#144958=CARTESIAN_POINT('Ctrl Pts',(96.7435267318481,-12.478330271283,57.3908940457572));
#144959=CARTESIAN_POINT('Ctrl Pts',(96.7865304254406,-12.4800904383511,
57.3966083483396));
#144960=CARTESIAN_POINT('Ctrl Pts',(96.8299370827375,-12.4807719117444,
57.404022119513));
#144961=CARTESIAN_POINT('Ctrl Pts',(96.8737937555444,-12.4814604502659,
57.4115127524449));
#144962=CARTESIAN_POINT('Ctrl Pts',(96.9180615393185,-12.4810473177835,
57.4207389690825));
#144963=CARTESIAN_POINT('Ctrl Pts',(96.9624667943407,-12.4794367139336,
57.4317912123836));
#144964=CARTESIAN_POINT('Ctrl Pts',(97.0068720493629,-12.4778261100836,
57.4428434556847));
#144965=CARTESIAN_POINT('Ctrl Pts',(97.0514142010242,-12.4750175693876,
57.4557223128417));
#144966=CARTESIAN_POINT('Ctrl Pts',(97.0957849195706,-12.470938813128,57.4704761434959));
#144967=CARTESIAN_POINT('Ctrl Pts',(97.1377011296428,-12.4670856863405,
57.4844138187315));
#144968=CARTESIAN_POINT('Ctrl Pts',(97.1794634177598,-12.4620989057031,
57.5000247223907));
#144969=CARTESIAN_POINT('Ctrl Pts',(97.2207917445358,-12.4559422742179,
57.5173087968349));
#144970=CARTESIAN_POINT('Ctrl Pts',(97.2617036898199,-12.4498476705862,
57.5344187348147));
#144971=CARTESIAN_POINT('Ctrl Pts',(97.3021896319551,-12.4426064948674,
57.5531684176607));
#144972=CARTESIAN_POINT('Ctrl Pts',(97.3419691595277,-12.434210692175,57.5735154359813));
#144973=CARTESIAN_POINT('Ctrl Pts',(97.3814382133613,-12.4258804175673,
57.5937036486236));
#144974=CARTESIAN_POINT('Ctrl Pts',(97.4202110615909,-12.4164133950479,
57.6154643206232));
#144975=CARTESIAN_POINT('Ctrl Pts',(97.4580164616892,-12.4058304019727,
57.638713508724));
#144976=CARTESIAN_POINT('Ctrl Pts',(97.4955830607536,-12.3953142572759,
57.6618158413454));
#144977=CARTESIAN_POINT('Ctrl Pts',(97.5321936397794,-12.3836962334291,
57.6863877413472));
#144978=CARTESIAN_POINT('Ctrl Pts',(97.5675961378212,-12.3710253925851,
57.7123065004887));
#144979=CARTESIAN_POINT('Ctrl Pts',(97.6029196551025,-12.3583828195952,
57.7381674364984));
#144980=CARTESIAN_POINT('Ctrl Pts',(97.6370397771934,-12.3446922587843,
57.7653688874088));
#144981=CARTESIAN_POINT('Ctrl Pts',(97.6697311107884,-12.3300298030798,
57.7937527192353));
#144982=CARTESIAN_POINT('Ctrl Pts',(97.7024160707833,-12.3153702060115,
57.8221310172651));
#144983=CARTESIAN_POINT('Ctrl Pts',(97.7336722081264,-12.2997393319065,
57.851690761331));
#144984=CARTESIAN_POINT('Ctrl Pts',(97.7633089944017,-12.2832377915447,
57.882243760512));
#144985=CARTESIAN_POINT('Ctrl Pts',(97.7930004653707,-12.2667058031555,
57.9128531349486));
#144986=CARTESIAN_POINT('Ctrl Pts',(97.8210661605585,-12.24930025847,57.94445885743));
#144987=CARTESIAN_POINT('Ctrl Pts',(97.8473571927605,-12.2311427286913,
57.9768493419059));
#144988=CARTESIAN_POINT('Ctrl Pts',(97.8738603842561,-12.2128386740951,
58.0095012060892));
#144989=CARTESIAN_POINT('Ctrl Pts',(97.898559852216,-12.1937708354519,58.042949909243));
#144990=CARTESIAN_POINT('Ctrl Pts',(97.9213521725345,-12.1740790873495,
58.0769652049586));
#144991=CARTESIAN_POINT('Ctrl Pts',(97.9442669650766,-12.1542815276342,
58.1111632784186));
#144992=CARTESIAN_POINT('Ctrl Pts',(97.9652539912341,-12.1338537746444,
58.1459333767709));
#144993=CARTESIAN_POINT('Ctrl Pts',(97.9842603705065,-12.1129471224486,
58.1810379229406));
#144994=CARTESIAN_POINT('Ctrl Pts',(98.0035173027979,-12.0917648667436,
58.2166052374207));
#144995=CARTESIAN_POINT('Ctrl Pts',(98.0207411070807,-12.0700914563442,
58.2525152097198));
#144996=CARTESIAN_POINT('Ctrl Pts',(98.0359302430688,-12.0480868126932,
58.2885272816885));
#144997=CARTESIAN_POINT('Ctrl Pts',(98.0481980866499,-12.030314272729,58.3176132327453));
#144998=CARTESIAN_POINT('Ctrl Pts',(98.0591397681909,-12.0123257910484,
58.3467658050509));
#144999=CARTESIAN_POINT('Ctrl Pts',(98.0687781393095,-11.9942038529267,
58.3758655187164));
#145000=CARTESIAN_POINT('Ctrl Pts',(98.0809676575064,-11.9712852817514,
58.4126675348335));
#145001=CARTESIAN_POINT('Ctrl Pts',(98.0910715461646,-11.9481538719064,
58.449383929842));
#145002=CARTESIAN_POINT('Ctrl Pts',(98.099178380364,-11.9249674616475,58.485794544027));
#145003=CARTESIAN_POINT('Ctrl Pts',(98.1077036599592,-11.9005842529365,
58.524084542136));
#145004=CARTESIAN_POINT('Ctrl Pts',(98.1140208053483,-11.876140710328,58.5620357186189));
#145005=CARTESIAN_POINT('Ctrl Pts',(98.118278757214,-11.851802770553,58.5994274744218));
#145006=CARTESIAN_POINT('Ctrl Pts',(98.1224939549306,-11.8277092083423,
58.636443779127));
#145007=CARTESIAN_POINT('Ctrl Pts',(98.1246919997929,-11.8037193227494,
58.6729117391277));
#145008=CARTESIAN_POINT('Ctrl Pts',(98.1250506186695,-11.7799723843313,
58.7086564524736));
#145009=CARTESIAN_POINT('Ctrl Pts',(98.1254196683622,-11.7555347406445,
58.7454408392881));
#145010=CARTESIAN_POINT('Ctrl Pts',(98.1238414891517,-11.7313546018995,
58.7814591122462));
#145011=CARTESIAN_POINT('Ctrl Pts',(98.1205327574654,-11.7075573331155,
58.8165648437517));
#145012=CARTESIAN_POINT('Ctrl Pts',(98.1173132273221,-11.6844016252964,
58.8507241445059));
#145013=CARTESIAN_POINT('Ctrl Pts',(98.1124559595994,-11.6616082826077,
58.8840198016753));
#145014=CARTESIAN_POINT('Ctrl Pts',(98.1061703789843,-11.63926799201,58.9163561174313));
#145015=CARTESIAN_POINT('Ctrl Pts',(96.5106393247643,-11.5155613004658,
56.8741302153513));
#145016=CARTESIAN_POINT('Ctrl Pts',(96.5066749286283,-11.5631862216957,
56.8970227527718));
#145017=CARTESIAN_POINT('Ctrl Pts',(96.5030313220881,-11.6080902015577,
56.918671656639));
#145018=CARTESIAN_POINT('Ctrl Pts',(96.4996983376335,-11.6502777389037,
56.9391304643533));
#145019=CARTESIAN_POINT('Ctrl Pts',(96.4963653531789,-11.6924652762497,
56.9595892720676));
#145020=CARTESIAN_POINT('Ctrl Pts',(96.4933429523757,-11.7319365505139,
56.9788582111886));
#145021=CARTESIAN_POINT('Ctrl Pts',(96.4906224361774,-11.7687490610692,
56.9969987578413));
#145022=CARTESIAN_POINT('Ctrl Pts',(96.4899581736939,-11.7777374911698,
57.0014280953984));
#145023=CARTESIAN_POINT('Ctrl Pts',(96.4893117294717,-11.7865742664474,
57.0057934108544));
#145024=CARTESIAN_POINT('Ctrl Pts',(96.4886826702735,-11.7952521909895,
57.0100916153233));
#145025=CARTESIAN_POINT('Ctrl Pts',(96.4867353898755,-11.8221150878399,
57.0233968961805));
#145026=CARTESIAN_POINT('Ctrl Pts',(96.4849547223737,-11.8474563107511,
57.0360607843061));
#145027=CARTESIAN_POINT('Ctrl Pts',(96.4833381269162,-11.8713352449221,
57.0481183769609));
#145028=CARTESIAN_POINT('Ctrl Pts',(96.4822687126468,-11.8871316971652,
57.0560947458044));
#145029=CARTESIAN_POINT('Ctrl Pts',(96.481271504146,-11.9022829407061,57.0638029876073));
#145030=CARTESIAN_POINT('Ctrl Pts',(96.4803555906446,-11.9167127980408,
57.0711991016382));
#145031=CARTESIAN_POINT('Ctrl Pts',(96.4798976338939,-11.9239277267081,
57.0748971586537));
#145032=CARTESIAN_POINT('Ctrl Pts',(96.47946022252,-11.9309599342884,57.0785158470131));
#145033=CARTESIAN_POINT('Ctrl Pts',(96.4790447553625,-11.9377979344283,
57.0820479225602));
#145034=CARTESIAN_POINT('Ctrl Pts',(96.4787394115283,-11.9428234608584,
57.0846437895757));
#145035=CARTESIAN_POINT('Ctrl Pts',(96.4784827063687,-11.9470974167123,
57.0868576939403));
#145036=CARTESIAN_POINT('Ctrl Pts',(96.4781940917681,-11.9520431752827,
57.0894262281173));
#145037=CARTESIAN_POINT('Ctrl Pts',(96.4780900019015,-11.9538268804346,
57.090352578965));
#145038=CARTESIAN_POINT('Ctrl Pts',(96.477981737352,-11.9556975042579,57.0913249890787));
#145039=CARTESIAN_POINT('Ctrl Pts',(96.4778654307572,-11.9577201783725,
57.0923778281301));
#145040=CARTESIAN_POINT('Ctrl Pts',(96.4770494692035,-11.9719104684157,
57.0997641349011));
#145041=CARTESIAN_POINT('Ctrl Pts',(96.4761923774212,-11.9868735820673,
57.1076221122303));
#145042=CARTESIAN_POINT('Ctrl Pts',(96.4752940421185,-12.002493003654,57.1159265339759));
#145043=CARTESIAN_POINT('Ctrl Pts',(96.4748697035453,-12.0098710094506,
57.1198492190405));
#145044=CARTESIAN_POINT('Ctrl Pts',(96.4744361763087,-12.0173960951725,
57.1238718803706));
#145045=CARTESIAN_POINT('Ctrl Pts',(96.4739935249068,-12.0250595572787,
57.1279938365111));
#145046=CARTESIAN_POINT('Ctrl Pts',(96.472933032369,-12.0434194773924,57.1378691101673));
#145047=CARTESIAN_POINT('Ctrl Pts',(96.4718199186621,-12.0625706369947,
57.1483134352813));
#145048=CARTESIAN_POINT('Ctrl Pts',(96.4706592173138,-12.0823880798194,
57.1592984892521));
#145049=CARTESIAN_POINT('Ctrl Pts',(96.4694477493664,-12.1030722952861,
57.1707640060321));
#145050=CARTESIAN_POINT('Ctrl Pts',(96.4681844326933,-12.1244823456784,
57.1828188137631));
#145051=CARTESIAN_POINT('Ctrl Pts',(96.4668787205247,-12.146531406365,57.1954486131704));
#145052=CARTESIAN_POINT('Ctrl Pts',(96.4663072983083,-12.1561807942083,
57.2009758251726));
#145053=CARTESIAN_POINT('Ctrl Pts',(96.4657278037075,-12.1659532578178,
57.206613363283));
#145054=CARTESIAN_POINT('Ctrl Pts',(96.465141233958,-12.1758444703791,57.2123607911272));
#145055=CARTESIAN_POINT('Ctrl Pts',(96.4639672349064,-12.1956413899699,
57.2238640690296));
#145056=CARTESIAN_POINT('Ctrl Pts',(96.4627716846492,-12.2156634952071,
57.2356621888345));
#145057=CARTESIAN_POINT('Ctrl Pts',(96.4615437003296,-12.2361742041662,
57.2479153418891));
#145058=CARTESIAN_POINT('Ctrl Pts',(96.4600634931821,-12.2608977267049,
57.2626852411802));
#145059=CARTESIAN_POINT('Ctrl Pts',(96.4585362478738,-12.2863371469124,
57.2781186113081));
#145060=CARTESIAN_POINT('Ctrl Pts',(96.4569321323794,-12.3126258335614,
57.294351191593));
#145061=CARTESIAN_POINT('Ctrl Pts',(96.4556292751448,-12.3339774168546,
57.3075352389607));
#145062=CARTESIAN_POINT('Ctrl Pts',(96.4542757135791,-12.355889621406,57.321247095118));
#145063=CARTESIAN_POINT('Ctrl Pts',(96.4528558209465,-12.3784018160607,
57.3355555749792));
#145064=CARTESIAN_POINT('Ctrl Pts',(96.4514434113654,-12.4007953680047,
57.349788646962));
#145065=CARTESIAN_POINT('Ctrl Pts',(96.4499653524067,-12.4237840599592,
57.3646127482254));
#145066=CARTESIAN_POINT('Ctrl Pts',(96.4484067536389,-12.447357368126,57.3800825052753));
#145067=CARTESIAN_POINT('Ctrl Pts',(90.9278844222691,-12.40246332161,58.22971617592));
#145068=CARTESIAN_POINT('Ctrl Pts',(90.9171817651691,-12.29937061118,58.16611616086));
#145069=CARTESIAN_POINT('Ctrl Pts',(90.9025093010691,-12.11530240729,58.06236938668));
#145070=CARTESIAN_POINT('Ctrl Pts',(90.8813150710691,-11.82300855506,57.91626489308));
#145071=CARTESIAN_POINT('Ctrl Pts',(90.8566702536691,-11.50876591956,57.77089205131));
#145072=CARTESIAN_POINT('Ctrl Pts',(90.8378431748691,-11.25540710816,57.660165762));
#145073=CARTESIAN_POINT('Ctrl Pts',(90.8276461323691,-11.0930235466,57.58955284956));
#145074=CARTESIAN_POINT('Ctrl Pts',(93.0012603032691,-12.49640477047,57.92011916884));
#145075=CARTESIAN_POINT('Ctrl Pts',(92.9715256168691,-12.39034853487,57.85501455448));
#145076=CARTESIAN_POINT('Ctrl Pts',(92.9264209346691,-12.20156124715,57.74887203586));
#145077=CARTESIAN_POINT('Ctrl Pts',(92.8658417595691,-11.93067689713,57.61478182321));
#145078=CARTESIAN_POINT('Ctrl Pts',(92.8056300846691,-11.64110581084,57.48530032852));
#145079=CARTESIAN_POINT('Ctrl Pts',(92.7626282873691,-11.38507271696,57.37719145258));
#145080=CARTESIAN_POINT('Ctrl Pts',(92.7377365505691,-11.21498097297,57.30490731823));
#145081=CARTESIAN_POINT('Ctrl Pts',(95.0799851341691,-12.55698062284,57.65477957029));
#145082=CARTESIAN_POINT('Ctrl Pts',(95.0311505215691,-12.44946610374,57.5884392369));
#145083=CARTESIAN_POINT('Ctrl Pts',(94.9556138692691,-12.25709808174,57.47998237856));
#145084=CARTESIAN_POINT('Ctrl Pts',(94.8560974936691,-11.99852059974,57.35274250657));
#145085=CARTESIAN_POINT('Ctrl Pts',(94.7605596055691,-11.72521941751,57.23289934619));
#145086=CARTESIAN_POINT('Ctrl Pts',(94.6929890760691,-11.46925250975,57.12614789029));
#145087=CARTESIAN_POINT('Ctrl Pts',(94.6530499956691,-11.29502925224,57.05268887033));
#145088=CARTESIAN_POINT('Ctrl Pts',(97.1903838030691,-12.59070340104,57.36655831744));
#145089=CARTESIAN_POINT('Ctrl Pts',(97.1225479932691,-12.48219631072,57.30079562324));
#145090=CARTESIAN_POINT('Ctrl Pts',(97.0166594629691,-12.28831915113,57.19301649588));
#145091=CARTESIAN_POINT('Ctrl Pts',(96.8780171988691,-12.03579204712,57.07122310877));
#145092=CARTESIAN_POINT('Ctrl Pts',(96.7465770377691,-11.77136893742,56.9580407289));
#145093=CARTESIAN_POINT('Ctrl Pts',(96.6537324103691,-11.51851036624,56.85379357844));
#145094=CARTESIAN_POINT('Ctrl Pts',(96.5983080857691,-11.34492571889,56.78118190673));
#145095=CARTESIAN_POINT('Ctrl Pts',(90.9923722612358,-11.2699867077028,
57.6397093617629));
#145096=CARTESIAN_POINT('Ctrl Pts',(92.8191441570593,-11.3889082784922,
57.3718321147041));
#145097=CARTESIAN_POINT('Ctrl Pts',(94.6514920487796,-11.4676844930577,
57.1318009631947));
#145098=CARTESIAN_POINT('Ctrl Pts',(96.5106393247643,-11.5155613004658,
56.8741302153513));
#145099=CARTESIAN_POINT('Ctrl Pts',(91.0788478348321,-12.2836022595699,
58.1301370595523));
#145100=CARTESIAN_POINT('Ctrl Pts',(92.2850753424178,-12.3359375090943,
57.9484854194747));
#145101=CARTESIAN_POINT('Ctrl Pts',(93.4933486351873,-12.3773001586785,
57.7816267963501));
#145102=CARTESIAN_POINT('Ctrl Pts',(94.7090794812645,-12.4088635897447,
57.6162793126818));
#145103=CARTESIAN_POINT('Ctrl Pts',(95.2869785032647,-12.4238673021232,
57.5376812007639));
#145104=CARTESIAN_POINT('Ctrl Pts',(95.866561870591,-12.4366566914144,57.4594245164494));
#145105=CARTESIAN_POINT('Ctrl Pts',(96.4484067536153,-12.4473573684819,
57.3800825055088));
#145106=CARTESIAN_POINT('Ctrl Pts',(91.7196664240691,-14.99486169804,63.073579399731));
#145107=CARTESIAN_POINT('Ctrl Pts',(91.6086219852691,-15.02536569563,62.38693020624));
#145108=CARTESIAN_POINT('Ctrl Pts',(91.3904040401691,-14.82128093489,61.04174493848));
#145109=CARTESIAN_POINT('Ctrl Pts',(91.1055790545691,-13.80539132818,59.26782647843));
#145110=CARTESIAN_POINT('Ctrl Pts',(90.9674151548691,-12.74459813474,58.4019492402));
#145111=CARTESIAN_POINT('Ctrl Pts',(90.9189065908691,-12.15226092818,58.08327559231));
#145112=CARTESIAN_POINT('Ctrl Pts',(94.5341587467691,-14.99518185508,62.57017586031));
#145113=CARTESIAN_POINT('Ctrl Pts',(94.3058556568691,-15.02368077332,61.93133855973));
#145114=CARTESIAN_POINT('Ctrl Pts',(93.8619238271691,-14.84035203637,60.68236085645));
#145115=CARTESIAN_POINT('Ctrl Pts',(93.2453658119691,-13.87785869838,58.97788256701));
#145116=CARTESIAN_POINT('Ctrl Pts',(92.9143512058691,-12.83695860105,58.12194824018));
#145117=CARTESIAN_POINT('Ctrl Pts',(92.7770364957691,-12.23327460907,57.79774621738));
#145118=CARTESIAN_POINT('Ctrl Pts',(97.3508737698691,-14.99520415789,62.08198995714));
#145119=CARTESIAN_POINT('Ctrl Pts',(97.0060920033691,-15.01646079956,61.49512945037));
#145120=CARTESIAN_POINT('Ctrl Pts',(96.3371921958691,-14.84261766533,60.34754264612));
#145121=CARTESIAN_POINT('Ctrl Pts',(95.3895471494691,-13.92370897909,58.72466409135));
#145122=CARTESIAN_POINT('Ctrl Pts',(94.8658120496691,-12.90001659179,57.87944249812));
#145123=CARTESIAN_POINT('Ctrl Pts',(94.6396504020691,-12.28798925498,57.54917879558));
#145124=CARTESIAN_POINT('Ctrl Pts',(100.153009715269,-14.99408560257,61.51961813125));
#145125=CARTESIAN_POINT('Ctrl Pts',(99.6992618204691,-15.00733180495,60.98982798051));
#145126=CARTESIAN_POINT('Ctrl Pts',(98.8190522278691,-14.83552964287,59.95248048231));
#145127=CARTESIAN_POINT('Ctrl Pts',(97.5553693844691,-13.94727437632,58.43815492047));
#145128=CARTESIAN_POINT('Ctrl Pts',(96.8420798112691,-12.93817712032,57.6191720668));
#145129=CARTESIAN_POINT('Ctrl Pts',(96.5270565421691,-12.32101949327,57.28901682961));
#145130=CARTESIAN_POINT('',(95.9754284248432,-14.9956419886409,61.9303999844587));
#145131=CARTESIAN_POINT('Origin',(98.8105231949682,-12.3613099371181,62.2951126343007));
#145132=CARTESIAN_POINT('Ctrl Pts',(96.4484067501759,-12.4473573835336,
57.3800824823133));
#145133=CARTESIAN_POINT('Ctrl Pts',(96.4428162056186,-12.5283681372492,
57.4332801275737));
#145134=CARTESIAN_POINT('Ctrl Pts',(96.4368593228261,-12.6103539483408,
57.4900322201445));
#145135=CARTESIAN_POINT('Ctrl Pts',(96.4305324801312,-12.692936721428,57.5506122478589));
#145136=CARTESIAN_POINT('Ctrl Pts',(96.4244080470619,-12.7728774898076,
57.6092541871269));
#145137=CARTESIAN_POINT('Ctrl Pts',(96.4179369598139,-12.853377918145,57.6714834137224));
#145138=CARTESIAN_POINT('Ctrl Pts',(96.4110862810531,-12.9340584971688,
57.7375404927103));
#145139=CARTESIAN_POINT('Ctrl Pts',(96.404572653096,-13.0107696222229,57.8003475883988));
#145140=CARTESIAN_POINT('Ctrl Pts',(96.3977157598507,-13.0876437966098,
57.8666154103833));
#145141=CARTESIAN_POINT('Ctrl Pts',(96.390460874326,-13.1643180271825,57.9365394324825));
#145142=CARTESIAN_POINT('Ctrl Pts',(96.3865098506456,-13.2060749507934,
57.9746201804411));
#145143=CARTESIAN_POINT('Ctrl Pts',(96.3824403273612,-13.2477719091297,
58.0137851031057));
#145144=CARTESIAN_POINT('Ctrl Pts',(96.3782400812873,-13.2893449453626,
58.0540638211877));
#145145=CARTESIAN_POINT('Ctrl Pts',(96.3708527587521,-13.3624629060766,
58.1249053567887));
#145146=CARTESIAN_POINT('Ctrl Pts',(96.3630604453054,-13.4352201280504,
58.1992131566058));
#145147=CARTESIAN_POINT('Ctrl Pts',(96.3548763444432,-13.5072188387596,
58.2771077118593));
#145148=CARTESIAN_POINT('Ctrl Pts',(96.3471245472971,-13.5754144059446,
58.3508876910257));
#145149=CARTESIAN_POINT('Ctrl Pts',(96.3390210681869,-13.6429296388791,
58.4278856448029));
#145150=CARTESIAN_POINT('Ctrl Pts',(96.3305652270021,-13.7093879100516,
58.5081822841182));
#145151=CARTESIAN_POINT('Ctrl Pts',(96.3243339046578,-13.7583626839465,
58.5673549000412));
#145152=CARTESIAN_POINT('Ctrl Pts',(96.3179109801911,-13.8067627338357,
58.6283184846363));
#145153=CARTESIAN_POINT('Ctrl Pts',(96.311292573197,-13.8544217822592,58.6910964484846));
#145154=CARTESIAN_POINT('Ctrl Pts',(96.3012126802154,-13.9270069387988,
58.7867078482902));
#145155=CARTESIAN_POINT('Ctrl Pts',(96.2906794509788,-13.9978731788578,
58.886529385776));
#145156=CARTESIAN_POINT('Ctrl Pts',(96.2796863362393,-14.0665428342779,
58.9906502113008));
#145157=CARTESIAN_POINT('Ctrl Pts',(96.2782723638938,-14.0753753622774,
59.0040425911105));
#145158=CARTESIAN_POINT('Ctrl Pts',(96.2768507738921,-14.0841715045556,
59.0175060445161));
#145159=CARTESIAN_POINT('Ctrl Pts',(96.2754215448577,-14.0929302031139,
59.0310407123128));
#145160=CARTESIAN_POINT('Ctrl Pts',(96.2648460395679,-14.1577397337775,
59.1311897768977));
#145161=CARTESIAN_POINT('Ctrl Pts',(96.2538646209972,-14.2204403323873,
59.2351481203322));
#145162=CARTESIAN_POINT('Ctrl Pts',(96.2424880512788,-14.2805792843769,
59.342886235106));
#145163=CARTESIAN_POINT('Ctrl Pts',(96.2313797913637,-14.3392998940383,
59.4480834088842));
#145164=CARTESIAN_POINT('Ctrl Pts',(96.2198944628484,-14.3955784719746,
59.5568842666274));
#145165=CARTESIAN_POINT('Ctrl Pts',(96.2080501970947,-14.448974966694,59.6692175922599));
#145166=CARTESIAN_POINT('Ctrl Pts',(96.1966034480307,-14.5005793707712,
59.7777807921056));
#145167=CARTESIAN_POINT('Ctrl Pts',(96.1848211929471,-14.5494920202302,
59.8896433046505));
#145168=CARTESIAN_POINT('Ctrl Pts',(96.1727317296069,-14.595295785503,60.0046990841294));
#145169=CARTESIAN_POINT('Ctrl Pts',(96.1614756943887,-14.6379419130047,
60.1118231035683));
#145170=CARTESIAN_POINT('Ctrl Pts',(96.1499532633247,-14.6778929586248,
60.2217150214299));
#145171=CARTESIAN_POINT('Ctrl Pts',(96.1382000098369,-14.7147945678952,
60.334254885635));
#145172=CARTESIAN_POINT('Ctrl Pts',(96.1381781684374,-14.7148631431872,
60.3344640216106));
#145173=CARTESIAN_POINT('Ctrl Pts',(96.1381563262449,-14.7149317079431,
60.3346731667205));
#145174=CARTESIAN_POINT('Ctrl Pts',(96.1381344832597,-14.7150002621608,
60.3348823209644));
#145175=CARTESIAN_POINT('Ctrl Pts',(96.1265419877911,-14.7513833137882,
60.4458845307021));
#145176=CARTESIAN_POINT('Ctrl Pts',(96.1147289493766,-14.784784785401,60.5594202667816));
#145177=CARTESIAN_POINT('Ctrl Pts',(96.1027197551907,-14.8149038052703,
60.6753933684173));
#145178=CARTESIAN_POINT('Ctrl Pts',(96.0911665365054,-14.8438792400707,
60.7869631027453));
#145179=CARTESIAN_POINT('Ctrl Pts',(96.0794317393021,-14.8698167501967,
60.9007887087091));
#145180=CARTESIAN_POINT('Ctrl Pts',(96.0675444498865,-14.8924386342188,
61.0167379648425));
#145181=CARTESIAN_POINT('Ctrl Pts',(96.0558646668671,-14.9146656270705,
61.1306631924994));
#145182=CARTESIAN_POINT('Ctrl Pts',(96.0440376212459,-14.9336917478691,
61.2466387514315));
#145183=CARTESIAN_POINT('Ctrl Pts',(96.0320988027607,-14.9492438342748,
61.3644912538338));
#145184=CARTESIAN_POINT('Ctrl Pts',(96.0204085402785,-14.9644721395256,
61.4798901678028));
#145185=CARTESIAN_POINT('Ctrl Pts',(96.0086110796642,-14.9763695368615,
61.5970887700541));
#145186=CARTESIAN_POINT('Ctrl Pts',(95.9967479481211,-14.9846702418281,
61.7158760293545));
#145187=CARTESIAN_POINT('Ctrl Pts',(95.9896612697387,-14.9896288335989,
61.78683596936));
#145188=CARTESIAN_POINT('Ctrl Pts',(95.9825513164671,-14.9933037637515,
61.8583618898565));
#145189=CARTESIAN_POINT('Ctrl Pts',(95.9754284498954,-14.9956367981312,
61.9304001540396));
#145190=CARTESIAN_POINT('Ctrl Pts',(96.1768270765691,-12.21821914294,57.31259750763));
#145191=CARTESIAN_POINT('Ctrl Pts',(96.1765540719691,-12.22049670601,57.31400198718));
#145192=CARTESIAN_POINT('Ctrl Pts',(96.125013223869,-12.64979361445,57.57915534127));
#145193=CARTESIAN_POINT('Ctrl Pts',(96.0004379081691,-13.43109859674,58.22003658354));
#145194=CARTESIAN_POINT('Ctrl Pts',(95.760653910069,-14.28932658605,59.45361215821));
#145195=CARTESIAN_POINT('Ctrl Pts',(95.508664051869,-14.73991191643,60.74998112612));
#145196=CARTESIAN_POINT('Ctrl Pts',(95.3400117127691,-14.82639922299,61.61761786439));
#145197=CARTESIAN_POINT('Ctrl Pts',(95.2660621166691,-14.82530888696,61.99805365762));
#145198=CARTESIAN_POINT('Ctrl Pts',(97.5558858534691,-12.58079776334,56.99230719877));
#145199=CARTESIAN_POINT('Ctrl Pts',(97.5555797012692,-12.58335181252,56.99388220715));
#145200=CARTESIAN_POINT('Ctrl Pts',(97.4977808113692,-13.06476520039,57.2912302344301));
#145201=CARTESIAN_POINT('Ctrl Pts',(97.3580539159691,-13.94156754952,58.01005920855));
#145202=CARTESIAN_POINT('Ctrl Pts',(97.0882075430691,-14.90739617189,59.39829152191));
#145203=CARTESIAN_POINT('Ctrl Pts',(96.8057546118691,-15.41176909157,60.8513786323701));
#145204=CARTESIAN_POINT('Ctrl Pts',(96.6172881371691,-15.50847663767,61.82094975328));
#145205=CARTESIAN_POINT('Ctrl Pts',(96.5345613751691,-15.50723744476,62.2465399249501));
#145206=CARTESIAN_POINT('Ctrl Pts',(98.5620168036692,-12.11465513185,57.94428625613));
#145207=CARTESIAN_POINT('Ctrl Pts',(98.5617532670691,-12.11685372168,57.9456420272201));
#145208=CARTESIAN_POINT('Ctrl Pts',(98.5119999151691,-12.53126450239,58.2015995564401));
#145209=CARTESIAN_POINT('Ctrl Pts',(98.3917523736692,-13.28529239276,58.82021644193));
#145210=CARTESIAN_POINT('Ctrl Pts',(98.1605551479692,-14.11278621153,60.00961712239));
#145211=CARTESIAN_POINT('Ctrl Pts',(97.9172665143691,-14.54800809194,61.2612223934401));
#145212=CARTESIAN_POINT('Ctrl Pts',(97.7542737240691,-14.63157617232,62.0997434229));
#145213=CARTESIAN_POINT('Ctrl Pts',(97.682831166269,-14.63052835456,62.46728168636));
#145214=CARTESIAN_POINT('Ctrl Pts',(98.0436849069692,-11.35329989804,59.07897747768));
#145215=CARTESIAN_POINT('Ctrl Pts',(98.043490974869,-11.3549179127,59.0799751663801));
#145216=CARTESIAN_POINT('Ctrl Pts',(98.0068784773692,-11.6598926921,59.26832919789));
#145217=CARTESIAN_POINT('Ctrl Pts',(97.9184467516692,-12.21339188063,59.72326871723));
#145218=CARTESIAN_POINT('Ctrl Pts',(97.7503755488691,-12.81494213701,60.58791578338));
#145219=CARTESIAN_POINT('Ctrl Pts',(97.5710543385692,-13.13721896131,61.51043883242));
#145220=CARTESIAN_POINT('Ctrl Pts',(97.449667961469,-13.19932622623,62.13491448977));
#145221=CARTESIAN_POINT('Ctrl Pts',(97.3966560026691,-13.19859098334,62.40763601439));
#145222=CARTESIAN_POINT('Origin',(95.9826151700641,-13.4964585873305,61.979706126618));
#145223=CARTESIAN_POINT('Ctrl Pts',(95.682105874569,-14.96190022504,61.8692911014));
#145224=CARTESIAN_POINT('Ctrl Pts',(95.664293696769,-14.96450789965,61.95534281803));
#145225=CARTESIAN_POINT('Ctrl Pts',(95.6496298637692,-14.9654665309,62.04260905828));
#145226=CARTESIAN_POINT('Ctrl Pts',(95.6382530725691,-14.96464552087,62.13064087233));
#145227=CARTESIAN_POINT('Ctrl Pts',(96.8346494067691,-15.21462566969,62.08646545812));
#145228=CARTESIAN_POINT('Ctrl Pts',(96.8206261241691,-15.21734286754,62.15227511246));
#145229=CARTESIAN_POINT('Ctrl Pts',(96.8091979606691,-15.21834430824,62.21938009097));
#145230=CARTESIAN_POINT('Ctrl Pts',(96.8005323646691,-15.21748720413,62.2873715029101));
#145231=CARTESIAN_POINT('Ctrl Pts',(97.6665770469691,-14.37138217867,62.2768002444601));
#145232=CARTESIAN_POINT('Ctrl Pts',(97.6586537487692,-14.3737339414,62.31431226909));
#145233=CARTESIAN_POINT('Ctrl Pts',(97.6521769500692,-14.37459254412,62.35249859934));
#145234=CARTESIAN_POINT('Ctrl Pts',(97.6472313728691,-14.37385587149,62.39113761776));
#145235=CARTESIAN_POINT('Ctrl Pts',(97.4238295483692,-13.19648568652,62.26777600234));
#145236=CARTESIAN_POINT('Ctrl Pts',(97.418788297569,-13.19832828617,62.29458380256));
#145237=CARTESIAN_POINT('Ctrl Pts',(97.4144906416691,-13.19898787182,62.32130596198));
#145238=CARTESIAN_POINT('Ctrl Pts',(97.4109020818691,-13.19841899715,62.34788560615));
#145239=CARTESIAN_POINT('Ctrl Pts',(90.8406504123691,-11.39533572462,57.72321044074));
#145240=CARTESIAN_POINT('Ctrl Pts',(90.8052024597691,-10.89290348004,57.50129529369));
#145241=CARTESIAN_POINT('Ctrl Pts',(90.7750420804691,-10.40751804626,57.29731207447));
#145242=CARTESIAN_POINT('Ctrl Pts',(90.7446611131691,-9.91698402361699,
57.10972154207));
#145243=CARTESIAN_POINT('Ctrl Pts',(92.9567503555691,-11.53858517108,57.4125624132));
#145244=CARTESIAN_POINT('Ctrl Pts',(92.8693838873691,-11.02060249956,57.19158992276));
#145245=CARTESIAN_POINT('Ctrl Pts',(92.7895817403691,-10.54376807816,56.9954777013));
#145246=CARTESIAN_POINT('Ctrl Pts',(92.7150350010691,-10.04738352125,56.81106258288));
#145247=CARTESIAN_POINT('Ctrl Pts',(95.0797166483691,-11.62590813736,57.14090192696));
#145248=CARTESIAN_POINT('Ctrl Pts',(94.9392588749691,-11.10213102618,56.91987534728));
#145249=CARTESIAN_POINT('Ctrl Pts',(94.8096789677691,-10.63281944271,56.72802165784));
#145250=CARTESIAN_POINT('Ctrl Pts',(94.6903690477691,-10.13427439673,56.54465061292));
#145251=CARTESIAN_POINT('Ctrl Pts',(97.2420359135691,-11.67063354251,56.83720086782));
#145252=CARTESIAN_POINT('Ctrl Pts',(97.0468268665691,-11.15380442011,56.6213857415));
#145253=CARTESIAN_POINT('Ctrl Pts',(96.8658778707691,-10.69185373956,56.43600362222));
#145254=CARTESIAN_POINT('Ctrl Pts',(96.6996976194691,-10.19607748941,56.25706068473));
#145255=CARTESIAN_POINT('Origin',(91.5481555916691,0.0433429899084342,83.15732261681));
#145256=CARTESIAN_POINT('',(86.2399318207952,-9.45371065428624,58.8116592805523));
#145257=CARTESIAN_POINT('Ctrl Pts',(87.0626987426128,-9.81003033307946,
57.7183966791295));
#145258=CARTESIAN_POINT('Ctrl Pts',(87.0192701258182,-9.8100014211504,57.7260378243172));
#145259=CARTESIAN_POINT('Ctrl Pts',(86.9763075420885,-9.8089355749407,57.7363696650627));
#145260=CARTESIAN_POINT('Ctrl Pts',(86.9341886174092,-9.80684024658477,
57.7493037322963));
#145261=CARTESIAN_POINT('Ctrl Pts',(86.8920820972307,-9.80474553532679,
57.7622339903005));
#145262=CARTESIAN_POINT('Ctrl Pts',(86.8508191937219,-9.80162196779496,
57.7777648091818));
#145263=CARTESIAN_POINT('Ctrl Pts',(86.8107626708517,-9.79749540496822,
57.7957613018672));
#145264=CARTESIAN_POINT('Ctrl Pts',(86.770702975838,-9.79336851535201,57.8137592197251));
#145265=CARTESIAN_POINT('Ctrl Pts',(86.7318502861524,-9.78823851310647,
57.8342230140293));
#145266=CARTESIAN_POINT('Ctrl Pts',(86.6945462489452,-9.78214922936584,
57.8569736609505));
#145267=CARTESIAN_POINT('Ctrl Pts',(86.6572512799027,-9.77606142585717,
57.879718777462));
#145268=CARTESIAN_POINT('Ctrl Pts',(86.6215046120629,-9.76901487191784,
57.9047493908735));
#145269=CARTESIAN_POINT('Ctrl Pts',(86.587620182679,-9.76107052191038,57.9318457730919));
#145270=CARTESIAN_POINT('Ctrl Pts',(86.5537279197534,-9.75312433529542,
57.9589484195632));
#145271=CARTESIAN_POINT('Ctrl Pts',(86.5216991222089,-9.74428002199653,
57.9881174996962));
#145272=CARTESIAN_POINT('Ctrl Pts',(86.4918147021235,-9.7346146247997,58.0190962830994));
#145273=CARTESIAN_POINT('Ctrl Pts',(86.4639209041257,-9.72559304645865,
58.0480115481104));
#145274=CARTESIAN_POINT('Ctrl Pts',(86.4378952152105,-9.71585634607102,
58.078502889963));
#145275=CARTESIAN_POINT('Ctrl Pts',(86.413935969951,-9.7054786939897,58.1103361914022));
#145276=CARTESIAN_POINT('Ctrl Pts',(86.3881332862203,-9.6943025792323,58.1446187658424));
#145277=CARTESIAN_POINT('Ctrl Pts',(86.3647255207292,-9.68238195554693,
58.1804608615058));
#145278=CARTESIAN_POINT('Ctrl Pts',(86.3439192905833,-9.66982318943558,
58.2175466712203));
#145279=CARTESIAN_POINT('Ctrl Pts',(86.3231146153295,-9.6572653618665,58.2546297094365));
#145280=CARTESIAN_POINT('Ctrl Pts',(86.3049113029344,-9.64406961852703,
58.29295588904));
#145281=CARTESIAN_POINT('Ctrl Pts',(86.2894700249156,-9.63035355780913,
58.3321875341742));
#145282=CARTESIAN_POINT('Ctrl Pts',(86.2740248074335,-9.61663399777479,
58.3714291883004));
#145283=CARTESIAN_POINT('Ctrl Pts',(86.2613431970179,-9.60239399767873,
58.411576361447));
#145284=CARTESIAN_POINT('Ctrl Pts',(86.251537209766,-9.58776045017598,58.4522751389188));
#145285=CARTESIAN_POINT('Ctrl Pts',(86.2417330684947,-9.57312965744369,
58.4929662548314));
#145286=CARTESIAN_POINT('Ctrl Pts',(86.2348035684838,-9.55810561832479,
58.5342083427317));
#145287=CARTESIAN_POINT('Ctrl Pts',(86.2308099331657,-9.54282213213603,
58.5756379736388));
#145288=CARTESIAN_POINT('Ctrl Pts',(86.2268156286862,-9.5275360850929,58.6170745463686));
#145289=CARTESIAN_POINT('Ctrl Pts',(86.225758215939,-9.51199066333907,58.6586982928197));
#145290=CARTESIAN_POINT('Ctrl Pts',(86.2276471137534,-9.49632437130441,
58.7001423158925));
#145291=CARTESIAN_POINT('Ctrl Pts',(86.2293520725841,-9.48218364715038,
58.7375505613668));
#145292=CARTESIAN_POINT('Ctrl Pts',(86.2334567965308,-9.46794459032098,
58.7748121163149));
#145293=CARTESIAN_POINT('Ctrl Pts',(86.2399318207952,-9.45371065428624,
58.8116592805523));
#145294=CARTESIAN_POINT('Origin',(90.5633478388691,0.0433429899084242,83.33097079443));
#145295=CARTESIAN_POINT('Origin',(84.8686633886791,111.0724296188,51.03481040504));
#145296=CARTESIAN_POINT('',(85.8121822997791,-3.09682809692899,56.38577205054));
#145297=CARTESIAN_POINT('Ctrl Pts',(86.2399316748491,-9.45371065431499,
58.81165930621));
#145298=CARTESIAN_POINT('Ctrl Pts',(86.2050308571491,-8.92719465950899,
58.61372693326));
#145299=CARTESIAN_POINT('Ctrl Pts',(86.1286442510291,-7.86795581398499,
58.18051696283));
#145300=CARTESIAN_POINT('Ctrl Pts',(85.9950408985391,-6.11431423260199,
57.42281469856));
#145301=CARTESIAN_POINT('Ctrl Pts',(85.8853720513791,-4.53306565801299,
56.80085176037));
#145302=CARTESIAN_POINT('Ctrl Pts',(85.8329578397391,-3.56074610599299,
56.5035959926));
#145303=CARTESIAN_POINT('Ctrl Pts',(85.8121822997791,-3.09682809692899,
56.38577205054));
#145304=CARTESIAN_POINT('',(85.7414326542391,-3.07748116878498E-13,55.9845308734));
#145305=CARTESIAN_POINT('Ctrl Pts',(85.8121822996917,-3.09682809692899,
56.3857720505554));
#145306=CARTESIAN_POINT('Ctrl Pts',(85.8042550696392,-2.91956454869101,
56.340814494886));
#145307=CARTESIAN_POINT('Ctrl Pts',(85.7970341308756,-2.74414917508697,
56.2998625139189));
#145308=CARTESIAN_POINT('Ctrl Pts',(85.7905101366221,-2.57080491642329,
56.2628631023544));
#145309=CARTESIAN_POINT('Ctrl Pts',(85.7839861423686,-2.39746065775961,
56.2258636907898));
#145310=CARTESIAN_POINT('Ctrl Pts',(85.7781590605377,-2.22618751960296,
56.1928166717312));
#145311=CARTESIAN_POINT('Ctrl Pts',(85.7730109343456,-2.0571911640259,56.1636201991709));
#145312=CARTESIAN_POINT('Ctrl Pts',(85.7725980204189,-2.04363653343167,
56.161278448079));
#145313=CARTESIAN_POINT('Ctrl Pts',(85.7721894698494,-2.03009654045611,
56.1589614427568));
#145314=CARTESIAN_POINT('Ctrl Pts',(85.7717852626336,-2.01657131006667,
56.1566690697222));
#145315=CARTESIAN_POINT('Ctrl Pts',(85.7674981318306,-1.87311906688457,
56.1323555427397));
#145316=CARTESIAN_POINT('Ctrl Pts',(85.7637062630122,-1.73132285554557,
56.1108507779212));
#145317=CARTESIAN_POINT('Ctrl Pts',(85.7603785874086,-1.59087479019068,
56.0919785903473));
#145318=CARTESIAN_POINT('Ctrl Pts',(85.7570556544217,-1.45062689198,56.0731332994906));
#145319=CARTESIAN_POINT('Ctrl Pts',(85.7541955755858,-1.31172299355045,
56.0569129905777));
#145320=CARTESIAN_POINT('Ctrl Pts',(85.7517759592566,-1.17384006401943,
56.0431906681962));
#145321=CARTESIAN_POINT('Ctrl Pts',(85.7506934950497,-1.11215535220779,
56.0370517102819));
#145322=CARTESIAN_POINT('Ctrl Pts',(85.7496993006597,-1.0506747851408,56.0314133550991));
#145323=CARTESIAN_POINT('Ctrl Pts',(85.7487919406473,-0.989368607252711,
56.0262674607562));
#145324=CARTESIAN_POINT('Ctrl Pts',(85.7484214945406,-0.964339253293176,
56.0241665564854));
#145325=CARTESIAN_POINT('Ctrl Pts',(85.7480653344121,-0.93933926649891,
56.0221466717985));
#145326=CARTESIAN_POINT('Ctrl Pts',(85.7477234313339,-0.914369143509711,
56.0202076428128));
#145327=CARTESIAN_POINT('Ctrl Pts',(85.7445918678451,-0.685662441327941,
56.0024476612164));
#145328=CARTESIAN_POINT('Ctrl Pts',(85.7426566455784,-0.459465001269848,
55.9914724733907));
#145329=CARTESIAN_POINT('Ctrl Pts',(85.7418573532768,-0.236281071834248,
55.9869394614726));
#145330=CARTESIAN_POINT('Ctrl Pts',(85.7415739067142,-0.157135160499135,
55.9853319561281));
#145331=CARTESIAN_POINT('Ctrl Pts',(85.7414332766001,-0.0783677830622838,
55.9845344027693));
#145332=CARTESIAN_POINT('Ctrl Pts',(85.7414326542756,-3.07551343926051E-13,
55.9845308733936));
#145333=CARTESIAN_POINT('',(85.8121820990868,3.09687523453428,56.3857703184204));
#145334=CARTESIAN_POINT('Ctrl Pts',(85.7414326542187,-3.07700181072834E-13,
55.9845308734036));
#145335=CARTESIAN_POINT('Ctrl Pts',(85.7414342469354,0.217224571779936,
55.9845399061576));
#145336=CARTESIAN_POINT('Ctrl Pts',(85.7425133790675,0.437429466837711,
55.9906599649905));
#145337=CARTESIAN_POINT('Ctrl Pts',(85.7447232224476,0.660115966676029,
56.0031926097539));
#145338=CARTESIAN_POINT('Ctrl Pts',(85.7456168491695,0.75016696696471,56.0082606188071));
#145339=CARTESIAN_POINT('Ctrl Pts',(85.7466953170994,0.840623293120425,
56.0143769162074));
#145340=CARTESIAN_POINT('Ctrl Pts',(85.7479618986746,0.931450000602351,
56.021560058383));
#145341=CARTESIAN_POINT('Ctrl Pts',(85.7482352910711,0.951055000164376,
56.0231105439517));
#145342=CARTESIAN_POINT('Ctrl Pts',(85.7485174474739,0.970677252051475,
56.0247107325998));
#145343=CARTESIAN_POINT('Ctrl Pts',(85.7488083786006,0.990316494777137,
56.0263606850092));
#145344=CARTESIAN_POINT('Ctrl Pts',(85.750804498331,1.12506412505384,56.037681242545));
#145345=CARTESIAN_POINT('Ctrl Pts',(85.7532186801139,1.26060419693265,56.0513727400778));
#145346=CARTESIAN_POINT('Ctrl Pts',(85.7560682381979,1.39727469347661,56.0675333839879));
#145347=CARTESIAN_POINT('Ctrl Pts',(85.7589245668126,1.53426991819143,56.0837324254781));
#145348=CARTESIAN_POINT('Ctrl Pts',(85.7622183598749,1.67240122844942,56.1024124570235));
#145349=CARTESIAN_POINT('Ctrl Pts',(85.765975812552,1.81199514782755,56.123722035509));
#145350=CARTESIAN_POINT('Ctrl Pts',(85.7678064767031,1.88000653902479,56.1341042504728));
#145351=CARTESIAN_POINT('Ctrl Pts',(85.7697473312333,1.94836487803584,56.1451113863991));
#145352=CARTESIAN_POINT('Ctrl Pts',(85.7718021388295,2.01710641374184,56.1567647793634));
#145353=CARTESIAN_POINT('Ctrl Pts',(85.7723664816671,2.03598593968704,56.1599653266389));
#145354=CARTESIAN_POINT('Ctrl Pts',(85.772939283409,2.05489449159769,56.1632138465122));
#145355=CARTESIAN_POINT('Ctrl Pts',(85.7735205983484,2.07383170835384,56.1665106470066));
#145356=CARTESIAN_POINT('Ctrl Pts',(85.7786559456038,2.24112344215451,56.1956346454168));
#145357=CARTESIAN_POINT('Ctrl Pts',(85.7844563508405,2.41065351637206,56.2285303729545));
#145358=CARTESIAN_POINT('Ctrl Pts',(85.7909391303511,2.58220810972347,56.2652960441803));
#145359=CARTESIAN_POINT('Ctrl Pts',(85.7973499416829,2.75185820028397,56.3016535635632));
#145360=CARTESIAN_POINT('Ctrl Pts',(85.8044280722384,2.92348806511701,56.3417956397942));
#145361=CARTESIAN_POINT('Ctrl Pts',(85.8121819977014,3.09687523453422,56.3857703362983));
#145362=CARTESIAN_POINT('',(86.2399778829169,9.45364604184037,58.8119255183517));
#145363=CARTESIAN_POINT('Ctrl Pts',(85.8121821021391,3.09687523453501,56.38577031788));
#145364=CARTESIAN_POINT('Ctrl Pts',(85.8156355274938,3.1740050849032,56.4053562795853));
#145365=CARTESIAN_POINT('Ctrl Pts',(85.822202833005,3.31500708348416,56.4426013199344));
#145366=CARTESIAN_POINT('Ctrl Pts',(85.829686486828,3.46655241282912,56.4850432298054));
#145367=CARTESIAN_POINT('Ctrl Pts',(85.8341872722727,3.55573178407053,56.5105684524717));
#145368=CARTESIAN_POINT('Ctrl Pts',(85.8354069598104,3.5797232594888,56.5174856442303));
#145369=CARTESIAN_POINT('Ctrl Pts',(85.8430146168074,3.7284293012332,56.5606308110469));
#145370=CARTESIAN_POINT('Ctrl Pts',(85.8495034720024,3.85058241988637,56.5974309375446));
#145371=CARTESIAN_POINT('Ctrl Pts',(85.8581126207165,4.00637430763456,56.6462558461291));
#145372=CARTESIAN_POINT('Ctrl Pts',(85.8603552199655,4.04638499592307,56.6589742584787));
#145373=CARTESIAN_POINT('Ctrl Pts',(85.8783041873205,4.3623958073411,56.7607679107204));
#145374=CARTESIAN_POINT('Ctrl Pts',(85.8963538313168,4.65690735461759,56.8631325285659));
#145375=CARTESIAN_POINT('Ctrl Pts',(85.9172071280309,4.97600702371672,56.9813974511006));
#145376=CARTESIAN_POINT('Ctrl Pts',(85.9179810042478,4.98782294542579,56.9857863212208));
#145377=CARTESIAN_POINT('Ctrl Pts',(85.9354066199147,5.25345961164944,57.0846118985475));
#145378=CARTESIAN_POINT('Ctrl Pts',(85.9545355436378,5.53172004014412,57.1930974158877));
#145379=CARTESIAN_POINT('Ctrl Pts',(85.9762431292321,5.83552461324838,57.3162072514163));
#145380=CARTESIAN_POINT('Ctrl Pts',(85.9766657534864,5.84143542331735,57.3186040726661));
#145381=CARTESIAN_POINT('Ctrl Pts',(85.9932700223378,6.07355818889181,57.4127715607314));
#145382=CARTESIAN_POINT('Ctrl Pts',(86.0125400581796,6.33673275251046,57.5220573646636));
#145383=CARTESIAN_POINT('Ctrl Pts',(86.0349080414051,6.63690299677357,57.6489125012727));
#145384=CARTESIAN_POINT('Ctrl Pts',(86.0352247765358,6.64115272418706,57.650708795461));
#145385=CARTESIAN_POINT('Ctrl Pts',(86.0394882418842,6.69835306693705,57.6748881089797));
#145386=CARTESIAN_POINT('Ctrl Pts',(86.0580652377802,6.94590676687942,57.7802434880673));
#145387=CARTESIAN_POINT('Ctrl Pts',(86.09124831534,7.38771230747788,57.9684340725516));
#145388=CARTESIAN_POINT('Ctrl Pts',(86.0916010803591,7.39240906229862,57.970434702391));
#145389=CARTESIAN_POINT('Ctrl Pts',(86.112649716,7.67265227052037,58.0898074470287));
#145390=CARTESIAN_POINT('Ctrl Pts',(86.1300138532744,7.90547540138447,58.1882843630672));
#145391=CARTESIAN_POINT('Ctrl Pts',(86.1443085918483,8.09917346504611,58.2693538540572));
#145392=CARTESIAN_POINT('Ctrl Pts',(86.1446022539483,8.10315349725212,58.2710192945862));
#145393=CARTESIAN_POINT('Ctrl Pts',(86.1828731263993,8.62218252871381,58.4880641977383));
#145394=CARTESIAN_POINT('Ctrl Pts',(86.2144528885248,9.06971500218893,58.6671619285489));
#145395=CARTESIAN_POINT('Ctrl Pts',(86.2399778829169,9.45364604184037,58.8119255183517));
#145396=CARTESIAN_POINT('Origin',(90.5633473677691,-0.0433423696915958,
83.33096812237));
#145397=CARTESIAN_POINT('',(87.2268073772291,-13.97255334344,64.408496138118));
#145398=CARTESIAN_POINT('Origin',(85.7495940118791,-15.20679038041,64.668971957449));
#145399=CARTESIAN_POINT('',(86.0102742699191,-13.59507145206,66.146140280904));
#145400=CARTESIAN_POINT('Origin',(87.4872779078691,111.0724296188,65.885711320467));
#145401=CARTESIAN_POINT('',(69.2683344771691,-3.46410161513799,69.098202607305));
#145402=CARTESIAN_POINT('',(69.2686179994291,13.59506703911,69.098152483414));
#145403=CARTESIAN_POINT('Origin',(69.5288067436691,15.14946593626,70.575414236823));
#145404=CARTESIAN_POINT('',(68.051595113123,15.14946593626,70.8358864974945));
#145405=CARTESIAN_POINT('Origin',(67.7911228476491,111.0724296188,69.358674873805));
#145406=CARTESIAN_POINT('Origin',(74.4243048522391,1.4210854715202E-14,
66.665926000619));
#145407=CARTESIAN_POINT('Origin',(74.0770084968991,1.4210854715202E-14,
64.696310494595));
#145408=CARTESIAN_POINT('',(64.805817992169,1.27380650104997,66.3310715238674));
#145409=CARTESIAN_POINT('',(64.805817992169,-1.27380650104994,66.3310715238674));
#145410=CARTESIAN_POINT('Origin',(74.0770084968991,1.4210854715202E-14,
64.696310494595));
#145411=CARTESIAN_POINT('',(64.8058179921691,-1.27380650101999,66.331071523868));
#145412=CARTESIAN_POINT('Origin',(66.2853705616391,-11.87963525096,66.577899792436));
#145413=CARTESIAN_POINT('',(66.0249519193982,-6.80058507386928,65.1006787085175));
#145414=CARTESIAN_POINT('',(66.0248982949952,-5.12347538298166,65.100688162132));
#145415=CARTESIAN_POINT('',(66.0248749202791,-6.80071698562199,65.100691123259));
#145416=CARTESIAN_POINT('',(64.8081589327399,-6.16441400339199,66.8383720624473));
#145417=CARTESIAN_POINT('Ctrl Pts',(64.8081589327399,-6.16441400339199,
66.8383720624473));
#145418=CARTESIAN_POINT('Ctrl Pts',(64.8018782379671,-6.16444558364484,
66.802752472863));
#145419=CARTESIAN_POINT('Ctrl Pts',(64.7966397238661,-6.16496886332639,
66.7654979979585));
#145420=CARTESIAN_POINT('Ctrl Pts',(64.7927790828751,-6.16617417900185,
66.726798004383));
#145421=CARTESIAN_POINT('Ctrl Pts',(64.7890472955959,-6.16733926576218,
66.6893896713979));
#145422=CARTESIAN_POINT('Ctrl Pts',(64.7866035704855,-6.16914162068152,
66.6506309119591));
#145423=CARTESIAN_POINT('Ctrl Pts',(64.7857300260124,-6.17175315117691,
66.6107367214207));
#145424=CARTESIAN_POINT('Ctrl Pts',(64.7848703921967,-6.17432309465844,
66.5714778212829));
#145425=CARTESIAN_POINT('Ctrl Pts',(64.7855319205551,-6.17767664766678,
66.531119607349));
#145426=CARTESIAN_POINT('Ctrl Pts',(64.7879536899489,-6.18197763514565,
66.4899071087765));
#145427=CARTESIAN_POINT('Ctrl Pts',(64.7903316449724,-6.18620080965898,
66.4494402219379));
#145428=CARTESIAN_POINT('Ctrl Pts',(64.7944071927674,-6.19133744700491,
66.408150068017));
#145429=CARTESIAN_POINT('Ctrl Pts',(64.8003699641285,-6.19754264031923,
66.3663029460676));
#145430=CARTESIAN_POINT('Ctrl Pts',(64.802891495943,-6.20016668732857,66.3486066697974));
#145431=CARTESIAN_POINT('Ctrl Pts',(64.805750019028,-6.20298182077583,66.3308111840328));
#145432=CARTESIAN_POINT('Ctrl Pts',(64.8089575523694,-6.20599976913376,
66.3129382366224));
#145433=CARTESIAN_POINT('Ctrl Pts',(64.8175795013529,-6.21411210780888,
66.264895200321));
#145434=CARTESIAN_POINT('Ctrl Pts',(64.8287186518659,-6.22341884736779,
66.2163193093983));
#145435=CARTESIAN_POINT('Ctrl Pts',(64.8426026562989,-6.23382808779138,
66.1675087943377));
#145436=CARTESIAN_POINT('Ctrl Pts',(64.844338156853,-6.23512924284433,66.1614074799551));
#145437=CARTESIAN_POINT('Ctrl Pts',(64.8461166196411,-6.23644769982519,
66.155302198922));
#145438=CARTESIAN_POINT('Ctrl Pts',(64.8479385087963,-6.23778316422518,
66.1491934903362));
#145439=CARTESIAN_POINT('Ctrl Pts',(64.8492890733101,-6.23877314257979,
66.1446651110888));
#145440=CARTESIAN_POINT('Ctrl Pts',(64.8508084707658,-6.23987842321675,
66.139666922722));
#145441=CARTESIAN_POINT('Ctrl Pts',(64.8520035489644,-6.24073954596106,
66.1357923315445));
#145442=CARTESIAN_POINT('Ctrl Pts',(64.8524206114576,-6.24104006353311,
66.1344401634116));
#145443=CARTESIAN_POINT('Ctrl Pts',(64.8527976450016,-6.24131084525289,
66.1332246742856));
#145444=CARTESIAN_POINT('Ctrl Pts',(64.8531123985251,-6.24153661316581,
66.132213182593));
#145445=CARTESIAN_POINT('Ctrl Pts',(64.8555457363169,-6.24328200933677,
66.1243934100468));
#145446=CARTESIAN_POINT('Ctrl Pts',(64.8581071814899,-6.24508366804847,
66.1163875900722));
#145447=CARTESIAN_POINT('Ctrl Pts',(64.860805733643,-6.24694729562907,66.1082030276649));
#145448=CARTESIAN_POINT('Ctrl Pts',(64.866202837949,-6.25067455079026,66.0918339028505));
#145449=CARTESIAN_POINT('Ctrl Pts',(64.8721481952012,-6.25464968142705,
66.0747497098203));
#145450=CARTESIAN_POINT('Ctrl Pts',(64.8787136065186,-6.25890835103562,
66.0570195656937));
#145451=CARTESIAN_POINT('Ctrl Pts',(64.8890331042377,-6.26560211768438,
66.0291513677959));
#145452=CARTESIAN_POINT('Ctrl Pts',(64.9008837340019,-6.27302883205694,
65.9996869371169));
#145453=CARTESIAN_POINT('Ctrl Pts',(64.9145547240413,-6.28129575024242,
65.9689137996651));
#145454=CARTESIAN_POINT('Ctrl Pts',(64.9277534687516,-6.28927709924174,
65.939203677429));
#145455=CARTESIAN_POINT('Ctrl Pts',(64.9426498964942,-6.29804160729299,
65.9082737349583));
#145456=CARTESIAN_POINT('Ctrl Pts',(64.9594971235488,-6.30768579498066,
65.8764301735881));
#145457=CARTESIAN_POINT('Ctrl Pts',(64.9696076707388,-6.31347357325478,
65.8573198577546));
#145458=CARTESIAN_POINT('Ctrl Pts',(64.9804206152209,-6.31957817474758,
65.8378814163225));
#145459=CARTESIAN_POINT('Ctrl Pts',(64.9919872957414,-6.32602046158861,
65.8181895006169));
#145460=CARTESIAN_POINT('Ctrl Pts',(65.010333486147,-6.33623872782528,65.7869556790943));
#145461=CARTESIAN_POINT('Ctrl Pts',(65.0305763187481,-6.34730016361858,
65.7550828730331));
#145462=CARTESIAN_POINT('Ctrl Pts',(65.0529182172327,-6.35923156460288,
65.7228786121327));
#145463=CARTESIAN_POINT('Ctrl Pts',(65.0615104126933,-6.36382011509899,
65.7104935722262));
#145464=CARTESIAN_POINT('Ctrl Pts',(65.0704128213947,-6.36853733343909,
65.6980599905497));
#145465=CARTESIAN_POINT('Ctrl Pts',(65.0796359212282,-6.373384743733,65.6855971661296));
#145466=CARTESIAN_POINT('Ctrl Pts',(65.0879372988571,-6.377747721918,65.6743798299085));
#145467=CARTESIAN_POINT('Ctrl Pts',(65.096924391596,-6.38244554878342,65.6625720000334));
#145468=CARTESIAN_POINT('Ctrl Pts',(65.106284192454,-6.38730345565473,65.6506698673355));
#145469=CARTESIAN_POINT('Ctrl Pts',(65.1149591713286,-6.39180592746183,
65.6396385696313));
#145470=CARTESIAN_POINT('Ctrl Pts',(65.1239539050347,-6.39644591130927,
65.6285262888787));
#145471=CARTESIAN_POINT('Ctrl Pts',(65.1329773043374,-6.40108426173598,
65.6176968032063));
#145472=CARTESIAN_POINT('Ctrl Pts',(65.1336896313987,-6.40145042335839,
65.6168418996999));
#145473=CARTESIAN_POINT('Ctrl Pts',(65.1344021162251,-6.40181657480153,
65.6159887414984));
#145474=CARTESIAN_POINT('Ctrl Pts',(65.1351146049841,-6.40218264761172,
65.6151374987312));
#145475=CARTESIAN_POINT('Ctrl Pts',(65.1545904777191,-6.41218924402872,
65.59186878664));
#145476=CARTESIAN_POINT('Ctrl Pts',(65.174534446433,-6.42233208182421,65.5694744033257));
#145477=CARTESIAN_POINT('Ctrl Pts',(65.1948880277455,-6.43256527208665,
65.5479251115468));
#145478=CARTESIAN_POINT('Ctrl Pts',(65.2282806527171,-6.44935411526127,
65.5125707722916));
#145479=CARTESIAN_POINT('Ctrl Pts',(65.2627791595159,-6.46636865768246,
65.4794863823339));
#145480=CARTESIAN_POINT('Ctrl Pts',(65.2981340375824,-6.48349628267055,
65.4485796227903));
#145481=CARTESIAN_POINT('Ctrl Pts',(65.3349584684363,-6.50133583060725,
65.4163881999382));
#145482=CARTESIAN_POINT('Ctrl Pts',(65.3727120202401,-6.51929805721341,
65.3865585271715));
#145483=CARTESIAN_POINT('Ctrl Pts',(65.4111687378838,-6.53725571101636,
65.3589776573745));
#145484=CARTESIAN_POINT('Ctrl Pts',(65.4258093262544,-6.54409224396922,
65.3484775370746));
#145485=CARTESIAN_POINT('Ctrl Pts',(65.4405523805545,-6.55092811416381,
65.3383033134471));
#145486=CARTESIAN_POINT('Ctrl Pts',(65.4553873823056,-6.55775630023164,
65.3284487441658));
#145487=CARTESIAN_POINT('Ctrl Pts',(65.5009941420158,-6.57874796888649,
65.2981531647785));
#145488=CARTESIAN_POINT('Ctrl Pts',(65.5474757338804,-6.59965827117149,
65.2708737574508));
#145489=CARTESIAN_POINT('Ctrl Pts',(65.5944928291456,-6.62040649357933,
65.2464765093496));
#145490=CARTESIAN_POINT('Ctrl Pts',(65.641450338879,-6.64112842142649,65.2221101802788));
#145491=CARTESIAN_POINT('Ctrl Pts',(65.6889424427869,-6.66168867994912,
65.2006179488416));
#145492=CARTESIAN_POINT('Ctrl Pts',(65.7366880486402,-6.68200686211981,
65.181852694402));
#145493=CARTESIAN_POINT('Ctrl Pts',(65.786825709474,-6.70334298527137,65.162147300665));
#145494=CARTESIAN_POINT('Ctrl Pts',(65.837243007763,-6.72441216840512,65.1454483117514));
#145495=CARTESIAN_POINT('Ctrl Pts',(65.8876737008058,-6.74512130373806,
65.1315812912464));
#145496=CARTESIAN_POINT('Ctrl Pts',(65.9334751418892,-6.76392945775325,
65.1189871846748));
#145497=CARTESIAN_POINT('Ctrl Pts',(65.9792887073989,-6.78244063083012,
65.1087286556775));
#145498=CARTESIAN_POINT('Ctrl Pts',(66.0249519193982,-6.80058507386928,
65.1006787085175));
#145499=CARTESIAN_POINT('',(64.8081615004591,6.16441400309888,66.8383716061749));
#145500=CARTESIAN_POINT('',(64.8081632946491,-6.16441400339199,66.838371293325));
#145501=CARTESIAN_POINT('',(66.0248982951649,6.80073525439801,65.1006881629131));
#145502=CARTESIAN_POINT('Ctrl Pts',(64.8081589321389,6.16441400309901,66.8383720590391));
#145503=CARTESIAN_POINT('Ctrl Pts',(64.7987827821794,6.16441838682887,66.7851972702575));
#145504=CARTESIAN_POINT('Ctrl Pts',(64.7921811970201,6.16585112404424,66.7309524641975));
#145505=CARTESIAN_POINT('Ctrl Pts',(64.7885778066817,6.16871221474511,66.6759377886771));
#145506=CARTESIAN_POINT('Ctrl Pts',(64.785040627147,6.17152073409038,66.6219339850137));
#145507=CARTESIAN_POINT('Ctrl Pts',(64.7843928677463,6.17570559836315,66.567188560321));
#145508=CARTESIAN_POINT('Ctrl Pts',(64.786817703994,6.18126680756346,66.5120261797856));
#145509=CARTESIAN_POINT('Ctrl Pts',(64.7891026366133,6.18650715660429,66.4600464542408));
#145510=CARTESIAN_POINT('Ctrl Pts',(64.7941159419607,6.19296961269943,66.407696948985));
#145511=CARTESIAN_POINT('Ctrl Pts',(64.8019823066183,6.20065417584886,66.3552806448622));
#145512=CARTESIAN_POINT('Ctrl Pts',(64.8101411712435,6.20862447892643,66.3009153124495));
#145513=CARTESIAN_POINT('Ctrl Pts',(64.8213698492503,6.21790946351572,66.246478174084));
#145514=CARTESIAN_POINT('Ctrl Pts',(64.8357695591531,6.22850912961671,66.1923392477849));
#145515=CARTESIAN_POINT('Ctrl Pts',(64.8499503796991,6.23894767065946,66.1390232849235));
#145516=CARTESIAN_POINT('Ctrl Pts',(64.8672068571494,6.25066122816447,66.085996883417));
#145517=CARTESIAN_POINT('Ctrl Pts',(64.8875930217995,6.26364980213172,66.0336407097191));
#145518=CARTESIAN_POINT('Ctrl Pts',(64.8935435202088,6.26744102476029,66.0183585154636));
#145519=CARTESIAN_POINT('Ctrl Pts',(64.8997603692193,6.2713408778002,66.0031335845166));
#145520=CARTESIAN_POINT('Ctrl Pts',(64.9062441577029,6.27534936125144,65.9879757617626));
#145521=CARTESIAN_POINT('Ctrl Pts',(64.9147863329762,6.28063040462715,65.9680058353756));
#145522=CARTESIAN_POINT('Ctrl Pts',(64.9237918809422,6.28609999981175,65.9481523759262));
#145523=CARTESIAN_POINT('Ctrl Pts',(64.9332611821828,6.29175814680523,65.9284383032111));
#145524=CARTESIAN_POINT('Ctrl Pts',(64.9379958328031,6.29458722030197,65.9185812668535));
#145525=CARTESIAN_POINT('Ctrl Pts',(64.942846410463,6.29746343175093,65.90875907166));
#145526=CARTESIAN_POINT('Ctrl Pts',(64.9478128497735,6.30038678115212,65.8989746364514));
#145527=CARTESIAN_POINT('Ctrl Pts',(64.9502960694287,6.30184845585272,65.894082418847));
#145528=CARTESIAN_POINT('Ctrl Pts',(64.9528082537229,6.30332191504137,65.8891996408788));
#145529=CARTESIAN_POINT('Ctrl Pts',(64.9553493886184,6.30480715871807,65.8843266677285));
#145530=CARTESIAN_POINT('Ctrl Pts',(64.9571933289268,6.30588490578621,65.8807906603997));
#145531=CARTESIAN_POINT('Ctrl Pts',(64.9594293287966,6.30718965479531,65.876547760901));
#145532=CARTESIAN_POINT('Ctrl Pts',(64.9612383475702,6.30824075099125,65.8731488579457));
#145533=CARTESIAN_POINT('Ctrl Pts',(64.9619223383106,6.30863817089411,65.8718637313441));
#145534=CARTESIAN_POINT('Ctrl Pts',(64.9625447294431,6.30899932861105,65.8706989672381));
#145535=CARTESIAN_POINT('Ctrl Pts',(64.9630596273281,6.30929824321235,65.8697375278373));
#145536=CARTESIAN_POINT('Ctrl Pts',(64.9746693744909,6.31603807075048,65.848059310308));
#145537=CARTESIAN_POINT('Ctrl Pts',(64.9876834635193,6.32365695723595,65.8250329634241));
#145538=CARTESIAN_POINT('Ctrl Pts',(65.0023383654708,6.33215490266875,65.80083584166));
#145539=CARTESIAN_POINT('Ctrl Pts',(65.0166474478898,6.34045231755374,65.7772097122753));
#145540=CARTESIAN_POINT('Ctrl Pts',(65.0325214116991,6.34958779363933,65.7524671037607));
#145541=CARTESIAN_POINT('Ctrl Pts',(65.0501936356578,6.35956133092553,65.7268193253099));
#145542=CARTESIAN_POINT('Ctrl Pts',(65.0674105003129,6.36927788057936,65.7018324118733));
#145543=CARTESIAN_POINT('Ctrl Pts',(65.0863347707334,6.37978985929114,65.6759861648845));
#145544=CARTESIAN_POINT('Ctrl Pts',(65.1071861193518,6.39109726706087,65.6495241034221));
#145545=CARTESIAN_POINT('Ctrl Pts',(65.1274779738104,6.40210126862294,65.6237720856654));
#145546=CARTESIAN_POINT('Ctrl Pts',(65.1495955070102,6.41385858521217,65.5974367512891));
#145547=CARTESIAN_POINT('Ctrl Pts',(65.1737357905544,6.42636921682857,65.5707909920993));
#145548=CARTESIAN_POINT('Ctrl Pts',(65.1972228978337,6.4385413417486,65.5448662011383));
#145549=CARTESIAN_POINT('Ctrl Pts',(65.2226253937009,6.45142656752832,65.5186475517802));
#145550=CARTESIAN_POINT('Ctrl Pts',(65.2501105477758,6.46502489416772,65.4924336696594));
#145551=CARTESIAN_POINT('Ctrl Pts',(65.2765224236187,6.4780922145798,65.4672434233886));
#145552=CARTESIAN_POINT('Ctrl Pts',(65.3048580009356,6.4918180309331,65.4420577603538));
#145553=CARTESIAN_POINT('Ctrl Pts',(65.3352442528554,6.50620234322766,65.4171844968716));
#145554=CARTESIAN_POINT('Ctrl Pts',(65.364957714832,6.5202681687053,65.3928619588152));
#145555=CARTESIAN_POINT('Ctrl Pts',(65.3966325957644,6.53496365308086,65.3688382857725));
#145556=CARTESIAN_POINT('Ctrl Pts',(65.4303588502056,6.55028879635433,65.3454408789985));
#145557=CARTESIAN_POINT('Ctrl Pts',(65.4630069700259,6.56512403738972,65.3227914222919));
#145558=CARTESIAN_POINT('Ctrl Pts',(65.4975778418086,6.58054932388348,65.3007291172199));
#145559=CARTESIAN_POINT('Ctrl Pts',(65.5341187593121,6.59656465583564,65.2795852198071));
#145560=CARTESIAN_POINT('Ctrl Pts',(65.5552586448087,6.60582994819253,65.2673529169315));
#145561=CARTESIAN_POINT('Ctrl Pts',(65.5770572174507,6.61529272451413,65.255428621325));
#145562=CARTESIAN_POINT('Ctrl Pts',(65.5995172355066,6.62495298480042,65.2438813461494));
#145563=CARTESIAN_POINT('Ctrl Pts',(65.6367046710099,6.64094764274979,65.2247623254182));
#145564=CARTESIAN_POINT('Ctrl Pts',(65.6757078881928,6.65748368305192,65.2066757042188));
#145565=CARTESIAN_POINT('Ctrl Pts',(65.7165057812049,6.6745611057068,65.1899542381791));
#145566=CARTESIAN_POINT('Ctrl Pts',(65.7565231187389,6.69131179884646,65.1735526914037));
#145567=CARTESIAN_POINT('Ctrl Pts',(65.7982674702529,6.70858335678332,65.1584649442466));
#145568=CARTESIAN_POINT('Ctrl Pts',(65.8416731700358,6.72637577951738,65.1450241437196));
#145569=CARTESIAN_POINT('Ctrl Pts',(65.8839311284249,6.7436977317794,65.1319387472803));
#145570=CARTESIAN_POINT('Ctrl Pts',(65.927763957186,6.76151336741847,65.120414793424));
#145571=CARTESIAN_POINT('Ctrl Pts',(65.9730632002797,6.77982268643461,65.1107719479587));
#145572=CARTESIAN_POINT('Ctrl Pts',(65.9901363495624,6.78672341402914,65.1071375883337));
#145573=CARTESIAN_POINT('Ctrl Pts',(66.007417292501,6.79369427001695,65.1037705353322));
#145574=CARTESIAN_POINT('Ctrl Pts',(66.0248982951649,6.80073525439801,65.1006881629131));
#145575=CARTESIAN_POINT('',(66.0248982950042,5.12347538298277,65.1006881621786));
#145576=CARTESIAN_POINT('',(66.0248982951391,5.12347538298101,65.100688162917));
#145577=CARTESIAN_POINT('Ctrl Pts',(66.0248982951388,5.12347538298986,65.1006881629177));
#145578=CARTESIAN_POINT('Ctrl Pts',(65.5457633364347,4.36379356331096,65.1851725835393));
#145579=CARTESIAN_POINT('Ctrl Pts',(65.2016180936169,3.51046595110393,65.471515880299));
#145580=CARTESIAN_POINT('Ctrl Pts',(64.9003152941216,2.17972224640472,65.9694338758958));
#145581=CARTESIAN_POINT('Ctrl Pts',(64.8358888771522,1.72400278119682,66.1508188509989));
#145582=CARTESIAN_POINT('Ctrl Pts',(64.8058179921649,1.27380650105203,66.3310715238719));
#145583=CARTESIAN_POINT('Ctrl Pts',(64.8058179921649,-1.27380650105201,
66.3310715238719));
#145584=CARTESIAN_POINT('Ctrl Pts',(64.8358888771522,-1.72400278119679,
66.1508188509989));
#145585=CARTESIAN_POINT('Ctrl Pts',(64.9003152941216,-2.17972224640469,
65.9694338758958));
#145586=CARTESIAN_POINT('Ctrl Pts',(65.2016180936169,-3.5104659511039,65.471515880299));
#145587=CARTESIAN_POINT('Ctrl Pts',(65.5457633364338,-4.36379356331136,
65.185172583538));
#145588=CARTESIAN_POINT('Ctrl Pts',(66.0248982951388,-5.12347538298983,
65.1006881629177));
#145589=CARTESIAN_POINT('Origin',(71.6139524734691,1.4210854715202E-14,
50.72762564822));
#145590=CARTESIAN_POINT('',(83.2590339728491,-3.72445119722915E-6,62.06184505375));
#145591=CARTESIAN_POINT('Origin',(73.9033603192391,1.4210854715202E-14,
63.711502741582));
#145592=CARTESIAN_POINT('Origin',(73.9033603192391,1.4210854715202E-14,
63.711502741582));
#145593=CARTESIAN_POINT('Origin',(73.9033603192391,1.4210854715202E-14,
63.711502741582));
#145594=CARTESIAN_POINT('',(83.2590347531395,-6.98291828557661,62.0618512036248));
#145595=CARTESIAN_POINT('',(83.2590347341691,-6.98291575896899,62.06184938817));
#145596=CARTESIAN_POINT('',(81.0965926396278,-7.61327390186262,62.4431418050118));
#145597=CARTESIAN_POINT('Origin',(82.7666300963491,-9.38083151964699,62.14866914261));
#145598=CARTESIAN_POINT('',(67.5092874005591,-8.31611745004299,64.838950313787));
#145599=CARTESIAN_POINT('Origin',(73.9033603192391,1.4210854715202E-14,
63.711502741607));
#145600=CARTESIAN_POINT('',(66.2209546742975,-7.02799158729797,65.0661181389945));
#145601=CARTESIAN_POINT('Ctrl Pts',(66.2209546733633,-7.02799158729799,
65.0661181336967));
#145602=CARTESIAN_POINT('Ctrl Pts',(66.3246656027716,-7.14505369148099,
65.0478310986477));
#145603=CARTESIAN_POINT('Ctrl Pts',(66.4234442496545,-7.25629879530099,
65.0304137580844));
#145604=CARTESIAN_POINT('Ctrl Pts',(66.5178883954126,-7.36052989680883,
65.0137607070173));
#145605=CARTESIAN_POINT('Ctrl Pts',(66.6123325411707,-7.46476099831666,
64.9971076559501));
#145606=CARTESIAN_POINT('Ctrl Pts',(66.702442185804,-7.56197809751232,64.9812188943793));
#145607=CARTESIAN_POINT('Ctrl Pts',(66.7896495528575,-7.65283723712582,
64.9658418826512));
#145608=CARTESIAN_POINT('Ctrl Pts',(66.876856919911,-7.74369637673932,64.9504648709231));
#145609=CARTESIAN_POINT('Ctrl Pts',(66.9611620093849,-7.82819755677066,
64.9355996090378));
#145610=CARTESIAN_POINT('Ctrl Pts',(67.0429998000091,-7.90686402925032,
64.9211693985092));
#145611=CARTESIAN_POINT('Ctrl Pts',(67.1248375906334,-7.98553050172999,
64.9067391879805));
#145612=CARTESIAN_POINT('Ctrl Pts',(67.2042080824082,-8.05836226665799,
64.8927440288086));
#145613=CARTESIAN_POINT('Ctrl Pts',(67.2818820035575,-8.12639721364099,
64.8790480208125));
#145614=CARTESIAN_POINT('Ctrl Pts',(67.3595559247068,-8.19443216062399,
64.8653520128165));
#145615=CARTESIAN_POINT('Ctrl Pts',(67.4355332752307,-8.25767028966199,
64.8519551559964));
#145616=CARTESIAN_POINT('Ctrl Pts',(67.5092874005549,-8.31611745004299,
64.8389503137632));
#145617=CARTESIAN_POINT('Origin',(73.9033603209991,1.4210854715202E-14,
63.711502751597));
#145618=CARTESIAN_POINT('Origin',(73.9033603192391,1.4210854715202E-14,
63.711502741582));
#145619=CARTESIAN_POINT('',(66.2208875197039,7.02805194586377,65.0661299774239));
#145620=CARTESIAN_POINT('Origin',(73.9033603203091,1.4210854715202E-14,
63.711502747645));
#145621=CARTESIAN_POINT('',(67.5092801231572,8.31611453423868,64.8389516048533));
#145622=CARTESIAN_POINT('Ctrl Pts',(66.2208657833691,7.02807183034301,65.066133808363));
#145623=CARTESIAN_POINT('Ctrl Pts',(66.4309100471391,7.26505475676601,65.029097337517));
#145624=CARTESIAN_POINT('Ctrl Pts',(66.8419704590391,7.72821672095301,64.956616290815));
#145625=CARTESIAN_POINT('Ctrl Pts',(67.2799358526991,8.13398401787701,64.879391187598));
#145626=CARTESIAN_POINT('Ctrl Pts',(67.5092801218091,8.31611453424001,64.838951597214));
#145627=CARTESIAN_POINT('',(81.0965921351133,7.61327336788956,62.4431418939603));
#145628=CARTESIAN_POINT('Origin',(73.9033603192391,1.4210854715202E-14,
63.711502741594));
#145629=CARTESIAN_POINT('',(83.2590339201892,6.98291692033359,62.0618459037933));
#145630=CARTESIAN_POINT('Origin',(82.7666300963491,9.38083151964701,62.14866914259));
#145631=CARTESIAN_POINT('',(83.2590339728491,-8.07105361845785E-10,62.06184505375));
#145632=CARTESIAN_POINT('Origin',(74.0770084968991,1.4210854715202E-14,
64.696310494594));
#145633=CARTESIAN_POINT('',(65.6628224406878,-7.69741850331449,66.1799585170539));
#145634=CARTESIAN_POINT('Origin',(66.3946016642385,-7.02812664320015,66.0509721790387));
#145635=CARTESIAN_POINT('',(65.4482167555244,-7.44842431834834,66.2177992895134));
#145636=CARTESIAN_POINT('Origin',(74.0770084968991,1.4210854715202E-14,
64.696310494594));
#145637=CARTESIAN_POINT('Origin',(66.1985464660391,-6.80073524628799,66.085495917122));
#145638=CARTESIAN_POINT('Ctrl Pts',(65.1021721393592,-6.87149439123999,
66.825730951951));
#145639=CARTESIAN_POINT('Ctrl Pts',(65.0984324276291,-6.86890400994998,
66.81588333904));
#145640=CARTESIAN_POINT('Ctrl Pts',(65.0923058811291,-6.86568651314798,
66.795286809766));
#145641=CARTESIAN_POINT('Ctrl Pts',(65.0880224526391,-6.86745667141899,
66.7631974852071));
#145642=CARTESIAN_POINT('Ctrl Pts',(65.0892419555591,-6.87754968651898,
66.72582778172));
#145643=CARTESIAN_POINT('Ctrl Pts',(65.0975331340091,-6.89813731240698,
66.682874279271));
#145644=CARTESIAN_POINT('Ctrl Pts',(65.1141392786591,-6.93040430719099,
66.635952050429));
#145645=CARTESIAN_POINT('Ctrl Pts',(65.1393962274192,-6.97394855130398,
66.5877397397371));
#145646=CARTESIAN_POINT('Ctrl Pts',(65.1730883139991,-7.02767577688599,
66.540401613751));
#145647=CARTESIAN_POINT('Ctrl Pts',(65.2156473534191,-7.09157262362899,
66.494759786697));
#145648=CARTESIAN_POINT('Ctrl Pts',(65.2686593298991,-7.16704019306199,
66.451322347829));
#145649=CARTESIAN_POINT('Ctrl Pts',(65.3339085497291,-7.255260014411,66.411786713305));
#145650=CARTESIAN_POINT('Ctrl Pts',(65.4124751097891,-7.35606512702098,
66.3792619117831));
#145651=CARTESIAN_POINT('Ctrl Pts',(65.4996859213891,-7.46199868601399,
66.359128467309));
#145652=CARTESIAN_POINT('Ctrl Pts',(65.5607994574491,-7.53227090791299,
66.355726537549));
#145653=CARTESIAN_POINT('Ctrl Pts',(65.5903804255091,-7.56541214625599,
66.356593540049));
#145654=CARTESIAN_POINT('Ctrl Pts',(64.5846873418391,-6.30826130801998,
67.129516993943));
#145655=CARTESIAN_POINT('Ctrl Pts',(64.5644558003891,-6.29438263574299,
67.070569230962));
#145656=CARTESIAN_POINT('Ctrl Pts',(64.5270818293391,-6.27495791837099,
66.936568367789));
#145657=CARTESIAN_POINT('Ctrl Pts',(64.4965238099191,-6.286222366815,66.718086212213));
#145658=CARTESIAN_POINT('Ctrl Pts',(64.4976343803391,-6.34198098713299,
66.5003543309391));
#145659=CARTESIAN_POINT('Ctrl Pts',(64.5265729662991,-6.42999665028198,
66.309045559806));
#145660=CARTESIAN_POINT('Ctrl Pts',(64.5750030295691,-6.53664105447099,
66.1491720266271));
#145661=CARTESIAN_POINT('Ctrl Pts',(64.6365600582891,-6.65313100744599,
66.01733044383));
#145662=CARTESIAN_POINT('Ctrl Pts',(64.7080223585791,-6.77577809653398,
65.907554455012));
#145663=CARTESIAN_POINT('Ctrl Pts',(64.7897203452091,-6.90580213921598,
65.813630090375));
#145664=CARTESIAN_POINT('Ctrl Pts',(64.8846591549891,-7.04714751738299,
65.731602763897));
#145665=CARTESIAN_POINT('Ctrl Pts',(64.9965114148391,-7.20324351350999,
65.661153574081));
#145666=CARTESIAN_POINT('Ctrl Pts',(65.1287226451391,-7.376030976721,65.604985997049));
#145667=CARTESIAN_POINT('Ctrl Pts',(65.2766685793991,-7.55657323556499,
65.57041707536));
#145668=CARTESIAN_POINT('Ctrl Pts',(65.3842659312291,-7.67917213547799,
65.564613257377));
#145669=CARTESIAN_POINT('Ctrl Pts',(65.4380564282991,-7.73843473867099,
65.5665426449911));
#145670=CARTESIAN_POINT('Ctrl Pts',(64.8058317116991,-5.52201624219599,
67.230640282151));
#145671=CARTESIAN_POINT('Ctrl Pts',(64.7749331788191,-5.50098256085199,
67.139286972566));
#145672=CARTESIAN_POINT('Ctrl Pts',(64.7172313694291,-5.47125424467599,
66.930476149142));
#145673=CARTESIAN_POINT('Ctrl Pts',(64.6691975511091,-5.48856163605999,
66.589141421244));
#145674=CARTESIAN_POINT('Ctrl Pts',(64.6694234445891,-5.573288773669,66.252648819473));
#145675=CARTESIAN_POINT('Ctrl Pts',(64.7105157551291,-5.70372966028198,
65.96379370785));
#145676=CARTESIAN_POINT('Ctrl Pts',(64.7778773578891,-5.85658577094199,
65.729818042446));
#145677=CARTESIAN_POINT('Ctrl Pts',(64.8607965267891,-6.01766835912799,
65.543296669127));
#145678=CARTESIAN_POINT('Ctrl Pts',(64.9541226473491,-6.18167532475599,
65.392893794028));
#145679=CARTESIAN_POINT('Ctrl Pts',(65.0580897008191,-6.35062629697198,
65.267762114542));
#145680=CARTESIAN_POINT('Ctrl Pts',(65.1765251610991,-6.53002757612,65.161024986461));
#145681=CARTESIAN_POINT('Ctrl Pts',(65.3142335534391,-6.72469234998399,
65.071054169118));
#145682=CARTESIAN_POINT('Ctrl Pts',(65.4761613813492,-6.93793738304699,
65.000296079579));
#145683=CARTESIAN_POINT('Ctrl Pts',(65.6580540847291,-7.16032441324298,
64.957284899351));
#145684=CARTESIAN_POINT('Ctrl Pts',(65.7921103656691,-7.31251780163099,
64.950635666937));
#145685=CARTESIAN_POINT('Ctrl Pts',(65.8598469333291,-7.38667276704598,
64.953620573712));
#145686=CARTESIAN_POINT('Ctrl Pts',(65.5578261387191,-5.25148611811499,
67.034089097041));
#145687=CARTESIAN_POINT('Ctrl Pts',(65.5321077652491,-5.23415329278699,
66.95747190315));
#145688=CARTESIAN_POINT('Ctrl Pts',(65.4840969924091,-5.20970588176098,
66.782734178228));
#145689=CARTESIAN_POINT('Ctrl Pts',(65.4438057846191,-5.22392714208799,
66.497514891794));
#145690=CARTESIAN_POINT('Ctrl Pts',(65.4432024666191,-5.29370795646599,
66.2154462285421));
#145691=CARTESIAN_POINT('Ctrl Pts',(65.4765356265291,-5.40171007433599,
65.971504655737));
#145692=CARTESIAN_POINT('Ctrl Pts',(65.5321490119791,-5.52919337005599,
65.771899666165));
#145693=CARTESIAN_POINT('Ctrl Pts',(65.6014213006191,-5.66461792108999,
65.61102310247));
#145694=CARTESIAN_POINT('Ctrl Pts',(65.6801624072491,-5.80356455863799,
65.479975844625));
#145695=CARTESIAN_POINT('Ctrl Pts',(65.7686054516391,-5.94766788378599,
65.370033317402));
#145696=CARTESIAN_POINT('Ctrl Pts',(65.8700307916591,-6.10154723232999,
65.275682893811));
#145697=CARTESIAN_POINT('Ctrl Pts',(65.9885549385691,-6.26923558293999,
65.195924179394));
#145698=CARTESIAN_POINT('Ctrl Pts',(66.1283506701291,-6.45340096160299,
65.133336548868));
#145699=CARTESIAN_POINT('Ctrl Pts',(66.2855066543292,-6.64555302768198,
65.095808364164));
#145700=CARTESIAN_POINT('Ctrl Pts',(66.4011371417991,-6.77680282292298,
65.090664511393));
#145701=CARTESIAN_POINT('Ctrl Pts',(66.4594531070191,-6.84062883253698,
65.093706344424));
#145702=CARTESIAN_POINT('',(64.9957413110435,-6.75150108785322,66.8052962244274));
#145703=CARTESIAN_POINT('Origin',(65.7929813465701,-6.16441562760705,66.6647005262893));
#145704=CARTESIAN_POINT('Ctrl Pts',(64.9957412482689,-6.75150113408116,
66.8052962354967));
#145705=CARTESIAN_POINT('Ctrl Pts',(64.9936068689243,-6.75150289354447,
66.7931850942144));
#145706=CARTESIAN_POINT('Ctrl Pts',(64.9919613219775,-6.75218103920743,
66.7810210222568));
#145707=CARTESIAN_POINT('Ctrl Pts',(64.990806008816,-6.75354673203848,66.7687616839126));
#145708=CARTESIAN_POINT('Ctrl Pts',(64.9903420903241,-6.75409512894045,
66.7638389201582));
#145709=CARTESIAN_POINT('Ctrl Pts',(64.9899575702403,-6.75475486043816,
66.7589008141091));
#145710=CARTESIAN_POINT('Ctrl Pts',(64.9896539598328,-6.75552852608416,
66.7539448192927));
#145711=CARTESIAN_POINT('Ctrl Pts',(64.9893478909668,-6.75630845641968,
66.7489486937441));
#145712=CARTESIAN_POINT('Ctrl Pts',(64.9891240499354,-6.75720417922191,
66.7439343836253));
#145713=CARTESIAN_POINT('Ctrl Pts',(64.9889836964078,-6.75821773879896,
66.7388992431453));
#145714=CARTESIAN_POINT('Ctrl Pts',(64.9886052261716,-6.76095085238226,
66.7253217375389));
#145715=CARTESIAN_POINT('Ctrl Pts',(64.9888244029213,-6.76452830191135,
66.7115917024379));
#145716=CARTESIAN_POINT('Ctrl Pts',(64.9896557162724,-6.76892729155128,
66.6978610038703));
#145717=CARTESIAN_POINT('Ctrl Pts',(64.9899520038508,-6.77049513114639,
66.6929672590232));
#145718=CARTESIAN_POINT('Ctrl Pts',(64.9903257678605,-6.77216693305507,
66.6880734760077));
#145719=CARTESIAN_POINT('Ctrl Pts',(64.9907767352693,-6.77394038232406,
66.6831866144325));
#145720=CARTESIAN_POINT('Ctrl Pts',(64.9911543157406,-6.77542523421738,
66.679095002798));
#145721=CARTESIAN_POINT('Ctrl Pts',(64.9915860087853,-6.77698133095018,
66.6750082448231));
#145722=CARTESIAN_POINT('Ctrl Pts',(64.9920709510125,-6.77860638547479,
66.6709299942178));
#145723=CARTESIAN_POINT('Ctrl Pts',(64.9942163426786,-6.78579565099697,
66.6528877525432));
#145724=CARTESIAN_POINT('Ctrl Pts',(64.9974229200744,-6.79435931348434,
66.6350163464812));
#145725=CARTESIAN_POINT('Ctrl Pts',(65.0016435135698,-6.80419766155188,
66.6173706480389));
#145726=CARTESIAN_POINT('Ctrl Pts',(65.0019806050124,-6.80498343325606,
66.6159613168746));
#145727=CARTESIAN_POINT('Ctrl Pts',(65.0023241818192,-6.80577735725546,
66.6145534283434));
#145728=CARTESIAN_POINT('Ctrl Pts',(65.0026742287018,-6.80657939339643,
66.6131470124946));
#145729=CARTESIAN_POINT('Ctrl Pts',(65.0034351778336,-6.80832289901075,
66.6100896765428));
#145730=CARTESIAN_POINT('Ctrl Pts',(65.004226700411,-6.81010473762457,66.6070392992945));
#145731=CARTESIAN_POINT('Ctrl Pts',(65.0050485723587,-6.81192444442103,
66.6039959761068));
#145732=CARTESIAN_POINT('Ctrl Pts',(65.0104135833997,-6.8238031161308,66.5841297882549));
#145733=CARTESIAN_POINT('Ctrl Pts',(65.017069095402,-6.83729073382415,66.564569670163));
#145734=CARTESIAN_POINT('Ctrl Pts',(65.0249308931841,-6.85218801398523,
66.5455059081924));
#145735=CARTESIAN_POINT('Ctrl Pts',(65.0257641556693,-6.85376695878043,
66.5434853630046));
#145736=CARTESIAN_POINT('Ctrl Pts',(65.0266109458093,-6.85536170153071,
66.5414704078398));
#145737=CARTESIAN_POINT('Ctrl Pts',(65.0274711486299,-6.85697199978835,
66.5394612146089));
#145738=CARTESIAN_POINT('Ctrl Pts',(65.034734709266,-6.87056937328712,66.5224955682377));
#145739=CARTESIAN_POINT('Ctrl Pts',(65.0429553072957,-6.88527632463471,
66.5059424169631));
#145740=CARTESIAN_POINT('Ctrl Pts',(65.0520130228369,-6.9008714845568,66.4899416996529));
#145741=CARTESIAN_POINT('Ctrl Pts',(65.0535496605724,-6.90351719705656,
66.4872271845082));
#145742=CARTESIAN_POINT('Ctrl Pts',(65.0551103163824,-6.90618838620459,
66.4845285292667));
#145743=CARTESIAN_POINT('Ctrl Pts',(65.0566943166813,-6.90888387134211,
66.4818463664612));
#145744=CARTESIAN_POINT('Ctrl Pts',(65.0573117932484,-6.90993462803117,
66.4808008030969));
#145745=CARTESIAN_POINT('Ctrl Pts',(65.0579328170036,-6.91098907647978,
66.4797577457591));
#145746=CARTESIAN_POINT('Ctrl Pts',(65.0585573503357,-6.91204715324597,
66.4787172235966));
#145747=CARTESIAN_POINT('Ctrl Pts',(65.0675938222681,-6.92735663395535,
66.4636617432355));
#145748=CARTESIAN_POINT('Ctrl Pts',(65.0773692007275,-6.94343040892352,
66.4491422646466));
#145749=CARTESIAN_POINT('Ctrl Pts',(65.0878742964325,-6.96024444379511,
66.4351010898323));
#145750=CARTESIAN_POINT('Ctrl Pts',(65.0907837768044,-6.96490124139173,
66.431212260671));
#145751=CARTESIAN_POINT('Ctrl Pts',(65.0937494246626,-6.96961500088883,
66.4273602900493));
#145752=CARTESIAN_POINT('Ctrl Pts',(65.0967714585411,-6.97438556823907,
66.4235443627965));
#145753=CARTESIAN_POINT('Ctrl Pts',(65.0969296794135,-6.97463533490569,
66.4233445770352));
#145754=CARTESIAN_POINT('Ctrl Pts',(65.0970880548828,-6.97488525731564,
66.4231448901174));
#145755=CARTESIAN_POINT('Ctrl Pts',(65.0972465850298,-6.97513533553087,
66.4229453018999));
#145756=CARTESIAN_POINT('Ctrl Pts',(65.1056308360837,-6.98836132805345,
66.4123895952783));
#145757=CARTESIAN_POINT('Ctrl Pts',(65.11444874283,-7.00202418757555,66.4021137805335));
#145758=CARTESIAN_POINT('Ctrl Pts',(65.1238002910885,-7.01625762713036,
66.3920320193054));
#145759=CARTESIAN_POINT('Ctrl Pts',(65.1301969814149,-7.02599365186076,
66.3851358452454));
#145760=CARTESIAN_POINT('Ctrl Pts',(65.1368440523132,-7.03599724609615,
66.3783311899346));
#145761=CARTESIAN_POINT('Ctrl Pts',(65.1437809996806,-7.0463159938978,66.3716013649534));
#145762=CARTESIAN_POINT('Ctrl Pts',(65.1443196991528,-7.04711731235965,
66.3710787498933));
#145763=CARTESIAN_POINT('Ctrl Pts',(65.1448601355016,-7.0479205171145,66.3705565810029));
#145764=CARTESIAN_POINT('Ctrl Pts',(65.1454023195242,-7.04872561738837,
66.3700348626769));
#145765=CARTESIAN_POINT('Ctrl Pts',(65.157176549479,-7.06620941507775,66.3587050718933));
#145766=CARTESIAN_POINT('Ctrl Pts',(65.1697742873168,-7.08458819847325,
66.3475839151916));
#145767=CARTESIAN_POINT('Ctrl Pts',(65.1833198536002,-7.10396819551667,
66.3367353431686));
#145768=CARTESIAN_POINT('Ctrl Pts',(65.1889252349162,-7.11198796162014,
66.332246023073));
#145769=CARTESIAN_POINT('Ctrl Pts',(65.1946930184249,-7.12017901613353,
66.3278039355833));
#145770=CARTESIAN_POINT('Ctrl Pts',(65.2006322564015,-7.12854790835301,
66.323416097461));
#145771=CARTESIAN_POINT('Ctrl Pts',(65.2021783884733,-7.13072654014328,
66.322273833542));
#145772=CARTESIAN_POINT('Ctrl Pts',(65.2037360963087,-7.13291718540268,
66.3211351618697));
#145773=CARTESIAN_POINT('Ctrl Pts',(65.2053053865769,-7.13511973984414,
66.3200003169949));
#145774=CARTESIAN_POINT('Ctrl Pts',(65.2199248637306,-7.15563869353206,
66.3094281245488));
#145775=CARTESIAN_POINT('Ctrl Pts',(65.2355518767617,-7.17719463681946,
66.2991875114242));
#145776=CARTESIAN_POINT('Ctrl Pts',(65.2521863781437,-7.19970040895401,
66.2894705284383));
#145777=CARTESIAN_POINT('Ctrl Pts',(65.2579637656283,-7.20751696824105,
66.286095688724));
#145778=CARTESIAN_POINT('Ctrl Pts',(65.2638624291241,-7.21544772945101,
66.2827840693087));
#145779=CARTESIAN_POINT('Ctrl Pts',(65.2698815295365,-7.22348782013174,
66.2795438864646));
#145780=CARTESIAN_POINT('Ctrl Pts',(65.2728140576992,-7.22740498228831,
66.2779652573022));
#145781=CARTESIAN_POINT('Ctrl Pts',(65.2757752682902,-7.23134816203923,
66.2764038098071));
#145782=CARTESIAN_POINT('Ctrl Pts',(65.2787654844822,-7.23531735155886,
66.2748602419139));
#145783=CARTESIAN_POINT('Ctrl Pts',(65.2953143393923,-7.25728417176686,
66.266317621759));
#145784=CARTESIAN_POINT('Ctrl Pts',(65.3127524129375,-7.28004996710753,
66.2583195996746));
#145785=CARTESIAN_POINT('Ctrl Pts',(65.331133299115,-7.30361038858351,66.2510082076709));
#145786=CARTESIAN_POINT('Ctrl Pts',(65.3379826757077,-7.31238984555927,
66.2482837211164));
#145787=CARTESIAN_POINT('Ctrl Pts',(65.3449628620906,-7.32127934330882,
66.2456549583717));
#145788=CARTESIAN_POINT('Ctrl Pts',(65.352076172117,-7.33027746437928,66.2431306889924));
#145789=CARTESIAN_POINT('Ctrl Pts',(65.3567887585433,-7.33623874303322,
66.2414583539515));
#145790=CARTESIAN_POINT('Ctrl Pts',(65.3615598154622,-7.34224766988668,
66.2398322314557));
#145791=CARTESIAN_POINT('Ctrl Pts',(65.3663903157263,-7.34830410595062,
66.2382550148849));
#145792=CARTESIAN_POINT('Ctrl Pts',(65.3837209722507,-7.37003312105212,
66.2325963465985));
#145793=CARTESIAN_POINT('Ctrl Pts',(65.4018176405439,-7.39237575559042,
66.2275642249406));
#145794=CARTESIAN_POINT('Ctrl Pts',(65.4207235793857,-7.41532150571302,
66.2233112864293));
#145795=CARTESIAN_POINT('Ctrl Pts',(65.4297043454721,-7.42622127727429,
66.2212910405019));
#145796=CARTESIAN_POINT('Ctrl Pts',(65.4388675593786,-7.43725674442328,
66.2194471739687));
#145797=CARTESIAN_POINT('Ctrl Pts',(65.4482167623584,-7.44842431244937,
66.2177992883089));
#145798=CARTESIAN_POINT('Origin',(77.1089102519491,1.4210854715202E-14,
81.89107979688));
#145799=CARTESIAN_POINT('',(65.0614528323817,-6.75160559577343,67.1773204194393));
#145800=CARTESIAN_POINT('Ctrl Pts',(65.6628233895018,-7.69741763536957,
66.1799583497825));
#145801=CARTESIAN_POINT('Ctrl Pts',(65.6127075559676,-7.63232133342805,
66.2334606385732));
#145802=CARTESIAN_POINT('Ctrl Pts',(65.5649450822481,-7.56794231263672,
66.2888414104336));
#145803=CARTESIAN_POINT('Ctrl Pts',(65.5194507398504,-7.50436891431119,
66.3461211498897));
#145804=CARTESIAN_POINT('Ctrl Pts',(65.5035580018977,-7.48216054054206,
66.3661309322318));
#145805=CARTESIAN_POINT('Ctrl Pts',(65.4879424060478,-7.46005074136449,
66.3863723088932));
#145806=CARTESIAN_POINT('Ctrl Pts',(65.472601424378,-7.43804417092933,66.4068456354934));
#145807=CARTESIAN_POINT('Ctrl Pts',(65.4692867937749,-7.43328934797185,
66.4112691799808));
#145808=CARTESIAN_POINT('Ctrl Pts',(65.4659849791221,-7.42853931851314,
66.4157036512151));
#145809=CARTESIAN_POINT('Ctrl Pts',(65.4626959189898,-7.4237941090516,66.420148940823));
#145810=CARTESIAN_POINT('Ctrl Pts',(65.4365856047165,-7.38612410444588,
66.4554380216017));
#145811=CARTESIAN_POINT('Ctrl Pts',(65.4112792364022,-7.34875798046335,
66.4914096876316));
#145812=CARTESIAN_POINT('Ctrl Pts',(65.3867600614493,-7.31171561938907,
66.5280685818853));
#145813=CARTESIAN_POINT('Ctrl Pts',(65.3729561601058,-7.29086136557404,
66.5487069500447));
#145814=CARTESIAN_POINT('Ctrl Pts',(65.3592361678855,-7.26985646092619,
66.5698166149439));
#145815=CARTESIAN_POINT('Ctrl Pts',(65.3458495281046,-7.24908536245234,
66.591022713179));
#145816=CARTESIAN_POINT('Ctrl Pts',(65.3324628883238,-7.22831426397849,
66.612228811414));
#145817=CARTESIAN_POINT('Ctrl Pts',(65.3194096074541,-7.20777716874016,
66.6335313515063));
#145818=CARTESIAN_POINT('Ctrl Pts',(65.3069059172977,-7.18784778724475,
66.6545146388941));
#145819=CARTESIAN_POINT('Ctrl Pts',(65.2686650771674,-7.12689647750146,
66.7186891768395));
#145820=CARTESIAN_POINT('Ctrl Pts',(65.2332616977372,-7.06794612605696,
66.7838861851928));
#145821=CARTESIAN_POINT('Ctrl Pts',(65.200445601414,-7.01101868563781,66.8499281049124));
#145822=CARTESIAN_POINT('Ctrl Pts',(65.1773957807998,-6.9710332078783,66.8963155358718));
#145823=CARTESIAN_POINT('Ctrl Pts',(65.1556242548341,-6.93204598359059,
66.9431219028185));
#145824=CARTESIAN_POINT('Ctrl Pts',(65.1351143718149,-6.8941175358365,66.9904058935751));
#145825=CARTESIAN_POINT('Ctrl Pts',(65.1129261116537,-6.85308530442445,
67.0415592564385));
#145826=CARTESIAN_POINT('Ctrl Pts',(65.0922142864307,-6.81329230333574,
67.0932711865362));
#145827=CARTESIAN_POINT('Ctrl Pts',(65.0729367663882,-6.77479600626462,
67.1455623671584));
#145828=CARTESIAN_POINT('Ctrl Pts',(65.0690422793673,-6.76701889961564,
67.1561263465393));
#145829=CARTESIAN_POINT('Ctrl Pts',(65.0652062714112,-6.75929465525485,
67.1667138179077));
#145830=CARTESIAN_POINT('Ctrl Pts',(65.0614283108073,-6.75162365816252,
67.1773247406763));
#145831=CARTESIAN_POINT('',(65.0614295862717,-6.75162271773899,67.1773245146892));
#145832=CARTESIAN_POINT('Origin',(77.1089102519491,1.4210854715202E-14,
81.89107979688));
#145833=CARTESIAN_POINT('',(64.9957413410401,6.7515010657631,66.8052962191372));
#145834=CARTESIAN_POINT('',(65.0614282834239,6.75162228554997,67.1773189309182));
#145835=CARTESIAN_POINT('',(65.6628212128545,7.69739984953404,66.1799651776145));
#145836=CARTESIAN_POINT('Ctrl Pts',(65.0614282834239,6.75162228554997,67.1773189309182));
#145837=CARTESIAN_POINT('Ctrl Pts',(65.0936086814867,6.81696027379672,67.086937637008));
#145838=CARTESIAN_POINT('Ctrl Pts',(65.1299716419799,6.88614028642303,66.9982120934198));
#145839=CARTESIAN_POINT('Ctrl Pts',(65.1707899936982,6.95892998196222,66.9110941930759));
#145840=CARTESIAN_POINT('Ctrl Pts',(65.1911991695574,6.99532482973182,66.8675352429039));
#145841=CARTESIAN_POINT('Ctrl Pts',(65.2127225848764,7.03262146593794,66.8243781344839));
#145842=CARTESIAN_POINT('Ctrl Pts',(65.2353966066073,7.07078698935139,66.7816164553411));
#145843=CARTESIAN_POINT('Ctrl Pts',(65.2515080065354,7.09790613118162,66.7512314392885));
#145844=CARTESIAN_POINT('Ctrl Pts',(65.2678894704613,7.12496058509741,66.721572719888));
#145845=CARTESIAN_POINT('Ctrl Pts',(65.2852160836108,7.15301162432833,66.6915154711413));
#145846=CARTESIAN_POINT('Ctrl Pts',(65.2922736955954,7.16443759367097,66.6792723168012));
#145847=CARTESIAN_POINT('Ctrl Pts',(65.2994885686195,7.17602855145341,66.6669629614903));
#145848=CARTESIAN_POINT('Ctrl Pts',(65.3069082509523,7.18785463689311,66.654511047652));
#145849=CARTESIAN_POINT('Ctrl Pts',(65.3692579692799,7.287232624119,66.5498740449287));
#145850=CARTESIAN_POINT('Ctrl Pts',(65.4373698278873,7.38919787124566,66.4504117121515));
#145851=CARTESIAN_POINT('Ctrl Pts',(65.5115870550174,7.49335931066728,66.3560635289208));
#145852=CARTESIAN_POINT('Ctrl Pts',(65.5594279581965,7.5605024461771,66.2952460816299));
#145853=CARTESIAN_POINT('Ctrl Pts',(65.6098058991986,7.62855713753377,66.2365536262945));
#145854=CARTESIAN_POINT('Ctrl Pts',(65.662813434262,7.69740712101228,66.1799698427528));
#145855=CARTESIAN_POINT('',(65.4482167089465,7.44842435396614,66.2177992977254));
#145856=CARTESIAN_POINT('Origin',(74.0770084968991,1.4210854715202E-14,
64.696310494594));
#145857=CARTESIAN_POINT('Ctrl Pts',(64.9957413309291,6.75150107320901,66.80529622092));
#145858=CARTESIAN_POINT('Ctrl Pts',(64.9939147746393,6.75150118167963,66.7949374485334));
#145859=CARTESIAN_POINT('Ctrl Pts',(64.9894338048507,6.7530267160936,66.7631516371945));
#145860=CARTESIAN_POINT('Ctrl Pts',(64.9875165633987,6.76373848476411,66.7075258057507));
#145861=CARTESIAN_POINT('Ctrl Pts',(64.9953306241186,6.79090605225776,66.63784977939));
#145862=CARTESIAN_POINT('Ctrl Pts',(65.0150684046813,6.83452434266292,66.5653197541562));
#145863=CARTESIAN_POINT('Ctrl Pts',(65.0481757788599,6.89549721919369,66.4921639904142));
#145864=CARTESIAN_POINT('Ctrl Pts',(65.0958776509467,6.97417184586988,66.4206746812155));
#145865=CARTESIAN_POINT('Ctrl Pts',(65.1594070364026,7.07061581212493,66.3532950647828));
#145866=CARTESIAN_POINT('Ctrl Pts',(65.2401133825063,7.1846757117932,66.2929751276064));
#145867=CARTESIAN_POINT('Ctrl Pts',(65.3374029752483,7.31312989194673,66.2447445995378));
#145868=CARTESIAN_POINT('Ctrl Pts',(65.410159366793,7.40296747944908,66.2245011702614));
#145869=CARTESIAN_POINT('Ctrl Pts',(65.4482167191791,7.44842434513301,66.217799295921));
#145870=CARTESIAN_POINT('Origin',(65.9936985527191,-6.16441400296899,67.803130872521));
#145871=CARTESIAN_POINT('Ctrl Pts',(65.0614295956489,-6.75162271329526,
67.1773245130358));
#145872=CARTESIAN_POINT('Ctrl Pts',(65.0357806317137,-6.71568906787898,
67.1819829434292));
#145873=CARTESIAN_POINT('Ctrl Pts',(65.0124824624939,-6.67801772235096,
67.1861703445779));
#145874=CARTESIAN_POINT('Ctrl Pts',(64.9917449493442,-6.6389415340824,67.1898735572973));
#145875=CARTESIAN_POINT('Ctrl Pts',(64.9710061590129,-6.59986293919032,
67.1935769980901));
#145876=CARTESIAN_POINT('Ctrl Pts',(64.9528285550174,-6.55937973262129,
67.1967961529284));
#145877=CARTESIAN_POINT('Ctrl Pts',(64.9373768558342,-6.51784954555001,
67.1995258269408));
#145878=CARTESIAN_POINT('Ctrl Pts',(64.9311493087832,-6.50111150328317,
67.2006259760664));
#145879=CARTESIAN_POINT('Ctrl Pts',(64.9253640162319,-6.48420364016903,
67.2016467094416));
#145880=CARTESIAN_POINT('Ctrl Pts',(64.9200295766639,-6.46715026990716,
67.2025880722727));
#145881=CARTESIAN_POINT('',(64.8738238573791,-6.16438935871099,67.210776354606));
#145882=CARTESIAN_POINT('Origin',(67.8574209319491,111.0724296188,84.13159620183));
#145883=CARTESIAN_POINT('',(65.1554501449391,-13.43008249787,68.807974748468));
#145884=CARTESIAN_POINT('Origin',(64.9111938245191,0.499074165591614,67.422711970997));
#145885=CARTESIAN_POINT('',(65.1554596847291,6.92820316569601,68.807986718554));
#145886=CARTESIAN_POINT('',(64.8738236000791,6.16438877351401,67.210774895336));
#145887=CARTESIAN_POINT('Ctrl Pts',(65.1269899167215,6.68586918419113,68.6465524198017));
#145888=CARTESIAN_POINT('Ctrl Pts',(65.1258607393499,6.6788598129293,68.640148532931));
#145889=CARTESIAN_POINT('Ctrl Pts',(65.124702511399,6.67185299366292,68.6335798904187));
#145890=CARTESIAN_POINT('Ctrl Pts',(65.1235144956525,6.66484982371274,68.6268423120024));
#145891=CARTESIAN_POINT('Ctrl Pts',(65.120473486417,6.64692354238209,68.6095958754548));
#145892=CARTESIAN_POINT('Ctrl Pts',(65.117237346027,6.62901914992627,68.5912427894659));
#145893=CARTESIAN_POINT('Ctrl Pts',(65.1137875519203,6.61115996404497,68.5716780151953));
#145894=CARTESIAN_POINT('Ctrl Pts',(65.1102351559665,6.59276962024424,68.5515313563492));
#145895=CARTESIAN_POINT('Ctrl Pts',(65.106456074087,6.57442649737051,68.530099099943));
#145896=CARTESIAN_POINT('Ctrl Pts',(65.1024308862485,6.55619573439959,68.5072711131346));
#145897=CARTESIAN_POINT('Ctrl Pts',(65.09832758876,6.53761119948784,68.4840001442517));
#145898=CARTESIAN_POINT('Ctrl Pts',(65.09396848797,6.51914372357155,68.4592784487402));
#145899=CARTESIAN_POINT('Ctrl Pts',(65.0893316050564,6.50087699663407,68.4329813787262));
#145900=CARTESIAN_POINT('Ctrl Pts',(65.0846447485376,6.48241340162472,68.4064008943114));
#145901=CARTESIAN_POINT('Ctrl Pts',(65.0796740241207,6.46415513437845,68.3782105212977));
#145902=CARTESIAN_POINT('Ctrl Pts',(65.0743965924953,6.44621207552659,68.3482807294666));
#145903=CARTESIAN_POINT('Ctrl Pts',(65.0690851709034,6.42815345213261,68.318158171022));
#145904=CARTESIAN_POINT('Ctrl Pts',(65.0634629542406,6.41041440358812,68.2862730103171));
#145905=CARTESIAN_POINT('Ctrl Pts',(65.0575092298989,6.39313250902638,68.2525077772224));
#145906=CARTESIAN_POINT('Ctrl Pts',(65.0527301358131,6.37926021744024,68.2254042002801));
#145907=CARTESIAN_POINT('Ctrl Pts',(65.047737608407,6.3656837258347,68.1970901834972));
#145908=CARTESIAN_POINT('Ctrl Pts',(65.0425198259768,6.3524726480596,68.16749868105));
#145909=CARTESIAN_POINT('Ctrl Pts',(65.0411986195115,6.34912744123976,68.1600057499295));
#145910=CARTESIAN_POINT('Ctrl Pts',(65.0398532109862,6.34578094414381,68.1523755620387));
#145911=CARTESIAN_POINT('Ctrl Pts',(65.0384839951051,6.3424383158584,68.1446103558303));
#145912=CARTESIAN_POINT('Ctrl Pts',(65.0330448194473,6.32915980904687,68.1137632694282));
#145913=CARTESIAN_POINT('Ctrl Pts',(65.0272294990806,6.31594506631054,68.0807829588119));
#145914=CARTESIAN_POINT('Ctrl Pts',(65.0210597275564,6.30310947651882,68.0457924531821));
#145915=CARTESIAN_POINT('Ctrl Pts',(65.0197620560254,6.300409801273,68.0384329937868));
#145916=CARTESIAN_POINT('Ctrl Pts',(65.0184487265847,6.29772676799765,68.0309847338614));
#145917=CARTESIAN_POINT('Ctrl Pts',(65.0171199775613,6.29506309001698,68.0234490250218));
#145918=CARTESIAN_POINT('Ctrl Pts',(65.0111943844742,6.28318434425673,67.9898433226514));
#145919=CARTESIAN_POINT('Ctrl Pts',(65.0049615477093,6.27169277400508,67.9544951524432));
#145920=CARTESIAN_POINT('Ctrl Pts',(64.9984504770749,6.26082766944341,67.9175690374176));
#145921=CARTESIAN_POINT('Ctrl Pts',(64.9967188376108,6.25793806112909,67.907748422403));
#145922=CARTESIAN_POINT('Ctrl Pts',(64.9949675588263,6.25509260064891,67.8978164271211));
#145923=CARTESIAN_POINT('Ctrl Pts',(64.9931972748634,6.25229542027833,67.8877766479843));
#145924=CARTESIAN_POINT('Ctrl Pts',(64.9865434827275,6.24178193366082,67.8500411180529));
#145925=CARTESIAN_POINT('Ctrl Pts',(64.9796207498768,6.23195352672873,67.8107803476211));
#145926=CARTESIAN_POINT('Ctrl Pts',(64.9724629900716,6.22299781395229,67.7701866722689));
#145927=CARTESIAN_POINT('Ctrl Pts',(64.9705097863249,6.22055398624287,67.7591095027427));
#145928=CARTESIAN_POINT('Ctrl Pts',(64.9685391158548,6.21817491653994,67.7479332744464));
#145929=CARTESIAN_POINT('Ctrl Pts',(64.9665517437151,6.21586389941347,67.7366623262435));
#145930=CARTESIAN_POINT('Ctrl Pts',(64.9594137719853,6.20756350383758,67.6961808743631));
#145931=CARTESIAN_POINT('Ctrl Pts',(64.9520599251814,6.20014425028192,67.6544751336973));
#145932=CARTESIAN_POINT('Ctrl Pts',(64.9445307639359,6.19372173806413,67.6117751362589));
#145933=CARTESIAN_POINT('Ctrl Pts',(64.9420607517207,6.1916147724788,67.5977670001828));
#145934=CARTESIAN_POINT('Ctrl Pts',(64.9395719148494,6.18961474102989,67.5836521042657));
#145935=CARTESIAN_POINT('Ctrl Pts',(64.9370658072044,6.18772473138426,67.5694392610461));
#145936=CARTESIAN_POINT('Ctrl Pts',(64.9290840161445,6.18170517267833,67.5241722729452));
#145937=CARTESIAN_POINT('Ctrl Pts',(64.9209269430576,6.17680556358816,67.4779112124193));
#145938=CARTESIAN_POINT('Ctrl Pts',(64.9126296391413,6.17308359635863,67.4308548650867));
#145939=CARTESIAN_POINT('Ctrl Pts',(64.9099778113126,6.17189405137193,67.4158156026189));
#145940=CARTESIAN_POINT('Ctrl Pts',(64.9073116720097,6.17082440163475,67.4006951759143));
#145941=CARTESIAN_POINT('Ctrl Pts',(64.9046323987211,6.16987543159412,67.3855002628188));
#145942=CARTESIAN_POINT('Ctrl Pts',(64.89575649588,6.16673168141535,67.3351625190385));
#145943=CARTESIAN_POINT('Ctrl Pts',(64.886736281088,6.16491611625309,67.2840063433688));
#145944=CARTESIAN_POINT('Ctrl Pts',(64.8776208551351,6.16448731723589,67.2323101971345));
#145945=CARTESIAN_POINT('Ctrl Pts',(64.8763568863287,6.16442785884253,67.2251418742725));
#145946=CARTESIAN_POINT('Ctrl Pts',(64.8750910900749,6.16439498447354,67.2179631874115));
#145947=CARTESIAN_POINT('Ctrl Pts',(64.8738236001678,6.16438877351401,67.2107748953204));
#145948=CARTESIAN_POINT('',(64.8738236000791,6.16438877351401,67.210774895336));
#145949=CARTESIAN_POINT('Origin',(65.9862249718391,6.16441400296901,67.760746089178));
#145950=CARTESIAN_POINT('Origin',(65.8588926025934,6.16441457066984,67.038621762377));
#145951=CARTESIAN_POINT('Origin',(65.7929806594911,6.16441569484309,66.6647268826104));
#145952=CARTESIAN_POINT('Ctrl Pts',(65.2148209050525,5.35492257705576,66.7666660125659));
#145953=CARTESIAN_POINT('Ctrl Pts',(65.2067722047426,5.35492482391508,66.7210106884506));
#145954=CARTESIAN_POINT('Ctrl Pts',(65.1864417669287,5.36110944695451,66.5810340695068));
#145955=CARTESIAN_POINT('Ctrl Pts',(65.1750536527964,5.40441097153357,66.3436679578443));
#145956=CARTESIAN_POINT('Ctrl Pts',(65.1976263796561,5.5026709611402,66.0785753213486));
#145957=CARTESIAN_POINT('Ctrl Pts',(65.2514687636523,5.6366770529586,65.8445384223639));
#145958=CARTESIAN_POINT('Ctrl Pts',(65.3294129760629,5.79388364819421,65.6465729402952));
#145959=CARTESIAN_POINT('Ctrl Pts',(65.4269859006806,5.96721711211323,65.481370283013));
#145960=CARTESIAN_POINT('Ctrl Pts',(65.5434369630249,6.15480444083051,65.3440105246222));
#145961=CARTESIAN_POINT('Ctrl Pts',(65.6810291451864,6.35793052064432,65.2315827919279));
#145962=CARTESIAN_POINT('Ctrl Pts',(65.8411083711151,6.57500738265653,65.1465990105339));
#145963=CARTESIAN_POINT('Ctrl Pts',(65.9609957865493,6.72440924846806,65.1119429840824));
#145964=CARTESIAN_POINT('Ctrl Pts',(66.024898044746,6.80073525449069,65.1006867422596));
#145965=CARTESIAN_POINT('Ctrl Pts',(64.7478165014519,5.69883052261465,66.8490114890303));
#145966=CARTESIAN_POINT('Ctrl Pts',(64.7397678016923,5.69883277272402,66.8033561572532));
#145967=CARTESIAN_POINT('Ctrl Pts',(64.719492874681,5.70509510400391,66.6633697271873));
#145968=CARTESIAN_POINT('Ctrl Pts',(64.7084945927605,5.7489422686341,66.425934839464));
#145969=CARTESIAN_POINT('Ctrl Pts',(64.7320602908078,5.84858612855244,66.160667075277));
#145970=CARTESIAN_POINT('Ctrl Pts',(64.7875095659817,5.98481406017563,65.9263468057011));
#145971=CARTESIAN_POINT('Ctrl Pts',(64.8677266075285,6.14512650416259,65.7279805382333));
#145972=CARTESIAN_POINT('Ctrl Pts',(64.9682788441699,6.32246750877359,65.5622525302054));
#145973=CARTESIAN_POINT('Ctrl Pts',(65.0884553317283,6.5149675127728,65.4242358662292));
#145974=CARTESIAN_POINT('Ctrl Pts',(65.2305600206851,6.72390358841762,65.3110124480889));
#145975=CARTESIAN_POINT('Ctrl Pts',(65.3958656909537,6.9475236623724,65.2251070982072));
#145976=CARTESIAN_POINT('Ctrl Pts',(65.5195237655255,7.10150168396956,65.1897862015458));
#145977=CARTESIAN_POINT('Ctrl Pts',(65.5853645199204,7.18014318571723,65.1781881505423));
#145978=CARTESIAN_POINT('Ctrl Pts',(64.6570714587516,6.27731354668077,66.8650128591567));
#145979=CARTESIAN_POINT('Ctrl Pts',(64.6516000319702,6.27731489253399,66.8339775578073));
#145980=CARTESIAN_POINT('Ctrl Pts',(64.6378901917127,6.28164735941406,66.7388053795214));
#145981=CARTESIAN_POINT('Ctrl Pts',(64.6308148861991,6.31199535826295,66.5766500360433));
#145982=CARTESIAN_POINT('Ctrl Pts',(64.6482673217965,6.38219167007379,66.3923267568599));
#145983=CARTESIAN_POINT('Ctrl Pts',(64.689589956481,6.48097961696787,66.2249050521873));
#145984=CARTESIAN_POINT('Ctrl Pts',(64.7512349038882,6.60143060796609,66.078236838856));
#145985=CARTESIAN_POINT('Ctrl Pts',(64.8311297980253,6.73956249720055,65.9513263032596));
#145986=CARTESIAN_POINT('Ctrl Pts',(64.9293853272694,6.8943095462238,65.8422964628036));
#145987=CARTESIAN_POINT('Ctrl Pts',(65.0479270422314,7.06635306504569,65.7506568750857));
#145988=CARTESIAN_POINT('Ctrl Pts',(65.1872242958992,7.2532642842925,65.6799752747044));
#145989=CARTESIAN_POINT('Ctrl Pts',(65.2913599872053,7.38256988089626,65.6506242928727));
#145990=CARTESIAN_POINT('Ctrl Pts',(65.3464951967837,7.44842499426927,65.6409115118738));
#145991=CARTESIAN_POINT('Ctrl Pts',(64.9957431297417,6.75150352764831,66.8052967130971));
#145992=CARTESIAN_POINT('Ctrl Pts',(64.993916514239,6.75150359144112,66.7949372501368));
#145993=CARTESIAN_POINT('Ctrl Pts',(64.9894355913503,6.7530291115906,66.7631517609198));
#145994=CARTESIAN_POINT('Ctrl Pts',(64.9875183761111,6.7637407804721,66.7075264708465));
#145995=CARTESIAN_POINT('Ctrl Pts',(64.99533238785,6.79090812929874,66.6378510271096));
#145996=CARTESIAN_POINT('Ctrl Pts',(65.0150700587209,6.83452613933823,66.5653214841042));
#145997=CARTESIAN_POINT('Ctrl Pts',(65.0481772878749,6.89549871360824,66.4921660939439));
#145998=CARTESIAN_POINT('Ctrl Pts',(65.0958789963607,6.97417303812965,66.4206770663893));
#145999=CARTESIAN_POINT('Ctrl Pts',(65.1594082053423,7.07061670809534,66.3532976616181));
#146000=CARTESIAN_POINT('Ctrl Pts',(65.2401143591712,7.18467631309772,66.2929778836045));
#146001=CARTESIAN_POINT('Ctrl Pts',(65.3374037384352,7.31313019617951,66.2447474696296));
#146002=CARTESIAN_POINT('Ctrl Pts',(65.4101599705141,7.40296758311013,66.2245040866366));
#146003=CARTESIAN_POINT('Ctrl Pts',(65.4482167677065,7.44842452942846,66.2177992873806));
#146004=CARTESIAN_POINT('Origin',(66.19854598009,6.80073540805928,66.0854943910165));
#146005=CARTESIAN_POINT('Origin',(74.0770084968991,1.4210854715202E-14,
64.696310494594));
#146006=CARTESIAN_POINT('Ctrl Pts',(66.2208657833691,7.02807183034301,65.066133808363));
#146007=CARTESIAN_POINT('Ctrl Pts',(65.7922441264735,7.4201337906415,65.1417542799438));
#146008=CARTESIAN_POINT('Ctrl Pts',(65.5610416355161,7.69728092662338,65.6031233574458));
#146009=CARTESIAN_POINT('Ctrl Pts',(65.6628292019748,7.69739218035355,66.1799637693547));
#146010=CARTESIAN_POINT('Ctrl Pts',(66.3469292448691,6.71669427049301,65.089883295194));
#146011=CARTESIAN_POINT('Ctrl Pts',(66.4172621304691,6.79578693974001,65.077481709831));
#146012=CARTESIAN_POINT('Ctrl Pts',(66.7042933355591,7.12081872370401,65.026870364069));
#146013=CARTESIAN_POINT('Ctrl Pts',(67.1737243974691,7.637641242897,64.9440970022721));
#146014=CARTESIAN_POINT('Ctrl Pts',(67.5996249658591,8.01039274550502,64.8689992409641));
#146015=CARTESIAN_POINT('Ctrl Pts',(67.8135694122091,8.17107382160801,64.8312750627));
#146016=CARTESIAN_POINT('Ctrl Pts',(65.6590187149691,7.304104680347,64.933907788844));
#146017=CARTESIAN_POINT('Ctrl Pts',(65.7282021697291,7.38185342331901,64.9217088791509));
#146018=CARTESIAN_POINT('Ctrl Pts',(66.0154107300992,7.70671666045502,64.871066260868));
#146019=CARTESIAN_POINT('Ctrl Pts',(66.5149459070591,8.25911872987902,64.782984731357));
#146020=CARTESIAN_POINT('Ctrl Pts',(67.0067799852291,8.69061703812601,64.696261113344));
#146021=CARTESIAN_POINT('Ctrl Pts',(67.2535719696491,8.87601922441701,64.652745027867));
#146022=CARTESIAN_POINT('Ctrl Pts',(65.2973419556991,7.73916500145001,65.656703935734));
#146023=CARTESIAN_POINT('Ctrl Pts',(65.3656740946791,7.81591837732301,65.6446551359809));
#146024=CARTESIAN_POINT('Ctrl Pts',(65.6530140116592,8.140656781741,65.593989355983));
#146025=CARTESIAN_POINT('Ctrl Pts',(66.1748455349991,8.71941053014201,65.501976379035));
#146026=CARTESIAN_POINT('Ctrl Pts',(66.7155126836291,9.19441914004002,65.406642173149));
#146027=CARTESIAN_POINT('Ctrl Pts',(66.9866329063991,9.39813079779402,65.358836362857));
#146028=CARTESIAN_POINT('Ctrl Pts',(65.6490951182391,7.55611768221601,66.484476132488));
#146029=CARTESIAN_POINT('Ctrl Pts',(65.7177854398991,7.63328984893302,66.472364175465));
#146030=CARTESIAN_POINT('Ctrl Pts',(66.0050700898891,7.95808077548001,66.421708140529));
#146031=CARTESIAN_POINT('Ctrl Pts',(66.5175206464091,8.52574731606101,66.331349281135));
#146032=CARTESIAN_POINT('Ctrl Pts',(67.0376417645191,8.98244939766902,66.239637894777));
#146033=CARTESIAN_POINT('Ctrl Pts',(67.2985261220691,9.17845752672701,66.193636943696));
#146034=CARTESIAN_POINT('',(67.0545200752973,9.08847803716292,65.7314839970685));
#146035=CARTESIAN_POINT('Ctrl Pts',(65.6628302778855,7.69739278665024,66.1799667264387));
#146036=CARTESIAN_POINT('Ctrl Pts',(65.8925920723134,7.96901192097917,66.0738323942691));
#146037=CARTESIAN_POINT('Ctrl Pts',(66.1235380564785,8.22889166321445,65.9816475253631));
#146038=CARTESIAN_POINT('Ctrl Pts',(66.5910239409522,8.69801793251633,65.8306234162482));
#146039=CARTESIAN_POINT('Ctrl Pts',(66.8277216597037,8.90785102579189,65.7715384074934));
#146040=CARTESIAN_POINT('Ctrl Pts',(67.0545035221437,9.08849832361973,65.7314815782556));
#146041=CARTESIAN_POINT('Ctrl Pts',(67.5092801258532,8.31611453423606,64.8389516201314));
#146042=CARTESIAN_POINT('Ctrl Pts',(67.4857251216335,8.34676180112001,64.8431135225438));
#146043=CARTESIAN_POINT('Ctrl Pts',(67.4625360504388,8.37744483878468,64.8495177543901));
#146044=CARTESIAN_POINT('Ctrl Pts',(67.4398979647076,8.40792091496171,64.8581222512767));
#146045=CARTESIAN_POINT('Ctrl Pts',(67.4164854557802,8.43943954308423,64.8670210982271));
#146046=CARTESIAN_POINT('Ctrl Pts',(67.3936625517779,8.47073630068296,64.8782726210766));
#146047=CARTESIAN_POINT('Ctrl Pts',(67.3716088947925,8.50156426811195,64.8917847097676));
#146048=CARTESIAN_POINT('Ctrl Pts',(67.3479088056494,8.53469372036818,64.9063055534854));
#146049=CARTESIAN_POINT('Ctrl Pts',(67.3250973264477,8.56728134404552,64.9234363998483));
#146050=CARTESIAN_POINT('Ctrl Pts',(67.303364532704,8.59905323088256,64.9430221214877));
#146051=CARTESIAN_POINT('Ctrl Pts',(67.2803811050845,8.63265346056626,64.9637349217372));
#146052=CARTESIAN_POINT('Ctrl Pts',(67.2586038660606,8.66534146643593,64.9871924753379));
#146053=CARTESIAN_POINT('Ctrl Pts',(67.2382220938984,8.69683126854594,65.0131798314819));
#146054=CARTESIAN_POINT('Ctrl Pts',(67.2157747527014,8.73151237117853,65.041800848611));
#146055=CARTESIAN_POINT('Ctrl Pts',(67.1950196746371,8.76474056465054,65.0734903266037));
#146056=CARTESIAN_POINT('Ctrl Pts',(67.1761723506734,8.79617468174395,65.1079321649017));
#146057=CARTESIAN_POINT('Ctrl Pts',(67.1724545513139,8.80237533604492,65.114726118495));
#146058=CARTESIAN_POINT('Ctrl Pts',(67.1688108901592,8.80850628147018,65.1216270832089));
#146059=CARTESIAN_POINT('Ctrl Pts',(67.1652428932428,8.81456503217954,65.1286325013422));
#146060=CARTESIAN_POINT('Ctrl Pts',(67.1485433751963,8.84292218023257,65.1614203958617));
#146061=CARTESIAN_POINT('Ctrl Pts',(67.1335316836684,8.86964762216346,65.1964438190701));
#146062=CARTESIAN_POINT('Ctrl Pts',(67.1203440833421,8.89449767307029,65.2333741365688));
#146063=CARTESIAN_POINT('Ctrl Pts',(67.107445608841,8.91880290981096,65.2694947913344));
#146064=CARTESIAN_POINT('Ctrl Pts',(67.0962919734964,8.94131432017231,65.3074398519547));
#146065=CARTESIAN_POINT('Ctrl Pts',(67.0869839112616,8.96183111467034,65.3468720680325));
#146066=CARTESIAN_POINT('Ctrl Pts',(67.0780132010575,8.98160431913696,65.3848751425944));
#146067=CARTESIAN_POINT('Ctrl Pts',(67.0707567941787,8.9995248045942,65.4242597030815));
#146068=CARTESIAN_POINT('Ctrl Pts',(67.0652801409245,9.01543717558087,65.4646929574987));
#146069=CARTESIAN_POINT('Ctrl Pts',(67.0599874736179,9.03081497690973,65.5037678731116));
#146070=CARTESIAN_POINT('Ctrl Pts',(67.056357246951,9.04431699425133,65.5438221960967));
#146071=CARTESIAN_POINT('Ctrl Pts',(67.0544223752917,9.05582913806265,65.5845248385036));
#146072=CARTESIAN_POINT('Ctrl Pts',(67.0525682421163,9.06686090218874,65.6235290376954));
#146073=CARTESIAN_POINT('Ctrl Pts',(67.0522711608951,9.07606503075263,65.6631282571404));
#146074=CARTESIAN_POINT('Ctrl Pts',(67.0535320899779,9.08337060870084,65.703004933018));
#146075=CARTESIAN_POINT('Ctrl Pts',(67.0538320909252,9.08510875586153,65.7124924138779));
#146076=CARTESIAN_POINT('Ctrl Pts',(67.0542201467146,9.08673958372169,65.7219954934958));
#146077=CARTESIAN_POINT('Ctrl Pts',(67.0546960008595,9.08826243435977,65.7315097040137));
#146078=CARTESIAN_POINT('Origin',(74.0770084968991,1.4210854715202E-14,
64.696310494594));
#146079=CARTESIAN_POINT('Origin',(74.0422787428291,1.4210854715202E-14,
64.499348271719));
#146080=CARTESIAN_POINT('Origin',(81.2702407042791,7.61327378225101,63.427949577933));
#146081=CARTESIAN_POINT('Origin',(82.9402782740091,9.38083151964701,63.133476895592));
#146082=CARTESIAN_POINT('Ctrl Pts',(83.2590337349668,6.9829169115756,62.061845095692));
#146083=CARTESIAN_POINT('Ctrl Pts',(83.2524681440442,7.01494834582241,62.0630028256722));
#146084=CARTESIAN_POINT('Ctrl Pts',(83.2460602430039,7.04755385579359,62.0657666515928));
#146085=CARTESIAN_POINT('Ctrl Pts',(83.2398870046894,7.08049337601265,62.0702775505784));
#146086=CARTESIAN_POINT('Ctrl Pts',(83.2337573121717,7.11320054206366,62.0747566298479));
#146087=CARTESIAN_POINT('Ctrl Pts',(83.2278591570096,7.14623651559213,62.080958589238));
#146088=CARTESIAN_POINT('Ctrl Pts',(83.2222654955408,7.17934027904419,62.0889773710341));
#146089=CARTESIAN_POINT('Ctrl Pts',(83.2167138008256,7.21219567968504,62.0969359914775));
#146090=CARTESIAN_POINT('Ctrl Pts',(83.2114622148937,7.24511726789558,62.1066845109911));
#146091=CARTESIAN_POINT('Ctrl Pts',(83.2065771533963,7.27783234147448,62.118266712207));
#146092=CARTESIAN_POINT('Ctrl Pts',(83.2053707477099,7.28591159509624,62.1211270310412));
#146093=CARTESIAN_POINT('Ctrl Pts',(83.2041866654247,7.29397819403508,62.1240989435197));
#146094=CARTESIAN_POINT('Ctrl Pts',(83.2030258423652,7.30202793164075,62.1271826320233));
#146095=CARTESIAN_POINT('Ctrl Pts',(83.19860460872,7.33268701481915,62.1389274946462));
#146096=CARTESIAN_POINT('Ctrl Pts',(83.1945222541898,7.36309703825039,62.1522961884262));
#146097=CARTESIAN_POINT('Ctrl Pts',(83.1908277125425,7.39300060942899,62.1672570785533));
#146098=CARTESIAN_POINT('Ctrl Pts',(83.1871429333242,7.42282516363598,62.1821784361368));
#146099=CARTESIAN_POINT('Ctrl Pts',(83.1838440400959,7.45214526961887,62.1986834628478));
#146100=CARTESIAN_POINT('Ctrl Pts',(83.1809688698346,7.48071466530648,62.2166909562356));
#146101=CARTESIAN_POINT('Ctrl Pts',(83.1780985493129,7.50923587110803,62.2346680751952));
#146102=CARTESIAN_POINT('Ctrl Pts',(83.1756506115634,7.53700825892937,62.2541423288748));
#146103=CARTESIAN_POINT('Ctrl Pts',(83.1736504501174,7.56380570618642,62.2749861383518));
#146104=CARTESIAN_POINT('Ctrl Pts',(83.1726807704526,7.57679712731737,62.2850912317322));
#146105=CARTESIAN_POINT('Ctrl Pts',(83.1718161401716,7.5895597503054,62.2955175369264));
#146106=CARTESIAN_POINT('Ctrl Pts',(83.1710583345944,7.60207007330836,62.3062468954608));
#146107=CARTESIAN_POINT('Ctrl Pts',(83.1694945364883,7.6278862193032,62.3283878654653));
#146108=CARTESIAN_POINT('Ctrl Pts',(83.1683868692723,7.65261988916478,62.3518166476268));
#146109=CARTESIAN_POINT('Ctrl Pts',(83.1677401427287,7.67609101314316,62.3763440729722));
#146110=CARTESIAN_POINT('Ctrl Pts',(83.1670929160326,7.69958028874797,62.4008904668451));
#146111=CARTESIAN_POINT('Ctrl Pts',(83.1669073340634,7.72180464093114,62.4265366428937));
#146112=CARTESIAN_POINT('Ctrl Pts',(83.1671743331004,7.74262337818449,62.4530620968364));
#146113=CARTESIAN_POINT('Ctrl Pts',(83.1674422460852,7.76351337877165,62.4796783484224));
#146114=CARTESIAN_POINT('Ctrl Pts',(83.168165798699,7.78298781481648,62.5071792800384));
#146115=CARTESIAN_POINT('Ctrl Pts',(83.1693222591529,7.80095017263617,62.5353199757027));
#146116=CARTESIAN_POINT('Ctrl Pts',(83.1698800666457,7.80961414185904,62.5488933675476));
#146117=CARTESIAN_POINT('Ctrl Pts',(83.1705383935998,7.81792703037044,62.5626153323347));
#146118=CARTESIAN_POINT('Ctrl Pts',(83.1712936299296,7.82588204732521,62.5764572343032));
#146119=CARTESIAN_POINT('Ctrl Pts',(83.1729608242511,7.84344285388512,62.6070134184412));
#146120=CARTESIAN_POINT('Ctrl Pts',(83.1751006289793,7.85925388829909,62.6381492155685));
#146121=CARTESIAN_POINT('Ctrl Pts',(83.17766709906,7.87330063587728,62.6695823984758));
#146122=CARTESIAN_POINT('Ctrl Pts',(83.1802465167818,7.88741824819954,62.701174159335));
#146123=CARTESIAN_POINT('Ctrl Pts',(83.1832567722595,7.89975384871325,62.7330656671778));
#146124=CARTESIAN_POINT('Ctrl Pts',(83.1866415987951,7.91034406890545,62.764977860896));
#146125=CARTESIAN_POINT('Ctrl Pts',(83.1900590807601,7.92103645923368,62.7971979304766));
#146126=CARTESIAN_POINT('Ctrl Pts',(83.193858237161,7.92994985743764,62.8294384796007));
#146127=CARTESIAN_POINT('Ctrl Pts',(83.1979736594296,7.93717160592385,62.8614294256434));
#146128=CARTESIAN_POINT('Ctrl Pts',(83.1989615480552,7.93890515420172,62.8691087085104));
#146129=CARTESIAN_POINT('Ctrl Pts',(83.1999676331307,7.94054143931416,62.8767737085479));
#146130=CARTESIAN_POINT('Ctrl Pts',(83.2009909626463,7.94208206232058,62.884420892197));
#146131=CARTESIAN_POINT('Ctrl Pts',(83.242348512759,6.67578265849103,62.10784857529));
#146132=CARTESIAN_POINT('Ctrl Pts',(83.334216228839,6.69096397737702,62.09800920288));
#146133=CARTESIAN_POINT('Ctrl Pts',(83.5256285431791,6.73684934210602,62.05584375918));
#146134=CARTESIAN_POINT('Ctrl Pts',(83.7924340751291,6.85036777994202,61.93083026476));
#146135=CARTESIAN_POINT('Ctrl Pts',(84.0221202772992,7.00517611130302,61.75968809345));
#146136=CARTESIAN_POINT('Ctrl Pts',(84.200186923649,7.18247783205801,61.57459024573));
#146137=CARTESIAN_POINT('Ctrl Pts',(84.2989069319091,7.32373971183602,61.43963697091));
#146138=CARTESIAN_POINT('Ctrl Pts',(84.3428871274891,7.40063711210602,61.37092003534));
#146139=CARTESIAN_POINT('Ctrl Pts',(84.3463939118291,7.40686952189903,61.36538012251));
#146140=CARTESIAN_POINT('Ctrl Pts',(83.0958792419792,7.42621601280802,61.89557920747));
#146141=CARTESIAN_POINT('Ctrl Pts',(83.1362882878291,7.43291182363202,61.89126897542));
#146142=CARTESIAN_POINT('Ctrl Pts',(83.2238974325991,7.45354780331802,61.87244519502));
#146143=CARTESIAN_POINT('Ctrl Pts',(83.3610746157191,7.51102643264402,61.8092817005701));
#146144=CARTESIAN_POINT('Ctrl Pts',(83.4921444347992,7.59854355671501,61.7124454520401));
#146145=CARTESIAN_POINT('Ctrl Pts',(83.6020881389591,7.70731505400102,61.59874227206));
#146146=CARTESIAN_POINT('Ctrl Pts',(83.6669013461292,7.79960598128501,61.51044916098));
#146147=CARTESIAN_POINT('Ctrl Pts',(83.6965467594992,7.85143798067902,61.46412926414));
#146148=CARTESIAN_POINT('Ctrl Pts',(83.6989158545292,7.85564850803701,61.46038646796));
#146149=CARTESIAN_POINT('Ctrl Pts',(83.0522723709792,8.02658218017502,62.41261250749));
#146150=CARTESIAN_POINT('Ctrl Pts',(83.1010403436091,8.03463924435402,62.40738738284));
#146151=CARTESIAN_POINT('Ctrl Pts',(83.2022866993591,8.05894910171303,62.38503344276));
#146152=CARTESIAN_POINT('Ctrl Pts',(83.3418023981191,8.11840394021002,62.31954363205));
#146153=CARTESIAN_POINT('Ctrl Pts',(83.4605211614992,8.198508337366,62.23099651645));
#146154=CARTESIAN_POINT('Ctrl Pts',(83.5516689143291,8.28933933996001,62.13618749888));
#146155=CARTESIAN_POINT('Ctrl Pts',(83.6017886106891,8.36110570925201,62.06763936861));
#146156=CARTESIAN_POINT('Ctrl Pts',(83.6240347796191,8.40000231746901,62.0328808413001));
#146157=CARTESIAN_POINT('Ctrl Pts',(83.6258080231391,8.40315379574102,62.03007954256));
#146158=CARTESIAN_POINT('Ctrl Pts',(83.1506552483792,7.93818769792802,63.195027498728));
#146159=CARTESIAN_POINT('Ctrl Pts',(83.2600994900291,7.95623135848103,63.183264358631));
#146160=CARTESIAN_POINT('Ctrl Pts',(83.480187110879,8.00984187819102,63.133675959378));
#146161=CARTESIAN_POINT('Ctrl Pts',(83.7519098984791,8.12751574075102,63.003770861248));
#146162=CARTESIAN_POINT('Ctrl Pts',(83.955625225199,8.266737144798,62.85005845822));
#146163=CARTESIAN_POINT('Ctrl Pts',(84.0941691519691,8.406314936159,62.704689841));
#146164=CARTESIAN_POINT('Ctrl Pts',(84.161992745499,8.50441931165102,62.61125483392));
#146165=CARTESIAN_POINT('Ctrl Pts',(84.1904143637091,8.55411713956403,62.56684828082));
#146166=CARTESIAN_POINT('Ctrl Pts',(84.1926682360992,8.55812266020902,62.56328807835));
#146167=CARTESIAN_POINT('',(83.867026488919,7.66994743046555,61.7007979888644));
#146168=CARTESIAN_POINT('Ctrl Pts',(83.2590342120925,6.98291585998354,62.0618450115583));
#146169=CARTESIAN_POINT('Ctrl Pts',(83.2985801165605,6.99966990543866,62.0548719917187));
#146170=CARTESIAN_POINT('Ctrl Pts',(83.3371733496626,7.01917008559866,62.0456086668951));
#146171=CARTESIAN_POINT('Ctrl Pts',(83.3745860713862,7.04141640046354,62.0343059151991));
#146172=CARTESIAN_POINT('Ctrl Pts',(83.4125223967804,7.06397406001513,62.0228449776774));
#146173=CARTESIAN_POINT('Ctrl Pts',(83.4492449461013,7.08935525832009,62.0092876911224));
#146174=CARTESIAN_POINT('Ctrl Pts',(83.4845685636801,7.11755999537844,61.9939086752094));
#146175=CARTESIAN_POINT('Ctrl Pts',(83.5206198762617,7.14634577276098,61.978212839169));
#146176=CARTESIAN_POINT('Ctrl Pts',(83.5552140688648,7.17807262153736,61.9606199922247));
#146177=CARTESIAN_POINT('Ctrl Pts',(83.5882081719665,7.21274054170755,61.9414270608567));
#146178=CARTESIAN_POINT('Ctrl Pts',(83.5958566796105,7.22077706422198,61.9369778633191));
#146179=CARTESIAN_POINT('Ctrl Pts',(83.603419423539,7.2289716337605,61.9324426815318));
#146180=CARTESIAN_POINT('Ctrl Pts',(83.6108950178491,7.2373242503231,61.9278252043225));
#146181=CARTESIAN_POINT('Ctrl Pts',(83.644056689583,7.27437638518764,61.9073421153394));
#146182=CARTESIAN_POINT('Ctrl Pts',(83.6754993164493,7.31453857244295,61.8852402508517));
#146183=CARTESIAN_POINT('Ctrl Pts',(83.7051350131012,7.35781081208902,61.8618372159296));
#146184=CARTESIAN_POINT('Ctrl Pts',(83.7361099877997,7.40303858398611,61.8373765655493));
#146185=CARTESIAN_POINT('Ctrl Pts',(83.7651110757759,7.45166385493483,61.8114950975671));
#146186=CARTESIAN_POINT('Ctrl Pts',(83.7920957448294,7.50368662493516,61.784540690884));
#146187=CARTESIAN_POINT('Ctrl Pts',(83.8190804138829,7.55570939493549,61.7575862842009));
#146188=CARTESIAN_POINT('Ctrl Pts',(83.8440491912441,7.61112966398742,61.7295593489844));
#146189=CARTESIAN_POINT('Ctrl Pts',(83.867011027257,7.66994743209099,61.7007856446916));
#146190=CARTESIAN_POINT('Ctrl Pts',(83.8670140452191,7.66994743515001,61.70078805062));
#146191=CARTESIAN_POINT('Ctrl Pts',(83.7214305777816,7.96200600407947,61.8832377455994));
#146192=CARTESIAN_POINT('Ctrl Pts',(83.7447899946214,8.21344901265172,62.1589320257208));
#146193=CARTESIAN_POINT('Ctrl Pts',(83.9303991623891,8.35407161789501,62.45142897117));
#146194=CARTESIAN_POINT('Ctrl Pts',(83.923859788829,7.37500816633501,61.67980641543));
#146195=CARTESIAN_POINT('Ctrl Pts',(83.9474802174891,7.38948776532201,61.65713017491));
#146196=CARTESIAN_POINT('Ctrl Pts',(84.0969682792491,7.48649501079001,61.50740188505));
#146197=CARTESIAN_POINT('Ctrl Pts',(84.3516500303791,7.72224899427102,61.17584896249));
#146198=CARTESIAN_POINT('Ctrl Pts',(84.6144842408191,8.16135276122401,60.63977389717));
#146199=CARTESIAN_POINT('Ctrl Pts',(84.7190477994991,8.56508431282901,60.20675032062));
#146200=CARTESIAN_POINT('Ctrl Pts',(84.7401260464792,8.81729927669401,59.95524756863));
#146201=CARTESIAN_POINT('Ctrl Pts',(84.7426394798291,8.86307976508602,59.91006480899));
#146202=CARTESIAN_POINT('Ctrl Pts',(83.5705122279591,7.87114698302502,61.85476420882));
#146203=CARTESIAN_POINT('Ctrl Pts',(83.5866454972991,7.88005369856502,61.83276215457));
#146204=CARTESIAN_POINT('Ctrl Pts',(83.6891686261191,7.94042075304802,61.6872892090601));
#146205=CARTESIAN_POINT('Ctrl Pts',(83.8676830517891,8.09595590885602,61.36311992254));
#146206=CARTESIAN_POINT('Ctrl Pts',(84.0543623951891,8.40203920228501,60.83553875239));
#146207=CARTESIAN_POINT('Ctrl Pts',(84.1282774583391,8.69307089532703,60.40662520731));
#146208=CARTESIAN_POINT('Ctrl Pts',(84.1420710017191,8.87760775573002,60.15662647416));
#146209=CARTESIAN_POINT('Ctrl Pts',(84.1436085530091,8.91117885085303,60.11169514057));
#146210=CARTESIAN_POINT('Ctrl Pts',(83.6270194382592,8.28666180430202,62.32998012357));
#146211=CARTESIAN_POINT('Ctrl Pts',(83.6393529195991,8.29846705592401,62.30586584266));
#146212=CARTESIAN_POINT('Ctrl Pts',(83.7156644082391,8.37619228209003,62.1476760354101));
#146213=CARTESIAN_POINT('Ctrl Pts',(83.8268510679491,8.54776921997102,61.8093361559901));
#146214=CARTESIAN_POINT('Ctrl Pts',(83.9072499723091,8.83518363827502,61.27924397807));
#146215=CARTESIAN_POINT('Ctrl Pts',(83.9054400779791,9.08060190236402,60.85810918613));
#146216=CARTESIAN_POINT('Ctrl Pts',(83.8814528874491,9.22856801730202,60.61571769384));
#146217=CARTESIAN_POINT('Ctrl Pts',(83.8764274466691,9.25527854442902,60.57228534855));
#146218=CARTESIAN_POINT('Ctrl Pts',(84.0561521783491,8.34779461768502,62.79236264607));
#146219=CARTESIAN_POINT('Ctrl Pts',(84.0708766974291,8.36906015182102,62.76474134613));
#146220=CARTESIAN_POINT('Ctrl Pts',(84.1589991300091,8.50670564499601,62.58524085521));
#146221=CARTESIAN_POINT('Ctrl Pts',(84.2560558454591,8.78001599820902,62.22051231515));
#146222=CARTESIAN_POINT('Ctrl Pts',(84.270070601449,9.175412951701,61.67855858024));
#146223=CARTESIAN_POINT('Ctrl Pts',(84.1973499601592,9.472356192965,61.26374630513));
#146224=CARTESIAN_POINT('Ctrl Pts',(84.1299774848391,9.63895321041302,61.030053317));
#146225=CARTESIAN_POINT('Ctrl Pts',(84.1171259072791,9.668672015192,60.98837992798));
#146226=CARTESIAN_POINT('',(84.0701935481991,9.38083151964701,60.90338912307));
#146227=CARTESIAN_POINT('Ctrl Pts',(83.867026488919,7.66994743046555,61.7007979888644));
#146228=CARTESIAN_POINT('Ctrl Pts',(83.884582223782,7.71471713563798,61.678837513214));
#146229=CARTESIAN_POINT('Ctrl Pts',(83.9016620036984,7.76247170792999,61.6555494980752));
#146230=CARTESIAN_POINT('Ctrl Pts',(83.9180456775371,7.81324485204552,61.6309189637823));
#146231=CARTESIAN_POINT('Ctrl Pts',(83.9330478039022,7.85973656882848,61.6083653905399));
#146232=CARTESIAN_POINT('Ctrl Pts',(83.9474668456226,7.90875951572417,61.584686124707));
#146233=CARTESIAN_POINT('Ctrl Pts',(83.9611283868236,7.96029842515161,61.5598856861656));
#146234=CARTESIAN_POINT('Ctrl Pts',(83.9654983093753,7.97678419636026,61.5519527601451));
#146235=CARTESIAN_POINT('Ctrl Pts',(83.9697906548141,7.99352703929664,61.5439052536026));
#146236=CARTESIAN_POINT('Ctrl Pts',(83.9739995139489,8.01052537813633,61.5357437222096));
#146237=CARTESIAN_POINT('Ctrl Pts',(83.9840684003346,8.05119063611737,61.5162188272922));
#146238=CARTESIAN_POINT('Ctrl Pts',(83.9936614914402,8.09332906917797,61.4960360616513));
#146239=CARTESIAN_POINT('Ctrl Pts',(84.0026899628803,8.13694385455923,61.4752245468069));
#146240=CARTESIAN_POINT('Ctrl Pts',(84.0078901294678,8.16206484554452,61.463237651257));
#146241=CARTESIAN_POINT('Ctrl Pts',(84.0129031535625,8.18767518208293,61.4510425428714));
#146242=CARTESIAN_POINT('Ctrl Pts',(84.0177140596479,8.21377418741589,61.4386368596428));
#146243=CARTESIAN_POINT('Ctrl Pts',(84.0242958335317,8.24948009159392,61.4216647133494));
#146244=CARTESIAN_POINT('Ctrl Pts',(84.0304965944768,8.28610154671648,61.404304876692));
#146245=CARTESIAN_POINT('Ctrl Pts',(84.0362709480598,8.32363855283814,61.3865709028769));
#146246=CARTESIAN_POINT('Ctrl Pts',(84.0391581248513,8.34240705589897,61.3777039159694));
#146247=CARTESIAN_POINT('Ctrl Pts',(84.0419387065085,8.36140444671648,61.3687434010195));
#146248=CARTESIAN_POINT('Ctrl Pts',(84.0446069334968,8.38063072531699,61.3596915411556));
#146249=CARTESIAN_POINT('Ctrl Pts',(84.045941046991,8.39024386461724,61.3551656112237));
#146250=CARTESIAN_POINT('Ctrl Pts',(84.0472470726545,8.3999142258631,61.3506168455892));
#146251=CARTESIAN_POINT('Ctrl Pts',(84.048524291865,8.40964180905692,61.3460455336731));
#146252=CARTESIAN_POINT('Ctrl Pts',(84.0491629014703,8.41450560065383,61.3437598777151));
#146253=CARTESIAN_POINT('Ctrl Pts',(84.0497943095174,8.41938369773772,61.3414685852175));
#146254=CARTESIAN_POINT('Ctrl Pts',(84.0504184260876,8.42427610030878,61.339171694199));
#146255=CARTESIAN_POINT('Ctrl Pts',(84.0510425426579,8.42916850287983,61.3368748031805));
#146256=CARTESIAN_POINT('Ctrl Pts',(84.0518355651505,8.43549793372503,61.3339050293409));
#146257=CARTESIAN_POINT('Ctrl Pts',(84.0522688115884,8.43899622448362,61.3322642642359));
#146258=CARTESIAN_POINT('Ctrl Pts',(84.0573240123512,8.47981493772962,61.3131195089983));
#146259=CARTESIAN_POINT('Ctrl Pts',(84.0621702402961,8.52350054174341,61.2924539443833));
#146260=CARTESIAN_POINT('Ctrl Pts',(84.0665105235108,8.57016855648445,61.2704338298668));
#146261=CARTESIAN_POINT('Ctrl Pts',(84.0704464936509,8.61248927691592,61.2504649686352));
#146262=CARTESIAN_POINT('Ctrl Pts',(84.0739658923583,8.65726283209245,61.2293828862379));
#146263=CARTESIAN_POINT('Ctrl Pts',(84.0768640731261,8.7045331478027,61.2073213444561));
#146264=CARTESIAN_POINT('Ctrl Pts',(84.0771617817812,8.7093888773934,61.2050551255905));
#146265=CARTESIAN_POINT('Ctrl Pts',(84.077452954973,8.71427091126197,61.2027785750419));
#146266=CARTESIAN_POINT('Ctrl Pts',(84.0777373852218,8.71917926764842,61.2004918392959));
#146267=CARTESIAN_POINT('Ctrl Pts',(84.0804044531795,8.76520433036884,61.1790493954613));
#146268=CARTESIAN_POINT('Ctrl Pts',(84.0824780972373,8.81354674953817,61.1567137657027));
#146269=CARTESIAN_POINT('Ctrl Pts',(84.0837834793078,8.8642306082537,61.1335396096708));
#146270=CARTESIAN_POINT('Ctrl Pts',(84.0850466303684,8.91327477036905,61.1111151713166));
#146271=CARTESIAN_POINT('Ctrl Pts',(84.0855909918429,8.96451147248083,61.087905989582));
#146272=CARTESIAN_POINT('Ctrl Pts',(84.0852600172611,9.01792742128314,61.0639311405896));
#146273=CARTESIAN_POINT('Ctrl Pts',(84.0849366685859,9.07011262592673,61.0405086903847));
#146274=CARTESIAN_POINT('Ctrl Pts',(84.0837786226198,9.12437776788739,61.0163556535295));
#146275=CARTESIAN_POINT('Ctrl Pts',(84.0816318863806,9.18067552376136,60.9914557007812));
#146276=CARTESIAN_POINT('Ctrl Pts',(84.0795194919131,9.23607267310616,60.9669540775874));
#146277=CARTESIAN_POINT('Ctrl Pts',(84.0764506397482,9.29343763867521,60.9417291457114));
#146278=CARTESIAN_POINT('Ctrl Pts',(84.072258679203,9.35269346002768,60.9157310279044));
#146279=CARTESIAN_POINT('Ctrl Pts',(84.0715984568464,9.36202609033123,60.911636395233));
#146280=CARTESIAN_POINT('Ctrl Pts',(84.0709103193938,9.37140556504035,60.9075225163887));
#146281=CARTESIAN_POINT('Ctrl Pts',(84.070193548197,9.38083151964701,60.9033891230704));
#146282=CARTESIAN_POINT('Ctrl Pts',(83.9304072607132,8.35406389118647,62.4514275465134));
#146283=CARTESIAN_POINT('Ctrl Pts',(83.9919651482484,8.44374030577409,62.3149821809302));
#146284=CARTESIAN_POINT('Ctrl Pts',(84.0355872880004,8.53794851523683,62.1709248993271));
#146285=CARTESIAN_POINT('Ctrl Pts',(84.0658026794286,8.63442789447643,62.0238615241773));
#146286=CARTESIAN_POINT('Ctrl Pts',(84.0883721371628,8.7064933938474,61.9140121900202));
#146287=CARTESIAN_POINT('Ctrl Pts',(84.1034614695384,8.77982608633684,61.802485617024));
#146288=CARTESIAN_POINT('Ctrl Pts',(84.111900980885,8.85387175171245,61.6903694643091));
#146289=CARTESIAN_POINT('Ctrl Pts',(84.1168352776888,8.89716374753911,61.6248189423331));
#146290=CARTESIAN_POINT('Ctrl Pts',(84.119496399077,8.94069937035746,61.5590669038891));
#146291=CARTESIAN_POINT('Ctrl Pts',(84.1200502816288,8.98436778258147,61.4933307421339));
#146292=CARTESIAN_POINT('Ctrl Pts',(84.121712032341,9.11538114432835,61.2961100258022));
#146293=CARTESIAN_POINT('Ctrl Pts',(84.1044062545909,9.24758975113299,61.0990322197026));
#146294=CARTESIAN_POINT('Ctrl Pts',(84.070193548197,9.38083151964701,60.9033891230704));
#146295=CARTESIAN_POINT('Origin',(82.9247768442291,9.38083151964701,63.045563918654));
#146296=CARTESIAN_POINT('',(84.0701935481991,9.38083151964701,60.90338912307));
#146297=CARTESIAN_POINT('Origin',(84.5911380811991,111.0724296188,63.857812382104));
#146298=CARTESIAN_POINT('',(84.330665814698,13.1050084134069,62.3806007525954));
#146299=CARTESIAN_POINT('',(84.3306658146991,13.10501209624,62.3806007526));
#146300=CARTESIAN_POINT('',(84.0366017122669,11.5683493747171,60.7128624132734));
#146301=CARTESIAN_POINT('Ctrl Pts',(84.3306655653021,13.105011407238,62.3805993381869));
#146302=CARTESIAN_POINT('Ctrl Pts',(84.2899365191375,12.9924913368189,62.149613439143));
#146303=CARTESIAN_POINT('Ctrl Pts',(84.251904294216,12.8600934104913,61.9339219733862));
#146304=CARTESIAN_POINT('Ctrl Pts',(84.2161389657171,12.7062180549234,61.731086716098));
#146305=CARTESIAN_POINT('Ctrl Pts',(84.1803735642168,12.5523423852767,61.5282510447979));
#146306=CARTESIAN_POINT('Ctrl Pts',(84.1468750683932,12.3769891987133,61.3382716344487));
#146307=CARTESIAN_POINT('Ctrl Pts',(84.1167829985401,12.1867580683441,61.1676110257763));
#146308=CARTESIAN_POINT('Ctrl Pts',(84.086690928687,11.996526937975,60.996950417104));
#146309=CARTESIAN_POINT('Ctrl Pts',(84.0600052848046,11.7914178638,60.8456086101085));
#146310=CARTESIAN_POINT('Ctrl Pts',(84.0365986439827,11.56834937513,60.7128629535571));
#146311=CARTESIAN_POINT('',(83.740534258072,9.21680318446827,59.0338374816974));
#146312=CARTESIAN_POINT('Ctrl Pts',(84.0366011831691,11.56834937513,60.71286250583));
#146313=CARTESIAN_POINT('Ctrl Pts',(84.0167422397526,11.3787529588475,60.6002516892439));
#146314=CARTESIAN_POINT('Ctrl Pts',(83.9799695099432,11.0446386484641,60.3917031752184));
#146315=CARTESIAN_POINT('Ctrl Pts',(83.9396547409223,10.7064633197752,60.1630667586076));
#146316=CARTESIAN_POINT('Ctrl Pts',(83.9157502918788,10.5122257397148,60.0274978913397));
#146317=CARTESIAN_POINT('Ctrl Pts',(83.9098596338177,10.4648391987288,59.9940903093718));
#146318=CARTESIAN_POINT('Ctrl Pts',(83.8533537997807,10.0150112533668,59.6736298000958));
#146319=CARTESIAN_POINT('Ctrl Pts',(83.7990070452368,9.6156595428362,59.3654140390955));
#146320=CARTESIAN_POINT('Ctrl Pts',(83.7405348394891,9.21680318431901,59.03383737954));
#146321=CARTESIAN_POINT('',(83.6360715663934,8.5371408778779,58.4413608714745));
#146322=CARTESIAN_POINT('Ctrl Pts',(83.740540996078,9.21680318437712,59.0338362937156));
#146323=CARTESIAN_POINT('Ctrl Pts',(83.727194557133,9.12572250911644,58.9581448314892));
#146324=CARTESIAN_POINT('Ctrl Pts',(83.7136768037681,9.0352116665213,58.8814821806832));
#146325=CARTESIAN_POINT('Ctrl Pts',(83.6999874765571,8.94527466677724,58.8038461597189));
#146326=CARTESIAN_POINT('Ctrl Pts',(83.6963779326866,8.92156045926676,58.7833754222396));
#146327=CARTESIAN_POINT('Ctrl Pts',(83.6927564621468,8.89788616303864,58.7628370117057));
#146328=CARTESIAN_POINT('Ctrl Pts',(83.6891230432056,8.87425175631427,58.7422308289417));
#146329=CARTESIAN_POINT('Ctrl Pts',(83.6717100607189,8.76098501855649,58.6434767063383));
#146330=CARTESIAN_POINT('Ctrl Pts',(83.6540227449861,8.64863571554548,58.5431668919965));
#146331=CARTESIAN_POINT('Ctrl Pts',(83.6360740268018,8.5371330073123,58.4413748701116));
#146332=CARTESIAN_POINT('',(83.6360659838734,-8.53719636731526,58.4413293403224));
#146333=CARTESIAN_POINT('',(83.6360730593091,8.53712703774001,58.44136942158));
#146334=CARTESIAN_POINT('',(83.7405267536393,-9.2167985425004,59.0338347984847));
#146335=CARTESIAN_POINT('Ctrl Pts',(83.6360729920622,-8.53720311761702,
58.4413691055294));
#146336=CARTESIAN_POINT('Ctrl Pts',(83.6540184616861,-8.64860998521598,
58.5431429211518));
#146337=CARTESIAN_POINT('Ctrl Pts',(83.6717001000893,-8.76092172492552,
58.6434204755692));
#146338=CARTESIAN_POINT('Ctrl Pts',(83.6891112932783,-8.874175396646,58.7421642589597));
#146339=CARTESIAN_POINT('Ctrl Pts',(83.7065246051586,-8.98744284970651,
58.8409200580459));
#146340=CARTESIAN_POINT('Ctrl Pts',(83.7236674060021,-9.101652464031,58.9381417128067));
#146341=CARTESIAN_POINT('Ctrl Pts',(83.7405402591061,-9.21679854220001,
59.0338324178608));
#146342=CARTESIAN_POINT('',(84.0366041203994,-11.56837406741,60.7128837058028));
#146343=CARTESIAN_POINT('Ctrl Pts',(83.7405343424891,-9.21679854219999,
59.03383346112));
#146344=CARTESIAN_POINT('Ctrl Pts',(83.7697426624094,-9.41601561043767,
59.1994474768037));
#146345=CARTESIAN_POINT('Ctrl Pts',(83.8190639716081,-9.76498641488459,
59.4791625209821));
#146346=CARTESIAN_POINT('Ctrl Pts',(83.8652652117883,-10.1145538556358,
59.7411827744601));
#146347=CARTESIAN_POINT('Ctrl Pts',(83.8909018219276,-10.3144527939354,
59.8865752154596));
#146348=CARTESIAN_POINT('Ctrl Pts',(83.8974093805898,-10.365729764731,59.923481414591));
#146349=CARTESIAN_POINT('Ctrl Pts',(83.9524868765521,-10.8041110086998,
60.2358414161119));
#146350=CARTESIAN_POINT('Ctrl Pts',(83.9968446284176,-11.1887561005569,
60.4874067278259));
#146351=CARTESIAN_POINT('Ctrl Pts',(84.0366050016191,-11.56837406741,60.71288355042));
#146352=CARTESIAN_POINT('',(84.330665789694,-13.1050131369444,62.3806006107895));
#146353=CARTESIAN_POINT('Ctrl Pts',(84.0366023579599,-11.56837406741,60.7128840165684));
#146354=CARTESIAN_POINT('Ctrl Pts',(84.0600599759165,-11.79192430949,60.8459187788173));
#146355=CARTESIAN_POINT('Ctrl Pts',(84.0867960216265,-11.99729070149,60.9975464287807));
#146356=CARTESIAN_POINT('Ctrl Pts',(84.1169120167458,-12.1875766534583,
61.1683427243805));
#146357=CARTESIAN_POINT('Ctrl Pts',(84.1470280118651,-12.3778626054267,
61.3391390199804));
#146358=CARTESIAN_POINT('Ctrl Pts',(84.1805239563937,-12.5530681173634,
61.5291039612167));
#146359=CARTESIAN_POINT('Ctrl Pts',(84.216268215619,-12.7067726588867,61.7318197287167));
#146360=CARTESIAN_POINT('Ctrl Pts',(84.2520124748443,-12.86047720041,61.9345354962168));
#146361=CARTESIAN_POINT('Ctrl Pts',(84.2900050487662,-12.99268077152,62.1500020899805));
#146362=CARTESIAN_POINT('Ctrl Pts',(84.3306658146978,-13.10501209624,62.3806007525802));
#146363=CARTESIAN_POINT('',(84.3306658146583,-9.38083151966199,62.3806007523748));
#146364=CARTESIAN_POINT('',(84.3306658146191,-9.38083151966199,62.38060075216));
#146365=CARTESIAN_POINT('',(84.0701935481991,-9.38083151964699,60.90338912307));
#146366=CARTESIAN_POINT('',(84.3306658146191,-9.38083151966199,62.38060075216));
#146367=CARTESIAN_POINT('',(84.0701935481991,-9.38083151964699,60.90338912307));
#146368=CARTESIAN_POINT('Origin',(83.0853857951891,-11.87956405717,61.07703730073));
#146369=CARTESIAN_POINT('',(83.8670110335795,-7.66994744389929,61.7007856367688));
#146370=CARTESIAN_POINT('Ctrl Pts',(83.8670110335795,-7.66994744389929,
61.7007856367688));
#146371=CARTESIAN_POINT('Ctrl Pts',(83.8877308381727,-7.72304817206258,
61.67482144373));
#146372=CARTESIAN_POINT('Ctrl Pts',(83.9066801507776,-7.77708798385845,
61.648427071772));
#146373=CARTESIAN_POINT('Ctrl Pts',(83.9239978184073,-7.83191890481131,
61.6217664761134));
#146374=CARTESIAN_POINT('Ctrl Pts',(83.942232338449,-7.88965274913706,61.593694383713));
#146375=CARTESIAN_POINT('Ctrl Pts',(83.9586585766351,-7.94826368775387,
61.5653269014276));
#146376=CARTESIAN_POINT('Ctrl Pts',(83.9734288711074,-8.00757897719989,
61.5367975592492));
#146377=CARTESIAN_POINT('Ctrl Pts',(83.9886134799562,-8.06855809110232,
61.5074679543107));
#146378=CARTESIAN_POINT('Ctrl Pts',(84.0020485456467,-8.13028162484728,
61.477966711392));
#146379=CARTESIAN_POINT('Ctrl Pts',(84.0138793093052,-8.19256188677082,
61.4483859162442));
#146380=CARTESIAN_POINT('Ctrl Pts',(84.0261862036942,-8.25734862650568,
61.4176146378776));
#146381=CARTESIAN_POINT('Ctrl Pts',(84.0367576686922,-8.32273780734182,
61.3867566809908));
#146382=CARTESIAN_POINT('Ctrl Pts',(84.045726040153,-8.388518152353,61.3558680987108));
#146383=CARTESIAN_POINT('Ctrl Pts',(84.0509005473253,-8.42647162791296,
61.3380462242216));
#146384=CARTESIAN_POINT('Ctrl Pts',(84.0555407617356,-8.46455532113187,
61.3202133320056));
#146385=CARTESIAN_POINT('Ctrl Pts',(84.0596665974345,-8.5027286514264,61.3023746442309));
#146386=CARTESIAN_POINT('Ctrl Pts',(84.0679871904554,-8.57971299322025,
61.2663992754013));
#146387=CARTESIAN_POINT('Ctrl Pts',(84.0742039804002,-8.65709134161381,
61.2304615370746));
#146388=CARTESIAN_POINT('Ctrl Pts',(84.078445246042,-8.73478433456591,61.1946507654007));
#146389=CARTESIAN_POINT('Ctrl Pts',(84.0827823726163,-8.81423334173372,
61.1580305999612));
#146390=CARTESIAN_POINT('Ctrl Pts',(84.0850540629707,-8.89401137736572,
61.1215421469891));
#146391=CARTESIAN_POINT('Ctrl Pts',(84.0853520837786,-8.97403357566445,
61.0852483715776));
#146392=CARTESIAN_POINT('Ctrl Pts',(84.0856564729272,-9.05576575058707,
61.0481790425214));
#146393=CARTESIAN_POINT('Ctrl Pts',(84.0839021793659,-9.13775263458298,
61.0113116213905));
#146394=CARTESIAN_POINT('Ctrl Pts',(84.0801352228852,-9.21990380433592,
60.9746968097292));
#146395=CARTESIAN_POINT('Ctrl Pts',(84.0776783196428,-9.27348485215759,
60.95081571369));
#146396=CARTESIAN_POINT('Ctrl Pts',(84.0743641506513,-9.32713578672443,
60.9270417849153));
#146397=CARTESIAN_POINT('Ctrl Pts',(84.0701935482024,-9.38083151964699,
60.9033891230694));
#146398=CARTESIAN_POINT('Ctrl Pts',(83.2590363734724,-6.9829160281516,62.0618549710651));
#146399=CARTESIAN_POINT('Ctrl Pts',(83.282289361152,-6.99276570574769,62.0577559880571));
#146400=CARTESIAN_POINT('Ctrl Pts',(83.3067925291477,-7.00454606434442,
62.0525868755333));
#146401=CARTESIAN_POINT('Ctrl Pts',(83.3323113975882,-7.01851063662673,
62.046084087642));
#146402=CARTESIAN_POINT('Ctrl Pts',(83.3578302660286,-7.03247520890904,
62.0395812997506));
#146403=CARTESIAN_POINT('Ctrl Pts',(83.3843643714203,-7.0486240708107,62.0317442661474));
#146404=CARTESIAN_POINT('Ctrl Pts',(83.4116337788324,-7.06724343137114,
62.0223229982725));
#146405=CARTESIAN_POINT('Ctrl Pts',(83.436142258631,-7.08397764987694,62.0138555992601));
#146406=CARTESIAN_POINT('Ctrl Pts',(83.4612451921201,-7.10270815720052,
62.0041068565072));
#146407=CARTESIAN_POINT('Ctrl Pts',(83.4866821771397,-7.12365747172556,
61.9929546294659));
#146408=CARTESIAN_POINT('Ctrl Pts',(83.5121191621594,-7.14460678625059,
61.9818024024245));
#146409=CARTESIAN_POINT('Ctrl Pts',(83.5378901428163,-7.16777501729968,
61.9692463862192));
#146410=CARTESIAN_POINT('Ctrl Pts',(83.5636960707018,-7.19340099565594,
61.9552021971918));
#146411=CARTESIAN_POINT('Ctrl Pts',(83.5864308247299,-7.21597721602059,
61.9428294127494));
#146412=CARTESIAN_POINT('Ctrl Pts',(83.6091922328673,-7.24046130049242,
61.9293019787599));
#146413=CARTESIAN_POINT('Ctrl Pts',(83.6317511913142,-7.26702562691842,
61.9145891050788));
#146414=CARTESIAN_POINT('Ctrl Pts',(83.6541863104381,-7.29344412621307,
61.8999569989702));
#146415=CARTESIAN_POINT('Ctrl Pts',(83.6764207471435,-7.32192008762135,
61.8841506374782));
#146416=CARTESIAN_POINT('Ctrl Pts',(83.6982293579439,-7.35263870495623,
61.8672313618185));
#146417=CARTESIAN_POINT('Ctrl Pts',(83.7195548675035,-7.38267684785449,
61.8506868795439));
#146418=CARTESIAN_POINT('Ctrl Pts',(83.7404731816077,-7.41485975670852,
61.8330781446068));
#146419=CARTESIAN_POINT('Ctrl Pts',(83.7607573278311,-7.44936440703707,
61.8145090737762));
#146420=CARTESIAN_POINT('Ctrl Pts',(83.7696671104134,-7.46452052596472,
61.806352635638));
#146421=CARTESIAN_POINT('Ctrl Pts',(83.778454322578,-7.48012461781848,61.7980115321834));
#146422=CARTESIAN_POINT('Ctrl Pts',(83.7870987073549,-7.49619158640237,
61.7894976170954));
#146423=CARTESIAN_POINT('Ctrl Pts',(83.8052065587327,-7.5298479178492,61.7716630674965));
#146424=CARTESIAN_POINT('Ctrl Pts',(83.8226877130566,-7.56553553137317,
61.7530667791856));
#146425=CARTESIAN_POINT('Ctrl Pts',(83.8393888914259,-7.60341084157583,
61.7338939949398));
#146426=CARTESIAN_POINT('Ctrl Pts',(83.8488547931309,-7.62487782764677,
61.7230272352976));
#146427=CARTESIAN_POINT('Ctrl Pts',(83.8580700758562,-7.64704755743563,
61.7119761780314));
#146428=CARTESIAN_POINT('Ctrl Pts',(83.8670064350194,-7.669947443743,61.7007819662909));
#146429=CARTESIAN_POINT('Ctrl Pts',(83.1513105236491,-7.93829473335598,
63.194966112929));
#146430=CARTESIAN_POINT('Ctrl Pts',(83.264872395859,-7.957053728333,63.182689563492));
#146431=CARTESIAN_POINT('Ctrl Pts',(83.5018558838091,-8.01558777810299,
63.1281192597161));
#146432=CARTESIAN_POINT('Ctrl Pts',(83.793035941679,-8.14822056533799,62.98049002751));
#146433=CARTESIAN_POINT('Ctrl Pts',(84.007518739009,-8.31001055232898,62.80322092744));
#146434=CARTESIAN_POINT('Ctrl Pts',(84.1262881301092,-8.44906746979797,
62.6628219159601));
#146435=CARTESIAN_POINT('Ctrl Pts',(84.1780214029591,-8.53201891951698,
62.5865012713));
#146436=CARTESIAN_POINT('Ctrl Pts',(84.1930532967891,-8.55878077391199,
62.56272764659));
#146437=CARTESIAN_POINT('Ctrl Pts',(83.0525582468391,-8.02666120745799,
62.41257219589));
#146438=CARTESIAN_POINT('Ctrl Pts',(83.1031659906391,-8.03504796986499,
62.40712679656));
#146439=CARTESIAN_POINT('Ctrl Pts',(83.2123457583091,-8.06157435232,62.38250638988));
#146440=CARTESIAN_POINT('Ctrl Pts',(83.3637640416291,-8.12919594766799,
62.30742514836));
#146441=CARTESIAN_POINT('Ctrl Pts',(83.4927183665891,-8.22488484773499,
62.20236174747));
#146442=CARTESIAN_POINT('Ctrl Pts',(83.5748180822491,-8.31962531502999,
62.1063728352201));
#146443=CARTESIAN_POINT('Ctrl Pts',(83.6142389534991,-8.38260961938299,
62.04833795058));
#146444=CARTESIAN_POINT('Ctrl Pts',(83.6260728217892,-8.40367762948599,
62.02962298588));
#146445=CARTESIAN_POINT('Ctrl Pts',(83.0961181729091,-7.42626321265199,
61.89553186311));
#146446=CARTESIAN_POINT('Ctrl Pts',(83.1380603031291,-7.43324549126899,
61.89104875086));
#146447=CARTESIAN_POINT('Ctrl Pts',(83.2327226191091,-7.45574602055999,
61.8702911395001));
#146448=CARTESIAN_POINT('Ctrl Pts',(83.3835527426891,-7.52175173551999,
61.79719441311));
#146449=CARTESIAN_POINT('Ctrl Pts',(83.5294730142391,-7.62865565051299,
61.67962372064));
#146450=CARTESIAN_POINT('Ctrl Pts',(83.6316464408291,-7.74551728364799,
61.56096647174));
#146451=CARTESIAN_POINT('Ctrl Pts',(83.6834667115091,-7.82815871933699,
61.48476057679));
#146452=CARTESIAN_POINT('Ctrl Pts',(83.6992824959991,-7.85631560981899,
61.45974886626));
#146453=CARTESIAN_POINT('Ctrl Pts',(83.2429027023891,-6.67585548217199,
62.10780057242));
#146454=CARTESIAN_POINT('Ctrl Pts',(83.3382436431191,-6.69166131028399,
62.09754739579));
#146455=CARTESIAN_POINT('Ctrl Pts',(83.544701711279,-6.74173031670498,62.05109927843));
#146456=CARTESIAN_POINT('Ctrl Pts',(83.8346450628892,-6.87096543964799,
61.90764282796));
#146457=CARTESIAN_POINT('Ctrl Pts',(84.0848016584592,-7.05633690953499,
61.7040750128));
#146458=CARTESIAN_POINT('Ctrl Pts',(84.2457794526591,-7.24190735349899,
61.51601195481));
#146459=CARTESIAN_POINT('Ctrl Pts',(84.3235845789591,-7.36619127664198,
61.4014836598));
#146460=CARTESIAN_POINT('Ctrl Pts',(84.3469891311591,-7.40785871185899,
61.36447005234));
#146461=CARTESIAN_POINT('',(83.2009909607981,-7.94208206191376,62.8844208924415));
#146462=CARTESIAN_POINT('Ctrl Pts',(83.2009862869082,-7.94210140073919,
62.8844176222466));
#146463=CARTESIAN_POINT('Ctrl Pts',(83.1968609444218,-7.93589258748885,
62.8535949750669));
#146464=CARTESIAN_POINT('Ctrl Pts',(83.1930177536416,-7.92812896197403,
62.8224913291405));
#146465=CARTESIAN_POINT('Ctrl Pts',(83.1895151218238,-7.91871788470194,
62.791331832236));
#146466=CARTESIAN_POINT('Ctrl Pts',(83.1860613434666,-7.90943806978235,
62.7606069368919));
#146467=CARTESIAN_POINT('Ctrl Pts',(83.1829389107385,-7.8985558891018,62.7298283228265));
#146468=CARTESIAN_POINT('Ctrl Pts',(83.1802003270392,-7.88602364173719,
62.6992405351296));
#146469=CARTESIAN_POINT('Ctrl Pts',(83.1775058788668,-7.87369336641399,
62.6691457059375));
#146470=CARTESIAN_POINT('Ctrl Pts',(83.1751832107692,-7.85976544420628,
62.6392363428651));
#146471=CARTESIAN_POINT('Ctrl Pts',(83.1732757839844,-7.84424106305769,
62.6097634807669));
#146472=CARTESIAN_POINT('Ctrl Pts',(83.1725527987444,-7.83835674890296,
62.5985921768699));
#146473=CARTESIAN_POINT('Ctrl Pts',(83.1718893871919,-7.83224358151196,
62.5874837139982));
#146474=CARTESIAN_POINT('Ctrl Pts',(83.1712875738902,-7.82590353889161,
62.5764520960335));
#146475=CARTESIAN_POINT('Ctrl Pts',(83.1697259221037,-7.80945169434663,
62.5478260323457));
#146476=CARTESIAN_POINT('Ctrl Pts',(83.1685797522826,-7.79146864491412,
62.5197178703259));
#146477=CARTESIAN_POINT('Ctrl Pts',(83.1678774334007,-7.77202362631577,
62.4923718004139));
#146478=CARTESIAN_POINT('Ctrl Pts',(83.1671796572841,-7.7527043827144,62.4652026113747));
#146479=CARTESIAN_POINT('Ctrl Pts',(83.1669201223469,-7.73194218273304,
62.438786525598));
#146480=CARTESIAN_POINT('Ctrl Pts',(83.1671144478248,-7.70985343530854,
62.4133520640267));
#146481=CARTESIAN_POINT('Ctrl Pts',(83.1673079982892,-7.68785278275714,
62.3880190407859));
#146482=CARTESIAN_POINT('Ctrl Pts',(83.1679518517265,-7.66453652820068,
62.3636606057523));
#146483=CARTESIAN_POINT('Ctrl Pts',(83.1690480192404,-7.64006390061212,
62.3404795080263));
#146484=CARTESIAN_POINT('Ctrl Pts',(83.1701512360192,-7.61543389376028,
62.3171493366436));
#146485=CARTESIAN_POINT('Ctrl Pts',(83.1717126130741,-7.58963314283984,
62.2950124109263));
#146486=CARTESIAN_POINT('Ctrl Pts',(83.1737200409363,-7.56286188520676,
62.274240623076));
#146487=CARTESIAN_POINT('Ctrl Pts',(83.1757178816941,-7.53621848215234,
62.2535680374456));
#146488=CARTESIAN_POINT('Ctrl Pts',(83.1781574363581,-7.50861459563722,
62.2342480221177));
#146489=CARTESIAN_POINT('Ctrl Pts',(83.1810134084009,-7.48027493168117,
62.216407035279));
#146490=CARTESIAN_POINT('Ctrl Pts',(83.1838931323914,-7.4516995783667,62.1984176722723));
#146491=CARTESIAN_POINT('Ctrl Pts',(83.1871961048047,-7.4223769946218,62.1819323415515));
#146492=CARTESIAN_POINT('Ctrl Pts',(83.1908843299669,-7.39255325226539,
62.1670311076611));
#146493=CARTESIAN_POINT('Ctrl Pts',(83.1945643726918,-7.36279567476835,
62.1521629326013));
#146494=CARTESIAN_POINT('Ctrl Pts',(83.1986277702836,-7.33254001686404,
62.1388717827871));
#146495=CARTESIAN_POINT('Ctrl Pts',(83.2030272346504,-7.30203343974707,
62.1271862973236));
#146496=CARTESIAN_POINT('Ctrl Pts',(83.2075236494605,-7.27085459302483,
62.1152433002858));
#146497=CARTESIAN_POINT('Ctrl Pts',(83.2123707521351,-7.23941441702322,
62.1049774188593));
#146498=CARTESIAN_POINT('Ctrl Pts',(83.217510289309,-7.20796636671036,62.096367038009));
#146499=CARTESIAN_POINT('Ctrl Pts',(83.2227040839583,-7.17618632311442,
62.0876657584042));
#146500=CARTESIAN_POINT('Ctrl Pts',(83.2281962897528,-7.14439897464933,
62.0806546693344));
#146501=CARTESIAN_POINT('Ctrl Pts',(83.2339228693355,-7.11284321740108,
62.0752629920924));
#146502=CARTESIAN_POINT('Ctrl Pts',(83.2397622659586,-7.08066579287576,
62.0697650955865));
#146503=CARTESIAN_POINT('Ctrl Pts',(83.245845131012,-7.04872979197433,62.0659504563783));
#146504=CARTESIAN_POINT('Ctrl Pts',(83.2521030588475,-7.01725456501231,
62.0637017729808));
#146505=CARTESIAN_POINT('Ctrl Pts',(83.2543914510472,-7.00574473847601,
62.0628794768979));
#146506=CARTESIAN_POINT('Ctrl Pts',(83.2567032652368,-6.99429616000662,
62.062266226382));
#146507=CARTESIAN_POINT('Ctrl Pts',(83.2590352295789,-6.98291823983333,
62.0618551727003));
#146508=CARTESIAN_POINT('',(83.9305070695251,-8.35425122912034,62.451223254077));
#146509=CARTESIAN_POINT('Ctrl Pts',(83.9304978963085,-8.3542226563704,62.4512190361288));
#146510=CARTESIAN_POINT('Ctrl Pts',(83.9171890192848,-8.34413946079924,
62.4302377284297));
#146511=CARTESIAN_POINT('Ctrl Pts',(83.9042062657205,-8.33297575049901,
62.4084312846382));
#146512=CARTESIAN_POINT('Ctrl Pts',(83.8917600544071,-8.32062588453196,
62.3858523588766));
#146513=CARTESIAN_POINT('Ctrl Pts',(83.8797850045273,-8.30874353276729,
62.3641281766803));
#146514=CARTESIAN_POINT('Ctrl Pts',(83.8683071406987,-8.29576258438283,
62.3416887413461));
#146515=CARTESIAN_POINT('Ctrl Pts',(83.8575356795425,-8.28160799316187,
62.3186183448306));
#146516=CARTESIAN_POINT('Ctrl Pts',(83.8480119751002,-8.26909305750599,
62.2982204030292));
#146517=CARTESIAN_POINT('Ctrl Pts',(83.8390410731563,-8.2556605856278,62.2773296366975));
#146518=CARTESIAN_POINT('Ctrl Pts',(83.8307772578393,-8.24127725732503,
62.2560312206357));
#146519=CARTESIAN_POINT('Ctrl Pts',(83.82186485708,-8.22576505367934,62.2330611986542));
#146520=CARTESIAN_POINT('Ctrl Pts',(83.8137756270682,-8.20914632687142,
62.2096168110415));
#146521=CARTESIAN_POINT('Ctrl Pts',(83.8067059121274,-8.19140860833201,
62.185842001208));
#146522=CARTESIAN_POINT('Ctrl Pts',(83.8029369618848,-8.1819524167948,62.1731673635399));
#146523=CARTESIAN_POINT('Ctrl Pts',(83.7994577864604,-8.17217878861295,
62.1603994365102));
#146524=CARTESIAN_POINT('Ctrl Pts',(83.7962975892537,-8.16209030713504,
62.1475641665206));
#146525=CARTESIAN_POINT('Ctrl Pts',(83.7917535760363,-8.14758418926295,
62.1291084713005));
#146526=CARTESIAN_POINT('Ctrl Pts',(83.7878694125071,-8.13242640488484,
62.1105131109079));
#146527=CARTESIAN_POINT('Ctrl Pts',(83.7847278327247,-8.116637410475,62.0918650260291));
#146528=CARTESIAN_POINT('Ctrl Pts',(83.7831570428335,-8.10874291327008,
62.0825409835898));
#146529=CARTESIAN_POINT('Ctrl Pts',(83.78177180665,-8.10069085666175,62.0732039349876));
#146530=CARTESIAN_POINT('Ctrl Pts',(83.7805817563341,-8.09248530304138,
62.0638657206417));
#146531=CARTESIAN_POINT('Ctrl Pts',(83.7799240917833,-8.08795061936961,
62.0587050879681));
#146532=CARTESIAN_POINT('Ctrl Pts',(83.7792933688352,-8.08311536214206,
62.0532586758234));
#146533=CARTESIAN_POINT('Ctrl Pts',(83.778749465815,-8.07839873268998,62.0480028192095));
#146534=CARTESIAN_POINT('Ctrl Pts',(83.7783091711006,-8.07458057588619,
62.0437481528436));
#146535=CARTESIAN_POINT('Ctrl Pts',(83.7779247392201,-8.07084079598696,
62.0396181897044));
#146536=CARTESIAN_POINT('Ctrl Pts',(83.7776061937308,-8.0674132493151,62.035859999865));
#146537=CARTESIAN_POINT('Ctrl Pts',(83.7754984072372,-8.04473348512597,
62.0109923999474));
#146538=CARTESIAN_POINT('Ctrl Pts',(83.7748802107319,-8.02137383895631,
61.98661819215));
#146539=CARTESIAN_POINT('Ctrl Pts',(83.7757452476007,-7.9975176531896,61.9629193749232));
#146540=CARTESIAN_POINT('Ctrl Pts',(83.7766127091347,-7.97359459944707,
61.9391541308186));
#146541=CARTESIAN_POINT('Ctrl Pts',(83.7789715750591,-7.94917288402073,
61.9160686262253));
#146542=CARTESIAN_POINT('Ctrl Pts',(83.7827704559858,-7.92444881313273,
61.8938221111338));
#146543=CARTESIAN_POINT('Ctrl Pts',(83.7866067112694,-7.89948150054621,
61.8713567291679));
#146544=CARTESIAN_POINT('Ctrl Pts',(83.7919111255218,-7.87420655012517,
61.8497473758364));
#146545=CARTESIAN_POINT('Ctrl Pts',(83.7985885813855,-7.84882739185262,
61.8291255942874));
#146546=CARTESIAN_POINT('Ctrl Pts',(83.8053127266468,-7.82327078012543,
61.808359623308));
#146547=CARTESIAN_POINT('Ctrl Pts',(83.8134286419699,-7.79760916121798,
61.7885953306014));
#146548=CARTESIAN_POINT('Ctrl Pts',(83.8228032789842,-7.77204117685951,
61.7699289893133));
#146549=CARTESIAN_POINT('Ctrl Pts',(83.8323126753202,-7.74610565568599,
61.7509943215301));
#146550=CARTESIAN_POINT('Ctrl Pts',(83.8431165916147,-7.72026707691074,
61.7331894893711));
#146551=CARTESIAN_POINT('Ctrl Pts',(83.8550483663382,-7.69471378481215,
61.7165732848687));
#146552=CARTESIAN_POINT('Ctrl Pts',(83.8589179758298,-7.68642656317606,
61.7111844618188));
#146553=CARTESIAN_POINT('Ctrl Pts',(83.862906037903,-7.67816916362773,61.7059203292459));
#146554=CARTESIAN_POINT('Ctrl Pts',(83.8670064351955,-7.66994744419446,
61.7007819660702));
#146555=CARTESIAN_POINT('Ctrl Pts',(83.2009909607981,-7.94208206191376,
62.8844208924415));
#146556=CARTESIAN_POINT('Ctrl Pts',(83.2281670225282,-7.94783420853062,
62.8796179614531));
#146557=CARTESIAN_POINT('Ctrl Pts',(83.2557799101056,-7.95432167821131,
62.8736428485721));
#146558=CARTESIAN_POINT('Ctrl Pts',(83.2837135173524,-7.96165657404679,
62.866504562709));
#146559=CARTESIAN_POINT('Ctrl Pts',(83.3074796736338,-7.96789716729324,
62.8604312469391));
#146560=CARTESIAN_POINT('Ctrl Pts',(83.3314783642032,-7.9747513011514,62.8535164195537));
#146561=CARTESIAN_POINT('Ctrl Pts',(83.3556339282506,-7.98228535354528,
62.8457291378132));
#146562=CARTESIAN_POINT('Ctrl Pts',(83.3777271527932,-7.98917616805606,
62.8386067140217));
#146563=CARTESIAN_POINT('Ctrl Pts',(83.3999519971398,-7.99663580775826,
62.8307546185476));
#146564=CARTESIAN_POINT('Ctrl Pts',(83.4222414954207,-8.00471164959767,
62.8221119623137));
#146565=CARTESIAN_POINT('Ctrl Pts',(83.4497231308661,-8.01466868580137,
62.8114560774255));
#146566=CARTESIAN_POINT('Ctrl Pts',(83.4772986038528,-8.02556596420315,
62.7996349070896));
#146567=CARTESIAN_POINT('Ctrl Pts',(83.5048073038998,-8.03749391859776,
62.7866175289148));
#146568=CARTESIAN_POINT('Ctrl Pts',(83.5149872747595,-8.04190802133417,
62.7818002700016));
#146569=CARTESIAN_POINT('Ctrl Pts',(83.5251579439255,-8.04646318982533,
62.7768187441885));
#146570=CARTESIAN_POINT('Ctrl Pts',(83.5353104485783,-8.05116368426297,
62.7716696637962));
#146571=CARTESIAN_POINT('Ctrl Pts',(83.5541039408197,-8.05986485789111,
62.7621381042734));
#146572=CARTESIAN_POINT('Ctrl Pts',(83.5728350316721,-8.06906427407646,
62.7520359380708));
#146573=CARTESIAN_POINT('Ctrl Pts',(83.5914414113032,-8.07878738133277,
62.7413522091509));
#146574=CARTESIAN_POINT('Ctrl Pts',(83.6007446011188,-8.08364893496093,
62.7360103446909));
#146575=CARTESIAN_POINT('Ctrl Pts',(83.6100166058091,-8.08864142410212,
62.7305230886088));
#146576=CARTESIAN_POINT('Ctrl Pts',(83.6192489219252,-8.09376770771874,
62.724889277636));
#146577=CARTESIAN_POINT('Ctrl Pts',(83.6238650799833,-8.09633084952704,
62.7220723721496));
#146578=CARTESIAN_POINT('Ctrl Pts',(83.6284713157787,-8.09892744021904,
62.7192188279071));
#146579=CARTESIAN_POINT('Ctrl Pts',(83.6330665448275,-8.1015578272724,62.7163285084698));
#146580=CARTESIAN_POINT('Ctrl Pts',(83.6353641593519,-8.10287302079907,
62.7148833487512));
#146581=CARTESIAN_POINT('Ctrl Pts',(83.6376590221754,-8.10419666343821,
62.713428995233));
#146582=CARTESIAN_POINT('Ctrl Pts',(83.6399509952151,-8.10552879729796,
62.7119654317475));
#146583=CARTESIAN_POINT('Ctrl Pts',(83.6415565080225,-8.10646194875131,
62.7109402146616));
#146584=CARTESIAN_POINT('Ctrl Pts',(83.6437083400293,-8.10772030426501,
62.7095596759605));
#146585=CARTESIAN_POINT('Ctrl Pts',(83.6452547229997,-8.10862970828445,
62.7085597546232));
#146586=CARTESIAN_POINT('Ctrl Pts',(83.6459159014145,-8.10901853713185,
62.7081322237867));
#146587=CARTESIAN_POINT('Ctrl Pts',(83.6464667190264,-8.10934333658453,
62.7077748921016));
#146588=CARTESIAN_POINT('Ctrl Pts',(83.6468181061104,-8.10955071426685,
62.7075470955155));
#146589=CARTESIAN_POINT('Ctrl Pts',(83.6609113500737,-8.11786810669007,
62.6984107526942));
#146590=CARTESIAN_POINT('Ctrl Pts',(83.6761493632529,-8.12725369277389,
62.6881873915792));
#146591=CARTESIAN_POINT('Ctrl Pts',(83.6923132574621,-8.13783350053357,
62.6767294536937));
#146592=CARTESIAN_POINT('Ctrl Pts',(83.7079130162838,-8.14804406287054,
62.6656714088133));
#146593=CARTESIAN_POINT('Ctrl Pts',(83.7243749174002,-8.15936730271737,
62.6534622780592));
#146594=CARTESIAN_POINT('Ctrl Pts',(83.741461207875,-8.17193021827758,62.6399908037421));
#146595=CARTESIAN_POINT('Ctrl Pts',(83.7576258179059,-8.18381545639761,
62.6272460169671));
#146596=CARTESIAN_POINT('Ctrl Pts',(83.7743487743116,-8.19681056643385,
62.6133706978287));
#146597=CARTESIAN_POINT('Ctrl Pts',(83.791396945696,-8.21103063117005,62.5983031779341));
#146598=CARTESIAN_POINT('Ctrl Pts',(83.8079720798566,-8.22485613042504,
62.5836537379392));
#146599=CARTESIAN_POINT('Ctrl Pts',(83.8248541767592,-8.23983981935114,
62.5678767447202));
#146600=CARTESIAN_POINT('Ctrl Pts',(83.8418047246299,-8.25609055218577,
62.5509566094758));
#146601=CARTESIAN_POINT('Ctrl Pts',(83.8581533560038,-8.27176421906046,
62.5346373107714));
#146602=CARTESIAN_POINT('Ctrl Pts',(83.8745651391945,-8.28861678574483,
62.5172543098411));
#146603=CARTESIAN_POINT('Ctrl Pts',(83.8908103573094,-8.30674512902824,
62.4988387136964));
#146604=CARTESIAN_POINT('Ctrl Pts',(83.9042019757953,-8.32168908701729,
62.4836579610579));
#146605=CARTESIAN_POINT('Ctrl Pts',(83.917479982152,-8.33750004403912,62.4677762256421));
#146606=CARTESIAN_POINT('Ctrl Pts',(83.9305111742816,-8.35423003346305,
62.4512372195408));
#146607=CARTESIAN_POINT('Origin',(82.8534541851791,-9.38083151964699,62.64107301909));
#146608=CARTESIAN_POINT('Origin',(82.8534541851791,-9.38083151964699,62.64107301909));
#146609=CARTESIAN_POINT('',(83.1139265222929,-9.38083161253521,64.1182846361553));
#146610=CARTESIAN_POINT('Origin',(82.8534541851791,-9.38083151964699,62.64107301909));
#146611=CARTESIAN_POINT('',(81.9035260552726,-8.32029685773108,63.1131988274128));
#146612=CARTESIAN_POINT('Origin',(82.8534541851791,-9.38083151964699,62.64107301909));
#146613=CARTESIAN_POINT('Origin',(82.9055487652491,-9.38083151964699,62.93651606395));
#146614=CARTESIAN_POINT('Origin',(82.9402782740091,-9.38083151964699,63.133476895592));
#146615=CARTESIAN_POINT('Origin',(81.2702407042791,-7.61327378225099,63.427949577933));
#146616=CARTESIAN_POINT('Origin',(74.0770084968991,1.4210854715202E-14,
64.696310494594));
#146617=CARTESIAN_POINT('',(67.0545019141992,-9.08849701091377,65.731481543374));
#146618=CARTESIAN_POINT('Ctrl Pts',(67.0545019147976,-9.08849701139183,
65.7314815432678));
#146619=CARTESIAN_POINT('Ctrl Pts',(67.05231832276,-9.08149629921886,65.6877553753418));
#146620=CARTESIAN_POINT('Ctrl Pts',(67.0519935097677,-9.07221722874611,
65.6443013928565));
#146621=CARTESIAN_POINT('Ctrl Pts',(67.0535297172201,-9.06074116961122,
65.6015030780834));
#146622=CARTESIAN_POINT('Ctrl Pts',(67.0551227184189,-9.04884083939825,
65.5571225052427));
#146623=CARTESIAN_POINT('Ctrl Pts',(67.0587170898111,-9.03457794627075,
65.5134475618804));
#146624=CARTESIAN_POINT('Ctrl Pts',(67.0642780735054,-9.01808724623876,
65.4708926217762));
#146625=CARTESIAN_POINT('Ctrl Pts',(67.0696412490677,-9.00218313209702,
65.4298513910583));
#146626=CARTESIAN_POINT('Ctrl Pts',(67.0768333564601,-8.98420728490995,
65.3898522398811));
#146627=CARTESIAN_POINT('Ctrl Pts',(67.085790362286,-8.9643178708117,65.3512482201939));
#146628=CARTESIAN_POINT('Ctrl Pts',(67.094746074706,-8.9444313287763,65.3126497749882));
#146629=CARTESIAN_POINT('Ctrl Pts',(67.1054660812389,-8.92263198011543,
65.2754464602497));
#146630=CARTESIAN_POINT('Ctrl Pts',(67.1178552704815,-8.89911169370504,
65.2399665586183));
#146631=CARTESIAN_POINT('Ctrl Pts',(67.1302446240882,-8.87559109525728,
65.2044861862845));
#146632=CARTESIAN_POINT('Ctrl Pts',(67.1443030751752,-8.85034975810816,
65.170729642724));
#146633=CARTESIAN_POINT('Ctrl Pts',(67.159906081631,-8.8236099380638,65.1389948090526));
#146634=CARTESIAN_POINT('Ctrl Pts',(67.1616370485728,-8.82064347485965,
65.1354742088309));
#146635=CARTESIAN_POINT('Ctrl Pts',(67.16338699617,-8.81765859794769,65.1319784562168));
#146636=CARTESIAN_POINT('Ctrl Pts',(67.1651557332315,-8.81465563169097,
65.1285079318638));
#146637=CARTESIAN_POINT('Ctrl Pts',(67.1810999456227,-8.7875855075655,65.0972230232154));
#146638=CARTESIAN_POINT('Ctrl Pts',(67.1985731460612,-8.75904344674962,
65.067991317463));
#146639=CARTESIAN_POINT('Ctrl Pts',(67.2174209748346,-8.72928110048734,
65.0410707466328));
#146640=CARTESIAN_POINT('Ctrl Pts',(67.2369656124516,-8.69841843299819,
65.0131549157091));
#146641=CARTESIAN_POINT('Ctrl Pts',(67.2579883376272,-8.66624379144337,
64.9877248586781));
#146642=CARTESIAN_POINT('Ctrl Pts',(67.2802895307771,-8.6330621782672,64.965021818082));
#146643=CARTESIAN_POINT('Ctrl Pts',(67.3017974531902,-8.60106086080673,
64.943126342248));
#146644=CARTESIAN_POINT('Ctrl Pts',(67.3244941408036,-8.56812339116989,
64.9237672910116));
#146645=CARTESIAN_POINT('Ctrl Pts',(67.3481791255317,-8.5345402554752,64.9071155221357));
#146646=CARTESIAN_POINT('Ctrl Pts',(67.3718606906226,-8.50096196851232,
64.8904661574415));
#146647=CARTESIAN_POINT('Ctrl Pts',(67.3965300201918,-8.46673855222839,
64.8765234658199));
#146648=CARTESIAN_POINT('Ctrl Pts',(67.4219693026433,-8.43217175319865,
64.8654104757455));
#146649=CARTESIAN_POINT('Ctrl Pts',(67.4474089232091,-8.39760449474063,
64.8542973379681));
#146650=CARTESIAN_POINT('Ctrl Pts',(67.4736182520635,-8.36269420470903,
64.8460140928845));
#146651=CARTESIAN_POINT('Ctrl Pts',(67.5003658828917,-8.32774869419913,
64.8406338471304));
#146652=CARTESIAN_POINT('Ctrl Pts',(67.5033332164201,-8.32387190280511,
64.8400369724494));
#146653=CARTESIAN_POINT('Ctrl Pts',(67.5063071636439,-8.31999468080688,
64.8394757742891));
#146654=CARTESIAN_POINT('Ctrl Pts',(67.5092874005591,-8.31611745004299,
64.8389503137869));
#146655=CARTESIAN_POINT('Origin',(74.0422786883791,1.4210854715202E-14,
64.499347962919));
#146656=CARTESIAN_POINT('Origin',(73.9901844080691,1.4210854715202E-14,
64.203906618088));
#146657=CARTESIAN_POINT('',(66.3719565885174,-10.2467348102415,67.0703602807809));
#146658=CARTESIAN_POINT('Origin',(74.2506566745691,1.4210854715202E-14,
65.681118247606));
#146659=CARTESIAN_POINT('Ctrl Pts',(66.3719377767423,-10.2467141764814,
67.0703489624824));
#146660=CARTESIAN_POINT('Ctrl Pts',(66.4084017164395,-10.199381809132,67.0639183297397));
#146661=CARTESIAN_POINT('Ctrl Pts',(66.4442296537897,-10.1520433256366,
67.0539284012353));
#146662=CARTESIAN_POINT('Ctrl Pts',(66.4791651716259,-10.1050413196356,
67.0404508581616));
#146663=CARTESIAN_POINT('Ctrl Pts',(66.5140986365642,-10.0580420755894,
67.0269741070618));
#146664=CARTESIAN_POINT('Ctrl Pts',(66.5481395450799,-10.0113795967587,
67.0100102452616));
#146665=CARTESIAN_POINT('Ctrl Pts',(66.5810442303557,-9.96539144021289,
66.9896812286782));
#146666=CARTESIAN_POINT('Ctrl Pts',(66.6139549715822,-9.91939481976567,
66.969348470636));
#146667=CARTESIAN_POINT('Ctrl Pts',(66.6457288424415,-9.87407309027168,
66.9456494588101));
#146668=CARTESIAN_POINT('Ctrl Pts',(66.6761382860771,-9.82975415389626,
66.9187547716618));
#146669=CARTESIAN_POINT('Ctrl Pts',(66.7065433412699,-9.78544161326815,
66.8918639657354));
#146670=CARTESIAN_POINT('Ctrl Pts',(66.7355841521626,-9.74213188408042,
66.8617785948035));
#146671=CARTESIAN_POINT('Ctrl Pts',(66.7630527981812,-9.70013817434927,
66.8287152352373));
#146672=CARTESIAN_POINT('Ctrl Pts',(66.790524079827,-9.65814043530542,66.7956487032289));
#146673=CARTESIAN_POINT('Ctrl Pts',(66.8164227032188,-9.61745926028037,
66.7596038403276));
#146674=CARTESIAN_POINT('Ctrl Pts',(66.8405632538059,-9.57838888827831,
66.7208402393864));
#146675=CARTESIAN_POINT('Ctrl Pts',(66.8573825149536,-9.55116768686174,
66.6938327722244));
#146676=CARTESIAN_POINT('Ctrl Pts',(66.8733488394468,-9.52472800867184,
66.6655064724249));
#146677=CARTESIAN_POINT('Ctrl Pts',(66.8884067047024,-9.49916279037104,
66.6359604921911));
#146678=CARTESIAN_POINT('Ctrl Pts',(66.9100174794419,-9.46247205337188,
66.5935566379629));
#146679=CARTESIAN_POINT('Ctrl Pts',(66.929755988921,-9.42758391409385,66.5486391633832));
#146680=CARTESIAN_POINT('Ctrl Pts',(66.9474800086736,-9.39474983739101,
66.501531784445));
#146681=CARTESIAN_POINT('Ctrl Pts',(66.9652029887504,-9.36191768670704,
66.4544271687855));
#146682=CARTESIAN_POINT('Ctrl Pts',(66.9809115925191,-9.33113958549307,
66.4051332333531));
#146683=CARTESIAN_POINT('Ctrl Pts',(66.9944926518804,-9.30263735104727,
66.3540051939298));
#146684=CARTESIAN_POINT('Ctrl Pts',(67.0080762112771,-9.27412986983884,
66.3028677427291));
#146685=CARTESIAN_POINT('Ctrl Pts',(67.0195313475018,-9.2478992925461,66.2498958669422));
#146686=CARTESIAN_POINT('Ctrl Pts',(67.0287755137373,-9.22413473587621,
66.1954714264602));
#146687=CARTESIAN_POINT('Ctrl Pts',(67.0380183454304,-9.20037360999825,
66.1410548430123));
#146688=CARTESIAN_POINT('Ctrl Pts',(67.0450507819468,-9.17907795707956,
66.0851864930388));
#146689=CARTESIAN_POINT('Ctrl Pts',(67.0498221747758,-9.16040127550207,
66.0282690003933));
#146690=CARTESIAN_POINT('Ctrl Pts',(67.0545940249536,-9.14172280372224,
65.9713460520768));
#146691=CARTESIAN_POINT('Ctrl Pts',(67.0571043642474,-9.12566393580531,
65.9133741554404));
#146692=CARTESIAN_POINT('Ctrl Pts',(67.0573351324854,-9.11234045373913,
65.85477117363));
#146693=CARTESIAN_POINT('Ctrl Pts',(67.0574959471453,-9.10305576509771,
65.8139327173717));
#146694=CARTESIAN_POINT('Ctrl Pts',(67.0565504325796,-9.09509865285608,
65.7727881131849));
#146695=CARTESIAN_POINT('Ctrl Pts',(67.0545019148004,-9.0884970113884,65.7314815432682));
#146696=CARTESIAN_POINT('Ctrl Pts',(66.3062970743491,-10.66489088643,67.041769621825));
#146697=CARTESIAN_POINT('Ctrl Pts',(66.2504617153091,-10.58427361457,67.053542835718));
#146698=CARTESIAN_POINT('Ctrl Pts',(66.0547528912291,-10.2876201762,67.106528502032));
#146699=CARTESIAN_POINT('Ctrl Pts',(65.7753967212292,-9.779459606408,67.246161639635));
#146700=CARTESIAN_POINT('Ctrl Pts',(65.5119315184691,-9.16743128369398,
67.4698540222511));
#146701=CARTESIAN_POINT('Ctrl Pts',(65.3288460021691,-8.62877957219299,
67.705374609763));
#146702=CARTESIAN_POINT('Ctrl Pts',(65.2062279860991,-8.16440041052299,
67.942334778192));
#146703=CARTESIAN_POINT('Ctrl Pts',(65.1320446995391,-7.77960342737999,
68.174487400817));
#146704=CARTESIAN_POINT('Ctrl Pts',(65.0980975644191,-7.48390022505899,
68.396209689244));
#146705=CARTESIAN_POINT('Ctrl Pts',(65.0969663795691,-7.29264316256499,
68.598155241067));
#146706=CARTESIAN_POINT('Ctrl Pts',(65.1139303495591,-7.22517886813799,
68.749749824733));
#146707=CARTESIAN_POINT('Ctrl Pts',(65.1293731629891,-7.22766901996699,
68.835084325791));
#146708=CARTESIAN_POINT('Ctrl Pts',(65.1353202143191,-7.23318211597299,
68.864201267989));
#146709=CARTESIAN_POINT('Ctrl Pts',(66.9228783679491,-9.857884207097,67.18800044511));
#146710=CARTESIAN_POINT('Ctrl Pts',(66.8813725186591,-9.78412567680498,
67.1771385985831));
#146711=CARTESIAN_POINT('Ctrl Pts',(66.7297181498991,-9.510843685412,67.145288462166));
#146712=CARTESIAN_POINT('Ctrl Pts',(66.4767641188491,-9.03120867882798,
67.138102774496));
#146713=CARTESIAN_POINT('Ctrl Pts',(66.1820507100991,-8.43327718432299,
67.201352307393));
#146714=CARTESIAN_POINT('Ctrl Pts',(65.9284768389591,-7.88808399311499,
67.317910472815));
#146715=CARTESIAN_POINT('Ctrl Pts',(65.7113975443191,-7.39715233850599,
67.480135816037));
#146716=CARTESIAN_POINT('Ctrl Pts',(65.5295093985692,-6.96458385138599,
67.6891203028381));
#146717=CARTESIAN_POINT('Ctrl Pts',(65.3870747679392,-6.59986960464899,
67.9543145934371));
#146718=CARTESIAN_POINT('Ctrl Pts',(65.2999640064091,-6.32849541217299,
68.288796224779));
#146719=CARTESIAN_POINT('Ctrl Pts',(65.2986301726591,-6.21755287707399,
68.628674831736));
#146720=CARTESIAN_POINT('Ctrl Pts',(65.3361506337991,-6.222198461074,68.82847382208));
#146721=CARTESIAN_POINT('Ctrl Pts',(65.3527548091692,-6.23109205796199,
68.8946036571191));
#146722=CARTESIAN_POINT('Ctrl Pts',(67.3317483081991,-9.21987568814898,
66.4962091862191));
#146723=CARTESIAN_POINT('Ctrl Pts',(67.2730998070291,-9.15153958578098,
66.470222614952));
#146724=CARTESIAN_POINT('Ctrl Pts',(67.0554617533692,-8.89673474290699,
66.386577884774));
#146725=CARTESIAN_POINT('Ctrl Pts',(66.6734667414291,-8.43965165912399,
66.3162259117851));
#146726=CARTESIAN_POINT('Ctrl Pts',(66.2034070026591,-7.85286492552099,
66.349711667394));
#146727=CARTESIAN_POINT('Ctrl Pts',(65.7813830547891,-7.30250012931199,
66.48266933916));
#146728=CARTESIAN_POINT('Ctrl Pts',(65.4063407259891,-6.79057643445299,
66.704345376687));
#146729=CARTESIAN_POINT('Ctrl Pts',(65.0805829419992,-6.32024044517699,
67.019393916489));
#146730=CARTESIAN_POINT('Ctrl Pts',(64.8157501610991,-5.90096700411599,
67.448562171506));
#146731=CARTESIAN_POINT('Ctrl Pts',(64.6458675632491,-5.56625329692299,
68.021190828507));
#146732=CARTESIAN_POINT('Ctrl Pts',(64.6364193785091,-5.42093745532399,
68.624674676515));
#146733=CARTESIAN_POINT('Ctrl Pts',(64.7035612536991,-5.42728709471999,
68.980959567861));
#146734=CARTESIAN_POINT('Ctrl Pts',(64.7336316140092,-5.438853269687,69.098531485314));
#146735=CARTESIAN_POINT('Ctrl Pts',(67.2323151506591,-9.21991446919998,
65.474984814013));
#146736=CARTESIAN_POINT('Ctrl Pts',(67.1376547180191,-9.15157803723199,
65.452503202276));
#146737=CARTESIAN_POINT('Ctrl Pts',(66.7925045216491,-8.896772071233,65.388183277361));
#146738=CARTESIAN_POINT('Ctrl Pts',(66.2208933601991,-8.43968761664299,
65.384755954266));
#146739=CARTESIAN_POINT('Ctrl Pts',(65.5602997427191,-7.85290020560999,
65.541038647212));
#146740=CARTESIAN_POINT('Ctrl Pts',(64.9957046052491,-7.30253572375499,
65.813701215149));
#146741=CARTESIAN_POINT('Ctrl Pts',(64.5153282640591,-6.79061330488699,
66.185306688001));
#146742=CARTESIAN_POINT('Ctrl Pts',(64.1153057006891,-6.32027961129199,
66.657675625535));
#146743=CARTESIAN_POINT('Ctrl Pts',(63.8041484102192,-5.90100948658499,
67.250769932652));
#146744=CARTESIAN_POINT('Ctrl Pts',(63.6155536603191,-5.56629962945499,
67.992076363979));
#146745=CARTESIAN_POINT('Ctrl Pts',(63.6141400609291,-5.42098587722199,
68.740690180875));
#146746=CARTESIAN_POINT('Ctrl Pts',(63.6966701364891,-5.42733541303799,
69.180437561794));
#146747=CARTESIAN_POINT('Ctrl Pts',(63.7331157142191,-5.43890142555399,
69.32606171939));
#146748=CARTESIAN_POINT('Ctrl Pts',(65.6628221245791,-7.69741879281999,
66.179958572744));
#146749=CARTESIAN_POINT('Ctrl Pts',(65.880635783277,-7.95491253744867,66.079322299056));
#146750=CARTESIAN_POINT('Ctrl Pts',(66.098391668443,-8.20085114340354,65.9933372157089));
#146751=CARTESIAN_POINT('Ctrl Pts',(66.5559400877547,-8.66510116739808,
65.8421362758434));
#146752=CARTESIAN_POINT('Ctrl Pts',(66.7955834923,-8.88331642583493,65.7770795900716));
#146753=CARTESIAN_POINT('Ctrl Pts',(67.0545019147991,-9.08849701138999,
65.731481543268));
#146754=CARTESIAN_POINT('Ctrl Pts',(66.3719249731476,-10.2467348134123,
67.0703693338527));
#146755=CARTESIAN_POINT('Ctrl Pts',(66.3587699159923,-10.2258771100607,
67.0726860040253));
#146756=CARTESIAN_POINT('Ctrl Pts',(66.3456963439005,-10.204931303275,67.0751687775537));
#146757=CARTESIAN_POINT('Ctrl Pts',(66.3327087066816,-10.1839044520611,
67.0778129159232));
#146758=CARTESIAN_POINT('Ctrl Pts',(66.2013322819353,-9.97120737024384,
67.1045596936215));
#146759=CARTESIAN_POINT('Ctrl Pts',(66.0787482680444,-9.75021642292389,
67.1478203956863));
#146760=CARTESIAN_POINT('Ctrl Pts',(65.9657693900773,-9.52542421822077,
67.2039202363711));
#146761=CARTESIAN_POINT('Ctrl Pts',(65.9267523303586,-9.44779261988124,
67.2232942191331));
#146762=CARTESIAN_POINT('Ctrl Pts',(65.8888808777626,-9.36970777215893,
67.2441991958904));
#146763=CARTESIAN_POINT('Ctrl Pts',(65.8521738661728,-9.29135080903652,
67.2665615746551));
#146764=CARTESIAN_POINT('Ctrl Pts',(65.795534694387,-9.17044547507714,67.3010668791606));
#146765=CARTESIAN_POINT('Ctrl Pts',(65.7416673787108,-9.04889180086284,
67.3390422948992));
#146766=CARTESIAN_POINT('Ctrl Pts',(65.6906372195148,-8.92735669390233,
67.3802192562758));
#146767=CARTESIAN_POINT('Ctrl Pts',(65.615348862804,-8.74804746520514,67.4409705023081));
#146768=CARTESIAN_POINT('Ctrl Pts',(65.5462361893532,-8.56877865507418,
67.5086905980588));
#146769=CARTESIAN_POINT('Ctrl Pts',(65.4836031430187,-8.39215335319471,
67.5833304387398));
#146770=CARTESIAN_POINT('Ctrl Pts',(65.4273219721058,-8.23344035128313,
67.6504007454888));
#146771=CARTESIAN_POINT('Ctrl Pts',(65.3762728187147,-8.07686186894069,
67.7230584414322));
#146772=CARTESIAN_POINT('Ctrl Pts',(65.3310788970486,-7.925489868639,67.8019493212137));
#146773=CARTESIAN_POINT('Ctrl Pts',(65.290241741339,-7.78871037001386,67.8732349946612));
#146774=CARTESIAN_POINT('Ctrl Pts',(65.2541853212793,-7.65618191234247,
67.9496099938284));
#146775=CARTESIAN_POINT('Ctrl Pts',(65.2240011710327,-7.53224655616877,
68.0320923495727));
#146776=CARTESIAN_POINT('Ctrl Pts',(65.196700477153,-7.42015059878312,68.1066952628982));
#146777=CARTESIAN_POINT('Ctrl Pts',(65.1742036921384,-7.315084379016,68.1862944018207));
#146778=CARTESIAN_POINT('Ctrl Pts',(65.1582250830977,-7.2235599576371,68.271795733124));
#146779=CARTESIAN_POINT('Ctrl Pts',(65.1480055899892,-7.16502337343489,
68.3264801092046));
#146780=CARTESIAN_POINT('Ctrl Pts',(65.140452382556,-7.11202611388141,68.3835788078871));
#146781=CARTESIAN_POINT('Ctrl Pts',(65.1363083340697,-7.0676644135367,68.4428285860919));
#146782=CARTESIAN_POINT('Ctrl Pts',(65.1345887505014,-7.0492564119832,68.4674144338111));
#146783=CARTESIAN_POINT('Ctrl Pts',(65.1334561730655,-7.03233529570783,
68.4923707145794));
#146784=CARTESIAN_POINT('Ctrl Pts',(65.1329636891759,-7.01712232415006,
68.5176785935998));
#146785=CARTESIAN_POINT('Ctrl Pts',(65.1314613787278,-6.9707155145032,68.5948796795156));
#146786=CARTESIAN_POINT('Ctrl Pts',(65.1359154341253,-6.94020380920389,
68.6753525626475));
#146787=CARTESIAN_POINT('Ctrl Pts',(65.1471893670695,-6.93113776553883,
68.7557374140826));
#146788=CARTESIAN_POINT('Ctrl Pts',(65.1496362012979,-6.92917011981428,
68.7731837131618));
#146789=CARTESIAN_POINT('Ctrl Pts',(65.1524042774959,-6.92821264454784,
68.7906258645289));
#146790=CARTESIAN_POINT('Ctrl Pts',(65.1554789178604,-6.92824180418985,
68.8080164594658));
#146791=CARTESIAN_POINT('Ctrl Pts',(65.0995290409545,-6.72702913922128,
68.2204986910971));
#146792=CARTESIAN_POINT('Ctrl Pts',(65.0988514463376,-6.72473836951761,
68.2093410230739));
#146793=CARTESIAN_POINT('Ctrl Pts',(65.0981431109678,-6.72240545263861,
68.1975201313493));
#146794=CARTESIAN_POINT('Ctrl Pts',(65.0974068849537,-6.72006496510622,
68.185017239628));
#146795=CARTESIAN_POINT('Ctrl Pts',(65.095956155403,-6.71545304653674,68.1603803561993));
#146796=CARTESIAN_POINT('Ctrl Pts',(65.0943969051797,-6.71080899338494,
68.1330953877451));
#146797=CARTESIAN_POINT('Ctrl Pts',(65.0927528773071,-6.70642531220498,
68.1030094464778));
#146798=CARTESIAN_POINT('Ctrl Pts',(65.092564261298,-6.70592238128561,68.099557746986));
#146799=CARTESIAN_POINT('Ctrl Pts',(65.0923745342892,-6.70542293357853,
68.0960691845815));
#146800=CARTESIAN_POINT('Ctrl Pts',(65.0921837359439,-6.70492745545278,
68.0925435338524));
#146801=CARTESIAN_POINT('Ctrl Pts',(65.0905324080161,-6.70063917472585,
68.0620296134879));
#146802=CARTESIAN_POINT('Ctrl Pts',(65.0888002238557,-6.6966448016099,68.0287347627108));
#146803=CARTESIAN_POINT('Ctrl Pts',(65.0870164722665,-6.69326342402229,
67.992527598533));
#146804=CARTESIAN_POINT('Ctrl Pts',(65.0858004314016,-6.69095823009796,
67.967844009458));
#146805=CARTESIAN_POINT('Ctrl Pts',(65.0845601918433,-6.68893784615693,
67.9418052937458));
#146806=CARTESIAN_POINT('Ctrl Pts',(65.0833114663123,-6.68733036335121,
67.914406116581));
#146807=CARTESIAN_POINT('Ctrl Pts',(65.0828758257721,-6.68676956383172,
67.9048474168961));
#146808=CARTESIAN_POINT('Ctrl Pts',(65.0824392146896,-6.68625922884587,
67.8951235016651));
#146809=CARTESIAN_POINT('Ctrl Pts',(65.0820025323917,-6.68580556870411,
67.8852355166209));
#146810=CARTESIAN_POINT('Ctrl Pts',(65.0812623939487,-6.68503665429501,
67.8684762435933));
#146811=CARTESIAN_POINT('Ctrl Pts',(65.0805220832648,-6.68443058742722,
67.8512457977658));
#146812=CARTESIAN_POINT('Ctrl Pts',(65.0797840166927,-6.68401364421596,
67.833538954931));
#146813=CARTESIAN_POINT('Ctrl Pts',(65.0789318710392,-6.68353225627798,
67.8130952582115));
#146814=CARTESIAN_POINT('Ctrl Pts',(65.0780775318777,-6.68329142394815,
67.7920156087582));
#146815=CARTESIAN_POINT('Ctrl Pts',(65.0772270244056,-6.68333895508708,
67.7703021843689));
#146816=CARTESIAN_POINT('Ctrl Pts',(65.0756899091387,-6.68342485772956,
67.7310596883076));
#146817=CARTESIAN_POINT('Ctrl Pts',(65.0741648682245,-6.68445235162658,
67.6897441658871));
#146818=CARTESIAN_POINT('Ctrl Pts',(65.0726921564383,-6.68669839222721,
67.6463985424324));
#146819=CARTESIAN_POINT('Ctrl Pts',(65.0712383938668,-6.6889155332793,67.6036106421764));
#146820=CARTESIAN_POINT('Ctrl Pts',(65.0698366208069,-6.69232153309281,
67.558849859444));
#146821=CARTESIAN_POINT('Ctrl Pts',(65.0685138680218,-6.69715122989116,
67.5121000321052));
#146822=CARTESIAN_POINT('Ctrl Pts',(65.0673678998273,-6.70133544252872,
67.4715982725699));
#146823=CARTESIAN_POINT('Ctrl Pts',(65.0662802825402,-6.70658810797603,
67.4295981517366));
#146824=CARTESIAN_POINT('Ctrl Pts',(65.0652803514322,-6.71304062012262,
67.3861644948326));
#146825=CARTESIAN_POINT('Ctrl Pts',(65.0651262182528,-6.71403523485581,
67.3794694659676));
#146826=CARTESIAN_POINT('Ctrl Pts',(65.0649741827216,-6.71505834890559,
67.3727404754684));
#146827=CARTESIAN_POINT('Ctrl Pts',(65.0648243687283,-6.71611043536287,
67.3659778759423));
#146828=CARTESIAN_POINT('Ctrl Pts',(65.0640048900083,-6.72186532143319,
67.3289866291271));
#146829=CARTESIAN_POINT('Ctrl Pts',(65.0632512908526,-6.7284869270308,67.2909859159469));
#146830=CARTESIAN_POINT('Ctrl Pts',(65.0625891014791,-6.73607132014469,
67.2520668980457));
#146831=CARTESIAN_POINT('Ctrl Pts',(65.0623372359469,-6.73895606472791,
67.237263943559));
#146832=CARTESIAN_POINT('Ctrl Pts',(65.062098671377,-6.74198011486308,67.2223286428493));
#146833=CARTESIAN_POINT('Ctrl Pts',(65.0618751224679,-6.74514886085747,
67.2072680328656));
#146834=CARTESIAN_POINT('Ctrl Pts',(65.0617277540022,-6.7472377694431,67.1973397402365));
#146835=CARTESIAN_POINT('Ctrl Pts',(65.0615869183904,-6.74938956300479,
67.1873570366761));
#146836=CARTESIAN_POINT('Ctrl Pts',(65.0614528323817,-6.75160559577343,
67.1773204194393));
#146837=CARTESIAN_POINT('Ctrl Pts',(65.2414845310557,-7.08609081947666,
68.1857750435771));
#146838=CARTESIAN_POINT('Ctrl Pts',(65.2409930225825,-7.08307946957817,
68.1829875467368));
#146839=CARTESIAN_POINT('Ctrl Pts',(65.2390270370096,-7.07130660341053,
68.1718378108095));
#146840=CARTESIAN_POINT('Ctrl Pts',(65.2350498086539,-7.04943590107549,
68.149281891156));
#146841=CARTESIAN_POINT('Ctrl Pts',(65.2289662965972,-7.01998916036024,
68.1147805561278));
#146842=CARTESIAN_POINT('Ctrl Pts',(65.2215006476313,-6.98832976483916,
68.0724407641344));
#146843=CARTESIAN_POINT('Ctrl Pts',(65.2124609423225,-6.95501062438879,
68.0211740455227));
#146844=CARTESIAN_POINT('Ctrl Pts',(65.2016910752082,-6.92085388141908,
67.9600950946355));
#146845=CARTESIAN_POINT('Ctrl Pts',(65.1890769486371,-6.88686554625872,
67.8885568277298));
#146846=CARTESIAN_POINT('Ctrl Pts',(65.174545294336,-6.85408467185527,67.8061437209722));
#146847=CARTESIAN_POINT('Ctrl Pts',(65.158112543083,-6.8238577244596,67.7129489575022));
#146848=CARTESIAN_POINT('Ctrl Pts',(65.1395177520264,-6.79716341683066,
67.6074926570354));
#146849=CARTESIAN_POINT('Ctrl Pts',(65.1184916003832,-6.77532627398624,
67.4882474255094));
#146850=CARTESIAN_POINT('Ctrl Pts',(65.0946850953443,-6.75993711427478,
67.3532340262738));
#146851=CARTESIAN_POINT('Ctrl Pts',(65.0754454868457,-6.75486817113625,
67.2441207843846));
#146852=CARTESIAN_POINT('Ctrl Pts',(65.0642368910678,-6.75456867256639,
67.1805536789273));
#146853=CARTESIAN_POINT('Ctrl Pts',(65.061993565123,-6.75461306050176,67.1678311452813));
#146854=CARTESIAN_POINT('Ctrl Pts',(65.1897746446634,-7.02642538409721,
68.2593549473257));
#146855=CARTESIAN_POINT('Ctrl Pts',(65.1892024303291,-7.02291951297361,
68.2561097468352));
#146856=CARTESIAN_POINT('Ctrl Pts',(65.1869252802611,-7.00928483992008,
68.2431953208314));
#146857=CARTESIAN_POINT('Ctrl Pts',(65.1823929989191,-6.98437727076367,
68.2174915299371));
#146858=CARTESIAN_POINT('Ctrl Pts',(65.1755690707742,-6.95136155253651,
68.1787910901047));
#146859=CARTESIAN_POINT('Ctrl Pts',(65.1673123831504,-6.91636344682656,
68.1319650938863));
#146860=CARTESIAN_POINT('Ctrl Pts',(65.1574350184448,-6.87997139936304,
68.0759477730928));
#146861=CARTESIAN_POINT('Ctrl Pts',(65.1457914940052,-6.84305859113378,
68.0099140652061));
#146862=CARTESIAN_POINT('Ctrl Pts',(65.1322865151918,-6.80668404378828,
67.9333235241955));
#146863=CARTESIAN_POINT('Ctrl Pts',(65.1168576306764,-6.77189004270382,
67.845821972033));
#146864=CARTESIAN_POINT('Ctrl Pts',(65.0994927393792,-6.73995596016165,
67.7473407796801));
#146865=CARTESIAN_POINT('Ctrl Pts',(65.0799361853932,-6.71188987072493,
67.636430050595));
#146866=CARTESIAN_POINT('Ctrl Pts',(65.0579186559581,-6.68903360033692,
67.5115624362205));
#146867=CARTESIAN_POINT('Ctrl Pts',(65.0331151814423,-6.67301084343169,
67.370894942116));
#146868=CARTESIAN_POINT('Ctrl Pts',(65.013150050025,-6.66775695913348,67.2576670552906));
#146869=CARTESIAN_POINT('Ctrl Pts',(65.0015330056641,-6.66744694909317,
67.1917835228098));
#146870=CARTESIAN_POINT('Ctrl Pts',(64.9992085127703,-6.66749296220202,
67.1786006685223));
#146871=CARTESIAN_POINT('Ctrl Pts',(65.1535738069259,-6.96027158061405,
68.3372101679681));
#146872=CARTESIAN_POINT('Ctrl Pts',(65.1529121103036,-6.95621741113752,
68.3334574904581));
#146873=CARTESIAN_POINT('Ctrl Pts',(65.1502899578951,-6.94051846743772,
68.3185864716667));
#146874=CARTESIAN_POINT('Ctrl Pts',(65.1451422638615,-6.91224378481554,
68.2893924916179));
#146875=CARTESIAN_POINT('Ctrl Pts',(65.1374974024557,-6.87527097760616,
68.2460363117872));
#146876=CARTESIAN_POINT('Ctrl Pts',(65.1283636540082,-6.83657109085138,
68.1942362552807));
#146877=CARTESIAN_POINT('Ctrl Pts',(65.1175575379276,-6.79677197050921,
68.1329517240636));
#146878=CARTESIAN_POINT('Ctrl Pts',(65.1049453495612,-6.75680338637883,
68.0614244499476));
#146879=CARTESIAN_POINT('Ctrl Pts',(65.0904526420255,-6.71778313619111,
67.9792322210226));
#146880=CARTESIAN_POINT('Ctrl Pts',(65.0740289572397,-6.68075708926638,
67.886088876167));
#146881=CARTESIAN_POINT('Ctrl Pts',(65.055630559543,-6.64693022772616,67.7817463777627));
#146882=CARTESIAN_POINT('Ctrl Pts',(65.0350076549065,-6.61734318091172,
67.6647880736179));
#146883=CARTESIAN_POINT('Ctrl Pts',(65.011890939465,-6.59335695709566,67.533686665629));
#146884=CARTESIAN_POINT('Ctrl Pts',(64.9859820791854,-6.5766317019353,67.3867502173394));
#146885=CARTESIAN_POINT('Ctrl Pts',(64.9652125272479,-6.57117276489505,
67.268960235043));
#146886=CARTESIAN_POINT('Ctrl Pts',(64.9531426172181,-6.57085110030559,
67.2005083737279));
#146887=CARTESIAN_POINT('Ctrl Pts',(64.9507281308072,-6.57089891531876,
67.1868151408426));
#146888=CARTESIAN_POINT('Ctrl Pts',(65.1342438570207,-6.88922545630012,
68.4173762199009));
#146889=CARTESIAN_POINT('Ctrl Pts',(65.133486060561,-6.88458243975978,68.4130785355508));
#146890=CARTESIAN_POINT('Ctrl Pts',(65.1304933916005,-6.86666656489,68.3961062266279));
#146891=CARTESIAN_POINT('Ctrl Pts',(65.1246847728085,-6.83477575818617,
68.3631639449019));
#146892=CARTESIAN_POINT('Ctrl Pts',(65.1161582670608,-6.79355322048586,
68.3148077157122));
#146893=CARTESIAN_POINT('Ctrl Pts',(65.1060825958666,-6.75087779215306,
68.2576657485828));
#146894=CARTESIAN_POINT('Ctrl Pts',(65.0942790437781,-6.70741963316853,
68.1907244770599));
#146895=CARTESIAN_POINT('Ctrl Pts',(65.0806265551699,-6.66416928709678,
68.1132973669754));
#146896=CARTESIAN_POINT('Ctrl Pts',(65.0650730726838,-6.62230767446081,
68.0250891843942));
#146897=CARTESIAN_POINT('Ctrl Pts',(65.0475810184328,-6.58288451356995,
67.9258868152054));
#146898=CARTESIAN_POINT('Ctrl Pts',(65.0280726826782,-6.5470248949559,67.8152495452771));
#146899=CARTESIAN_POINT('Ctrl Pts',(65.0063045667778,-6.51580441028536,
67.6917964253113));
#146900=CARTESIAN_POINT('Ctrl Pts',(64.9820073764202,-6.49060466876522,
67.5540002113891));
#146901=CARTESIAN_POINT('Ctrl Pts',(64.9549113829709,-6.47312496298017,
67.4003311963398));
#146902=CARTESIAN_POINT('Ctrl Pts',(64.9332779206116,-6.46744580878183,
67.2776417345743));
#146903=CARTESIAN_POINT('Ctrl Pts',(64.9207216538056,-6.46711162774576,
67.2064316069159));
#146904=CARTESIAN_POINT('Ctrl Pts',(64.9182105185209,-6.46716137792081,
67.1921902510292));
#146905=CARTESIAN_POINT('Origin',(66.6326669169691,-15.387431115,68.54751529846));
#146906=CARTESIAN_POINT('',(66.3723475853491,-13.10500468188,67.070279796935));
#146907=CARTESIAN_POINT('Origin',(64.8949830209491,111.0724296188,67.330775935442));
#146908=CARTESIAN_POINT('',(83.1139264516123,-13.1050132065526,64.118284648618));
#146909=CARTESIAN_POINT('',(83.1139264526491,-9.38083151849399,64.118284648434));
#146910=CARTESIAN_POINT('',(83.1139264515391,-13.10501209623,64.118284648628));
#146911=CARTESIAN_POINT('Origin',(64.8949830209491,111.0724296188,67.330775935442));
#146912=CARTESIAN_POINT('',(66.37195527291,10.2467337056388,67.0703617289055));
#146913=CARTESIAN_POINT('',(66.372346455996,13.1050047578536,67.0702791546134));
#146914=CARTESIAN_POINT('',(66.3720475457991,10.24677906507,67.0703345259));
#146915=CARTESIAN_POINT('',(83.1139264516833,13.1050084134076,64.1182846486046));
#146916=CARTESIAN_POINT('',(66.3723465844291,13.10500475785,67.070279883));
#146917=CARTESIAN_POINT('',(83.1139264516891,13.10501209624,64.118284648603));
#146918=CARTESIAN_POINT('Origin',(74.2506566745691,1.4210854715202E-14,
65.681118247606));
#146919=CARTESIAN_POINT('Origin',(83.3948788947791,-13.10501209624,62.54560523476));
#146920=CARTESIAN_POINT('Origin',(82.8534541851791,-13.10501209624,62.64107301909));
#146921=CARTESIAN_POINT('Origin',(82.8534541851791,-13.10501209624,62.64107301909));
#146922=CARTESIAN_POINT('Origin',(82.8534541851791,-13.10501431796,62.64107301909));
#146923=CARTESIAN_POINT('Origin',(82.8534541851791,-13.10501209624,62.64107301909));
#146924=CARTESIAN_POINT('Origin',(83.1537660643691,-9.5,64.344226319777));
#146925=CARTESIAN_POINT('Ctrl Pts',(82.3363233957455,-12.343665452965,59.7087760102195));
#146926=CARTESIAN_POINT('Ctrl Pts',(82.5103580067827,-12.3443368485801,
59.6774248403774));
#146927=CARTESIAN_POINT('Ctrl Pts',(82.7030337161479,-12.3276047655723,
59.6714205660576));
#146928=CARTESIAN_POINT('Ctrl Pts',(83.0885922050506,-12.2518831267182,
59.7305332382176));
#146929=CARTESIAN_POINT('Ctrl Pts',(83.2804190043815,-12.1926335983454,
59.7962739132679));
#146930=CARTESIAN_POINT('Ctrl Pts',(83.6124903709299,-12.0410881150009,
59.9924860734914));
#146931=CARTESIAN_POINT('Ctrl Pts',(83.7516096696434,-11.9493050886816,
60.1222919943206));
#146932=CARTESIAN_POINT('Ctrl Pts',(83.9504113602448,-11.7582926728204,
60.4084317135998));
#146933=CARTESIAN_POINT('Ctrl Pts',(84.0104131841654,-11.6596554556486,
60.563712095989));
#146934=CARTESIAN_POINT('Ctrl Pts',(84.0366050016191,-11.56837406741,60.71288355042));
#146935=CARTESIAN_POINT('Ctrl Pts',(82.0553296437291,-10.06961035349,58.06788670299));
#146936=CARTESIAN_POINT('Ctrl Pts',(82.0508297110692,-10.32189652016,58.28772795841));
#146937=CARTESIAN_POINT('Ctrl Pts',(82.044185238899,-10.85545409583,58.73637934571));
#146938=CARTESIAN_POINT('Ctrl Pts',(82.0434349722091,-11.65068683102,59.33916327135));
#146939=CARTESIAN_POINT('Ctrl Pts',(82.0448098099991,-12.20048376736,59.70692633614));
#146940=CARTESIAN_POINT('Ctrl Pts',(82.0452134587591,-12.45553486127,59.86597852961));
#146941=CARTESIAN_POINT('Ctrl Pts',(83.2289392944191,-10.06541382727,57.8659223213401));
#146942=CARTESIAN_POINT('Ctrl Pts',(83.2201513675491,-10.3397788344,58.06049300364));
#146943=CARTESIAN_POINT('Ctrl Pts',(83.2017243183791,-10.91461113645,58.45747334811));
#146944=CARTESIAN_POINT('Ctrl Pts',(83.1784930097592,-11.75261430238,58.9905418745401));
#146945=CARTESIAN_POINT('Ctrl Pts',(83.1625683469792,-12.32074716019,59.313379833));
#146946=CARTESIAN_POINT('Ctrl Pts',(83.1546752474691,-12.58190616187,59.45208388284));
#146947=CARTESIAN_POINT('Ctrl Pts',(84.0014320878491,-9.416662390436,58.49880899002));
#146948=CARTESIAN_POINT('Ctrl Pts',(84.0197603423191,-9.71427756945499,
58.68408877132));
#146949=CARTESIAN_POINT('Ctrl Pts',(84.0535870702291,-10.3409287432,59.06357280994));
#146950=CARTESIAN_POINT('Ctrl Pts',(84.0914425043691,-11.25380191593,59.57276536302));
#146951=CARTESIAN_POINT('Ctrl Pts',(84.1097895903591,-11.87370493252,59.88080283618));
#146952=CARTESIAN_POINT('Ctrl Pts',(84.1164333695691,-12.1590724314,60.01281199009));
#146953=CARTESIAN_POINT('Ctrl Pts',(83.6792160484492,-8.70584534846799,
59.39830177706));
#146954=CARTESIAN_POINT('Ctrl Pts',(83.7317180692091,-9.00700658342599,
59.59861227705));
#146955=CARTESIAN_POINT('Ctrl Pts',(83.834918244039,-9.64949457496699,60.01048401614));
#146956=CARTESIAN_POINT('Ctrl Pts',(83.9625807365691,-10.60211439156,60.56307735249));
#146957=CARTESIAN_POINT('Ctrl Pts',(84.0359995174791,-11.26073934252,60.8997277557));
#146958=CARTESIAN_POINT('Ctrl Pts',(84.0669616904391,-11.5666800367,61.04470635445));
#146959=CARTESIAN_POINT('',(82.3525647217089,-10.1664213136743,58.1365952838437));
#146960=CARTESIAN_POINT('Ctrl Pts',(82.3525700953787,-10.166478497124,58.1365255250151));
#146961=CARTESIAN_POINT('Ctrl Pts',(82.3951531597494,-10.1611675921044,
58.135452276721));
#146962=CARTESIAN_POINT('Ctrl Pts',(82.4382846388827,-10.1545975757461,
58.1357792398753));
#146963=CARTESIAN_POINT('Ctrl Pts',(82.4817296150921,-10.1467003204195,
58.1376346901912));
#146964=CARTESIAN_POINT('Ctrl Pts',(82.5246216655268,-10.1389035737455,
58.1394665261243));
#146965=CARTESIAN_POINT('Ctrl Pts',(82.5678188296875,-10.1298128164637,
58.1427886782012));
#146966=CARTESIAN_POINT('Ctrl Pts',(82.6110610457748,-10.1193888719939,
58.147698859281));
#146967=CARTESIAN_POINT('Ctrl Pts',(82.6536135361689,-10.1091311924147,
58.1525307215707));
#146968=CARTESIAN_POINT('Ctrl Pts',(82.6962090421351,-10.0975822925618,
58.158900732393));
#146969=CARTESIAN_POINT('Ctrl Pts',(82.7385745301759,-10.0847346980979,
58.1668705743677));
#146970=CARTESIAN_POINT('Ctrl Pts',(82.770926444484,-10.0749237813735,58.172956651893));
#146971=CARTESIAN_POINT('Ctrl Pts',(82.8031436173484,-10.0643561291815,
58.1799750588118));
#146972=CARTESIAN_POINT('Ctrl Pts',(82.8350979729569,-10.0530414423116,
58.1879387605769));
#146973=CARTESIAN_POINT('Ctrl Pts',(82.8762053001496,-10.0384857885866,
58.1981835765931));
#146974=CARTESIAN_POINT('Ctrl Pts',(82.9168777867966,-10.0226925608224,
58.2099942907058));
#146975=CARTESIAN_POINT('Ctrl Pts',(82.9568372896724,-10.0057091209681,
58.2233628773243));
#146976=CARTESIAN_POINT('Ctrl Pts',(82.9965729684327,-9.98882081001011,
58.2366565828292));
#146977=CARTESIAN_POINT('Ctrl Pts',(83.0356028553504,-9.97075565883965,
58.2514908027958));
#146978=CARTESIAN_POINT('Ctrl Pts',(83.0736579528351,-9.95159249143506,
58.2678180795554));
#146979=CARTESIAN_POINT('Ctrl Pts',(83.1115465711695,-9.93251315689487,
58.2840739295853));
#146980=CARTESIAN_POINT('Ctrl Pts',(83.1484681595522,-9.912345594257,58.301809691031));
#146981=CARTESIAN_POINT('Ctrl Pts',(83.1841731300037,-9.89119758550829,
58.3209396729932));
#146982=CARTESIAN_POINT('Ctrl Pts',(83.2163800673443,-9.87212145733807,
58.3381954814308));
#146983=CARTESIAN_POINT('Ctrl Pts',(83.2475969420267,-9.85224812681749,
58.3565850795893));
#146984=CARTESIAN_POINT('Ctrl Pts',(83.2776590840935,-9.83167513719697,
58.3760201451493));
#146985=CARTESIAN_POINT('Ctrl Pts',(83.3109913998323,-9.80886420828183,
58.3975693661001));
#146986=CARTESIAN_POINT('Ctrl Pts',(83.3429030393085,-9.78519311877206,
58.4204040341745));
#146987=CARTESIAN_POINT('Ctrl Pts',(83.3732035467558,-9.7608150923811,58.4443733288806));
#146988=CARTESIAN_POINT('Ctrl Pts',(83.40356420074,-9.73638867558394,58.4683902026601));
#146989=CARTESIAN_POINT('Ctrl Pts',(83.4323068914428,-9.71125298127848,
58.4935457242152));
#146990=CARTESIAN_POINT('Ctrl Pts',(83.4592833428956,-9.68557718695221,
58.5196624506196));
#146991=CARTESIAN_POINT('Ctrl Pts',(83.4864770128165,-9.65969464724576,
58.5459894728559));
#146992=CARTESIAN_POINT('Ctrl Pts',(83.5118756015812,-9.63326378255559,
58.5732926811178));
#146993=CARTESIAN_POINT('Ctrl Pts',(83.5353766794126,-9.60646576177959,
58.6013721221683));
#146994=CARTESIAN_POINT('Ctrl Pts',(83.5564064501732,-9.58248574529688,
58.626498808383));
#146995=CARTESIAN_POINT('Ctrl Pts',(83.5759174780459,-9.558212083325,58.6522465149794));
#146996=CARTESIAN_POINT('Ctrl Pts',(83.5938712055915,-9.53377483715701,
58.6784655241524));
#146997=CARTESIAN_POINT('Ctrl Pts',(83.6143253646157,-9.5059341941504,58.7083360778702));
#146998=CARTESIAN_POINT('Ctrl Pts',(83.6327573590749,-9.47788182466822,
58.738817802516));
#146999=CARTESIAN_POINT('Ctrl Pts',(83.6491609908517,-9.4498040488955,58.7696891456885));
#147000=CARTESIAN_POINT('Ctrl Pts',(83.6657208741947,-9.42145882037187,
58.800854551529));
#147001=CARTESIAN_POINT('Ctrl Pts',(83.6802138906995,-9.39308814599666,
58.8324164399566));
#147002=CARTESIAN_POINT('Ctrl Pts',(83.6926849067531,-9.36486944317266,
58.8641550268704));
#147003=CARTESIAN_POINT('Ctrl Pts',(83.7053978734835,-9.33610326817695,
58.8965093753666));
#147004=CARTESIAN_POINT('Ctrl Pts',(83.716010056729,-9.3074954147027,58.9290467923253));
#147005=CARTESIAN_POINT('Ctrl Pts',(83.7246162927773,-9.27921253917801,
58.9615517347137));
#147006=CARTESIAN_POINT('Ctrl Pts',(83.7310073805458,-9.25820935743756,
58.9856902708343));
#147007=CARTESIAN_POINT('Ctrl Pts',(83.7362932957204,-9.23738494648499,
59.0098112489987));
#147008=CARTESIAN_POINT('Ctrl Pts',(83.7405267536393,-9.2167985425004,59.0338347984847));
#147009=CARTESIAN_POINT('Ctrl Pts',(82.3525700823783,-10.1664785168028,
58.1365255401533));
#147010=CARTESIAN_POINT('Ctrl Pts',(82.3488876921889,-10.3859560294258,
58.3162559244322));
#147011=CARTESIAN_POINT('Ctrl Pts',(82.3460217722092,-10.6066582564664,
58.4916352097824));
#147012=CARTESIAN_POINT('Ctrl Pts',(82.3439687240532,-10.829866174788,58.6621421225721));
#147013=CARTESIAN_POINT('Ctrl Pts',(82.3415371907178,-11.0942230981875,
58.8640824624238));
#147014=CARTESIAN_POINT('Ctrl Pts',(82.3402450190165,-11.3620941909475,
59.0591873596057));
#147015=CARTESIAN_POINT('Ctrl Pts',(82.339146797498,-11.6336159214709,59.2457463654941));
#147016=CARTESIAN_POINT('Ctrl Pts',(82.3390437206752,-11.6591003950567,
59.2632564117383));
#147017=CARTESIAN_POINT('Ctrl Pts',(82.3389423585988,-11.6846170092359,
59.2806912063098));
#147018=CARTESIAN_POINT('Ctrl Pts',(82.3388419338635,-11.7101658660261,
59.2980493546135));
#147019=CARTESIAN_POINT('Ctrl Pts',(82.3380197652076,-11.9193321553656,
59.4401590192575));
#147020=CARTESIAN_POINT('Ctrl Pts',(82.3372600244892,-12.130659856514,59.5771301339812));
#147021=CARTESIAN_POINT('Ctrl Pts',(82.3361472036304,-12.3441228986193,
59.7080238558997));
#147022=CARTESIAN_POINT('Ctrl Pts',(62.3774191338491,-11.93682814514,62.997303880638));
#147023=CARTESIAN_POINT('Ctrl Pts',(62.8594167896691,-11.31836793413,62.63949114694));
#147024=CARTESIAN_POINT('Ctrl Pts',(63.7016296262191,-10.28886737917,61.77926831279));
#147025=CARTESIAN_POINT('Ctrl Pts',(64.4353443697491,-9.50098361185099,
60.52921910213));
#147026=CARTESIAN_POINT('Ctrl Pts',(64.7094707273291,-9.22984173748599,
59.95551214223));
#147027=CARTESIAN_POINT('Ctrl Pts',(63.2468805636391,-12.17561401984,62.96400152021));
#147028=CARTESIAN_POINT('Ctrl Pts',(63.6737193233791,-11.57121353012,62.58432057163));
#147029=CARTESIAN_POINT('Ctrl Pts',(64.4147249566291,-10.57536035644,61.70772610609));
#147030=CARTESIAN_POINT('Ctrl Pts',(65.0622360532691,-9.81899150863899,
60.48721794767));
#147031=CARTESIAN_POINT('Ctrl Pts',(65.3060138057191,-9.55843720322299,
59.93191843234));
#147032=CARTESIAN_POINT('Ctrl Pts',(64.9762859395291,-12.57208772501,62.89914697212));
#147033=CARTESIAN_POINT('Ctrl Pts',(65.3033337930391,-12.00439019394,62.48973876938));
#147034=CARTESIAN_POINT('Ctrl Pts',(65.8640127693391,-11.0832288162,61.60122473724));
#147035=CARTESIAN_POINT('Ctrl Pts',(66.3552140056091,-10.38653655991,60.44446305748));
#147036=CARTESIAN_POINT('Ctrl Pts',(66.5422504654091,-10.14466666957,59.92552707855));
#147037=CARTESIAN_POINT('Ctrl Pts',(67.2900608069791,-12.92642311826,62.76588968559));
#147038=CARTESIAN_POINT('Ctrl Pts',(67.5005502484191,-12.40978705063,62.34387880989));
#147039=CARTESIAN_POINT('Ctrl Pts',(67.8553038215491,-11.57897812252,61.47239442111));
#147040=CARTESIAN_POINT('Ctrl Pts',(68.1616279566091,-10.94422799439,60.39769057588));
#147041=CARTESIAN_POINT('Ctrl Pts',(68.2781957858191,-10.72029903218,59.92119556699));
#147042=CARTESIAN_POINT('Ctrl Pts',(69.1793814374391,-13.12660404221,62.60480660922));
#147043=CARTESIAN_POINT('Ctrl Pts',(69.3025957496291,-12.64231047897,62.18346776903));
#147044=CARTESIAN_POINT('Ctrl Pts',(69.5039001954291,-11.86638416497,61.33529575915));
#147045=CARTESIAN_POINT('Ctrl Pts',(69.6676543241791,-11.26766155885,60.31872861861));
#147046=CARTESIAN_POINT('Ctrl Pts',(69.7281187264291,-11.05395501206,59.87083582562));
#147047=CARTESIAN_POINT('Ctrl Pts',(70.6290331937791,-13.2354548215,62.4487226016));
#147048=CARTESIAN_POINT('Ctrl Pts',(70.6877066225591,-12.77011721816,62.03193358429));
#147049=CARTESIAN_POINT('Ctrl Pts',(70.7757857175191,-12.02562572997,61.20384952745));
#147050=CARTESIAN_POINT('Ctrl Pts',(70.8324235385491,-11.44701084757,60.22578653053));
#147051=CARTESIAN_POINT('Ctrl Pts',(70.8500678830391,-11.23893116136,59.79623434573));
#147052=CARTESIAN_POINT('Ctrl Pts',(72.1029034837291,-13.30219283541,62.25362486817));
#147053=CARTESIAN_POINT('Ctrl Pts',(72.0972809910691,-12.84940037151,61.84484177145));
#147054=CARTESIAN_POINT('Ctrl Pts',(72.0725811599691,-12.12531389286,61.03819560464));
#147055=CARTESIAN_POINT('Ctrl Pts',(72.0209865447691,-11.55943931721,60.09237908051));
#147056=CARTESIAN_POINT('Ctrl Pts',(71.9948866285191,-11.35486963736,59.67756847178));
#147057=CARTESIAN_POINT('Ctrl Pts',(73.5959843581491,-13.32506131179,62.01408346482));
#147058=CARTESIAN_POINT('Ctrl Pts',(73.5261098994091,-12.87698220968,61.61585739229));
#147059=CARTESIAN_POINT('Ctrl Pts',(73.3882074986691,-12.16043554427,60.83032202918));
#147060=CARTESIAN_POINT('Ctrl Pts',(73.2263446677791,-11.59915063933,59.90895273874));
#147061=CARTESIAN_POINT('Ctrl Pts',(73.1553017064691,-11.39582011201,59.50465582683));
#147062=CARTESIAN_POINT('Ctrl Pts',(75.0808070354991,-13.30270992682,61.72903176202));
#147063=CARTESIAN_POINT('Ctrl Pts',(74.9469689190791,-12.85001089683,61.34282758741));
#147064=CARTESIAN_POINT('Ctrl Pts',(74.6955188142491,-12.1260767583,60.57617067235));
#147065=CARTESIAN_POINT('Ctrl Pts',(74.4217256775691,-11.56029813203,59.66963151356));
#147066=CARTESIAN_POINT('Ctrl Pts',(74.3048733948091,-11.3557551519,59.27087592838));
#147067=CARTESIAN_POINT('Ctrl Pts',(76.5328601007591,-13.2364944323,61.40866159641));
#147068=CARTESIAN_POINT('Ctrl Pts',(76.3358699248491,-12.77133451632,61.03688416139));
#147069=CARTESIAN_POINT('Ctrl Pts',(75.9711298326091,-12.02713706143,60.28864044243));
#147070=CARTESIAN_POINT('Ctrl Pts',(75.5846252539191,-11.44871074133,59.388898241));
#147071=CARTESIAN_POINT('Ctrl Pts',(75.4216320368191,-11.24068411792,58.99129878541));
#147072=CARTESIAN_POINT('Ctrl Pts',(77.9498391600291,-13.12798216966,61.05954876707));
#147073=CARTESIAN_POINT('Ctrl Pts',(77.6905880595291,-12.64391742949,60.7055511469));
#147074=CARTESIAN_POINT('Ctrl Pts',(77.2125004260691,-11.86837549639,59.97715614722));
#147075=CARTESIAN_POINT('Ctrl Pts',(76.7121050136191,-11.26990259162,59.07792972341));
#147076=CARTESIAN_POINT('Ctrl Pts',(76.5025735472391,-11.05626656671,58.67777561906));
#147077=CARTESIAN_POINT('Ctrl Pts',(79.7859365961591,-12.92767443376,60.56353474153));
#147078=CARTESIAN_POINT('Ctrl Pts',(79.4441950016891,-12.41122585012,60.23879024504));
#147079=CARTESIAN_POINT('Ctrl Pts',(78.8135085271691,-11.58074421675,59.54101492748));
#147080=CARTESIAN_POINT('Ctrl Pts',(78.1588401911891,-10.94621534765,58.63594665383));
#147081=CARTESIAN_POINT('Ctrl Pts',(77.8866345956591,-10.72235004384,58.22811289685));
#147082=CARTESIAN_POINT('Ctrl Pts',(82.0128595054191,-12.5725402543,59.89542135394));
#147083=CARTESIAN_POINT('Ctrl Pts',(81.5655827020591,-12.0048890977,59.6224962674));
#147084=CARTESIAN_POINT('Ctrl Pts',(80.7349790983591,-11.08381973837,58.97925604537));
#147085=CARTESIAN_POINT('Ctrl Pts',(79.8779241817091,-10.38719737489,58.0602712301));
#147086=CARTESIAN_POINT('Ctrl Pts',(79.5247423704091,-10.14534841056,57.63662074318));
#147087=CARTESIAN_POINT('Ctrl Pts',(83.6613481708691,-12.17565886824,59.36439714515));
#147088=CARTESIAN_POINT('Ctrl Pts',(83.1304065130891,-11.57125651121,59.15359310812));
#147089=CARTESIAN_POINT('Ctrl Pts',(82.1343014018491,-10.57540150418,58.58329052728));
#147090=CARTESIAN_POINT('Ctrl Pts',(81.1084241173391,-9.81903260043799,
57.65784452337));
#147091=CARTESIAN_POINT('Ctrl Pts',(80.6894326096791,-9.55847843356399,
57.21940958338));
#147092=CARTESIAN_POINT('Ctrl Pts',(84.4900685407791,-11.93678967047,59.098228309));
#147093=CARTESIAN_POINT('Ctrl Pts',(83.9147510912491,-11.31832804455,58.92685361738));
#147094=CARTESIAN_POINT('Ctrl Pts',(82.8290997230891,-10.28882373832,58.4065707627));
#147095=CARTESIAN_POINT('Ctrl Pts',(81.7120752713391,-9.50093629271799,
57.48285528109));
#147096=CARTESIAN_POINT('Ctrl Pts',(81.2582553288491,-9.22979318182899,
57.03750320808));
#147097=CARTESIAN_POINT('',(64.4192382040804,-9.75938259365387,60.7790388614543));
#147098=CARTESIAN_POINT('Ctrl Pts',(62.670809092837,-11.8749841815823,62.918604792603));
#147099=CARTESIAN_POINT('Ctrl Pts',(62.8226759631422,-11.6771183294842,
62.7956341012768));
#147100=CARTESIAN_POINT('Ctrl Pts',(62.9747638129586,-11.4821292443563,
62.6583787294019));
#147101=CARTESIAN_POINT('Ctrl Pts',(63.1257819325367,-11.2918678559167,
62.5071312698821));
#147102=CARTESIAN_POINT('Ctrl Pts',(63.2686085750815,-11.1119265654766,
62.3640877271803));
#147103=CARTESIAN_POINT('Ctrl Pts',(63.4104791030648,-10.9362130860917,
62.2085281972315));
#147104=CARTESIAN_POINT('Ctrl Pts',(63.5502962427671,-10.7663115879761,
62.0406536860054));
#147105=CARTESIAN_POINT('Ctrl Pts',(63.5583151170356,-10.7565672980105,
62.031025648976));
#147106=CARTESIAN_POINT('Ctrl Pts',(63.56632723384,-10.7468421329298,62.0213570921456));
#147107=CARTESIAN_POINT('Ctrl Pts',(63.5743323848798,-10.7371363944787,
62.0116480491215));
#147108=CARTESIAN_POINT('Ctrl Pts',(63.7064941004239,-10.576898687788,61.8513557853052));
#147109=CARTESIAN_POINT('Ctrl Pts',(63.8366793388084,-10.4220504821042,
61.6801213857542));
#147110=CARTESIAN_POINT('Ctrl Pts',(63.9638878042343,-10.274013906201,61.4982248136155));
#147111=CARTESIAN_POINT('Ctrl Pts',(64.1207829204576,-10.091430021521,61.2738790223918));
#147112=CARTESIAN_POINT('Ctrl Pts',(64.2731491329682,-9.91920894240649,
61.0333138935713));
#147113=CARTESIAN_POINT('Ctrl Pts',(64.4192367794444,-9.75938555497426,
60.7790363314927));
#147114=CARTESIAN_POINT('',(81.8125095647161,-9.7594394284026,57.7121067929141));
#147115=CARTESIAN_POINT('Origin',(81.9839346339093,-12.2832340267788,54.5148848282765));
#147116=CARTESIAN_POINT('Ctrl Pts',(64.4192213382197,-9.75941427061367,
60.779009237256));
#147117=CARTESIAN_POINT('Ctrl Pts',(64.5917519527215,-9.83352394633715,
60.7599201369048));
#147118=CARTESIAN_POINT('Ctrl Pts',(64.7636436728503,-9.90338401441579,
60.7407900832214));
#147119=CARTESIAN_POINT('Ctrl Pts',(64.9346888991107,-9.96953429478545,
60.7216255705971));
#147120=CARTESIAN_POINT('Ctrl Pts',(65.1120846075897,-10.0381405699141,
60.7017495274652));
#147121=CARTESIAN_POINT('Ctrl Pts',(65.2885702109627,-10.1027569733337,
60.6818363413983));
#147122=CARTESIAN_POINT('Ctrl Pts',(65.4639649804991,-10.163959985253,60.6618886487032));
#147123=CARTESIAN_POINT('Ctrl Pts',(65.6217577290577,-10.2190208715972,
60.6439428384256));
#147124=CARTESIAN_POINT('Ctrl Pts',(65.7786685868604,-10.2713189031568,
60.6259689958084));
#147125=CARTESIAN_POINT('Ctrl Pts',(65.9345948041783,-10.3212524718176,
60.6079667941811));
#147126=CARTESIAN_POINT('Ctrl Pts',(66.1617756184333,-10.3940045014771,
60.5817380117839));
#147127=CARTESIAN_POINT('Ctrl Pts',(66.3868666255169,-10.4617357625455,
60.5554485392112));
#147128=CARTESIAN_POINT('Ctrl Pts',(66.6097177236863,-10.5249661998724,
60.5290770483234));
#147129=CARTESIAN_POINT('Ctrl Pts',(66.6556411171841,-10.5379962287942,
60.5236426198502));
#147130=CARTESIAN_POINT('Ctrl Pts',(66.7014695395411,-10.5508350301772,
60.5182047170576));
#147131=CARTESIAN_POINT('Ctrl Pts',(66.7472018955564,-10.5634869991576,
60.5127631675472));
#147132=CARTESIAN_POINT('Ctrl Pts',(66.9802171685718,-10.627951248609,60.4850374115337));
#147133=CARTESIAN_POINT('Ctrl Pts',(67.2107340791529,-10.6875669815364,
60.457215529793));
#147134=CARTESIAN_POINT('Ctrl Pts',(67.4386303704974,-10.74289155313,60.4292758802627));
#147135=CARTESIAN_POINT('Ctrl Pts',(67.5998059025019,-10.782018856198,60.4095160682424));
#147136=CARTESIAN_POINT('Ctrl Pts',(67.7596715637253,-10.8189990303699,
60.3896974299897));
#147137=CARTESIAN_POINT('Ctrl Pts',(67.9181936648736,-10.8540169049373,
60.3698135497309));
#147138=CARTESIAN_POINT('Ctrl Pts',(68.1914973421711,-10.9143902776157,
60.3355322882897));
#147139=CARTESIAN_POINT('Ctrl Pts',(68.4608051825333,-10.9689305948752,
60.3010566373054));
#147140=CARTESIAN_POINT('Ctrl Pts',(68.7259000127629,-11.0181836739645,
60.2663757344958));
#147141=CARTESIAN_POINT('Ctrl Pts',(69.0001300308213,-11.0691340178712,
60.2304997251617));
#147142=CARTESIAN_POINT('Ctrl Pts',(69.2698521901208,-11.1144268899995,
60.1944041771647));
#147143=CARTESIAN_POINT('Ctrl Pts',(69.5348702087699,-11.1546321440666,
60.1580854692593));
#147144=CARTESIAN_POINT('Ctrl Pts',(69.7478446792571,-11.1869419950699,
60.1288989346063));
#147145=CARTESIAN_POINT('Ctrl Pts',(69.9577821379011,-11.2159655707178,
60.0995684697029));
#147146=CARTESIAN_POINT('Ctrl Pts',(70.164597028615,-11.2419808637392,60.0700952271198));
#147147=CARTESIAN_POINT('Ctrl Pts',(70.4576205793241,-11.2788403640756,
60.0283363665135));
#147148=CARTESIAN_POINT('Ctrl Pts',(70.7443728961861,-11.3096600624236,
59.9862909687595));
#147149=CARTESIAN_POINT('Ctrl Pts',(71.0245712394748,-11.3350228063679,
59.9439827482278));
#147150=CARTESIAN_POINT('Ctrl Pts',(71.3047695827635,-11.3603855503121,
59.9016745276962));
#147151=CARTESIAN_POINT('Ctrl Pts',(71.5784145540188,-11.3802916869536,
59.8591036487755));
#147152=CARTESIAN_POINT('Ctrl Pts',(71.8452775886959,-11.3952984906318,
59.816295698531));
#147153=CARTESIAN_POINT('Ctrl Pts',(71.9953031740864,-11.4037350450215,
59.7922298409177));
#147154=CARTESIAN_POINT('Ctrl Pts',(72.1431862617957,-11.4106226810622,
59.7680890736475));
#147155=CARTESIAN_POINT('Ctrl Pts',(72.2888927362891,-11.4160562736744,
59.7438779705844));
#147156=CARTESIAN_POINT('Ctrl Pts',(72.3617459735358,-11.4187730699805,
59.7317724190528));
#147157=CARTESIAN_POINT('Ctrl Pts',(72.4340550627953,-11.4211263104244,
59.719649306186));
#147158=CARTESIAN_POINT('Ctrl Pts',(72.5058162028691,-11.4231275454711,
59.7075091748962));
#147159=CARTESIAN_POINT('Ctrl Pts',(72.541696772906,-11.4241281629944,59.7014391092512));
#147160=CARTESIAN_POINT('Ctrl Pts',(72.5774403560181,-11.4250407762218,
59.6953647904832));
#147161=CARTESIAN_POINT('Ctrl Pts',(72.6130464884757,-11.4258668097512,
59.6892862902963));
#147162=CARTESIAN_POINT('Ctrl Pts',(72.6308495547045,-11.4262798265159,
59.6862470402029));
#147163=CARTESIAN_POINT('Ctrl Pts',(72.6486182582896,-11.4266711981716,
59.6832067448475));
#147164=CARTESIAN_POINT('Ctrl Pts',(72.6663525427507,-11.4270411015404,
59.6801654131775));
#147165=CARTESIAN_POINT('Ctrl Pts',(72.6752196849812,-11.4272260532248,
59.6786447473425));
#147166=CARTESIAN_POINT('Ctrl Pts',(72.684078222432,-11.4274056378258,59.6771238224347));
#147167=CARTESIAN_POINT('Ctrl Pts',(72.6929281481366,-11.4275798773662,
59.6756026395695));
#147168=CARTESIAN_POINT('Ctrl Pts',(72.6964426804789,-11.4276490723539,
59.6749985388621));
#147169=CARTESIAN_POINT('Ctrl Pts',(72.6997502454414,-11.4277134482094,
59.6744298198451));
#147170=CARTESIAN_POINT('Ctrl Pts',(72.7030957980396,-11.4277778278489,
59.6738542816511));
#147171=CARTESIAN_POINT('Ctrl Pts',(72.7081746641268,-11.4278755622465,
59.6729805600971));
#147172=CARTESIAN_POINT('Ctrl Pts',(72.7133410737757,-11.4279734137452,
59.6720911235426));
#147173=CARTESIAN_POINT('Ctrl Pts',(72.7194520827137,-11.428086583983,59.6710383182928));
#147174=CARTESIAN_POINT('Ctrl Pts',(72.9810700988372,-11.4329315078579,
59.6259667395027));
#147175=CARTESIAN_POINT('Ctrl Pts',(73.2479207672801,-11.4334108481625,
59.5785889245677));
#147176=CARTESIAN_POINT('Ctrl Pts',(73.519805288403,-11.4291105759769,59.5289406205662));
#147177=CARTESIAN_POINT('Ctrl Pts',(73.7881294221,-11.4248666167985,59.479942471993));
#147178=CARTESIAN_POINT('Ctrl Pts',(74.0613566957298,-11.4159672194884,
59.4287328216431));
#147179=CARTESIAN_POINT('Ctrl Pts',(74.3392563577797,-11.4019861630037,
59.3753589727235));
#147180=CARTESIAN_POINT('Ctrl Pts',(74.6123805523945,-11.388245358988,59.3229023076376));
#147181=CARTESIAN_POINT('Ctrl Pts',(74.8900180959707,-11.3695958349094,
59.2683550418568));
#147182=CARTESIAN_POINT('Ctrl Pts',(75.1719082682765,-11.3456084272083,
59.2117763741919));
#147183=CARTESIAN_POINT('Ctrl Pts',(75.2718400877254,-11.3371047419758,
59.1917188845835));
#147184=CARTESIAN_POINT('Ctrl Pts',(75.3723059570812,-11.3279300071673,
59.1714062426861));
#147185=CARTESIAN_POINT('Ctrl Pts',(75.4732929209364,-11.3180644214381,
59.1508415889956));
#147186=CARTESIAN_POINT('Ctrl Pts',(75.7652124079432,-11.2895463175644,
59.0913960632897));
#147187=CARTESIAN_POINT('Ctrl Pts',(76.0614882663886,-11.2552580782005,
59.0298433493103));
#147188=CARTESIAN_POINT('Ctrl Pts',(76.3619250156597,-11.2146421120415,
58.9662470746486));
#147189=CARTESIAN_POINT('Ctrl Pts',(76.6471518824436,-11.1760823659484,
58.9058704189801));
#147190=CARTESIAN_POINT('Ctrl Pts',(76.9361293595584,-11.1318188885074,
58.8436516267443));
#147191=CARTESIAN_POINT('Ctrl Pts',(77.2286584914008,-11.0813483885709,
58.7796645919439));
#147192=CARTESIAN_POINT('Ctrl Pts',(77.4808729255173,-11.0378334452869,
58.7244958855955));
#147193=CARTESIAN_POINT('Ctrl Pts',(77.7357273295204,-10.989703883753,58.6680128402438));
#147194=CARTESIAN_POINT('Ctrl Pts',(77.9930700490635,-10.9366243447965,
58.610277964424));
#147195=CARTESIAN_POINT('Ctrl Pts',(78.2338867509886,-10.8869534641363,
58.556250703013));
#147196=CARTESIAN_POINT('Ctrl Pts',(78.4768827703228,-10.832950409161,58.501127128419));
#147197=CARTESIAN_POINT('Ctrl Pts',(78.7219624690903,-10.7740694948733,
58.4449636970163));
#147198=CARTESIAN_POINT('Ctrl Pts',(78.9234244085341,-10.7256678392149,
58.3987958835535));
#147199=CARTESIAN_POINT('Ctrl Pts',(79.126294167326,-10.6739692719136,58.3519255825824));
#147200=CARTESIAN_POINT('Ctrl Pts',(79.3305018595802,-10.6186523159379,
58.3043932560179));
#147201=CARTESIAN_POINT('Ctrl Pts',(79.5640892996969,-10.555376804625,58.2500223635092));
#147202=CARTESIAN_POINT('Ctrl Pts',(79.799427858751,-10.4873682963686,58.1947861358713));
#147203=CARTESIAN_POINT('Ctrl Pts',(80.03638006309,-10.4141215949237,58.138760307174));
#147204=CARTESIAN_POINT('Ctrl Pts',(80.0775805354926,-10.4013856986281,
58.1290187197703));
#147205=CARTESIAN_POINT('Ctrl Pts',(80.118829689162,-10.3884913809975,58.1192533088284));
#147206=CARTESIAN_POINT('Ctrl Pts',(80.1601266628084,-10.3754359204086,
58.1094645360177));
#147207=CARTESIAN_POINT('Ctrl Pts',(80.3413664727616,-10.318139489531,58.0665046005249));
#147208=CARTESIAN_POINT('Ctrl Pts',(80.5235305056401,-10.2577417309642,
58.0230937615654));
#147209=CARTESIAN_POINT('Ctrl Pts',(80.7064782053457,-10.1936443957154,
57.9792858696897));
#147210=CARTESIAN_POINT('Ctrl Pts',(80.8895041300135,-10.1295196536633,
57.9354592463914));
#147211=CARTESIAN_POINT('Ctrl Pts',(81.0733151387544,-10.0616917875014,
57.89123506624));
#147212=CARTESIAN_POINT('Ctrl Pts',(81.2577249642791,-9.98953601001032,
57.8466803522544));
#147213=CARTESIAN_POINT('Ctrl Pts',(81.4299851561752,-9.92213413464029,
57.8050610754117));
#147214=CARTESIAN_POINT('Ctrl Pts',(81.6027680171716,-9.85095528252832,
57.7631533837741));
#147215=CARTESIAN_POINT('Ctrl Pts',(81.7758764615611,-9.77547488249053,
57.7210242487723));
#147216=CARTESIAN_POINT('Ctrl Pts',(81.7880859230404,-9.77015119628938,
57.7180528509715));
#147217=CARTESIAN_POINT('Ctrl Pts',(81.8002969836653,-9.76480610695126,
57.7150803570125));
#147218=CARTESIAN_POINT('Ctrl Pts',(81.8125095647161,-9.7594394284026,57.7121067929141));
#147219=CARTESIAN_POINT('Ctrl Pts',(64.2331132192591,-10.03116309748,61.45331963667));
#147220=CARTESIAN_POINT('Ctrl Pts',(64.8063721520591,-10.24997839378,61.35223861989));
#147221=CARTESIAN_POINT('Ctrl Pts',(66.0434889198791,-10.63841202821,61.13410155544));
#147222=CARTESIAN_POINT('Ctrl Pts',(68.0303682092991,-11.08801271264,60.7837611293));
#147223=CARTESIAN_POINT('Ctrl Pts',(70.2942220615191,-11.4211637098,60.38458261477));
#147224=CARTESIAN_POINT('Ctrl Pts',(72.8294884823191,-11.58264132366,59.9375467415));
#147225=CARTESIAN_POINT('Ctrl Pts',(75.4730113240291,-11.49327715213,59.47142234039));
#147226=CARTESIAN_POINT('Ctrl Pts',(77.9968724871491,-11.16992495207,59.02639752177));
#147227=CARTESIAN_POINT('Ctrl Pts',(80.2177679758191,-10.69349944306,58.63479372578));
#147228=CARTESIAN_POINT('Ctrl Pts',(81.5864419160991,-10.2722145784,58.39345958232));
#147229=CARTESIAN_POINT('Ctrl Pts',(82.2177997746791,-10.03126774286,58.28213415737));
#147230=CARTESIAN_POINT('Ctrl Pts',(64.1715173750991,-9.822263906076,60.65197132249));
#147231=CARTESIAN_POINT('Ctrl Pts',(64.7364200849891,-10.03788724212,60.55236373326));
#147232=CARTESIAN_POINT('Ctrl Pts',(65.9600066241391,-10.4222368381,60.33661241318));
#147233=CARTESIAN_POINT('Ctrl Pts',(67.9308405009391,-10.86825461979,59.9891012262));
#147234=CARTESIAN_POINT('Ctrl Pts',(70.1779537377492,-11.19894289262,59.59287453385));
#147235=CARTESIAN_POINT('Ctrl Pts',(72.6937925515491,-11.35916309554,59.14926427186));
#147236=CARTESIAN_POINT('Ctrl Pts',(75.3164862035391,-11.2705174991,58.68681261888));
#147237=CARTESIAN_POINT('Ctrl Pts',(77.8218404664591,-10.94955206463,58.2450510661));
#147238=CARTESIAN_POINT('Ctrl Pts',(80.0252868599591,-10.47682216277,57.8565240163801));
#147239=CARTESIAN_POINT('Ctrl Pts',(81.3794504710091,-10.05980091539,57.61774843546));
#147240=CARTESIAN_POINT('Ctrl Pts',(82.0016116056192,-9.82236568198599,
57.50804464108));
#147241=CARTESIAN_POINT('Ctrl Pts',(64.3417810494792,-9.15894490746699,
60.18227954555));
#147242=CARTESIAN_POINT('Ctrl Pts',(64.8801501889191,-9.36443279080099,
60.08735054068));
#147243=CARTESIAN_POINT('Ctrl Pts',(66.0607741025291,-9.73581431216599,
59.8791746906401));
#147244=CARTESIAN_POINT('Ctrl Pts',(67.9806588733992,-10.17045527885,59.54064720569));
#147245=CARTESIAN_POINT('Ctrl Pts',(70.1746155222091,-10.49332364665,59.153793454));
#147246=CARTESIAN_POINT('Ctrl Pts',(72.6287657256591,-10.6495511842,58.72106055842));
#147247=CARTESIAN_POINT('Ctrl Pts',(75.1853203123391,-10.56318728404,58.27027100713));
#147248=CARTESIAN_POINT('Ctrl Pts',(77.6319094913791,-10.24980056232,57.83887132416));
#147249=CARTESIAN_POINT('Ctrl Pts',(79.7799496563691,-9.78880534654499,
57.4601138874301));
#147250=CARTESIAN_POINT('Ctrl Pts',(81.0880385219991,-9.38532239160899,
57.22946252725));
#147251=CARTESIAN_POINT('Ctrl Pts',(81.6809972375691,-9.15903757193999,
57.12490790725));
#147252=CARTESIAN_POINT('Ctrl Pts',(64.6524871507491,-8.39735190850099,
60.29642878604));
#147253=CARTESIAN_POINT('Ctrl Pts',(65.1603916396291,-8.59120272152199,
60.20687152102));
#147254=CARTESIAN_POINT('Ctrl Pts',(66.2916878016091,-8.94769488368699,
60.0073934845));
#147255=CARTESIAN_POINT('Ctrl Pts',(68.1530751037291,-9.36927350378199,
59.67918068158));
#147256=CARTESIAN_POINT('Ctrl Pts',(70.2859997523291,-9.68316340882398,
59.30308851822));
#147257=CARTESIAN_POINT('Ctrl Pts',(72.6693218717691,-9.83480674783699,
58.88284452484));
#147258=CARTESIAN_POINT('Ctrl Pts',(75.1499385624891,-9.75106258857898,
58.44544487347));
#147259=CARTESIAN_POINT('Ctrl Pts',(77.5290563189391,-9.44637740348698,
58.02594222273));
#147260=CARTESIAN_POINT('Ctrl Pts',(79.6134815477891,-8.99885542575598,
57.65840181561));
#147261=CARTESIAN_POINT('Ctrl Pts',(80.8686694659091,-8.61091652845699,
57.43707831978));
#147262=CARTESIAN_POINT('Ctrl Pts',(81.4280992791691,-8.39743411163299,
57.33843574989));
#147263=CARTESIAN_POINT('',(81.3676320540161,-8.73787997306191,57.3182172534742));
#147264=CARTESIAN_POINT('Origin',(81.6276298114341,-8.73683444149237,58.7943917882984));
#147265=CARTESIAN_POINT('',(64.7026106475202,-8.73788137707176,60.2567101732879));
#147266=CARTESIAN_POINT('Ctrl Pts',(64.7026106495657,-8.73788137707563,
60.2567101848969));
#147267=CARTESIAN_POINT('Ctrl Pts',(64.8615289588377,-8.79636287531833,
60.2286885992441));
#147268=CARTESIAN_POINT('Ctrl Pts',(65.0242194072014,-8.85311144898981,
60.2000018670068));
#147269=CARTESIAN_POINT('Ctrl Pts',(65.1906746728955,-8.9081752454954,60.1706512945918));
#147270=CARTESIAN_POINT('Ctrl Pts',(65.3484303793116,-8.96036120716788,
60.1428346901381));
#147271=CARTESIAN_POINT('Ctrl Pts',(65.5095676690178,-9.01103369452827,
60.1144218212214));
#147272=CARTESIAN_POINT('Ctrl Pts',(65.6740443346344,-9.06026075602945,
60.0854201373193));
#147273=CARTESIAN_POINT('Ctrl Pts',(65.8254175891191,-9.1055660306726,60.0587289391403));
#147274=CARTESIAN_POINT('Ctrl Pts',(65.9796191823325,-9.14964703194275,
60.031539034199));
#147275=CARTESIAN_POINT('Ctrl Pts',(66.1365862032439,-9.19258130032827,
60.0038615123292));
#147276=CARTESIAN_POINT('Ctrl Pts',(66.1994474557214,-9.20977536994396,
59.9927773770751));
#147277=CARTESIAN_POINT('Ctrl Pts',(66.2627518288678,-9.226785877604,59.9816151080364));
#147278=CARTESIAN_POINT('Ctrl Pts',(66.3265033459271,-9.24360804472882,
59.9703739955178));
#147279=CARTESIAN_POINT('Ctrl Pts',(66.5717190342031,-9.3083133173261,59.927135853582));
#147280=CARTESIAN_POINT('Ctrl Pts',(66.8234929969238,-9.37029807677882,
59.8827413125373));
#147281=CARTESIAN_POINT('Ctrl Pts',(67.0820950773821,-9.4293459458507,59.8371427899164));
#147282=CARTESIAN_POINT('Ctrl Pts',(67.3236004841906,-9.48449004838888,
59.7945588720458));
#147283=CARTESIAN_POINT('Ctrl Pts',(67.5710612273839,-9.53707216271436,
59.7509248662921));
#147284=CARTESIAN_POINT('Ctrl Pts',(67.8246519491363,-9.58691921072333,
59.7062099778814));
#147285=CARTESIAN_POINT('Ctrl Pts',(67.8916055025385,-9.60007993272353,
59.6944042594056));
#147286=CARTESIAN_POINT('Ctrl Pts',(67.9589860937402,-9.61305004355902,
59.6825232425739));
#147287=CARTESIAN_POINT('Ctrl Pts',(68.0267963286315,-9.62582647639699,
59.6705664681337));
#147288=CARTESIAN_POINT('Ctrl Pts',(68.0758505082094,-9.63506899608155,
59.6619168924245));
#147289=CARTESIAN_POINT('Ctrl Pts',(68.125129516931,-9.64421016985909,59.6532276733608));
#147290=CARTESIAN_POINT('Ctrl Pts',(68.1746351227241,-9.65324707650833,
59.6444984993631));
#147291=CARTESIAN_POINT('Ctrl Pts',(68.4597847662522,-9.70529917582814,
59.5942189236698));
#147292=CARTESIAN_POINT('Ctrl Pts',(68.7524450534309,-9.75392338446086,
59.5426150331964));
#147293=CARTESIAN_POINT('Ctrl Pts',(69.0526690215057,-9.79862110545472,
59.4896774592567));
#147294=CARTESIAN_POINT('Ctrl Pts',(69.3443409468083,-9.84204558759224,
59.4382478408593));
#147295=CARTESIAN_POINT('Ctrl Pts',(69.6431520356423,-9.88176400622764,
59.3855593785784));
#147296=CARTESIAN_POINT('Ctrl Pts',(69.9491160079193,-9.91728452785944,
59.3316096557762));
#147297=CARTESIAN_POINT('Ctrl Pts',(70.021529525791,-9.92569128865828,59.3188411942243));
#147298=CARTESIAN_POINT('Ctrl Pts',(70.0943435402784,-9.93386275391163,
59.3060021142891));
#147299=CARTESIAN_POINT('Ctrl Pts',(70.1675579135585,-9.941792116299,59.29309244248));
#147300=CARTESIAN_POINT('Ctrl Pts',(70.1976472393991,-9.94505089128939,
59.2877868815067));
#147301=CARTESIAN_POINT('Ctrl Pts',(70.2278041846103,-9.94826877393099,
59.2824693977986));
#147302=CARTESIAN_POINT('Ctrl Pts',(70.2580287970341,-9.95144511113433,
59.2771399831468));
#147303=CARTESIAN_POINT('Ctrl Pts',(70.457293110271,-9.97238601328903,59.2420043084309));
#147304=CARTESIAN_POINT('Ctrl Pts',(70.659489612735,-9.99147794137391,59.2063516429878));
#147305=CARTESIAN_POINT('Ctrl Pts',(70.8649999857744,-10.0084667689348,
59.1701146740796));
#147306=CARTESIAN_POINT('Ctrl Pts',(71.0666836824957,-10.0251392584777,
59.1345524504346));
#147307=CARTESIAN_POINT('Ctrl Pts',(71.2715591381151,-10.039786381797,59.0984274494948));
#147308=CARTESIAN_POINT('Ctrl Pts',(71.4799768039724,-10.0521198835458,
59.061677815081));
#147309=CARTESIAN_POINT('Ctrl Pts',(71.6822225627885,-10.0640881512538,
59.0260164537101));
#147310=CARTESIAN_POINT('Ctrl Pts',(71.8878039703601,-10.073877845892,58.9897668731155));
#147311=CARTESIAN_POINT('Ctrl Pts',(72.0970295004326,-10.0811786262709,
58.9528746912693));
#147312=CARTESIAN_POINT('Ctrl Pts',(72.2571003275373,-10.0867641872365,
58.9246498276029));
#147313=CARTESIAN_POINT('Ctrl Pts',(72.4193039333546,-10.0908920360261,
58.8960488701054));
#147314=CARTESIAN_POINT('Ctrl Pts',(72.5837728363951,-10.0934033137685,
58.8670485590694));
#147315=CARTESIAN_POINT('Ctrl Pts',(72.5889778711876,-10.09348278951,58.8661307708119));
#147316=CARTESIAN_POINT('Ctrl Pts',(72.5941851743727,-10.0935606446403,
58.8652125826667));
#147317=CARTESIAN_POINT('Ctrl Pts',(72.5993947501158,-10.0936368748965,
58.8642939939051));
#147318=CARTESIAN_POINT('Ctrl Pts',(72.7565181226876,-10.0959360170016,
58.8365889040207));
#147319=CARTESIAN_POINT('Ctrl Pts',(72.9157167769922,-10.0969060819709,
58.8085179695934));
#147320=CARTESIAN_POINT('Ctrl Pts',(73.0762555072849,-10.0964561144708,
58.7802107415833));
#147321=CARTESIAN_POINT('Ctrl Pts',(73.2361228133097,-10.0960080288785,
58.752021903446));
#147322=CARTESIAN_POINT('Ctrl Pts',(73.3973188990355,-10.0941517228034,
58.7235987642996));
#147323=CARTESIAN_POINT('Ctrl Pts',(73.5591156265634,-10.0908491089493,
58.695069677654));
#147324=CARTESIAN_POINT('Ctrl Pts',(73.7212252509706,-10.0875401082073,
58.6664854189273));
#147325=CARTESIAN_POINT('Ctrl Pts',(73.8839377243019,-10.0827791874739,
58.6377948239968));
#147326=CARTESIAN_POINT('Ctrl Pts',(74.0465202638102,-10.0765805590394,
58.6091271032536));
#147327=CARTESIAN_POINT('Ctrl Pts',(74.2098916585598,-10.0703518546783,
58.58032028589));
#147328=CARTESIAN_POINT('Ctrl Pts',(74.3731317315009,-10.0626714977316,
58.5515365876632));
#147329=CARTESIAN_POINT('Ctrl Pts',(74.5354983984075,-10.0536067189506,
58.5229068885933));
#147330=CARTESIAN_POINT('Ctrl Pts',(74.6999245212776,-10.0444269626741,
58.4939140509211));
#147331=CARTESIAN_POINT('Ctrl Pts',(74.8634548104611,-10.0338274966925,
58.4650791673765));
#147332=CARTESIAN_POINT('Ctrl Pts',(75.0253219776175,-10.0219315564534,
58.4365375853093));
#147333=CARTESIAN_POINT('Ctrl Pts',(75.0712160880304,-10.0185587069473,
58.4284452059728));
#147334=CARTESIAN_POINT('Ctrl Pts',(75.1169765291583,-10.0150819570383,
58.4203764001192));
#147335=CARTESIAN_POINT('Ctrl Pts',(75.1625858832791,-10.011504868184,58.4123342404151));
#147336=CARTESIAN_POINT('Ctrl Pts',(75.1858092673094,-10.0096834850538,
58.4082393312272));
#147337=CARTESIAN_POINT('Ctrl Pts',(75.2089936066737,-10.0078333411188,
58.4041513080727));
#147338=CARTESIAN_POINT('Ctrl Pts',(75.2321388545488,-10.0059548274891,
58.4000701788148));
#147339=CARTESIAN_POINT('Ctrl Pts',(75.5062487793658,-9.98370752935837,
58.3517372320221));
#147340=CARTESIAN_POINT('Ctrl Pts',(75.7748719275291,-9.95748323024815,
58.3043718338795));
#147341=CARTESIAN_POINT('Ctrl Pts',(76.0379123704695,-9.9278821710273,58.2579907107122));
#147342=CARTESIAN_POINT('Ctrl Pts',(76.3079786025199,-9.89749046989149,
58.2103707514693));
#147343=CARTESIAN_POINT('Ctrl Pts',(76.5721601181975,-9.86353936051064,
58.1637883594333));
#147344=CARTESIAN_POINT('Ctrl Pts',(76.8304008668996,-9.82665083638614,
58.1182535083477));
#147345=CARTESIAN_POINT('Ctrl Pts',(77.0672365918304,-9.79281992319151,
58.0764929437557));
#147346=CARTESIAN_POINT('Ctrl Pts',(77.2990762891904,-9.75651805774799,
58.0356133378304));
#147347=CARTESIAN_POINT('Ctrl Pts',(77.5259085168275,-9.71820412518583,
57.9956166960039));
#147348=CARTESIAN_POINT('Ctrl Pts',(77.5722835992516,-9.71037097114477,
57.98743951774));
#147349=CARTESIAN_POINT('Ctrl Pts',(77.6184484777247,-9.70245252846947,
57.979299404357));
#147350=CARTESIAN_POINT('Ctrl Pts',(77.6644058729966,-9.69445110924848,
57.9711958759488));
#147351=CARTESIAN_POINT('Ctrl Pts',(77.9366797519281,-9.64704682457646,
57.9231866469732));
#147352=CARTESIAN_POINT('Ctrl Pts',(78.2016673585848,-9.59673221438433,
57.8764621844258));
#147353=CARTESIAN_POINT('Ctrl Pts',(78.4598486734758,-9.54366743699993,
57.8309378514623));
#147354=CARTESIAN_POINT('Ctrl Pts',(78.7237453817438,-9.48942795773075,
57.7844057404137));
#147355=CARTESIAN_POINT('Ctrl Pts',(78.9805321306992,-9.43231602864913,
57.7391273064302));
#147356=CARTESIAN_POINT('Ctrl Pts',(79.2307594684004,-9.3724652090838,57.6950054752351));
#147357=CARTESIAN_POINT('Ctrl Pts',(79.3496677215687,-9.3440240464571,57.674038741855));
#147358=CARTESIAN_POINT('Ctrl Pts',(79.4670952051025,-9.31496378084444,
57.6533331082674));
#147359=CARTESIAN_POINT('Ctrl Pts',(79.5831029172942,-9.28529511169891,
57.6328778186374));
#147360=CARTESIAN_POINT('Ctrl Pts',(79.6454199770665,-9.26935768656075,
57.621889639641));
#147361=CARTESIAN_POINT('Ctrl Pts',(79.7073248346892,-9.2532431425775,57.6109741429906));
#147362=CARTESIAN_POINT('Ctrl Pts',(79.768819522112,-9.23695668243318,57.6001309705432));
#147363=CARTESIAN_POINT('Ctrl Pts',(79.9384711523821,-9.19202557324938,
57.5702168111239));
#147364=CARTESIAN_POINT('Ctrl Pts',(80.1049977223805,-9.14578298969952,
57.5408536853916));
#147365=CARTESIAN_POINT('Ctrl Pts',(80.2682871329044,-9.09815175589844,
57.5120613640152));
#147366=CARTESIAN_POINT('Ctrl Pts',(80.4355213763116,-9.04936982128483,
57.482573462345));
#147367=CARTESIAN_POINT('Ctrl Pts',(80.5993602988871,-8.99913154808042,
57.4536842539922));
#147368=CARTESIAN_POINT('Ctrl Pts',(80.7597247279027,-8.94739041898081,
57.4254076950173));
#147369=CARTESIAN_POINT('Ctrl Pts',(80.9258767490569,-8.8937819396599,57.3961106279944));
#147370=CARTESIAN_POINT('Ctrl Pts',(81.0882990124221,-8.83856036728512,
57.3674712197974));
#147371=CARTESIAN_POINT('Ctrl Pts',(81.246945842003,-8.78170943534271,57.3394975102689));
#147372=CARTESIAN_POINT('Ctrl Pts',(81.2874202232777,-8.76720548148913,
57.3323607865908));
#147373=CARTESIAN_POINT('Ctrl Pts',(81.3276490768491,-8.75259564200151,
57.3252673552758));
#147374=CARTESIAN_POINT('Ctrl Pts',(81.36763205815,-8.73787997306976,57.3182172769027));
#147375=CARTESIAN_POINT('Origin',(64.963008146268,-8.7384120949578,61.7339660696974));
#147376=CARTESIAN_POINT('Ctrl Pts',(61.3161921152491,-8.63494495661699,
61.56839581797));
#147377=CARTESIAN_POINT('Ctrl Pts',(61.6689613460491,-8.80141153096799,
61.50619308462));
#147378=CARTESIAN_POINT('Ctrl Pts',(62.3879498808491,-9.12917633459899,
61.3794160071101));
#147379=CARTESIAN_POINT('Ctrl Pts',(63.4646091717291,-9.58075322763798,
61.1895719251));
#147380=CARTESIAN_POINT('Ctrl Pts',(64.1905860164991,-9.85765191546899,
61.06156262));
#147381=CARTESIAN_POINT('Ctrl Pts',(64.5445578719791,-9.98587197454498,
60.99914783146));
#147382=CARTESIAN_POINT('Ctrl Pts',(61.3635047997591,-8.32363710783399,
61.00358429971));
#147383=CARTESIAN_POINT('Ctrl Pts',(61.7136157253391,-8.48884930107399,
60.94185029729));
#147384=CARTESIAN_POINT('Ctrl Pts',(62.4267246286491,-8.813927159173,60.81610995745));
#147385=CARTESIAN_POINT('Ctrl Pts',(63.4936241370291,-9.26140270324298,
60.6279867884201));
#147386=CARTESIAN_POINT('Ctrl Pts',(64.2125417155791,-9.53560504453799,
60.50122222242));
#147387=CARTESIAN_POINT('Ctrl Pts',(64.5629831003891,-9.66254624807698,
60.43942995112));
#147388=CARTESIAN_POINT('Ctrl Pts',(61.5659552580091,-7.78462977649199,
60.70922393812));
#147389=CARTESIAN_POINT('Ctrl Pts',(61.9114635177491,-7.94767009832599,
60.64830150987));
#147390=CARTESIAN_POINT('Ctrl Pts',(62.6143922585991,-8.26809570192399,
60.52435620734));
#147391=CARTESIAN_POINT('Ctrl Pts',(63.6643933998191,-8.70847005284398,
60.33921267637));
#147392=CARTESIAN_POINT('Ctrl Pts',(64.3710883625392,-8.97800386246999,
60.21460328731));
#147393=CARTESIAN_POINT('Ctrl Pts',(64.7154169892491,-9.10273081888299,
60.15388886019));
#147394=CARTESIAN_POINT('Ctrl Pts',(61.8513779092791,-7.21005775654899,
60.7902425591001));
#147395=CARTESIAN_POINT('Ctrl Pts',(62.1919798108591,-7.37078290293399,
60.73018525417));
#147396=CARTESIAN_POINT('Ctrl Pts',(62.8840566835191,-7.68624928777699,
60.60815342879));
#147397=CARTESIAN_POINT('Ctrl Pts',(63.9160444724591,-8.119053895848,60.42618613784));
#147398=CARTESIAN_POINT('Ctrl Pts',(64.6097103488191,-8.38361113555599,
60.30387412824));
#147399=CARTESIAN_POINT('Ctrl Pts',(64.9475228864791,-8.50597774477099,
60.24430866343));
#147400=CARTESIAN_POINT('',(61.8556180259586,-7.547638577278,60.7587117050873));
#147401=CARTESIAN_POINT('Ctrl Pts',(61.8556180259591,-7.54763857727799,
60.75871170509));
#147402=CARTESIAN_POINT('Ctrl Pts',(62.1807441003591,-7.69967237513199,
60.70138320604));
#147403=CARTESIAN_POINT('Ctrl Pts',(62.8258076996291,-7.98759295852699,
60.58764109685));
#147404=CARTESIAN_POINT('Ctrl Pts',(63.7736235103591,-8.38552632889799,
60.42051556228));
#147405=CARTESIAN_POINT('Ctrl Pts',(64.3947998691991,-8.62477639321799,
60.31098549452));
#147406=CARTESIAN_POINT('Ctrl Pts',(64.7026106434291,-8.73788137706399,
60.25671015007));
#147407=CARTESIAN_POINT('',(61.5370694839504,-8.36456075042586,61.1190591594443));
#147408=CARTESIAN_POINT('Ctrl Pts',(61.537069464754,-8.36456080303529,61.1190590948193));
#147409=CARTESIAN_POINT('Ctrl Pts',(61.572528837482,-8.25039306980219,61.0155853898407));
#147410=CARTESIAN_POINT('Ctrl Pts',(61.619097823721,-8.11839868372747,60.9296178865568));
#147411=CARTESIAN_POINT('Ctrl Pts',(61.72823931643,-7.83865781611668,60.8067047653259));
#147412=CARTESIAN_POINT('Ctrl Pts',(61.7906680935864,-7.69127956002283,
60.7699199295052));
#147413=CARTESIAN_POINT('Ctrl Pts',(61.8556180259591,-7.54763857727799,
60.75871170509));
#147414=CARTESIAN_POINT('Ctrl Pts',(61.5375998153948,-8.36381223691337,
61.1200821961353));
#147415=CARTESIAN_POINT('Ctrl Pts',(61.7638676019835,-8.48785590553016,
61.0935564776125));
#147416=CARTESIAN_POINT('Ctrl Pts',(61.9904255296258,-8.60865722923069,
61.0669821445775));
#147417=CARTESIAN_POINT('Ctrl Pts',(62.2172365718248,-8.72616597744292,
61.0403576980771));
#147418=CARTESIAN_POINT('Ctrl Pts',(62.4543428442658,-8.84900859126664,
61.0125247354297));
#147419=CARTESIAN_POINT('Ctrl Pts',(62.6917262477102,-8.96825216347004,
60.9846367825683));
#147420=CARTESIAN_POINT('Ctrl Pts',(62.92930835593,-9.08381469527325,60.9566563455559));
#147421=CARTESIAN_POINT('Ctrl Pts',(63.1774284872662,-9.20450303659402,
60.9274348281683));
#147422=CARTESIAN_POINT('Ctrl Pts',(63.42576597902,-9.32117554294915,60.8981120121884));
#147423=CARTESIAN_POINT('Ctrl Pts',(63.6741838693174,-9.43372663307082,
60.8686121173679));
#147424=CARTESIAN_POINT('Ctrl Pts',(63.9226017596147,-9.54627772319248,
60.8391122225473));
#147425=CARTESIAN_POINT('Ctrl Pts',(64.1711003449158,-9.65470638105591,
60.8094345145158));
#147426=CARTESIAN_POINT('Ctrl Pts',(64.4194894281585,-9.75891075203393,
60.7794801263297));
#147427=CARTESIAN_POINT('Ctrl Pts',(59.3595940627791,-9.91651499671599,
62.64129792143));
#147428=CARTESIAN_POINT('Ctrl Pts',(61.9983506403891,-7.63333700038399,
61.37410443204));
#147429=CARTESIAN_POINT('Ctrl Pts',(63.8659696541791,-6.480223454794,58.3422073918001));
#147430=CARTESIAN_POINT('Ctrl Pts',(64.2231073245191,-6.94208487257399,
54.61475371526));
#147431=CARTESIAN_POINT('Ctrl Pts',(60.3806855157591,-10.72894715554,62.78026368079));
#147432=CARTESIAN_POINT('Ctrl Pts',(62.7316376310391,-8.36267113991899,
61.44466582565));
#147433=CARTESIAN_POINT('Ctrl Pts',(64.4149724654791,-7.13948508442198,
58.48833863363));
#147434=CARTESIAN_POINT('Ctrl Pts',(64.8063219458291,-7.53992389692399,
54.8938706937));
#147435=CARTESIAN_POINT('Ctrl Pts',(61.5100324248391,-11.44895486624,62.90864202214));
#147436=CARTESIAN_POINT('Ctrl Pts',(63.5792248770391,-9.04876204197899,
61.51862151364));
#147437=CARTESIAN_POINT('Ctrl Pts',(65.0678444367891,-7.77042731743899,
58.6411780333901));
#147438=CARTESIAN_POINT('Ctrl Pts',(65.4595128993991,-8.081181454842,55.1748163377));
#147439=CARTESIAN_POINT('Ctrl Pts',(62.7519440770891,-12.07793713058,63.001930692665));
#147440=CARTESIAN_POINT('Ctrl Pts',(64.5506391796491,-9.66794220213098,
61.5739182200701));
#147441=CARTESIAN_POINT('Ctrl Pts',(65.8341505913691,-8.345140508031,58.7751971799));
#147442=CARTESIAN_POINT('Ctrl Pts',(66.1846613547391,-8.56004330716699,
55.4275781765));
#147443=CARTESIAN_POINT('',(59.6330689813191,-9.92669794294899,62.60067797587));
#147444=CARTESIAN_POINT('Origin',(59.0283126277726,-11.8776332136077,56.407512485888));
#147445=CARTESIAN_POINT('Ctrl Pts',(62.6710204155491,-11.87440155793,62.91980324276));
#147446=CARTESIAN_POINT('Ctrl Pts',(61.5797032381311,-11.3041158507879,
62.8377246971986));
#147447=CARTESIAN_POINT('Ctrl Pts',(60.5660753810985,-10.656617993369,62.7258066167314));
#147448=CARTESIAN_POINT('Ctrl Pts',(59.6330689813191,-9.92669794294899,
62.60067797587));
#147449=CARTESIAN_POINT('Origin',(48.9523887185591,1.4210854715202E-14,
90.52409909588));
#147450=CARTESIAN_POINT('',(59.6330698027491,9.92669722269101,62.60067754791));
#147451=CARTESIAN_POINT('Ctrl Pts',(59.6330689813191,-9.92669794294899,
62.60067797587));
#147452=CARTESIAN_POINT('Ctrl Pts',(58.8256240021749,-9.29268345738896,
62.4965871587399));
#147453=CARTESIAN_POINT('Ctrl Pts',(58.1121214390089,-8.59697796096149,
62.3761470806078));
#147454=CARTESIAN_POINT('Ctrl Pts',(57.1869930364504,-7.45620088899646,
62.1948494800253));
#147455=CARTESIAN_POINT('Ctrl Pts',(56.9028114774077,-7.0597600374091,62.1343504064346));
#147456=CARTESIAN_POINT('Ctrl Pts',(56.5133433337057,-6.44066295576373,
62.0464075659451));
#147457=CARTESIAN_POINT('Ctrl Pts',(56.3278109528225,-6.12500857788751,
62.0031412305677));
#147458=CARTESIAN_POINT('Ctrl Pts',(56.1275782079375,-5.74606076495384,
61.9545711474323));
#147459=CARTESIAN_POINT('Ctrl Pts',(56.0315325883226,-5.55391891982303,
61.9308498620689));
#147460=CARTESIAN_POINT('Ctrl Pts',(55.9912441373022,-5.47100113770906,
61.920813777626));
#147461=CARTESIAN_POINT('Ctrl Pts',(55.9645795676856,-5.4155957217327,61.9141530327728));
#147462=CARTESIAN_POINT('Ctrl Pts',(55.9504938767487,-5.38602774362974,
61.9106239994492));
#147463=CARTESIAN_POINT('Ctrl Pts',(55.5450166264099,-4.52711198014621,
61.8087787806478));
#147464=CARTESIAN_POINT('Ctrl Pts',(55.2489854890233,-3.66087265800569,
61.726882166269));
#147465=CARTESIAN_POINT('Ctrl Pts',(54.8540101262023,-1.86737516575817,
61.6125178560279));
#147466=CARTESIAN_POINT('Ctrl Pts',(54.7550696578738,-0.939068762628913,
61.5800655192276));
#147467=CARTESIAN_POINT('Ctrl Pts',(54.7571025726164,0.965762057650877,
61.5806459286186));
#147468=CARTESIAN_POINT('Ctrl Pts',(54.8576920430293,1.89157838449658,61.6136107485148));
#147469=CARTESIAN_POINT('Ctrl Pts',(55.1557894049005,3.23393920163968,61.6998972699383));
#147470=CARTESIAN_POINT('Ctrl Pts',(55.2796908290689,3.67369113242594,61.7347999542579));
#147471=CARTESIAN_POINT('Ctrl Pts',(55.5020817713188,4.32117592818264,61.7948638456308));
#147472=CARTESIAN_POINT('Ctrl Pts',(55.6224120031278,4.64188471197103,61.8268235931936));
#147473=CARTESIAN_POINT('Ctrl Pts',(55.778725961735,5.01062902444841,61.8671595443865));
#147474=CARTESIAN_POINT('Ctrl Pts',(55.8608580366601,5.19363538838132,61.8880497823729));
#147475=CARTESIAN_POINT('Ctrl Pts',(55.896908547343,5.27177278704354,61.8971532233772));
#147476=CARTESIAN_POINT('Ctrl Pts',(55.9211312595259,5.3237989424665,61.9032551490484));
#147477=CARTESIAN_POINT('Ctrl Pts',(55.93249072425,5.34799379679885,61.9061103997539));
#147478=CARTESIAN_POINT('Ctrl Pts',(56.7870303300843,7.15064334101463,62.1203429205986));
#147479=CARTESIAN_POINT('Ctrl Pts',(58.0232520392425,8.66387025801734,62.3909057621657));
#147480=CARTESIAN_POINT('Ctrl Pts',(59.6330698027491,9.92669722269101,62.60067754791));
#147481=CARTESIAN_POINT('Ctrl Pts',(59.6330698027491,9.92669722269101,62.60067754791));
#147482=CARTESIAN_POINT('Ctrl Pts',(60.5660767630722,10.6566178221567,62.7258062817894));
#147483=CARTESIAN_POINT('Ctrl Pts',(61.5797045052489,11.304115765727,62.8377244443988));
#147484=CARTESIAN_POINT('Ctrl Pts',(62.6710208743191,11.87440113975,62.91980295862));
#147485=CARTESIAN_POINT('Ctrl Pts',(-3.58430183424491,-12.77734752092,56.71623037308));
#147486=CARTESIAN_POINT('Ctrl Pts',(-2.82654579637091,-13.56823877579,56.66356760301));
#147487=CARTESIAN_POINT('Ctrl Pts',(-1.22510960093091,-14.96301005098,56.57763219321));
#147488=CARTESIAN_POINT('Ctrl Pts',(1.36103340034909,-16.52464473566,56.54069563469));
#147489=CARTESIAN_POINT('Ctrl Pts',(3.87584585923909,-17.55452762874,56.60358098145));
#147490=CARTESIAN_POINT('Ctrl Pts',(6.19710063835909,-18.15797232338,56.74716429009));
#147491=CARTESIAN_POINT('Ctrl Pts',(8.31505282592909,-18.45204200109,56.94959224141));
#147492=CARTESIAN_POINT('Ctrl Pts',(10.3190076082391,-18.5227178858,57.20308600798));
#147493=CARTESIAN_POINT('Ctrl Pts',(12.2966611152891,-18.39728886114,57.51358361024));
#147494=CARTESIAN_POINT('Ctrl Pts',(14.2762842352891,-18.07077538528,57.88694259276));
#147495=CARTESIAN_POINT('Ctrl Pts',(16.1913087147191,-17.5550687573,58.30881641828));
#147496=CARTESIAN_POINT('Ctrl Pts',(18.0106355730791,-16.87094604643,58.76532096745));
#147497=CARTESIAN_POINT('Ctrl Pts',(19.7936798013391,-16.00018983021,59.26535024511));
#147498=CARTESIAN_POINT('Ctrl Pts',(21.6152587953191,-14.87219739396,59.8316118168));
#147499=CARTESIAN_POINT('Ctrl Pts',(23.5037332083091,-13.38226243744,60.48072054854));
#147500=CARTESIAN_POINT('Ctrl Pts',(25.4089773760291,-11.42609024385,61.20195839564));
#147501=CARTESIAN_POINT('Ctrl Pts',(27.1843832993891,-8.93696435445999,
61.93748494782));
#147502=CARTESIAN_POINT('Ctrl Pts',(28.5837262234791,-5.98779183204199,
62.56306222481));
#147503=CARTESIAN_POINT('Ctrl Pts',(29.4131721215591,-2.80038937228799,
62.95281639517));
#147504=CARTESIAN_POINT('Ctrl Pts',(29.5612752799991,-0.620166171525686,
63.023935917286));
#147505=CARTESIAN_POINT('Ctrl Pts',(29.5343220504091,0.444915684091514,
63.011087634094));
#147506=CARTESIAN_POINT('Ctrl Pts',(29.5338703742191,0.461774656562614,
63.0108722771));
#147507=CARTESIAN_POINT('Ctrl Pts',(-3.72288960953291,-12.85329830414,55.62299833527));
#147508=CARTESIAN_POINT('Ctrl Pts',(-2.94901860386991,-13.64890746123,55.56862071173));
#147509=CARTESIAN_POINT('Ctrl Pts',(-1.31349980804092,-15.05199668853,55.47970165767));
#147510=CARTESIAN_POINT('Ctrl Pts',(1.32767713553909,-16.6228801163,55.44051598947));
#147511=CARTESIAN_POINT('Ctrl Pts',(3.89588111527909,-17.65877088157,55.5036943663299));
#147512=CARTESIAN_POINT('Ctrl Pts',(6.26621663463909,-18.26566107639,55.64967374489));
#147513=CARTESIAN_POINT('Ctrl Pts',(8.42872386496909,-18.56136755362,55.8560400985301));
#147514=CARTESIAN_POINT('Ctrl Pts',(10.4746065168291,-18.63242271852,56.11476044379));
#147515=CARTESIAN_POINT('Ctrl Pts',(12.4933994745791,-18.50631935278,56.431858726));
#147516=CARTESIAN_POINT('Ctrl Pts',(14.5139561217791,-18.17810478474,56.81330363737));
#147517=CARTESIAN_POINT('Ctrl Pts',(16.4683569012591,-17.65977495691,57.24442226139));
#147518=CARTESIAN_POINT('Ctrl Pts',(18.3249224039791,-16.97222998037,57.71101147142));
#147519=CARTESIAN_POINT('Ctrl Pts',(20.1443477633591,-16.09715278017,58.22215868751));
#147520=CARTESIAN_POINT('Ctrl Pts',(22.0030374225591,-14.96355146807,58.80109378072));
#147521=CARTESIAN_POINT('Ctrl Pts',(23.9300250610891,-13.46607983077,59.4648497644901));
#147522=CARTESIAN_POINT('Ctrl Pts',(25.8743271231091,-11.49961504094,60.20254853862));
#147523=CARTESIAN_POINT('Ctrl Pts',(27.6865453689491,-8.99647741870398,
60.9551385269801));
#147524=CARTESIAN_POINT('Ctrl Pts',(29.1154374711391,-6.02908615362698,
61.59554524518));
#147525=CARTESIAN_POINT('Ctrl Pts',(29.9627342908991,-2.82017517727099,
61.99473019848));
#147526=CARTESIAN_POINT('Ctrl Pts',(30.1140601046791,-0.624535642130786,
62.06759020103));
#147527=CARTESIAN_POINT('Ctrl Pts',(30.0865221951591,0.448052485067714,
62.05442854821));
#147528=CARTESIAN_POINT('Ctrl Pts',(30.0860607192791,0.465030265795814,
62.05420793871));
#147529=CARTESIAN_POINT('Ctrl Pts',(-3.17320105054691,-12.28484166745,54.85174559045));
#147530=CARTESIAN_POINT('Ctrl Pts',(-2.42508695642091,-13.04513949903,54.80503919576));
#147531=CARTESIAN_POINT('Ctrl Pts',(-0.844253174050915,-14.3859726853,54.73047035947));
#147532=CARTESIAN_POINT('Ctrl Pts',(1.70866986857909,-15.8876335301,54.70700946437));
#147533=CARTESIAN_POINT('Ctrl Pts',(4.19228482572909,-16.87855813869,54.77837472681));
#147534=CARTESIAN_POINT('Ctrl Pts',(6.48653288913908,-17.45966035134,54.92597342556));
#147535=CARTESIAN_POINT('Ctrl Pts',(8.58186134395909,-17.74311613794,55.12908301981));
#147536=CARTESIAN_POINT('Ctrl Pts',(10.5664452653491,-17.81133256526,55.38081209437));
#147537=CARTESIAN_POINT('Ctrl Pts',(12.5270981927391,-17.69027633198,55.68738173201));
#147538=CARTESIAN_POINT('Ctrl Pts',(14.4918977503591,-17.37479365556,56.05469422228));
#147539=CARTESIAN_POINT('Ctrl Pts',(16.3945506037791,-16.87609727056,56.4687746378201));
#147540=CARTESIAN_POINT('Ctrl Pts',(18.2036342066391,-16.21416637664,56.91612646381));
#147541=CARTESIAN_POINT('Ctrl Pts',(19.9776601847591,-15.37142975168,57.40549259896));
#147542=CARTESIAN_POINT('Ctrl Pts',(21.7905301121891,-14.27980829232,57.95894164));
#147543=CARTESIAN_POINT('Ctrl Pts',(23.6696227303091,-12.83874523999,58.59230118133));
#147544=CARTESIAN_POINT('Ctrl Pts',(25.5636008457491,-10.94931579331,59.29438635056));
#147545=CARTESIAN_POINT('Ctrl Pts',(27.3248106085391,-8.55104953890899,
60.00792469414));
#147546=CARTESIAN_POINT('Ctrl Pts',(28.7082158942091,-5.72001717281198,
60.61198629947));
#147547=CARTESIAN_POINT('Ctrl Pts',(29.5252295808991,-2.67208753843899,
60.98663314509));
#147548=CARTESIAN_POINT('Ctrl Pts',(29.6707996220691,-0.591832166815786,
61.0548216514));
#147549=CARTESIAN_POINT('Ctrl Pts',(29.6442913120391,0.424574974273814,
61.04249344665));
#147550=CARTESIAN_POINT('Ctrl Pts',(29.6438471072391,0.440663529910414,
61.04228680651));
#147551=CARTESIAN_POINT('Ctrl Pts',(-2.38244347352091,-11.53445397631,55.02993629904));
#147552=CARTESIAN_POINT('Ctrl Pts',(-1.68100325115091,-12.24813930956,54.99404617299));
#147553=CARTESIAN_POINT('Ctrl Pts',(-0.199132288740913,-13.50679179131,
54.93948658306));
#147554=CARTESIAN_POINT('Ctrl Pts',(2.19404928560909,-14.91707579071,54.93693122039));
#147555=CARTESIAN_POINT('Ctrl Pts',(4.52391333623909,-15.8486431004,55.0177166612));
#147556=CARTESIAN_POINT('Ctrl Pts',(6.67880783080909,-16.3957040456,55.16484050833));
#147557=CARTESIAN_POINT('Ctrl Pts',(8.6498779854791,-16.6629883833,55.36014776661));
#147558=CARTESIAN_POINT('Ctrl Pts',(10.5198070717491,-16.72745755252,55.5983555735));
#147559=CARTESIAN_POINT('Ctrl Pts',(12.3703411755791,-16.61306375545,55.88583297768));
#147560=CARTESIAN_POINT('Ctrl Pts',(14.2280550377091,-16.31438773435,56.22829233863));
#147561=CARTESIAN_POINT('Ctrl Pts',(16.0299360351191,-15.84160835493,56.61291322706));
#147562=CARTESIAN_POINT('Ctrl Pts',(17.7454468009191,-15.21348917344,57.02735648449));
#147563=CARTESIAN_POINT('Ctrl Pts',(19.4292282283691,-14.41344352614,57.47976284219));
#147564=CARTESIAN_POINT('Ctrl Pts',(21.1506253523991,-13.37723731351,57.99030081481));
#147565=CARTESIAN_POINT('Ctrl Pts',(22.9343804115591,-12.01063606723,58.57294969782));
#147566=CARTESIAN_POINT('Ctrl Pts',(24.7295945359991,-10.22289665205,59.2163207090301));
#147567=CARTESIAN_POINT('Ctrl Pts',(26.3934737214891,-7.96306520251299,
59.86646337428));
#147568=CARTESIAN_POINT('Ctrl Pts',(27.6933626732391,-5.31203256334299,
60.41257442068));
#147569=CARTESIAN_POINT('Ctrl Pts',(28.4565964661691,-2.47660536052199,
60.74867761106));
#147570=CARTESIAN_POINT('Ctrl Pts',(28.5921150013391,-0.548662145128386,
60.80958320983));
#147571=CARTESIAN_POINT('Ctrl Pts',(28.5674129242191,0.393583630375914,
60.79855720673));
#147572=CARTESIAN_POINT('Ctrl Pts',(28.5669990101191,0.408498369893214,
60.79837239285));
#147573=CARTESIAN_POINT('',(25.6004794355172,-11.218697295749,60.475052154922));
#147574=CARTESIAN_POINT('',(25.5799831827151,-11.2436247403821,60.4681283373529));
#147575=CARTESIAN_POINT('Origin',(21.9145513802835,-0.849633245104839,64.0093316151609));
#147576=CARTESIAN_POINT('',(28.8585550967729,1.26413730018565E-6,60.8967821146319));
#147577=CARTESIAN_POINT('Origin',(28.2409971615791,4.54795488838455E-7,
62.26375785167));
#147578=CARTESIAN_POINT('Ctrl Pts',(24.9372765286891,-10.33197973489,59.27186775219));
#147579=CARTESIAN_POINT('Ctrl Pts',(25.0884729081682,-10.1544298226021,
59.3290195277117));
#147580=CARTESIAN_POINT('Ctrl Pts',(25.2354201309973,-9.9748009926422,59.3851860135425));
#147581=CARTESIAN_POINT('Ctrl Pts',(25.5208782555178,-9.61138944051975,
59.4953766986517));
#147582=CARTESIAN_POINT('Ctrl Pts',(25.6598691932805,-9.42681391865182,
59.5495917842428));
#147583=CARTESIAN_POINT('Ctrl Pts',(25.8594487747258,-9.15113148708486,
59.6281484626401));
#147584=CARTESIAN_POINT('Ctrl Pts',(25.9245460860465,-9.05934679202463,
59.6538934847045));
#147585=CARTESIAN_POINT('Ctrl Pts',(26.0518918830672,-8.87599629949502,
59.7044763172425));
#147586=CARTESIAN_POINT('Ctrl Pts',(26.1136416461275,-8.7852514273904,59.7291135015114));
#147587=CARTESIAN_POINT('Ctrl Pts',(26.2377099140975,-8.59835774438392,
59.7788244733545));
#147588=CARTESIAN_POINT('Ctrl Pts',(26.3309422684908,-8.45454220553908,
59.8163406575038));
#147589=CARTESIAN_POINT('Ctrl Pts',(26.4244444582738,-8.30525875180928,
59.8542091925063));
#147590=CARTESIAN_POINT('Ctrl Pts',(26.4868390017902,-8.20452135712609,
59.8795335075995));
#147591=CARTESIAN_POINT('Ctrl Pts',(26.5169758557494,-8.15534444186653,
59.8917905523518));
#147592=CARTESIAN_POINT('Ctrl Pts',(26.8081007315441,-7.67489638239888,
60.0104588863508));
#147593=CARTESIAN_POINT('Ctrl Pts',(27.0450450385791,-7.24149359007942,
60.1089036136706));
#147594=CARTESIAN_POINT('Ctrl Pts',(27.3681375817506,-6.58188262574454,
60.2449193946893));
#147595=CARTESIAN_POINT('Ctrl Pts',(27.4704472110256,-6.36042784165697,
60.2883182251975));
#147596=CARTESIAN_POINT('Ctrl Pts',(27.6643543418031,-5.9143493481966,60.3710792742253));
#147597=CARTESIAN_POINT('Ctrl Pts',(27.7564152946973,-5.6885104661461,60.4106417290895));
#147598=CARTESIAN_POINT('Ctrl Pts',(27.9280295321704,-5.2385244674707,60.4847886476882));
#147599=CARTESIAN_POINT('Ctrl Pts',(28.0492171779347,-4.89688936050973,
60.5374646811016));
#147600=CARTESIAN_POINT('Ctrl Pts',(28.1591754869717,-4.54903584161711,
60.5856085834238));
#147601=CARTESIAN_POINT('Ctrl Pts',(28.229991130401,-4.31575162637056,60.6166845351935));
#147602=CARTESIAN_POINT('Ctrl Pts',(28.2647375028393,-4.19632677709933,
60.6319696429302));
#147603=CARTESIAN_POINT('Ctrl Pts',(28.3617489734771,-3.84853026724173,
60.6747331281475));
#147604=CARTESIAN_POINT('Ctrl Pts',(28.4205039887194,-3.61803496350203,
60.7007531586585));
#147605=CARTESIAN_POINT('Ctrl Pts',(28.5262194626522,-3.15978242835333,
60.7477144820933));
#147606=CARTESIAN_POINT('Ctrl Pts',(28.573570911436,-2.92987058514986,60.7688305329133));
#147607=CARTESIAN_POINT('Ctrl Pts',(28.7770209552515,-1.80870266790406,
60.8597651208632));
#147608=CARTESIAN_POINT('Ctrl Pts',(28.8583068535147,-0.906823667388817,
60.8966776934278));
#147609=CARTESIAN_POINT('Ctrl Pts',(28.8585550967491,1.26413730024185E-6,
60.89678211462));
#147610=CARTESIAN_POINT('Origin',(27.8340462222691,-10.33198915989,80.111318784329));
#147611=CARTESIAN_POINT('',(25.5859599196424,-11.2434451392657,60.5013612007571));
#147612=CARTESIAN_POINT('Ctrl Pts',(25.5859731978904,-11.2434554550835,
60.5013588594437));
#147613=CARTESIAN_POINT('Ctrl Pts',(25.5617439507817,-11.2756175802506,
60.5056541712706));
#147614=CARTESIAN_POINT('Ctrl Pts',(25.5355170543215,-11.3077304797386,
60.5102892020757));
#147615=CARTESIAN_POINT('Ctrl Pts',(25.5071495594106,-11.3395024335167,
60.5152935580816));
#147616=CARTESIAN_POINT('Ctrl Pts',(25.4797518807739,-11.3701881807781,
60.5201268272181));
#147617=CARTESIAN_POINT('Ctrl Pts',(25.450357033342,-11.400555707154,60.5253046767574));
#147618=CARTESIAN_POINT('Ctrl Pts',(25.4188616887057,-11.430302309678,60.5308492906578));
#147619=CARTESIAN_POINT('Ctrl Pts',(25.3876284774293,-11.4598013334899,
60.536347757158));
#147620=CARTESIAN_POINT('Ctrl Pts',(25.3543290304519,-11.4886896256522,
60.5422070066329));
#147621=CARTESIAN_POINT('Ctrl Pts',(25.3188954936569,-11.5166339195595,
60.5484428698022));
#147622=CARTESIAN_POINT('Ctrl Pts',(25.2851308147859,-11.5432620858504,
60.5543850346674));
#147623=CARTESIAN_POINT('Ctrl Pts',(25.2494225844771,-11.569035071514,60.560670192729));
#147624=CARTESIAN_POINT('Ctrl Pts',(25.2117913961462,-11.5936084226505,
60.567294816086));
#147625=CARTESIAN_POINT('Ctrl Pts',(25.1746664986275,-11.6178511633954,
60.5738303116187));
#147626=CARTESIAN_POINT('Ctrl Pts',(25.1356698214058,-11.6409258437336,
60.5806962377468));
#147627=CARTESIAN_POINT('Ctrl Pts',(25.0948699814531,-11.662492632175,60.587880594608));
#147628=CARTESIAN_POINT('Ctrl Pts',(25.0547695127091,-11.6836897331148,
60.5949418006837));
#147629=CARTESIAN_POINT('Ctrl Pts',(25.0129270804413,-11.7034296793926,
60.6023106299535));
#147630=CARTESIAN_POINT('Ctrl Pts',(24.969457530366,-11.721388378979,60.6099669261679));
#147631=CARTESIAN_POINT('Ctrl Pts',(24.9583766179001,-11.7259662680479,
60.6119186083919));
#147632=CARTESIAN_POINT('Ctrl Pts',(24.9471902337381,-11.7304284263342,
60.6138889246517));
#147633=CARTESIAN_POINT('Ctrl Pts',(24.9359008166787,-11.7347695342002,
60.615877446481));
#147634=CARTESIAN_POINT('Ctrl Pts',(24.8950689026342,-11.7504705878782,
60.6230695939568));
#147635=CARTESIAN_POINT('Ctrl Pts',(24.8528848469115,-11.7645863342241,
60.6305006701846));
#147636=CARTESIAN_POINT('Ctrl Pts',(24.8095371872525,-11.7768605936715,
60.6381374890892));
#147637=CARTESIAN_POINT('Ctrl Pts',(24.7664707110653,-11.7890552336211,
60.6457247702041));
#147638=CARTESIAN_POINT('Ctrl Pts',(24.7222559707473,-11.7994316951804,
60.6535150818304));
#147639=CARTESIAN_POINT('Ctrl Pts',(24.6771182451751,-11.8077693443997,
60.6614687583141));
#147640=CARTESIAN_POINT('Ctrl Pts',(24.6323179488033,-11.8160446651282,
60.6693629767134));
#147641=CARTESIAN_POINT('Ctrl Pts',(24.5866088138828,-11.8223111141212,
60.6774180563243));
#147642=CARTESIAN_POINT('Ctrl Pts',(24.5402458485445,-11.8263901448243,
60.6855890881521));
#147643=CARTESIAN_POINT('Ctrl Pts',(24.5118636392179,-11.8288872220156,
60.6905911826916));
#147644=CARTESIAN_POINT('Ctrl Pts',(24.4832370623221,-11.8305653058195,
60.6956366147681));
#147645=CARTESIAN_POINT('Ctrl Pts',(24.4544300514047,-11.8313913716027,
60.700714123978));
#147646=CARTESIAN_POINT('Ctrl Pts',(24.4102349808851,-11.8326587032134,
60.7085039248094));
#147647=CARTESIAN_POINT('Ctrl Pts',(24.3656202037618,-11.8319176257155,
60.7163683549808));
#147648=CARTESIAN_POINT('Ctrl Pts',(24.3208617900099,-11.8290857387875,
60.724258732631));
#147649=CARTESIAN_POINT('Ctrl Pts',(24.2762129275026,-11.8262607832209,
60.7321297976958));
#147650=CARTESIAN_POINT('Ctrl Pts',(24.2314217272845,-11.8213550940037,
60.7400265781715));
#147651=CARTESIAN_POINT('Ctrl Pts',(24.1867724304541,-11.8143375855243,
60.7478989514316));
#147652=CARTESIAN_POINT('Ctrl Pts',(24.1421965809794,-11.8073316207304,
60.7557583747677));
#147653=CARTESIAN_POINT('Ctrl Pts',(24.0977627877234,-11.7982207526536,
60.763593361921));
#147654=CARTESIAN_POINT('Ctrl Pts',(24.0537549386197,-11.7870259624055,
60.7713538525533));
#147655=CARTESIAN_POINT('Ctrl Pts',(24.015060944415,-11.7771829194528,60.7781772803205));
#147656=CARTESIAN_POINT('Ctrl Pts',(23.9766965226053,-11.7657296368449,
60.784943066333));
#147657=CARTESIAN_POINT('Ctrl Pts',(23.938849578094,-11.7527133111511,60.791618075687));
#147658=CARTESIAN_POINT('Ctrl Pts',(23.8958012397551,-11.7379081214686,
60.7992104471397));
#147659=CARTESIAN_POINT('Ctrl Pts',(23.8534319854631,-11.7210830022974,
60.8066836786859));
#147660=CARTESIAN_POINT('Ctrl Pts',(23.8120016585327,-11.7023562910476,
60.8139918950497));
#147661=CARTESIAN_POINT('Ctrl Pts',(23.7705439333247,-11.6836171956418,
60.8213049444079));
#147662=CARTESIAN_POINT('Ctrl Pts',(23.7300269189893,-11.6629743125864,
60.828452664821));
#147663=CARTESIAN_POINT('Ctrl Pts',(23.6906856655416,-11.6405917607177,
60.8353935526258));
#147664=CARTESIAN_POINT('Ctrl Pts',(23.6512108294834,-11.6181332092444,
60.8423580081067));
#147665=CARTESIAN_POINT('Ctrl Pts',(23.61292023339,-11.5939235627926,60.8491141391936));
#147666=CARTESIAN_POINT('Ctrl Pts',(23.5760181235856,-11.5681689960332,
60.8556258731524));
#147667=CARTESIAN_POINT('Ctrl Pts',(23.5436778970136,-11.5455982398168,
60.8613326187212));
#147668=CARTESIAN_POINT('Ctrl Pts',(23.5124037313837,-11.5218417453141,
60.8668517195986));
#147669=CARTESIAN_POINT('Ctrl Pts',(23.4823083059907,-11.4970595304308,
60.8721632679438));
#147670=CARTESIAN_POINT('Ctrl Pts',(23.4457177470307,-11.4669288682786,
60.8786211438621));
#147671=CARTESIAN_POINT('Ctrl Pts',(23.4108755040482,-11.4352865540032,
60.8847711606764));
#147672=CARTESIAN_POINT('Ctrl Pts',(23.3779075667015,-11.4024230541389,
60.8905910114592));
#147673=CARTESIAN_POINT('Ctrl Pts',(23.3447898798322,-11.369410279136,60.8964372976198));
#147674=CARTESIAN_POINT('Ctrl Pts',(23.3135636764316,-11.3351657988586,
60.9019503917891));
#147675=CARTESIAN_POINT('Ctrl Pts',(23.2843063996213,-11.2999978236278,
60.9071165458509));
#147676=CARTESIAN_POINT('Ctrl Pts',(23.2547721708609,-11.264496945257,60.9123316031803));
#147677=CARTESIAN_POINT('Ctrl Pts',(23.2272443510674,-11.2280556116708,
60.9171931157136));
#147678=CARTESIAN_POINT('Ctrl Pts',(23.2017503470999,-11.1909957260633,
60.9216961554168));
#147679=CARTESIAN_POINT('Ctrl Pts',(23.1863525897707,-11.1686124579834,
60.9244158816976));
#147680=CARTESIAN_POINT('Ctrl Pts',(23.1716957239107,-11.1460036003936,
60.9270050212694));
#147681=CARTESIAN_POINT('Ctrl Pts',(23.1577767525345,-11.1232395308346,
60.9294640815484));
#147682=CARTESIAN_POINT('Ctrl Pts',(23.1327166558873,-11.0822544775707,
60.9338914409119));
#147683=CARTESIAN_POINT('Ctrl Pts',(23.1100497867108,-11.0407673431689,
60.9378969026038));
#147684=CARTESIAN_POINT('Ctrl Pts',(23.0896832982784,-10.9991169831627,
60.9414967508537));
#147685=CARTESIAN_POINT('Ctrl Pts',(23.0690722941755,-10.9569665779111,
60.9451398181057));
#147686=CARTESIAN_POINT('Ctrl Pts',(23.0508168200725,-10.9146493658429,
60.9483675477527));
#147687=CARTESIAN_POINT('Ctrl Pts',(23.0347783054181,-10.8724843186724,
60.9512042831912));
#147688=CARTESIAN_POINT('Ctrl Pts',(23.0184359877794,-10.8295205773937,
60.9540947523269));
#147689=CARTESIAN_POINT('Ctrl Pts',(23.0043949684957,-10.7867151439778,
60.9565793528));
#147690=CARTESIAN_POINT('Ctrl Pts',(22.9924714929908,-10.7443668699682,
60.9586903899386));
#147691=CARTESIAN_POINT('Ctrl Pts',(22.9895840444815,-10.7341115999663,
60.9592016092586));
#147692=CARTESIAN_POINT('Ctrl Pts',(22.9868206267988,-10.7238829530939,
60.9596909478518));
#147693=CARTESIAN_POINT('Ctrl Pts',(22.9841783578299,-10.7136848126932,
60.9601589125555));
#147694=CARTESIAN_POINT('Ctrl Pts',(22.9727445921569,-10.6695548815562,
60.9621839141084));
#147695=CARTESIAN_POINT('Ctrl Pts',(22.9635782890116,-10.6259943202261,
60.9638088760509));
#147696=CARTESIAN_POINT('Ctrl Pts',(22.9564244603178,-10.5832263381758,
60.9650802235541));
#147697=CARTESIAN_POINT('Ctrl Pts',(22.9490201628826,-10.5389609701676,
60.9663960832789));
#147698=CARTESIAN_POINT('Ctrl Pts',(22.9437711795339,-10.495544595905,60.9673332303685));
#147699=CARTESIAN_POINT('Ctrl Pts',(22.940391170487,-10.4531675797244,60.9679437773532));
#147700=CARTESIAN_POINT('Ctrl Pts',(22.9370852180643,-10.4117190518159,
60.9685409471403));
#147701=CARTESIAN_POINT('Ctrl Pts',(22.9355668160252,-10.3712642552272,
60.9688257461811));
#147702=CARTESIAN_POINT('Ctrl Pts',(22.9355719204515,-10.33193324195,60.9688462512761));
#147703=CARTESIAN_POINT('Ctrl Pts',(25.5859731981751,-11.2434554547056,
60.5013588593932));
#147704=CARTESIAN_POINT('Ctrl Pts',(25.5844441899389,-11.2434658445421,
60.4927332003613));
#147705=CARTESIAN_POINT('Ctrl Pts',(25.5814984568459,-11.2436306576258,
60.4767534011199));
#147706=CARTESIAN_POINT('Ctrl Pts',(25.5799825962517,-11.2436242846107,
60.468128440764));
#147707=CARTESIAN_POINT('Origin',(17.7894674803291,1.4210854715202E-14,
100.88908350184));
#147708=CARTESIAN_POINT('Ctrl Pts',(25.585946658962,-11.2434347939771,60.5013635109443));
#147709=CARTESIAN_POINT('Ctrl Pts',(25.5908280517064,-11.2352178056434,
60.4925865053532));
#147710=CARTESIAN_POINT('Ctrl Pts',(25.5956760553759,-11.2269748700148,
60.4838153871567));
#147711=CARTESIAN_POINT('Ctrl Pts',(25.6004962205391,-11.21871037585,60.47504917764));
#147712=CARTESIAN_POINT('Origin',(17.7894674803291,1.4210854715202E-14,
100.88908350184));
#147713=CARTESIAN_POINT('',(25.600494243824,11.2187561752663,60.4750587214126));
#147714=CARTESIAN_POINT('',(25.6004957464494,11.2187573377186,60.4750584567717));
#147715=CARTESIAN_POINT('',(25.5858158203339,11.2436003008624,60.5011154491916));
#147716=CARTESIAN_POINT('Ctrl Pts',(25.6004937437591,11.2187557868,60.4750588099));
#147717=CARTESIAN_POINT('Ctrl Pts',(25.5980190908531,11.2229268927494,60.4793882956317));
#147718=CARTESIAN_POINT('Ctrl Pts',(25.5932000195592,11.2311758344546,60.4882199299609));
#147719=CARTESIAN_POINT('Ctrl Pts',(25.5882867359841,11.2394404119784,60.4967919610514));
#147720=CARTESIAN_POINT('Ctrl Pts',(25.585824508856,11.2435868068197,60.5011009711373));
#147721=CARTESIAN_POINT('',(25.5799682824491,11.24364172947,60.46812340452));
#147722=CARTESIAN_POINT('Ctrl Pts',(17.4667653729091,-22.5257212764,77.256905072711));
#147723=CARTESIAN_POINT('Ctrl Pts',(17.4522156153291,-22.52947690984,77.201794509167));
#147724=CARTESIAN_POINT('Ctrl Pts',(17.2326821287691,-22.58361462996,76.351112313277));
#147725=CARTESIAN_POINT('Ctrl Pts',(16.9332603507591,-22.57430986834,74.585159968858));
#147726=CARTESIAN_POINT('Ctrl Pts',(16.9282178457291,-22.22368100432,72.0018522533659));
#147727=CARTESIAN_POINT('Ctrl Pts',(17.3279784679891,-21.55585890438,69.568778249818));
#147728=CARTESIAN_POINT('Ctrl Pts',(18.0359271396891,-20.63613602496,67.425763312453));
#147729=CARTESIAN_POINT('Ctrl Pts',(18.9494515331591,-19.52905542686,65.598121631019));
#147730=CARTESIAN_POINT('Ctrl Pts',(20.0049202231791,-18.26930231769,64.050828430023));
#147731=CARTESIAN_POINT('Ctrl Pts',(21.1756845328891,-16.86079661466,62.74165530726));
#147732=CARTESIAN_POINT('Ctrl Pts',(22.4532806921391,-15.29024780344,61.65009812484));
#147733=CARTESIAN_POINT('Ctrl Pts',(23.8321876788191,-13.5386198194,60.78746444366));
#147734=CARTESIAN_POINT('Ctrl Pts',(24.9093942416691,-12.10874261238,60.35716873393));
#147735=CARTESIAN_POINT('Ctrl Pts',(25.5188775489791,-11.26992181782,60.2071336687));
#147736=CARTESIAN_POINT('Ctrl Pts',(25.6673509880891,-11.06368060085,60.17641247788));
#147737=CARTESIAN_POINT('Ctrl Pts',(18.7773649827691,-17.75527490826,76.717063290409));
#147738=CARTESIAN_POINT('Ctrl Pts',(18.7654556117691,-17.75828882524,76.674914380299));
#147739=CARTESIAN_POINT('Ctrl Pts',(18.5862635620091,-17.80174165801,76.0240512343981));
#147740=CARTESIAN_POINT('Ctrl Pts',(18.3577568645891,-17.79425534819,74.665378823862));
#147741=CARTESIAN_POINT('Ctrl Pts',(18.4246335003491,-17.51291935268,72.6770817004958));
#147742=CARTESIAN_POINT('Ctrl Pts',(18.8714641952291,-16.98119012651,70.822183427483));
#147743=CARTESIAN_POINT('Ctrl Pts',(19.6142963879091,-16.25801796827,69.218239633607));
#147744=CARTESIAN_POINT('Ctrl Pts',(20.5621683937491,-15.40160733776,67.8849620187121));
#147745=CARTESIAN_POINT('Ctrl Pts',(21.6579870981791,-14.44562122449,66.791899033372));
#147746=CARTESIAN_POINT('Ctrl Pts',(22.8780955574091,-13.40004445027,65.903735017982));
#147747=CARTESIAN_POINT('Ctrl Pts',(24.2153171433191,-12.26374841242,65.203217298719));
#147748=CARTESIAN_POINT('Ctrl Pts',(25.6646851711591,-11.03571934281,64.698047871997));
#147749=CARTESIAN_POINT('Ctrl Pts',(26.8015432713391,-10.07428690511,64.495800893793));
#147750=CARTESIAN_POINT('Ctrl Pts',(27.4463952672191,-9.53132694979998,
64.453831767256));
#147751=CARTESIAN_POINT('Ctrl Pts',(27.6035705906891,-9.399240458337,64.448068196782));
#147752=CARTESIAN_POINT('Ctrl Pts',(22.6527444970191,-14.84009533989,75.599270274124));
#147753=CARTESIAN_POINT('Ctrl Pts',(22.6450480694791,-14.8417831418,75.575183427031));
#147754=CARTESIAN_POINT('Ctrl Pts',(22.5298127564291,-14.866114563,75.203116801731));
#147755=CARTESIAN_POINT('Ctrl Pts',(22.4006621202491,-14.86192846848,74.422696506464));
#147756=CARTESIAN_POINT('Ctrl Pts',(22.5181198569391,-14.70436463479,73.2633823361753));
#147757=CARTESIAN_POINT('Ctrl Pts',(22.9377195244991,-14.4052238805,72.1556566073007));
#147758=CARTESIAN_POINT('Ctrl Pts',(23.6141508774891,-13.99538058674,71.163675788398));
#147759=CARTESIAN_POINT('Ctrl Pts',(24.4918032145691,-13.50533859052,70.299994638951));
#147760=CARTESIAN_POINT('Ctrl Pts',(25.5329266094991,-12.95204779512,69.5496905418731));
#147761=CARTESIAN_POINT('Ctrl Pts',(26.7219181594991,-12.33886835717,68.8939981611091));
#147762=CARTESIAN_POINT('Ctrl Pts',(28.0550484564891,-11.66205659809,68.32348737336));
#147763=CARTESIAN_POINT('Ctrl Pts',(29.5302626991891,-10.91639130965,67.842821810496));
#147764=CARTESIAN_POINT('Ctrl Pts',(30.7112123601191,-10.3172835446,67.571237827604));
#147765=CARTESIAN_POINT('Ctrl Pts',(31.3905930089891,-9.97074480891598,
67.457066442736));
#147766=CARTESIAN_POINT('Ctrl Pts',(31.5567731140791,-9.88587105497599,
67.431705971039));
#147767=CARTESIAN_POINT('Ctrl Pts',(27.4727097388691,-14.99894242272,74.370845864195));
#147768=CARTESIAN_POINT('Ctrl Pts',(27.4690374908891,-14.99927412475,74.362370216541));
#147769=CARTESIAN_POINT('Ctrl Pts',(27.4146355861491,-15.00404176909,74.231520094978));
#147770=CARTESIAN_POINT('Ctrl Pts',(27.3717438376491,-15.00325792021,73.9585721062895));
#147771=CARTESIAN_POINT('Ctrl Pts',(27.4972980083791,-14.97219965841,73.5156372957745));
#147772=CARTESIAN_POINT('Ctrl Pts',(27.8267501244891,-14.90490385564,73.0117077491551));
#147773=CARTESIAN_POINT('Ctrl Pts',(28.3632567205591,-14.79417301808,72.4487361234403));
#147774=CARTESIAN_POINT('Ctrl Pts',(29.0954791031191,-14.63302923949,71.833557915698));
#147775=CARTESIAN_POINT('Ctrl Pts',(30.0097285339691,-14.41300577028,71.171242909551));
#147776=CARTESIAN_POINT('Ctrl Pts',(31.1001512767791,-14.12091813026,70.4622944187711));
#147777=CARTESIAN_POINT('Ctrl Pts',(32.3671840294791,-13.73672387177,69.7064055545461));
#147778=CARTESIAN_POINT('Ctrl Pts',(33.8128240385791,-13.23052362994,68.90703904439));
#147779=CARTESIAN_POINT('Ctrl Pts',(35.0038717625891,-12.73614203142,68.297720297344));
#147780=CARTESIAN_POINT('Ctrl Pts',(35.7025055078291,-12.40446635354,67.961264321001));
#147781=CARTESIAN_POINT('Ctrl Pts',(35.8742286296091,-12.32012494619,67.879945375125));
#147782=CARTESIAN_POINT('',(28.2952879006395,-10.3188826735431,64.2104019363119));
#147783=CARTESIAN_POINT('',(26.0141520549875,-12.1870332282214,64.6126277311938));
#147784=CARTESIAN_POINT('Ctrl Pts',(28.2952879006395,-10.3188826735431,
64.2104019363119));
#147785=CARTESIAN_POINT('Ctrl Pts',(27.9287930576915,-10.6438766835605,
64.2750248654141));
#147786=CARTESIAN_POINT('Ctrl Pts',(27.5458477659422,-10.9632373020545,
64.3425484525577));
#147787=CARTESIAN_POINT('Ctrl Pts',(26.7888573507576,-11.5772327263092,
64.4760262868924));
#147788=CARTESIAN_POINT('Ctrl Pts',(26.3839963435794,-11.8964640257404,
64.5474142058218));
#147789=CARTESIAN_POINT('Ctrl Pts',(26.0141587646837,-12.1870420332971,
64.612626549461));
#147790=CARTESIAN_POINT('Ctrl Pts',(25.6004488369058,-11.2186736973405,
60.4750575395639));
#147791=CARTESIAN_POINT('Ctrl Pts',(25.6771414538508,-11.1557830040577,
60.6337815308351));
#147792=CARTESIAN_POINT('Ctrl Pts',(25.7584151174531,-11.0953949289909,
60.7932143542437));
#147793=CARTESIAN_POINT('Ctrl Pts',(25.844310928499,-11.037781455913,60.9529979077714));
#147794=CARTESIAN_POINT('Ctrl Pts',(25.9295618292542,-10.9806005478371,
61.1115817979316));
#147795=CARTESIAN_POINT('Ctrl Pts',(26.0193659247053,-10.9261530587674,
61.2705108944446));
#147796=CARTESIAN_POINT('Ctrl Pts',(26.113720684445,-10.8746965781389,61.4294088726265));
#147797=CARTESIAN_POINT('Ctrl Pts',(26.2086156080668,-10.8229455184938,
61.5892165129072));
#147798=CARTESIAN_POINT('Ctrl Pts',(26.3081136900117,-10.7742201760057,
61.7489923872755));
#147799=CARTESIAN_POINT('Ctrl Pts',(26.4121655715204,-10.7287689378137,
61.9083312146541));
#147800=CARTESIAN_POINT('Ctrl Pts',(26.5162174530291,-10.6833176996217,
62.0676700420328));
#147801=CARTESIAN_POINT('Ctrl Pts',(26.6248232672778,-10.6411409234484,
62.2265714462408));
#147802=CARTESIAN_POINT('Ctrl Pts',(26.7378842407237,-10.6024679594409,
62.3846128012655));
#147803=CARTESIAN_POINT('Ctrl Pts',(26.8508360347518,-10.5638323406955,
62.5425015407359));
#147804=CARTESIAN_POINT('Ctrl Pts',(26.9682348811087,-10.528693532743,62.6995312136569));
#147805=CARTESIAN_POINT('Ctrl Pts',(27.0899297391689,-10.4972591991273,
62.8552717178284));
#147806=CARTESIAN_POINT('Ctrl Pts',(27.2075046724398,-10.466889060765,63.005739697145));
#147807=CARTESIAN_POINT('Ctrl Pts',(27.3290893789845,-10.43997694453,63.1550038764423));
#147808=CARTESIAN_POINT('Ctrl Pts',(27.4545028264304,-10.416683963319,63.3026721539028));
#147809=CARTESIAN_POINT('Ctrl Pts',(27.5794141640008,-10.3934842387413,
63.4497492212345));
#147810=CARTESIAN_POINT('Ctrl Pts',(27.7081235256901,-10.373874942025,63.5952427264035));
#147811=CARTESIAN_POINT('Ctrl Pts',(27.8404094539594,-10.3579861278288,
63.7387672788158));
#147812=CARTESIAN_POINT('Ctrl Pts',(27.9721230978152,-10.342166050503,63.8816709272108));
#147813=CARTESIAN_POINT('Ctrl Pts',(28.1073822405416,-10.330034502476,64.022622210721));
#147814=CARTESIAN_POINT('Ctrl Pts',(28.2459282980801,-10.3216880682509,
64.1612488914306));
#147815=CARTESIAN_POINT('Ctrl Pts',(28.2623353354503,-10.3206996586153,
64.1776654764373));
#147816=CARTESIAN_POINT('Ctrl Pts',(28.2787884243379,-10.319764293024,64.1940494748701));
#147817=CARTESIAN_POINT('Ctrl Pts',(28.2952871000938,-10.3188821006174,
64.2104002803598));
#147818=CARTESIAN_POINT('Ctrl Pts',(26.0141520557349,-12.1870332282901,
64.6126277283268));
#147819=CARTESIAN_POINT('Ctrl Pts',(26.0012422809462,-12.1388602075693,
64.4661526914882));
#147820=CARTESIAN_POINT('Ctrl Pts',(25.9872836532194,-12.087933236017,64.3090583874833));
#147821=CARTESIAN_POINT('Ctrl Pts',(25.9645184990504,-12.0084297043005,
64.057478451471));
#147822=CARTESIAN_POINT('Ctrl Pts',(25.9566253013141,-11.9814136956279,
63.9709621319751));
#147823=CARTESIAN_POINT('Ctrl Pts',(25.944299540303,-11.9402823435069,63.8371998866629));
#147824=CARTESIAN_POINT('Ctrl Pts',(25.9380151379575,-11.9195652713876,
63.7693217847163));
#147825=CARTESIAN_POINT('Ctrl Pts',(25.9304640520936,-11.895171370767,63.6883847335085));
#147826=CARTESIAN_POINT('Ctrl Pts',(25.9263591770947,-11.8820491146581,
63.6445577240038));
#147827=CARTESIAN_POINT('Ctrl Pts',(25.9244272053296,-11.8759114862136,
63.6239777222435));
#147828=CARTESIAN_POINT('Ctrl Pts',(25.9233191909306,-11.8724010161351,
63.6121865158046));
#147829=CARTESIAN_POINT('Ctrl Pts',(25.9231709220948,-11.8719313157875,
63.6106087420972));
#147830=CARTESIAN_POINT('Ctrl Pts',(25.8707006041343,-11.7059929720678,
63.0526023350243));
#147831=CARTESIAN_POINT('Ctrl Pts',(25.8210422190118,-11.581613044566,62.5685125411034));
#147832=CARTESIAN_POINT('Ctrl Pts',(25.687446953851,-11.3093598897932,61.3232443887802));
#147833=CARTESIAN_POINT('Ctrl Pts',(25.6201332141581,-11.2608219841326,
60.7717569482344));
#147834=CARTESIAN_POINT('Ctrl Pts',(25.5859466416791,-11.24343482307,60.50136354202));
#147835=CARTESIAN_POINT('Ctrl Pts',(28.1799730489391,-14.15117801268,74.301595852087));
#147836=CARTESIAN_POINT('Ctrl Pts',(28.1735718783691,-14.15291478505,74.2652930097969));
#147837=CARTESIAN_POINT('Ctrl Pts',(28.1587242848691,-14.15609086467,74.181088122743));
#147838=CARTESIAN_POINT('Ctrl Pts',(28.1345641629891,-14.15802842506,74.044069262757));
#147839=CARTESIAN_POINT('Ctrl Pts',(28.1065660850191,-14.1557638184,73.8852842721588));
#147840=CARTESIAN_POINT('Ctrl Pts',(28.0757500096891,-14.14785693146,73.7105176244119));
#147841=CARTESIAN_POINT('Ctrl Pts',(28.0418954916191,-14.13302748591,73.5185191115803));
#147842=CARTESIAN_POINT('Ctrl Pts',(28.0048627881991,-14.11015935491,73.3084962139256));
#147843=CARTESIAN_POINT('Ctrl Pts',(27.9645715192991,-14.07834643848,73.0799930731187));
#147844=CARTESIAN_POINT('Ctrl Pts',(27.9208888531191,-14.036930053,72.8322563625702));
#147845=CARTESIAN_POINT('Ctrl Pts',(27.8735693541391,-13.98520775603,72.5638941483318));
#147846=CARTESIAN_POINT('Ctrl Pts',(27.8223275617791,-13.92248791285,72.2732875029045));
#147847=CARTESIAN_POINT('Ctrl Pts',(27.7669353440791,-13.84821962507,71.9591426257));
#147848=CARTESIAN_POINT('Ctrl Pts',(27.7071659871591,-13.76186996469,71.620173758449));
#147849=CARTESIAN_POINT('Ctrl Pts',(27.6427331848091,-13.66295161782,71.2547571778699));
#147850=CARTESIAN_POINT('Ctrl Pts',(27.5731736312291,-13.55077370827,70.860265346269));
#147851=CARTESIAN_POINT('Ctrl Pts',(27.4979482253291,-13.42445216333,70.433640869453));
#147852=CARTESIAN_POINT('Ctrl Pts',(27.4168343894691,-13.28392357974,69.97362144678));
#147853=CARTESIAN_POINT('Ctrl Pts',(27.3294747454891,-13.12902729583,69.478180286149));
#147854=CARTESIAN_POINT('Ctrl Pts',(27.2352897672591,-12.95931585803,68.944030731412));
#147855=CARTESIAN_POINT('Ctrl Pts',(27.1330543177591,-12.77375947438,68.36422468536));
#147856=CARTESIAN_POINT('Ctrl Pts',(27.0215516935991,-12.57148328781,67.731861880101));
#147857=CARTESIAN_POINT('Ctrl Pts',(26.8998844749991,-12.35307312972,67.041852795234));
#147858=CARTESIAN_POINT('Ctrl Pts',(26.7675133818891,-12.12114868892,66.2911390213841));
#147859=CARTESIAN_POINT('Ctrl Pts',(26.6238265063091,-11.87925312292,65.4762502561861));
#147860=CARTESIAN_POINT('Ctrl Pts',(26.4673150737591,-11.63288870712,64.588629814245));
#147861=CARTESIAN_POINT('Ctrl Pts',(26.2960779423591,-11.39104634332,63.617495784079));
#147862=CARTESIAN_POINT('Ctrl Pts',(26.1146351892191,-11.17902244978,62.5884827969));
#147863=CARTESIAN_POINT('Ctrl Pts',(25.9376619630691,-11.03545945137,61.5848177569));
#147864=CARTESIAN_POINT('Ctrl Pts',(25.8044546378291,-10.98673841047,60.8293614750201));
#147865=CARTESIAN_POINT('Ctrl Pts',(25.7335896270191,-10.98615918857,60.42746602756));
#147866=CARTESIAN_POINT('Ctrl Pts',(25.7147102194091,-10.98797446009,60.3203955863901));
#147867=CARTESIAN_POINT('Ctrl Pts',(27.1734273383791,-16.2916628133,74.5810090502221));
#147868=CARTESIAN_POINT('Ctrl Pts',(27.1646108851991,-16.29406243743,74.531008459631));
#147869=CARTESIAN_POINT('Ctrl Pts',(27.1440760525391,-16.29846019828,74.414549636477));
#147870=CARTESIAN_POINT('Ctrl Pts',(27.1104807962291,-16.30115793748,74.224021470152));
#147871=CARTESIAN_POINT('Ctrl Pts',(27.0715520564091,-16.29800450584,74.003245615733));
#147872=CARTESIAN_POINT('Ctrl Pts',(27.0290761160691,-16.28707212928,73.7623525874979));
#147873=CARTESIAN_POINT('Ctrl Pts',(26.9836467347891,-16.26711075281,73.5047097634025));
#147874=CARTESIAN_POINT('Ctrl Pts',(26.9353870206991,-16.23724121735,73.231015324247));
#147875=CARTESIAN_POINT('Ctrl Pts',(26.8847204870791,-16.19715982767,72.9436711332555));
#147876=CARTESIAN_POINT('Ctrl Pts',(26.8316423236691,-16.14677063562,72.6426499101076));
#147877=CARTESIAN_POINT('Ctrl Pts',(26.7758815320691,-16.08576509839,72.3264147464796));
#147878=CARTESIAN_POINT('Ctrl Pts',(26.7171808327491,-16.01386768581,71.9935065376213));
#147879=CARTESIAN_POINT('Ctrl Pts',(26.6552374104291,-15.93077840098,71.642207932743));
#147880=CARTESIAN_POINT('Ctrl Pts',(26.5897379537191,-15.83611958068,71.2707420546911));
#147881=CARTESIAN_POINT('Ctrl Pts',(26.5204490164191,-15.72972144342,70.877784964302));
#147882=CARTESIAN_POINT('Ctrl Pts',(26.4467441668391,-15.61084028714,70.45978399085));
#147883=CARTESIAN_POINT('Ctrl Pts',(26.3680895688091,-15.47874470736,70.0137115990481));
#147884=CARTESIAN_POINT('Ctrl Pts',(26.2843664547391,-15.33368482781,69.5388942243469));
#147885=CARTESIAN_POINT('Ctrl Pts',(26.1950217273191,-15.17526161349,69.032195096033));
#147886=CARTESIAN_POINT('Ctrl Pts',(26.0996654749091,-15.00343453373,68.491402915343));
#147887=CARTESIAN_POINT('Ctrl Pts',(25.9971340390191,-14.81733951027,67.9099182470231));
#147888=CARTESIAN_POINT('Ctrl Pts',(25.8861065416291,-14.61592784221,67.2802500196189));
#147889=CARTESIAN_POINT('Ctrl Pts',(25.7662123528591,-14.40070911901,66.600296286566));
#147890=CARTESIAN_POINT('Ctrl Pts',(25.6369459663191,-14.17424139564,65.867190178725));
#147891=CARTESIAN_POINT('Ctrl Pts',(25.4982315426691,-13.940759467,65.080501589758));
#147892=CARTESIAN_POINT('Ctrl Pts',(25.3495581035291,-13.70681104471,64.2373326172561));
#147893=CARTESIAN_POINT('Ctrl Pts',(25.1899312459191,-13.48155823901,63.3320437218209));
#147894=CARTESIAN_POINT('Ctrl Pts',(25.0263288417991,-13.29087482736,62.4042083816401));
#147895=CARTESIAN_POINT('Ctrl Pts',(24.8740404427791,-13.16819509687,61.54053795295));
#147896=CARTESIAN_POINT('Ctrl Pts',(24.7660208233591,-13.12950137129,60.9279282491701));
#147897=CARTESIAN_POINT('Ctrl Pts',(24.7113232798591,-13.12914167291,60.61772306514));
#147898=CARTESIAN_POINT('Ctrl Pts',(24.6969486285791,-13.13052501539,60.53620036667));
#147899=CARTESIAN_POINT('Ctrl Pts',(24.9455852428891,-15.52840338343,74.937490541193));
#147900=CARTESIAN_POINT('Ctrl Pts',(24.9376300372391,-15.53056664622,74.89237432799));
#147901=CARTESIAN_POINT('Ctrl Pts',(24.9191231745591,-15.53452877692,74.787416694133));
#147902=CARTESIAN_POINT('Ctrl Pts',(24.8888923221091,-15.53695544966,74.6159690102469));
#147903=CARTESIAN_POINT('Ctrl Pts',(24.8538612650591,-15.53411895745,74.417298013271));
#147904=CARTESIAN_POINT('Ctrl Pts',(24.8155430285791,-15.52426541755,74.1999844953681));
#147905=CARTESIAN_POINT('Ctrl Pts',(24.7742410410091,-15.50613399786,73.9657492841528));
#147906=CARTESIAN_POINT('Ctrl Pts',(24.7299846824891,-15.47876104073,73.7147590026961));
#147907=CARTESIAN_POINT('Ctrl Pts',(24.6830177867491,-15.44162804395,73.4483965007143));
#147908=CARTESIAN_POINT('Ctrl Pts',(24.6332898932691,-15.39443839773,73.1663756024908));
#147909=CARTESIAN_POINT('Ctrl Pts',(24.5805391189291,-15.33674310157,72.8672110950277));
#147910=CARTESIAN_POINT('Ctrl Pts',(24.5244981353291,-15.26811824966,72.5493868835785));
#147911=CARTESIAN_POINT('Ctrl Pts',(24.4648907579491,-15.18817437804,72.2113366479453));
#147912=CARTESIAN_POINT('Ctrl Pts',(24.4014345545691,-15.0964784588,71.851458635375));
#147913=CARTESIAN_POINT('Ctrl Pts',(24.3338772300291,-14.99274748392,71.468322008935));
#147914=CARTESIAN_POINT('Ctrl Pts',(24.2616505204791,-14.87625658814,71.05870398415));
#147915=CARTESIAN_POINT('Ctrl Pts',(24.1842187123691,-14.74621992816,70.61956637857));
#147916=CARTESIAN_POINT('Ctrl Pts',(24.1014260212591,-14.60277582948,70.150025694656));
#147917=CARTESIAN_POINT('Ctrl Pts',(24.0127891398591,-14.44561025683,69.647340960648));
#147918=CARTESIAN_POINT('Ctrl Pts',(23.9178505433291,-14.27453757798,69.108917424153));
#147919=CARTESIAN_POINT('Ctrl Pts',(23.8154246510091,-14.08863462405,68.5280313231649));
#147920=CARTESIAN_POINT('Ctrl Pts',(23.7042277317191,-13.88691468382,67.897402256442));
#147921=CARTESIAN_POINT('Ctrl Pts',(23.5837013115391,-13.67055795077,67.213862960861));
#147922=CARTESIAN_POINT('Ctrl Pts',(23.4533278409591,-13.44214445744,66.4744782673861));
#147923=CARTESIAN_POINT('Ctrl Pts',(23.3128403279491,-13.20566237292,65.677733988967));
#147924=CARTESIAN_POINT('Ctrl Pts',(23.1613719974891,-12.96728662458,64.818714400188));
#147925=CARTESIAN_POINT('Ctrl Pts',(22.9976051193791,-12.73611827271,63.889946281738));
#147926=CARTESIAN_POINT('Ctrl Pts',(22.8276411589291,-12.53782521859,62.9260327628401));
#147927=CARTESIAN_POINT('Ctrl Pts',(22.6665505824491,-12.40769888014,62.0124427051201));
#147928=CARTESIAN_POINT('Ctrl Pts',(22.5495494678191,-12.36542958935,61.34889641084));
#147929=CARTESIAN_POINT('Ctrl Pts',(22.4890868883391,-12.36499161272,61.00599608308));
#147930=CARTESIAN_POINT('Ctrl Pts',(22.4731059197691,-12.36652897355,60.91536350656));
#147931=CARTESIAN_POINT('Ctrl Pts',(25.3958369987791,-13.19733209216,74.747091056725));
#147932=CARTESIAN_POINT('Ctrl Pts',(25.3905121299191,-13.19877348358,74.716892224767));
#147933=CARTESIAN_POINT('Ctrl Pts',(25.3781988921391,-13.20140515586,74.6470603831829));
#147934=CARTESIAN_POINT('Ctrl Pts',(25.3582432684491,-13.20300396427,74.533886417376));
#147935=CARTESIAN_POINT('Ctrl Pts',(25.3351161277591,-13.20113543707,74.40272588482));
#147936=CARTESIAN_POINT('Ctrl Pts',(25.3094959382791,-13.19457677317,74.25742657001));
#147937=CARTESIAN_POINT('Ctrl Pts',(25.2807994274291,-13.18203422608,74.0946805697331));
#147938=CARTESIAN_POINT('Ctrl Pts',(25.2487697206791,-13.16228607101,73.9130310761299));
#147939=CARTESIAN_POINT('Ctrl Pts',(25.2131018921891,-13.13415776355,73.7107487688747));
#147940=CARTESIAN_POINT('Ctrl Pts',(25.1736060610091,-13.09673985306,73.4867567795944));
#147941=CARTESIAN_POINT('Ctrl Pts',(25.1300481830191,-13.04915436699,73.2397277780308));
#147942=CARTESIAN_POINT('Ctrl Pts',(25.0821302395191,-12.99052424551,72.9679716162406));
#147943=CARTESIAN_POINT('Ctrl Pts',(25.0296573790591,-12.92018678314,72.6703832366873));
#147944=CARTESIAN_POINT('Ctrl Pts',(24.9724414774691,-12.83753986258,72.345895734205));
#147945=CARTESIAN_POINT('Ctrl Pts',(24.9101726729691,-12.74195467067,71.9927517952847));
#147946=CARTESIAN_POINT('Ctrl Pts',(24.8424603521591,-12.63276387159,71.6087361413429));
#147947=CARTESIAN_POINT('Ctrl Pts',(24.7687630678091,-12.50901536037,71.190778072421));
#147948=CARTESIAN_POINT('Ctrl Pts',(24.6888119822491,-12.37050601941,70.737352934449));
#147949=CARTESIAN_POINT('Ctrl Pts',(24.6023369340291,-12.21718141131,70.246928565596));
#147950=CARTESIAN_POINT('Ctrl Pts',(24.5086739006791,-12.04841274893,69.715739107405));
#147951=CARTESIAN_POINT('Ctrl Pts',(24.4065703490691,-11.86309639472,69.1366810914259));
#147952=CARTESIAN_POINT('Ctrl Pts',(24.2948559982191,-11.66043496018,68.503117524501));
#147953=CARTESIAN_POINT('Ctrl Pts',(24.1723986795191,-11.44060263028,67.8086275592741));
#147954=CARTESIAN_POINT('Ctrl Pts',(24.0386440625791,-11.20624655919,67.0500674319299));
#147955=CARTESIAN_POINT('Ctrl Pts',(23.8927413558091,-10.96060169599,66.222612063574));
#147956=CARTESIAN_POINT('Ctrl Pts',(23.7327371453591,-10.70870444727,65.315183093782));
#147957=CARTESIAN_POINT('Ctrl Pts',(23.5563262270191,-10.45946942069,64.314707059819));
#147958=CARTESIAN_POINT('Ctrl Pts',(23.3669334318491,-10.23793575087,63.240607143819));
#147959=CARTESIAN_POINT('Ctrl Pts',(23.1789601174791,-10.08506672053,62.1745575034399));
#147960=CARTESIAN_POINT('Ctrl Pts',(23.0345286104791,-10.03187729293,61.35544572364));
#147961=CARTESIAN_POINT('Ctrl Pts',(22.9564590295991,-10.03120024663,60.9126911289));
#147962=CARTESIAN_POINT('Ctrl Pts',(22.9355722059791,-10.033207995,60.79423606582));
#147963=CARTESIAN_POINT('Ctrl Pts',(23.651525801475,-10.9473150473928,65.0292224863858));
#147964=CARTESIAN_POINT('Ctrl Pts',(23.6515257621658,-11.1312070918152,
65.0292224933171));
#147965=CARTESIAN_POINT('Ctrl Pts',(23.6828327230095,-11.3139663116835,
65.0237022314369));
#147966=CARTESIAN_POINT('Ctrl Pts',(23.807271208638,-11.6646282261749,65.0017603689821));
#147967=CARTESIAN_POINT('Ctrl Pts',(23.9012088684855,-11.8295758620756,
64.9851966250261));
#147968=CARTESIAN_POINT('Ctrl Pts',(24.1432300222825,-12.1167462245558,
64.9425217657095));
#147969=CARTESIAN_POINT('Ctrl Pts',(24.2894314553903,-12.2364947812159,
64.9167425084553));
#147970=CARTESIAN_POINT('Ctrl Pts',(24.6217353068813,-12.4156530859415,
64.8581483736441));
#147971=CARTESIAN_POINT('Ctrl Pts',(24.80507951085,-12.4718672970602,64.8258198437246));
#147972=CARTESIAN_POINT('Ctrl Pts',(25.1736178642303,-12.5072619289281,
64.7608365885978));
#147973=CARTESIAN_POINT('Ctrl Pts',(25.3543120349207,-12.4898627065513,
64.7289753310509));
#147974=CARTESIAN_POINT('Ctrl Pts',(25.7039070130317,-12.3869706731887,
64.6673323040898));
#147975=CARTESIAN_POINT('Ctrl Pts',(25.8687813243819,-12.3012676530536,
64.6382605145725));
#147976=CARTESIAN_POINT('Ctrl Pts',(26.0141453440937,-12.1870244234308,
64.6126289158731));
#147977=CARTESIAN_POINT('Ctrl Pts',(25.3886736533591,-11.44208510792,60.2115109699));
#147978=CARTESIAN_POINT('Ctrl Pts',(25.5981770475491,-11.17175375805,60.22632667139));
#147979=CARTESIAN_POINT('Ctrl Pts',(25.8078177068491,-10.88204468039,60.24561988886));
#147980=CARTESIAN_POINT('Ctrl Pts',(26.0168787184791,-10.57129328633,60.270855635));
#147981=CARTESIAN_POINT('Ctrl Pts',(27.3087836696091,-9.624602273718,64.44463626086));
#147982=CARTESIAN_POINT('Ctrl Pts',(27.5425179224791,-9.479512324536,64.50183542974));
#147983=CARTESIAN_POINT('Ctrl Pts',(27.7759878147791,-9.32787789472698,
64.56281239081));
#147984=CARTESIAN_POINT('Ctrl Pts',(28.0092438744591,-9.16583693103399,
64.625382279757));
#147985=CARTESIAN_POINT('Ctrl Pts',(31.2407814247091,-10.04443147536,67.489770329979));
#147986=CARTESIAN_POINT('Ctrl Pts',(31.5318184331991,-9.93037722233698,
67.468249475135));
#147987=CARTESIAN_POINT('Ctrl Pts',(31.8153253258691,-9.81435677539199,
67.4542319002));
#147988=CARTESIAN_POINT('Ctrl Pts',(32.0927104552091,-9.69360679656099,
67.4456953393931));
#147989=CARTESIAN_POINT('Ctrl Pts',(35.5328635075091,-12.52520554518,68.067674694392));
#147990=CARTESIAN_POINT('Ctrl Pts',(35.8902027012991,-12.3349434155,67.879400029176));
#147991=CARTESIAN_POINT('Ctrl Pts',(36.2289341849091,-12.1371151135,67.705214293035));
#147992=CARTESIAN_POINT('Ctrl Pts',(36.5518441070791,-11.93289063421,67.547001987805));
#147993=CARTESIAN_POINT('Ctrl Pts',(28.7123816359948,-9.91606170434255,
64.1368570572843));
#147994=CARTESIAN_POINT('Ctrl Pts',(28.6457638811355,-9.98626732421584,
64.1486035648602));
#147995=CARTESIAN_POINT('Ctrl Pts',(28.5777184993322,-10.0548652908716,
64.1606018015785));
#147996=CARTESIAN_POINT('Ctrl Pts',(28.4385393129266,-10.1892126190695,
64.1851428472949));
#147997=CARTESIAN_POINT('Ctrl Pts',(28.3676165512144,-10.2547579475351,
64.1976484437373));
#147998=CARTESIAN_POINT('Ctrl Pts',(28.295281579335,-10.3188753218672,64.2104030509284));
#147999=CARTESIAN_POINT('Ctrl Pts',(36.2511910984291,-0.816951121684487,
99.13095237507));
#148000=CARTESIAN_POINT('Ctrl Pts',(36.2200982088991,-1.45683196280799,
99.1098451401801));
#148001=CARTESIAN_POINT('Ctrl Pts',(36.0778630790891,-2.85039942836099,
99.0419676728901));
#148002=CARTESIAN_POINT('Ctrl Pts',(35.6275483510391,-4.94247000735899,
98.84599903898));
#148003=CARTESIAN_POINT('Ctrl Pts',(34.9397597871691,-7.05113172994599,
98.51977184372));
#148004=CARTESIAN_POINT('Ctrl Pts',(34.0734741662491,-9.09163743804897,
98.0649602571899));
#148005=CARTESIAN_POINT('Ctrl Pts',(33.0099168483791,-11.12983443612,97.44906592845));
#148006=CARTESIAN_POINT('Ctrl Pts',(31.7699785170891,-13.12298748389,96.6589115129399));
#148007=CARTESIAN_POINT('Ctrl Pts',(30.4746258290591,-14.92251334854,95.75721789378));
#148008=CARTESIAN_POINT('Ctrl Pts',(29.1968815731991,-16.50069944243,94.7947864407199));
#148009=CARTESIAN_POINT('Ctrl Pts',(27.9225293421991,-17.92619343051,93.76208048801));
#148010=CARTESIAN_POINT('Ctrl Pts',(26.5896727465691,-19.28349187111,92.5956876894801));
#148011=CARTESIAN_POINT('Ctrl Pts',(25.1814694175691,-20.58838494568,91.25117303266));
#148012=CARTESIAN_POINT('Ctrl Pts',(23.7249591534991,-21.81419974781,89.71266771848));
#148013=CARTESIAN_POINT('Ctrl Pts',(22.2142909846591,-22.9637208008,87.91364117654));
#148014=CARTESIAN_POINT('Ctrl Pts',(20.6065395382091,-24.05476593901,85.68623624305));
#148015=CARTESIAN_POINT('Ctrl Pts',(18.9416778012191,-25.02348229969,82.825890425796));
#148016=CARTESIAN_POINT('Ctrl Pts',(17.5339994345191,-25.65356630387,79.417420667109));
#148017=CARTESIAN_POINT('Ctrl Pts',(16.9242179391691,-25.78353110717,76.926255793732));
#148018=CARTESIAN_POINT('Ctrl Pts',(16.7312453442491,-25.77964745785,75.805602355198));
#148019=CARTESIAN_POINT('Ctrl Pts',(34.9680768531591,-0.377262712455286,
92.83793248162));
#148020=CARTESIAN_POINT('Ctrl Pts',(34.9401900659091,-0.768818210978587,
92.83356221903));
#148021=CARTESIAN_POINT('Ctrl Pts',(34.8109275223991,-1.62812620872499,
92.8325719567701));
#148022=CARTESIAN_POINT('Ctrl Pts',(34.3972755661991,-2.97122279462399,
92.8255990532501));
#148023=CARTESIAN_POINT('Ctrl Pts',(33.7599966114291,-4.39375486831299,
92.76261787049));
#148024=CARTESIAN_POINT('Ctrl Pts',(32.9521573659891,-5.82931930270299,
92.61621541888));
#148025=CARTESIAN_POINT('Ctrl Pts',(31.9551618598791,-7.31697565127499,
92.35621163472));
#148026=CARTESIAN_POINT('Ctrl Pts',(30.7878189799691,-8.81951599642399,
91.9596113594201));
#148027=CARTESIAN_POINT('Ctrl Pts',(29.5643467643691,-10.21287137887,91.45281600972));
#148028=CARTESIAN_POINT('Ctrl Pts',(28.3547145027491,-11.46125770319,90.86912642514));
#148029=CARTESIAN_POINT('Ctrl Pts',(27.1462246720591,-12.60932492795,90.2068010813201));
#148030=CARTESIAN_POINT('Ctrl Pts',(25.8804633212691,-13.72121825748,89.42218714027));
#148031=CARTESIAN_POINT('Ctrl Pts',(24.5415426038291,-14.80846467629,88.4770655865801));
#148032=CARTESIAN_POINT('Ctrl Pts',(23.1553900553591,-15.84725088264,87.34998754959));
#148033=CARTESIAN_POINT('Ctrl Pts',(21.7169286490991,-16.83785256507,85.9795861337301));
#148034=CARTESIAN_POINT('Ctrl Pts',(20.1864646779891,-17.79411649535,84.2176273015201));
#148035=CARTESIAN_POINT('Ctrl Pts',(18.6056376920291,-18.65837811088,81.868380902977));
#148036=CARTESIAN_POINT('Ctrl Pts',(17.2833457609491,-19.22934869733,78.9739891356611));
#148037=CARTESIAN_POINT('Ctrl Pts',(16.7318898964791,-19.34793907064,76.820460370021));
#148038=CARTESIAN_POINT('Ctrl Pts',(16.5654152065891,-19.34439445674,75.849914932886));
#148039=CARTESIAN_POINT('Ctrl Pts',(38.6686947048191,-0.267618408180286,
87.57152762521));
#148040=CARTESIAN_POINT('Ctrl Pts',(38.6331457099391,-0.640502714598286,
87.56228047755));
#148041=CARTESIAN_POINT('Ctrl Pts',(38.4681697649291,-1.45257130791499,
87.5371031361401));
#148042=CARTESIAN_POINT('Ctrl Pts',(37.9543196144491,-2.67152049410099,
87.46697907679));
#148043=CARTESIAN_POINT('Ctrl Pts',(37.1964789572891,-3.89993484531899,
87.33954011223));
#148044=CARTESIAN_POINT('Ctrl Pts',(36.2722354399091,-5.08847143352099,
87.1482156939501));
#148045=CARTESIAN_POINT('Ctrl Pts',(35.1711071623791,-6.27550574943099,
86.8740206795701));
#148046=CARTESIAN_POINT('Ctrl Pts',(33.9234036585391,-7.436166673543,86.50611895787));
#148047=CARTESIAN_POINT('Ctrl Pts',(32.6526782149891,-8.48396598041999,
86.07171874038));
#148048=CARTESIAN_POINT('Ctrl Pts',(31.4266015655591,-9.40280963542199,
85.5959755830301));
#148049=CARTESIAN_POINT('Ctrl Pts',(30.2282183070691,-10.23269364386,85.07485106796));
#148050=CARTESIAN_POINT('Ctrl Pts',(29.0009821455491,-11.02282107056,84.4750277186701));
#148051=CARTESIAN_POINT('Ctrl Pts',(27.7349646372491,-11.7823880216,83.77066674245));
#148052=CARTESIAN_POINT('Ctrl Pts',(26.4611997445191,-12.49587308951,82.949856613029));
#148053=CARTESIAN_POINT('Ctrl Pts',(25.1820693516891,-13.16490311603,81.9728674396441));
#148054=CARTESIAN_POINT('Ctrl Pts',(23.8728795301391,-13.79985263807,80.741966022882));
#148055=CARTESIAN_POINT('Ctrl Pts',(22.5850112147791,-14.36356654138,79.133191069062));
#148056=CARTESIAN_POINT('Ctrl Pts',(21.5697113092491,-14.73019815096,77.183930116823));
#148057=CARTESIAN_POINT('Ctrl Pts',(21.1758003549191,-14.80581932552,75.7409655371681));
#148058=CARTESIAN_POINT('Ctrl Pts',(21.0646250899491,-14.8035595922,75.088550558094));
#148059=CARTESIAN_POINT('Ctrl Pts',(45.0312706731691,-0.556809233210386,
86.63588923546));
#148060=CARTESIAN_POINT('Ctrl Pts',(44.9819984429591,-1.15239083593299,
86.6032111113799));
#148061=CARTESIAN_POINT('Ctrl Pts',(44.7550297579291,-2.43387817146999,
86.47794742155));
#148062=CARTESIAN_POINT('Ctrl Pts',(44.0669849657891,-4.23139684260399,
86.1321464635101));
#148063=CARTESIAN_POINT('Ctrl Pts',(43.0931519133991,-5.87949518942999,
85.65298684557));
#148064=CARTESIAN_POINT('Ctrl Pts',(41.9506857162891,-7.33390305288999,
85.0915934778799));
#148065=CARTESIAN_POINT('Ctrl Pts',(40.6400631633491,-8.65884473130499,
84.44202906066));
#148066=CARTESIAN_POINT('Ctrl Pts',(39.2094613534091,-9.84085525044999,
83.71996478425));
#148067=CARTESIAN_POINT('Ctrl Pts',(37.8019957376891,-10.82051536224,82.99003573172));
#148068=CARTESIAN_POINT('Ctrl Pts',(36.4852355554891,-11.6168290835,82.283717786993));
#148069=CARTESIAN_POINT('Ctrl Pts',(35.2348621603691,-12.28740211764,81.586024678646));
#148070=CARTESIAN_POINT('Ctrl Pts',(33.9934103628291,-12.88127932846,80.858065721516));
#148071=CARTESIAN_POINT('Ctrl Pts',(32.7581770629291,-13.40872065919,80.08477919832));
#148072=CARTESIAN_POINT('Ctrl Pts',(31.5683175582891,-13.86272653758,79.272924596943));
#148073=CARTESIAN_POINT('Ctrl Pts',(30.4356778789491,-14.24928723071,78.407307267481));
#148074=CARTESIAN_POINT('Ctrl Pts',(29.3529211006491,-14.57798235441,77.439888248051));
#148075=CARTESIAN_POINT('Ctrl Pts',(28.3831326036191,-14.83361972799,76.336383711929));
#148076=CARTESIAN_POINT('Ctrl Pts',(27.7038229907891,-14.97888942575,75.170329705841));
#148077=CARTESIAN_POINT('Ctrl Pts',(27.4678322792991,-15.00690558171,74.365048202755));
#148078=CARTESIAN_POINT('Ctrl Pts',(27.4060630052191,-15.00607043787,73.999190543978));
#148079=CARTESIAN_POINT('',(39.4126085609146,-0.605361527076818,89.303184116066));
#148080=CARTESIAN_POINT('Origin',(46.4982593122882,-1.66437591746992,96.9778062066542));
#148081=CARTESIAN_POINT('Ctrl Pts',(39.4126085609146,-0.605361527076818,
89.303184116066));
#148082=CARTESIAN_POINT('Ctrl Pts',(39.4099252318568,-0.683444947045363,
89.2948644632298));
#148083=CARTESIAN_POINT('Ctrl Pts',(39.4065580192006,-0.766708479631635,
89.2850814479826));
#148084=CARTESIAN_POINT('Ctrl Pts',(39.4024210385378,-0.855040525558286,
89.2733819496395));
#148085=CARTESIAN_POINT('Ctrl Pts',(39.398394517039,-0.941014067848123,
89.2619948329367));
#148086=CARTESIAN_POINT('Ctrl Pts',(39.3936386153616,-1.03178968344965,
89.2487913177301));
#148087=CARTESIAN_POINT('Ctrl Pts',(39.3880680095067,-1.12722013107941,
89.2333348457709));
#148088=CARTESIAN_POINT('Ctrl Pts',(39.3827970165748,-1.21751788827826,
89.2187096942936));
#148089=CARTESIAN_POINT('Ctrl Pts',(39.376796440701,-1.31198352671711,89.2020666380893));
#148090=CARTESIAN_POINT('Ctrl Pts',(39.3699907959889,-1.41044597584285,
89.18303073602));
#148091=CARTESIAN_POINT('Ctrl Pts',(39.3680156935601,-1.43902128804925,
89.1775062254112));
#148092=CARTESIAN_POINT('Ctrl Pts',(39.3659727708971,-1.46793290362972,
89.1717801833692));
#148093=CARTESIAN_POINT('Ctrl Pts',(39.3638601573462,-1.49717579541164,
89.165843500559));
#148094=CARTESIAN_POINT('Ctrl Pts',(39.3570424034594,-1.59154745132835,
89.1466848417087));
#148095=CARTESIAN_POINT('Ctrl Pts',(39.349498818428,-1.68937304753144,89.1253315940075));
#148096=CARTESIAN_POINT('Ctrl Pts',(39.3411664250101,-1.79045253825546,
89.1014834303828));
#148097=CARTESIAN_POINT('Ctrl Pts',(39.3332784622089,-1.88614068244171,
89.0789072727156));
#148098=CARTESIAN_POINT('Ctrl Pts',(39.3246835089933,-1.98474496992307,
89.0540948478411));
#148099=CARTESIAN_POINT('Ctrl Pts',(39.3153290594718,-2.08605049367797,
89.02680462528));
#148100=CARTESIAN_POINT('Ctrl Pts',(39.3125220352183,-2.1164496167415,89.0186155472978));
#148101=CARTESIAN_POINT('Ctrl Pts',(39.3096466338812,-2.14709164187481,
89.0102034744062));
#148102=CARTESIAN_POINT('Ctrl Pts',(39.3067014714057,-2.17796988374068,
89.0015622132242));
#148103=CARTESIAN_POINT('Ctrl Pts',(39.2953949077397,-2.29651234462463,
88.9683881623794));
#148104=CARTESIAN_POINT('Ctrl Pts',(39.2830597414625,-2.41853715928627,
88.931832687132));
#148105=CARTESIAN_POINT('Ctrl Pts',(39.2696208587223,-2.5438092321937,88.8915720104783));
#148106=CARTESIAN_POINT('Ctrl Pts',(39.2573429243572,-2.65825939287037,
88.8547893437193));
#148107=CARTESIAN_POINT('Ctrl Pts',(39.2441436631701,-2.77541978677909,
88.8149137769909));
#148108=CARTESIAN_POINT('Ctrl Pts',(39.2299712767101,-2.89509818012012,
88.771739172233));
#148109=CARTESIAN_POINT('Ctrl Pts',(39.2163617007677,-3.01002393291677,
88.730279107346));
#148110=CARTESIAN_POINT('Ctrl Pts',(39.2018546701449,-3.12727157407915,
88.6857764236995));
#148111=CARTESIAN_POINT('Ctrl Pts',(39.1864107197701,-3.24666035753036,
88.6380926390761));
#148112=CARTESIAN_POINT('Ctrl Pts',(39.1718165907419,-3.3594796341998,88.593032710207));
#148113=CARTESIAN_POINT('Ctrl Pts',(39.1563857726419,-3.47421079212239,
88.5451319765576));
#148114=CARTESIAN_POINT('Ctrl Pts',(39.1400916515551,-3.59069318020269,
88.4943174196277));
#148115=CARTESIAN_POINT('Ctrl Pts',(39.1242484391298,-3.7039521408009,88.4449090584498));
#148116=CARTESIAN_POINT('Ctrl Pts',(39.1075889810899,-3.81886668350723,
88.3927456112529));
#148117=CARTESIAN_POINT('Ctrl Pts',(39.0900961118598,-3.93528238987657,
88.3378061841039));
#148118=CARTESIAN_POINT('Ctrl Pts',(39.0698623223758,-4.06993902420666,
88.2742584156573));
#148119=CARTESIAN_POINT('Ctrl Pts',(39.0485138104168,-4.20660231927269,
88.2069983091697));
#148120=CARTESIAN_POINT('Ctrl Pts',(39.0260063500057,-4.34510209183181,
88.1359004735261));
#148121=CARTESIAN_POINT('Ctrl Pts',(39.0038129707741,-4.48166916424905,
88.0657947752304));
#148122=CARTESIAN_POINT('Ctrl Pts',(38.9804926658221,-4.62002153013926,
87.9919572692072));
#148123=CARTESIAN_POINT('Ctrl Pts',(38.956010639519,-4.76001118441306,87.9143169217427));
#148124=CARTESIAN_POINT('Ctrl Pts',(38.9329641196511,-4.89179252916653,
87.8412290250045));
#148125=CARTESIAN_POINT('Ctrl Pts',(38.9088880990889,-5.02502466824429,
87.7647711919074));
#148126=CARTESIAN_POINT('Ctrl Pts',(38.8837610666994,-5.15960032747597,
87.6849303671281));
#148127=CARTESIAN_POINT('Ctrl Pts',(38.8821959706719,-5.16798268741426,
87.6799572944723));
#148128=CARTESIAN_POINT('Ctrl Pts',(38.8806267996404,-5.17637026567736,
87.6749711124725));
#148129=CARTESIAN_POINT('Ctrl Pts',(38.8790535494728,-5.18476303873876,
87.669971824328));
#148130=CARTESIAN_POINT('Ctrl Pts',(38.8667928540052,-5.25016982321366,
87.6310112376653));
#148131=CARTESIAN_POINT('Ctrl Pts',(38.8542843732491,-5.31589201516666,
87.5912544160014));
#148132=CARTESIAN_POINT('Ctrl Pts',(38.8415264249196,-5.38191912340202,
87.5507045284967));
#148133=CARTESIAN_POINT('Ctrl Pts',(38.8351474507548,-5.4149326775197,87.5304295847443));
#148134=CARTESIAN_POINT('Ctrl Pts',(38.8287061320204,-5.4480224845055,87.5099564060667));
#148135=CARTESIAN_POINT('Ctrl Pts',(38.8222022899081,-5.4811873405972,87.4892856894754));
#148136=CARTESIAN_POINT('Ctrl Pts',(38.8189503688519,-5.49776976864305,
87.4789503311798));
#148137=CARTESIAN_POINT('Ctrl Pts',(38.8156828184417,-5.51437096051822,
87.4685655904894));
#148138=CARTESIAN_POINT('Ctrl Pts',(38.8123996220168,-5.53099077426008,
87.4581315703589));
#148139=CARTESIAN_POINT('Ctrl Pts',(38.8107580238043,-5.53930068113101,
87.4529145602937));
#148140=CARTESIAN_POINT('Ctrl Pts',(38.8091125141816,-5.54761524357118,
87.4476852305022));
#148141=CARTESIAN_POINT('Ctrl Pts',(38.8074630912624,-5.55593444431467,
87.4424435950278));
#148142=CARTESIAN_POINT('Ctrl Pts',(38.8066383798028,-5.56009404468641,
87.4398227772906));
#148143=CARTESIAN_POINT('Ctrl Pts',(38.805812690025,-5.5642548046405,87.4371988831411));
#148144=CARTESIAN_POINT('Ctrl Pts',(38.8049860217041,-5.5684167220486,87.4345719144101));
#148145=CARTESIAN_POINT('Ctrl Pts',(38.8041593533833,-5.5725786394567,87.4319449456791));
#148146=CARTESIAN_POINT('Ctrl Pts',(38.8035398266194,-5.57569581376081,
87.429976243687));
#148147=CARTESIAN_POINT('Ctrl Pts',(38.8025030809044,-5.58090594453013,
87.4266817863445));
#148148=CARTESIAN_POINT('Ctrl Pts',(38.7941338525687,-5.62296522043224,
87.4000869662815));
#148149=CARTESIAN_POINT('Ctrl Pts',(38.785795322314,-5.66453645375523,87.3735549895261));
#148150=CARTESIAN_POINT('Ctrl Pts',(38.7774907818068,-5.70562997173392,
87.3471006541145));
#148151=CARTESIAN_POINT('Ctrl Pts',(38.7517807423839,-5.83285145573393,
87.2652006374005));
#148152=CARTESIAN_POINT('Ctrl Pts',(38.7263971118217,-5.95549632462261,
87.1840477757184));
#148153=CARTESIAN_POINT('Ctrl Pts',(38.7014116402201,-6.07382542997955,
87.1039392551767));
#148154=CARTESIAN_POINT('Ctrl Pts',(38.6759210529494,-6.19454672093023,
87.0222112307251));
#148155=CARTESIAN_POINT('Ctrl Pts',(38.6508448633532,-6.31077597806947,
86.9415700268134));
#148156=CARTESIAN_POINT('Ctrl Pts',(38.6262499273492,-6.42276010232269,
86.8622868002747));
#148157=CARTESIAN_POINT('Ctrl Pts',(38.600834152501,-6.53848161865936,86.7803575513182));
#148158=CARTESIAN_POINT('Ctrl Pts',(38.5759322826389,-6.64966995204747,
86.6998783321325));
#148159=CARTESIAN_POINT('Ctrl Pts',(38.5516084311598,-6.75656543709959,
86.6211034109643));
#148160=CARTESIAN_POINT('Ctrl Pts',(38.5267820277867,-6.86566947569938,
86.5407009315176));
#148161=CARTESIAN_POINT('Ctrl Pts',(38.5025577418917,-6.97030138917467,
86.4620736868377));
#148162=CARTESIAN_POINT('Ctrl Pts',(38.4789941794526,-7.07068405749413,
86.3854485627193));
#148163=CARTESIAN_POINT('Ctrl Pts',(38.4546485284467,-7.17439848591595,
86.3062802054348));
#148164=CARTESIAN_POINT('Ctrl Pts',(38.431008169128,-7.27357690004313,86.2292489218633));
#148165=CARTESIAN_POINT('Ctrl Pts',(38.4081280055139,-7.36843108572141,
86.1545617683574));
#148166=CARTESIAN_POINT('Ctrl Pts',(38.3990610478215,-7.40601992918434,
86.1249647220937));
#148167=CARTESIAN_POINT('Ctrl Pts',(38.3901133666663,-7.4429293396309,86.0957353418035));
#148168=CARTESIAN_POINT('Ctrl Pts',(38.3812879877655,-7.47917110582456,
86.0668848138656));
#148169=CARTESIAN_POINT('Ctrl Pts',(38.3558773358293,-7.58352094923186,
85.983816343735));
#148170=CARTESIAN_POINT('Ctrl Pts',(38.3314812804312,-7.68233842547393,
85.9038911148172));
#148171=CARTESIAN_POINT('Ctrl Pts',(38.3081575920777,-7.7758529635305,85.8273073700796));
#148172=CARTESIAN_POINT('Ctrl Pts',(38.284046918763,-7.87252285737706,85.7481395462523));
#148173=CARTESIAN_POINT('Ctrl Pts',(38.2610821761243,-7.96352586312083,
85.6725423438921));
#148174=CARTESIAN_POINT('Ctrl Pts',(38.23931671923,-8.04907660758938,85.6006963800654));
#148175=CARTESIAN_POINT('Ctrl Pts',(38.2333882777533,-8.07237878701643,
85.5811270875876));
#148176=CARTESIAN_POINT('Ctrl Pts',(38.2275487544219,-8.09527625006559,
85.5618358942794));
#148177=CARTESIAN_POINT('Ctrl Pts',(38.2217991031176,-8.11777286689644,
85.5428260041036));
#148178=CARTESIAN_POINT('Ctrl Pts',(38.2114933540447,-8.15809609273672,
85.5087524320407));
#148179=CARTESIAN_POINT('Ctrl Pts',(38.2014763692145,-8.19713161021553,
85.4755827144277));
#148180=CARTESIAN_POINT('Ctrl Pts',(38.1917532454106,-8.23490019381938,
85.4433338928739));
#148181=CARTESIAN_POINT('Ctrl Pts',(38.1868916835087,-8.25378448562131,
85.4272094820971));
#148182=CARTESIAN_POINT('Ctrl Pts',(38.1821035743238,-8.27235201668672,
85.4113152672317));
#148183=CARTESIAN_POINT('Ctrl Pts',(38.1773895147866,-8.29060520596237,
85.3956532183678));
#148184=CARTESIAN_POINT('Ctrl Pts',(38.1750324850179,-8.29973180060019,
85.3878221939358));
#148185=CARTESIAN_POINT('Ctrl Pts',(38.1726939669064,-8.30877980817986,
85.3800492093379));
#148186=CARTESIAN_POINT('Ctrl Pts',(38.1703740314513,-8.31774952095548,
85.372334501168));
#148187=CARTESIAN_POINT('Ctrl Pts',(38.1692140637238,-8.32223437734328,
85.368477147083));
#148188=CARTESIAN_POINT('Ctrl Pts',(38.1680587416159,-8.32669965993112,
85.3646343620035));
#148189=CARTESIAN_POINT('Ctrl Pts',(38.1669080738451,-8.3311454045957,85.3608061749156));
#148190=CARTESIAN_POINT('Ctrl Pts',(38.1657574060743,-8.33559114926027,
85.3569779878277));
#148191=CARTESIAN_POINT('Ctrl Pts',(38.1650167285598,-8.33845237175655,
85.3545135513215));
#148192=CARTESIAN_POINT('Ctrl Pts',(38.1634700421177,-8.34442406028693,
85.3493654362194));
#148193=CARTESIAN_POINT('Ctrl Pts',(38.1209894227077,-8.50843986904196,
85.2079695382673));
#148194=CARTESIAN_POINT('Ctrl Pts',(38.0774939924553,-8.67347496440427,
85.0627533003965));
#148195=CARTESIAN_POINT('Ctrl Pts',(38.032998366253,-8.83954481212098,84.913779614927));
#148196=CARTESIAN_POINT('Ctrl Pts',(37.9948607039445,-8.9818849995149,84.786092725356));
#148197=CARTESIAN_POINT('Ctrl Pts',(37.955988367647,-9.12498584008693,84.6556458945396));
#148198=CARTESIAN_POINT('Ctrl Pts',(37.9163956452311,-9.26888020790597,
84.5224980340405));
#148199=CARTESIAN_POINT('Ctrl Pts',(37.8643469034322,-9.45804428503791,
84.3474613558498));
#148200=CARTESIAN_POINT('Ctrl Pts',(37.8110530695196,-9.64857949412737,
84.1677572350173));
#148201=CARTESIAN_POINT('Ctrl Pts',(37.7565315729619,-9.84047473256546,
83.9834084838153));
#148202=CARTESIAN_POINT('Ctrl Pts',(37.7036370545627,-10.0266436175219,
83.8045608910676));
#148203=CARTESIAN_POINT('Ctrl Pts',(37.6495870319644,-10.2140924789878,
83.6213416835189));
#148204=CARTESIAN_POINT('Ctrl Pts',(37.5944071466661,-10.4028513988054,
83.4337976900769));
#148205=CARTESIAN_POINT('Ctrl Pts',(37.5649595694911,-10.5035854403633,
83.3337120122845));
#148206=CARTESIAN_POINT('Ctrl Pts',(37.535190377774,-10.6046932838906,83.232395092593));
#148207=CARTESIAN_POINT('Ctrl Pts',(37.505104684855,-10.7061845463452,83.1298573144579));
#148208=CARTESIAN_POINT('Ctrl Pts',(39.6168697557491,-0.401447571728686,
89.09878183643));
#148209=CARTESIAN_POINT('Ctrl Pts',(39.6164986632191,-0.423699213959886,
89.0966772661));
#148210=CARTESIAN_POINT('Ctrl Pts',(39.6062991625191,-1.00745211277799,
89.03883302323));
#148211=CARTESIAN_POINT('Ctrl Pts',(39.5603644817491,-2.20004318169699,
88.77832450325));
#148212=CARTESIAN_POINT('Ctrl Pts',(39.4305948837391,-3.89800233267899,
88.04236454135));
#148213=CARTESIAN_POINT('Ctrl Pts',(39.2432936369891,-5.59810631869199,
86.98012638587));
#148214=CARTESIAN_POINT('Ctrl Pts',(39.0062523874891,-7.30762248550998,
85.6357986570799));
#148215=CARTESIAN_POINT('Ctrl Pts',(38.7409445539891,-8.95066677755598,
84.13116316432));
#148216=CARTESIAN_POINT('Ctrl Pts',(38.5531406949991,-10.01036398978,83.0660745532));
#148217=CARTESIAN_POINT('Ctrl Pts',(38.4618769343391,-10.51042279016,82.54849204656));
#148218=CARTESIAN_POINT('Ctrl Pts',(38.5589532493791,-0.521574169437586,
90.55113115247));
#148219=CARTESIAN_POINT('Ctrl Pts',(38.5585212780491,-0.547502548905586,
90.54868132133));
#148220=CARTESIAN_POINT('Ctrl Pts',(38.5466482255191,-1.22751162701999,
90.48134589437));
#148221=CARTESIAN_POINT('Ctrl Pts',(38.4932267806791,-2.60548887972399,
90.1783778255));
#148222=CARTESIAN_POINT('Ctrl Pts',(38.3476657190791,-4.50165028275699,
89.35286002319));
#148223=CARTESIAN_POINT('Ctrl Pts',(38.1451917885991,-6.335462567224,88.2045733022701));
#148224=CARTESIAN_POINT('Ctrl Pts',(37.8958275904891,-8.13206152847199,
86.79035865909));
#148225=CARTESIAN_POINT('Ctrl Pts',(37.6219025168191,-9.82769184312899,
85.2368523688499));
#148226=CARTESIAN_POINT('Ctrl Pts',(37.4302304055891,-10.90908042546,84.1498258091));
#148227=CARTESIAN_POINT('Ctrl Pts',(37.3374134759791,-11.41764050787,83.62343484366));
#148228=CARTESIAN_POINT('Ctrl Pts',(36.8542747409091,-0.438522368068186,
89.97657015498));
#148229=CARTESIAN_POINT('Ctrl Pts',(36.8538848592891,-0.461908765523086,
89.97435902645));
#148230=CARTESIAN_POINT('Ctrl Pts',(36.8431688485591,-1.07536930870899,
89.91358550959));
#148231=CARTESIAN_POINT('Ctrl Pts',(36.7949235200291,-2.32517630764799,
89.63997265504));
#148232=CARTESIAN_POINT('Ctrl Pts',(36.6602801862491,-4.08430682507998,
88.8763723640501));
#148233=CARTESIAN_POINT('Ctrl Pts',(36.4682961783991,-5.82567734180799,
87.78757695064));
#148234=CARTESIAN_POINT('Ctrl Pts',(36.2274516844991,-7.56206996171599,
86.42167995104));
#148235=CARTESIAN_POINT('Ctrl Pts',(35.9594843032291,-9.22134393241599,
84.9019614134));
#148236=CARTESIAN_POINT('Ctrl Pts',(35.7704865815491,-10.28773577467,83.83010207047));
#148237=CARTESIAN_POINT('Ctrl Pts',(35.6787434647391,-10.79041833453,83.30980100006));
#148238=CARTESIAN_POINT('Ctrl Pts',(36.9040323489391,-0.269278349005186,
88.1844214108399));
#148239=CARTESIAN_POINT('Ctrl Pts',(36.9037282382691,-0.287484663123986,
88.1826967135399));
#148240=CARTESIAN_POINT('Ctrl Pts',(36.8953700620491,-0.765331753880986,
88.1352951406999));
#148241=CARTESIAN_POINT('Ctrl Pts',(36.8576726892891,-1.75395177657199,
87.92150271593));
#148242=CARTESIAN_POINT('Ctrl Pts',(36.7452776403791,-3.23383900930099,
87.28407871843));
#148243=CARTESIAN_POINT('Ctrl Pts',(36.5746701305291,-4.78683051385399,
86.31651544951));
#148244=CARTESIAN_POINT('Ctrl Pts',(36.3511871984191,-6.40053388423998,
85.04908075965));
#148245=CARTESIAN_POINT('Ctrl Pts',(36.0953604786391,-7.98572043397698,
83.5982153347901));
#148246=CARTESIAN_POINT('Ctrl Pts',(35.9118126620491,-9.02155172821997,
82.55726393953));
#148247=CARTESIAN_POINT('Ctrl Pts',(35.8222577746591,-9.51225699775298,
82.049372934817));
#148248=CARTESIAN_POINT('',(35.848007777729,-9.62145567905125,82.3699746323318));
#148249=CARTESIAN_POINT('Ctrl Pts',(37.5051004487691,-10.70616518419,83.12983477216));
#148250=CARTESIAN_POINT('Ctrl Pts',(36.5978347423554,-10.7058101101168,
83.2902037073864));
#148251=CARTESIAN_POINT('Ctrl Pts',(35.9481946009574,-10.2251893971186,
82.9382716566004));
#148252=CARTESIAN_POINT('Ctrl Pts',(35.8480077820191,-9.62145570514599,
82.369974656902));
#148253=CARTESIAN_POINT('',(36.9231078832491,-0.454164387253686,88.46717031284));
#148254=CARTESIAN_POINT('Ctrl Pts',(36.9231078836017,-0.454164387253684,
88.4671703127778));
#148255=CARTESIAN_POINT('Ctrl Pts',(36.9204855400661,-0.579215517453633,
88.4522982635594));
#148256=CARTESIAN_POINT('Ctrl Pts',(36.9172067488959,-0.705401523346811,
88.4337033100507));
#148257=CARTESIAN_POINT('Ctrl Pts',(36.91324787678,-0.832819212190252,88.41125141964));
#148258=CARTESIAN_POINT('Ctrl Pts',(36.9093083236504,-0.959615112677564,
88.3889090926985));
#148259=CARTESIAN_POINT('Ctrl Pts',(36.9046952253662,-1.0876312092335,88.3627468944092));
#148260=CARTESIAN_POINT('Ctrl Pts',(36.8993790061486,-1.21692649295543,
88.3325971105308));
#148261=CARTESIAN_POINT('Ctrl Pts',(36.8941653038762,-1.34372847138129,
88.3030287292655));
#148262=CARTESIAN_POINT('Ctrl Pts',(36.8882752386231,-1.47176119273405,
88.2696245200025));
#148263=CARTESIAN_POINT('Ctrl Pts',(36.881676227213,-1.60103855818878,88.2321996896396));
#148264=CARTESIAN_POINT('Ctrl Pts',(36.8786089337181,-1.66112810758537,
88.214804214532));
#148265=CARTESIAN_POINT('Ctrl Pts',(36.8753884149429,-1.72148592772201,
88.1965397574779));
#148266=CARTESIAN_POINT('Ctrl Pts',(36.8720111362573,-1.78210985327536,
88.1773862624852));
#148267=CARTESIAN_POINT('Ctrl Pts',(36.8713476061124,-1.79402056774533,
88.1736231968658));
#148268=CARTESIAN_POINT('Ctrl Pts',(36.8706780245898,-1.80594154616967,
88.1698258118269));
#148269=CARTESIAN_POINT('Ctrl Pts',(36.8700023719187,-1.81787287878656,
88.1659939951173));
#148270=CARTESIAN_POINT('Ctrl Pts',(36.862917561535,-1.94298335764443,88.1258140387938));
#148271=CARTESIAN_POINT('Ctrl Pts',(36.8551789643605,-2.06925582542825,
88.0819262305807));
#148272=CARTESIAN_POINT('Ctrl Pts',(36.846783675606,-2.19653931916896,88.0343141627442));
#148273=CARTESIAN_POINT('Ctrl Pts',(36.8384573156836,-2.3227777621871,87.9870930098994));
#148274=CARTESIAN_POINT('Ctrl Pts',(36.8294849882894,-2.45001066457938,
87.9362084117139));
#148275=CARTESIAN_POINT('Ctrl Pts',(36.8198726336355,-2.57808496455812,
87.8816940519132));
#148276=CARTESIAN_POINT('Ctrl Pts',(36.8103596902718,-2.70483471588556,
87.8277434814267));
#148277=CARTESIAN_POINT('Ctrl Pts',(36.8002198826719,-2.83240851462995,
87.7702377975226));
#148278=CARTESIAN_POINT('Ctrl Pts',(36.7894677550147,-2.96065282739329,
87.7092594667506));
#148279=CARTESIAN_POINT('Ctrl Pts',(36.7808506229816,-3.06343231539864,
87.660389294802));
#148280=CARTESIAN_POINT('Ctrl Pts',(36.7718403631796,-3.16664236853377,
87.609289579579));
#148281=CARTESIAN_POINT('Ctrl Pts',(36.7624486466323,-3.27020175607686,
87.556026508269));
#148282=CARTESIAN_POINT('Ctrl Pts',(36.7613578466867,-3.28222965041635,
87.5498402743687));
#148283=CARTESIAN_POINT('Ctrl Pts',(36.7602618544229,-3.2942624067366,87.5436245932785));
#148284=CARTESIAN_POINT('Ctrl Pts',(36.7591606886614,-3.30629995569941,
87.5373795717616));
#148285=CARTESIAN_POINT('Ctrl Pts',(36.7454949420224,-3.45568899414377,
87.4598772693939));
#148286=CARTESIAN_POINT('Ctrl Pts',(36.7310316990482,-3.6058155140173,87.3778521356401));
#148287=CARTESIAN_POINT('Ctrl Pts',(36.7157841777847,-3.75665276525037,
87.2913791460365));
#148288=CARTESIAN_POINT('Ctrl Pts',(36.7008648563705,-3.90424327478115,
87.2067674702607));
#148289=CARTESIAN_POINT('Ctrl Pts',(36.6851946205673,-4.05251425759033,
87.1178971509139));
#148290=CARTESIAN_POINT('Ctrl Pts',(36.6687943330814,-4.20144801214735,
87.0248865006242));
#148291=CARTESIAN_POINT('Ctrl Pts',(36.6528740097125,-4.34602313225598,
86.9345978620479));
#148292=CARTESIAN_POINT('Ctrl Pts',(36.6362657192849,-4.49122280935251,
86.840407566456));
#148293=CARTESIAN_POINT('Ctrl Pts',(36.6189970158369,-4.63703770276595,
86.7424718825201));
#148294=CARTESIAN_POINT('Ctrl Pts',(36.6134116009886,-4.68420028640901,
86.7107954208286));
#148295=CARTESIAN_POINT('Ctrl Pts',(36.6077571665088,-4.7314272847846,86.6787275293833));
#148296=CARTESIAN_POINT('Ctrl Pts',(36.6020348484833,-4.77871854018616,
86.6462746511988));
#148297=CARTESIAN_POINT('Ctrl Pts',(36.5974580311413,-4.81654297372506,
86.6203182302154));
#148298=CARTESIAN_POINT('Ctrl Pts',(36.5928372138935,-4.85440937352727,
86.5941122733467));
#148299=CARTESIAN_POINT('Ctrl Pts',(36.5881730494456,-4.89231733944232,
86.5676604823064));
#148300=CARTESIAN_POINT('Ctrl Pts',(36.5685170244251,-5.05207155369143,
86.4561856249483));
#148301=CARTESIAN_POINT('Ctrl Pts',(36.5480905445439,-5.21256245260813,
86.3403413012061));
#148302=CARTESIAN_POINT('Ctrl Pts',(36.5269096847282,-5.37380385031308,
86.2202186747469));
#148303=CARTESIAN_POINT('Ctrl Pts',(36.5060987806526,-5.53222892322571,
86.1021941715726));
#148304=CARTESIAN_POINT('Ctrl Pts',(36.4845595894665,-5.6913784719199,85.980039345428));
#148305=CARTESIAN_POINT('Ctrl Pts',(36.4623154504218,-5.85128432563395,
85.8538865639369));
#148306=CARTESIAN_POINT('Ctrl Pts',(36.4400713113771,-6.011190179348,85.7277337824458));
#148307=CARTESIAN_POINT('Ctrl Pts',(36.4171221689588,-6.17185223853716,
85.5975827335966));
#148308=CARTESIAN_POINT('Ctrl Pts',(36.3935001965489,-6.33332230407614,
85.4636158709251));
#148309=CARTESIAN_POINT('Ctrl Pts',(36.3839537583239,-6.39857782038479,
85.4094753293783));
#148310=CARTESIAN_POINT('Ctrl Pts',(36.3742956241308,-6.46396357224032,
85.3547013272084));
#148311=CARTESIAN_POINT('Ctrl Pts',(36.3645278890673,-6.52948729328553,
85.2993057480396));
#148312=CARTESIAN_POINT('Ctrl Pts',(36.33721729842,-6.71269164019927,85.1444196893474));
#148313=CARTESIAN_POINT('Ctrl Pts',(36.3090494265076,-6.89697275943275,
84.9846717516336));
#148314=CARTESIAN_POINT('Ctrl Pts',(36.2800326420702,-7.08247408334454,
84.8201093911229));
#148315=CARTESIAN_POINT('Ctrl Pts',(36.2523166598315,-7.25965951234608,
84.662924246404));
#148316=CARTESIAN_POINT('Ctrl Pts',(36.2238261451942,-7.43795816874329,
84.5013465077463));
#148317=CARTESIAN_POINT('Ctrl Pts',(36.1945754362192,-7.61751897861946,
84.3354574934946));
#148318=CARTESIAN_POINT('Ctrl Pts',(36.1770708801192,-7.72497388757679,
84.2361842225859));
#148319=CARTESIAN_POINT('Ctrl Pts',(36.1592942197124,-7.83288126073805,
84.1353677724498));
#148320=CARTESIAN_POINT('Ctrl Pts',(36.1412498888878,-7.94127751027461,
84.0330332870971));
#148321=CARTESIAN_POINT('Ctrl Pts',(36.1254304032814,-8.03630862702806,
83.9433165259818));
#148322=CARTESIAN_POINT('Ctrl Pts',(36.1094026818148,-8.13170908607084,
83.8524187996686));
#148323=CARTESIAN_POINT('Ctrl Pts',(36.0931717062841,-8.22749574121146,
83.7603683628236));
#148324=CARTESIAN_POINT('Ctrl Pts',(36.0600954702211,-8.42269423751378,
83.572783705757));
#148325=CARTESIAN_POINT('Ctrl Pts',(36.0261748143884,-8.61949496237244,
83.380410108411));
#148326=CARTESIAN_POINT('Ctrl Pts',(35.9914249486467,-8.81798075492089,
83.1833338271658));
#148327=CARTESIAN_POINT('Ctrl Pts',(35.9576129973166,-9.01110932719348,
82.9915767228563));
#148328=CARTESIAN_POINT('Ctrl Pts',(35.9230159764349,-9.20583318997005,
82.795367266301));
#148329=CARTESIAN_POINT('Ctrl Pts',(35.8876549358059,-9.40225689693438,
82.5948248385148));
#148330=CARTESIAN_POINT('Ctrl Pts',(35.8745437364782,-9.4750870605519,82.5204675317842));
#148331=CARTESIAN_POINT('Ctrl Pts',(35.8613275731665,-9.54815120444581,
82.4455149448095));
#148332=CARTESIAN_POINT('Ctrl Pts',(35.84800778227,-9.62145570514599,82.3699746568577));
#148333=CARTESIAN_POINT('Ctrl Pts',(39.4126085609146,-0.605361527076818,
89.303184116066));
#148334=CARTESIAN_POINT('Ctrl Pts',(39.3830826694109,-0.607949740687352,
89.3300849028713));
#148335=CARTESIAN_POINT('Ctrl Pts',(39.3517747790665,-0.610432005932147,
89.3564534797));
#148336=CARTESIAN_POINT('Ctrl Pts',(39.3186428950151,-0.612776874303673,
89.3820233316278));
#148337=CARTESIAN_POINT('Ctrl Pts',(39.2863134838357,-0.615064948643988,
89.4069738673561));
#148338=CARTESIAN_POINT('Ctrl Pts',(39.2522468551104,-0.617222132514938,
89.4311634103301));
#148339=CARTESIAN_POINT('Ctrl Pts',(39.2164458244507,-0.619217002864159,
89.4543179667453));
#148340=CARTESIAN_POINT('Ctrl Pts',(39.181806346853,-0.621147150278882,
89.4767212809363));
#148341=CARTESIAN_POINT('Ctrl Pts',(39.145542886646,-0.622925266528472,
89.4981550600761));
#148342=CARTESIAN_POINT('Ctrl Pts',(39.1077034021859,-0.624521879320095,
89.5183542503743));
#148343=CARTESIAN_POINT('Ctrl Pts',(39.070516042106,-0.626090976141504,
89.5382053285181));
#148344=CARTESIAN_POINT('Ctrl Pts',(39.031806250036,-0.6274846871524,89.5568633344759));
#148345=CARTESIAN_POINT('Ctrl Pts',(38.9916684203604,-0.62867524175512,
89.574069494001));
#148346=CARTESIAN_POINT('Ctrl Pts',(38.9524709787942,-0.629837902886744,
89.5908725308871));
#148347=CARTESIAN_POINT('Ctrl Pts',(38.9119116024645,-0.630806730929495,
89.6062902404851));
#148348=CARTESIAN_POINT('Ctrl Pts',(38.8701272580662,-0.631557299395677,
89.6200848773503));
#148349=CARTESIAN_POINT('Ctrl Pts',(38.836450628922,-0.63216222969306,89.6312028421426));
#148350=CARTESIAN_POINT('Ctrl Pts',(38.801979225164,-0.632625389896376,
89.6412663788308));
#148351=CARTESIAN_POINT('Ctrl Pts',(38.766808573118,-0.632935279074347,
89.6501576115731));
#148352=CARTESIAN_POINT('Ctrl Pts',(38.7243785122306,-0.633309131019783,
89.6608840418402));
#148353=CARTESIAN_POINT('Ctrl Pts',(38.6809298997421,-0.633459689529876,
89.6699030852832));
#148354=CARTESIAN_POINT('Ctrl Pts',(38.6366711021073,-0.633369300936823,
89.6770286079621));
#148355=CARTESIAN_POINT('Ctrl Pts',(38.5928762441042,-0.633279859835633,
89.684079437867));
#148356=CARTESIAN_POINT('Ctrl Pts',(38.5482885036326,-0.632954428539797,
89.6892755904881));
#148357=CARTESIAN_POINT('Ctrl Pts',(38.503149051083,-0.632380513370048,
89.6924686713012));
#148358=CARTESIAN_POINT('Ctrl Pts',(38.4585245181781,-0.631813145027487,
89.6956253276575));
#148359=CARTESIAN_POINT('Ctrl Pts',(38.4133613629055,-0.6310028806348,89.6968238366789));
#148360=CARTESIAN_POINT('Ctrl Pts',(38.3679238893794,-0.629943047301416,
89.6959608290385));
#148361=CARTESIAN_POINT('Ctrl Pts',(38.361206822858,-0.629786371094542,
89.695833249768));
#148362=CARTESIAN_POINT('Ctrl Pts',(38.3544838081868,-0.62962425123485,
89.6956606977974));
#148363=CARTESIAN_POINT('Ctrl Pts',(38.3477557452501,-0.629456677211184,
89.6954429242308));
#148364=CARTESIAN_POINT('Ctrl Pts',(38.3027202313773,-0.62833498998285,
89.6939852172245));
#148365=CARTESIAN_POINT('Ctrl Pts',(38.2574572497619,-0.626968432168449,
89.6904973541722));
#148366=CARTESIAN_POINT('Ctrl Pts',(38.2122466402006,-0.625357297113154,
89.6849323266811));
#148367=CARTESIAN_POINT('Ctrl Pts',(38.1672370341778,-0.623753325063409,
89.6793920409537));
#148368=CARTESIAN_POINT('Ctrl Pts',(38.1222800998557,-0.621906940809301,
89.6717928435791));
#148369=CARTESIAN_POINT('Ctrl Pts',(38.0776608857395,-0.619824596328343,
89.6621387514638));
#148370=CARTESIAN_POINT('Ctrl Pts',(38.0331730893736,-0.617748385012941,
89.6525130937146));
#148371=CARTESIAN_POINT('Ctrl Pts',(37.9890218157171,-0.61543762055268,
89.6408446505096));
#148372=CARTESIAN_POINT('Ctrl Pts',(37.9454868331697,-0.61290473306776,
89.6271887923972));
#148373=CARTESIAN_POINT('Ctrl Pts',(37.9355265063314,-0.612325236173121,
89.6240644817372));
#148374=CARTESIAN_POINT('Ctrl Pts',(37.9255983994401,-0.611734136535927,
89.6208363517161));
#148375=CARTESIAN_POINT('Ctrl Pts',(37.9157057758992,-0.6111316252669,89.6175054371492));
#148376=CARTESIAN_POINT('Ctrl Pts',(37.8724267966282,-0.608495714518348,
89.6029331063716));
#148377=CARTESIAN_POINT('Ctrl Pts',(37.8298286826496,-0.605640984164935,
89.5863897887462));
#148378=CARTESIAN_POINT('Ctrl Pts',(37.7881725496278,-0.602586648415914,
89.567991787781));
#148379=CARTESIAN_POINT('Ctrl Pts',(37.7464396078346,-0.5995266808485,89.5495598631713));
#148380=CARTESIAN_POINT('Ctrl Pts',(37.7056527864113,-0.59626643688015,
89.5292668474361));
#148381=CARTESIAN_POINT('Ctrl Pts',(37.6660467507015,-0.592829880871123,
89.507273757858));
#148382=CARTESIAN_POINT('Ctrl Pts',(37.6262056706644,-0.589372930420163,
89.4851501490079));
#148383=CARTESIAN_POINT('Ctrl Pts',(37.5875599780202,-0.585737648835415,
89.4613068050183));
#148384=CARTESIAN_POINT('Ctrl Pts',(37.5503111464723,-0.58195202546577,
89.4359445295695));
#148385=CARTESIAN_POINT('Ctrl Pts',(37.541937453631,-0.581101001527752,
89.4302429841641));
#148386=CARTESIAN_POINT('Ctrl Pts',(37.5336341875282,-0.580242391247806,
89.4244648026186));
#148387=CARTESIAN_POINT('Ctrl Pts',(37.5254033402407,-0.579376530745491,
89.4186124714025));
#148388=CARTESIAN_POINT('Ctrl Pts',(37.4883253743076,-0.575476039691987,
89.3922491421023));
#148389=CARTESIAN_POINT('Ctrl Pts',(37.4527208525358,-0.571428301082649,
89.3643794486022));
#148390=CARTESIAN_POINT('Ctrl Pts',(37.4187425064932,-0.56726506356026,
89.3352448517187));
#148391=CARTESIAN_POINT('Ctrl Pts',(37.3844890561168,-0.563068118550058,
89.3058743677247));
#148392=CARTESIAN_POINT('Ctrl Pts',(37.3518883561261,-0.55875389246498,
89.2752191981415));
#148393=CARTESIAN_POINT('Ctrl Pts',(37.3210457848244,-0.554355573082808,
89.2435412610773));
#148394=CARTESIAN_POINT('Ctrl Pts',(37.2897623391319,-0.549894382600837,
89.2114105086147));
#148395=CARTESIAN_POINT('Ctrl Pts',(37.2602876182062,-0.545346770319937,
89.1782283273344));
#148396=CARTESIAN_POINT('Ctrl Pts',(37.2326783053699,-0.54074660372001,
89.1442709319909));
#148397=CARTESIAN_POINT('Ctrl Pts',(37.2288889262586,-0.540115230700122,
89.1396102783429));
#148398=CARTESIAN_POINT('Ctrl Pts',(37.2251346069408,-0.539482865285731,
89.1349350153405));
#148399=CARTESIAN_POINT('Ctrl Pts',(37.2214154186073,-0.538849592483184,
89.1302458487828));
#148400=CARTESIAN_POINT('Ctrl Pts',(37.193700854511,-0.534130584435423,
89.0953032227386));
#148401=CARTESIAN_POINT('Ctrl Pts',(37.1679412772532,-0.529361330935144,
89.0595897996328));
#148402=CARTESIAN_POINT('Ctrl Pts',(37.144136481793,-0.524575905972413,
89.0233898608578));
#148403=CARTESIAN_POINT('Ctrl Pts',(37.1199332686332,-0.519710387987728,
88.986584048516));
#148404=CARTESIAN_POINT('Ctrl Pts',(37.0977503832959,-0.514828222470887,
88.9492759630769));
#148405=CARTESIAN_POINT('Ctrl Pts',(37.0775381404591,-0.509961568520209,
88.9117425176981));
#148406=CARTESIAN_POINT('Ctrl Pts',(37.0567000583587,-0.50494422653606,
88.8730469101579));
#148407=CARTESIAN_POINT('Ctrl Pts',(37.0379560348227,-0.49994343426556,
88.834112388713));
#148408=CARTESIAN_POINT('Ctrl Pts',(37.021206637527,-0.494989533180578,
88.79520925528));
#148409=CARTESIAN_POINT('Ctrl Pts',(37.0041561906232,-0.489946591877963,
88.7556068863539));
#148410=CARTESIAN_POINT('Ctrl Pts',(36.9891719984924,-0.484952271510473,
88.7160374157217));
#148411=CARTESIAN_POINT('Ctrl Pts',(36.9761129012183,-0.480032883108771,
88.6767445821553));
#148412=CARTESIAN_POINT('Ctrl Pts',(36.962628390604,-0.474953240639975,
88.6361717446794));
#148413=CARTESIAN_POINT('Ctrl Pts',(36.9511957079229,-0.469953510914846,
88.5958941545307));
#148414=CARTESIAN_POINT('Ctrl Pts',(36.9416322998081,-0.465056243063057,
88.5561310553602));
#148415=CARTESIAN_POINT('Ctrl Pts',(36.9344242400316,-0.461365111303961,
88.526161112398));
#148416=CARTESIAN_POINT('Ctrl Pts',(36.9282774544592,-0.457732046663515,
88.4964823808057));
#148417=CARTESIAN_POINT('Ctrl Pts',(36.9231078836017,-0.454164387253685,
88.4671703127778));
#148418=CARTESIAN_POINT('Ctrl Pts',(39.6230428380891,0.194165912825814,
89.10440256372));
#148419=CARTESIAN_POINT('Ctrl Pts',(39.6230835571391,0.188318965759814,
89.1046334929299));
#148420=CARTESIAN_POINT('Ctrl Pts',(39.6238267343091,0.0765431320962642,
89.10884826011));
#148421=CARTESIAN_POINT('Ctrl Pts',(39.6239646769391,-0.140676791074186,
89.10963057164));
#148422=CARTESIAN_POINT('Ctrl Pts',(39.6205750423291,-0.456053684225086,
89.0904069985));
#148423=CARTESIAN_POINT('Ctrl Pts',(39.6159638777391,-0.665968720299886,
89.06425578459));
#148424=CARTESIAN_POINT('Ctrl Pts',(39.6130667616891,-0.771133841521687,
89.0478254230199));
#148425=CARTESIAN_POINT('Ctrl Pts',(39.6130033270391,-0.773426316473186,
89.04746566723));
#148426=CARTESIAN_POINT('Ctrl Pts',(38.5691068518391,0.244771599243314,
90.5717118808201));
#148427=CARTESIAN_POINT('Ctrl Pts',(38.5691581710291,0.237403022922614,
90.5720029264299));
#148428=CARTESIAN_POINT('Ctrl Pts',(38.5700948214891,0.0965319925331742,
90.57731493513));
#148429=CARTESIAN_POINT('Ctrl Pts',(38.5702688861991,-0.177441261231286,
90.5783021051901));
#148430=CARTESIAN_POINT('Ctrl Pts',(38.5659956750091,-0.574725948486886,
90.5540675202501));
#148431=CARTESIAN_POINT('Ctrl Pts',(38.5602096181291,-0.837927759919986,
90.5212531610201));
#148432=CARTESIAN_POINT('Ctrl Pts',(38.5565902006391,-0.969313074494586,
90.50072642442));
#148433=CARTESIAN_POINT('Ctrl Pts',(38.5565109568191,-0.972176888914785,
90.50027701038));
#148434=CARTESIAN_POINT('Ctrl Pts',(36.8563477221291,0.210105182233614,
89.99587069318));
#148435=CARTESIAN_POINT('Ctrl Pts',(36.8563917799091,0.203778967710814,
89.99612055725));
#148436=CARTESIAN_POINT('Ctrl Pts',(36.8571958953491,0.0828390220290842,
90.00068092251));
#148437=CARTESIAN_POINT('Ctrl Pts',(36.8573452153491,-0.152256493592886,
90.0015277583201));
#148438=CARTESIAN_POINT('Ctrl Pts',(36.8536772806891,-0.493431878756386,
89.98072586715));
#148439=CARTESIAN_POINT('Ctrl Pts',(36.8486960603491,-0.720130646629686,
89.95247596284));
#148440=CARTESIAN_POINT('Ctrl Pts',(36.8455714410691,-0.833554340264386,
89.93475536632));
#148441=CARTESIAN_POINT('Ctrl Pts',(36.8455030270091,-0.836026769967186,
89.93436737088));
#148442=CARTESIAN_POINT('Ctrl Pts',(36.9051284241591,0.139155051791214,
88.19062138055));
#148443=CARTESIAN_POINT('Ctrl Pts',(36.9051576203291,0.134962190291614,
88.19078696029));
#148444=CARTESIAN_POINT('Ctrl Pts',(36.9056904825591,0.0548142612602442,
88.19380897218));
#148445=CARTESIAN_POINT('Ctrl Pts',(36.9057891587191,-0.100712010394486,
88.1943685924501));
#148446=CARTESIAN_POINT('Ctrl Pts',(36.9033600151491,-0.327051117515386,
88.1805922347));
#148447=CARTESIAN_POINT('Ctrl Pts',(36.9000260160591,-0.479040817491986,
88.16168418626));
#148448=CARTESIAN_POINT('Ctrl Pts',(36.8979140770691,-0.555703303635986,
88.14970678509));
#148449=CARTESIAN_POINT('Ctrl Pts',(36.8978678277591,-0.557374704586886,
88.14944449221));
#148450=CARTESIAN_POINT('',(36.9278603430303,-1.00177063435092E-6,88.4941228548076));
#148451=CARTESIAN_POINT('Ctrl Pts',(36.9278603430291,-2.97267519524715E-6,
88.4941228548));
#148452=CARTESIAN_POINT('Ctrl Pts',(36.9278604219491,-0.0762479038749758,
88.49412330237));
#148453=CARTESIAN_POINT('Ctrl Pts',(36.9270606224491,-0.228190456260686,
88.4895874156));
#148454=CARTESIAN_POINT('Ctrl Pts',(36.9246749306291,-0.379014038241186,
88.47605748015));
#148455=CARTESIAN_POINT('Ctrl Pts',(36.9231078832491,-0.454164387253686,
88.46717031284));
#148456=CARTESIAN_POINT('',(39.4241793029232,-9.78010097509158E-7,89.3342949669387));
#148457=CARTESIAN_POINT('Origin',(38.4050719433491,9.69735768033255E-7,
88.23365042271));
#148458=CARTESIAN_POINT('Origin',(36.6903869784213,-0.361278919426404,81.9235440633504));
#148459=CARTESIAN_POINT('Ctrl Pts',(36.2786061953091,0.207874208027314,
99.1854858506699));
#148460=CARTESIAN_POINT('Ctrl Pts',(36.2804402733591,0.0518199014528942,
99.18628534125));
#148461=CARTESIAN_POINT('Ctrl Pts',(36.2798690360391,-0.330489837835886,
99.18604356481));
#148462=CARTESIAN_POINT('Ctrl Pts',(36.2628587211991,-0.832940233787786,
99.1786077462799));
#148463=CARTESIAN_POINT('Ctrl Pts',(36.2409501422491,-1.18047906866699,
99.16880011873));
#148464=CARTESIAN_POINT('Ctrl Pts',(36.2321464823691,-1.30088361809899,
99.16482121612));
#148465=CARTESIAN_POINT('Ctrl Pts',(34.9573762488691,0.103201196527414,
92.86118521246));
#148466=CARTESIAN_POINT('Ctrl Pts',(34.9589714992491,0.0257039272848542,
92.86073498844));
#148467=CARTESIAN_POINT('Ctrl Pts',(34.9584734757791,-0.163964725101886,
92.8608772735799));
#148468=CARTESIAN_POINT('Ctrl Pts',(34.9436819944391,-0.413997315175786,
92.86504889005));
#148469=CARTESIAN_POINT('Ctrl Pts',(34.9246064026991,-0.588616325050186,
92.8700772173199));
#148470=CARTESIAN_POINT('Ctrl Pts',(34.9169358794491,-0.649381969463186,
92.87203589546));
#148471=CARTESIAN_POINT('Ctrl Pts',(38.6633388710591,0.0807359298002742,
87.56791503177));
#148472=CARTESIAN_POINT('Ctrl Pts',(38.6653943621291,0.0201178049123542,
87.56771699648));
#148473=CARTESIAN_POINT('Ctrl Pts',(38.6647586993891,-0.128317194034386,
87.5677800351001));
#148474=CARTESIAN_POINT('Ctrl Pts',(38.6456800868891,-0.323682344850186,
87.56961385163));
#148475=CARTESIAN_POINT('Ctrl Pts',(38.6212145471391,-0.459440396730986,
87.57177962771));
#148476=CARTESIAN_POINT('Ctrl Pts',(38.6114058460491,-0.506574295099986,
87.57261479282));
#148477=CARTESIAN_POINT('Ctrl Pts',(45.0583801383591,0.154651878623914,
86.6452310386901));
#148478=CARTESIAN_POINT('Ctrl Pts',(45.0613045698591,0.0385858522600842,
86.6466279881101));
#148479=CARTESIAN_POINT('Ctrl Pts',(45.0604072521791,-0.246037484612986,
86.64619846919));
#148480=CARTESIAN_POINT('Ctrl Pts',(45.0332403204891,-0.618975576296886,
86.6332241827699));
#148481=CARTESIAN_POINT('Ctrl Pts',(44.9985624478491,-0.874449147389286,
86.6166349022499));
#148482=CARTESIAN_POINT('Ctrl Pts',(44.9846932436191,-0.962558808579585,
86.6099942916699));
#148483=CARTESIAN_POINT('Origin',(46.5579300163491,-6.05980869095053E-8,
97.03881113036));
#148484=CARTESIAN_POINT('Origin',(-15.5675364833309,-75.,72.98888938658));
#148485=CARTESIAN_POINT('',(-15.5675364833309,-86.22497216032,82.938763757646));
#148486=CARTESIAN_POINT('',(-15.5675364833309,-63.77502783969,82.938763757662));
#148487=CARTESIAN_POINT('Origin',(-15.5675364833309,-75.,72.98888938658));
#148488=CARTESIAN_POINT('',(-15.5675364833309,-63.77502783968,63.039015015514));
#148489=CARTESIAN_POINT('Ctrl Pts',(-15.5675364833309,-63.7750278396901,
82.938763757662));
#148490=CARTESIAN_POINT('Ctrl Pts',(-15.5675364833309,-62.6179303673713,
81.6333817569256));
#148491=CARTESIAN_POINT('Ctrl Pts',(-15.5675364831843,-61.6763643545582,
80.0979293949852));
#148492=CARTESIAN_POINT('Ctrl Pts',(-15.5675364831843,-60.3554402463129,
76.7331391278798));
#148493=CARTESIAN_POINT('Ctrl Pts',(-15.5675364833367,-60.0000151056028,
74.8473853384574));
#148494=CARTESIAN_POINT('Ctrl Pts',(-15.5675364833367,-59.9999845441923,
71.2120906405687));
#148495=CARTESIAN_POINT('Ctrl Pts',(-15.5675364832353,-60.3254915562694,
69.3197329090816));
#148496=CARTESIAN_POINT('Ctrl Pts',(-15.5675364832353,-61.7205672754213,
65.7681234014825));
#148497=CARTESIAN_POINT('Ctrl Pts',(-15.5675364833309,-62.6886244946971,
64.2646432845299));
#148498=CARTESIAN_POINT('Ctrl Pts',(-15.5675364833309,-63.7750278396796,
63.0390150155136));
#148499=CARTESIAN_POINT('',(-15.5675722559773,-86.2249610151766,63.0390024421084));
#148500=CARTESIAN_POINT('Origin',(-15.5675364833309,-75.,72.98888938658));
#148501=CARTESIAN_POINT('',(-15.5675362859867,-87.7888428218549,65.1501692217888));
#148502=CARTESIAN_POINT('Ctrl Pts',(-15.5675364833309,-86.22496630623,63.039008410399));
#148503=CARTESIAN_POINT('Ctrl Pts',(-15.5675364833309,-86.8043901271152,
63.6926858768345));
#148504=CARTESIAN_POINT('Ctrl Pts',(-15.5675364833309,-87.3248767325505,
64.3932124764954));
#148505=CARTESIAN_POINT('Ctrl Pts',(-15.5675364833309,-87.7888432730159,
65.1501689452555));
#148506=CARTESIAN_POINT('',(-15.5675362859827,-87.7888428219253,80.8276095513668));
#148507=CARTESIAN_POINT('Ctrl Pts',(-15.5675364833309,-87.78884383193,65.150169857118));
#148508=CARTESIAN_POINT('Ctrl Pts',(-15.5675364833309,-88.1384521311545,
65.7205578137845));
#148509=CARTESIAN_POINT('Ctrl Pts',(-15.5675364833309,-88.4562376776849,
66.3283180635497));
#148510=CARTESIAN_POINT('Ctrl Pts',(-15.5675364833309,-88.7331232623695,
66.9594691299437));
#148511=CARTESIAN_POINT('Ctrl Pts',(-15.5675364833309,-89.0100091596637,
67.5906209089204));
#148512=CARTESIAN_POINT('Ctrl Pts',(-15.5675364833309,-89.2459950027582,
68.2451635573432));
#148513=CARTESIAN_POINT('Ctrl Pts',(-15.5675364833309,-89.434356875338,
68.9085289128966));
#148514=CARTESIAN_POINT('Ctrl Pts',(-15.5675364833309,-89.6227187479178,
69.5718942684499));
#148515=CARTESIAN_POINT('Ctrl Pts',(-15.5675364833309,-89.763456649983,
70.2440823311337));
#148516=CARTESIAN_POINT('Ctrl Pts',(-15.5675364833309,-89.8578157866714,
70.9238061165624));
#148517=CARTESIAN_POINT('Ctrl Pts',(-15.5675364833309,-89.9049953550156,
71.2636680092768));
#148518=CARTESIAN_POINT('Ctrl Pts',(-15.5675364833309,-89.9405802320157,
71.6054138326774));
#148519=CARTESIAN_POINT('Ctrl Pts',(-15.5675364833309,-89.9643226891465,
71.9496920446505));
#148520=CARTESIAN_POINT('Ctrl Pts',(-15.5675364833309,-89.9880651462773,
72.2939702566235));
#148521=CARTESIAN_POINT('Ctrl Pts',(-15.5675364833309,-89.9999651835389,
72.6407808571691));
#148522=CARTESIAN_POINT('Ctrl Pts',(-15.5675364833309,-89.9999999415976,
72.9875657846074));
#148523=CARTESIAN_POINT('Ctrl Pts',(-15.5675364833309,-90.0000346996564,
73.3343507120457));
#148524=CARTESIAN_POINT('Ctrl Pts',(-15.5675364833309,-89.9882041785122,
73.6811099663768));
#148525=CARTESIAN_POINT('Ctrl Pts',(-15.5675364833309,-89.964544078123,
74.025310009284));
#148526=CARTESIAN_POINT('Ctrl Pts',(-15.5675364833309,-89.9408839777337,
74.3695100521911));
#148527=CARTESIAN_POINT('Ctrl Pts',(-15.5675364833309,-89.9053942980993,
74.7111508836743));
#148528=CARTESIAN_POINT('Ctrl Pts',(-15.5675364833309,-89.8582821639484,
75.0509875740311));
#148529=CARTESIAN_POINT('Ctrl Pts',(-15.5675364833309,-89.7640578956464,
75.7306609547447));
#148530=CARTESIAN_POINT('Ctrl Pts',(-15.5675364833309,-89.623343809278,
76.4031177709525));
#148531=CARTESIAN_POINT('Ctrl Pts',(-15.5675364833309,-89.4350795265403,
77.066692601835));
#148532=CARTESIAN_POINT('Ctrl Pts',(-15.5675364833309,-89.2468152438025,
77.7302674327175));
#148533=CARTESIAN_POINT('Ctrl Pts',(-15.5675364833309,-89.0110007646955,
78.3849602782747));
#148534=CARTESIAN_POINT('Ctrl Pts',(-15.5675364833309,-88.7341288890014,
79.016341571848));
#148535=CARTESIAN_POINT('Ctrl Pts',(-15.5675364833309,-88.4572573251297,
79.6477221543386));
#148536=CARTESIAN_POINT('Ctrl Pts',(-15.5675364833309,-88.1393284571513,
80.2557912373537));
#148537=CARTESIAN_POINT('Ctrl Pts',(-15.5675364833309,-87.78884383202,80.827608916005));
#148538=CARTESIAN_POINT('Ctrl Pts',(-15.5675364833309,-87.7888432730861,
80.8276098278998));
#148539=CARTESIAN_POINT('Ctrl Pts',(-15.5675364833309,-87.3288337727753,
81.578110400252));
#148540=CARTESIAN_POINT('Ctrl Pts',(-15.5675364833309,-86.8094297339697,
82.2794066895671));
#148541=CARTESIAN_POINT('Ctrl Pts',(-15.5675364833309,-86.22497216032,82.938763757646));
#148542=CARTESIAN_POINT('Ctrl Pts',(-11.5022227331779,-92.24059357535,82.170676098169));
#148543=CARTESIAN_POINT('Ctrl Pts',(-11.6900590068975,-90.08199127819,81.018814103239));
#148544=CARTESIAN_POINT('Ctrl Pts',(-13.340335337564,-88.3574125816099,
80.449317902351));
#148545=CARTESIAN_POINT('Ctrl Pts',(-15.7224335390679,-87.8306099166801,
80.7144498191781));
#148546=CARTESIAN_POINT('Ctrl Pts',(-11.2606355037699,-91.60559269606,83.19560543535));
#148547=CARTESIAN_POINT('Ctrl Pts',(-11.5151253257779,-89.4713091151301,
81.8775645334381));
#148548=CARTESIAN_POINT('Ctrl Pts',(-13.2736598773321,-87.7877285948101,
81.2333685902111));
#148549=CARTESIAN_POINT('Ctrl Pts',(-15.7260522384459,-87.33074482682,81.559964759865));
#148550=CARTESIAN_POINT('Ctrl Pts',(-10.9937695135339,-90.85061125929,84.14672603444));
#148551=CARTESIAN_POINT('Ctrl Pts',(-11.3301258891669,-88.76446201931,82.6491481018461));
#148552=CARTESIAN_POINT('Ctrl Pts',(-13.2094624536123,-87.14018413018,81.934204163023));
#148553=CARTESIAN_POINT('Ctrl Pts',(-15.7293652895189,-86.75795515826,82.345374479499));
#148554=CARTESIAN_POINT('Ctrl Pts',(-10.7185240592019,-89.96317024714,85.01999559162));
#148555=CARTESIAN_POINT('Ctrl Pts',(-11.1489392586529,-87.96379513296,83.3387148150201));
#148556=CARTESIAN_POINT('Ctrl Pts',(-13.1546927793304,-86.41956569116,82.5627311416799));
#148557=CARTESIAN_POINT('Ctrl Pts',(-15.7319333912539,-86.10357629771,83.0806217453801));
#148558=CARTESIAN_POINT('',(-11.4804365249865,-91.9999348338944,82.2509739592588));
#148559=CARTESIAN_POINT('Origin',(-16.3445396267105,-91.9999999945449,83.4087740069438));
#148560=CARTESIAN_POINT('',(-10.7897592617989,-89.96662731952,84.7813312827));
#148561=CARTESIAN_POINT('Ctrl Pts',(-10.7897592617989,-89.96662731952,84.7813312827));
#148562=CARTESIAN_POINT('Ctrl Pts',(-11.0308907230739,-90.74601077157,83.99976427574));
#148563=CARTESIAN_POINT('Ctrl Pts',(-11.2651526237029,-91.42091161506,83.15544542039));
#148564=CARTESIAN_POINT('Ctrl Pts',(-11.4804394903149,-91.99991170272,82.250961503044));
#148565=CARTESIAN_POINT('Origin',(-15.5675364833161,-89.9666295470565,86.2553885480345));
#148566=CARTESIAN_POINT('Ctrl Pts',(-14.1113299480839,-82.00270966797,86.25689542676));
#148567=CARTESIAN_POINT('Ctrl Pts',(-11.8626405705278,-82.36550259023,85.9811177666601));
#148568=CARTESIAN_POINT('Ctrl Pts',(-10.0162267657079,-83.30617916224,86.96615946002));
#148569=CARTESIAN_POINT('Ctrl Pts',(-9.30362299642891,-84.4520975419701,
88.8218429037501));
#148570=CARTESIAN_POINT('Ctrl Pts',(-14.6084235581879,-83.63151313314,85.3977275067));
#148571=CARTESIAN_POINT('Ctrl Pts',(-12.276179191861,-84.05626187835,85.01902796749));
#148572=CARTESIAN_POINT('Ctrl Pts',(-10.3874061607449,-85.22811992478,85.94969573067));
#148573=CARTESIAN_POINT('Ctrl Pts',(-9.74725467143191,-86.64761078011,87.79310189116));
#148574=CARTESIAN_POINT('Ctrl Pts',(-15.2202405060039,-85.09580522496,84.23630032922));
#148575=CARTESIAN_POINT('Ctrl Pts',(-12.769810936277,-85.4989458425199,
83.74870650635));
#148576=CARTESIAN_POINT('Ctrl Pts',(-10.8264676087449,-86.88819562728,84.6034677629701));
#148577=CARTESIAN_POINT('Ctrl Pts',(-10.2937231765359,-88.61774941448,86.4032922329));
#148578=CARTESIAN_POINT('Ctrl Pts',(-15.7858253484419,-86.2968668049501,
82.861956262163));
#148579=CARTESIAN_POINT('Ctrl Pts',(-13.2006025443896,-86.61561365093,82.351027486014));
#148580=CARTESIAN_POINT('Ctrl Pts',(-11.2038824748679,-88.19070270453,83.1115754237));
#148581=CARTESIAN_POINT('Ctrl Pts',(-10.7993506281129,-90.23051883621,84.76141092968));
#148582=CARTESIAN_POINT('',(-13.9923004473311,-82.1549149953847,86.172484981779));
#148583=CARTESIAN_POINT('Ctrl Pts',(-15.5675364833309,-86.2249721603224,
82.9387637576481));
#148584=CARTESIAN_POINT('Ctrl Pts',(-15.4656120592592,-86.0053159811617,
83.186569348349));
#148585=CARTESIAN_POINT('Ctrl Pts',(-15.3632750078612,-85.7773435514771,
83.4269937600978));
#148586=CARTESIAN_POINT('Ctrl Pts',(-15.2605270092227,-85.5416684370871,
83.6596025386694));
#148587=CARTESIAN_POINT('Ctrl Pts',(-15.2286260724226,-85.4684966281066,
83.7318223195185));
#148588=CARTESIAN_POINT('Ctrl Pts',(-15.1966858016408,-85.3945820821006,
83.8032886910187));
#148589=CARTESIAN_POINT('Ctrl Pts',(-15.164707060717,-85.3199424351608,
83.8739887164398));
#148590=CARTESIAN_POINT('Ctrl Pts',(-15.0972183933928,-85.1624212146251,
84.0231956694847));
#148591=CARTESIAN_POINT('Ctrl Pts',(-15.0295559702083,-85.0016705180204,
84.1689897085444));
#148592=CARTESIAN_POINT('Ctrl Pts',(-14.9617196972663,-84.8378521215638,
84.3112487193089));
#148593=CARTESIAN_POINT('Ctrl Pts',(-14.9278015607953,-84.7559429233355,
84.3823782246912));
#148594=CARTESIAN_POINT('Ctrl Pts',(-14.8938399616955,-84.6732667166982,
84.4526239646191));
#148595=CARTESIAN_POINT('Ctrl Pts',(-14.8598348933904,-84.5898433513543,
84.5219705847097));
#148596=CARTESIAN_POINT('Ctrl Pts',(-14.8428323592378,-84.5481316686824,
84.556643894755));
#148597=CARTESIAN_POINT('Ctrl Pts',(-14.8258189578757,-84.5062331934517,
84.591092423657));
#148598=CARTESIAN_POINT('Ctrl Pts',(-14.8087946891932,-84.4641503913645,
84.62531424654));
#148599=CARTESIAN_POINT('Ctrl Pts',(-14.800282554852,-84.4431089903209,
84.6424251579815));
#148600=CARTESIAN_POINT('Ctrl Pts',(-14.7917677036892,-84.4220215074326,
84.6594793928585));
#148601=CARTESIAN_POINT('Ctrl Pts',(-14.7832501357467,-84.4008882502899,
84.6764767101802));
#148602=CARTESIAN_POINT('Ctrl Pts',(-14.7789913517754,-84.3903216217185,
84.6849753688411));
#148603=CARTESIAN_POINT('Ctrl Pts',(-14.7747318886098,-84.3797435495776,
84.6934597981097));
#148604=CARTESIAN_POINT('Ctrl Pts',(-14.7704717462589,-84.369154072285,
84.7019299678404));
#148605=CARTESIAN_POINT('Ctrl Pts',(-14.766211603908,-84.3585645949924,
84.7104001375712));
#148606=CARTESIAN_POINT('Ctrl Pts',(-14.7614487457711,-84.3467135103602,
84.7198505336849));
#148607=CARTESIAN_POINT('Ctrl Pts',(-14.7576892816615,-84.3373514633523,
84.7272976682604));
#148608=CARTESIAN_POINT('Ctrl Pts',(-14.7244766462451,-84.2546433312974,
84.7930886848384));
#148609=CARTESIAN_POINT('Ctrl Pts',(-14.6899790214534,-84.1668123881177,
84.8615417050829));
#148610=CARTESIAN_POINT('Ctrl Pts',(-14.6541527336378,-84.0736496771072,
84.9323421676274));
#148611=CARTESIAN_POINT('Ctrl Pts',(-14.6190512769554,-83.9823718176266,
85.0017102077069));
#148612=CARTESIAN_POINT('Ctrl Pts',(-14.5826740707097,-83.8859755482417,
85.0733317188635));
#148613=CARTESIAN_POINT('Ctrl Pts',(-14.5450085622793,-83.7842556594628,
85.1468719738496));
#148614=CARTESIAN_POINT('Ctrl Pts',(-14.5085310419877,-83.6857440645948,
85.2180927340436));
#148615=CARTESIAN_POINT('Ctrl Pts',(-14.4708449976359,-83.5822391858921,
85.2911130827089));
#148616=CARTESIAN_POINT('Ctrl Pts',(-14.4319696764409,-83.4735492502824,
85.3655920748298));
#148617=CARTESIAN_POINT('Ctrl Pts',(-14.403554012694,-83.3941030471894,
85.4200320107907));
#148618=CARTESIAN_POINT('Ctrl Pts',(-14.3745035450076,-83.3118864615012,
85.4752505271231));
#148619=CARTESIAN_POINT('Ctrl Pts',(-14.3448377050704,-83.226823529824,
85.5311014069342));
#148620=CARTESIAN_POINT('Ctrl Pts',(-14.3254712279096,-83.1712926792887,
85.5675620225972));
#148621=CARTESIAN_POINT('Ctrl Pts',(-14.305834205992,-83.1145490552796,
85.6042917190634));
#148622=CARTESIAN_POINT('Ctrl Pts',(-14.2859266399296,-83.0565718014343,
85.6412469333113));
#148623=CARTESIAN_POINT('Ctrl Pts',(-14.2834381941718,-83.0493246447036,
85.6458663350923));
#148624=CARTESIAN_POINT('Ctrl Pts',(-14.2809455211633,-83.0420582113039,
85.6504892585988));
#148625=CARTESIAN_POINT('Ctrl Pts',(-14.2784486209066,-83.0347724632451,
85.6551156146363));
#148626=CARTESIAN_POINT('Ctrl Pts',(-14.2759517206499,-83.0274867151863,
85.6597419706738));
#148627=CARTESIAN_POINT('Ctrl Pts',(-14.2743733488263,-83.0228757247468,
85.6626637660008));
#148628=CARTESIAN_POINT('Ctrl Pts',(-14.2724657592636,-83.0172989205455,
85.6661941687955));
#148629=CARTESIAN_POINT('Ctrl Pts',(-14.2686505801383,-83.0061453121428,
85.6732549743849));
#148630=CARTESIAN_POINT('Ctrl Pts',(-14.2648485991046,-82.995009046459,
85.6802841527487));
#148631=CARTESIAN_POINT('Ctrl Pts',(-14.2610598161618,-82.9838902900655,
85.6872818862916));
#148632=CARTESIAN_POINT('Ctrl Pts',(-14.2534822502762,-82.9616527772784,
85.7012773533773));
#148633=CARTESIAN_POINT('Ctrl Pts',(-14.2459574767545,-82.9394853020566,
85.7151470420563));
#148634=CARTESIAN_POINT('Ctrl Pts',(-14.2384854955891,-82.9173892245883,
85.728892379904));
#148635=CARTESIAN_POINT('Ctrl Pts',(-14.2085975709273,-82.8290049147154,
85.7838737312947));
#148636=CARTESIAN_POINT('Ctrl Pts',(-14.1795543240126,-82.7417631278529,
85.8368657570438));
#148637=CARTESIAN_POINT('Ctrl Pts',(-14.1513557539548,-82.6557450291385,
85.8879604016492));
#148638=CARTESIAN_POINT('Ctrl Pts',(-14.1056922840827,-82.5164512688153,
85.9707007235795));
#148639=CARTESIAN_POINT('Ctrl Pts',(-14.0622424879955,-82.3803683376981,
86.0484660866791));
#148640=CARTESIAN_POINT('Ctrl Pts',(-14.021009930264,-82.247807422868,86.1216401981717));
#148641=CARTESIAN_POINT('Ctrl Pts',(-14.0113177916852,-82.216647610638,
86.138840528881));
#148642=CARTESIAN_POINT('Ctrl Pts',(-14.001748027803,-82.1856822216306,
86.1557871400861));
#148643=CARTESIAN_POINT('Ctrl Pts',(-13.9923004473314,-82.154914973001,
86.1724849405352));
#148644=CARTESIAN_POINT('',(-9.38953228746991,-84.5398910625,88.61388938658));
#148645=CARTESIAN_POINT('Ctrl Pts',(-9.38953228746955,-84.5398910625,88.6138893865798));
#148646=CARTESIAN_POINT('Ctrl Pts',(-9.46732490041307,-84.9199146414493,
88.4305627134663));
#148647=CARTESIAN_POINT('Ctrl Pts',(-9.5481939019438,-85.2933517189332,
88.2361911028148));
#148648=CARTESIAN_POINT('Ctrl Pts',(-9.63163192688313,-85.6602022949516,
88.0305923802988));
#148649=CARTESIAN_POINT('Ctrl Pts',(-9.71506995182247,-86.0270528709701,
87.8249936577829));
#148650=CARTESIAN_POINT('Ctrl Pts',(-9.80107708871513,-86.3873169455232,
87.6081675118582));
#148651=CARTESIAN_POINT('Ctrl Pts',(-9.88908546297492,-86.7409945186108,
87.3799276312666));
#148652=CARTESIAN_POINT('Ctrl Pts',(-9.93149206319931,-86.9114131131639,
87.2699508540234));
#148653=CARTESIAN_POINT('Ctrl Pts',(-9.97460623810215,-87.0812177182641,
87.1566792372891));
#148654=CARTESIAN_POINT('Ctrl Pts',(-10.017829253044,-87.2484237990849,
87.0414895539076));
#148655=CARTESIAN_POINT('Ctrl Pts',(-10.0344080496992,-87.312558048331,
86.9973069271257));
#148656=CARTESIAN_POINT('Ctrl Pts',(-10.0510033555079,-87.3763099990063,
86.9528423147313));
#148657=CARTESIAN_POINT('Ctrl Pts',(-10.0675832966058,-87.4395676628322,
86.9081741743193));
#148658=CARTESIAN_POINT('Ctrl Pts',(-10.1642601017378,-87.8084199285117,
86.6477164874846));
#148659=CARTESIAN_POINT('Ctrl Pts',(-10.2617137234065,-88.1657810428126,
86.3768586594466));
#148660=CARTESIAN_POINT('Ctrl Pts',(-10.359310849766,-88.5116510057349,
86.0954446257135));
#148661=CARTESIAN_POINT('Ctrl Pts',(-10.4558982141828,-88.8539425197962,
85.8169421652203));
#148662=CARTESIAN_POINT('Ctrl Pts',(-10.5526260811727,-89.1849794325178,
85.5281004989366));
#148663=CARTESIAN_POINT('Ctrl Pts',(-10.6488314986673,-89.5047617438996,
85.2287819496263));
#148664=CARTESIAN_POINT('Ctrl Pts',(-10.6959609636712,-89.6614178828744,
85.0821506739443));
#148665=CARTESIAN_POINT('Ctrl Pts',(-10.7429643021365,-89.8153730747478,
84.9330053285659));
#148666=CARTESIAN_POINT('Ctrl Pts',(-10.7897592617965,-89.96662731952,84.7813312826992));
#148667=CARTESIAN_POINT('Origin',(-13.9922814971304,-84.5398910366688,90.5670141989917));
#148668=CARTESIAN_POINT('Ctrl Pts',(-9.36316543113591,-84.79485741396,88.68507306022));
#148669=CARTESIAN_POINT('Ctrl Pts',(-9.52089785507191,-84.52189181462,88.25909049769));
#148670=CARTESIAN_POINT('Ctrl Pts',(-9.99271929691491,-83.97055140082,87.46229833598));
#148671=CARTESIAN_POINT('Ctrl Pts',(-11.1638051091349,-83.19637684992,86.55460492855));
#148672=CARTESIAN_POINT('Ctrl Pts',(-12.6378577027309,-82.58312137528,86.06242162813));
#148673=CARTESIAN_POINT('Ctrl Pts',(-13.6855439527239,-82.3368973288,86.05405719771));
#148674=CARTESIAN_POINT('Ctrl Pts',(-14.2037341389199,-82.25481693243,86.12140353019));
#148675=CARTESIAN_POINT('Ctrl Pts',(-9.24767657508891,-84.00598446336,88.94968435057));
#148676=CARTESIAN_POINT('Ctrl Pts',(-9.42115179510291,-83.75855212272,88.5312692084));
#148677=CARTESIAN_POINT('Ctrl Pts',(-9.91247134952491,-83.26101823161,87.75513773229));
#148678=CARTESIAN_POINT('Ctrl Pts',(-11.0704798546419,-82.56016909489,86.87706862434));
#148679=CARTESIAN_POINT('Ctrl Pts',(-12.5011304605773,-81.99370416917,86.3973053855));
#148680=CARTESIAN_POINT('Ctrl Pts',(-13.5150380396684,-81.75325243071,86.38291437305));
#148681=CARTESIAN_POINT('Ctrl Pts',(-14.0186219503769,-81.66825256106,86.44526609955));
#148682=CARTESIAN_POINT('Ctrl Pts',(-9.02110732129691,-82.43288905337,89.39524706291));
#148683=CARTESIAN_POINT('Ctrl Pts',(-9.21938651903491,-82.23328319354,88.99421222644));
#148684=CARTESIAN_POINT('Ctrl Pts',(-9.73855112510891,-81.83512480463,88.25989487262));
#148685=CARTESIAN_POINT('Ctrl Pts',(-10.8679585310409,-81.27152859285,87.43449506429));
#148686=CARTESIAN_POINT('Ctrl Pts',(-12.2214087371624,-80.80111226951,86.97204043525));
#148687=CARTESIAN_POINT('Ctrl Pts',(-13.1759013667958,-80.58377622138,86.94116396896));
#148688=CARTESIAN_POINT('Ctrl Pts',(-13.6534062038429,-80.50032404056,86.99087839766));
#148689=CARTESIAN_POINT('Ctrl Pts',(-8.63390385764391,-79.20559950703,90.01976900704));
#148690=CARTESIAN_POINT('Ctrl Pts',(-8.86287624956091,-79.09733565716,89.65283473253));
#148691=CARTESIAN_POINT('Ctrl Pts',(-9.41039510203091,-78.88383521299,88.99091950632));
#148692=CARTESIAN_POINT('Ctrl Pts',(-10.4863410151329,-78.5781942732,88.24450783708));
#148693=CARTESIAN_POINT('Ctrl Pts',(-11.722657985102,-78.30941010548,87.79963352364));
#148694=CARTESIAN_POINT('Ctrl Pts',(-12.5878203220956,-78.16912067339,87.73316725532));
#148695=CARTESIAN_POINT('Ctrl Pts',(-13.0250798682998,-78.10921981045,87.75627315149));
#148696=CARTESIAN_POINT('Ctrl Pts',(-8.43646722755891,-75.82295460461,90.27567271427));
#148697=CARTESIAN_POINT('Ctrl Pts',(-8.67457228700691,-75.80159547571,89.9271492125));
#148698=CARTESIAN_POINT('Ctrl Pts',(-9.22633231332491,-75.75956225844,89.30069277592));
#148699=CARTESIAN_POINT('Ctrl Pts',(-10.2725773694299,-75.69964845786,88.5884829841));
#148700=CARTESIAN_POINT('Ctrl Pts',(-11.4566903832199,-75.64722956981,88.14814037352));
#148701=CARTESIAN_POINT('Ctrl Pts',(-12.2830364939519,-75.62002220028,88.06199406937));
#148702=CARTESIAN_POINT('Ctrl Pts',(-12.7024212510196,-75.6084141972,88.07026937053));
#148703=CARTESIAN_POINT('Ctrl Pts',(-8.53644251351991,-72.45433594609,90.14553315307));
#148704=CARTESIAN_POINT('Ctrl Pts',(-8.76988752817891,-72.52017514507,89.78750600586));
#148705=CARTESIAN_POINT('Ctrl Pts',(-9.31940153097291,-72.64985744622,89.14272588511));
#148706=CARTESIAN_POINT('Ctrl Pts',(-10.3807195496249,-72.83504863245,88.41288548734));
#148707=CARTESIAN_POINT('Ctrl Pts',(-11.5914114362033,-72.99743164875,87.9703890705));
#148708=CARTESIAN_POINT('Ctrl Pts',(-12.4374024314272,-73.08191917965,87.89458815261));
#148709=CARTESIAN_POINT('Ctrl Pts',(-12.8657678794551,-73.11797934746,87.91059102918));
#148710=CARTESIAN_POINT('Ctrl Pts',(-8.80312062497391,-69.07786522395,89.75884753243));
#148711=CARTESIAN_POINT('Ctrl Pts',(-9.01991246902591,-69.23307671621,89.3769250268));
#148712=CARTESIAN_POINT('Ctrl Pts',(-9.55697366388591,-69.54076372218,88.68389914341));
#148713=CARTESIAN_POINT('Ctrl Pts',(-10.6566609744269,-69.97917371075,87.90432815956));
#148714=CARTESIAN_POINT('Ctrl Pts',(-11.9426748847926,-70.35617472473,87.45249436166));
#148715=CARTESIAN_POINT('Ctrl Pts',(-12.8456722144427,-70.54333343852,87.40161797299));
#148716=CARTESIAN_POINT('Ctrl Pts',(-13.3001072668109,-70.62003610521,87.4364636821));
#148717=CARTESIAN_POINT('Ctrl Pts',(-9.14077283870491,-66.72557398356,89.19463338426));
#148718=CARTESIAN_POINT('Ctrl Pts',(-9.32880949855591,-66.94937144786,88.78323786731));
#148719=CARTESIAN_POINT('Ctrl Pts',(-9.83816023021391,-67.39707941798,88.02624050682));
#148720=CARTESIAN_POINT('Ctrl Pts',(-10.9840980003949,-68.02992693744,87.17553264098));
#148721=CARTESIAN_POINT('Ctrl Pts',(-12.3746508960219,-68.55282376321,86.70717184876));
#148722=CARTESIAN_POINT('Ctrl Pts',(-13.3573195647358,-68.78769939384,86.6871470724));
#148723=CARTESIAN_POINT('Ctrl Pts',(-13.8473824995249,-68.87528428493,86.74485486738));
#148724=CARTESIAN_POINT('Ctrl Pts',(-9.36320138448591,-65.20481666306,88.68499094841));
#148725=CARTESIAN_POINT('Ctrl Pts',(-9.52093025095291,-65.47779132966,88.25900375063));
#148726=CARTESIAN_POINT('Ctrl Pts',(-9.99274691583291,-66.02915171764,87.46220423853));
#148727=CARTESIAN_POINT('Ctrl Pts',(-11.1638314564919,-66.80336097775,86.55450907384));
#148728=CARTESIAN_POINT('Ctrl Pts',(-12.63788868308,-67.41665312944,86.0623326859));
#148729=CARTESIAN_POINT('Ctrl Pts',(-13.6855831157219,-67.66289929178,86.05397688329));
#148730=CARTESIAN_POINT('Ctrl Pts',(-14.2037786680419,-67.74498930276,86.1213279171));
#148731=CARTESIAN_POINT('Ctrl Pts',(-9.38953228746991,-65.4601089375,88.61388938658));
#148732=CARTESIAN_POINT('Ctrl Pts',(-9.28328709691747,-66.2097609713885,
88.8642676240639));
#148733=CARTESIAN_POINT('Ctrl Pts',(-9.17708486958767,-66.9655883719527,
89.0795251225669));
#148734=CARTESIAN_POINT('Ctrl Pts',(-9.0302280749938,-68.1085925228124,
89.3540432573925));
#148735=CARTESIAN_POINT('Ctrl Pts',(-8.98330754389956,-68.4911377481012,
89.4374960493532));
#148736=CARTESIAN_POINT('Ctrl Pts',(-8.91715535501208,-69.0672713485378,
89.5511487398476));
#148737=CARTESIAN_POINT('Ctrl Pts',(-8.88513273745213,-69.3559170893819,
89.6050931419384));
#148738=CARTESIAN_POINT('Ctrl Pts',(-8.84983719738048,-69.6936835997954,
89.6630999929911));
#148739=CARTESIAN_POINT('Ctrl Pts',(-8.83273032605669,-69.8628201415259,
89.6908850775549));
#148740=CARTESIAN_POINT('Ctrl Pts',(-8.82551731869127,-69.9353615065227,
89.7025333452868));
#148741=CARTESIAN_POINT('Ctrl Pts',(-8.82073526432502,-69.9837344777835,
89.7102413212732));
#148742=CARTESIAN_POINT('Ctrl Pts',(-8.81853574016785,-70.0061031598871,
89.7137803985326));
#148743=CARTESIAN_POINT('Ctrl Pts',(-8.73463441113894,-70.8648417345999,
89.8485086409056));
#148744=CARTESIAN_POINT('Ctrl Pts',(-8.67003768437608,-71.6936986475477,
89.944358023184));
#148745=CARTESIAN_POINT('Ctrl Pts',(-8.60463652245025,-72.9311950958996,
90.0398919577533));
#148746=CARTESIAN_POINT('Ctrl Pts',(-8.58803785671435,-73.3427290918387,
90.0636744407946));
#148747=CARTESIAN_POINT('Ctrl Pts',(-8.57132975194435,-73.9585828554797,
90.0875200458021));
#148748=CARTESIAN_POINT('Ctrl Pts',(-8.56712264234536,-74.1636262383155,
90.0934954812812));
#148749=CARTESIAN_POINT('Ctrl Pts',(-8.56146522762817,-74.5732305938979,
90.1015227750632));
#148750=CARTESIAN_POINT('Ctrl Pts',(-8.56001530984221,-74.7765851842616,
90.1035740849179));
#148751=CARTESIAN_POINT('Ctrl Pts',(-8.55968148378128,-75.8042159346871,
90.1040468034545));
#148752=CARTESIAN_POINT('Ctrl Pts',(-8.58177592616641,-76.6283044763792,
90.0732381391729));
#148753=CARTESIAN_POINT('Ctrl Pts',(-8.64644160601739,-77.867413200945,
89.9788480269719));
#148754=CARTESIAN_POINT('Ctrl Pts',(-8.67320843583484,-78.2809454278049,
89.9393254017685));
#148755=CARTESIAN_POINT('Ctrl Pts',(-8.72052840036098,-78.9019877461016,
89.8675311439229));
#148756=CARTESIAN_POINT('Ctrl Pts',(-8.74597657546545,-79.2126948997517,
89.8285040402398));
#148757=CARTESIAN_POINT('Ctrl Pts',(-8.77860779189364,-79.5755120693882,
89.7773794891791));
#148758=CARTESIAN_POINT('Ctrl Pts',(-8.79563181834841,-79.7570020268009,
89.7504030045294));
#148759=CARTESIAN_POINT('Ctrl Pts',(-8.80307665120823,-79.8348008741052,
89.7385368699022));
#148760=CARTESIAN_POINT('Ctrl Pts',(-8.80807260339695,-79.8866706471935,
89.7305581866392));
#148761=CARTESIAN_POINT('Ctrl Pts',(-8.81073338330589,-79.9141085081485,
89.7263000880263));
#148762=CARTESIAN_POINT('Ctrl Pts',(-8.9656995991205,-81.5025605981437,
89.4778327793481));
#148763=CARTESIAN_POINT('Ctrl Pts',(-9.17644065973502,-83.0363422081069,
89.1160627640075));
#148764=CARTESIAN_POINT('Ctrl Pts',(-9.38953228746991,-84.5398910625,88.61388938658));
#148765=CARTESIAN_POINT('',(-13.9922632538745,-67.8450784104076,86.1724813495899));
#148766=CARTESIAN_POINT('Origin',(-13.9922817629778,-65.4601089375625,90.5670143866247));
#148767=CARTESIAN_POINT('Ctrl Pts',(-13.9922632538729,-67.8450784104129,
86.1724813495793));
#148768=CARTESIAN_POINT('Ctrl Pts',(-13.9285551321338,-68.0520701946722,
86.2848187148604));
#148769=CARTESIAN_POINT('Ctrl Pts',(-13.8647015765799,-68.2609196751036,
86.3918585032884));
#148770=CARTESIAN_POINT('Ctrl Pts',(-13.8013730345684,-68.4716504870294,
86.4937275061761));
#148771=CARTESIAN_POINT('Ctrl Pts',(-13.7378365702574,-68.6830731771134,
86.5959309686403));
#148772=CARTESIAN_POINT('Ctrl Pts',(-13.6748285726308,-68.8963899825192,
86.6929298523555));
#148773=CARTESIAN_POINT('Ctrl Pts',(-13.6130261144539,-69.1116541348552,
86.7848084560886));
#148774=CARTESIAN_POINT('Ctrl Pts',(-13.5511371715245,-69.3272195222469,
86.87681563235));
#148775=CARTESIAN_POINT('Ctrl Pts',(-13.4904571444066,-69.5447381338853,
86.9636883767891));
#148776=CARTESIAN_POINT('Ctrl Pts',(-13.431665952279,-69.7642865478471,
87.0454645258856));
#148777=CARTESIAN_POINT('Ctrl Pts',(-13.3830763120145,-69.9457385318768,
87.1130507326457));
#148778=CARTESIAN_POINT('Ctrl Pts',(-13.3357768712037,-70.1285775377871,
87.1771548238835));
#148779=CARTESIAN_POINT('Ctrl Pts',(-13.2901514710066,-70.3128555667207,
87.2377727484992));
#148780=CARTESIAN_POINT('Ctrl Pts',(-13.2637884073469,-70.4193342690851,
87.2727987252283));
#148781=CARTESIAN_POINT('Ctrl Pts',(-13.2379850419819,-70.5262944514629,
87.3066606384413));
#148782=CARTESIAN_POINT('Ctrl Pts',(-13.2128161545854,-70.6337472099288,
87.3393540680178));
#148783=CARTESIAN_POINT('Ctrl Pts',(-13.2096700436608,-70.647178804737,
87.3434407467149));
#148784=CARTESIAN_POINT('Ctrl Pts',(-13.2065338464545,-70.6606180964965,
87.347509164306));
#148785=CARTESIAN_POINT('Ctrl Pts',(-13.2034077096942,-70.6740651067791,
87.351559308973));
#148786=CARTESIAN_POINT('Ctrl Pts',(-13.2005271864215,-70.6864556159081,
87.3552912429432));
#148787=CARTESIAN_POINT('Ctrl Pts',(-13.1986999834587,-70.6943412175539,
87.3576538279662));
#148788=CARTESIAN_POINT('Ctrl Pts',(-13.1966065552207,-70.7033861337611,
87.3603579713991));
#148789=CARTESIAN_POINT('Ctrl Pts',(-13.1964280549407,-70.7041573663479,
87.3605885455125));
#148790=CARTESIAN_POINT('Ctrl Pts',(-13.1962476190816,-70.7049370361643,
87.3608215746784));
#148791=CARTESIAN_POINT('Ctrl Pts',(-13.1960644296178,-70.7057286591898,
87.3610581043308));
#148792=CARTESIAN_POINT('Ctrl Pts',(-13.1914012059293,-70.7258800105199,
87.3670791420875));
#148793=CARTESIAN_POINT('Ctrl Pts',(-13.1867535757959,-70.7460473567043,
87.3730587939704));
#148794=CARTESIAN_POINT('Ctrl Pts',(-13.1821220573804,-70.7662307481179,
87.3789970276582));
#148795=CARTESIAN_POINT('Ctrl Pts',(-13.1728590205494,-70.8065975309452,
87.3908734950339));
#148796=CARTESIAN_POINT('Ctrl Pts',(-13.1636604305903,-70.847028493799,
87.4025842960819));
#148797=CARTESIAN_POINT('Ctrl Pts',(-13.1545307665253,-70.8875252185154,
87.4141294598562));
#148798=CARTESIAN_POINT('Ctrl Pts',(-13.1180121102655,-71.0495121173814,
87.4603101149533));
#148799=CARTESIAN_POINT('Ctrl Pts',(-13.0825962683134,-71.2125513108651,
87.5038416280283));
#148800=CARTESIAN_POINT('Ctrl Pts',(-13.0485477116034,-71.3766762962778,
87.5446966585263));
#148801=CARTESIAN_POINT('Ctrl Pts',(-13.0031366647857,-71.5955721355358,
87.5991855967357));
#148802=CARTESIAN_POINT('Ctrl Pts',(-12.9601460521461,-71.8163441963887,
87.648893413177));
#148803=CARTESIAN_POINT('Ctrl Pts',(-12.9200620589948,-72.0385592644602,
87.6936460581433));
#148804=CARTESIAN_POINT('Ctrl Pts',(-12.9000372367978,-72.1495715882784,
87.7160032059183));
#148805=CARTESIAN_POINT('Ctrl Pts',(-12.8807378246369,-72.2609437584287,
87.7371244433808));
#148806=CARTESIAN_POINT('Ctrl Pts',(-12.8622244395765,-72.3726202435535,
87.7569927047253));
#148807=CARTESIAN_POINT('Ctrl Pts',(-12.8344384838983,-72.5402307510792,
87.7868121368456));
#148808=CARTESIAN_POINT('Ctrl Pts',(-12.8084219928603,-72.7085275052885,
87.8138085585889));
#148809=CARTESIAN_POINT('Ctrl Pts',(-12.7843726877417,-72.8773244673507,
87.8379381299538));
#148810=CARTESIAN_POINT('Ctrl Pts',(-12.7813665246019,-72.8984240876085,
87.8409543263744));
#148811=CARTESIAN_POINT('Ctrl Pts',(-12.7783910987421,-72.9195315229508,
87.8439257486868));
#148812=CARTESIAN_POINT('Ctrl Pts',(-12.7754467790334,-72.9406464143135,
87.8468523293632));
#148813=CARTESIAN_POINT('Ctrl Pts',(-12.7750787390698,-72.9432857757339,
87.8472181519478));
#148814=CARTESIAN_POINT('Ctrl Pts',(-12.7747111851399,-72.9459252721915,
87.8475831396505));
#148815=CARTESIAN_POINT('Ctrl Pts',(-12.7744712210636,-72.9476510013597,
87.8478215012301));
#148816=CARTESIAN_POINT('Ctrl Pts',(-12.7742312569873,-72.9493767305279,
87.8480598628097));
#148817=CARTESIAN_POINT('Ctrl Pts',(-12.7741183959124,-72.9501886470366,
87.8481717891691));
#148818=CARTESIAN_POINT('Ctrl Pts',(-12.7740743827478,-72.9505060053221,
87.8482155612684));
#148819=CARTESIAN_POINT('Ctrl Pts',(-12.7739863564187,-72.951140721893,
87.8483031054669));
#148820=CARTESIAN_POINT('Ctrl Pts',(-12.7738970129558,-72.9517866318275,
87.8483921520975));
#148821=CARTESIAN_POINT('Ctrl Pts',(-12.7738063561645,-72.9524437358476,
87.8484826967998));
#148822=CARTESIAN_POINT('Ctrl Pts',(-12.7736250425818,-72.9537579438877,
87.8486637862044));
#148823=CARTESIAN_POINT('Ctrl Pts',(-12.7734384756853,-72.9551169282491,
87.8488508680473));
#148824=CARTESIAN_POINT('Ctrl Pts',(-12.7732466858366,-72.9565206948447,
87.8490439056084));
#148825=CARTESIAN_POINT('Ctrl Pts',(-12.7724795264419,-72.962135761227,
87.8498160558532));
#148826=CARTESIAN_POINT('Ctrl Pts',(-12.7716287998118,-72.9684673368165,
87.8506835461686));
#148827=CARTESIAN_POINT('Ctrl Pts',(-12.7706965559355,-72.9755158673858,
87.8516436399744));
#148828=CARTESIAN_POINT('Ctrl Pts',(-12.7688320681828,-72.9896129285244,
87.853563827586));
#148829=CARTESIAN_POINT('Ctrl Pts',(-12.7666415114454,-73.0065777253166,
87.8558550511194));
#148830=CARTESIAN_POINT('Ctrl Pts',(-12.7641489210632,-73.0264146540014,
87.8584879313309));
#148831=CARTESIAN_POINT('Ctrl Pts',(-12.7603881731616,-73.0563440352818,
87.8624603444484));
#148832=CARTESIAN_POINT('Ctrl Pts',(-12.7559136899501,-73.0928109209032,
87.8672128776889));
#148833=CARTESIAN_POINT('Ctrl Pts',(-12.7508847748352,-73.1358347705,87.872601557847));
#148834=CARTESIAN_POINT('Ctrl Pts',(-12.7458602570049,-73.1788210000318,
87.8779855261419));
#148835=CARTESIAN_POINT('Ctrl Pts',(-12.740282276438,-73.2283528810644,
87.8840045407208));
#148836=CARTESIAN_POINT('Ctrl Pts',(-12.7343097190214,-73.2844532911088,
87.8904631118485));
#148837=CARTESIAN_POINT('Ctrl Pts',(-12.730411970744,-73.3210649569928,
87.8946780373371));
#148838=CARTESIAN_POINT('Ctrl Pts',(-12.726346172469,-73.3604742247497,
87.8990791121011));
#148839=CARTESIAN_POINT('Ctrl Pts',(-12.7221564858865,-73.4026877304981,
87.9036000278797));
#148840=CARTESIAN_POINT('Ctrl Pts',(-12.7157559134418,-73.4671771848689,
87.9105066182385));
#148841=CARTESIAN_POINT('Ctrl Pts',(-12.7090596196822,-73.5382113626362,
87.9176953668346));
#148842=CARTESIAN_POINT('Ctrl Pts',(-12.7023689986799,-73.6158148009317,
87.9248872218329));
#148843=CARTESIAN_POINT('Ctrl Pts',(-12.6957025587298,-73.6931377670874,
87.9320530842334));
#148844=CARTESIAN_POINT('Ctrl Pts',(-12.6890417506065,-73.7769828554256,
87.9392220142129));
#148845=CARTESIAN_POINT('Ctrl Pts',(-12.6826847123091,-73.8673696091889,
87.9460665399673));
#148846=CARTESIAN_POINT('Ctrl Pts',(-12.6784412431516,-73.9277048445438,
87.9506354182054));
#148847=CARTESIAN_POINT('Ctrl Pts',(-12.6743331298586,-73.9909548630671,
87.9550586877087));
#148848=CARTESIAN_POINT('Ctrl Pts',(-12.6704490504521,-74.057123363438,
87.9592261779894));
#148849=CARTESIAN_POINT('Ctrl Pts',(-12.6646823504542,-74.1553638603548,
87.9654136586451));
#148850=CARTESIAN_POINT('Ctrl Pts',(-12.6594351109689,-74.2600388012238,
87.9710396197401));
#148851=CARTESIAN_POINT('Ctrl Pts',(-12.6551289584109,-74.3711533682616,
87.9757019867879));
#148852=CARTESIAN_POINT('Ctrl Pts',(-12.6536321151853,-74.4097774264428,
87.9773226522049));
#148853=CARTESIAN_POINT('Ctrl Pts',(-12.6522489832399,-74.4491794557137,
87.9788264449859));
#148854=CARTESIAN_POINT('Ctrl Pts',(-12.6509972713499,-74.4893592249046,
87.9801950668338));
#148855=CARTESIAN_POINT('Ctrl Pts',(-12.6485709388204,-74.5672441453867,
87.9828480189523));
#148856=CARTESIAN_POINT('Ctrl Pts',(-12.6466421084436,-74.6480517625337,
87.9849937078946));
#148857=CARTESIAN_POINT('Ctrl Pts',(-12.6453635744747,-74.7317783140308,
87.9864910990931));
#148858=CARTESIAN_POINT('Ctrl Pts',(-12.6447243074902,-74.7736415897794,
87.9872397946923));
#148859=CARTESIAN_POINT('Ctrl Pts',(-12.6442478758437,-74.8162345453753,
87.9878262556343));
#148860=CARTESIAN_POINT('Ctrl Pts',(-12.6439550111987,-74.8595563603345,
87.9882318916392));
#148861=CARTESIAN_POINT('Ctrl Pts',(-12.6438085788762,-74.8812172678141,
87.9884347096417));
#148862=CARTESIAN_POINT('Ctrl Pts',(-12.643708038304,-74.9030603906,87.9885923114367));
#148863=CARTESIAN_POINT('Ctrl Pts',(-12.6436561075558,-74.9250855971942,
87.9887023131552));
#148864=CARTESIAN_POINT('Ctrl Pts',(-12.6436301421817,-74.9360982004913,
87.9887573140144));
#148865=CARTESIAN_POINT('Ctrl Pts',(-12.6436163292635,-74.9471563247771,
87.9888004142327));
#148866=CARTESIAN_POINT('Ctrl Pts',(-12.6436150126614,-74.9582599527134,
87.9888313120827));
#148867=CARTESIAN_POINT('Ctrl Pts',(-12.6436136960593,-74.9693635806496,
87.9888622099326));
#148868=CARTESIAN_POINT('Ctrl Pts',(-12.6436289425738,-74.9824075328569,
87.9888819529563));
#148869=CARTESIAN_POINT('Ctrl Pts',(-12.643648897583,-74.9917073296298,
87.9888870943004));
#148870=CARTESIAN_POINT('Ctrl Pts',(-12.6441957679959,-75.2465698379219,
87.9890279937067));
#148871=CARTESIAN_POINT('Ctrl Pts',(-12.6513772313359,-75.5018909548218,
87.9826693312941));
#148872=CARTESIAN_POINT('Ctrl Pts',(-12.6647090535987,-75.757165505727,
87.9697672112249));
#148873=CARTESIAN_POINT('Ctrl Pts',(-12.6780337951938,-76.0123044776953,
87.9568719436042));
#148874=CARTESIAN_POINT('Ctrl Pts',(-12.6975023644089,-76.2673965773429,
87.9374401515452));
#148875=CARTESIAN_POINT('Ctrl Pts',(-12.7226312983753,-76.5219356309839,
87.9114800442085));
#148876=CARTESIAN_POINT('Ctrl Pts',(-12.7310755095397,-76.6074697615364,
87.9027565293752));
#148877=CARTESIAN_POINT('Ctrl Pts',(-12.7401588878712,-76.6929414509161,
87.8932962737769));
#148878=CARTESIAN_POINT('Ctrl Pts',(-12.74986308835,-76.7783315551092,87.8831009091851));
#148879=CARTESIAN_POINT('Ctrl Pts',(-12.7782149982648,-77.027808320039,
87.8533140082358));
#148880=CARTESIAN_POINT('Ctrl Pts',(-12.8118641877124,-77.2765816129467,
87.8172492980099));
#148881=CARTESIAN_POINT('Ctrl Pts',(-12.8503429439184,-77.5241603024399,
87.7749847050739));
#148882=CARTESIAN_POINT('Ctrl Pts',(-12.8576532392744,-77.5711959533419,
87.7669551664939));
#148883=CARTESIAN_POINT('Ctrl Pts',(-12.8651378501164,-77.6181885118085,
87.7587020021747));
#148884=CARTESIAN_POINT('Ctrl Pts',(-12.872793569282,-77.6651346488302,
87.7502259555904));
#148885=CARTESIAN_POINT('Ctrl Pts',(-12.8967699000968,-77.8121614777091,
87.7236805073432));
#148886=CARTESIAN_POINT('Ctrl Pts',(-12.9224245115847,-77.9587328844472,
87.6949484881787));
#148887=CARTESIAN_POINT('Ctrl Pts',(-12.9496575490047,-78.1047475853005,
87.6640569301405));
#148888=CARTESIAN_POINT('Ctrl Pts',(-12.9632740677147,-78.1777549357272,
87.6486111511213));
#148889=CARTESIAN_POINT('Ctrl Pts',(-12.9772851929078,-78.2506231495068,
87.6326255837542));
#148890=CARTESIAN_POINT('Ctrl Pts',(-12.9916784029335,-78.3233398291162,
87.6161041720479));
#148891=CARTESIAN_POINT('Ctrl Pts',(-12.9988750079464,-78.3596981689209,
87.6078434661947));
#148892=CARTESIAN_POINT('Ctrl Pts',(-13.0061671341675,-78.3960186283675,
87.5994488049755));
#148893=CARTESIAN_POINT('Ctrl Pts',(-13.0135532117496,-78.4322996754754,
87.5909207157386));
#148894=CARTESIAN_POINT('Ctrl Pts',(-13.0204776594828,-78.4663131571391,
87.5829256320791));
#148895=CARTESIAN_POINT('Ctrl Pts',(-13.0274846816545,-78.5002919991374,
87.5748132779195));
#148896=CARTESIAN_POINT('Ctrl Pts',(-13.0345729827054,-78.53423494977,87.5665841055616));
#148897=CARTESIAN_POINT('Ctrl Pts',(-13.0350455361088,-78.5364978131455,
87.5660354940711));
#148898=CARTESIAN_POINT('Ctrl Pts',(-13.0358533538705,-78.5403615571573,
87.5650974156943));
#148899=CARTESIAN_POINT('Ctrl Pts',(-13.0359917262273,-78.5410230609782,
87.5649367136718));
#148900=CARTESIAN_POINT('Ctrl Pts',(-13.0404196416454,-78.5621911832477,
87.5597942489534));
#148901=CARTESIAN_POINT('Ctrl Pts',(-13.0461916289288,-78.5902495695812,
87.5529342151086));
#148902=CARTESIAN_POINT('Ctrl Pts',(-13.0534262917923,-78.6251519329629,
87.5442414421963));
#148903=CARTESIAN_POINT('Ctrl Pts',(-13.0604266942057,-78.6589241478486,
87.535830143754));
#148904=CARTESIAN_POINT('Ctrl Pts',(-13.0687965820832,-78.6991043297429,
87.5257025283007));
#148905=CARTESIAN_POINT('Ctrl Pts',(-13.0786434069086,-78.7456357479416,
87.5137030805226));
#148906=CARTESIAN_POINT('Ctrl Pts',(-13.0889845008086,-78.7945028470755,
87.5011013110768));
#148907=CARTESIAN_POINT('Ctrl Pts',(-13.1009545249819,-78.8503751368275,
87.4864354576878));
#148908=CARTESIAN_POINT('Ctrl Pts',(-13.1146779375454,-78.9131671994993,
87.4694668083806));
#148909=CARTESIAN_POINT('Ctrl Pts',(-13.1284013501089,-78.9759592621712,
87.4524981590734));
#148910=CARTESIAN_POINT('Ctrl Pts',(-13.1438781510625,-79.0456713500959,
87.4332265985393));
#148911=CARTESIAN_POINT('Ctrl Pts',(-13.161232798523,-79.1221945220809,
87.4113549289942));
#148912=CARTESIAN_POINT('Ctrl Pts',(-13.1783109482994,-79.1974985117185,
87.3898317232246));
#148913=CARTESIAN_POINT('Ctrl Pts',(-13.1972368930209,-79.2793960174767,
87.3657911402542));
#148914=CARTESIAN_POINT('Ctrl Pts',(-13.218151617703,-79.3677741621452,
87.338891089315));
#148915=CARTESIAN_POINT('Ctrl Pts',(-13.2390663423851,-79.4561523068137,
87.3119910383758));
#148916=CARTESIAN_POINT('Ctrl Pts',(-13.2619698470278,-79.5510114316163,
87.2822313862799));
#148917=CARTESIAN_POINT('Ctrl Pts',(-13.2870031166466,-79.6522076225808,
87.2492177220848));
#148918=CARTESIAN_POINT('Ctrl Pts',(-13.3106570500547,-79.7478278910742,
87.2180231148154));
#148919=CARTESIAN_POINT('Ctrl Pts',(-13.3362102523045,-79.8491089599361,
87.1839219451345));
#148920=CARTESIAN_POINT('Ctrl Pts',(-13.3637483455945,-79.9559219629347,
87.1465317573033));
#148921=CARTESIAN_POINT('Ctrl Pts',(-13.3653541795417,-79.9621505694112,
87.1443514163379));
#148922=CARTESIAN_POINT('Ctrl Pts',(-13.3669667629672,-79.9683979776324,
87.1421598797651));
#148923=CARTESIAN_POINT('Ctrl Pts',(-13.3685861128491,-79.974664158566,
87.1399570674823));
#148924=CARTESIAN_POINT('Ctrl Pts',(-13.3832807253308,-80.0315259285838,
87.1199678895857));
#148925=CARTESIAN_POINT('Ctrl Pts',(-13.3985319081437,-80.0899341144083,
87.0990503614809));
#148926=CARTESIAN_POINT('Ctrl Pts',(-13.4143477726808,-80.1498678263095,
87.0771419883593));
#148927=CARTESIAN_POINT('Ctrl Pts',(-13.4222557049493,-80.1798346822601,
87.0661878017985));
#148928=CARTESIAN_POINT('Ctrl Pts',(-13.4303048076488,-80.2101828977198,
87.0549858456473));
#148929=CARTESIAN_POINT('Ctrl Pts',(-13.438495672417,-80.2409097575134,
87.0435279416479));
#148930=CARTESIAN_POINT('Ctrl Pts',(-13.4425911048011,-80.2562731874102,
87.0377989896482));
#148931=CARTESIAN_POINT('Ctrl Pts',(-13.4467219777023,-80.2717312769617,
87.0320060469452));
#148932=CARTESIAN_POINT('Ctrl Pts',(-13.4508883493137,-80.2872836790015,
87.0261480683085));
#148933=CARTESIAN_POINT('Ctrl Pts',(-13.4529715351194,-80.2950598800215,
87.0232190789902));
#148934=CARTESIAN_POINT('Ctrl Pts',(-13.4550635956026,-80.3028596590685,
87.0202738304531));
#148935=CARTESIAN_POINT('Ctrl Pts',(-13.4571645363622,-80.310682972302,
87.0173121905769));
#148936=CARTESIAN_POINT('Ctrl Pts',(-13.4592654771218,-80.3185062855355,
87.0143505507008));
#148937=CARTESIAN_POINT('Ctrl Pts',(-13.4618074963136,-80.327958614595,
87.0107616557018));
#148938=CARTESIAN_POINT('Ctrl Pts',(-13.4634940045304,-80.3342234703738,
87.0083779638468));
#148939=CARTESIAN_POINT('Ctrl Pts',(-13.5025360795712,-80.4792526893253,
86.9531963315527));
#148940=CARTESIAN_POINT('Ctrl Pts',(-13.5406679976172,-80.6176638563657,
86.8979602069061));
#148941=CARTESIAN_POINT('Ctrl Pts',(-13.5776553922539,-80.7495778925329,
86.8432155722051));
#148942=CARTESIAN_POINT('Ctrl Pts',(-13.6150631201262,-80.8829910300608,
86.7878488069199));
#148943=CARTESIAN_POINT('Ctrl Pts',(-13.6513001635259,-81.0097589628704,
86.7329848246882));
#148944=CARTESIAN_POINT('Ctrl Pts',(-13.6861240747114,-81.1300193085492,
86.6791363995748));
#148945=CARTESIAN_POINT('Ctrl Pts',(-13.7120606592147,-81.2195883004261,
86.639030501622));
#148946=CARTESIAN_POINT('Ctrl Pts',(-13.7372133570588,-81.3055477211668,
86.5994868643739));
#148947=CARTESIAN_POINT('Ctrl Pts',(-13.7614820014301,-81.387956741055,
86.5606987233784));
#148948=CARTESIAN_POINT('Ctrl Pts',(-13.7942709972533,-81.4992983128203,
86.5082926567835));
#148949=CARTESIAN_POINT('Ctrl Pts',(-13.8254696763634,-81.6041576702389,
86.4572683615342));
#148950=CARTESIAN_POINT('Ctrl Pts',(-13.8550187233761,-81.7026898173829,
86.4080528929969));
#148951=CARTESIAN_POINT('Ctrl Pts',(-13.8847124905224,-81.8017045379744,
86.3585963855803));
#148952=CARTESIAN_POINT('Ctrl Pts',(-13.9127404274452,-81.8943302867114,
86.3109664100033));
#148953=CARTESIAN_POINT('Ctrl Pts',(-13.9390423429716,-81.9807195923339,
86.265543858743));
#148954=CARTESIAN_POINT('Ctrl Pts',(-13.957667695685,-82.0418950335774,
86.2333784813768));
#148955=CARTESIAN_POINT('Ctrl Pts',(-13.9754275217782,-82.0999430662178,
86.2023189351202));
#148956=CARTESIAN_POINT('Ctrl Pts',(-13.9923004473309,-82.154914972983,
86.1724849405017));
#148957=CARTESIAN_POINT('Origin',(-15.5675364833309,-75.,72.98888938658));
#148958=CARTESIAN_POINT('Ctrl Pts',(-13.9922632538729,-67.8450784104129,
86.1724813495793));
#148959=CARTESIAN_POINT('Ctrl Pts',(-14.0172702688094,-67.7636406775926,
86.1282839415892));
#148960=CARTESIAN_POINT('Ctrl Pts',(-14.0444973895826,-67.6769323819869,
86.0802539845106));
#148961=CARTESIAN_POINT('Ctrl Pts',(-14.0739446161924,-67.5851571089398,
86.0280651619461));
#148962=CARTESIAN_POINT('Ctrl Pts',(-14.1032441861568,-67.4938420228274,
85.9761380287613));
#148963=CARTESIAN_POINT('Ctrl Pts',(-14.1347416533126,-67.3975103985407,
85.9200933988725));
#148964=CARTESIAN_POINT('Ctrl Pts',(-14.1684370176596,-67.296401626475,
85.8595759300175));
#148965=CARTESIAN_POINT('Ctrl Pts',(-14.2017938107947,-67.196308795924,
85.7996665410326));
#148966=CARTESIAN_POINT('Ctrl Pts',(-14.2373045540593,-67.0915341169454,
85.7353734611614));
#148967=CARTESIAN_POINT('Ctrl Pts',(-14.2749692474532,-66.9823514351676,
85.6663225451827));
#148968=CARTESIAN_POINT('Ctrl Pts',(-14.3123575914211,-66.8739698370767,
85.5977782623207));
#148969=CARTESIAN_POINT('Ctrl Pts',(-14.3518683939993,-66.7612444428563,
85.5245454041851));
#148970=CARTESIAN_POINT('Ctrl Pts',(-14.3935016551879,-66.6444877606173,
85.4462332133163));
#148971=CARTESIAN_POINT('Ctrl Pts',(-14.4346033139423,-66.5292219088997,
85.3689209669655));
#148972=CARTESIAN_POINT('Ctrl Pts',(-14.4777735752965,-66.4100268721727,
85.2866579311862));
#148973=CARTESIAN_POINT('Ctrl Pts',(-14.5230124392504,-66.2872501238768,
85.1990486646613));
#148974=CARTESIAN_POINT('Ctrl Pts',(-14.544098664004,-66.2300228223309,
85.1582132297502));
#148975=CARTESIAN_POINT('Ctrl Pts',(-14.5656343076739,-66.1720180533392,
85.1162160408558));
#148976=CARTESIAN_POINT('Ctrl Pts',(-14.5876193702598,-66.1132747231402,
85.0730159108109));
#148977=CARTESIAN_POINT('Ctrl Pts',(-14.6338698573215,-65.9896950142947,
84.9821347933299));
#148978=CARTESIAN_POINT('Ctrl Pts',(-14.6821093158676,-65.8628433973624,
84.8859304129358));
#148979=CARTESIAN_POINT('Ctrl Pts',(-14.7323378288026,-65.7331185860723,
84.7840116352132));
#148980=CARTESIAN_POINT('Ctrl Pts',(-14.7818996441456,-65.6051156497544,
84.6834456549301));
#148981=CARTESIAN_POINT('Ctrl Pts',(-14.8333980617202,-65.4743151543327,
84.577315594984));
#148982=CARTESIAN_POINT('Ctrl Pts',(-14.8868331611732,-65.3411504316446,
84.465240070307));
#148983=CARTESIAN_POINT('Ctrl Pts',(-14.9391086331413,-65.2108755973263,
84.3555967645297));
#148984=CARTESIAN_POINT('Ctrl Pts',(-14.9932376408722,-65.0783380079684,
84.2402628757793));
#148985=CARTESIAN_POINT('Ctrl Pts',(-15.049220258939,-64.9439929085543,
84.1188813621743));
#148986=CARTESIAN_POINT('Ctrl Pts',(-15.1044918229534,-64.811354171412,
83.9990415559796));
#148987=CARTESIAN_POINT('Ctrl Pts',(-15.1615702096795,-64.676953472949,
83.8733064025776));
#148988=CARTESIAN_POINT('Ctrl Pts',(-15.2204554908848,-64.5412786150475,
83.7413378050537));
#148989=CARTESIAN_POINT('Ctrl Pts',(-15.2781110133641,-64.4084371874531,
83.6121252363886));
#148990=CARTESIAN_POINT('Ctrl Pts',(-15.3374987481049,-64.2743742884252,
83.4769365119666));
#148991=CARTESIAN_POINT('Ctrl Pts',(-15.3986187624717,-64.1395959885378,
83.335464892892));
#148992=CARTESIAN_POINT('Ctrl Pts',(-15.4535266119418,-64.0185163932739,
83.208372279369));
#148993=CARTESIAN_POINT('Ctrl Pts',(-15.5098325026146,-63.8968599934556,
83.0762089638245));
#148994=CARTESIAN_POINT('Ctrl Pts',(-15.5675364833309,-63.7750278396912,
82.9387637576609));
#148995=CARTESIAN_POINT('Ctrl Pts',(-15.7859374982489,-63.70265213093,82.861383624057));
#148996=CARTESIAN_POINT('Ctrl Pts',(-13.2002732600734,-63.38383560984,82.350395801635));
#148997=CARTESIAN_POINT('Ctrl Pts',(-11.2034697254109,-61.8083020344701,
83.11121227182));
#148998=CARTESIAN_POINT('Ctrl Pts',(-10.7994091717229,-59.76814774659,84.76133204249));
#148999=CARTESIAN_POINT('Ctrl Pts',(-15.2200740724999,-64.90402508323,84.23663134082));
#149000=CARTESIAN_POINT('Ctrl Pts',(-12.7693205181935,-64.50074857368,83.74901632495));
#149001=CARTESIAN_POINT('Ctrl Pts',(-10.8258933224599,-63.11114403357,84.60411552944));
#149002=CARTESIAN_POINT('Ctrl Pts',(-10.2935001377589,-61.38139141585,86.40429721953));
#149003=CARTESIAN_POINT('Ctrl Pts',(-14.6041660747459,-66.38156201951,85.4050021444));
#149004=CARTESIAN_POINT('Ctrl Pts',(-12.2722897776818,-65.95698671183,85.02702776225));
#149005=CARTESIAN_POINT('Ctrl Pts',(-10.3838362619619,-64.78669608641,85.95842638835));
#149006=CARTESIAN_POINT('Ctrl Pts',(-9.74335915314591,-63.36928148601,87.80238251478));
#149007=CARTESIAN_POINT('Ctrl Pts',(-14.1110631602059,-67.99782845316,86.2571636203899));
#149008=CARTESIAN_POINT('Ctrl Pts',(-11.8620763883513,-67.6350035382001,
85.98143506887));
#149009=CARTESIAN_POINT('Ctrl Pts',(-10.0155685768079,-66.69421658395,86.96682116639));
#149010=CARTESIAN_POINT('Ctrl Pts',(-9.30321403080591,-65.54825406424,88.82286146046));
#149011=CARTESIAN_POINT('Origin',(-15.5675402745283,-60.0333674837764,86.255392349124));
#149012=CARTESIAN_POINT('Ctrl Pts',(-10.7041478512819,-60.09386358317,85.0646713926));
#149013=CARTESIAN_POINT('Ctrl Pts',(-10.7993782800689,-60.52820765432,84.69634244083));
#149014=CARTESIAN_POINT('Ctrl Pts',(-11.1849148787739,-61.42183746252,83.9980255694));
#149015=CARTESIAN_POINT('Ctrl Pts',(-12.3843078552043,-62.66523363698,83.23440107119));
#149016=CARTESIAN_POINT('Ctrl Pts',(-14.0046199477159,-63.57750343473,82.906426537614));
#149017=CARTESIAN_POINT('Ctrl Pts',(-15.1626528546819,-63.86437128804,83.00677838687));
#149018=CARTESIAN_POINT('Ctrl Pts',(-15.7241364691869,-63.93250661788,83.12048790153));
#149019=CARTESIAN_POINT('Ctrl Pts',(-10.9677003684169,-59.23917692107,84.23345016192));
#149020=CARTESIAN_POINT('Ctrl Pts',(-11.0441856921629,-59.69432284707,83.89966200941));
#149021=CARTESIAN_POINT('Ctrl Pts',(-11.3853725838139,-60.62794654061,83.26859435449));
#149022=CARTESIAN_POINT('Ctrl Pts',(-12.4999814042177,-61.9296416061,82.572868554654));
#149023=CARTESIAN_POINT('Ctrl Pts',(-14.0404250630399,-62.89957197101,82.257638700836));
#149024=CARTESIAN_POINT('Ctrl Pts',(-15.1678421958949,-63.22153762943,82.32904067551));
#149025=CARTESIAN_POINT('Ctrl Pts',(-15.7218484252699,-63.30516960113,82.422318246836));
#149026=CARTESIAN_POINT('Ctrl Pts',(-11.3522936220239,-58.1404827969,82.865207710886));
#149027=CARTESIAN_POINT('Ctrl Pts',(-11.4036986376399,-58.61682481435,82.583952417586));
#149028=CARTESIAN_POINT('Ctrl Pts',(-11.6848368356737,-59.58954811194,82.054712944551));
#149029=CARTESIAN_POINT('Ctrl Pts',(-12.6807018187587,-60.95041422044,81.466427752057));
#149030=CARTESIAN_POINT('Ctrl Pts',(-14.1030936751929,-61.98838456191,81.183450354301));
#149031=CARTESIAN_POINT('Ctrl Pts',(-15.1787465752679,-62.36041090116,81.223135164807));
#149032=CARTESIAN_POINT('Ctrl Pts',(-15.7172649246479,-62.46838269082,81.291197010499));
#149033=CARTESIAN_POINT('Ctrl Pts',(-11.7927722579691,-57.0209055347,80.87660427494));
#149034=CARTESIAN_POINT('Ctrl Pts',(-11.8176818813139,-57.51258307741,80.664597756629));
#149035=CARTESIAN_POINT('Ctrl Pts',(-12.0347761979652,-58.51132096518,80.267386771243));
#149036=CARTESIAN_POINT('Ctrl Pts',(-12.900196635276,-59.91385972122,79.821483937711));
#149037=CARTESIAN_POINT('Ctrl Pts',(-14.1863686741569,-61.01129527968,79.593672952375));
#149038=CARTESIAN_POINT('Ctrl Pts',(-15.1950629340279,-61.43683394942,79.60664069943));
#149039=CARTESIAN_POINT('Ctrl Pts',(-15.7105937362879,-61.57320926475,79.649025591868));
#149040=CARTESIAN_POINT('Ctrl Pts',(-12.0661314106457,-56.37283617373,79.38235543526));
#149041=CARTESIAN_POINT('Ctrl Pts',(-12.0758434847391,-56.87031895131,79.218299414597));
#149042=CARTESIAN_POINT('Ctrl Pts',(-12.255568884686,-57.87753552957,78.911808500822));
#149043=CARTESIAN_POINT('Ctrl Pts',(-13.0422585423339,-59.29546209928,78.565409307254));
#149044=CARTESIAN_POINT('Ctrl Pts',(-14.2430805630429,-60.42240614723,78.381490093937));
#149045=CARTESIAN_POINT('Ctrl Pts',(-15.2068409041219,-60.87953638866,78.382502187017));
#149046=CARTESIAN_POINT('Ctrl Pts',(-15.7058387404459,-61.0336884742,78.410472854166));
#149047=CARTESIAN_POINT('Ctrl Pts',(-12.2840775879539,-55.88110902617,77.838409205923));
#149048=CARTESIAN_POINT('Ctrl Pts',(-12.2827124321547,-56.38084424398,77.718226582429));
#149049=CARTESIAN_POINT('Ctrl Pts',(-12.4345336551895,-57.3898254788,77.49440046578));
#149050=CARTESIAN_POINT('Ctrl Pts',(-13.1600193818496,-58.81285577353,77.240660890849));
#149051=CARTESIAN_POINT('Ctrl Pts',(-14.2920472090029,-59.95780874928,77.102673904364));
#149052=CARTESIAN_POINT('Ctrl Pts',(-15.2174560511349,-60.43844112167,77.099030649501));
#149053=CARTESIAN_POINT('Ctrl Pts',(-15.7015914388329,-60.60654655031,77.117122227125));
#149054=CARTESIAN_POINT('Ctrl Pts',(-12.4455223641938,-55.53147356832,76.248194310692));
#149055=CARTESIAN_POINT('Ctrl Pts',(-12.4364409723141,-56.03153659583,76.169508058991));
#149056=CARTESIAN_POINT('Ctrl Pts',(-12.5684953465771,-57.03906368194,76.023333781968));
#149057=CARTESIAN_POINT('Ctrl Pts',(-13.2494610073287,-58.46199397328,75.857320665731));
#149058=CARTESIAN_POINT('Ctrl Pts',(-14.3302328652499,-59.61727660643,75.76553819577));
#149059=CARTESIAN_POINT('Ctrl Pts',(-15.2259605578989,-60.11434751671,75.761106780194));
#149060=CARTESIAN_POINT('Ctrl Pts',(-15.6982072375269,-60.29264234043,75.771817510397));
#149061=CARTESIAN_POINT('Ctrl Pts',(-12.5457498999123,-55.32390979009,74.632044951833));
#149062=CARTESIAN_POINT('Ctrl Pts',(-12.5323125837539,-55.82305995791,74.593269618371));
#149063=CARTESIAN_POINT('Ctrl Pts',(-12.6528329390154,-56.82750771549,74.521337406159));
#149064=CARTESIAN_POINT('Ctrl Pts',(-13.3066685414211,-58.24764282185,74.439492266471));
#149065=CARTESIAN_POINT('Ctrl Pts',(-14.3552787532369,-59.40754337176,74.393701806354));
#149066=CARTESIAN_POINT('Ctrl Pts',(-15.2316755631149,-59.91449324558,74.390782624317));
#149067=CARTESIAN_POINT('Ctrl Pts',(-15.6959440082919,-60.09919481949,74.39565266482));
#149068=CARTESIAN_POINT('Ctrl Pts',(-12.5810013147727,-55.25465453146,73.0095737856597));
#149069=CARTESIAN_POINT('Ctrl Pts',(-12.5662393202892,-55.75295766122,73.0090978203629));
#149070=CARTESIAN_POINT('Ctrl Pts',(-12.6830375165281,-56.75533192764,73.0082135404681));
#149071=CARTESIAN_POINT('Ctrl Pts',(-13.3275136480566,-58.17334349545,73.0071997776312));
#149072=CARTESIAN_POINT('Ctrl Pts',(-14.3646256854699,-59.33424330126,73.0066206299221));
#149073=CARTESIAN_POINT('Ctrl Pts',(-15.2338545192429,-59.84467210232,73.0065694532389));
#149074=CARTESIAN_POINT('Ctrl Pts',(-15.6950847124779,-60.03173379517,73.0066211743601));
#149075=CARTESIAN_POINT('Ctrl Pts',(-12.5475045162963,-55.32017430335,71.387087839408));
#149076=CARTESIAN_POINT('Ctrl Pts',(-12.533981149037,-55.8193273013,71.424862343681));
#149077=CARTESIAN_POINT('Ctrl Pts',(-12.654283968606,-56.82375706032,71.494940544456));
#149078=CARTESIAN_POINT('Ctrl Pts',(-13.3076377377326,-58.24388402961,71.574696849883));
#149079=CARTESIAN_POINT('Ctrl Pts',(-14.3556951419789,-59.4038845339,71.619353265881));
#149080=CARTESIAN_POINT('Ctrl Pts',(-15.2317691498139,-59.91100278183,71.622241360802));
#149081=CARTESIAN_POINT('Ctrl Pts',(-15.6959068347219,-60.0958104599,71.61752019893));
#149082=CARTESIAN_POINT('Ctrl Pts',(-12.4158905694987,-55.59282803409,69.229401204407));
#149083=CARTESIAN_POINT('Ctrl Pts',(-12.4081109279248,-56.09315502217,69.320374998153));
#149084=CARTESIAN_POINT('Ctrl Pts',(-12.5435994725067,-57.10157402003,69.489396119942));
#149085=CARTESIAN_POINT('Ctrl Pts',(-13.2325997356449,-58.52529383771,69.681292799115));
#149086=CARTESIAN_POINT('Ctrl Pts',(-14.3228650735119,-59.67918060652,69.787209745794));
#149087=CARTESIAN_POINT('Ctrl Pts',(-15.2242815937599,-60.17332252705,69.792102588723));
#149088=CARTESIAN_POINT('Ctrl Pts',(-15.6988723085229,-60.34972220064,69.779595279849));
#149089=CARTESIAN_POINT('Ctrl Pts',(-12.0984815213225,-56.28453201346,66.598496595256));
#149090=CARTESIAN_POINT('Ctrl Pts',(-12.1059032952083,-56.78383432926,66.759784999304));
#149091=CARTESIAN_POINT('Ctrl Pts',(-12.2803121570357,-57.79442431143,67.060817730495));
#149092=CARTESIAN_POINT('Ctrl Pts',(-13.0569396205602,-59.21756273984,67.402062653449));
#149093=CARTESIAN_POINT('Ctrl Pts',(-14.2480069695899,-60.35063110239,67.586009442708));
#149094=CARTESIAN_POINT('Ctrl Pts',(-15.2076486671699,-60.8123315191,67.588584775643));
#149095=CARTESIAN_POINT('Ctrl Pts',(-15.7054941595619,-60.96870853934,67.562980380674));
#149096=CARTESIAN_POINT('Ctrl Pts',(-11.4801382308969,-57.77429967396,63.567629022451));
#149097=CARTESIAN_POINT('Ctrl Pts',(-11.5230945717649,-58.25793556693,63.831385556471));
#149098=CARTESIAN_POINT('Ctrl Pts',(-11.784103413135,-59.24408794518,64.326760510344));
#149099=CARTESIAN_POINT('Ctrl Pts',(-12.7404495534908,-60.62500522954,64.879476066085));
#149100=CARTESIAN_POINT('Ctrl Pts',(-14.1237202044219,-61.68566477043,65.151993286447));
#149101=CARTESIAN_POINT('Ctrl Pts',(-15.1823110544269,-62.07418257557,65.123079900673));
#149102=CARTESIAN_POINT('Ctrl Pts',(-15.7157641330979,-62.19013200718,65.063526526587));
#149103=CARTESIAN_POINT('Ctrl Pts',(-10.9713079387679,-59.2277623056,61.75592042875));
#149104=CARTESIAN_POINT('Ctrl Pts',(-11.0475501095339,-59.68314485839,62.08924479198));
#149105=CARTESIAN_POINT('Ctrl Pts',(-11.3881525214239,-60.61722479436,62.71941099542));
#149106=CARTESIAN_POINT('Ctrl Pts',(-12.5016155027438,-61.91961304936,63.414226922204));
#149107=CARTESIAN_POINT('Ctrl Pts',(-14.0409546878489,-62.89027630592,63.729283079577));
#149108=CARTESIAN_POINT('Ctrl Pts',(-15.1679259362799,-63.21272241284,63.65826525009));
#149109=CARTESIAN_POINT('Ctrl Pts',(-15.7218123616389,-63.29657498626,63.565259667224));
#149110=CARTESIAN_POINT('Ctrl Pts',(-10.7040595554379,-60.0941142792,60.91280126868));
#149111=CARTESIAN_POINT('Ctrl Pts',(-10.7992944412109,-60.52845915509,61.28113961178));
#149112=CARTESIAN_POINT('Ctrl Pts',(-11.1848427857719,-61.42209035945,61.97947395869));
#149113=CARTESIAN_POINT('Ctrl Pts',(-12.3842618607264,-62.66548448627,62.7431137798));
#149114=CARTESIAN_POINT('Ctrl Pts',(-14.0046020364749,-63.57774528311,63.071087750167));
#149115=CARTESIAN_POINT('Ctrl Pts',(-15.1626491571459,-63.86460259476,62.97072528602));
#149116=CARTESIAN_POINT('Ctrl Pts',(-15.7241379640389,-63.9327320353,62.85700885034));
#149117=CARTESIAN_POINT('Origin',(-15.5675364833322,-60.0333704528863,59.7223902251838));
#149118=CARTESIAN_POINT('Ctrl Pts',(-14.1109587916119,-67.99806761864,59.72048255862));
#149119=CARTESIAN_POINT('Ctrl Pts',(-11.8622349709499,-67.6352743646101,
59.9961606353001));
#149120=CARTESIAN_POINT('Ctrl Pts',(-10.0158495894229,-66.69465820612,59.0109757487901));
#149121=CARTESIAN_POINT('Ctrl Pts',(-9.30331679897591,-65.5488541427201,
57.15519830438));
#149122=CARTESIAN_POINT('Ctrl Pts',(-14.6029404122129,-66.3855391917801,
60.57083234018));
#149123=CARTESIAN_POINT('Ctrl Pts',(-12.2714944067202,-65.96131004996,60.94839266561));
#149124=CARTESIAN_POINT('Ctrl Pts',(-10.3832434550279,-64.79176598389,60.0170714877401));
#149125=CARTESIAN_POINT('Ctrl Pts',(-9.74244088945891,-63.37501002094,58.17348929348));
#149126=CARTESIAN_POINT('Ctrl Pts',(-15.2156776004529,-64.91333674655,61.73072156537));
#149127=CARTESIAN_POINT('Ctrl Pts',(-12.7662414190393,-64.50943479782,62.21808717786));
#149128=CARTESIAN_POINT('Ctrl Pts',(-10.8233228751789,-63.12150890318,61.36245727412));
#149129=CARTESIAN_POINT('Ctrl Pts',(-10.2896898327509,-61.39440175993,59.56133749228));
#149130=CARTESIAN_POINT('Ctrl Pts',(-15.7859912232719,-63.70246439342,63.116600358883));
#149131=CARTESIAN_POINT('Ctrl Pts',(-13.2006081304612,-63.38367271774,63.627536549936));
#149132=CARTESIAN_POINT('Ctrl Pts',(-11.2038952684519,-61.8083637843599,
62.8669303902801));
#149133=CARTESIAN_POINT('Ctrl Pts',(-10.7995805712549,-59.76836009227,61.21707043588));
#149134=CARTESIAN_POINT('',(-13.9922553804024,-67.8450769206476,59.8052980196146));
#149135=CARTESIAN_POINT('Origin',(-13.9922814999513,-65.4601089597576,55.4107645745232));
#149136=CARTESIAN_POINT('Ctrl Pts',(-15.5675364833309,-63.775027839677,
63.0390150155114));
#149137=CARTESIAN_POINT('Ctrl Pts',(-15.5486560109279,-63.8156900744696,
62.9931418279215));
#149138=CARTESIAN_POINT('Ctrl Pts',(-15.5276796743979,-63.8610333030251,
62.9425581622453));
#149139=CARTESIAN_POINT('Ctrl Pts',(-15.504601517406,-63.9112558109,62.8874513628923));
#149140=CARTESIAN_POINT('Ctrl Pts',(-15.4815962090432,-63.9613197861483,
62.8325185139455));
#149141=CARTESIAN_POINT('Ctrl Pts',(-15.4565020002374,-64.016232557767,
62.7730908821243));
#149142=CARTESIAN_POINT('Ctrl Pts',(-15.429319211093,-64.0762215379075,
62.7093948971326));
#149143=CARTESIAN_POINT('Ctrl Pts',(-15.4195418942773,-64.097798840412,
62.686484230319));
#149144=CARTESIAN_POINT('Ctrl Pts',(-15.4094944497678,-64.1200331503125,
62.6630217404487));
#149145=CARTESIAN_POINT('Ctrl Pts',(-15.3991772236595,-64.1429359253291,
62.6390193286406));
#149146=CARTESIAN_POINT('Ctrl Pts',(-15.3671474528508,-64.2140374624055,
62.5645039752888));
#149147=CARTESIAN_POINT('Ctrl Pts',(-15.3324052214448,-64.2918409859351,
62.4845101324438));
#149148=CARTESIAN_POINT('Ctrl Pts',(-15.2950981599505,-64.3763510127759,
62.3998250092134));
#149149=CARTESIAN_POINT('Ctrl Pts',(-15.2583555496539,-64.4595824134272,
62.3164211613588));
#149150=CARTESIAN_POINT('Ctrl Pts',(-15.2191246511704,-64.5493200493604,
62.228467495124));
#149151=CARTESIAN_POINT('Ctrl Pts',(-15.177580101105,-64.6455612701451,
62.1367522446501));
#149152=CARTESIAN_POINT('Ctrl Pts',(-15.1720477058737,-64.6583774992313,
62.1245387289529));
#149153=CARTESIAN_POINT('Ctrl Pts',(-15.1664743364701,-64.6713090363615,
62.1122585525923));
#149154=CARTESIAN_POINT('Ctrl Pts',(-15.1608604577245,-64.6843558498199,
62.0999136179658));
#149155=CARTESIAN_POINT('Ctrl Pts',(-15.1243743065958,-64.7691507000761,
62.0196804724232));
#149156=CARTESIAN_POINT('Ctrl Pts',(-15.0897314949321,-64.8506403030421,
61.9444417012586));
#149157=CARTESIAN_POINT('Ctrl Pts',(-15.0569457220555,-64.9285380674421,
61.8739305478222));
#149158=CARTESIAN_POINT('Ctrl Pts',(-15.0233657115331,-65.0083229106442,
61.8017112567521));
#149159=CARTESIAN_POINT('Ctrl Pts',(-14.9917334822288,-65.0843399044684,
61.7344511114654));
#149160=CARTESIAN_POINT('Ctrl Pts',(-14.9620434453303,-65.1563274476019,
61.671884384849));
#149161=CARTESIAN_POINT('Ctrl Pts',(-14.9487610463081,-65.1885324352816,
61.6438939774516));
#149162=CARTESIAN_POINT('Ctrl Pts',(-14.9358671186469,-65.2199315701482,
61.616843208052));
#149163=CARTESIAN_POINT('Ctrl Pts',(-14.9233601493996,-65.2505042236718,
61.5907098279098));
#149164=CARTESIAN_POINT('Ctrl Pts',(-14.8947732166026,-65.3203835345124,
61.5309772766328));
#149165=CARTESIAN_POINT('Ctrl Pts',(-14.8682163869933,-65.3859411515636,
61.47603640133));
#149166=CARTESIAN_POINT('Ctrl Pts',(-14.8436906166197,-65.44695781362,61.4256453742038));
#149167=CARTESIAN_POINT('Ctrl Pts',(-14.8391498514624,-65.4582545977317,
61.4163158478838));
#149168=CARTESIAN_POINT('Ctrl Pts',(-14.8346786770759,-65.4693958425011,
61.4071423621721));
#149169=CARTESIAN_POINT('Ctrl Pts',(-14.8302770628544,-65.4803803100542,
61.3981234958639));
#149170=CARTESIAN_POINT('Ctrl Pts',(-14.8161891644792,-65.5155374262401,
61.3692575240608));
#149171=CARTESIAN_POINT('Ctrl Pts',(-14.8028142414204,-65.5490881151195,
61.3419752144693));
#149172=CARTESIAN_POINT('Ctrl Pts',(-14.7901522947983,-65.5809946859591,
61.3162327255843));
#149173=CARTESIAN_POINT('Ctrl Pts',(-14.7838213214872,-65.5969479713789,
61.3033614811419));
#149174=CARTESIAN_POINT('Ctrl Pts',(-14.7776685923084,-65.6124902860436,
61.2908752655851));
#149175=CARTESIAN_POINT('Ctrl Pts',(-14.7716941073786,-65.627617355836,
61.2787689719339));
#149176=CARTESIAN_POINT('Ctrl Pts',(-14.7687068649137,-65.6351808907321,
61.2727158251082));
#149177=CARTESIAN_POINT('Ctrl Pts',(-14.7657641835125,-65.6426406181008,
61.2667576633422));
#149178=CARTESIAN_POINT('Ctrl Pts',(-14.7628660631932,-65.6499960269563,
61.260893874795));
#149179=CARTESIAN_POINT('Ctrl Pts',(-14.7614170030336,-65.6536737313841,
61.2579619805214));
#149180=CARTESIAN_POINT('Ctrl Pts',(-14.7599790831445,-65.657325356411,
61.2550536798404));
#149181=CARTESIAN_POINT('Ctrl Pts',(-14.7585523035282,-65.6609508397835,
61.2521688977952));
#149182=CARTESIAN_POINT('Ctrl Pts',(-14.75783891372,-65.6627635814697,61.2507265067726));
#149183=CARTESIAN_POINT('Ctrl Pts',(-14.75712830898,-65.6645697877565,61.249289995427));
#149184=CARTESIAN_POINT('Ctrl Pts',(-14.7564204893085,-65.6663694509628,
61.2478593544845));
#149185=CARTESIAN_POINT('Ctrl Pts',(-14.7557126696371,-65.6681691141691,
61.246428713542));
#149186=CARTESIAN_POINT('Ctrl Pts',(-14.7555273948954,-65.6686399307073,
61.2460541282831));
#149187=CARTESIAN_POINT('Ctrl Pts',(-14.7543053854998,-65.6717488037198,
61.2435850336611));
#149188=CARTESIAN_POINT('Ctrl Pts',(-14.7009716673493,-65.8074333226892,
61.1358231808213));
#149189=CARTESIAN_POINT('Ctrl Pts',(-14.6492741378672,-65.9416405763828,
61.0330309177387));
#149190=CARTESIAN_POINT('Ctrl Pts',(-14.5992805060834,-66.0740270455773,
60.9349368939584));
#149191=CARTESIAN_POINT('Ctrl Pts',(-14.5480365872424,-66.2097243582351,
60.834389643958));
#149192=CARTESIAN_POINT('Ctrl Pts',(-14.4985826667428,-66.3435087517832,
60.7387783956766));
#149193=CARTESIAN_POINT('Ctrl Pts',(-14.4509563393972,-66.4750525354945,
60.6478083689958));
#149194=CARTESIAN_POINT('Ctrl Pts',(-14.4013843434623,-66.6119702504397,
60.5531219624608));
#149195=CARTESIAN_POINT('Ctrl Pts',(-14.3537921692459,-66.7464605320466,
60.4634635300441));
#149196=CARTESIAN_POINT('Ctrl Pts',(-14.3081869089074,-66.8781987461111,
60.3785008789946));
#149197=CARTESIAN_POINT('Ctrl Pts',(-14.2614817556639,-67.0131141797742,
60.2914891262324));
#149198=CARTESIAN_POINT('Ctrl Pts',(-14.2168602310794,-67.1451433252664,
60.2094021511291));
#149199=CARTESIAN_POINT('Ctrl Pts',(-14.1742971125142,-67.2739825744216,
60.1318868147313));
#149200=CARTESIAN_POINT('Ctrl Pts',(-14.1301511161401,-67.4076132203373,
60.0514887641441));
#149201=CARTESIAN_POINT('Ctrl Pts',(-14.0882192053369,-67.5378123569951,
59.9760084098408));
#149202=CARTESIAN_POINT('Ctrl Pts',(-14.0484424922265,-67.6642878599627,
59.9050597858963));
#149203=CARTESIAN_POINT('Ctrl Pts',(-14.0292131234284,-67.7254302696874,
59.8707608921751));
#149204=CARTESIAN_POINT('Ctrl Pts',(-14.0104870165509,-67.7857031151876,
59.8375212431477));
#149205=CARTESIAN_POINT('Ctrl Pts',(-13.9922553803942,-67.84507700969,59.8052981836874));
#149206=CARTESIAN_POINT('Origin',(-15.5675364833309,-75.,72.98888938658));
#149207=CARTESIAN_POINT('',(-13.992324693093,-82.1549107482684,59.80529132868));
#149208=CARTESIAN_POINT('Ctrl Pts',(-13.9923246930889,-82.1549106597401,
59.8052914918042));
#149209=CARTESIAN_POINT('Ctrl Pts',(-14.0326498230923,-82.2862352156339,
59.8765630424347));
#149210=CARTESIAN_POINT('Ctrl Pts',(-14.0753636476136,-82.4216623800802,
59.9525976352346));
#149211=CARTESIAN_POINT('Ctrl Pts',(-14.1204661666528,-82.5608583504549,
60.0338355077126));
#149212=CARTESIAN_POINT('Ctrl Pts',(-14.164833681325,-82.6977859409637,
60.1137495031144));
#149213=CARTESIAN_POINT('Ctrl Pts',(-14.2115126710949,-82.8383606652471,
60.1986989265006));
#149214=CARTESIAN_POINT('Ctrl Pts',(-14.2605031359626,-82.9822165051163,
60.2891169608454));
#149215=CARTESIAN_POINT('Ctrl Pts',(-14.2838382988673,-83.0507379912303,
60.3321849245127));
#149216=CARTESIAN_POINT('Ctrl Pts',(-14.3076978920675,-83.1200031737454,
60.376493789032));
#149217=CARTESIAN_POINT('Ctrl Pts',(-14.3320819155632,-83.189968386651,
60.4220911537103));
#149218=CARTESIAN_POINT('Ctrl Pts',(-14.3821603647954,-83.3336587568286,
60.5157362944545));
#149219=CARTESIAN_POINT('Ctrl Pts',(-14.4344507817197,-83.4803050486517,
60.6148159552382));
#149220=CARTESIAN_POINT('Ctrl Pts',(-14.4889531663359,-83.629491646429,
60.7197462248017));
#149221=CARTESIAN_POINT('Ctrl Pts',(-14.5038961495022,-83.6703943121549,
60.7485150807473));
#149222=CARTESIAN_POINT('Ctrl Pts',(-14.5190054059185,-83.7114876322699,
60.7777237429279));
#149223=CARTESIAN_POINT('Ctrl Pts',(-14.5342809355846,-83.7527623504291,
60.807380808538));
#149224=CARTESIAN_POINT('Ctrl Pts',(-14.5697763505206,-83.8486715123008,
60.8762942847067));
#149225=CARTESIAN_POINT('Ctrl Pts',(-14.6061695545896,-83.9455607506708,
60.9476289427235));
#149226=CARTESIAN_POINT('Ctrl Pts',(-14.6434605477914,-84.0433074223558,
61.0214923903754));
#149227=CARTESIAN_POINT('Ctrl Pts',(-14.6621060443923,-84.0921807581983,
61.0584241142014));
#149228=CARTESIAN_POINT('Ctrl Pts',(-14.6809759882764,-84.1412684034276,
61.0959880996756));
#149229=CARTESIAN_POINT('Ctrl Pts',(-14.7000703794438,-84.1905540445187,
61.1341976421785));
#149230=CARTESIAN_POINT('Ctrl Pts',(-14.7096175750275,-84.2151968650643,
61.15330241343));
#149231=CARTESIAN_POINT('Ctrl Pts',(-14.719220882432,-84.2398891817751,
61.1725685777272));
#149232=CARTESIAN_POINT('Ctrl Pts',(-14.7288803016573,-84.2646289158787,
61.1919978023081));
#149233=CARTESIAN_POINT('Ctrl Pts',(-14.7337100112699,-84.2769987829305,
61.2017124145986));
#149234=CARTESIAN_POINT('Ctrl Pts',(-14.7385537488377,-84.2893805041449,
61.2114677921951));
#149235=CARTESIAN_POINT('Ctrl Pts',(-14.7434115143608,-84.3017738161273,
61.2212641429886));
#149236=CARTESIAN_POINT('Ctrl Pts',(-14.7470548385031,-84.3110688001141,
61.2286114060838));
#149237=CARTESIAN_POINT('Ctrl Pts',(-14.7507060533702,-84.3203703038928,
61.2359817166214));
#149238=CARTESIAN_POINT('Ctrl Pts',(-14.7543651589621,-84.3296782155313,
61.2433751622201));
#149239=CARTESIAN_POINT('Ctrl Pts',(-14.755584860826,-84.3327808527442,
61.2458396440863));
#149240=CARTESIAN_POINT('Ctrl Pts',(-14.7573339681262,-84.3372273399798,
61.2493753137917));
#149241=CARTESIAN_POINT('Ctrl Pts',(-14.7580268947955,-84.3389882589171,
61.2507763227265));
#149242=CARTESIAN_POINT('Ctrl Pts',(-14.7768365894209,-84.386788912201,
61.2888071150147));
#149243=CARTESIAN_POINT('Ctrl Pts',(-14.7977293784119,-84.4394960083863,
61.3312128540246));
#149244=CARTESIAN_POINT('Ctrl Pts',(-14.8207052617688,-84.4969374834265,
61.3781969681284));
#149245=CARTESIAN_POINT('Ctrl Pts',(-14.8436265989847,-84.5542425889202,
61.425069539095));
#149246=CARTESIAN_POINT('Ctrl Pts',(-14.8686211515223,-84.6162597920851,
61.4764989573845));
#149247=CARTESIAN_POINT('Ctrl Pts',(-14.8956889193815,-84.6827791928586,
61.532721305483));
#149248=CARTESIAN_POINT('Ctrl Pts',(-14.9054580666535,-84.7067870026634,
61.5530127606711));
#149249=CARTESIAN_POINT('Ctrl Pts',(-14.9154972693076,-84.7313808828853,
61.5739288477366));
#149250=CARTESIAN_POINT('Ctrl Pts',(-14.9258065273436,-84.7565496415734,
61.5954816833722));
#149251=CARTESIAN_POINT('Ctrl Pts',(-14.9613055287583,-84.8432159949767,
61.6696969314578));
#149252=CARTESIAN_POINT('Ctrl Pts',(-15.0001623842594,-84.9370814084717,
61.7517856729689));
#149253=CARTESIAN_POINT('Ctrl Pts',(-15.0421313229565,-85.0370242993539,
61.8417757146836));
#149254=CARTESIAN_POINT('Ctrl Pts',(-15.0799715589912,-85.1271352885374,
61.9229129682091));
#149255=CARTESIAN_POINT('Ctrl Pts',(-15.1203416923637,-85.2221854894093,
62.0104747748732));
#149256=CARTESIAN_POINT('Ctrl Pts',(-15.1630615839724,-85.3213168395165,
62.1044776570324));
#149257=CARTESIAN_POINT('Ctrl Pts',(-15.2011471370805,-85.4096942243133,
62.1882829202475));
#149258=CARTESIAN_POINT('Ctrl Pts',(-15.2372063400547,-85.4924235671457,
62.2687710769314));
#149259=CARTESIAN_POINT('Ctrl Pts',(-15.271239192895,-85.5697904373298,
62.3456037044735));
#149260=CARTESIAN_POINT('Ctrl Pts',(-15.3055305040041,-85.6477448605887,
62.4230198278512));
#149261=CARTESIAN_POINT('Ctrl Pts',(-15.3377645703823,-85.7202553698275,
62.4967248514297));
#149262=CARTESIAN_POINT('Ctrl Pts',(-15.3679413920297,-85.7875924641561,
62.5664209252565));
#149263=CARTESIAN_POINT('Ctrl Pts',(-15.3982064291167,-85.8551264039793,
62.6363207405465));
#149264=CARTESIAN_POINT('Ctrl Pts',(-15.4264021760685,-85.917456901521,
62.7021883246434));
#149265=CARTESIAN_POINT('Ctrl Pts',(-15.4525286328851,-85.9748308097405,
62.7637689130809));
#149266=CARTESIAN_POINT('Ctrl Pts',(-15.4787359078586,-86.0323821952792,
62.8255399915529));
#149267=CARTESIAN_POINT('Ctrl Pts',(-15.5028610708378,-86.0849465067054,
62.8829976855202));
#149268=CARTESIAN_POINT('Ctrl Pts',(-15.5249041218226,-86.1327430496248,
62.9359280223336));
#149269=CARTESIAN_POINT('Ctrl Pts',(-15.540118771326,-86.1657333851503,
62.9724618271717));
#149270=CARTESIAN_POINT('Ctrl Pts',(-15.554341482711,-86.1964516844456,
63.006839651937));
#149271=CARTESIAN_POINT('Ctrl Pts',(-15.5675722559773,-86.2249610151766,
63.0390024421084));
#149272=CARTESIAN_POINT('Ctrl Pts',(-13.9923246931012,-82.1549108584552,
59.8052911256458));
#149273=CARTESIAN_POINT('Ctrl Pts',(-13.8764053214032,-81.7772458110216,
59.6003274086972));
#149274=CARTESIAN_POINT('Ctrl Pts',(-13.759594104912,-81.3911404276565,
59.4119043240187));
#149275=CARTESIAN_POINT('Ctrl Pts',(-13.6461287874938,-80.998246292647,
59.2404767632645));
#149276=CARTESIAN_POINT('Ctrl Pts',(-13.5955968116095,-80.8232702082617,
59.1641312017921));
#149277=CARTESIAN_POINT('Ctrl Pts',(-13.5457287373038,-80.6469483273635,
59.091156658539));
#149278=CARTESIAN_POINT('Ctrl Pts',(-13.4969004303083,-80.4694293652599,
59.0215935397703));
#149279=CARTESIAN_POINT('Ctrl Pts',(-13.4891180900334,-80.4411360851249,
59.0105064492247));
#149280=CARTESIAN_POINT('Ctrl Pts',(-13.4813621647133,-80.4128123990875,
58.9995060170376));
#149281=CARTESIAN_POINT('Ctrl Pts',(-13.4736342771085,-80.3844581946216,
58.9885923464971));
#149282=CARTESIAN_POINT('Ctrl Pts',(-13.3910906411719,-80.0815993474981,
58.8720205103256));
#149283=CARTESIAN_POINT('Ctrl Pts',(-13.3117448569047,-79.7752576428201,
58.76534781653));
#149284=CARTESIAN_POINT('Ctrl Pts',(-13.2375806890342,-79.4653029779942,
58.6686969596962));
#149285=CARTESIAN_POINT('Ctrl Pts',(-13.200498605099,-79.3103256455813,
58.6203715312792));
#149286=CARTESIAN_POINT('Ctrl Pts',(-13.1647119249596,-79.1544451175713,
58.5745514140121));
#149287=CARTESIAN_POINT('Ctrl Pts',(-13.1304700378892,-78.9976463931186,
58.5312511229017));
#149288=CARTESIAN_POINT('Ctrl Pts',(-13.1133490943541,-78.9192470308923,
58.5096009773465));
#149289=CARTESIAN_POINT('Ctrl Pts',(-13.0966143490608,-78.8406181238311,
58.4885807747893));
#149290=CARTESIAN_POINT('Ctrl Pts',(-13.0802970349933,-78.7617578322529,
58.468192245756));
#149291=CARTESIAN_POINT('Ctrl Pts',(-13.0761874678022,-78.7418966182315,
58.4630573301907));
#149292=CARTESIAN_POINT('Ctrl Pts',(-13.0721043779967,-78.7220207273617,
58.4579624813401));
#149293=CARTESIAN_POINT('Ctrl Pts',(-13.0680482612186,-78.7021301359867,
58.4529077276365));
#149294=CARTESIAN_POINT('Ctrl Pts',(-13.0640518352002,-78.6825322591894,
58.4479273608663));
#149295=CARTESIAN_POINT('Ctrl Pts',(-13.0600815941711,-78.6629201113842,
58.4429859178198));
#149296=CARTESIAN_POINT('Ctrl Pts',(-13.0561378076375,-78.6432939594342,
58.4380834580874));
#149297=CARTESIAN_POINT('Ctrl Pts',(-13.0521645688367,-78.623521239036,
58.4331443866995));
#149298=CARTESIAN_POINT('Ctrl Pts',(-13.0482182337873,-78.6037342324225,
58.4282448649682));
#149299=CARTESIAN_POINT('Ctrl Pts',(-13.0442990168641,-78.5839332966098,
58.4233849750262));
#149300=CARTESIAN_POINT('Ctrl Pts',(-13.0423394084025,-78.5740328287034,
58.4209550300552));
#149301=CARTESIAN_POINT('Ctrl Pts',(-13.0403865794723,-78.5641288785112,
58.4185349929956));
#149302=CARTESIAN_POINT('Ctrl Pts',(-13.0384405700567,-78.5542214726372,
58.4161248695598));
#149303=CARTESIAN_POINT('Ctrl Pts',(-13.036981062995,-78.5467909182318,
58.4143172769829));
#149304=CARTESIAN_POINT('Ctrl Pts',(-13.0355253919102,-78.5393584200044,
58.4125152608217));
#149305=CARTESIAN_POINT('Ctrl Pts',(-13.034073571557,-78.5319239920785,
58.4107188242082));
#149306=CARTESIAN_POINT('Ctrl Pts',(-13.0335896314393,-78.5294458494366,
58.4101200120037));
#149307=CARTESIAN_POINT('Ctrl Pts',(-13.0328644451769,-78.5257275292609,
58.4092228702754));
#149308=CARTESIAN_POINT('Ctrl Pts',(-13.0326230353278,-78.5244889214428,
58.4089242475597));
#149309=CARTESIAN_POINT('Ctrl Pts',(-13.0200682121633,-78.460073562334,
58.3933939972347));
#149310=CARTESIAN_POINT('Ctrl Pts',(-13.0065976875759,-78.3901336774366,
58.3769827524417));
#149311=CARTESIAN_POINT('Ctrl Pts',(-12.9923806697727,-78.31460200394,58.3599205538385));
#149312=CARTESIAN_POINT('Ctrl Pts',(-12.9777555199851,-78.2369020211531,
58.3423685458343));
#149313=CARTESIAN_POINT('Ctrl Pts',(-12.9623398683733,-78.1532842847873,
58.3241273990271));
#149314=CARTESIAN_POINT('Ctrl Pts',(-12.9463600484581,-78.0636753035669,
58.3054893939602));
#149315=CARTESIAN_POINT('Ctrl Pts',(-12.9315695409071,-77.9807355507775,
58.2882385390605));
#149316=CARTESIAN_POINT('Ctrl Pts',(-12.9162959040133,-77.8926629407206,
58.2706480744648));
#149317=CARTESIAN_POINT('Ctrl Pts',(-12.9007554028391,-77.7994028167243,
58.2529831582825));
#149318=CARTESIAN_POINT('Ctrl Pts',(-12.8855314124791,-77.7080421062309,
58.2356780205231));
#149319=CARTESIAN_POINT('Ctrl Pts',(-12.8700511623901,-77.61170279788,58.218301470208));
#149320=CARTESIAN_POINT('Ctrl Pts',(-12.8545549880426,-77.510340523674,
58.2011336697347));
#149321=CARTESIAN_POINT('Ctrl Pts',(-12.8393842755942,-77.4111071335083,
58.1843264398654));
#149322=CARTESIAN_POINT('Ctrl Pts',(-12.8241981560509,-77.3070593267112,
58.1677193176427));
#149323=CARTESIAN_POINT('Ctrl Pts',(-12.8092601697167,-77.1981656687249,
58.1516045550749));
#149324=CARTESIAN_POINT('Ctrl Pts',(-12.7946393385933,-77.0915839817282,
58.1358319323916));
#149325=CARTESIAN_POINT('Ctrl Pts',(-12.7802560819789,-76.9803598142564,
58.1205310146299));
#149326=CARTESIAN_POINT('Ctrl Pts',(-12.7663963661219,-76.8644767830903,
58.1060037986954));
#149327=CARTESIAN_POINT('Ctrl Pts',(-12.7527924430809,-76.7507324715907,
58.0917446948572));
#149328=CARTESIAN_POINT('Ctrl Pts',(-12.7396927706292,-76.6324994663116,
58.0782310111901));
#149329=CARTESIAN_POINT('Ctrl Pts',(-12.7274076754917,-76.509778133224,
58.0657752664847));
#149330=CARTESIAN_POINT('Ctrl Pts',(-12.7155212989591,-76.3910397793613,
58.053723778897));
#149331=CARTESIAN_POINT('Ctrl Pts',(-12.7043974504569,-76.2680995647439,
58.042662743653));
#149332=CARTESIAN_POINT('Ctrl Pts',(-12.6943560376396,-76.1409753244791,
58.0328999684157));
#149333=CARTESIAN_POINT('Ctrl Pts',(-12.6844879597932,-76.0160455041525,
58.0233057183046));
#149334=CARTESIAN_POINT('Ctrl Pts',(-12.675665147966,-75.8870746813651,
58.0149652977699));
#149335=CARTESIAN_POINT('Ctrl Pts',(-12.6682306289814,-75.7540994155384,
58.0081946946424));
#149336=CARTESIAN_POINT('Ctrl Pts',(-12.6609684644375,-75.6242069150686,
58.0015810543955));
#149337=CARTESIAN_POINT('Ctrl Pts',(-12.655030899086,-75.4904933443661,
57.9964653146573));
#149338=CARTESIAN_POINT('Ctrl Pts',(-12.6507769180658,-75.3530140123066,
57.9931646932654));
#149339=CARTESIAN_POINT('Ctrl Pts',(-12.6500770198269,-75.3303948370138,
57.9926216492113));
#149340=CARTESIAN_POINT('Ctrl Pts',(-12.6494227846886,-75.3076737752469,
57.992127789802));
#149341=CARTESIAN_POINT('Ctrl Pts',(-12.6488159186004,-75.2848511344054,
57.9916845878715));
#149342=CARTESIAN_POINT('Ctrl Pts',(-12.647423216751,-75.2324752730287,
57.990667480209));
#149343=CARTESIAN_POINT('Ctrl Pts',(-12.6462799292659,-75.1795643997014,
57.9899171327559));
#149344=CARTESIAN_POINT('Ctrl Pts',(-12.6454073095658,-75.1261226027846,
57.9894516915813));
#149345=CARTESIAN_POINT('Ctrl Pts',(-12.6449709997158,-75.0994017043262,
57.989218970994));
#149346=CARTESIAN_POINT('Ctrl Pts',(-12.6446023568134,-75.0725480749185,
57.9890574844566));
#149347=CARTESIAN_POINT('Ctrl Pts',(-12.6443041376411,-75.0455622853593,
57.9889695458607));
#149348=CARTESIAN_POINT('Ctrl Pts',(-12.644155028055,-75.0320693905796,
57.9889255765627));
#149349=CARTESIAN_POINT('Ctrl Pts',(-12.6440235244015,-75.0185434557562,
57.988899994721));
#149350=CARTESIAN_POINT('Ctrl Pts',(-12.6439099743117,-75.004984554064,
57.9888930924322));
#149351=CARTESIAN_POINT('Ctrl Pts',(-12.6438586623979,-74.9988574501932,
57.9888899733713));
#149352=CARTESIAN_POINT('Ctrl Pts',(-12.6438110165178,-74.992723614377,
57.9888906687514));
#149353=CARTESIAN_POINT('Ctrl Pts',(-12.643767068976,-74.9865830535138,
57.9888952056554));
#149354=CARTESIAN_POINT('Ctrl Pts',(-12.6437623899226,-74.9859292737851,
57.9888956886953));
#149355=CARTESIAN_POINT('Ctrl Pts',(-12.6437577527925,-74.9852754178238,
57.9888962152815));
#149356=CARTESIAN_POINT('Ctrl Pts',(-12.6437531576071,-74.9846214856349,
57.9888967854431));
#149357=CARTESIAN_POINT('Ctrl Pts',(-12.6437292801042,-74.9812235231251,
57.9888997481169));
#149358=CARTESIAN_POINT('Ctrl Pts',(-12.6437065355134,-74.9778235025011,
57.9889038873485));
#149359=CARTESIAN_POINT('Ctrl Pts',(-12.6436849263517,-74.974421424422,
57.9889092072289));
#149360=CARTESIAN_POINT('Ctrl Pts',(-12.6436741217709,-74.9727203853825,
57.988911867169));
#149361=CARTESIAN_POINT('Ctrl Pts',(-12.6436636010473,-74.9710188319792,
57.9889148222714));
#149362=CARTESIAN_POINT('Ctrl Pts',(-12.6436533645937,-74.9693167643124,
57.9889180730478));
#149363=CARTESIAN_POINT('Ctrl Pts',(-12.64364312814,-74.9676146966457,57.9889213238242));
#149364=CARTESIAN_POINT('Ctrl Pts',(-12.6436266975925,-74.9647708441181,
57.9889274452835));
#149365=CARTESIAN_POINT('Ctrl Pts',(-12.6436235084189,-74.9642090186155,
57.9889287129107));
#149366=CARTESIAN_POINT('Ctrl Pts',(-12.6423924798547,-74.7473430452712,
57.9894180200292));
#149367=CARTESIAN_POINT('Ctrl Pts',(-12.6464722421314,-74.5272810364192,
57.9946990479728));
#149368=CARTESIAN_POINT('Ctrl Pts',(-12.6559493112579,-74.3042892424013,
58.0051451784453));
#149369=CARTESIAN_POINT('Ctrl Pts',(-12.6590427852643,-74.2315009880133,
58.0085549702968));
#149370=CARTESIAN_POINT('Ctrl Pts',(-12.6627110658457,-74.1584008772902,
58.0125150158115));
#149371=CARTESIAN_POINT('Ctrl Pts',(-12.6669563735319,-74.0849990552687,
58.0170380732945));
#149372=CARTESIAN_POINT('Ctrl Pts',(-12.6755819225541,-73.9358623940509,
58.0262279499616));
#149373=CARTESIAN_POINT('Ctrl Pts',(-12.6865899761586,-73.7854797682283,
58.037742148481));
#149374=CARTESIAN_POINT('Ctrl Pts',(-12.6999939404739,-73.6339417234719,
58.0516862103875));
#149375=CARTESIAN_POINT('Ctrl Pts',(-12.7016694360133,-73.6149994678774,
58.0534292181258));
#149376=CARTESIAN_POINT('Ctrl Pts',(-12.7033823676581,-73.596039158706,
58.0552101908171));
#149377=CARTESIAN_POINT('Ctrl Pts',(-12.7051327395031,-73.5770609952093,
58.0570293310643));
#149378=CARTESIAN_POINT('Ctrl Pts',(-12.7060079254256,-73.567571913461,
58.0579389011879));
#149379=CARTESIAN_POINT('Ctrl Pts',(-12.7068924713982,-73.5580783681313,
58.0588580131901));
#149380=CARTESIAN_POINT('Ctrl Pts',(-12.7077863807806,-73.5485803811959,
58.0597866926387));
#149381=CARTESIAN_POINT('Ctrl Pts',(-12.7083434951339,-73.5426609167027,
58.0603654768652));
#149382=CARTESIAN_POINT('Ctrl Pts',(-12.7094999600431,-73.5304270822779,
58.0615666407172));
#149383=CARTESIAN_POINT('Ctrl Pts',(-12.7107956448812,-73.5169414277841,
58.062914021425));
#149384=CARTESIAN_POINT('Ctrl Pts',(-12.7115789314904,-73.5087888799804,
58.0637285599879));
#149385=CARTESIAN_POINT('Ctrl Pts',(-12.7124127687112,-73.5001787991258,
58.0645961630611));
#149386=CARTESIAN_POINT('Ctrl Pts',(-12.7131886153166,-73.492228755033,
58.0654037341901));
#149387=CARTESIAN_POINT('Ctrl Pts',(-12.7256079849222,-73.3649683722766,
58.0783309343132));
#149388=CARTESIAN_POINT('Ctrl Pts',(-12.7394903373919,-73.2379099565758,
58.0928780348362));
#149389=CARTESIAN_POINT('Ctrl Pts',(-12.7547724123794,-73.111094650057,
58.1090308435863));
#149390=CARTESIAN_POINT('Ctrl Pts',(-12.8005432352705,-72.7312744398236,
58.1574095715472));
#149391=CARTESIAN_POINT('Ctrl Pts',(-12.8588680404003,-72.3536377877317,
58.2201931924962));
#149392=CARTESIAN_POINT('Ctrl Pts',(-12.9276269165322,-71.9805430020649,
58.2966226816471));
#149393=CARTESIAN_POINT('Ctrl Pts',(-12.9713073127522,-71.7435273761213,
58.3451759820618));
#149394=CARTESIAN_POINT('Ctrl Pts',(-13.0191991735993,-71.5083440691444,
58.3992359930534));
#149395=CARTESIAN_POINT('Ctrl Pts',(-13.070764446851,-71.2755883075958,
58.4586057913291));
#149396=CARTESIAN_POINT('Ctrl Pts',(-13.0726976055627,-71.2668623996393,
58.4608315381451));
#149397=CARTESIAN_POINT('Ctrl Pts',(-13.0746359275625,-71.2581399024908,
58.4630647475309));
#149398=CARTESIAN_POINT('Ctrl Pts',(-13.0765793755592,-71.2494208109103,
58.4653054191105));
#149399=CARTESIAN_POINT('Ctrl Pts',(-13.0824690904162,-71.2229971745143,
58.4720958846719));
#149400=CARTESIAN_POINT('Ctrl Pts',(-13.088563822919,-71.1959483931376,
58.4791276115216));
#149401=CARTESIAN_POINT('Ctrl Pts',(-13.094365672755,-71.1703746713447,
58.4858479438368));
#149402=CARTESIAN_POINT('Ctrl Pts',(-13.0974641278934,-71.1567171255727,
58.4894369109391));
#149403=CARTESIAN_POINT('Ctrl Pts',(-13.1004785546761,-71.1434799258363,
58.4929362950644));
#149404=CARTESIAN_POINT('Ctrl Pts',(-13.1033301380902,-71.1309808245413,
58.4962571597016));
#149405=CARTESIAN_POINT('Ctrl Pts',(-13.117605932808,-71.0684069565064,
58.5128823026352));
#149406=CARTESIAN_POINT('Ctrl Pts',(-13.1333784859781,-70.9996257008027,
58.5315864012066));
#149407=CARTESIAN_POINT('Ctrl Pts',(-13.1507809817488,-70.9247447921021,
58.5526325801446));
#149408=CARTESIAN_POINT('Ctrl Pts',(-13.168897069721,-70.8467933794233,
58.5745417611118));
#149409=CARTESIAN_POINT('Ctrl Pts',(-13.1887803485131,-70.7622317902181,
58.5989886469898));
#149410=CARTESIAN_POINT('Ctrl Pts',(-13.2105817144479,-70.6712004295549,
58.6263267340083));
#149411=CARTESIAN_POINT('Ctrl Pts',(-13.2311438855887,-70.5853433129532,
58.6521109176973));
#149412=CARTESIAN_POINT('Ctrl Pts',(-13.2534130327245,-70.4937312430357,
58.6804674325607));
#149413=CARTESIAN_POINT('Ctrl Pts',(-13.2775048114296,-70.3964964858422,
58.711740169317));
#149414=CARTESIAN_POINT('Ctrl Pts',(-13.3010877577409,-70.3013153833359,
58.7423524076643));
#149415=CARTESIAN_POINT('Ctrl Pts',(-13.3264179063024,-70.2007467197002,
58.7757591300533));
#149416=CARTESIAN_POINT('Ctrl Pts',(-13.3535821398449,-70.0949263892232,
58.8123256645947));
#149417=CARTESIAN_POINT('Ctrl Pts',(-13.379711247878,-69.9931384686179,
58.8474987877359));
#149418=CARTESIAN_POINT('Ctrl Pts',(-13.4075379091794,-69.8864916331328,
58.8855957367618));
#149419=CARTESIAN_POINT('Ctrl Pts',(-13.4371097624152,-69.7751159602277,
58.9269786558671));
#149420=CARTESIAN_POINT('Ctrl Pts',(-13.4452861747418,-69.7443213591059,
58.938420745992));
#149421=CARTESIAN_POINT('Ctrl Pts',(-13.4535957952498,-69.7131652949402,
58.9501142568892));
#149422=CARTESIAN_POINT('Ctrl Pts',(-13.4620391155253,-69.6816506263856,
58.9620673329486));
#149423=CARTESIAN_POINT('Ctrl Pts',(-13.46677738784,-69.6639650386489,58.968775230733));
#149424=CARTESIAN_POINT('Ctrl Pts',(-13.4715577617754,-69.6461665165836,
58.9755648770865));
#149425=CARTESIAN_POINT('Ctrl Pts',(-13.4763802887566,-69.6282555714961,
58.9824377406472));
#149426=CARTESIAN_POINT('Ctrl Pts',(-13.4787915522472,-69.6193000989524,
58.9858741724276));
#149427=CARTESIAN_POINT('Ctrl Pts',(-13.481213354,-69.6103165207718,58.9893314088175));
#149428=CARTESIAN_POINT('Ctrl Pts',(-13.4836456973389,-69.6013049011923,
58.9928096353972));
#149429=CARTESIAN_POINT('Ctrl Pts',(-13.4859012793976,-69.592948166714,
58.9960350951191));
#149430=CARTESIAN_POINT('Ctrl Pts',(-13.4893480346654,-69.5801931700439,
59.0009709140122));
#149431=CARTESIAN_POINT('Ctrl Pts',(-13.4925521253834,-69.568363122783,
59.0055695370881));
#149432=CARTESIAN_POINT('Ctrl Pts',(-13.4928032176347,-69.5674360475342,
59.0059299134702));
#149433=CARTESIAN_POINT('Ctrl Pts',(-13.4930528122557,-69.5665146428691,
59.0062881936137));
#149434=CARTESIAN_POINT('Ctrl Pts',(-13.4933002153033,-69.5656014654837,
59.0066433785788));
#149435=CARTESIAN_POINT('Ctrl Pts',(-13.506917884383,-69.5153379478529,
59.0261936281169));
#149436=CARTESIAN_POINT('Ctrl Pts',(-13.520340769412,-69.4661983742167,
59.0456237114897));
#149437=CARTESIAN_POINT('Ctrl Pts',(-13.533551277004,-69.4181692104236,
59.0649008672749));
#149438=CARTESIAN_POINT('Ctrl Pts',(-13.559972292188,-69.3221108828374,
59.1034551788453));
#149439=CARTESIAN_POINT('Ctrl Pts',(-13.5855437946768,-69.2304936374915,
59.1413963750281));
#149440=CARTESIAN_POINT('Ctrl Pts',(-13.6101573958495,-69.1432184685839,
59.1784781910238));
#149441=CARTESIAN_POINT('Ctrl Pts',(-13.6375278398563,-69.046168057024,
59.219713350449));
#149442=CARTESIAN_POINT('Ctrl Pts',(-13.6637136362959,-68.9544866600855,
59.2598853043287));
#149443=CARTESIAN_POINT('Ctrl Pts',(-13.6886091518112,-68.8680542840001,
59.2986865946742));
#149444=CARTESIAN_POINT('Ctrl Pts',(-13.7140937238119,-68.7795768186437,
59.338405968106));
#149445=CARTESIAN_POINT('Ctrl Pts',(-13.7382267357766,-68.6965997193151,
59.3766888995997));
#149446=CARTESIAN_POINT('Ctrl Pts',(-13.7609340346995,-68.6190114939214,
59.4132413986414));
#149447=CARTESIAN_POINT('Ctrl Pts',(-13.7843489555268,-68.5390054059721,
59.4509329741125));
#149448=CARTESIAN_POINT('Ctrl Pts',(-13.8062484159958,-68.4647292758614,
59.4867843745649));
#149449=CARTESIAN_POINT('Ctrl Pts',(-13.8265845753271,-68.3960790089942,
59.5205137508794));
#149450=CARTESIAN_POINT('Ctrl Pts',(-13.8365619932143,-68.3623975065314,
59.5370622090755));
#149451=CARTESIAN_POINT('Ctrl Pts',(-13.846163558071,-68.3300704921782,
59.5531004967338));
#149452=CARTESIAN_POINT('Ctrl Pts',(-13.8553858823851,-68.2990872092859,
59.5685989544768));
#149453=CARTESIAN_POINT('Ctrl Pts',(-13.8747444748846,-68.2340501614248,
59.6011317865045));
#149454=CARTESIAN_POINT('Ctrl Pts',(-13.8924309393971,-68.1749327207469,
59.6312830134023));
#149455=CARTESIAN_POINT('Ctrl Pts',(-13.9084295097878,-68.1216492241398,
59.6588125801309));
#149456=CARTESIAN_POINT('Ctrl Pts',(-13.9245519020274,-68.0679533368688,
59.6865552135129));
#149457=CARTESIAN_POINT('Ctrl Pts',(-13.9389606952694,-68.0201820868406,
59.7116353842495));
#149458=CARTESIAN_POINT('Ctrl Pts',(-13.9516539764714,-67.97826618418,59.7338551628796));
#149459=CARTESIAN_POINT('Ctrl Pts',(-13.9644135161547,-67.936131481982,
59.7561909279724));
#149460=CARTESIAN_POINT('Ctrl Pts',(-13.9754400180266,-67.8999134516241,
59.7756363162961));
#149461=CARTESIAN_POINT('Ctrl Pts',(-13.9847386240222,-67.8695596322964,
59.7920391320418));
#149462=CARTESIAN_POINT('Ctrl Pts',(-13.9873839818165,-67.8609242828058,
59.7967055644621));
#149463=CARTESIAN_POINT('Ctrl Pts',(-13.989889515867,-67.8527636585599,
59.8011260517909));
#149464=CARTESIAN_POINT('Ctrl Pts',(-13.9922553804113,-67.8450768092218,
59.8052978142969));
#149465=CARTESIAN_POINT('Ctrl Pts',(-14.2053627384179,-82.25455936809,59.85616341864));
#149466=CARTESIAN_POINT('Ctrl Pts',(-13.6866847824119,-82.3366282815,59.92373292204));
#149467=CARTESIAN_POINT('Ctrl Pts',(-12.6383817091255,-82.58289982254,59.91553905833));
#149468=CARTESIAN_POINT('Ctrl Pts',(-11.1637780911499,-83.19639241636,59.42315761485));
#149469=CARTESIAN_POINT('Ctrl Pts',(-9.99316319052391,-83.97026149908,58.51581872871));
#149470=CARTESIAN_POINT('Ctrl Pts',(-9.52143302578291,-84.52126777961,57.71959030244));
#149471=CARTESIAN_POINT('Ctrl Pts',(-9.36367665720391,-84.79397357294,57.29408547033));
#149472=CARTESIAN_POINT('Ctrl Pts',(-14.0202046372369,-81.66798572512,59.53231650414));
#149473=CARTESIAN_POINT('Ctrl Pts',(-13.5161419891421,-81.7529897771,59.59488219199));
#149474=CARTESIAN_POINT('Ctrl Pts',(-12.5016391850972,-81.9934997129,59.58065052531));
#149475=CARTESIAN_POINT('Ctrl Pts',(-11.0704533736609,-82.56018318755,59.10069440813));
#149476=CARTESIAN_POINT('Ctrl Pts',(-9.91290994947291,-83.2607556917,58.2229682051));
#149477=CARTESIAN_POINT('Ctrl Pts',(-9.42170896486991,-83.75798893721,57.44738812635));
#149478=CARTESIAN_POINT('Ctrl Pts',(-9.24823875588991,-84.00518323524,57.0294496165));
#149479=CARTESIAN_POINT('Ctrl Pts',(-13.6549069241899,-80.50006195024,58.98674389696));
#149480=CARTESIAN_POINT('Ctrl Pts',(-13.1769404748632,-80.58353896436,59.03665035665));
#149481=CARTESIAN_POINT('Ctrl Pts',(-12.2218902458404,-80.80094275264,59.00590868676));
#149482=CARTESIAN_POINT('Ctrl Pts',(-10.8679330721049,-81.27153994433,58.54326883773));
#149483=CARTESIAN_POINT('Ctrl Pts',(-9.73897835675991,-81.83491357831,57.71819138306));
#149484=CARTESIAN_POINT('Ctrl Pts',(-9.21997508227391,-82.23283245568,56.98439768797));
#149485=CARTESIAN_POINT('Ctrl Pts',(-9.02174978536891,-82.43224264183,56.58383055835));
#149486=CARTESIAN_POINT('Ctrl Pts',(-13.0264541098134,-78.10903159314,58.22143278291));
#149487=CARTESIAN_POINT('Ctrl Pts',(-12.5887620025533,-78.16896765775,58.24468551411));
#149488=CARTESIAN_POINT('Ctrl Pts',(-11.7230981427644,-78.30931348211,58.17830836715));
#149489=CARTESIAN_POINT('Ctrl Pts',(-10.4863172342789,-78.57820044195,57.73325733766));
#149490=CARTESIAN_POINT('Ctrl Pts',(-9.41080141879391,-78.88372055786,56.98713738772));
#149491=CARTESIAN_POINT('Ctrl Pts',(-8.86349672505391,-79.09709391693,56.32569316036));
#149492=CARTESIAN_POINT('Ctrl Pts',(-8.63464566340091,-79.20524884609,55.9591981337));
#149493=CARTESIAN_POINT('Ctrl Pts',(-12.703739323494,-75.60837772321,57.90748319535));
#149494=CARTESIAN_POINT('Ctrl Pts',(-12.2839358655288,-75.61999252453,57.91587997198));
#149495=CARTESIAN_POINT('Ctrl Pts',(-11.4571120723489,-75.64721072235,57.82979946692));
#149496=CARTESIAN_POINT('Ctrl Pts',(-10.2725544129919,-75.69964966516,57.38928272527));
#149497=CARTESIAN_POINT('Ctrl Pts',(-9.22672717125391,-75.7595397854,56.67735146262));
#149498=CARTESIAN_POINT('Ctrl Pts',(-8.67519748870391,-75.80154788321,56.05133853923));
#149499=CARTESIAN_POINT('Ctrl Pts',(-8.43723858833691,-75.82288542366,55.70323479651));
#149500=CARTESIAN_POINT('Ctrl Pts',(-12.8671141721127,-73.11809265367,58.06713723927));
#149501=CARTESIAN_POINT('Ctrl Pts',(-12.4383232178021,-73.08201133181,58.08327470442));
#149502=CARTESIAN_POINT('Ctrl Pts',(-11.5918425291893,-72.9974900293,58.00755176422));
#149503=CARTESIAN_POINT('Ctrl Pts',(-10.3806961735769,-72.83504489813,57.56487994748));
#149504=CARTESIAN_POINT('Ctrl Pts',(-9.31980220568191,-72.64992691269,56.83532487628));
#149505=CARTESIAN_POINT('Ctrl Pts',(-8.77051022514591,-72.52032197963,56.19100248932));
#149506=CARTESIAN_POINT('Ctrl Pts',(-8.53719879336891,-72.4545491955,55.83340513874));
#149507=CARTESIAN_POINT('Ctrl Pts',(-13.3015354916696,-70.62027701925,58.54120535384));
#149508=CARTESIAN_POINT('Ctrl Pts',(-12.8466551590814,-70.5435375917,58.57621796265));
#149509=CARTESIAN_POINT('Ctrl Pts',(-11.9431325981647,-70.35631033313,58.52545042363));
#149510=CARTESIAN_POINT('Ctrl Pts',(-10.6566364727679,-69.97916480861,58.07343649006));
#149511=CARTESIAN_POINT('Ctrl Pts',(-9.55738924270591,-69.54092805089,57.29417007323));
#149512=CARTESIAN_POINT('Ctrl Pts',(-9.02052118745191,-69.23342500244,56.60163811033));
#149513=CARTESIAN_POINT('Ctrl Pts',(-8.80382301199891,-69.07836783959,56.22016816974));
#149514=CARTESIAN_POINT('Ctrl Pts',(-13.8489227043029,-68.87555927534,59.23274232687));
#149515=CARTESIAN_POINT('Ctrl Pts',(-13.3583894250031,-68.78795581714,59.29065555428));
#149516=CARTESIAN_POINT('Ctrl Pts',(-12.3751455164616,-68.5530122456,59.2707797108));
#149517=CARTESIAN_POINT('Ctrl Pts',(-10.9840720246409,-68.02991414936,58.80223087688));
#149518=CARTESIAN_POINT('Ctrl Pts',(-9.83859395163391,-67.39731651073,57.95185518517));
#149519=CARTESIAN_POINT('Ctrl Pts',(-9.32938702250191,-66.94987820901,57.19539776513));
#149520=CARTESIAN_POINT('Ctrl Pts',(-9.14138216248191,-66.72629866191,56.78447782593));
#149521=CARTESIAN_POINT('Ctrl Pts',(-14.2054072809129,-67.7452469082,59.85623901085));
#149522=CARTESIAN_POINT('Ctrl Pts',(-13.6867239510529,-67.66316837402,59.92381322088));
#149523=CARTESIAN_POINT('Ctrl Pts',(-12.638412688455,-67.41687470616,59.91562799188));
#149524=CARTESIAN_POINT('Ctrl Pts',(-11.1638044367439,-66.80334542226,59.42325346353));
#149525=CARTESIAN_POINT('Ctrl Pts',(-9.99319080751391,-66.0294416455,58.51591282125));
#149526=CARTESIAN_POINT('Ctrl Pts',(-9.52146541439891,-65.47841540134,57.71967705271));
#149527=CARTESIAN_POINT('Ctrl Pts',(-9.36371259686991,-65.20570054798,57.29416759219));
#149528=CARTESIAN_POINT('',(-9.38953228746991,-84.5398910625,57.36388938658));
#149529=CARTESIAN_POINT('Ctrl Pts',(-9.38953228746991,-84.5398910625,57.36388938658));
#149530=CARTESIAN_POINT('Ctrl Pts',(-9.28299760588214,-83.7881949943336,
57.1128289322841));
#149531=CARTESIAN_POINT('Ctrl Pts',(-9.17640320159037,-83.0289015577622,
56.8968437256352));
#149532=CARTESIAN_POINT('Ctrl Pts',(-9.0288200623923,-81.878565350298,56.6211725879014));
#149533=CARTESIAN_POINT('Ctrl Pts',(-8.98163454409537,-81.4932206057088,
56.5373250438838));
#149534=CARTESIAN_POINT('Ctrl Pts',(-8.91505371442895,-80.912354475673,
56.4230638276863));
#149535=CARTESIAN_POINT('Ctrl Pts',(-8.88280899763094,-80.6212091573672,
56.3688110463283));
#149536=CARTESIAN_POINT('Ctrl Pts',(-8.84724153253191,-80.2802931760899,
56.3104368697372));
#149537=CARTESIAN_POINT('Ctrl Pts',(-8.82999560524952,-80.1095235746376,
56.2824661787593));
#149538=CARTESIAN_POINT('Ctrl Pts',(-8.82272235145397,-80.036269828841,
56.2707379426101));
#149539=CARTESIAN_POINT('Ctrl Pts',(-8.81789998947072,-79.9874191596997,
56.2629765596512));
#149540=CARTESIAN_POINT('Ctrl Pts',(-8.81564686072979,-79.9644706595696,
56.2593567797579));
#149541=CARTESIAN_POINT('Ctrl Pts',(-8.73217725899237,-79.108964570998,
56.1255245945277));
#149542=CARTESIAN_POINT('Ctrl Pts',(-8.66805506192752,-78.2811374986499,
56.03048087595));
#149543=CARTESIAN_POINT('Ctrl Pts',(-8.60339061485789,-77.0420287740733,
55.9360899191963));
#149544=CARTESIAN_POINT('Ctrl Pts',(-8.58704180991944,-76.629431179872,
55.912677597911));
#149545=CARTESIAN_POINT('Ctrl Pts',(-8.57070859794398,-76.0111927595564,
55.8893750942785));
#149546=CARTESIAN_POINT('Ctrl Pts',(-8.5666264756538,-75.805222947949,55.8835786701577));
#149547=CARTESIAN_POINT('Ctrl Pts',(-8.56121809111822,-75.3935026483962,
55.875906038777));
#149548=CARTESIAN_POINT('Ctrl Pts',(-8.55989222037363,-75.1863169678766,
55.8740303858725));
#149549=CARTESIAN_POINT('Ctrl Pts',(-8.5601738412577,-74.1652888001767,
55.8744291786204));
#149550=CARTESIAN_POINT('Ctrl Pts',(-8.58277625686303,-73.3443787169755,
55.9059564905164));
#149551=CARTESIAN_POINT('Ctrl Pts',(-8.64817866699291,-72.1068822686112,
56.0014895705712));
#149552=CARTESIAN_POINT('Ctrl Pts',(-8.6751867907122,-71.6933615652295,
56.0414040317809));
#149553=CARTESIAN_POINT('Ctrl Pts',(-8.72285528790025,-71.0715476792663,
56.1138062125568));
#149554=CARTESIAN_POINT('Ctrl Pts',(-8.74847436625131,-70.7602575285621,
56.1531423150808));
#149555=CARTESIAN_POINT('Ctrl Pts',(-8.78129743014174,-70.3964150725592,
56.2046369603786));
#149556=CARTESIAN_POINT('Ctrl Pts',(-8.79841527834946,-70.2143261911791,
56.2318009811849));
#149557=CARTESIAN_POINT('Ctrl Pts',(-8.80589984657586,-70.136252173435,
56.2437480312132));
#149558=CARTESIAN_POINT('Ctrl Pts',(-8.81092218104178,-70.0841948447782,
56.2517807797118));
#149559=CARTESIAN_POINT('Ctrl Pts',(-8.81362946612278,-70.0563216785734,
56.2561199096933));
#149560=CARTESIAN_POINT('Ctrl Pts',(-8.96727708076544,-68.4835727284964,
56.5028463120566));
#149561=CARTESIAN_POINT('Ctrl Pts',(-9.17702010416681,-66.959567194033,
56.8630815323802));
#149562=CARTESIAN_POINT('Ctrl Pts',(-9.38953228747191,-65.46010893749,57.36388938658));
#149563=CARTESIAN_POINT('Origin',(-13.9922814988585,-84.5398910375432,55.4107645734512));
#149564=CARTESIAN_POINT('Ctrl Pts',(-15.7857783725409,-86.29661480505,63.115509260726));
#149565=CARTESIAN_POINT('Ctrl Pts',(-13.2009589750593,-86.61530731379,63.626388245958));
#149566=CARTESIAN_POINT('Ctrl Pts',(-11.2043264355719,-88.19001512956,62.8661053606));
#149567=CARTESIAN_POINT('Ctrl Pts',(-10.7993789544399,-90.22954893502,61.21655661769));
#149568=CARTESIAN_POINT('Ctrl Pts',(-15.2179723740469,-85.09055880868,61.73606668887));
#149569=CARTESIAN_POINT('Ctrl Pts',(-12.7684152553155,-85.49389189082,62.22346223447));
#149570=CARTESIAN_POINT('Ctrl Pts',(-10.8253714758709,-86.8819838928,61.36857549732));
#149571=CARTESIAN_POINT('Ctrl Pts',(-10.2917538863009,-88.6099845115701,
59.56845212724));
#149572=CARTESIAN_POINT('Ctrl Pts',(-14.6117331505359,-83.64165090183,60.58580302674));
#149573=CARTESIAN_POINT('Ctrl Pts',(-12.2792545314831,-84.06648481616,60.9650212480601));
#149574=CARTESIAN_POINT('Ctrl Pts',(-10.3902588488939,-85.23953592222,60.03498149361));
#149575=CARTESIAN_POINT('Ctrl Pts',(-9.75033914806491,-86.66066443089,58.19212486272));
#149576=CARTESIAN_POINT('Ctrl Pts',(-14.1114447652699,-82.00287655395,59.72095409226));
#149577=CARTESIAN_POINT('Ctrl Pts',(-11.863059732406,-82.36563442235,59.99674441583));
#149578=CARTESIAN_POINT('Ctrl Pts',(-10.0167553446379,-83.30615659356,59.01200819548));
#149579=CARTESIAN_POINT('Ctrl Pts',(-9.30390833655991,-84.4519641217,57.1566590954));
#149580=CARTESIAN_POINT('',(-10.7897586692569,-89.96662969245,61.19644556989));
#149581=CARTESIAN_POINT('Ctrl Pts',(-10.7897586692559,-89.96662969245,61.1964455698903));
#149582=CARTESIAN_POINT('Ctrl Pts',(-10.6961214763189,-89.6639756404415,
60.8929443067986));
#149583=CARTESIAN_POINT('Ctrl Pts',(-10.6017810121018,-89.3511888436508,
60.5999837275916));
#149584=CARTESIAN_POINT('Ctrl Pts',(-10.5074125253993,-89.0282693020777,
60.3174330412154));
#149585=CARTESIAN_POINT('Ctrl Pts',(-10.480907523704,-88.9375718320227,
60.2380738538097));
#149586=CARTESIAN_POINT('Ctrl Pts',(-10.4544000117395,-88.8460750270309,
60.1595357621056));
#149587=CARTESIAN_POINT('Ctrl Pts',(-10.4279042498625,-88.7537788871023,
60.08181564452));
#149588=CARTESIAN_POINT('Ctrl Pts',(-10.367488574311,-88.54332509187,59.9045981170654));
#149589=CARTESIAN_POINT('Ctrl Pts',(-10.3071345456509,-88.3287152994673,
59.7316336299325));
#149590=CARTESIAN_POINT('Ctrl Pts',(-10.2470052765235,-88.1099495098942,
59.562883596963));
#149591=CARTESIAN_POINT('Ctrl Pts',(-10.2169406419597,-88.0005666151076,
59.4785085804783));
#149592=CARTESIAN_POINT('Ctrl Pts',(-10.186932093323,-87.8901447210284,
59.3951872149272));
#149593=CARTESIAN_POINT('Ctrl Pts',(-10.1569992127604,-87.7786838276566,
59.3129144044139));
#149594=CARTESIAN_POINT('Ctrl Pts',(-10.1270663321978,-87.6672229342848,
59.2306415939007));
#149595=CARTESIAN_POINT('Ctrl Pts',(-10.0974532876728,-87.5556544419064,
59.1500751344039));
#149596=CARTESIAN_POINT('Ctrl Pts',(-10.0674467345878,-87.4411841496634,
59.0692366916427));
#149597=CARTESIAN_POINT('Ctrl Pts',(-9.97973503412739,-87.1065777736358,
58.8329390650181));
#149598=CARTESIAN_POINT('Ctrl Pts',(-9.89342048644049,-86.7651177864549,
58.6072399120118));
#149599=CARTESIAN_POINT('Ctrl Pts',(-9.80904654297317,-86.4168041881208,
58.3919743536847));
#149600=CARTESIAN_POINT('Ctrl Pts',(-9.72420583947613,-86.0665637050301,
58.1755179376796));
#149601=CARTESIAN_POINT('Ctrl Pts',(-9.64132724870226,-85.7093935721399,
57.969610592813));
#149602=CARTESIAN_POINT('Ctrl Pts',(-9.56091049367537,-85.3452937894501,
57.7740847762417));
#149603=CARTESIAN_POINT('Ctrl Pts',(-9.50242505129663,-85.0804915495003,
57.6318828946213));
#149604=CARTESIAN_POINT('Ctrl Pts',(-9.44524065669213,-84.8120239738502,
57.4951721601973));
#149605=CARTESIAN_POINT('Ctrl Pts',(-9.38953228746956,-84.5398910625,57.3638893865801));
#149606=CARTESIAN_POINT('Origin',(-15.5675364833292,-89.9666295471007,59.7223902251639));
#149607=CARTESIAN_POINT('Ctrl Pts',(-10.7183277173439,-89.9625444980999,
60.95715572325));
#149608=CARTESIAN_POINT('Ctrl Pts',(-11.1488047984679,-87.96322629393,62.63856744174));
#149609=CARTESIAN_POINT('Ctrl Pts',(-13.154649703826,-86.4190502844,63.414597018712));
#149610=CARTESIAN_POINT('Ctrl Pts',(-15.7319351985739,-86.1031085662201,
62.89663151716));
#149611=CARTESIAN_POINT('Ctrl Pts',(-10.9910678176069,-90.84201858795,61.82247418517));
#149612=CARTESIAN_POINT('Ctrl Pts',(-11.3283473228529,-88.7567304712899,
63.321898809999));
#149613=CARTESIAN_POINT('Ctrl Pts',(-13.2089159040587,-87.13321591558,64.037450008722));
#149614=CARTESIAN_POINT('Ctrl Pts',(-15.7293910876889,-86.75161252055,63.625211302696));
#149615=CARTESIAN_POINT('Ctrl Pts',(-11.2584139392729,-91.59984702702,62.77268895686));
#149616=CARTESIAN_POINT('Ctrl Pts',(-11.5134937823499,-89.46571522909,64.092206053233));
#149617=CARTESIAN_POINT('Ctrl Pts',(-13.2730319217104,-87.78250254908,64.7371138262451));
#149618=CARTESIAN_POINT('Ctrl Pts',(-15.7260859252339,-87.32621487051,64.4100287288261));
#149619=CARTESIAN_POINT('Ctrl Pts',(-11.5024576829099,-92.24121677998,63.808093557901));
#149620=CARTESIAN_POINT('Ctrl Pts',(-11.6902236879807,-90.08258370556,64.959788823145));
#149621=CARTESIAN_POINT('Ctrl Pts',(-13.3403958339825,-88.3579608586,65.529213168241));
#149622=CARTESIAN_POINT('Ctrl Pts',(-15.7224300293869,-87.83109219926,65.264145083567));
#149623=CARTESIAN_POINT('',(-11.4804281687819,-92.,63.72676972225));
#149624=CARTESIAN_POINT('Ctrl Pts',(-11.4804281687818,-92.,63.72676972225));
#149625=CARTESIAN_POINT('Ctrl Pts',(-11.3791659077606,-91.7276039629617,
63.3013371498193));
#149626=CARTESIAN_POINT('Ctrl Pts',(-11.2743320050127,-91.4356124926206,
62.8917472513322));
#149627=CARTESIAN_POINT('Ctrl Pts',(-11.1672746427287,-91.1239902090124,
62.4978437851762));
#149628=CARTESIAN_POINT('Ctrl Pts',(-11.0628000093336,-90.8198857257414,
62.1134431298476));
#149629=CARTESIAN_POINT('Ctrl Pts',(-10.9562080540964,-90.4970861151506,
61.7439811046052));
#149630=CARTESIAN_POINT('Ctrl Pts',(-10.8487288878876,-90.1556011109963,
61.3893000120327));
#149631=CARTESIAN_POINT('Ctrl Pts',(-10.829099340904,-90.0932337130188,
61.3245225354629));
#149632=CARTESIAN_POINT('Ctrl Pts',(-10.8094401338748,-90.030243166608,
61.2602380564391));
#149633=CARTESIAN_POINT('Ctrl Pts',(-10.7897586692573,-89.9666296924501,
61.1964455698899));
#149634=CARTESIAN_POINT('Origin',(-16.3445396385588,-92.0000000217413,62.5690048024171));
#149635=CARTESIAN_POINT('Ctrl Pts',(-15.7267485954679,-87.66539271722,80.98689185542));
#149636=CARTESIAN_POINT('Ctrl Pts',(-15.1845473504709,-87.78122714385,80.916890805709));
#149637=CARTESIAN_POINT('Ctrl Pts',(-14.1051578442959,-88.17294061374,80.871443999723));
#149638=CARTESIAN_POINT('Ctrl Pts',(-12.6905091994459,-89.25086783016,81.140906685209));
#149639=CARTESIAN_POINT('Ctrl Pts',(-11.7187170051615,-90.65190210376,81.710977340828));
#149640=CARTESIAN_POINT('Ctrl Pts',(-11.4633133420439,-91.64600244116,82.225570496093));
#149641=CARTESIAN_POINT('Ctrl Pts',(-11.4262749611389,-92.13114394692,82.498924437511));
#149642=CARTESIAN_POINT('Ctrl Pts',(-15.7173836160999,-88.05182477781,80.364280814309));
#149643=CARTESIAN_POINT('Ctrl Pts',(-15.2062426832829,-88.16375596495,80.330470883294));
#149644=CARTESIAN_POINT('Ctrl Pts',(-14.2055189094499,-88.52846025707,80.340232470926));
#149645=CARTESIAN_POINT('Ctrl Pts',(-12.8992702355175,-89.49997920196,80.607597479859));
#149646=CARTESIAN_POINT('Ctrl Pts',(-11.9627692360111,-90.76949848147,81.092123199415));
#149647=CARTESIAN_POINT('Ctrl Pts',(-11.666429117173,-91.70187736404,81.517563967468));
#149648=CARTESIAN_POINT('Ctrl Pts',(-11.5979936627015,-92.16979066453,81.745905912518));
#149649=CARTESIAN_POINT('Ctrl Pts',(-15.7002372525439,-88.72433818278,79.089598686914));
#149650=CARTESIAN_POINT('Ctrl Pts',(-15.2467375145529,-88.82579237976,79.100193597181));
#149651=CARTESIAN_POINT('Ctrl Pts',(-14.3760944340769,-89.13993303906,79.168545711718));
#149652=CARTESIAN_POINT('Ctrl Pts',(-13.2334233980418,-89.94290089825,79.413180303588));
#149653=CARTESIAN_POINT('Ctrl Pts',(-12.3569948357183,-90.99911727509,79.774927745118));
#149654=CARTESIAN_POINT('Ctrl Pts',(-12.0079449977392,-91.80959370206,80.073791601054));
#149655=CARTESIAN_POINT('Ctrl Pts',(-11.8932536346062,-92.23267061772,80.234650779147));
#149656=CARTESIAN_POINT('Ctrl Pts',(-15.6808989474229,-89.45529670407,77.067422189446));
#149657=CARTESIAN_POINT('Ctrl Pts',(-15.2931912697469,-89.54407975723,77.094016900249));
#149658=CARTESIAN_POINT('Ctrl Pts',(-14.5550845677969,-89.80455656405,77.169706300882));
#149659=CARTESIAN_POINT('Ctrl Pts',(-13.5661328445162,-90.44243352221,77.349989108941));
#149660=CARTESIAN_POINT('Ctrl Pts',(-12.7529608600718,-91.28077188604,77.584104760901));
#149661=CARTESIAN_POINT('Ctrl Pts',(-12.3659618936567,-91.94231099482,77.767814371209));
#149662=CARTESIAN_POINT('Ctrl Pts',(-12.211902366606,-92.29761926682,77.866438532652));
#149663=CARTESIAN_POINT('Ctrl Pts',(-15.6717957676439,-89.80966909398,75.388028487314));
#149664=CARTESIAN_POINT('Ctrl Pts',(-15.3151695191169,-89.89025483975,75.409280511305));
#149665=CARTESIAN_POINT('Ctrl Pts',(-14.6374260128379,-90.12244382554,75.46239351056));
#149666=CARTESIAN_POINT('Ctrl Pts',(-13.7177800254399,-90.68309838254,75.574038621683));
#149667=CARTESIAN_POINT('Ctrl Pts',(-12.9367807162256,-91.42083563943,75.711139278103));
#149668=CARTESIAN_POINT('Ctrl Pts',(-12.538043838553,-92.0102950282,75.815680084024));
#149669=CARTESIAN_POINT('Ctrl Pts',(-12.3689260666087,-92.33083105141,75.871517394051));
#149670=CARTESIAN_POINT('Ctrl Pts',(-15.6681296739329,-89.95257099154,74.024855121973));
#149671=CARTESIAN_POINT('Ctrl Pts',(-15.3240385042369,-90.03019457712,74.034896853418));
#149672=CARTESIAN_POINT('Ctrl Pts',(-14.6702817192719,-90.25160971085,74.059201836835));
#149673=CARTESIAN_POINT('Ctrl Pts',(-13.7779625534719,-90.78190268908,74.10851169455));
#149674=CARTESIAN_POINT('Ctrl Pts',(-13.0100010368838,-91.47919202969,74.168024423489));
#149675=CARTESIAN_POINT('Ctrl Pts',(-12.6072846536751,-92.03865947839,74.213003982407));
#149676=CARTESIAN_POINT('Ctrl Pts',(-12.4326148349899,-92.34428896209,74.236998274081));
#149677=CARTESIAN_POINT('Ctrl Pts',(-15.6672248087549,-89.98827259123,72.9875954719413));
#149678=CARTESIAN_POINT('Ctrl Pts',(-15.3262299348879,-90.06524457197,72.9875820642177));
#149679=CARTESIAN_POINT('Ctrl Pts',(-14.6783497519689,-90.28411903404,72.987550292389));
#149680=CARTESIAN_POINT('Ctrl Pts',(-13.7927252045719,-90.8069898723,72.9874874147133));
#149681=CARTESIAN_POINT('Ctrl Pts',(-13.0280723074446,-91.49419544011,72.987412580105));
#149682=CARTESIAN_POINT('Ctrl Pts',(-12.6245704860005,-92.04598955855,72.9873565731651));
#149683=CARTESIAN_POINT('Ctrl Pts',(-12.4486600227693,-92.34772416774,72.9873268080765));
#149684=CARTESIAN_POINT('Ctrl Pts',(-15.6681350491459,-89.9523609443,71.950180627016));
#149685=CARTESIAN_POINT('Ctrl Pts',(-15.3240254973829,-90.02998927862,71.940116172401));
#149686=CARTESIAN_POINT('Ctrl Pts',(-14.6702336070009,-90.25142080795,71.915752744234));
#149687=CARTESIAN_POINT('Ctrl Pts',(-13.7778744577689,-90.78175855918,71.866316228017));
#149688=CARTESIAN_POINT('Ctrl Pts',(-13.0098937512633,-91.47910696723,71.806645169241));
#149689=CARTESIAN_POINT('Ctrl Pts',(-12.6071830844856,-92.03861806362,71.761543025199));
#149690=CARTESIAN_POINT('Ctrl Pts',(-12.432521388372,-92.34426923603,71.737482735481));
#149691=CARTESIAN_POINT('Ctrl Pts',(-15.6718111921509,-89.80907524214,70.586583011817));
#149692=CARTESIAN_POINT('Ctrl Pts',(-15.3151322403169,-89.8896753559,70.565323380961));
#149693=CARTESIAN_POINT('Ctrl Pts',(-14.6372871557079,-90.12191254573,70.512171532443));
#149694=CARTESIAN_POINT('Ctrl Pts',(-13.7175254777709,-90.68269626992,70.400398310495));
#149695=CARTESIAN_POINT('Ctrl Pts',(-12.9364726797289,-91.42060119049,70.26311038424));
#149696=CARTESIAN_POINT('Ctrl Pts',(-12.5377554772725,-92.01018118362,70.158412233547));
#149697=CARTESIAN_POINT('Ctrl Pts',(-12.3686629807924,-92.33077573351,70.102488458309));
#149698=CARTESIAN_POINT('Ctrl Pts',(-15.6809151702919,-89.45464488429,68.907864632705));
#149699=CARTESIAN_POINT('Ctrl Pts',(-15.2931521975629,-89.54343665812,68.881249937272));
#149700=CARTESIAN_POINT('Ctrl Pts',(-14.5549361924049,-89.80395622407,68.805510076319));
#149701=CARTESIAN_POINT('Ctrl Pts',(-13.5658570449471,-90.44197313346,68.625123720347));
#149702=CARTESIAN_POINT('Ctrl Pts',(-12.7526267697373,-91.28050410382,68.390888386043));
#149703=CARTESIAN_POINT('Ctrl Pts',(-12.3656508008458,-91.94218435098,68.207096911123));
#149704=CARTESIAN_POINT('Ctrl Pts',(-12.2116193557359,-92.29756107263,68.10843240078));
#149705=CARTESIAN_POINT('Ctrl Pts',(-15.7002706718129,-88.7231701863,66.886166124211));
#149706=CARTESIAN_POINT('Ctrl Pts',(-15.2466574582849,-88.82466182876,66.87569843402));
#149707=CARTESIAN_POINT('Ctrl Pts',(-14.3757812509549,-89.13891694147,66.807519820801));
#149708=CARTESIAN_POINT('Ctrl Pts',(-13.2328406129946,-89.94217161044,66.56288459358));
#149709=CARTESIAN_POINT('Ctrl Pts',(-12.3563117520386,-90.99872782708,66.200892463384));
#149710=CARTESIAN_POINT('Ctrl Pts',(-12.0073444264764,-91.80940442047,65.901727738338));
#149711=CARTESIAN_POINT('Ctrl Pts',(-11.8927308025875,-92.23255966739,65.740692166119));
#149712=CARTESIAN_POINT('Ctrl Pts',(-15.7174074004949,-88.05102698964,65.612205998375));
#149713=CARTESIAN_POINT('Ctrl Pts',(-15.2061864647479,-88.16296384459,65.646084060879));
#149714=CARTESIAN_POINT('Ctrl Pts',(-14.2052830448809,-88.52771792363,65.636424008647));
#149715=CARTESIAN_POINT('Ctrl Pts',(-12.8988133538895,-89.49944296408,65.369043826289));
#149716=CARTESIAN_POINT('Ctrl Pts',(-11.9622505755144,-90.76922838303,64.884337945583));
#149717=CARTESIAN_POINT('Ctrl Pts',(-11.6659998956679,-91.70174963819,64.458710962093));
#149718=CARTESIAN_POINT('Ctrl Pts',(-11.5976315022519,-92.16971281076,64.230273662566));
#149719=CARTESIAN_POINT('Ctrl Pts',(-15.7267394992299,-87.66571800126,64.991418639046));
#149720=CARTESIAN_POINT('Ctrl Pts',(-15.1845687552979,-87.78154939555,65.06139114091));
#149721=CARTESIAN_POINT('Ctrl Pts',(-14.1052496752619,-88.17324122689,65.106795438126));
#149722=CARTESIAN_POINT('Ctrl Pts',(-12.6906903787521,-89.25108309904,64.837337670906));
#149723=CARTESIAN_POINT('Ctrl Pts',(-11.7189249564791,-90.65200901472,64.267339208866));
#149724=CARTESIAN_POINT('Ctrl Pts',(-11.4634864352539,-91.64605309874,63.752821353271));
#149725=CARTESIAN_POINT('Ctrl Pts',(-11.4264214263539,-92.13117582295,63.479506114825));
#149726=CARTESIAN_POINT('',(-12.4950500697605,-92.2592915992045,72.9888916301979));
#149727=CARTESIAN_POINT('Ctrl Pts',(-12.4950500697605,-92.2592915992045,
72.9888916301979));
#149728=CARTESIAN_POINT('Ctrl Pts',(-12.4950499645961,-92.2592918029314,
72.6614778940476));
#149729=CARTESIAN_POINT('Ctrl Pts',(-12.491624737793,-92.25830728403,72.3313232059512));
#149730=CARTESIAN_POINT('Ctrl Pts',(-12.4845501034544,-92.2563257071442,
71.9984875391328));
#149731=CARTESIAN_POINT('Ctrl Pts',(-12.4775098513783,-92.2543537605931,
71.6672694319906));
#149732=CARTESIAN_POINT('Ctrl Pts',(-12.4668556073995,-92.2513942171472,
71.3333959665445));
#149733=CARTESIAN_POINT('Ctrl Pts',(-12.4523224890172,-92.2474120640036,
70.9969401667793));
#149734=CARTESIAN_POINT('Ctrl Pts',(-12.4379614328067,-92.2434770568269,
70.6644677733357));
#149735=CARTESIAN_POINT('Ctrl Pts',(-12.4198128355913,-92.2385431083273,
70.3294734603283));
#149736=CARTESIAN_POINT('Ctrl Pts',(-12.3975777779154,-92.2325586333523,
69.9920467993465));
#149737=CARTESIAN_POINT('Ctrl Pts',(-12.384491286254,-92.2290364575613,
69.7934536025296));
#149738=CARTESIAN_POINT('Ctrl Pts',(-12.369988449416,-92.2251500697599,
69.5940182420788));
#149739=CARTESIAN_POINT('Ctrl Pts',(-12.3540010848255,-92.2208870301984,
69.3937629526273));
#149740=CARTESIAN_POINT('Ctrl Pts',(-12.3376237210235,-92.2165199971327,
69.1886225925616));
#149741=CARTESIAN_POINT('Ctrl Pts',(-12.3196885500552,-92.2117576623272,
68.9826217608456));
#149742=CARTESIAN_POINT('Ctrl Pts',(-12.3001162617764,-92.2065859680532,
68.7757882374567));
#149743=CARTESIAN_POINT('Ctrl Pts',(-12.290330117637,-92.2040001209162,
68.6723714757622));
#149744=CARTESIAN_POINT('Ctrl Pts',(-12.2801346070993,-92.2013118947475,
68.5687465506039));
#149745=CARTESIAN_POINT('Ctrl Pts',(-12.2695192254143,-92.198519576097,
68.4649174124185));
#149746=CARTESIAN_POINT('Ctrl Pts',(-12.2642115345717,-92.1971234167717,
68.4130028433258));
#149747=CARTESIAN_POINT('Ctrl Pts',(-12.2587988707683,-92.1957012318768,
68.3610372214912));
#149748=CARTESIAN_POINT('Ctrl Pts',(-12.253279885861,-92.1942528057138,
68.3090210593462));
#149749=CARTESIAN_POINT('Ctrl Pts',(-12.2505203934074,-92.1935285926323,
68.2830129782737));
#149750=CARTESIAN_POINT('Ctrl Pts',(-12.247734320347,-92.1927978190947,
68.2569922621632));
#149751=CARTESIAN_POINT('Ctrl Pts',(-12.2449214958836,-92.1920604584762,
68.2309589769342));
#149752=CARTESIAN_POINT('Ctrl Pts',(-12.2421086714201,-92.1913230978577,
68.2049256917052));
#149753=CARTESIAN_POINT('Ctrl Pts',(-12.2390463837868,-92.1905208353914,
68.1768552411708));
#149754=CARTESIAN_POINT('Ctrl Pts',(-12.2364025960719,-92.1898285886005,
68.1528214804896));
#149755=CARTESIAN_POINT('Ctrl Pts',(-12.1941019926332,-92.1787526399455,
67.7682813095912));
#149756=CARTESIAN_POINT('Ctrl Pts',(-12.1466029853855,-92.1665260937355,
67.3874265867434));
#149757=CARTESIAN_POINT('Ctrl Pts',(-12.0939475661605,-92.1531019687639,
67.0104245935852));
#149758=CARTESIAN_POINT('Ctrl Pts',(-12.044461672975,-92.1404858919339,
66.6561157562667));
#149759=CARTESIAN_POINT('Ctrl Pts',(-11.990420891063,-92.1268113856426,
66.305209676447));
#149760=CARTESIAN_POINT('Ctrl Pts',(-11.9318247232044,-92.1120654825007,
65.9578628232496));
#149761=CARTESIAN_POINT('Ctrl Pts',(-11.8750461046509,-92.0977769711471,
65.6212900540016));
#149762=CARTESIAN_POINT('Ctrl Pts',(-11.8139898351115,-92.0824817906833,
65.2880590602539));
#149763=CARTESIAN_POINT('Ctrl Pts',(-11.7486284014674,-92.0662034766387,
64.9583306855135));
#149764=CARTESIAN_POINT('Ctrl Pts',(-11.6860810945097,-92.0506260229549,
64.642798716312));
#149765=CARTESIAN_POINT('Ctrl Pts',(-11.619590763227,-92.0341477884734,
64.330474329946));
#149766=CARTESIAN_POINT('Ctrl Pts',(-11.5491159559696,-92.0168306342924,
64.0215155315664));
#149767=CARTESIAN_POINT('Ctrl Pts',(-11.5266264088242,-92.0113044757893,
63.9229222365642));
#149768=CARTESIAN_POINT('Ctrl Pts',(-11.5037310060279,-92.0056932411832,
63.8246718023983));
#149769=CARTESIAN_POINT('Ctrl Pts',(-11.4804281687818,-92.,63.72676972225));
#149770=CARTESIAN_POINT('Ctrl Pts',(-11.4804394788205,-91.9999117027221,
82.2509615003081));
#149771=CARTESIAN_POINT('Ctrl Pts',(-11.5530700737656,-92.0176752428972,
81.9458308790911));
#149772=CARTESIAN_POINT('Ctrl Pts',(-11.6217432522474,-92.0346347091691,
81.6373099655569));
#149773=CARTESIAN_POINT('Ctrl Pts',(-11.6865041851513,-92.0507147503459,
81.3255602912215));
#149774=CARTESIAN_POINT('Ctrl Pts',(-11.7540919465117,-92.0674966887306,
81.000202677482));
#149775=CARTESIAN_POINT('Ctrl Pts',(-11.8174191484055,-92.0833212628977,
80.6713283984278));
#149776=CARTESIAN_POINT('Ctrl Pts',(-11.8765199305579,-92.0981530040061,
80.3391017829893));
#149777=CARTESIAN_POINT('Ctrl Pts',(-11.8914927191536,-92.1019105265977,
80.2549343879455));
#149778=CARTESIAN_POINT('Ctrl Pts',(-11.9061941332142,-92.1056045451107,
80.1705517335308));
#149779=CARTESIAN_POINT('Ctrl Pts',(-11.9206244884779,-92.109234899873,
80.0859562980525));
#149780=CARTESIAN_POINT('Ctrl Pts',(-11.980343758288,-92.1242589330027,
79.7358625170093));
#149781=CARTESIAN_POINT('Ctrl Pts',(-12.0354233298406,-92.1381898452128,
79.3821260864904));
#149782=CARTESIAN_POINT('Ctrl Pts',(-12.0858651976485,-92.1510401785318,
79.024909586593));
#149783=CARTESIAN_POINT('Ctrl Pts',(-12.0886225005406,-92.1517426160656,
79.0053830676297));
#149784=CARTESIAN_POINT('Ctrl Pts',(-12.0913659372046,-92.1524418329199,
78.9858461451773));
#149785=CARTESIAN_POINT('Ctrl Pts',(-12.0940955049538,-92.153137833817,
78.9662988441322));
#149786=CARTESIAN_POINT('Ctrl Pts',(-12.1204275305434,-92.1598521252785,
78.7777268508298));
#149787=CARTESIAN_POINT('Ctrl Pts',(-12.1454690953703,-92.1662669790196,
78.5881890941633));
#149788=CARTESIAN_POINT('Ctrl Pts',(-12.1692162275469,-92.1723876925774,
78.3977071808957));
#149789=CARTESIAN_POINT('Ctrl Pts',(-12.1810897936351,-92.1754480493563,
78.3024662242619));
#149790=CARTESIAN_POINT('Ctrl Pts',(-12.1926397203039,-92.1784348592657,
78.2069892242869));
#149791=CARTESIAN_POINT('Ctrl Pts',(-12.2038652288885,-92.1813489786785,
78.1112787478959));
#149792=CARTESIAN_POINT('Ctrl Pts',(-12.2094779831807,-92.182806038385,
78.0634235097003));
#149793=CARTESIAN_POINT('Ctrl Pts',(-12.2150096307703,-92.1842449246855,
78.0155099020937));
#149794=CARTESIAN_POINT('Ctrl Pts',(-12.2204600597818,-92.1856657446596,
77.9675382424531));
#149795=CARTESIAN_POINT('Ctrl Pts',(-12.2231852742876,-92.1863761546466,
77.9435524126328));
#149796=CARTESIAN_POINT('Ctrl Pts',(-12.2258901840184,-92.187082047999,
77.9195520697877));
#149797=CARTESIAN_POINT('Ctrl Pts',(-12.2285747738969,-92.1877834386385,
77.8955372531514));
#149798=CARTESIAN_POINT('Ctrl Pts',(-12.2312593637755,-92.188484829278,
77.8715224365152));
#149799=CARTESIAN_POINT('Ctrl Pts',(-12.2337037293511,-92.1891241280636,
77.84949293961));
#149800=CARTESIAN_POINT('Ctrl Pts',(-12.236567568283,-92.189874116359,77.8234494209454));
#149801=CARTESIAN_POINT('Ctrl Pts',(-12.2736228920444,-92.1995782441962,
77.4864713160506));
#149802=CARTESIAN_POINT('Ctrl Pts',(-12.3061816785662,-92.208175820577,
77.1515711996581));
#149803=CARTESIAN_POINT('Ctrl Pts',(-12.3345957999658,-92.2157260680699,
76.8188790499968));
#149804=CARTESIAN_POINT('Ctrl Pts',(-12.363731878687,-92.2234681552605,
76.4777337255931));
#149805=CARTESIAN_POINT('Ctrl Pts',(-12.3885100948304,-92.2301097342852,
76.1389096533919));
#149806=CARTESIAN_POINT('Ctrl Pts',(-12.409264189783,-92.2357117772265,
75.8025164120411));
#149807=CARTESIAN_POINT('Ctrl Pts',(-12.4301989546193,-92.2413625874327,
75.4631947785863));
#149808=CARTESIAN_POINT('Ctrl Pts',(-12.4470391638925,-92.2459562388365,
75.1263460665604));
#149809=CARTESIAN_POINT('Ctrl Pts',(-12.4600815069596,-92.2495426758459,
74.7920579531015));
#149810=CARTESIAN_POINT('Ctrl Pts',(-12.4732389077876,-92.2531607519104,
74.4548207957765));
#149811=CARTESIAN_POINT('Ctrl Pts',(-12.4825310889809,-92.2557541419737,
74.1201892216622));
#149812=CARTESIAN_POINT('Ctrl Pts',(-12.4882171413017,-92.2573542389111,
73.7882342603867));
#149813=CARTESIAN_POINT('Ctrl Pts',(-12.4928112169424,-92.2586470455806,
73.5200295173804));
#149814=CARTESIAN_POINT('Ctrl Pts',(-12.4950503743449,-92.2592910724911,
73.2535716056014));
#149815=CARTESIAN_POINT('Ctrl Pts',(-12.4950500697605,-92.2592915992045,
72.9888916301979));
#149816=CARTESIAN_POINT('Origin',(27.4324635166691,-92.,72.98888938658));
#149817=CARTESIAN_POINT('',(-9.38953228746991,-92.,57.36388938658));
#149818=CARTESIAN_POINT('Origin',(27.4324635166691,-92.,72.98888938658));
#149819=CARTESIAN_POINT('',(-8.92925733991791,-92.5,57.55920188658));
#149820=CARTESIAN_POINT('Origin',(-8.92925733991791,-92.,57.55920188658));
#149821=CARTESIAN_POINT('',(-8.92925733991791,-92.5,88.41857688658));
#149822=CARTESIAN_POINT('Origin',(27.4324635166691,-92.5,72.98888938658));
#149823=CARTESIAN_POINT('',(-9.38953228746991,-92.,88.61388938658));
#149824=CARTESIAN_POINT('Origin',(-8.92925733991791,-92.,88.41857688658));
#149825=CARTESIAN_POINT('Origin',(27.4324635166691,-92.,72.98888938658));
#149826=CARTESIAN_POINT('Origin',(27.4324635166691,25.,72.98888938658));
#149827=CARTESIAN_POINT('',(-9.38953228746991,-84.5398910625,88.61388938658));
#149828=CARTESIAN_POINT('Origin',(-2.02513312664091,-92.5,85.48888938658));
#149829=CARTESIAN_POINT('',(-9.38953228746991,84.5398910625,88.61388938658));
#149830=CARTESIAN_POINT('Ctrl Pts',(-9.38953228746991,84.5398910625,88.61388938658));
#149831=CARTESIAN_POINT('Ctrl Pts',(-9.28328709694071,83.7902390287746,
88.8642676240091));
#149832=CARTESIAN_POINT('Ctrl Pts',(-9.17708486962772,83.034411628292,89.079525122487));
#149833=CARTESIAN_POINT('Ctrl Pts',(-9.03022807503691,81.8914074774324,
89.3540432573144));
#149834=CARTESIAN_POINT('Ctrl Pts',(-8.9833075439401,81.5088622521231,89.4374960492821));
#149835=CARTESIAN_POINT('Ctrl Pts',(-8.91715535504234,80.9327286516253,
89.5511487397963));
#149836=CARTESIAN_POINT('Ctrl Pts',(-8.88513273747567,80.6440829107429,
89.6050931418994));
#149837=CARTESIAN_POINT('Ctrl Pts',(-8.84983719739325,80.3063164002716,
89.6630999929703));
#149838=CARTESIAN_POINT('Ctrl Pts',(-8.83273032606334,80.1371798585086,
89.6908850775441));
#149839=CARTESIAN_POINT('Ctrl Pts',(-8.82551731869513,80.0646384934973,
89.7025333452805));
#149840=CARTESIAN_POINT('Ctrl Pts',(-8.82073526432699,80.0162655222266,
89.71024132127));
#149841=CARTESIAN_POINT('Ctrl Pts',(-8.81853574016787,79.9938968401075,
89.7137803985326));
#149842=CARTESIAN_POINT('Ctrl Pts',(-8.73463441113909,79.1351582655722,
89.8485086409054));
#149843=CARTESIAN_POINT('Ctrl Pts',(-8.6700376843763,78.3063013527105,89.9443580231836));
#149844=CARTESIAN_POINT('Ctrl Pts',(-8.60463652245047,77.0688049043587,
90.039891957753));
#149845=CARTESIAN_POINT('Ctrl Pts',(-8.58803785671456,76.6572709083983,
90.0636744407943));
#149846=CARTESIAN_POINT('Ctrl Pts',(-8.57132975194452,76.0414171446928,
90.0875200458018));
#149847=CARTESIAN_POINT('Ctrl Pts',(-8.56712264234551,75.8363737618302,
90.093495481281));
#149848=CARTESIAN_POINT('Ctrl Pts',(-8.56146522762828,75.4267694061832,
90.101522775063));
#149849=CARTESIAN_POINT('Ctrl Pts',(-8.56001530984225,75.2234148157065,
90.1035740849179));
#149850=CARTESIAN_POINT('Ctrl Pts',(-8.5596814837813,74.195784065444,90.1040468034545));
#149851=CARTESIAN_POINT('Ctrl Pts',(-8.58177592616642,73.3716955238175,
90.0732381391729));
#149852=CARTESIAN_POINT('Ctrl Pts',(-8.64644160601741,72.132586799253,89.9788480269718));
#149853=CARTESIAN_POINT('Ctrl Pts',(-8.67320843583488,71.7190545723774,
89.9393254017685));
#149854=CARTESIAN_POINT('Ctrl Pts',(-8.72052840036103,71.0980122540328,
89.8675311439228));
#149855=CARTESIAN_POINT('Ctrl Pts',(-8.74597657546552,70.7873051003526,
89.8285040402397));
#149856=CARTESIAN_POINT('Ctrl Pts',(-8.77860779189372,70.4244879306706,
89.777379489179));
#149857=CARTESIAN_POINT('Ctrl Pts',(-8.7956318183485,70.2429979732323,89.7504030045292));
#149858=CARTESIAN_POINT('Ctrl Pts',(-8.80307665120833,70.1651991259165,
89.7385368699021));
#149859=CARTESIAN_POINT('Ctrl Pts',(-8.80807260339705,70.1133293528205,
89.7305581866391));
#149860=CARTESIAN_POINT('Ctrl Pts',(-8.81073338330673,70.0858914918537,
89.726300088025));
#149861=CARTESIAN_POINT('Ctrl Pts',(-8.96569959907365,68.4974394021023,
89.4778327794232));
#149862=CARTESIAN_POINT('Ctrl Pts',(-9.17644065970042,66.963657792137,89.116062764089));
#149863=CARTESIAN_POINT('Ctrl Pts',(-9.38953228746991,65.4601089375,88.61388938658));
#149864=CARTESIAN_POINT('',(1.23275780153909,-92.,92.79547180931));
#149865=CARTESIAN_POINT('Origin',(-2.02513312664091,-92.,85.48888938658));
#149866=CARTESIAN_POINT('',(1.23275780153909,-24.69194692623,92.79547180931));
#149867=CARTESIAN_POINT('',(1.23275780153909,-24.69194692623,92.79547180931));
#149868=CARTESIAN_POINT('',(1.23275780153909,24.69194692623,92.79547180931));
#149869=CARTESIAN_POINT('Ctrl Pts',(1.23275780153909,-24.69194692623,92.79547180931));
#149870=CARTESIAN_POINT('Ctrl Pts',(0.699306919210318,-24.1238270516451,
93.033329221926));
#149871=CARTESIAN_POINT('Ctrl Pts',(0.153641228329698,-23.4653479951291,
93.2064179486881));
#149872=CARTESIAN_POINT('Ctrl Pts',(-0.660308888464234,-22.3420906374582,
93.3764797028993));
#149873=CARTESIAN_POINT('Ctrl Pts',(-0.93091665494534,-21.9450817227518,
93.4182936546966));
#149874=CARTESIAN_POINT('Ctrl Pts',(-1.33337035782043,-21.315683657468,
93.4600658810012));
#149875=CARTESIAN_POINT('Ctrl Pts',(-1.46694860399934,-21.1002368535027,
93.4705009261982));
#149876=CARTESIAN_POINT('Ctrl Pts',(-1.66618741489872,-20.7685954742487,
93.4811094260117));
#149877=CARTESIAN_POINT('Ctrl Pts',(-1.76552499736201,-20.6006569912952,
93.4851528403169));
#149878=CARTESIAN_POINT('Ctrl Pts',(-1.88087013739072,-20.4010226228614,
93.4877069287156));
#149879=CARTESIAN_POINT('Ctrl Pts',(-1.93839884063816,-20.3002789040641,
93.4884486918558));
#149880=CARTESIAN_POINT('Ctrl Pts',(-1.96302245967253,-20.2569044814552,
93.4886524817677));
#149881=CARTESIAN_POINT('Ctrl Pts',(-1.97943111860132,-20.2279440790216,
93.4887630506161));
#149882=CARTESIAN_POINT('Ctrl Pts',(-1.98827002315454,-20.21231115855,93.4888080269244));
#149883=CARTESIAN_POINT('Ctrl Pts',(-2.4796105271812,-19.3417230633289,
93.4906078204203));
#149884=CARTESIAN_POINT('Ctrl Pts',(-2.94214572836347,-18.4235503155145,
93.4484191451384));
#149885=CARTESIAN_POINT('Ctrl Pts',(-3.59503988466488,-16.9548237203979,
93.336446286239));
#149886=CARTESIAN_POINT('Ctrl Pts',(-3.80591399159718,-16.4500036097931,
93.2910065179068));
#149887=CARTESIAN_POINT('Ctrl Pts',(-4.11145661580154,-15.6699065755372,
93.2127684219845));
#149888=CARTESIAN_POINT('Ctrl Pts',(-4.26154056320608,-15.2741413413221,
93.1711286684841));
#149889=CARTESIAN_POINT('Ctrl Pts',(-4.43184466783831,-14.8024109798352,
93.1185820511613));
#149890=CARTESIAN_POINT('Ctrl Pts',(-4.50379795258712,-14.5980970560045,
93.095258574056));
#149891=CARTESIAN_POINT('Ctrl Pts',(-4.55153628454621,-14.4614113803602,
93.0795361718871));
#149892=CARTESIAN_POINT('Ctrl Pts',(-4.5747411202905,-14.3944288506155,
93.0717748303771));
#149893=CARTESIAN_POINT('Ctrl Pts',(-4.98592652946738,-13.1973273465102,
92.932058176407));
#149894=CARTESIAN_POINT('Ctrl Pts',(-5.3198620500585,-12.0688920126009,
92.7858901900897));
#149895=CARTESIAN_POINT('Ctrl Pts',(-5.74715455760815,-10.3736116637277,
92.5721034394466));
#149896=CARTESIAN_POINT('Ctrl Pts',(-5.8773686152273,-9.80808032276836,
92.5016614623134));
#149897=CARTESIAN_POINT('Ctrl Pts',(-6.05539233988914,-8.95912647432705,
92.3998721882845));
#149898=CARTESIAN_POINT('Ctrl Pts',(-6.11185164605444,-8.67603238534623,
92.3665827064308));
#149899=CARTESIAN_POINT('Ctrl Pts',(-6.19235016148506,-8.2512270426244,
92.3178926520071));
#149900=CARTESIAN_POINT('Ctrl Pts',(-6.23155181248203,-8.03878331895086,
92.2938581923587));
#149901=CARTESIAN_POINT('Ctrl Pts',(-6.27548255450619,-7.79086046645125,
92.2664186269981));
#149902=CARTESIAN_POINT('Ctrl Pts',(-6.29853734869913,-7.65802540934062,
92.2518870126521));
#149903=CARTESIAN_POINT('Ctrl Pts',(-6.30916623139605,-7.59603047757618,
92.245152345545));
#149904=CARTESIAN_POINT('Ctrl Pts',(-6.31520813159063,-7.56060351939743,
92.2413155915439));
#149905=CARTESIAN_POINT('Ctrl Pts',(-6.31649962626153,-7.5530196494862,
92.2404949532742));
#149906=CARTESIAN_POINT('Ctrl Pts',(-6.53857587101954,-6.24625869247446,
92.0992622520935));
#149907=CARTESIAN_POINT('Ctrl Pts',(-6.69735300861218,-4.97029942653783,
91.9840774441894));
#149908=CARTESIAN_POINT('Ctrl Pts',(-6.90717880053878,-2.45972441701621,
91.8278748390932));
#149909=CARTESIAN_POINT('Ctrl Pts',(-6.95835699251618,-1.2259449036321,
91.7867701797679));
#149910=CARTESIAN_POINT('Ctrl Pts',(-6.95905409394932,1.2036155215881,91.7862240675702));
#149911=CARTESIAN_POINT('Ctrl Pts',(-6.9084204097403,2.43929636195716,91.8269083023811));
#149912=CARTESIAN_POINT('Ctrl Pts',(-6.75167133250576,4.32416856414915,
91.9436613581591));
#149913=CARTESIAN_POINT('Ctrl Pts',(-6.68586311304225,4.9576844551529,91.9917478371863));
#149914=CARTESIAN_POINT('Ctrl Pts',(-6.56554449137394,5.91579602706811,
92.0757746632258));
#149915=CARTESIAN_POINT('Ctrl Pts',(-6.52183275150553,6.23647284027476,
92.1057581128436));
#149916=CARTESIAN_POINT('Ctrl Pts',(-6.45066355615867,6.71944749393717,
92.1533845086149));
#149917=CARTESIAN_POINT('Ctrl Pts',(-6.41367824672563,6.96142467923148,
92.1778596656006));
#149918=CARTESIAN_POINT('Ctrl Pts',(-6.36803224803482,7.2445886477186,92.2074953644351));
#149919=CARTESIAN_POINT('Ctrl Pts',(-6.34457929391623,7.38638494503977,
92.2225732149781));
#149920=CARTESIAN_POINT('Ctrl Pts',(-6.33269459525855,7.45733667196975,
92.2301758281113));
#149921=CARTESIAN_POINT('Ctrl Pts',(-6.32756716935408,7.48775603599745,
92.2334475955992));
#149922=CARTESIAN_POINT('Ctrl Pts',(-6.32414132469903,7.50803816336209,
92.2356317589976));
#149923=CARTESIAN_POINT('Ctrl Pts',(-6.32220703604282,7.51946334166994,
92.2368638227256));
#149924=CARTESIAN_POINT('Ctrl Pts',(-6.12833274488395,8.66250345548086,
92.3602612590921));
#149925=CARTESIAN_POINT('Ctrl Pts',(-5.89275515319288,9.79454916349254,
92.4990711709164));
#149926=CARTESIAN_POINT('Ctrl Pts',(-5.46622706734526,11.4894172809252,
92.7127498288003));
#149927=CARTESIAN_POINT('Ctrl Pts',(-5.31185728563353,12.0538399126387,
92.7848056604388));
#149928=CARTESIAN_POINT('Ctrl Pts',(-5.06112989749341,12.8996737490626,
92.8909810572153));
#149929=CARTESIAN_POINT('Ctrl Pts',(-4.9743606690004,13.1814850093462,92.9260492732788));
#149930=CARTESIAN_POINT('Ctrl Pts',(-4.83933084495306,13.6040018719851,
92.9777219906298));
#149931=CARTESIAN_POINT('Ctrl Pts',(-4.77059724301506,13.8152102963579,
93.0033254222042));
#149932=CARTESIAN_POINT('Ctrl Pts',(-4.70002259590991,14.0263437103108,
93.0284914261226));
#149933=CARTESIAN_POINT('Ctrl Pts',(-4.65256250400756,14.1670826506304,
93.0451614472216));
#149934=CARTESIAN_POINT('Ctrl Pts',(-4.62813328271855,14.238883430196,93.0536110760009));
#149935=CARTESIAN_POINT('Ctrl Pts',(-4.22613512108353,15.4104071039695,
93.1905351366738));
#149936=CARTESIAN_POINT('Ctrl Pts',(-3.81812010120504,16.4516269765654,
93.2978637470464));
#149937=CARTESIAN_POINT('Ctrl Pts',(-3.16554630125634,17.9213708196141,
93.4102641728471));
#149938=CARTESIAN_POINT('Ctrl Pts',(-2.94130847507913,18.3959377729894,
93.4396164690059));
#149939=CARTESIAN_POINT('Ctrl Pts',(-2.59583390833896,19.0847667115912,
93.4693442746077));
#149940=CARTESIAN_POINT('Ctrl Pts',(-2.47915954494509,19.3105394425483,
93.4768697171106));
#149941=CARTESIAN_POINT('Ctrl Pts',(-2.30202538350384,19.6434431661185,
93.48431452321));
#149942=CARTESIAN_POINT('Ctrl Pts',(-2.21292800063565,19.8084561846873,
93.4870760871862));
#149943=CARTESIAN_POINT('Ctrl Pts',(-2.10808999070051,19.998453397389,93.4885580276519));
#149944=CARTESIAN_POINT('Ctrl Pts',(-2.05545313008902,20.0928225098327,
93.4888567453215));
#149945=CARTESIAN_POINT('Ctrl Pts',(-2.03284832541677,20.1331315236142,
93.4888892195676));
#149946=CARTESIAN_POINT('Ctrl Pts',(-2.01776826009236,20.1599742235681,
93.4888895497571));
#149947=CARTESIAN_POINT('Ctrl Pts',(-2.01088755578811,20.1722021291677,
93.4888809205938));
#149948=CARTESIAN_POINT('Ctrl Pts',(-1.47693698316475,21.1192411119197,
93.487381835435));
#149949=CARTESIAN_POINT('Ctrl Pts',(-0.936180877114922,21.960906935257,
93.4338723147665));
#149950=CARTESIAN_POINT('Ctrl Pts',(0.151417256604318,23.4626319241098,
93.2071274730942));
#149951=CARTESIAN_POINT('Ctrl Pts',(0.698240340815898,24.1226910896253,
93.0338047925655));
#149952=CARTESIAN_POINT('Ctrl Pts',(1.23275780153909,24.69194692623,92.79547180931));
#149953=CARTESIAN_POINT('',(1.23275780153909,92.,92.79547180931));
#149954=CARTESIAN_POINT('',(1.23275780153909,92.,92.79547180931));
#149955=CARTESIAN_POINT('',(-9.38953228746991,92.,88.61388938658));
#149956=CARTESIAN_POINT('Origin',(-2.02513312664091,92.,85.48888938658));
#149957=CARTESIAN_POINT('',(-9.38953228746991,92.,88.61388938658));
#149958=CARTESIAN_POINT('Origin',(27.4324635166691,25.,72.98888938658));
#149959=CARTESIAN_POINT('',(-11.4804281687819,92.,82.25100905091));
#149960=CARTESIAN_POINT('',(-10.7897586692519,89.96662969243,84.78133320328));
#149961=CARTESIAN_POINT('Ctrl Pts',(-11.4804281687818,92.,82.25100905091));
#149962=CARTESIAN_POINT('Ctrl Pts',(-11.3989064198707,91.7807060486943,
82.5935059199151));
#149963=CARTESIAN_POINT('Ctrl Pts',(-11.3150515968862,91.5487028907016,
82.9257444363946));
#149964=CARTESIAN_POINT('Ctrl Pts',(-11.2295974501764,91.3039859861016,
83.2477899999947));
#149965=CARTESIAN_POINT('Ctrl Pts',(-11.1430417623464,91.0561145741593,
83.5739868709863));
#149966=CARTESIAN_POINT('Ctrl Pts',(-11.0548453666189,90.7951995316041,
83.8897266165751));
#149967=CARTESIAN_POINT('Ctrl Pts',(-10.9657236454974,90.5212361406782,
84.1951029602733));
#149968=CARTESIAN_POINT('Ctrl Pts',(-10.9074027231312,90.3419555180385,
84.3949401022091));
#149969=CARTESIAN_POINT('Ctrl Pts',(-10.8486845747637,90.1570871426494,
84.5903397936053));
#149970=CARTESIAN_POINT('Ctrl Pts',(-10.7897586692526,89.96662969243,84.7813332032802));
#149971=CARTESIAN_POINT('Ctrl Pts',(-10.7897586692519,89.96662969243,84.78133320328));
#149972=CARTESIAN_POINT('Ctrl Pts',(-10.6704705500044,89.5814629807082,
85.1679754522423));
#149973=CARTESIAN_POINT('Ctrl Pts',(-10.5499815065516,89.1792964266136,
85.5377153276576));
#149974=CARTESIAN_POINT('Ctrl Pts',(-10.3694940364216,88.5505468319125,
86.0673753755885));
#149975=CARTESIAN_POINT('Ctrl Pts',(-10.2793088439709,88.229797093672,86.3259690138416));
#149976=CARTESIAN_POINT('Ctrl Pts',(-10.1895685665396,87.899484944097,86.5752917864897));
#149977=CARTESIAN_POINT('Ctrl Pts',(-10.1298784240562,87.6771518640837,
86.7394565083492));
#149978=CARTESIAN_POINT('Ctrl Pts',(-10.1003990762871,87.5660572424311,
86.8197121966598));
#149979=CARTESIAN_POINT('Ctrl Pts',(-9.83051731905192,86.5362238831801,
87.5472559457811));
#149980=CARTESIAN_POINT('Ctrl Pts',(-9.60025783789904,85.5656437994716,
88.1172919252206));
#149981=CARTESIAN_POINT('Ctrl Pts',(-9.38953228746991,84.5398910625,88.61388938658));
#149982=CARTESIAN_POINT('Origin',(27.4324635166691,92.,72.98888938658));
#149983=CARTESIAN_POINT('Origin',(27.4324635166691,92.,72.98888938658));
#149984=CARTESIAN_POINT('',(-11.4804365249865,91.9999348338944,63.7268048139011));
#149985=CARTESIAN_POINT('',(-12.4950500697606,92.2592915992044,72.9888871429622));
#149986=CARTESIAN_POINT('Ctrl Pts',(-11.4804394788206,91.9999117027221,
63.7268172728519));
#149987=CARTESIAN_POINT('Ctrl Pts',(-11.5530700739286,92.0176752429416,
64.031947894754));
#149988=CARTESIAN_POINT('Ctrl Pts',(-11.6217432526045,92.0346347092598,
64.3404688091952));
#149989=CARTESIAN_POINT('Ctrl Pts',(-11.6865041857173,92.0507147504843,
64.652218484662));
#149990=CARTESIAN_POINT('Ctrl Pts',(-11.7540919472641,92.0674966889109,
64.9775760994306));
#149991=CARTESIAN_POINT('Ctrl Pts',(-11.8174191493645,92.0833212631222,
65.3064503797548));
#149992=CARTESIAN_POINT('Ctrl Pts',(-11.8765199317249,92.0981530042764,
65.6386769967062));
#149993=CARTESIAN_POINT('Ctrl Pts',(-11.8914927197326,92.1019105267189,
65.7228443885322));
#149994=CARTESIAN_POINT('Ctrl Pts',(-11.9061941332286,92.1056045450884,
65.8072270397262));
#149995=CARTESIAN_POINT('Ctrl Pts',(-11.9206244879506,92.1092348997126,
65.8918224719814));
#149996=CARTESIAN_POINT('Ctrl Pts',(-11.9803437580264,92.1242589329019,
66.241916254385));
#149997=CARTESIAN_POINT('Ctrl Pts',(-12.035423329848,92.1381898451751,66.5956526865277));
#149998=CARTESIAN_POINT('Ctrl Pts',(-12.0858651979061,92.1510401785601,
66.952869188313));
#149999=CARTESIAN_POINT('Ctrl Pts',(-12.0886225006044,92.1517426160446,
66.9723957059099));
#150000=CARTESIAN_POINT('Ctrl Pts',(-12.0913659370766,92.1524418328501,
66.991932626995));
#150001=CARTESIAN_POINT('Ctrl Pts',(-12.094095504636,92.1531378336989,67.0114799266722));
#150002=CARTESIAN_POINT('Ctrl Pts',(-12.1204275302738,92.1598521251739,
67.2000519202346));
#150003=CARTESIAN_POINT('Ctrl Pts',(-12.1454690951536,92.1662669789315,
67.3895896772274));
#150004=CARTESIAN_POINT('Ctrl Pts',(-12.1692162273843,92.1723876925088,
67.5800715908876));
#150005=CARTESIAN_POINT('Ctrl Pts',(-12.1810897934996,92.1754480492974,
67.6753125477177));
#150006=CARTESIAN_POINT('Ctrl Pts',(-12.1926397201958,92.1784348592172,
67.7707895479056));
#150007=CARTESIAN_POINT('Ctrl Pts',(-12.2038652288077,92.1813489786412,
67.8665000245261));
#150008=CARTESIAN_POINT('Ctrl Pts',(-12.2094779831137,92.1828060383532,
67.9143552628363));
#150009=CARTESIAN_POINT('Ctrl Pts',(-12.2150096307169,92.1842449246595,
67.9622688705619));
#150010=CARTESIAN_POINT('Ctrl Pts',(-12.220460059742,92.1856657446395,68.0102405303256));
#150011=CARTESIAN_POINT('Ctrl Pts',(-12.2231852742546,92.1863761546295,
68.0342263602074));
#150012=CARTESIAN_POINT('Ctrl Pts',(-12.2258901839921,92.187082047985,68.058226703115));
#150013=CARTESIAN_POINT('Ctrl Pts',(-12.2285747738774,92.1877834386275,
68.0822415198149));
#150014=CARTESIAN_POINT('Ctrl Pts',(-12.2312593637628,92.18848482927,68.1062563365148));
#150015=CARTESIAN_POINT('Ctrl Pts',(-12.2337037293575,92.1891241280619,
68.1282858335971));
#150016=CARTESIAN_POINT('Ctrl Pts',(-12.2365675682838,92.1898741163572,
68.1543293522149));
#150017=CARTESIAN_POINT('Ctrl Pts',(-12.2736228920578,92.1995782442172,
68.4913074572907));
#150018=CARTESIAN_POINT('Ctrl Pts',(-12.3061816786017,92.2081758206156,
68.8262075739754));
#150019=CARTESIAN_POINT('Ctrl Pts',(-12.3345958000255,92.2157260681214,
69.1588997240404));
#150020=CARTESIAN_POINT('Ctrl Pts',(-12.3637318787694,92.2234681553245,
69.5000450488309));
#150021=CARTESIAN_POINT('Ctrl Pts',(-12.3885100949383,92.2301097343569,
69.8388691215366));
#150022=CARTESIAN_POINT('Ctrl Pts',(-12.4092641899117,92.2357117773015,
70.1752623635098));
#150023=CARTESIAN_POINT('Ctrl Pts',(-12.4301989547663,92.2413625875103,
70.5145839975501));
#150024=CARTESIAN_POINT('Ctrl Pts',(-12.4470391640537,92.2459562389126,
70.8514327102822));
#150025=CARTESIAN_POINT('Ctrl Pts',(-12.4600815071228,92.2495426759163,
71.185720824568));
#150026=CARTESIAN_POINT('Ctrl Pts',(-12.4732389079497,92.2531607519744,
71.5229579826459));
#150027=CARTESIAN_POINT('Ctrl Pts',(-12.4825310891311,92.2557541420275,
71.8575895576373));
#150028=CARTESIAN_POINT('Ctrl Pts',(-12.4882171414205,92.2573542389513,
72.1895445199136));
#150029=CARTESIAN_POINT('Ctrl Pts',(-12.4928112169792,92.2586470455938,
72.4577492604156));
#150030=CARTESIAN_POINT('Ctrl Pts',(-12.495050374345,92.2592910724909,72.7242071698142));
#150031=CARTESIAN_POINT('Ctrl Pts',(-12.4950500697606,92.2592915992044,
72.9888871429622));
#150032=CARTESIAN_POINT('Ctrl Pts',(-12.4950500697606,92.2592915992044,
72.9888871429622));
#150033=CARTESIAN_POINT('Ctrl Pts',(-12.4950499645961,92.2592918029315,
73.3163008749631));
#150034=CARTESIAN_POINT('Ctrl Pts',(-12.4916247378875,92.2583072840424,
73.6464555593212));
#150035=CARTESIAN_POINT('Ctrl Pts',(-12.4845501037104,92.2563257071815,
73.9792912228145));
#150036=CARTESIAN_POINT('Ctrl Pts',(-12.4775098517978,92.254353760656,74.3105093265076));
#150037=CARTESIAN_POINT('Ctrl Pts',(-12.4668556080519,92.2513942172489,
74.6443827889115));
#150038=CARTESIAN_POINT('Ctrl Pts',(-12.4523224899448,92.2474120641582,
74.9808385860427));
#150039=CARTESIAN_POINT('Ctrl Pts',(-12.4379614340165,92.2434770570366,
75.3133109766448));
#150040=CARTESIAN_POINT('Ctrl Pts',(-12.4198128371299,92.2385431086074,
75.6483052872056));
#150041=CARTESIAN_POINT('Ctrl Pts',(-12.3975777798044,92.2325586337195,
75.9857319461363));
#150042=CARTESIAN_POINT('Ctrl Pts',(-12.3844912877986,92.2290364578315,
76.1843251501014));
#150043=CARTESIAN_POINT('Ctrl Pts',(-12.3699884505046,92.2251500699082,
76.3837605179081));
#150044=CARTESIAN_POINT('Ctrl Pts',(-12.3540010853324,92.2208870301987,
76.5840158149206));
#150045=CARTESIAN_POINT('Ctrl Pts',(-12.3376237215031,92.2165199971329,
76.789156175612));
#150046=CARTESIAN_POINT('Ctrl Pts',(-12.3196885504839,92.2117576623274,
76.9951570081091));
#150047=CARTESIAN_POINT('Ctrl Pts',(-12.300116262123,92.2065859680533,77.2019905324337));
#150048=CARTESIAN_POINT('Ctrl Pts',(-12.2903301179426,92.2040001209163,
77.305407294596));
#150049=CARTESIAN_POINT('Ctrl Pts',(-12.2801346073562,92.2013118947475,
77.4090322202606));
#150050=CARTESIAN_POINT('Ctrl Pts',(-12.2695192256138,92.198519576097,77.5128613589908));
#150051=CARTESIAN_POINT('Ctrl Pts',(-12.2642115347425,92.1971234167717,
77.564775928356));
#150052=CARTESIAN_POINT('Ctrl Pts',(-12.2587988709082,92.1957012318767,
77.6167415504726));
#150053=CARTESIAN_POINT('Ctrl Pts',(-12.2532798859677,92.1942528057137,
77.6687577129092));
#150054=CARTESIAN_POINT('Ctrl Pts',(-12.2505203934975,92.1935285926322,
77.6947657941275));
#150055=CARTESIAN_POINT('Ctrl Pts',(-12.24773432042,92.1927978190946,77.7207865103862));
#150056=CARTESIAN_POINT('Ctrl Pts',(-12.2449214959388,92.1920604584761,
77.7468197957659));
#150057=CARTESIAN_POINT('Ctrl Pts',(-12.2421086714576,92.1913230978576,
77.7728530811455));
#150058=CARTESIAN_POINT('Ctrl Pts',(-12.2390463837698,92.1905208353823,
77.8009235321599));
#150059=CARTESIAN_POINT('Ctrl Pts',(-12.2364025960721,92.1898285886004,
77.8249572926695));
#150060=CARTESIAN_POINT('Ctrl Pts',(-12.194101992908,92.1787526400903,78.2094974608232));
#150061=CARTESIAN_POINT('Ctrl Pts',(-12.1466029859566,92.1665260939933,
78.5903521816213));
#150062=CARTESIAN_POINT('Ctrl Pts',(-12.0939475669821,92.1531019690993,
78.9673541734208));
#150063=CARTESIAN_POINT('Ctrl Pts',(-12.0444616746194,92.140485892492,79.3216630052577));
#150064=CARTESIAN_POINT('Ctrl Pts',(-11.9904208935979,92.1268113864172,
79.6725690802869));
#150065=CARTESIAN_POINT('Ctrl Pts',(-11.9318247266413,92.1120654834831,
80.0199159293835));
#150066=CARTESIAN_POINT('Ctrl Pts',(-11.8750461090089,92.0977769723428,
80.356488694378));
#150067=CARTESIAN_POINT('Ctrl Pts',(-11.8139898404085,92.0824817920859,
80.6897196845255));
#150068=CARTESIAN_POINT('Ctrl Pts',(-11.7486284076709,92.0662034782385,
81.0194480563154));
#150069=CARTESIAN_POINT('Ctrl Pts',(-11.6860811016712,92.0506260247658,
81.3349800222365));
#150070=CARTESIAN_POINT('Ctrl Pts',(-11.619590771328,92.0341477904893,81.6473044059264));
#150071=CARTESIAN_POINT('Ctrl Pts',(-11.5491159649485,92.0168306365032,
81.9562632022298));
#150072=CARTESIAN_POINT('Ctrl Pts',(-11.5266264149309,92.0113044772877,
82.0548565103891));
#150073=CARTESIAN_POINT('Ctrl Pts',(-11.5037310091423,92.0056932419443,
82.1531069576772));
#150074=CARTESIAN_POINT('Ctrl Pts',(-11.4804281687818,92.,82.25100905091));
#150075=CARTESIAN_POINT('',(-8.92925733991791,92.5,88.41857688658));
#150076=CARTESIAN_POINT('Origin',(-8.92925733991791,92.,88.41857688658));
#150077=CARTESIAN_POINT('',(-8.92925733991791,92.5,57.55920188658));
#150078=CARTESIAN_POINT('Origin',(27.4324635166691,92.5,72.98888938658));
#150079=CARTESIAN_POINT('',(-9.38953228746991,92.,57.36388938658));
#150080=CARTESIAN_POINT('Origin',(-8.92925733991791,92.,57.55920188658));
#150081=CARTESIAN_POINT('Origin',(27.4324635166691,92.,72.98888938658));
#150082=CARTESIAN_POINT('Origin',(27.4324635166691,25.,72.98888938658));
#150083=CARTESIAN_POINT('',(-9.38953228747191,84.53989106251,57.36388938659));
#150084=CARTESIAN_POINT('',(-10.7897592617979,89.96662731952,61.19644749046));
#150085=CARTESIAN_POINT('Ctrl Pts',(-9.38953228747346,84.53989106251,57.3638893865893));
#150086=CARTESIAN_POINT('Ctrl Pts',(-9.46407393605236,84.9040360028837,
57.5395548119466));
#150087=CARTESIAN_POINT('Ctrl Pts',(-9.54149202137624,85.2622843930189,
57.7254840535312));
#150088=CARTESIAN_POINT('Ctrl Pts',(-9.62133538212254,85.6146362329159,
57.9218396698004));
#150089=CARTESIAN_POINT('Ctrl Pts',(-9.65220762867145,85.7508766512999,
57.9977625635772));
#150090=CARTESIAN_POINT('Ctrl Pts',(-9.68344192114709,85.8862354995815,
58.0752443252074));
#150091=CARTESIAN_POINT('Ctrl Pts',(-9.71501009391432,86.0207127777606,
58.1542945370059));
#150092=CARTESIAN_POINT('Ctrl Pts',(-9.79703933318159,86.3701491835071,
58.3597048654899));
#150093=CARTESIAN_POINT('Ctrl Pts',(-9.88155117347576,86.7144627113139,
58.5762881726688));
#150094=CARTESIAN_POINT('Ctrl Pts',(-9.96752404023887,87.0518501318954,
58.8029480803737));
#150095=CARTESIAN_POINT('Ctrl Pts',(-10.000205282342,87.1801026886582,58.8891093030674));
#150096=CARTESIAN_POINT('Ctrl Pts',(-10.0330980015701,87.307354408076,58.9767262639575));
#150097=CARTESIAN_POINT('Ctrl Pts',(-10.0661476244504,87.4335062383448,
59.0657373552651));
#150098=CARTESIAN_POINT('Ctrl Pts',(-10.1635306433684,87.8052214049021,
59.3280147440303));
#150099=CARTESIAN_POINT('Ctrl Pts',(-10.261646774493,88.1651378511986,59.6006888927839));
#150100=CARTESIAN_POINT('Ctrl Pts',(-10.3598592983923,88.5132555772343,
59.8839156650425));
#150101=CARTESIAN_POINT('Ctrl Pts',(-10.4570454426319,88.8577352646674,
60.164182548006));
#150102=CARTESIAN_POINT('Ctrl Pts',(-10.5543259257963,89.19066155062,60.4547829485653));
#150103=CARTESIAN_POINT('Ctrl Pts',(-10.6510347955172,89.5120344350921,
60.7558539372034));
#150104=CARTESIAN_POINT('Ctrl Pts',(-10.6974344449989,89.6662249373226,
60.9003038556258));
#150105=CARTESIAN_POINT('Ctrl Pts',(-10.7437017885551,89.8177558987986,
61.0471638206023));
#150106=CARTESIAN_POINT('Ctrl Pts',(-10.7897592617964,89.96662731952,61.1964474904605));
#150107=CARTESIAN_POINT('Ctrl Pts',(-10.7897592617979,89.96662731952,61.19644749046));
#150108=CARTESIAN_POINT('Ctrl Pts',(-11.0308907230829,90.74601077155,61.97801449744));
#150109=CARTESIAN_POINT('Ctrl Pts',(-11.2651526236999,91.42091161506,62.82233335276));
#150110=CARTESIAN_POINT('Ctrl Pts',(-11.4804394903149,91.99991170272,63.726817270116));
#150111=CARTESIAN_POINT('',(-9.38953228747191,84.53989106251,57.36388938659));
#150112=CARTESIAN_POINT('Origin',(-2.02513312664091,25.,60.48888938658));
#150113=CARTESIAN_POINT('Ctrl Pts',(-9.38953228746991,65.4601089375,57.36388938658));
#150114=CARTESIAN_POINT('Ctrl Pts',(-9.28299760589922,66.2118050055448,
57.1128289323244));
#150115=CARTESIAN_POINT('Ctrl Pts',(-9.17640320161983,66.9710984420553,
56.8968437256938));
#150116=CARTESIAN_POINT('Ctrl Pts',(-9.02882006242401,68.1214346495195,
56.6211725879589));
#150117=CARTESIAN_POINT('Ctrl Pts',(-8.98163454412516,68.5067793941239,
56.537325043936));
#150118=CARTESIAN_POINT('Ctrl Pts',(-8.91505371445119,69.0876455242053,
56.423063827724));
#150119=CARTESIAN_POINT('Ctrl Pts',(-8.88280899764823,69.3787908425396,
56.368811046357));
#150120=CARTESIAN_POINT('Ctrl Pts',(-8.84724153254128,69.7197068238602,
56.3104368697525));
#150121=CARTESIAN_POINT('Ctrl Pts',(-8.82999560525437,69.8904764253365,
56.2824661787672));
#150122=CARTESIAN_POINT('Ctrl Pts',(-8.82272235145676,69.963730171144,56.2707379426146));
#150123=CARTESIAN_POINT('Ctrl Pts',(-8.81789998947213,70.0125808402926,
56.2629765596535));
#150124=CARTESIAN_POINT('Ctrl Pts',(-8.8156468607298,70.0355293404337,56.2593567797579));
#150125=CARTESIAN_POINT('Ctrl Pts',(-8.73217725899094,70.8910354288936,
56.1255245945254));
#150126=CARTESIAN_POINT('Ctrl Pts',(-8.66805506192528,71.7188625011877,
56.0304808759467));
#150127=CARTESIAN_POINT('Ctrl Pts',(-8.60339061485563,72.9579712257644,
55.936089919193));
#150128=CARTESIAN_POINT('Ctrl Pts',(-8.58704180991737,73.3705688199792,
55.912677597908));
#150129=CARTESIAN_POINT('Ctrl Pts',(-8.57070859794248,73.9888072403353,
55.8893750942764));
#150130=CARTESIAN_POINT('Ctrl Pts',(-8.56662647565255,74.1947770519598,
55.8835786701559));
#150131=CARTESIAN_POINT('Ctrl Pts',(-8.56121809111756,74.6064973515531,
55.8759060387761));
#150132=CARTESIAN_POINT('Ctrl Pts',(-8.5598922203733,74.8136830320495,55.874030385872));
#150133=CARTESIAN_POINT('Ctrl Pts',(-8.56017384125938,75.8347112001197,
55.8744291786228));
#150134=CARTESIAN_POINT('Ctrl Pts',(-8.58277625686546,76.6556212834695,
55.9059564905199));
#150135=CARTESIAN_POINT('Ctrl Pts',(-8.64817866699516,77.8931177318349,
56.0014895705745));
#150136=CARTESIAN_POINT('Ctrl Pts',(-8.67518679071417,78.3066384351802,
56.0414040317839));
#150137=CARTESIAN_POINT('Ctrl Pts',(-8.72285528790153,78.9284523210332,
56.1138062125588));
#150138=CARTESIAN_POINT('Ctrl Pts',(-8.74847436625218,79.2397424716684,
56.1531423150821));
#150139=CARTESIAN_POINT('Ctrl Pts',(-8.78129743014201,79.6035849275667,
56.204636960379));
#150140=CARTESIAN_POINT('Ctrl Pts',(-8.79841527834941,79.7856738088883,
56.2318009811848));
#150141=CARTESIAN_POINT('Ctrl Pts',(-8.80589984657566,79.8637478266061,
56.2437480312129));
#150142=CARTESIAN_POINT('Ctrl Pts',(-8.81092218104148,79.9158051552451,
56.2517807797114));
#150143=CARTESIAN_POINT('Ctrl Pts',(-8.81362946612071,79.9436783214225,
56.2561199096899));
#150144=CARTESIAN_POINT('Ctrl Pts',(-8.96727708087226,81.5164272720892,
56.5028463122281));
#150145=CARTESIAN_POINT('Ctrl Pts',(-9.1770201042476,83.0404328065509,56.863081532569));
#150146=CARTESIAN_POINT('Ctrl Pts',(-9.38953228747191,84.53989106251,57.36388938659));
#150147=CARTESIAN_POINT('',(1.23275780153909,92.,53.18230696385));
#150148=CARTESIAN_POINT('Origin',(-2.02513312664091,92.,60.48888938658));
#150149=CARTESIAN_POINT('',(1.23275780350218,24.13180332306,53.1823069610377));
#150150=CARTESIAN_POINT('',(1.23275780153909,92.,53.18230696385));
#150151=CARTESIAN_POINT('',(-2.42457387236482,16.9255393804567,52.4988701141421));
#150152=CARTESIAN_POINT('Ctrl Pts',(1.23275780212727,24.13180332306,53.1823069641211));
#150153=CARTESIAN_POINT('Ctrl Pts',(1.09525026227048,23.9222975650672,53.1209945008038));
#150154=CARTESIAN_POINT('Ctrl Pts',(0.957371605292284,23.7068349358274,
53.0640496456824));
#150155=CARTESIAN_POINT('Ctrl Pts',(0.819366193047706,23.4853492447597,
53.0113999264875));
#150156=CARTESIAN_POINT('Ctrl Pts',(0.678897420682025,23.2599100926654,
52.9578104237252));
#150157=CARTESIAN_POINT('Ctrl Pts',(0.538297793952373,23.0282309049978,
52.9086708304224));
#150158=CARTESIAN_POINT('Ctrl Pts',(0.397838434541305,22.7902825142855,
52.8638717634787));
#150159=CARTESIAN_POINT('Ctrl Pts',(0.256254933206571,22.5504297452335,
52.8187141550358));
#150160=CARTESIAN_POINT('Ctrl Pts',(0.114814424623342,22.3042070568793,
52.7779668212956));
#150161=CARTESIAN_POINT('Ctrl Pts',(-0.0261990531770868,22.0516254172157,
52.7414840959157));
#150162=CARTESIAN_POINT('Ctrl Pts',(-0.169023217529076,21.7958004976526,
52.7045329133272));
#150163=CARTESIAN_POINT('Ctrl Pts',(-0.311408876098802,21.5334522976639,
52.6719565200889));
#150164=CARTESIAN_POINT('Ctrl Pts',(-0.45306134541689,21.2646335721508,
52.6435694854777));
#150165=CARTESIAN_POINT('Ctrl Pts',(-0.516137561329358,21.1449316844717,
52.6309290653504));
#150166=CARTESIAN_POINT('Ctrl Pts',(-0.57906844504845,21.0239473502742,
52.6191188750192));
#150167=CARTESIAN_POINT('Ctrl Pts',(-0.641828334153602,20.9016877827935,
52.6081204724598));
#150168=CARTESIAN_POINT('Ctrl Pts',(-0.769429273692215,20.653114436018,
52.5857589527053));
#150169=CARTESIAN_POINT('Ctrl Pts',(-0.896236804350713,20.3991574139139,
52.5667689819771));
#150170=CARTESIAN_POINT('Ctrl Pts',(-1.02217945969569,20.1398812142133,
52.550955736531));
#150171=CARTESIAN_POINT('Ctrl Pts',(-1.14550571933736,19.8859913479436,
52.5354710033536));
#150172=CARTESIAN_POINT('Ctrl Pts',(-1.26800325069717,19.6270006376272,
52.5230327116852));
#150173=CARTESIAN_POINT('Ctrl Pts',(-1.38957325127653,19.3629328949489,
52.513467924596));
#150174=CARTESIAN_POINT('Ctrl Pts',(-1.50940787880506,19.1026346352191,
52.5040396717971));
#150175=CARTESIAN_POINT('Ctrl Pts',(-1.62834174173715,18.8374029165924,
52.4974038626211));
#150176=CARTESIAN_POINT('Ctrl Pts',(-1.74624125684383,18.567229635568,52.4933993676503));
#150177=CARTESIAN_POINT('Ctrl Pts',(-1.86159178806976,18.3028974925474,
52.4894814497374));
#150178=CARTESIAN_POINT('Ctrl Pts',(-1.97595248783855,18.0338347696117,
52.4880827511661));
#150179=CARTESIAN_POINT('Ctrl Pts',(-2.08915530741183,17.7600093880497,
52.4890505267765));
#150180=CARTESIAN_POINT('Ctrl Pts',(-2.16757198876065,17.57032791393,52.4897209142451));
#150181=CARTESIAN_POINT('Ctrl Pts',(-2.245432170471,17.378360579323,52.491526829913));
#150182=CARTESIAN_POINT('Ctrl Pts',(-2.32266658659977,17.1840910996425,
52.4944150526792));
#150183=CARTESIAN_POINT('Ctrl Pts',(-2.32911013941652,17.1678834850097,
52.494656012822));
#150184=CARTESIAN_POINT('Ctrl Pts',(-2.33569707077722,17.1517522798405,
52.4949096119963));
#150185=CARTESIAN_POINT('Ctrl Pts',(-2.34230749508296,17.1356174290227,
52.4951723835218));
#150186=CARTESIAN_POINT('Ctrl Pts',(-2.34891128208127,17.1194987786725,
52.4954348912071));
#150187=CARTESIAN_POINT('Ctrl Pts',(-2.35553848932307,17.1033765093641,
52.4957065085865));
#150188=CARTESIAN_POINT('Ctrl Pts',(-2.36211074522106,17.0872026605915,
52.4959841149558));
#150189=CARTESIAN_POINT('Ctrl Pts',(-2.36868537913477,17.0710229596933,
52.4962618217703));
#150190=CARTESIAN_POINT('Ctrl Pts',(-2.37520500345411,17.0547916624888,
52.4965454828214));
#150191=CARTESIAN_POINT('Ctrl Pts',(-2.38163270894705,17.0384923626739,
52.4968329239004));
#150192=CARTESIAN_POINT('Ctrl Pts',(-2.38806757573677,17.022174903327,52.4971206852261));
#150193=CARTESIAN_POINT('Ctrl Pts',(-2.39441031079806,17.0057893164205,
52.497412192531));
#150194=CARTESIAN_POINT('Ctrl Pts',(-2.40066571962354,16.9893504652935,
52.4977068239092));
#150195=CARTESIAN_POINT('Ctrl Pts',(-2.40693939534868,16.9728636098151,
52.4980023156632));
#150196=CARTESIAN_POINT('Ctrl Pts',(-2.41312522812776,16.9563232079188,
52.4983009013797));
#150197=CARTESIAN_POINT('Ctrl Pts',(-2.41927024760488,16.9397753383813,
52.4986042071812));
#150198=CARTESIAN_POINT('Ctrl Pts',(-2.42103391321132,16.9350259785994,
52.4986912581682));
#150199=CARTESIAN_POINT('Ctrl Pts',(-2.42279448210005,16.9302761973306,
52.4987787146876));
#150200=CARTESIAN_POINT('Ctrl Pts',(-2.424553705362,16.9255275487788,52.4988666581252));
#150201=CARTESIAN_POINT('',(-2.42458295845305,-16.925539708287,52.4988706296686));
#150202=CARTESIAN_POINT('',(-2.42460157766091,-16.92552641542,52.49887156046));
#150203=CARTESIAN_POINT('',(1.23275780153909,-24.13180332393,53.18230696385));
#150204=CARTESIAN_POINT('Ctrl Pts',(-2.42455466529549,-16.925524957794,
52.4988667061117));
#150205=CARTESIAN_POINT('Ctrl Pts',(-2.41835263264369,-16.9422743869142,
52.4985566662608));
#150206=CARTESIAN_POINT('Ctrl Pts',(-2.41213098287879,-16.9590344309857,
52.4982525085495));
#150207=CARTESIAN_POINT('Ctrl Pts',(-2.40583009662638,-16.9757502119588,
52.497951814072));
#150208=CARTESIAN_POINT('Ctrl Pts',(-2.39954460352843,-16.9924251560419,
52.4976518541954));
#150209=CARTESIAN_POINT('Ctrl Pts',(-2.39318026048568,-17.0090560171085,
52.4973553905347));
#150210=CARTESIAN_POINT('Ctrl Pts',(-2.38671975157702,-17.0256188820132,
52.4970624787638));
#150211=CARTESIAN_POINT('Ctrl Pts',(-2.38027083356337,-17.0421520312358,
52.4967700925103));
#150212=CARTESIAN_POINT('Ctrl Pts',(-2.37372610356048,-17.0586174007026,
52.4964812904674));
#150213=CARTESIAN_POINT('Ctrl Pts',(-2.36711004809713,-17.0750221742194,
52.4961978656708));
#150214=CARTESIAN_POINT('Ctrl Pts',(-2.36049508485471,-17.0914242395308,
52.4959144876638));
#150215=CARTESIAN_POINT('Ctrl Pts',(-2.35380883249986,-17.1077657033903,
52.4956365252539));
#150216=CARTESIAN_POINT('Ctrl Pts',(-2.34711735211228,-17.1240851396031,
52.4953668745901));
#150217=CARTESIAN_POINT('Ctrl Pts',(-2.3404188180097,-17.1404217786837,
52.4950969396784));
#150218=CARTESIAN_POINT('Ctrl Pts',(-2.33371506507477,-17.1567363204905,
52.4948353762192));
#150219=CARTESIAN_POINT('Ctrl Pts',(-2.32711380675133,-17.1730992969542,
52.4945855879091));
#150220=CARTESIAN_POINT('Ctrl Pts',(-2.32505536676958,-17.1782016885473,
52.4945076975708));
#150221=CARTESIAN_POINT('Ctrl Pts',(-2.32300719438366,-17.1833090236636,
52.4944309532452));
#150222=CARTESIAN_POINT('Ctrl Pts',(-2.32097337228297,-17.188424077842,
52.4943554571288));
#150223=CARTESIAN_POINT('Ctrl Pts',(-2.21954797925199,-17.4435085221712,
52.4905905146218));
#150224=CARTESIAN_POINT('Ctrl Pts',(-2.11702976879158,-17.6945893285042,
52.4887010808945));
#150225=CARTESIAN_POINT('Ctrl Pts',(-2.01359961223417,-17.9417144089226,
52.4888021911267));
#150226=CARTESIAN_POINT('Ctrl Pts',(-1.9086896659158,-18.1923751425378,
52.4889047479572));
#150227=CARTESIAN_POINT('Ctrl Pts',(-1.80284129394811,-18.4389665694389,
52.4910546547565));
#150228=CARTESIAN_POINT('Ctrl Pts',(-1.69619391444929,-18.6815194107603,
52.4953644233417));
#150229=CARTESIAN_POINT('Ctrl Pts',(-1.58746267668813,-18.9288116628841,
52.4997584035308));
#150230=CARTESIAN_POINT('Ctrl Pts',(-1.47790061381537,-19.171906378998,
52.5063969849476));
#150231=CARTESIAN_POINT('Ctrl Pts',(-1.36760821367348,-19.4108097918281,
52.5153996784079));
#150232=CARTESIAN_POINT('Ctrl Pts',(-1.25621699724117,-19.6520933411093,
52.5244920635081));
#150233=CARTESIAN_POINT('Ctrl Pts',(-1.14408033744016,-19.889102004872,
52.5359954900293));
#150234=CARTESIAN_POINT('Ctrl Pts',(-1.03125997888467,-20.1218098515863,
52.5500402330157));
#150235=CARTESIAN_POINT('Ctrl Pts',(-0.91722611671491,-20.3570207200662,
52.5642360422334));
#150236=CARTESIAN_POINT('Ctrl Pts',(-0.802493180553639,-20.5878380901434,
52.5810277926978));
#150237=CARTESIAN_POINT('Ctrl Pts',(-0.68709057782042,-20.8141971117313,
52.6005629759781));
#150238=CARTESIAN_POINT('Ctrl Pts',(-0.671716883247116,-20.8443521895145,
52.6031654124403));
#150239=CARTESIAN_POINT('Ctrl Pts',(-0.656331262552002,-20.8744280858999,
52.6058165594344));
#150240=CARTESIAN_POINT('Ctrl Pts',(-0.640933749040346,-20.9044245923751,
52.6085167874446));
#150241=CARTESIAN_POINT('Ctrl Pts',(-0.501024753429229,-21.1769868531328,
52.6330523196617));
#150242=CARTESIAN_POINT('Ctrl Pts',(-0.360277472641413,-21.4431663440956,
52.6616144460825));
#150243=CARTESIAN_POINT('Ctrl Pts',(-0.218979784607261,-21.7028881581558,
52.6943972178819));
#150244=CARTESIAN_POINT('Ctrl Pts',(-0.0790390129840126,-21.9601157998295,
52.72686516867));
#150245=CARTESIAN_POINT('Ctrl Pts',(0.0614412526471609,-22.2110091853603,
52.7634731492255));
#150246=CARTESIAN_POINT('Ctrl Pts',(0.202178786129167,-22.4555374170789,
52.8043804173196));
#150247=CARTESIAN_POINT('Ctrl Pts',(0.342131600715697,-22.6987022177414,
52.8450595962505));
#150248=CARTESIAN_POINT('Ctrl Pts',(0.482338366082033,-22.9355726349923,
52.88999025376));
#150249=CARTESIAN_POINT('Ctrl Pts',(0.622525337285318,-23.1661601006708,
52.9392994974083));
#150250=CARTESIAN_POINT('Ctrl Pts',(0.760950939843198,-23.3938503674971,
52.9879891987772));
#150251=CARTESIAN_POINT('Ctrl Pts',(0.899356763048862,-23.6154146140776,
53.0409480806527));
#150252=CARTESIAN_POINT('Ctrl Pts',(1.03748989378346,-23.8309044364283,
53.0982702636116));
#150253=CARTESIAN_POINT('Ctrl Pts',(1.10264808140848,-23.9325522178211,
53.1253094650867));
#150254=CARTESIAN_POINT('Ctrl Pts',(1.16774579196361,-24.0328489872031,
53.1533191246783));
#150255=CARTESIAN_POINT('Ctrl Pts',(1.23275780153649,-24.13180332393,53.1823069638558));
#150256=CARTESIAN_POINT('',(1.23275780153909,-92.,53.18230696385));
#150257=CARTESIAN_POINT('',(1.23275780153909,-24.13180332393,53.18230696385));
#150258=CARTESIAN_POINT('Origin',(-2.02513312664091,-92.,60.48888938658));
#150259=CARTESIAN_POINT('',(-9.38953228746991,-92.,57.36388938658));
#150260=CARTESIAN_POINT('Ctrl Pts',(-15.7857783725339,63.70338519495,63.115509260727));
#150261=CARTESIAN_POINT('Ctrl Pts',(-13.2009589750562,63.38469268621,63.626388245956));
#150262=CARTESIAN_POINT('Ctrl Pts',(-11.2043264355729,61.80998487044,62.8661053606));
#150263=CARTESIAN_POINT('Ctrl Pts',(-10.7993789544399,59.77045106498,61.21655661769));
#150264=CARTESIAN_POINT('Ctrl Pts',(-15.2179723740729,64.90944119133,61.73606668886));
#150265=CARTESIAN_POINT('Ctrl Pts',(-12.7684152553161,64.50610810913,62.2234622344801));
#150266=CARTESIAN_POINT('Ctrl Pts',(-10.8253714758609,63.1180161071301,
61.36857549733));
#150267=CARTESIAN_POINT('Ctrl Pts',(-10.2917538862999,61.39001548839,59.56845212723));
#150268=CARTESIAN_POINT('Ctrl Pts',(-14.6117331505179,66.35834909817,60.58580302675));
#150269=CARTESIAN_POINT('Ctrl Pts',(-12.2792545314683,65.93351518384,60.96502124799));
#150270=CARTESIAN_POINT('Ctrl Pts',(-10.3902588488809,64.76046407779,60.03498149353));
#150271=CARTESIAN_POINT('Ctrl Pts',(-9.75033914805191,63.33933556912,58.1921248627));
#150272=CARTESIAN_POINT('Ctrl Pts',(-14.1114447652659,67.99712344605,59.72095409226));
#150273=CARTESIAN_POINT('Ctrl Pts',(-11.8630597324037,67.63436557765,59.99674441583));
#150274=CARTESIAN_POINT('Ctrl Pts',(-10.0167553446379,66.69384340644,59.01200819548));
#150275=CARTESIAN_POINT('Ctrl Pts',(-9.30390833655991,65.54803587831,57.15665909541));
#150276=CARTESIAN_POINT('',(-15.5675364833309,63.77502783968,63.039015015514));
#150277=CARTESIAN_POINT('Origin',(-15.5675364831312,60.0333704534644,59.7223902246598));
#150278=CARTESIAN_POINT('',(-13.9923246930869,67.84508927339,59.80529136859));
#150279=CARTESIAN_POINT('Ctrl Pts',(-13.9923246930881,67.8450893401677,
59.8052914916334));
#150280=CARTESIAN_POINT('Ctrl Pts',(-14.0321520574323,67.7153858292997,
59.8756832798915));
#150281=CARTESIAN_POINT('Ctrl Pts',(-14.0742956175811,67.5816710739956,
59.9507139079171));
#150282=CARTESIAN_POINT('Ctrl Pts',(-14.11877878484,67.4442748492075,60.0308072755673));
#150283=CARTESIAN_POINT('Ctrl Pts',(-14.161844373002,67.3112571349494,60.108348246642));
#150284=CARTESIAN_POINT('Ctrl Pts',(-14.2071031672786,67.1747888454886,
60.190634689278));
#150285=CARTESIAN_POINT('Ctrl Pts',(-14.2545486384612,67.0352046600873,
60.2780692905195));
#150286=CARTESIAN_POINT('Ctrl Pts',(-14.2797769640136,66.9609831341231,
60.3245611585456));
#150287=CARTESIAN_POINT('Ctrl Pts',(-14.3056230459681,66.8858812263002,
60.3725089025942));
#150288=CARTESIAN_POINT('Ctrl Pts',(-14.3320820314631,66.8099535694013,
60.421974853236));
#150289=CARTESIAN_POINT('Ctrl Pts',(-14.3803584923795,66.6714176999353,
60.5122292975455));
#150290=CARTESIAN_POINT('Ctrl Pts',(-14.4306882769546,66.5301340787245,
60.6075354406058));
#150291=CARTESIAN_POINT('Ctrl Pts',(-14.4830772813101,66.3864780506606,
60.7082683981477));
#150292=CARTESIAN_POINT('Ctrl Pts',(-14.4999323047482,66.3402598460997,
60.7406770377325));
#150293=CARTESIAN_POINT('Ctrl Pts',(-14.5170002006767,66.2937963570198,
60.7736474591747));
#150294=CARTESIAN_POINT('Ctrl Pts',(-14.5342803448823,66.2471008957992,
60.8071923009608));
#150295=CARTESIAN_POINT('Ctrl Pts',(-14.5697756021284,66.1511834434602,
60.8760969798981));
#150296=CARTESIAN_POINT('Ctrl Pts',(-14.6061686288561,66.0542871503293,
60.9474250351948));
#150297=CARTESIAN_POINT('Ctrl Pts',(-14.6434594244527,65.956535330544,61.0212846501146));
#150298=CARTESIAN_POINT('Ctrl Pts',(-14.6621048222509,65.9076594206514,
61.0582144575746));
#150299=CARTESIAN_POINT('Ctrl Pts',(-14.6809746622664,65.8585696766716,
61.095777214623));
#150300=CARTESIAN_POINT('Ctrl Pts',(-14.7000689443167,65.8092824831939,
61.1339862575457));
#150301=CARTESIAN_POINT('Ctrl Pts',(-14.7096160853419,65.784638886455,61.1530907790071));
#150302=CARTESIAN_POINT('Ctrl Pts',(-14.7192193368761,65.759945929971,61.1723568753724));
#150303=CARTESIAN_POINT('Ctrl Pts',(-14.7288786988963,65.735205700205,61.191786216759));
#150304=CARTESIAN_POINT('Ctrl Pts',(-14.7337083799064,65.7228355853219,
61.2015008874524));
#150305=CARTESIAN_POINT('Ctrl Pts',(-14.738552088538,65.7104536522903,61.211256369612));
#150306=CARTESIAN_POINT('Ctrl Pts',(-14.7434098247882,65.6980601653776,
61.22105287134));
#150307=CARTESIAN_POINT('Ctrl Pts',(-14.7470531269758,65.6887650501931,
61.228400247636));
#150308=CARTESIAN_POINT('Ctrl Pts',(-14.7507043196989,65.6794634359645,
61.2357706974564));
#150309=CARTESIAN_POINT('Ctrl Pts',(-14.7543634029561,65.6701554349684,
61.2431643084709));
#150310=CARTESIAN_POINT('Ctrl Pts',(-14.7555830973751,65.6670527679697,
61.2456288454757));
#150311=CARTESIAN_POINT('Ctrl Pts',(-14.7573321603146,65.6626063279641,
61.2491645315469));
#150312=CARTESIAN_POINT('Ctrl Pts',(-14.7580251163913,65.6608453092675,
61.2505656431045));
#150313=CARTESIAN_POINT('Ctrl Pts',(-14.7768289843091,65.6130587841394,
61.2885858258435));
#150314=CARTESIAN_POINT('Ctrl Pts',(-14.797711821438,65.5603698583314,61.330978651077));
#150315=CARTESIAN_POINT('Ctrl Pts',(-14.8206778684102,65.5029514681166,
61.3779472113108));
#150316=CARTESIAN_POINT('Ctrl Pts',(-14.8435571314035,65.445750050216,61.4247382869935));
#150317=CARTESIAN_POINT('Ctrl Pts',(-14.8685041894234,65.3838547534065,
61.4760707197307));
#150318=CARTESIAN_POINT('Ctrl Pts',(-14.8955171319156,65.3174744488824,
61.5321798820439));
#150319=CARTESIAN_POINT('Ctrl Pts',(-14.905340852726,65.2933341102596,61.5525849432709));
#150320=CARTESIAN_POINT('Ctrl Pts',(-14.9154377134962,65.268600982511,61.5736220664484));
#150321=CARTESIAN_POINT('Ctrl Pts',(-14.9258072946201,65.2432864000251,
61.5953036541628));
#150322=CARTESIAN_POINT('Ctrl Pts',(-14.9596821651009,65.1605898867583,
61.6661320672748));
#150323=CARTESIAN_POINT('Ctrl Pts',(-14.9966038285022,65.0713415229218,
61.744131678552));
#150324=CARTESIAN_POINT('Ctrl Pts',(-15.03637930123,64.9765154645022,61.8293260428297));
#150325=CARTESIAN_POINT('Ctrl Pts',(-15.0758681069583,64.8823728298055,
61.9139064002556));
#150326=CARTESIAN_POINT('Ctrl Pts',(-15.1181703187741,64.7827335245751,
62.0055795972903));
#150327=CARTESIAN_POINT('Ctrl Pts',(-15.1630587148956,64.6785840780694,
62.104371243476));
#150328=CARTESIAN_POINT('Ctrl Pts',(-15.2004689345102,64.5917853950428,
62.1867047082292));
#150329=CARTESIAN_POINT('Ctrl Pts',(-15.2359488874782,64.5104427706175,
62.2658310693622));
#150330=CARTESIAN_POINT('Ctrl Pts',(-15.269470099101,64.4342772954221,62.3414348811389));
#150331=CARTESIAN_POINT('Ctrl Pts',(-15.3035998098307,64.3567292143662,
62.4184111030919));
#150332=CARTESIAN_POINT('Ctrl Pts',(-15.3356993668365,64.2845477185496,
62.4917357694123));
#150333=CARTESIAN_POINT('Ctrl Pts',(-15.3657584993669,64.2174647565579,
62.561118959892));
#150334=CARTESIAN_POINT('Ctrl Pts',(-15.3960271377004,64.1499142404939,
62.6309857365507));
#150335=CARTESIAN_POINT('Ctrl Pts',(-15.4242271702903,64.0875334031512,
62.6968560124063));
#150336=CARTESIAN_POINT('Ctrl Pts',(-15.4503625601862,64.0300779903869,
62.7584757252218));
#150337=CARTESIAN_POINT('Ctrl Pts',(-15.4766688062985,63.9722469714244,
62.8204982677264));
#150338=CARTESIAN_POINT('Ctrl Pts',(-15.5008836555906,63.919405824393,62.8782145871554));
#150339=CARTESIAN_POINT('Ctrl Pts',(-15.523020519425,63.8713377355141,62.9314064107263));
#150340=CARTESIAN_POINT('Ctrl Pts',(-15.5389300947263,63.8367916098601,
62.969634920819));
#150341=CARTESIAN_POINT('Ctrl Pts',(-15.5537665555699,63.8047115232912,
63.0055273040344));
#150342=CARTESIAN_POINT('Ctrl Pts',(-15.5675364833309,63.7750278396776,
63.0390150155119));
#150343=CARTESIAN_POINT('Origin',(-13.9922817630625,65.460108937173,55.4107643867529));
#150344=CARTESIAN_POINT('Ctrl Pts',(-14.2053627384189,67.74544063191,59.85616341864));
#150345=CARTESIAN_POINT('Ctrl Pts',(-13.6866847824139,67.6633717185,59.92373292205));
#150346=CARTESIAN_POINT('Ctrl Pts',(-12.6383817091281,67.41710017746,59.91553905833));
#150347=CARTESIAN_POINT('Ctrl Pts',(-11.1637780911519,66.80360758364,59.42315761485));
#150348=CARTESIAN_POINT('Ctrl Pts',(-9.99316319052591,66.02973850092,58.51581872871));
#150349=CARTESIAN_POINT('Ctrl Pts',(-9.52143302578291,65.47873222039,57.71959030244));
#150350=CARTESIAN_POINT('Ctrl Pts',(-9.36367665720291,65.20602642706,57.29408547032));
#150351=CARTESIAN_POINT('Ctrl Pts',(-14.0202046372339,68.33201427489,59.53231650414));
#150352=CARTESIAN_POINT('Ctrl Pts',(-13.5161419891374,68.2470102229,59.59488219199));
#150353=CARTESIAN_POINT('Ctrl Pts',(-12.5016391850898,68.0065002871,59.58065052529));
#150354=CARTESIAN_POINT('Ctrl Pts',(-11.0704533736519,67.43981681245,59.10069440811));
#150355=CARTESIAN_POINT('Ctrl Pts',(-9.91290994946691,66.7392443083,58.22296820509));
#150356=CARTESIAN_POINT('Ctrl Pts',(-9.42170896486791,66.24201106279,57.44738812635));
#150357=CARTESIAN_POINT('Ctrl Pts',(-9.24823875588991,65.99481676477,57.0294496165));
#150358=CARTESIAN_POINT('Ctrl Pts',(-13.6549069241899,69.49993804976,58.98674389696));
#150359=CARTESIAN_POINT('Ctrl Pts',(-13.1769404748612,69.41646103563,59.03665035664));
#150360=CARTESIAN_POINT('Ctrl Pts',(-12.2218902458356,69.19905724735,59.00590868675));
#150361=CARTESIAN_POINT('Ctrl Pts',(-10.8679330720989,68.72846005566,58.54326883772));
#150362=CARTESIAN_POINT('Ctrl Pts',(-9.73897835675691,68.16508642168,57.71819138305));
#150363=CARTESIAN_POINT('Ctrl Pts',(-9.21997508227291,67.76716754432,56.98439768797));
#150364=CARTESIAN_POINT('Ctrl Pts',(-9.02174978537091,67.56775735817,56.58383055835));
#150365=CARTESIAN_POINT('Ctrl Pts',(-13.0264541098147,71.89096840686,58.22143278291));
#150366=CARTESIAN_POINT('Ctrl Pts',(-12.5887620025556,71.83103234225,58.24468551411));
#150367=CARTESIAN_POINT('Ctrl Pts',(-11.7230981427679,71.6906865179,58.17830836715));
#150368=CARTESIAN_POINT('Ctrl Pts',(-10.4863172342819,71.42179955806,57.73325733767));
#150369=CARTESIAN_POINT('Ctrl Pts',(-9.41080141879591,71.11627944215,56.98713738773));
#150370=CARTESIAN_POINT('Ctrl Pts',(-8.86349672505391,70.90290608307,56.32569316036));
#150371=CARTESIAN_POINT('Ctrl Pts',(-8.63464566339991,70.79475115391,55.9591981337));
#150372=CARTESIAN_POINT('Ctrl Pts',(-12.7037393234953,74.39162227679,57.90748319535));
#150373=CARTESIAN_POINT('Ctrl Pts',(-12.28393586553,74.38000747547,57.91587997198));
#150374=CARTESIAN_POINT('Ctrl Pts',(-11.4571120723499,74.35278927765,57.82979946692));
#150375=CARTESIAN_POINT('Ctrl Pts',(-10.2725544129929,74.30035033484,57.38928272527));
#150376=CARTESIAN_POINT('Ctrl Pts',(-9.22672717125391,74.2404602146,56.67735146262));
#150377=CARTESIAN_POINT('Ctrl Pts',(-8.67519748870391,74.19845211679,56.05133853923));
#150378=CARTESIAN_POINT('Ctrl Pts',(-8.43723858833691,74.17711457634,55.70323479651));
#150379=CARTESIAN_POINT('Ctrl Pts',(-12.8671141721126,76.88190734633,58.06713723927));
#150380=CARTESIAN_POINT('Ctrl Pts',(-12.4383232178018,76.91798866819,58.08327470442));
#150381=CARTESIAN_POINT('Ctrl Pts',(-11.5918425291884,77.0025099707,58.00755176421));
#150382=CARTESIAN_POINT('Ctrl Pts',(-10.3806961735749,77.16495510187,57.56487994748));
#150383=CARTESIAN_POINT('Ctrl Pts',(-9.31980220568091,77.35007308731,56.83532487627));
#150384=CARTESIAN_POINT('Ctrl Pts',(-8.77051022514491,77.47967802037,56.19100248932));
#150385=CARTESIAN_POINT('Ctrl Pts',(-8.53719879336791,77.5454508045,55.83340513874));
#150386=CARTESIAN_POINT('Ctrl Pts',(-13.3015354916722,79.37972298075,58.54120535384));
#150387=CARTESIAN_POINT('Ctrl Pts',(-12.846655159085,79.4564624083,58.57621796265));
#150388=CARTESIAN_POINT('Ctrl Pts',(-11.9431325981701,79.64368966687,58.52545042363));
#150389=CARTESIAN_POINT('Ctrl Pts',(-10.6566364727739,80.02083519139,58.07343649006));
#150390=CARTESIAN_POINT('Ctrl Pts',(-9.55738924270991,80.45907194911,57.29417007324));
#150391=CARTESIAN_POINT('Ctrl Pts',(-9.02052118745391,80.76657499756,56.60163811033));
#150392=CARTESIAN_POINT('Ctrl Pts',(-8.80382301199991,80.92163216041,56.22016816974));
#150393=CARTESIAN_POINT('Ctrl Pts',(-13.8489227042999,81.12444072467,59.23274232687));
#150394=CARTESIAN_POINT('Ctrl Pts',(-13.3583894249944,81.21204418286,59.29065555428));
#150395=CARTESIAN_POINT('Ctrl Pts',(-12.375145516444,81.44698775439,59.2707797108));
#150396=CARTESIAN_POINT('Ctrl Pts',(-10.9840720246189,81.97008585063,58.80223087688));
#150397=CARTESIAN_POINT('Ctrl Pts',(-9.83859395161891,82.60268348927,57.95185518517));
#150398=CARTESIAN_POINT('Ctrl Pts',(-9.32938702249691,83.05012179098,57.19539776513));
#150399=CARTESIAN_POINT('Ctrl Pts',(-9.14138216248191,83.27370133808,56.78447782593));
#150400=CARTESIAN_POINT('Ctrl Pts',(-14.2054072809149,82.2547530918,59.85623901085));
#150401=CARTESIAN_POINT('Ctrl Pts',(-13.6867239510549,82.33683162598,59.92381322088));
#150402=CARTESIAN_POINT('Ctrl Pts',(-12.6384126884581,82.58312529384,59.91562799188));
#150403=CARTESIAN_POINT('Ctrl Pts',(-11.1638044367469,83.19665457774,59.42325346353));
#150404=CARTESIAN_POINT('Ctrl Pts',(-9.99319080751591,83.9705583545,58.51591282125));
#150405=CARTESIAN_POINT('Ctrl Pts',(-9.52146541439991,84.52158459866,57.71967705271));
#150406=CARTESIAN_POINT('Ctrl Pts',(-9.36371259686991,84.79429945203,57.29416759219));
#150407=CARTESIAN_POINT('',(-13.9922553804019,82.154923079361,59.8052980196173));
#150408=CARTESIAN_POINT('Ctrl Pts',(-13.9923246930992,67.845089141546,59.8052911256481));
#150409=CARTESIAN_POINT('Ctrl Pts',(-13.8764053209202,68.222754190633,59.600327407802));
#150410=CARTESIAN_POINT('Ctrl Pts',(-13.7595941039321,68.6088595757193,
59.4119043223723));
#150411=CARTESIAN_POINT('Ctrl Pts',(-13.6461287860564,69.0017537124996,
59.2404767610183));
#150412=CARTESIAN_POINT('Ctrl Pts',(-13.5955968106831,69.1767297951989,
59.1641312003585));
#150413=CARTESIAN_POINT('Ctrl Pts',(-13.5457287368772,69.353051674383,59.0911566578527));
#150414=CARTESIAN_POINT('Ctrl Pts',(-13.4969004303597,69.530570634749,59.0215935397647));
#150415=CARTESIAN_POINT('Ctrl Pts',(-13.4891180900841,69.5588639148863,
59.0105064492183));
#150416=CARTESIAN_POINT('Ctrl Pts',(-13.4813621647634,69.5871876009258,
58.9995060170303));
#150417=CARTESIAN_POINT('Ctrl Pts',(-13.4736342771579,69.6155418053939,
58.988592346489));
#150418=CARTESIAN_POINT('Ctrl Pts',(-13.3910906412204,69.9184006525175,
58.8720205103174));
#150419=CARTESIAN_POINT('Ctrl Pts',(-13.3117448569473,70.2247423571956,
58.7653478165224));
#150420=CARTESIAN_POINT('Ctrl Pts',(-13.2375806890668,70.5346970220213,
58.6686969596893));
#150421=CARTESIAN_POINT('Ctrl Pts',(-13.2004986051266,70.6896743544342,
58.6203715312727));
#150422=CARTESIAN_POINT('Ctrl Pts',(-13.1647119249811,70.845554882444,58.574551414006));
#150423=CARTESIAN_POINT('Ctrl Pts',(-13.1304700379036,71.0023536068965,
58.5312511228961));
#150424=CARTESIAN_POINT('Ctrl Pts',(-13.1133490943649,71.0807529691228,
58.5096009773411));
#150425=CARTESIAN_POINT('Ctrl Pts',(-13.0966143490678,71.1593818761839,
58.4885807747841));
#150426=CARTESIAN_POINT('Ctrl Pts',(-13.0802970349962,71.238242167762,58.468192245751));
#150427=CARTESIAN_POINT('Ctrl Pts',(-13.0761874678052,71.2581033817783,
58.463057330187));
#150428=CARTESIAN_POINT('Ctrl Pts',(-13.0721043779997,71.2779792726429,
58.4579624813378));
#150429=CARTESIAN_POINT('Ctrl Pts',(-13.0680482612216,71.2978698640127,
58.4529077276355));
#150430=CARTESIAN_POINT('Ctrl Pts',(-13.0640518352011,71.3174677408151,
58.447927360864));
#150431=CARTESIAN_POINT('Ctrl Pts',(-13.0600815941699,71.3370798886255,
58.4429859178163));
#150432=CARTESIAN_POINT('Ctrl Pts',(-13.0561378076342,71.3567060405806,
58.4380834580827));
#150433=CARTESIAN_POINT('Ctrl Pts',(-13.0521645688323,71.3764787609788,
58.4331443866948));
#150434=CARTESIAN_POINT('Ctrl Pts',(-13.0482182337819,71.3962657675923,
58.4282448649636));
#150435=CARTESIAN_POINT('Ctrl Pts',(-13.0442990168575,71.416066703405,58.4233849750216));
#150436=CARTESIAN_POINT('Ctrl Pts',(-13.0423394083953,71.4259671713114,
58.4209550300506));
#150437=CARTESIAN_POINT('Ctrl Pts',(-13.0403865794646,71.4358711215037,
58.4185349929911));
#150438=CARTESIAN_POINT('Ctrl Pts',(-13.0384405700485,71.4457785273776,
58.4161248695553));
#150439=CARTESIAN_POINT('Ctrl Pts',(-13.0369810629863,71.453209081783,58.4143172769784));
#150440=CARTESIAN_POINT('Ctrl Pts',(-13.0355253919011,71.4606415800103,
58.4125152608173));
#150441=CARTESIAN_POINT('Ctrl Pts',(-13.0340735715475,71.4680760079362,
58.4107188242038));
#150442=CARTESIAN_POINT('Ctrl Pts',(-13.0335896314296,71.4705541505781,
58.4101200119993));
#150443=CARTESIAN_POINT('Ctrl Pts',(-13.0328644451741,71.4742724707177,
58.4092228702797));
#150444=CARTESIAN_POINT('Ctrl Pts',(-13.0326230353178,71.4755110785719,
58.4089242475553));
#150445=CARTESIAN_POINT('Ctrl Pts',(-13.020068211608,71.5399264404598,58.3933939965603));
#150446=CARTESIAN_POINT('Ctrl Pts',(-13.0065976865036,71.6098663281076,
58.3769827511436));
#150447=CARTESIAN_POINT('Ctrl Pts',(-12.9923806682185,71.6853980043269,
58.3599205519703));
#150448=CARTESIAN_POINT('Ctrl Pts',(-12.9777555181637,71.7630979887009,
58.3423685436538));
#150449=CARTESIAN_POINT('Ctrl Pts',(-12.9623398663465,71.8467157264396,
58.3241273966127));
#150450=CARTESIAN_POINT('Ctrl Pts',(-12.9463600462848,71.9363247088156,
58.305489391384));
#150451=CARTESIAN_POINT('Ctrl Pts',(-12.9315695383823,72.0192644638849,
58.2882385360829));
#150452=CARTESIAN_POINT('Ctrl Pts',(-12.916295901173,72.1073370761852,58.2706480711374));
#150453=CARTESIAN_POINT('Ctrl Pts',(-12.9007553997249,72.2005972023878,
58.2529831546617));
#150454=CARTESIAN_POINT('Ctrl Pts',(-12.8855314091007,72.2919579150175,
58.2356780166196));
#150455=CARTESIAN_POINT('Ctrl Pts',(-12.8700511587873,72.3882972254665,
58.2183014660757));
#150456=CARTESIAN_POINT('Ctrl Pts',(-12.8545549842605,72.4896595017306,
58.2011336654313));
#150457=CARTESIAN_POINT('Ctrl Pts',(-12.8393842716389,72.5888928938953,
58.1843264353971));
#150458=CARTESIAN_POINT('Ctrl Pts',(-12.8241981519655,72.6929407026516,
58.1677193130647));
#150459=CARTESIAN_POINT('Ctrl Pts',(-12.8092601655493,72.8018343625555,
58.1516045504453));
#150460=CARTESIAN_POINT('Ctrl Pts',(-12.7946393343453,72.908416051431,58.1358319277111));
#150461=CARTESIAN_POINT('Ctrl Pts',(-12.7802560776962,73.0196402207419,
58.1205310099541));
#150462=CARTESIAN_POINT('Ctrl Pts',(-12.7663963618552,73.1355232537047,
58.1060037940822));
#150463=CARTESIAN_POINT('Ctrl Pts',(-12.7527924392277,73.2492675636421,
58.0917446907225));
#150464=CARTESIAN_POINT('Ctrl Pts',(-12.739692767209,73.3675005670556,58.0782310075463));
#150465=CARTESIAN_POINT('Ctrl Pts',(-12.7274076725007,73.4902218979716,
58.0657752633181));
#150466=CARTESIAN_POINT('Ctrl Pts',(-12.7155212960257,73.608960253306,58.0537237758296));
#150467=CARTESIAN_POINT('Ctrl Pts',(-12.7043974476233,73.7319004693616,
58.0426627407316));
#150468=CARTESIAN_POINT('Ctrl Pts',(-12.6943560349518,73.8590247110285,
58.0328999656886));
#150469=CARTESIAN_POINT('Ctrl Pts',(-12.6844879572467,73.983954532757,58.0233057157666));
#150470=CARTESIAN_POINT('Ctrl Pts',(-12.6756651456058,74.112925356913,58.0149652954682));
#150471=CARTESIAN_POINT('Ctrl Pts',(-12.668230626856,74.2459006240721,58.0081946926255));
#150472=CARTESIAN_POINT('Ctrl Pts',(-12.6609684625286,74.375793126074,58.001581052645));
#150473=CARTESIAN_POINT('Ctrl Pts',(-12.6550308974448,74.5095066982876,
57.9964653132249));
#150474=CARTESIAN_POINT('Ctrl Pts',(-12.650776916749,74.6469860318338,57.9931646922056));
#150475=CARTESIAN_POINT('Ctrl Pts',(-12.6500770189875,74.6696051936677,
57.9926216485418));
#150476=CARTESIAN_POINT('Ctrl Pts',(-12.6494227842728,74.6923262418515,
57.9921277894647));
#150477=CARTESIAN_POINT('Ctrl Pts',(-12.6488159185513,74.7151488689863,
57.9916845878056));
#150478=CARTESIAN_POINT('Ctrl Pts',(-12.6474232167211,74.7675247298372,
57.9906674801653));
#150479=CARTESIAN_POINT('Ctrl Pts',(-12.6462799292503,74.8204356026201,
57.9899171327293));
#150480=CARTESIAN_POINT('Ctrl Pts',(-12.6454073095588,74.8738773989734,
57.9894516915659));
#150481=CARTESIAN_POINT('Ctrl Pts',(-12.644970999713,74.9005982971501,57.9892189709842));
#150482=CARTESIAN_POINT('Ctrl Pts',(-12.6446023568134,74.9274519262714,
57.989057484451));
#150483=CARTESIAN_POINT('Ctrl Pts',(-12.6443041376423,74.9544377155396,
57.9889695458577));
#150484=CARTESIAN_POINT('Ctrl Pts',(-12.6441550280568,74.9679306101737,
57.988925576561));
#150485=CARTESIAN_POINT('Ctrl Pts',(-12.6440235244035,74.9814565448504,
57.9888999947202));
#150486=CARTESIAN_POINT('Ctrl Pts',(-12.6439099743136,74.9950154463947,
57.9888930924319));
#150487=CARTESIAN_POINT('Ctrl Pts',(-12.6438586624004,75.0011425501131,
57.9888899733713));
#150488=CARTESIAN_POINT('Ctrl Pts',(-12.6438110165207,75.0072763857763,
57.9888906687515));
#150489=CARTESIAN_POINT('Ctrl Pts',(-12.6437670689792,75.0134169464862,
57.9888952056554));
#150490=CARTESIAN_POINT('Ctrl Pts',(-12.6437623899252,75.0140707262935,
57.9888956886953));
#150491=CARTESIAN_POINT('Ctrl Pts',(-12.6437577527944,75.0147245823336,
57.9888962152816));
#150492=CARTESIAN_POINT('Ctrl Pts',(-12.6437531576084,75.0153785146011,
57.9888967854433));
#150493=CARTESIAN_POINT('Ctrl Pts',(-12.6437292801054,75.0187764770737,
57.9888997481171));
#150494=CARTESIAN_POINT('Ctrl Pts',(-12.6437065355144,75.0221764976604,
57.9889038873487));
#150495=CARTESIAN_POINT('Ctrl Pts',(-12.6436849263525,75.025578575702,57.988909207229));
#150496=CARTESIAN_POINT('Ctrl Pts',(-12.6436741217715,75.0272796147229,
57.9889118671691));
#150497=CARTESIAN_POINT('Ctrl Pts',(-12.6436636010478,75.0289811681074,
57.9889148222715));
#150498=CARTESIAN_POINT('Ctrl Pts',(-12.6436533645941,75.0306832357554,
57.9889180730479));
#150499=CARTESIAN_POINT('Ctrl Pts',(-12.6436431281404,75.0323853034035,
57.9889213238242));
#150500=CARTESIAN_POINT('Ctrl Pts',(-12.6436266975926,75.0352291559008,
57.9889274452835));
#150501=CARTESIAN_POINT('Ctrl Pts',(-12.643623508419,75.0357909813961,57.9889287129107));
#150502=CARTESIAN_POINT('Ctrl Pts',(-12.6423924799616,75.2526569306915,
57.9894180199751));
#150503=CARTESIAN_POINT('Ctrl Pts',(-12.646472241189,75.4727189162619,57.9946990468044));
#150504=CARTESIAN_POINT('Ctrl Pts',(-12.6559493082686,75.6957106878421,
58.0051451751774));
#150505=CARTESIAN_POINT('Ctrl Pts',(-12.6590427828385,75.7684989638847,
58.0085549677011));
#150506=CARTESIAN_POINT('Ctrl Pts',(-12.6627110643347,75.8415990966006,
58.0125150142212));
#150507=CARTESIAN_POINT('Ctrl Pts',(-12.6669563732953,75.9150009409436,
58.017038073061));
#150508=CARTESIAN_POINT('Ctrl Pts',(-12.6755819223178,76.0641376027508,
58.0262279497264));
#150509=CARTESIAN_POINT('Ctrl Pts',(-12.6865899759768,76.2145202297719,
58.0377421482989));
#150510=CARTESIAN_POINT('Ctrl Pts',(-12.6999939404488,76.3660582763293,
58.0516862103691));
#150511=CARTESIAN_POINT('Ctrl Pts',(-12.7016694360078,76.385000532149,58.0534292181278));
#150512=CARTESIAN_POINT('Ctrl Pts',(-12.7033823676737,76.4039608415549,
58.0552101908413));
#150513=CARTESIAN_POINT('Ctrl Pts',(-12.7051327395416,76.4229390052955,
58.0570293311126));
#150514=CARTESIAN_POINT('Ctrl Pts',(-12.7060079254756,76.4324280871659,
58.0579389012482));
#150515=CARTESIAN_POINT('Ctrl Pts',(-12.70689247146,76.4419216326199,58.0588580132628));
#150516=CARTESIAN_POINT('Ctrl Pts',(-12.7077863808547,76.451419619682,58.0597866927244));
#150517=CARTESIAN_POINT('Ctrl Pts',(-12.7083434952166,76.4573390842646,
58.06036547696));
#150518=CARTESIAN_POINT('Ctrl Pts',(-12.7094999601304,76.4695729187318,
58.061566640817));
#150519=CARTESIAN_POINT('Ctrl Pts',(-12.7107956449714,76.4830585732496,
58.0629140215282));
#150520=CARTESIAN_POINT('Ctrl Pts',(-12.7115789315787,76.4912111210295,
58.0637285600892));
#150521=CARTESIAN_POINT('Ctrl Pts',(-12.7124127687965,76.4998212018493,
58.0645961631595));
#150522=CARTESIAN_POINT('Ctrl Pts',(-12.7131886154,76.5077712459183,58.0654037342866));
#150523=CARTESIAN_POINT('Ctrl Pts',(-12.7256079849799,76.635031628357,58.0783309343856));
#150524=CARTESIAN_POINT('Ctrl Pts',(-12.7394903374166,76.762090043741,58.0928780348764));
#150525=CARTESIAN_POINT('Ctrl Pts',(-12.7547724123643,76.8889053499444,
58.1090308435864));
#150526=CARTESIAN_POINT('Ctrl Pts',(-12.8005432353644,77.2687255611255,
58.157409571668));
#150527=CARTESIAN_POINT('Ctrl Pts',(-12.8588680406673,77.6463622141542,
58.2201931928097));
#150528=CARTESIAN_POINT('Ctrl Pts',(-12.9276269170201,78.0194570007294,
58.2966226822194));
#150529=CARTESIAN_POINT('Ctrl Pts',(-12.9713073131002,78.256472625729,58.345175982487));
#150530=CARTESIAN_POINT('Ctrl Pts',(-13.0191991737726,78.4916559317739,
58.3992359932875));
#150531=CARTESIAN_POINT('Ctrl Pts',(-13.0707644468211,78.7244116924096,
58.4586057913303));
#150532=CARTESIAN_POINT('Ctrl Pts',(-13.0726976055923,78.7331376006344,
58.4608315382147));
#150533=CARTESIAN_POINT('Ctrl Pts',(-13.0746359276518,78.7418600980509,
58.4630647476694));
#150534=CARTESIAN_POINT('Ctrl Pts',(-13.0765793757085,78.7505791898991,
58.4653054193184));
#150535=CARTESIAN_POINT('Ctrl Pts',(-13.0824690905492,78.7770028262172,
58.4720958848612));
#150536=CARTESIAN_POINT('Ctrl Pts',(-13.0885638230363,78.804051607521,58.4791276116934));
#150537=CARTESIAN_POINT('Ctrl Pts',(-13.0943656728559,78.8296253292383,
58.4858479439898));
#150538=CARTESIAN_POINT('Ctrl Pts',(-13.0974641280112,78.843282875083,58.4894369111118));
#150539=CARTESIAN_POINT('Ctrl Pts',(-13.1004785548092,78.8565200748843,
58.4929362952549));
#150540=CARTESIAN_POINT('Ctrl Pts',(-13.1033301382347,78.8690191762275,
58.4962571599057));
#150541=CARTESIAN_POINT('Ctrl Pts',(-13.1176059329182,78.9315930441025,
58.5128823028004));
#150542=CARTESIAN_POINT('Ctrl Pts',(-13.1333784860537,79.0003742996488,
58.5315864013316));
#150543=CARTESIAN_POINT('Ctrl Pts',(-13.1507809817894,79.0752552081944,
58.5526325802277));
#150544=CARTESIAN_POINT('Ctrl Pts',(-13.1688970697479,79.1532066208097,
58.5745417611787));
#150545=CARTESIAN_POINT('Ctrl Pts',(-13.1887803485302,79.2377682099706,
58.598988647045));
#150546=CARTESIAN_POINT('Ctrl Pts',(-13.2105817144596,79.3287995706086,
58.6263267340569));
#150547=CARTESIAN_POINT('Ctrl Pts',(-13.2311438855714,79.4146566870867,
58.6521109177099));
#150548=CARTESIAN_POINT('Ctrl Pts',(-13.2534130326781,79.5062687568842,
58.6804674325358));
#150549=CARTESIAN_POINT('Ctrl Pts',(-13.2775048113542,79.6035035139611,
58.7117401692531));
#150550=CARTESIAN_POINT('Ctrl Pts',(-13.3010877576402,79.6986846163658,
58.7423524075662));
#150551=CARTESIAN_POINT('Ctrl Pts',(-13.3264179061768,79.7992532799048,
58.7757591299201));
#150552=CARTESIAN_POINT('Ctrl Pts',(-13.3535821396951,79.9050736102897,
58.8123256644255));
#150553=CARTESIAN_POINT('Ctrl Pts',(-13.3797112477034,80.0068615308008,
58.8474987875301));
#150554=CARTESIAN_POINT('Ctrl Pts',(-13.4075379089805,80.1135083661954,
58.885595736518));
#150555=CARTESIAN_POINT('Ctrl Pts',(-13.4371097621925,80.2248840390139,
58.9269786555841));
#150556=CARTESIAN_POINT('Ctrl Pts',(-13.4452861746218,80.2556786405231,
58.9384207458511));
#150557=CARTESIAN_POINT('Ctrl Pts',(-13.4535957952361,80.2868347050863,
58.9501142568969));
#150558=CARTESIAN_POINT('Ctrl Pts',(-13.4620391156216,80.3183493740482,
58.9620673331119));
#150559=CARTESIAN_POINT('Ctrl Pts',(-13.4667773879387,80.3360349617922,
58.9687752308997));
#150560=CARTESIAN_POINT('Ctrl Pts',(-13.4715577618766,80.353833483865,58.9755648772567));
#150561=CARTESIAN_POINT('Ctrl Pts',(-13.4763802888604,80.3717444289602,
58.982437740821));
#150562=CARTESIAN_POINT('Ctrl Pts',(-13.4787915523522,80.3806999015078,
58.9858741726032));
#150563=CARTESIAN_POINT('Ctrl Pts',(-13.4812133541063,80.3896834796924,
58.989331408995));
#150564=CARTESIAN_POINT('Ctrl Pts',(-13.4836456974466,80.3986950992758,
58.9928096355766));
#150565=CARTESIAN_POINT('Ctrl Pts',(-13.4859012795059,80.4070518337555,
58.9960350952993));
#150566=CARTESIAN_POINT('Ctrl Pts',(-13.4893480347745,80.4198068304272,
59.0009709141936));
#150567=CARTESIAN_POINT('Ctrl Pts',(-13.4925521254936,80.431636877691,59.005569537271));
#150568=CARTESIAN_POINT('Ctrl Pts',(-13.492803217746,80.4325639529437,59.0059299136547));
#150569=CARTESIAN_POINT('Ctrl Pts',(-13.493052812368,80.4334853576126,59.0062881937997));
#150570=CARTESIAN_POINT('Ctrl Pts',(-13.4933002154167,80.4343985350018,
59.0066433787663));
#150571=CARTESIAN_POINT('Ctrl Pts',(-13.5069178845044,80.484662052657,59.0261936283159));
#150572=CARTESIAN_POINT('Ctrl Pts',(-13.520340769541,80.5338016263157,59.0456237116997));
#150573=CARTESIAN_POINT('Ctrl Pts',(-13.5335512771401,80.5818307901296,
59.0649008674955));
#150574=CARTESIAN_POINT('Ctrl Pts',(-13.5599722923383,80.6778891177573,
59.103455179087));
#150575=CARTESIAN_POINT('Ctrl Pts',(-13.5855437948394,80.7695063631374,
59.1413963752888));
#150576=CARTESIAN_POINT('Ctrl Pts',(-13.6101573960222,80.856781532072,59.1784781913009));
#150577=CARTESIAN_POINT('Ctrl Pts',(-13.6375278400217,80.9538319435956,
59.2197133507162));
#150578=CARTESIAN_POINT('Ctrl Pts',(-13.663713636453,81.0455133404965,59.2598853045842));
#150579=CARTESIAN_POINT('Ctrl Pts',(-13.6886091519591,81.1319457165426,
59.2986865949162));
#150580=CARTESIAN_POINT('Ctrl Pts',(-13.7140937239498,81.2204231818573,
59.3384059683335));
#150581=CARTESIAN_POINT('Ctrl Pts',(-13.7382267359038,81.3034002811428,
59.3766888998109));
#150582=CARTESIAN_POINT('Ctrl Pts',(-13.7609340348152,81.3809885064921,
59.4132413988346));
#150583=CARTESIAN_POINT('Ctrl Pts',(-13.7843489556299,81.4609945943934,
59.4509329742862));
#150584=CARTESIAN_POINT('Ctrl Pts',(-13.8062484160857,81.5352707244551,
59.4867843747173));
#150585=CARTESIAN_POINT('Ctrl Pts',(-13.8265845754031,81.603920991272,59.5205137510087));
#150586=CARTESIAN_POINT('Ctrl Pts',(-13.8365619933325,81.6376024938756,
59.5370622092749));
#150587=CARTESIAN_POINT('Ctrl Pts',(-13.8461635582274,81.6699295083559,
59.5531004969978));
#150588=CARTESIAN_POINT('Ctrl Pts',(-13.8553858825759,81.7009127913618,
59.5685989547995));
#150589=CARTESIAN_POINT('Ctrl Pts',(-13.8747444750509,81.7659498391365,
59.601131786788));
#150590=CARTESIAN_POINT('Ctrl Pts',(-13.8924309395384,81.825067279728,59.6312830136446));
#150591=CARTESIAN_POINT('Ctrl Pts',(-13.9084295099037,81.8783507762487,
59.6588125803306));
#150592=CARTESIAN_POINT('Ctrl Pts',(-13.9245519021174,81.9320466634317,
59.6865552136691));
#150593=CARTESIAN_POINT('Ctrl Pts',(-13.938960695333,81.9798179133721,59.7116353843609));
#150594=CARTESIAN_POINT('Ctrl Pts',(-13.9516539765085,82.0217338159453,
59.7338551629453));
#150595=CARTESIAN_POINT('Ctrl Pts',(-13.964413516165,82.0638685180553,59.756190927992));
#150596=CARTESIAN_POINT('Ctrl Pts',(-13.9754400180099,82.1000865483256,
59.7756363162688));
#150597=CARTESIAN_POINT('Ctrl Pts',(-13.9847386239781,82.1304403675663,
59.7920391319671));
#150598=CARTESIAN_POINT('Ctrl Pts',(-13.9873839817898,82.1390757171142,
59.7967055644184));
#150599=CARTESIAN_POINT('Ctrl Pts',(-13.989889515855,82.1472363414086,59.8011260517734));
#150600=CARTESIAN_POINT('Ctrl Pts',(-13.9922553804113,82.1549231907861,
59.8052978143008));
#150601=CARTESIAN_POINT('Origin',(-13.9922815033674,84.5398910545472,55.4107645820394));
#150602=CARTESIAN_POINT('Ctrl Pts',(-14.1109587916089,82.00193238136,59.72048255862));
#150603=CARTESIAN_POINT('Ctrl Pts',(-11.8622349709508,82.36472563539,59.9961606353001));
#150604=CARTESIAN_POINT('Ctrl Pts',(-10.0158495894259,83.30534179388,59.0109757487901));
#150605=CARTESIAN_POINT('Ctrl Pts',(-9.30331679897791,84.45114585728,57.15519830438));
#150606=CARTESIAN_POINT('Ctrl Pts',(-14.6029404122129,83.6144608082201,
60.57083234018));
#150607=CARTESIAN_POINT('Ctrl Pts',(-12.2714944067148,84.0386899500301,
60.94839266559));
#150608=CARTESIAN_POINT('Ctrl Pts',(-10.3832434550239,85.20823401609,60.01707148773));
#150609=CARTESIAN_POINT('Ctrl Pts',(-9.74244088945991,86.62498997905,58.17348929348));
#150610=CARTESIAN_POINT('Ctrl Pts',(-15.2156776004539,85.08666325345,61.73072156537));
#150611=CARTESIAN_POINT('Ctrl Pts',(-12.7662414190948,85.49056520221,62.21808717785));
#150612=CARTESIAN_POINT('Ctrl Pts',(-10.8233228752319,86.8784910968501,
61.36245727411));
#150613=CARTESIAN_POINT('Ctrl Pts',(-10.2896898327459,88.6055982400801,
59.56133749227));
#150614=CARTESIAN_POINT('Ctrl Pts',(-15.7859912232689,86.29753560658,63.116600358883));
#150615=CARTESIAN_POINT('Ctrl Pts',(-13.2006081304576,86.61632728226,63.627536549935));
#150616=CARTESIAN_POINT('Ctrl Pts',(-11.2038952684509,88.1916362156301,
62.86693039028));
#150617=CARTESIAN_POINT('Ctrl Pts',(-10.7995805712569,90.23163990772,61.2170704358901));
#150618=CARTESIAN_POINT('',(-15.5675364833309,86.22497216032,63.039015015514));
#150619=CARTESIAN_POINT('Ctrl Pts',(-15.5675364833309,86.2249721603231,
63.0390150155113));
#150620=CARTESIAN_POINT('Ctrl Pts',(-15.5486555635769,86.1843063248925,
62.9931377658538));
#150621=CARTESIAN_POINT('Ctrl Pts',(-15.527678303696,86.1389595646384,62.9425502180199));
#150622=CARTESIAN_POINT('Ctrl Pts',(-15.5045989540046,86.088733552719,62.887439691955));
#150623=CARTESIAN_POINT('Ctrl Pts',(-15.481592586095,86.0386663660651,62.8325034370219));
#150624=CARTESIAN_POINT('Ctrl Pts',(-15.456497073684,85.9837504650751,62.773072604199));
#150625=CARTESIAN_POINT('Ctrl Pts',(-15.4293129408974,85.9237584010294,
62.7093735960576));
#150626=CARTESIAN_POINT('Ctrl Pts',(-15.4195374529417,85.9021850919184,
62.6864672597852));
#150627=CARTESIAN_POINT('Ctrl Pts',(-15.4094919598478,85.8799550919683,
62.6630093844385));
#150628=CARTESIAN_POINT('Ctrl Pts',(-15.3991768168664,85.8570569499555,
62.6390118613801));
#150629=CARTESIAN_POINT('Ctrl Pts',(-15.3671738852249,85.7860150191872,
62.5645590795441));
#150630=CARTESIAN_POINT('Ctrl Pts',(-15.332464150594,85.7082848312241,62.4846395801313));
#150631=CARTESIAN_POINT('Ctrl Pts',(-15.2951936032702,85.6238591391515,
62.4000356000023));
#150632=CARTESIAN_POINT('Ctrl Pts',(-15.2584742717383,85.5406820677203,
62.3166828773205));
#150633=CARTESIAN_POINT('Ctrl Pts',(-15.2192688297427,85.4510049477835,
62.2287837813175));
#150634=CARTESIAN_POINT('Ctrl Pts',(-15.1777504002889,85.3548275184667,
62.1371227619183));
#150635=CARTESIAN_POINT('Ctrl Pts',(-15.1721628635966,85.341883991403,62.124787051828));
#150636=CARTESIAN_POINT('Ctrl Pts',(-15.166533491163,85.3288227570333,62.1123832542891));
#150637=CARTESIAN_POINT('Ctrl Pts',(-15.1608627590391,85.3156438405344,
62.0999133240707));
#150638=CARTESIAN_POINT('Ctrl Pts',(-15.1243771652748,85.2308504517586,
62.0196815659362));
#150639=CARTESIAN_POINT('Ctrl Pts',(-15.0897349273574,85.1493623839876,
61.9444441869956));
#150640=CARTESIAN_POINT('Ctrl Pts',(-15.0569497449735,85.071466224997,61.8739344323386));
#150641=CARTESIAN_POINT('Ctrl Pts',(-15.0233703574083,84.9916830692417,
61.8017166129884));
#150642=CARTESIAN_POINT('Ctrl Pts',(-14.991738766518,84.9156678324434,61.734457940933));
#150643=CARTESIAN_POINT('Ctrl Pts',(-14.9620493845024,84.8436821117079,
61.671892692347));
#150644=CARTESIAN_POINT('Ctrl Pts',(-14.9487644620143,84.8114711104913,
61.6438970110128));
#150645=CARTESIAN_POINT('Ctrl Pts',(-14.9358681789785,84.7800663170307,
61.616841367153));
#150646=CARTESIAN_POINT('Ctrl Pts',(-14.9233590215613,84.7494883724321,
61.5907034983332));
#150647=CARTESIAN_POINT('Ctrl Pts',(-14.8947731715385,84.6796118404519,
61.5309734003674));
#150648=CARTESIAN_POINT('Ctrl Pts',(-14.8682174376492,84.6140570837511,
61.4760349535713));
#150649=CARTESIAN_POINT('Ctrl Pts',(-14.8436927760689,84.5530433545044,
61.4256463383064));
#150650=CARTESIAN_POINT('Ctrl Pts',(-14.8391510492176,84.54174421011,61.4163148608383));
#150651=CARTESIAN_POINT('Ctrl Pts',(-14.8346789493652,84.5306006875076,
61.4071395036283));
#150652=CARTESIAN_POINT('Ctrl Pts',(-14.8302764458863,84.519614025464,61.3981188444365));
#150653=CARTESIAN_POINT('Ctrl Pts',(-14.816188756294,84.4844575093433,61.3692533938533));
#150654=CARTESIAN_POINT('Ctrl Pts',(-14.8028141038372,84.4509075776405,
61.3419717236838));
#150655=CARTESIAN_POINT('Ctrl Pts',(-14.7901524896367,84.419001923336,61.3162299894535));
#150656=CARTESIAN_POINT('Ctrl Pts',(-14.7838216825364,84.4030490961838,
61.3033591223383));
#150657=CARTESIAN_POINT('Ctrl Pts',(-14.7776691350233,84.3875072796161,
61.2908733129297));
#150658=CARTESIAN_POINT('Ctrl Pts',(-14.7716948472141,84.3723807479666,
61.2787674539506));
#150659=CARTESIAN_POINT('Ctrl Pts',(-14.7687077033096,84.3648174821419,
61.272714524461));
#150660=CARTESIAN_POINT('Ctrl Pts',(-14.7657651243324,84.3573580338555,
61.2667565871628));
#150661=CARTESIAN_POINT('Ctrl Pts',(-14.7628671103009,84.3500029141163,
61.2608930301829));
#150662=CARTESIAN_POINT('Ctrl Pts',(-14.7614181032852,84.3463253542468,
61.257961251693));
#150663=CARTESIAN_POINT('Ctrl Pts',(-14.7599802375059,84.3426738762865,
61.2550530685705));
#150664=CARTESIAN_POINT('Ctrl Pts',(-14.7585535129653,84.3390485424918,
61.2521684058551));
#150665=CARTESIAN_POINT('Ctrl Pts',(-14.7578401506951,84.3372358755944,
61.2507260744974));
#150666=CARTESIAN_POINT('Ctrl Pts',(-14.7571295737345,84.3354297447242,
61.2492896232594));
#150667=CARTESIAN_POINT('Ctrl Pts',(-14.7564217820838,84.3336301575628,
61.247859042867));
#150668=CARTESIAN_POINT('Ctrl Pts',(-14.7557139904332,84.3318305704013,
61.2464284624745));
#150669=CARTESIAN_POINT('Ctrl Pts',(-14.7555287793633,84.3313599170776,
61.2460540069098));
#150670=CARTESIAN_POINT('Ctrl Pts',(-14.7543067630621,84.3282510348247,
61.2435849050202));
#150671=CARTESIAN_POINT('Ctrl Pts',(-14.7009731122741,84.1925670507028,
61.1358234800683));
#150672=CARTESIAN_POINT('Ctrl Pts',(-14.6492756639653,84.0583603706525,
61.0330316455385));
#150673=CARTESIAN_POINT('Ctrl Pts',(-14.5992821274116,83.9259745135944,
60.934938049082));
#150674=CARTESIAN_POINT('Ctrl Pts',(-14.5480382949454,83.7902777986261,
60.8343912150441));
#150675=CARTESIAN_POINT('Ctrl Pts',(-14.4985844763709,83.656494044048,60.7387803835966));
#150676=CARTESIAN_POINT('Ctrl Pts',(-14.4509582668087,83.5249509404108,
60.6478107727522));
#150677=CARTESIAN_POINT('Ctrl Pts',(-14.4013863694749,83.388033867051,60.553124753211));
#150678=CARTESIAN_POINT('Ctrl Pts',(-14.3537943129532,83.2535442739116,
60.4634667115708));
#150679=CARTESIAN_POINT('Ctrl Pts',(-14.3081891898266,83.1218067953932,
60.3785044529254));
#150680=CARTESIAN_POINT('Ctrl Pts',(-14.2614841689706,82.98689209152,60.2914930868778));
#150681=CARTESIAN_POINT('Ctrl Pts',(-14.2168627979626,82.8548637261979,
60.2094065019078));
#150682=CARTESIAN_POINT('Ctrl Pts',(-14.1742998547136,82.7260253078505,
60.1318915570659));
#150683=CARTESIAN_POINT('Ctrl Pts',(-14.1301540233085,82.5923954725832,
60.0514938818783));
#150684=CARTESIAN_POINT('Ctrl Pts',(-14.0882223025456,82.4621972036696,
59.9760139082568));
#150685=CARTESIAN_POINT('Ctrl Pts',(-14.0484458053097,82.3357226260578,
59.9050656682173));
#150686=CARTESIAN_POINT('Ctrl Pts',(-14.0292152595889,82.274576589672,59.8707646746984));
#150687=CARTESIAN_POINT('Ctrl Pts',(-14.0104880489132,82.2143002468848,
59.8375230677923));
#150688=CARTESIAN_POINT('Ctrl Pts',(-13.9922553803942,82.1549229903178,
59.8052981836916));
#150689=CARTESIAN_POINT('Origin',(-15.5675364879071,89.9666295602638,59.722390240022));
#150690=CARTESIAN_POINT('Ctrl Pts',(-11.5022227331789,92.24059357536,63.80710267499));
#150691=CARTESIAN_POINT('Ctrl Pts',(-11.6900590068918,90.0819912782,64.9589646699191));
#150692=CARTESIAN_POINT('Ctrl Pts',(-13.3403353375583,88.35741258162,65.5284608708081));
#150693=CARTESIAN_POINT('Ctrl Pts',(-15.7224335390669,87.8306099166801,
65.263328953982));
#150694=CARTESIAN_POINT('Ctrl Pts',(-11.2606355037629,91.60559269607,62.78217333778));
#150695=CARTESIAN_POINT('Ctrl Pts',(-11.5151253257839,89.4713091151001,
64.100214239718));
#150696=CARTESIAN_POINT('Ctrl Pts',(-13.2736598773406,87.78772859478,64.744410182956));
#150697=CARTESIAN_POINT('Ctrl Pts',(-15.7260522384459,87.33074482683,64.417814013295));
#150698=CARTESIAN_POINT('Ctrl Pts',(-10.9937695135439,90.85061125927,61.83105273875));
#150699=CARTESIAN_POINT('Ctrl Pts',(-11.3301258891729,88.76446201931,63.328630671347));
#150700=CARTESIAN_POINT('Ctrl Pts',(-13.2094624536146,87.1401841301901,
64.0435746101571));
#150701=CARTESIAN_POINT('Ctrl Pts',(-15.7293652895179,86.75795515826,63.63240429366));
#150702=CARTESIAN_POINT('Ctrl Pts',(-10.7185240591989,89.96317024715,60.95778318153));
#150703=CARTESIAN_POINT('Ctrl Pts',(-11.1489392586459,87.96379513297,62.63906395814));
#150704=CARTESIAN_POINT('Ctrl Pts',(-13.1546927793252,86.41956569116,63.415047631478));
#150705=CARTESIAN_POINT('Ctrl Pts',(-15.7319333912539,86.10357629771,62.89715702778));
#150706=CARTESIAN_POINT('',(-15.5675364993575,87.7888410125626,65.1501684815529));
#150707=CARTESIAN_POINT('Ctrl Pts',(-15.5675364833309,87.78884038427,65.150168469018));
#150708=CARTESIAN_POINT('Ctrl Pts',(-15.5675364833309,87.328833019208,64.3996673554378));
#150709=CARTESIAN_POINT('Ctrl Pts',(-15.5675364833309,86.8094293099928,
63.6983716052815));
#150710=CARTESIAN_POINT('Ctrl Pts',(-15.5675364833309,86.22497216032,63.039015015514));
#150711=CARTESIAN_POINT('Origin',(-16.3445396268156,91.9999999945638,62.5690047661622));
#150712=CARTESIAN_POINT('Ctrl Pts',(-15.7267915542099,87.66538353981,64.99088137144));
#150713=CARTESIAN_POINT('Ctrl Pts',(-15.1845773178949,87.78121626868,65.060886705648));
#150714=CARTESIAN_POINT('Ctrl Pts',(-14.1051711636669,88.17293046477,65.106337310483));
#150715=CARTESIAN_POINT('Ctrl Pts',(-12.6905091996054,89.25086782998,64.83687208802));
#150716=CARTESIAN_POINT('Ctrl Pts',(-11.7187169000773,90.65190225521,64.266801370723));
#150717=CARTESIAN_POINT('Ctrl Pts',(-11.4633132605639,91.64600275828,63.752208112914));
#150718=CARTESIAN_POINT('Ctrl Pts',(-11.4262749273969,92.13114438891,63.478854086617));
#150719=CARTESIAN_POINT('Ctrl Pts',(-15.7174241139459,88.05181590963,65.61349528));
#150720=CARTESIAN_POINT('Ctrl Pts',(-15.2062704666909,88.16374583963,65.647308160843));
#150721=CARTESIAN_POINT('Ctrl Pts',(-14.2055312081989,88.52845110996,65.63754881954));
#150722=CARTESIAN_POINT('Ctrl Pts',(-12.8992702356658,89.4999792018,65.370181293364));
#150723=CARTESIAN_POINT('Ctrl Pts',(-11.9627691347456,90.7694986187,64.885655521381));
#150724=CARTESIAN_POINT('Ctrl Pts',(-11.6664290226336,91.70187766148,64.460214669977));
#150725=CARTESIAN_POINT('Ctrl Pts',(-11.5979936003541,92.16979109083,64.231872652613));
#150726=CARTESIAN_POINT('Ctrl Pts',(-15.7002731834799,88.72433014467,66.888180925632));
#150727=CARTESIAN_POINT('Ctrl Pts',(-15.2467616864919,88.82578365824,66.877587073637));
#150728=CARTESIAN_POINT('Ctrl Pts',(-14.3761051926899,89.1399254789,66.809235364743));
#150729=CARTESIAN_POINT('Ctrl Pts',(-13.2334233981792,89.94290089811,66.564598469622));
#150730=CARTESIAN_POINT('Ctrl Pts',(-12.3569947409571,90.99911738926,66.202850988947));
#150731=CARTESIAN_POINT('Ctrl Pts',(-12.0079448863869,91.80959396061,65.90398707677));
#150732=CARTESIAN_POINT('Ctrl Pts',(-11.8932535301169,92.23267100316,65.743127847465));
#150733=CARTESIAN_POINT('Ctrl Pts',(-15.6809296656369,89.45528966985,68.910358690794));
#150734=CARTESIAN_POINT('Ctrl Pts',(-15.2932117620329,89.54407252558,68.883763974286));
#150735=CARTESIAN_POINT('Ctrl Pts',(-14.5550938790869,89.80455055827,68.80807416969));
#150736=CARTESIAN_POINT('Ctrl Pts',(-13.5661328446367,90.4424335221,68.627789664249));
#150737=CARTESIAN_POINT('Ctrl Pts',(-12.7529607721535,91.28077197666,68.393673986953));
#150738=CARTESIAN_POINT('Ctrl Pts',(-12.365961770199,91.94231120585,68.209964343349));
#150739=CARTESIAN_POINT('Ctrl Pts',(-12.2119022262506,92.29761959052,68.111340150659));
#150740=CARTESIAN_POINT('Ctrl Pts',(-15.6718240232689,89.80966270923,70.589751969638));
#150741=CARTESIAN_POINT('Ctrl Pts',(-15.3151883355199,89.89024839345,70.568499736441));
#150742=CARTESIAN_POINT('Ctrl Pts',(-14.6374346715909,90.12243854682,70.515386313769));
#150743=CARTESIAN_POINT('Ctrl Pts',(-13.7177800255529,90.68309838244,70.403740151492));
#150744=CARTESIAN_POINT('Ctrl Pts',(-12.9367806317871,91.42083571917,70.266639480233));
#150745=CARTESIAN_POINT('Ctrl Pts',(-12.5380437113516,92.01029521624,70.162098655781));
#150746=CARTESIAN_POINT('Ctrl Pts',(-12.3689259125356,92.33083134343,70.106261328233));
#150747=CARTESIAN_POINT('Ctrl Pts',(-15.6681569363979,89.95256484147,71.952924446791));
#150748=CARTESIAN_POINT('Ctrl Pts',(-15.3240566546889,90.03018842994,71.942882594526));
#150749=CARTESIAN_POINT('Ctrl Pts',(-14.6702901207359,90.251604718,71.91857740059));
#150750=CARTESIAN_POINT('Ctrl Pts',(-13.7779625535849,90.781902689,71.869267078615));
#150751=CARTESIAN_POINT('Ctrl Pts',(-13.0100009538581,91.47919210506,71.809754343234));
#150752=CARTESIAN_POINT('Ctrl Pts',(-12.6072845252056,92.03865965686,71.7647747764));
#150753=CARTESIAN_POINT('Ctrl Pts',(-12.4326146758588,92.34428924054,71.740780477213));
#150754=CARTESIAN_POINT('Ctrl Pts',(-15.6672518258989,89.98826649279,72.9901833001568));
#150755=CARTESIAN_POINT('Ctrl Pts',(-15.3262479221849,90.06523849532,72.9901967080605));
#150756=CARTESIAN_POINT('Ctrl Pts',(-14.6783580903999,90.28411411107,72.9902284801791));
#150757=CARTESIAN_POINT('Ctrl Pts',(-13.7927252046839,90.80698987221,72.9902913584466));
#150758=CARTESIAN_POINT('Ctrl Pts',(-13.0280722247757,91.49419551439,72.9903661930626));
#150759=CARTESIAN_POINT('Ctrl Pts',(-12.6245703572795,92.04598973457,72.9904222000122));
#150760=CARTESIAN_POINT('Ctrl Pts',(-12.448659862507,92.34772444263,72.99045196511));
#150761=CARTESIAN_POINT('Ctrl Pts',(-15.6681623130659,89.95235479387,74.027597348738));
#150762=CARTESIAN_POINT('Ctrl Pts',(-15.3240436488079,90.02998313099,74.037661924352));
#150763=CARTESIAN_POINT('Ctrl Pts',(-14.6702420088379,90.25141581468,74.062025563468));
#150764=CARTESIAN_POINT('Ctrl Pts',(-13.7778744578779,90.78175855909,74.111462545138));
#150765=CARTESIAN_POINT('Ctrl Pts',(-13.0098936682318,91.4791070426,74.171133610375));
#150766=CARTESIAN_POINT('Ctrl Pts',(-12.607182956015,92.03861824211,74.216235762356));
#150767=CARTESIAN_POINT('Ctrl Pts',(-12.432521229246,92.34426951449,74.240296059607));
#150768=CARTESIAN_POINT('Ctrl Pts',(-15.6718394519489,89.80906885625,75.391194076941));
#150769=CARTESIAN_POINT('Ctrl Pts',(-15.3151510595369,89.88966890827,75.412453916529));
#150770=CARTESIAN_POINT('Ctrl Pts',(-14.6372958155469,90.1219072658,75.465606188341));
#150771=CARTESIAN_POINT('Ctrl Pts',(-13.7175254778809,90.68269626983,75.577380462654));
#150772=CARTESIAN_POINT('Ctrl Pts',(-12.9364725952808,91.42060127026,75.714668403773));
#150773=CARTESIAN_POINT('Ctrl Pts',(-12.5377553500737,92.0101813717,75.81936657303));
#150774=CARTESIAN_POINT('Ctrl Pts',(-12.3686628267388,92.33077602559,75.87529036582));
#150775=CARTESIAN_POINT('Ctrl Pts',(-15.6809458928869,89.45463784939,77.069912031792));
#150776=CARTESIAN_POINT('Ctrl Pts',(-15.2931726928849,89.54342942527,77.096526733112));
#150777=CARTESIAN_POINT('Ctrl Pts',(-14.5549455048969,89.80395021696,77.172266998453));
#150778=CARTESIAN_POINT('Ctrl Pts',(-13.5658570450709,90.44197313334,77.35265505278));
#150779=CARTESIAN_POINT('Ctrl Pts',(-12.7526266818154,91.28050419446,77.586890412431));
#150780=CARTESIAN_POINT('Ctrl Pts',(-12.365650677397,91.94218456205,77.770681920663));
#150781=CARTESIAN_POINT('Ctrl Pts',(-12.211619215407,92.29756139639,77.869346462264));
#150782=CARTESIAN_POINT('Ctrl Pts',(-15.7003066117399,88.72316214521,79.091611819645));
#150783=CARTESIAN_POINT('Ctrl Pts',(-15.2466816366939,88.82465310407,79.102078446305));
#150784=CARTESIAN_POINT('Ctrl Pts',(-14.3757920120989,89.13890937863,79.170256649061));
#150785=CARTESIAN_POINT('Ctrl Pts',(-13.2328406131236,89.94217161033,79.414894179539));
#150786=CARTESIAN_POINT('Ctrl Pts',(-12.3563116572606,90.9987279413,79.776886348901));
#150787=CARTESIAN_POINT('Ctrl Pts',(-12.0073443151488,91.80940467908,80.076051130249));
#150788=CARTESIAN_POINT('Ctrl Pts',(-11.8927306981703,92.23256005291,80.237086753741));
#150789=CARTESIAN_POINT('Ctrl Pts',(-15.7174479046779,88.05101812102,80.365575459028));
#150790=CARTESIAN_POINT('Ctrl Pts',(-15.2062142531389,88.1629537179,80.331694444122));
#150791=CARTESIAN_POINT('Ctrl Pts',(-14.2052953457019,88.5277087746,80.341352247073));
#150792=CARTESIAN_POINT('Ctrl Pts',(-12.8988133540273,89.49944296395,80.608734946825));
#150793=CARTESIAN_POINT('Ctrl Pts',(-11.9622504742339,90.76922852031,81.093440879978));
#150794=CARTESIAN_POINT('Ctrl Pts',(-11.665999801153,91.70174993568,81.519067946853));
#150795=CARTESIAN_POINT('Ctrl Pts',(-11.5976314399642,92.16971323709,81.747505318717));
#150796=CARTESIAN_POINT('Ctrl Pts',(-15.7267824555559,87.66570882409,80.986365678153));
#150797=CARTESIAN_POINT('Ctrl Pts',(-15.1845987207689,87.78153852098,80.916388892872));
#150798=CARTESIAN_POINT('Ctrl Pts',(-14.1052629937929,88.17323107872,80.870980798031));
#150799=CARTESIAN_POINT('Ctrl Pts',(-12.6906903789146,89.25108309886,81.14044110218));
#150800=CARTESIAN_POINT('Ctrl Pts',(-11.7189248514002,90.65200916615,81.71043962589));
#150801=CARTESIAN_POINT('Ctrl Pts',(-11.4634863537649,91.64605341585,82.224957584013));
#150802=CARTESIAN_POINT('Ctrl Pts',(-11.4264213925879,92.13117626492,82.498272907329));
#150803=CARTESIAN_POINT('',(-15.5675364993592,87.78884101254,80.8276102916413));
#150804=CARTESIAN_POINT('Ctrl Pts',(-15.5675364833309,87.7888410162132,
65.1501684793153));
#150805=CARTESIAN_POINT('Ctrl Pts',(-15.5675364833309,88.5016858245549,
66.3131718584543));
#150806=CARTESIAN_POINT('Ctrl Pts',(-15.5675364833309,89.0620994148936,
67.596770803385));
#150807=CARTESIAN_POINT('Ctrl Pts',(-15.5675364833309,89.8115874451887,
70.2378326687398));
#150808=CARTESIAN_POINT('Ctrl Pts',(-15.5675364833619,90.0000184154843,
71.6068563101325));
#150809=CARTESIAN_POINT('Ctrl Pts',(-15.5675364833619,89.9999816132753,
74.3712619372165));
#150810=CARTESIAN_POINT('Ctrl Pts',(-15.5675364832921,89.811422786206,75.7411963040703));
#150811=CARTESIAN_POINT('Ctrl Pts',(-15.5675364832921,89.0616726097933,
78.3818709723929));
#150812=CARTESIAN_POINT('Ctrl Pts',(-15.5675364833309,88.5006006367192,
79.6663773945077));
#150813=CARTESIAN_POINT('Ctrl Pts',(-15.5675364833309,87.7888410161944,
80.8276102938811));
#150814=CARTESIAN_POINT('Origin',(-16.3445396396806,92.0000000244254,83.4087739660212));
#150815=CARTESIAN_POINT('Ctrl Pts',(-10.7183277173379,89.96254449809,85.02062304992));
#150816=CARTESIAN_POINT('Ctrl Pts',(-11.1488047984589,87.9632262939201,
83.33921133143));
#150817=CARTESIAN_POINT('Ctrl Pts',(-13.1546497038193,86.4190502843901,
82.56318175446));
#150818=CARTESIAN_POINT('Ctrl Pts',(-15.7319351985739,86.1031085662,83.08114725601));
#150819=CARTESIAN_POINT('Ctrl Pts',(-10.9910678175989,90.84201858798,84.15530458801));
#150820=CARTESIAN_POINT('Ctrl Pts',(-11.3283473228609,88.7567304713001,
82.655879963167));
#150821=CARTESIAN_POINT('Ctrl Pts',(-13.2089159040691,87.13321591558,81.940328764438));
#150822=CARTESIAN_POINT('Ctrl Pts',(-15.7293910876869,86.75161252054,82.352567470474));
#150823=CARTESIAN_POINT('Ctrl Pts',(-11.2584139392769,91.59984702698,83.20508981628));
#150824=CARTESIAN_POINT('Ctrl Pts',(-11.5134937823379,89.46571522905,81.885572719919));
#150825=CARTESIAN_POINT('Ctrl Pts',(-13.2730319216979,87.78250254906,81.240664946913));
#150826=CARTESIAN_POINT('Ctrl Pts',(-15.7260859252379,87.32621487051,81.5677500443391));
#150827=CARTESIAN_POINT('Ctrl Pts',(-11.5024576829089,92.24121677999,82.169685215265));
#150828=CARTESIAN_POINT('Ctrl Pts',(-11.6902236879789,90.08258370557,81.017989950019));
#150829=CARTESIAN_POINT('Ctrl Pts',(-13.3403958339806,88.3579608586,80.44856560492));
#150830=CARTESIAN_POINT('Ctrl Pts',(-15.7224300293849,87.83109219926,80.713633689592));
#150831=CARTESIAN_POINT('',(-15.5675240107059,86.2249740704557,82.9387616027241));
#150832=CARTESIAN_POINT('Ctrl Pts',(-15.5675364833309,86.22497407053,82.93876160279));
#150833=CARTESIAN_POINT('Ctrl Pts',(-15.5675364833309,86.8043943602553,
82.2850871081574));
#150834=CARTESIAN_POINT('Ctrl Pts',(-15.5675364833309,87.3248780563056,
81.5845639231394));
#150835=CARTESIAN_POINT('Ctrl Pts',(-15.5675364833309,87.78884038418,80.827610304179));
#150836=CARTESIAN_POINT('Origin',(-15.5675364833255,89.9666295470783,86.2553885480238));
#150837=CARTESIAN_POINT('Ctrl Pts',(-15.7859374982469,86.2973478690701,
82.861383624054));
#150838=CARTESIAN_POINT('Ctrl Pts',(-13.2002732600763,86.61616439017,82.350395801636));
#150839=CARTESIAN_POINT('Ctrl Pts',(-11.2034697254169,88.19169796552,83.11121227181));
#150840=CARTESIAN_POINT('Ctrl Pts',(-10.7994091717259,90.2318522534,84.7613320424801));
#150841=CARTESIAN_POINT('Ctrl Pts',(-15.2200740724969,85.09597491677,84.23663134082));
#150842=CARTESIAN_POINT('Ctrl Pts',(-12.7693205182124,85.4992514263,83.74901632494));
#150843=CARTESIAN_POINT('Ctrl Pts',(-10.8258933224819,86.88885596641,84.6041155294301));
#150844=CARTESIAN_POINT('Ctrl Pts',(-10.2935001377599,88.61860858417,86.40429721952));
#150845=CARTESIAN_POINT('Ctrl Pts',(-14.6041660747529,83.61843798049,85.4050021444));
#150846=CARTESIAN_POINT('Ctrl Pts',(-12.2722897776884,84.0430132881801,
85.02702776225));
#150847=CARTESIAN_POINT('Ctrl Pts',(-10.3838362619649,85.2133039136001,
85.9584263883601));
#150848=CARTESIAN_POINT('Ctrl Pts',(-9.74335915314091,86.6307185139801,
87.80238251479));
#150849=CARTESIAN_POINT('Ctrl Pts',(-14.1110631602029,82.00217154684,86.2571636203899));
#150850=CARTESIAN_POINT('Ctrl Pts',(-11.8620763883538,82.3649964618,85.98143506887));
#150851=CARTESIAN_POINT('Ctrl Pts',(-10.0155685768139,83.30578341605,86.96682116639));
#150852=CARTESIAN_POINT('Ctrl Pts',(-9.30321403080992,84.45174593576,88.82286146045));
#150853=CARTESIAN_POINT('',(-13.9922632538737,82.1549216119811,86.172481390843));
#150854=CARTESIAN_POINT('Ctrl Pts',(-13.9922632538719,82.1549215895872,
86.1724813495793));
#150855=CARTESIAN_POINT('Ctrl Pts',(-14.0172691520505,82.2363556855938,
86.1282859153393));
#150856=CARTESIAN_POINT('Ctrl Pts',(-14.0444951537761,82.3230603988622,
86.0802579897279));
#150857=CARTESIAN_POINT('Ctrl Pts',(-14.0739412590485,82.4148321534633,
86.0280712679699));
#150858=CARTESIAN_POINT('Ctrl Pts',(-14.103239727916,82.5061437843298,85.9761461991509));
#150859=CARTESIAN_POINT('Ctrl Pts',(-14.1347360939012,82.6024720216257,
85.9201036981764));
#150860=CARTESIAN_POINT('Ctrl Pts',(-14.168430357004,82.7035774847945,85.8595884326989));
#150861=CARTESIAN_POINT('Ctrl Pts',(-14.2017860834929,82.8036671103104,
85.7996811826869));
#150862=CARTESIAN_POINT('Ctrl Pts',(-14.2372957630783,82.9084386673946,
85.7353903085883));
#150863=CARTESIAN_POINT('Ctrl Pts',(-14.2749593957603,83.0176183202769,
85.6663416728384));
#150864=CARTESIAN_POINT('Ctrl Pts',(-14.3123467036225,83.1259969604646,
85.5977996226319));
#150865=CARTESIAN_POINT('Ctrl Pts',(-14.3518564749289,83.238719492333,85.5245690663092));
#150866=CARTESIAN_POINT('Ctrl Pts',(-14.3934887096795,83.3554734177915,
85.4462592520283));
#150867=CARTESIAN_POINT('Ctrl Pts',(-14.4345893697325,83.4707365889582,
85.3689493244002));
#150868=CARTESIAN_POINT('Ctrl Pts',(-14.4777586385691,83.5899290508293,
85.2866886767035));
#150869=CARTESIAN_POINT('Ctrl Pts',(-14.5229965161894,83.7127033399285,
85.1990818711561));
#150870=CARTESIAN_POINT('Ctrl Pts',(-14.5440862344572,83.7699402242351,
85.1582399275344));
#150871=CARTESIAN_POINT('Ctrl Pts',(-14.565625541519,83.8279548927639,85.1162358101079));
#150872=CARTESIAN_POINT('Ctrl Pts',(-14.587614437375,83.8867084182141,85.0730283087226));
#150873=CARTESIAN_POINT('Ctrl Pts',(-14.6338638705101,84.0102852119087,
84.982149600699));
#150874=CARTESIAN_POINT('Ctrl Pts',(-14.6821022426349,84.1371339331067,
84.8859477694956));
#150875=CARTESIAN_POINT('Ctrl Pts',(-14.7323295537493,84.2668559002324,
84.7840316800976));
#150876=CARTESIAN_POINT('Ctrl Pts',(-14.7818901728027,84.3948560032224,
84.6834683736019));
#150877=CARTESIAN_POINT('Ctrl Pts',(-14.8333872809171,84.5256537143705,
84.5773411252745));
#150878=CARTESIAN_POINT('Ctrl Pts',(-14.8868208780926,84.6588157333711,
84.4652685467848));
#150879=CARTESIAN_POINT('Ctrl Pts',(-14.9390948549763,84.7890878593552,
84.3556281765504));
#150880=CARTESIAN_POINT('Ctrl Pts',(-14.9932221812818,84.9216228153263,
84.240297357683));
#150881=CARTESIAN_POINT('Ctrl Pts',(-15.0492028570091,85.0559653865393,
84.1189190426377));
#150882=CARTESIAN_POINT('Ctrl Pts',(-15.1044724993146,85.1886016178975,
83.9990824031357));
#150883=CARTESIAN_POINT('Ctrl Pts',(-15.1615487097392,85.322999912876,83.8733505427342));
#150884=CARTESIAN_POINT('Ctrl Pts',(-15.220431488283,85.4586724985529,83.7413853557963));
#150885=CARTESIAN_POINT('Ctrl Pts',(-15.2780845139391,85.5915115944024,
83.612176230541));
#150886=CARTESIAN_POINT('Ctrl Pts',(-15.3374694361964,85.7255722855737,
83.476991071888));
#150887=CARTESIAN_POINT('Ctrl Pts',(-15.3985862550548,85.8603485292922,
83.3355231300881));
#150888=CARTESIAN_POINT('Ctrl Pts',(-15.4535006297584,85.9814469975525,
83.2084120711414));
#150889=CARTESIAN_POINT('Ctrl Pts',(-15.5098132149755,86.1031225912152,
83.0762286641304));
#150890=CARTESIAN_POINT('Ctrl Pts',(-15.5675240107059,86.2249740704557,
82.9387616027241));
#150891=CARTESIAN_POINT('Origin',(-13.9922815003769,84.5398910501458,90.5670141919346));
#150892=CARTESIAN_POINT('Ctrl Pts',(-9.36316543113591,65.20514258604,88.68507306022));
#150893=CARTESIAN_POINT('Ctrl Pts',(-9.52089785507191,65.47810818538,88.25909049769));
#150894=CARTESIAN_POINT('Ctrl Pts',(-9.99271929691491,66.02944859918,87.46229833598));
#150895=CARTESIAN_POINT('Ctrl Pts',(-11.1638051091349,66.80362315008,86.55460492855));
#150896=CARTESIAN_POINT('Ctrl Pts',(-12.6378577027299,67.41687862472,86.06242162813));
#150897=CARTESIAN_POINT('Ctrl Pts',(-13.6855439527219,67.66310267119,86.05405719771));
#150898=CARTESIAN_POINT('Ctrl Pts',(-14.2037341389189,67.74518306757,86.12140353019));
#150899=CARTESIAN_POINT('Ctrl Pts',(-9.24767657508891,65.99401553665,88.94968435057));
#150900=CARTESIAN_POINT('Ctrl Pts',(-9.42115179510191,66.24144787729,88.5312692084));
#150901=CARTESIAN_POINT('Ctrl Pts',(-9.91247134952491,66.7389817684,87.75513773229));
#150902=CARTESIAN_POINT('Ctrl Pts',(-11.0704798546419,67.43983090513,86.87706862433));
#150903=CARTESIAN_POINT('Ctrl Pts',(-12.5011304605781,68.00629583084,86.3973053855));
#150904=CARTESIAN_POINT('Ctrl Pts',(-13.5150380396702,68.2467475693,86.38291437305));
#150905=CARTESIAN_POINT('Ctrl Pts',(-14.0186219503789,68.33174743894,86.44526609955));
#150906=CARTESIAN_POINT('Ctrl Pts',(-9.02110732129691,67.56711094663,89.39524706291));
#150907=CARTESIAN_POINT('Ctrl Pts',(-9.21938651903491,67.76671680646,88.99421222644));
#150908=CARTESIAN_POINT('Ctrl Pts',(-9.73855112510891,68.16487519537,88.25989487261));
#150909=CARTESIAN_POINT('Ctrl Pts',(-10.8679585310409,68.72847140715,87.43449506428));
#150910=CARTESIAN_POINT('Ctrl Pts',(-12.2214087371635,69.19888773049,86.97204043524));
#150911=CARTESIAN_POINT('Ctrl Pts',(-13.1759013667977,69.41622377861,86.94116396896));
#150912=CARTESIAN_POINT('Ctrl Pts',(-13.6534062038449,69.49967595943,86.99087839766));
#150913=CARTESIAN_POINT('Ctrl Pts',(-8.63390385764391,70.79440049297,90.01976900704));
#150914=CARTESIAN_POINT('Ctrl Pts',(-8.86287624955991,70.90266434284,89.65283473253));
#150915=CARTESIAN_POINT('Ctrl Pts',(-9.41039510203091,71.11616478701,88.99091950633));
#150916=CARTESIAN_POINT('Ctrl Pts',(-10.4863410151329,71.4218057268,88.24450783708));
#150917=CARTESIAN_POINT('Ctrl Pts',(-11.7226579851006,71.69058989452,87.79963352365));
#150918=CARTESIAN_POINT('Ctrl Pts',(-12.5878203220936,71.83087932662,87.73316725532));
#150919=CARTESIAN_POINT('Ctrl Pts',(-13.0250798682975,71.89078018955,87.75627315149));
#150920=CARTESIAN_POINT('Ctrl Pts',(-8.43646722755891,74.17704539539,90.27567271427));
#150921=CARTESIAN_POINT('Ctrl Pts',(-8.67457228700691,74.19840452429,89.9271492125));
#150922=CARTESIAN_POINT('Ctrl Pts',(-9.22633231332491,74.24043774156,89.30069277592));
#150923=CARTESIAN_POINT('Ctrl Pts',(-10.2725773694299,74.30035154213,88.5884829841));
#150924=CARTESIAN_POINT('Ctrl Pts',(-11.4566903832199,74.35277043018,88.14814037352));
#150925=CARTESIAN_POINT('Ctrl Pts',(-12.2830364939517,74.37997779971,88.06199406937));
#150926=CARTESIAN_POINT('Ctrl Pts',(-12.7024212510194,74.39158580279,88.07026937053));
#150927=CARTESIAN_POINT('Ctrl Pts',(-8.53644251351991,77.54566405391,90.14553315307));
#150928=CARTESIAN_POINT('Ctrl Pts',(-8.76988752817891,77.47982485493,89.78750600586));
#150929=CARTESIAN_POINT('Ctrl Pts',(-9.31940153097191,77.35014255379,89.14272588511));
#150930=CARTESIAN_POINT('Ctrl Pts',(-10.3807195496239,77.16495136756,88.41288548734));
#150931=CARTESIAN_POINT('Ctrl Pts',(-11.5914114362027,77.00256835126,87.97038907049));
#150932=CARTESIAN_POINT('Ctrl Pts',(-12.4374024314265,76.91808082036,87.89458815261));
#150933=CARTESIAN_POINT('Ctrl Pts',(-12.8657678794545,76.88202065256,87.91059102918));
#150934=CARTESIAN_POINT('Ctrl Pts',(-8.80312062497391,80.92213477605,89.75884753243));
#150935=CARTESIAN_POINT('Ctrl Pts',(-9.01991246902491,80.76692328379,89.3769250268));
#150936=CARTESIAN_POINT('Ctrl Pts',(-9.55697366388391,80.45923627782,88.68389914341));
#150937=CARTESIAN_POINT('Ctrl Pts',(-10.6566609744259,80.02082628925,87.90432815957));
#150938=CARTESIAN_POINT('Ctrl Pts',(-11.9426748847909,79.64382527526,87.45249436166));
#150939=CARTESIAN_POINT('Ctrl Pts',(-12.8456722144415,79.45666656147,87.40161797299));
#150940=CARTESIAN_POINT('Ctrl Pts',(-13.3001072668101,79.37996389478,87.4364636821));
#150941=CARTESIAN_POINT('Ctrl Pts',(-9.14077283870391,83.27442601644,89.19463338426));
#150942=CARTESIAN_POINT('Ctrl Pts',(-9.32880949855891,83.05062855214,88.78323786731));
#150943=CARTESIAN_POINT('Ctrl Pts',(-9.83816023022091,82.60292058201,88.0262405068));
#150944=CARTESIAN_POINT('Ctrl Pts',(-10.9840980004039,81.97007306255,87.17553264096));
#150945=CARTESIAN_POINT('Ctrl Pts',(-12.3746508960291,81.44717623679,86.70717184874));
#150946=CARTESIAN_POINT('Ctrl Pts',(-13.3573195647392,81.21230060616,86.68714707239));
#150947=CARTESIAN_POINT('Ctrl Pts',(-13.8473824995259,81.12471571508,86.74485486738));
#150948=CARTESIAN_POINT('Ctrl Pts',(-9.36320138448591,84.79518333694,88.68499094841));
#150949=CARTESIAN_POINT('Ctrl Pts',(-9.52093025095291,84.52220867034,88.25900375063));
#150950=CARTESIAN_POINT('Ctrl Pts',(-9.99274691583191,83.97084828236,87.46220423853));
#150951=CARTESIAN_POINT('Ctrl Pts',(-11.1638314564909,83.19663902225,86.55450907384));
#150952=CARTESIAN_POINT('Ctrl Pts',(-12.6378886830788,82.58334687056,86.0623326859));
#150953=CARTESIAN_POINT('Ctrl Pts',(-13.6855831157209,82.33710070822,86.05397688329));
#150954=CARTESIAN_POINT('Ctrl Pts',(-14.2037786680419,82.25501069724,86.1213279171));
#150955=CARTESIAN_POINT('',(-13.992300447329,67.8450850046154,86.1724849817789));
#150956=CARTESIAN_POINT('Ctrl Pts',(-13.9922632538719,82.1549215895871,
86.1724813495793));
#150957=CARTESIAN_POINT('Ctrl Pts',(-13.9285551321236,81.9479298053255,
86.2848187148616));
#150958=CARTESIAN_POINT('Ctrl Pts',(-13.8647015765576,81.7390803248916,
86.3918585032908));
#150959=CARTESIAN_POINT('Ctrl Pts',(-13.8013730345312,81.5283495129631,
86.4937275061797));
#150960=CARTESIAN_POINT('Ctrl Pts',(-13.7378365702042,81.3169268228726,
86.5959309686469));
#150961=CARTESIAN_POINT('Ctrl Pts',(-13.6748285725588,81.1036100174599,
86.6929298523649));
#150962=CARTESIAN_POINT('Ctrl Pts',(-13.6130261143607,80.8883458651168,
86.7848084561006));
#150963=CARTESIAN_POINT('Ctrl Pts',(-13.5511371714079,80.6727804777106,
86.8768156323676));
#150964=CARTESIAN_POINT('Ctrl Pts',(-13.4904571442642,80.4552618660574,
86.9636883768117));
#150965=CARTESIAN_POINT('Ctrl Pts',(-13.4316659521088,80.2357134520804,
87.0454645259126));
#150966=CARTESIAN_POINT('Ctrl Pts',(-13.3830763136172,80.0542614747445,
87.1130507301784));
#150967=CARTESIAN_POINT('Ctrl Pts',(-13.3357768744825,79.8714224756304,
87.1771548191785));
#150968=CARTESIAN_POINT('Ctrl Pts',(-13.2901514758223,79.6871444536011,
87.2377727418144));
#150969=CARTESIAN_POINT('Ctrl Pts',(-13.2637884122878,79.5806657521444,
87.2727987184132));
#150970=CARTESIAN_POINT('Ctrl Pts',(-13.2379850470338,79.4737055706827,
87.3066606315146));
#150971=CARTESIAN_POINT('Ctrl Pts',(-13.2128161597323,79.3662528131415,
87.3393540609985));
#150972=CARTESIAN_POINT('Ctrl Pts',(-13.2096700488196,79.3528212184489,
87.343440739684));
#150973=CARTESIAN_POINT('Ctrl Pts',(-13.2065338516249,79.3393819268051,
87.3475091572638));
#150974=CARTESIAN_POINT('Ctrl Pts',(-13.203407714876,79.3259349166383,87.3515593019199));
#150975=CARTESIAN_POINT('Ctrl Pts',(-13.2005271915918,79.3135444075215,
87.3552912359084));
#150976=CARTESIAN_POINT('Ctrl Pts',(-13.1986999886115,79.3056588058398,
87.3576538209563));
#150977=CARTESIAN_POINT('Ctrl Pts',(-13.1966065603476,79.2966138895657,
87.3603579644251));
#150978=CARTESIAN_POINT('Ctrl Pts',(-13.1964280600827,79.2958426570481,
87.3605885385192));
#150979=CARTESIAN_POINT('Ctrl Pts',(-13.1962476242391,79.2950629873024,
87.3608215676654));
#150980=CARTESIAN_POINT('Ctrl Pts',(-13.1960644347913,79.29427136435,87.3610580972974));
#150981=CARTESIAN_POINT('Ctrl Pts',(-13.1914012110925,79.2741200130764,
87.3670791350732));
#150982=CARTESIAN_POINT('Ctrl Pts',(-13.1867535809486,79.2539526669486,
87.3730587869752));
#150983=CARTESIAN_POINT('Ctrl Pts',(-13.1821220625226,79.2337692755917,
87.3789970206825));
#150984=CARTESIAN_POINT('Ctrl Pts',(-13.1728590256707,79.1934024928777,
87.3908734880971));
#150985=CARTESIAN_POINT('Ctrl Pts',(-13.1636604356901,79.1529715301373,
87.4025842891849));
#150986=CARTESIAN_POINT('Ctrl Pts',(-13.1545307716034,79.1124748055347,
87.4141294529997));
#150987=CARTESIAN_POINT('Ctrl Pts',(-13.1180121152563,78.9504879071245,
87.460310108259));
#150988=CARTESIAN_POINT('Ctrl Pts',(-13.0825962732094,78.7874487141038,
87.5038416215084));
#150989=CARTESIAN_POINT('Ctrl Pts',(-13.0485477163981,78.6233237291505,
87.5446966521965));
#150990=CARTESIAN_POINT('Ctrl Pts',(-13.0031366693941,78.4044278902592,
87.5991855907208));
#150991=CARTESIAN_POINT('Ctrl Pts',(-12.9601460565636,78.1836558297552,
87.6488934074955));
#150992=CARTESIAN_POINT('Ctrl Pts',(-12.9200620632149,77.9614407620136,
87.6936460528116));
#150993=CARTESIAN_POINT('Ctrl Pts',(-12.9000372409868,77.8504284387346,
87.716003200686));
#150994=CARTESIAN_POINT('Ctrl Pts',(-12.8807378287883,77.7390562691211,
87.7371244382603));
#150995=CARTESIAN_POINT('Ctrl Pts',(-12.862224443683,77.6273797845303,87.756992699729));
#150996=CARTESIAN_POINT('Ctrl Pts',(-12.8344384878748,77.459769277429,87.7868121321026));
#150997=CARTESIAN_POINT('Ctrl Pts',(-12.8084219966983,77.2914725236344,
87.8138085541141));
#150998=CARTESIAN_POINT('Ctrl Pts',(-12.7843726914315,77.1226755619766,
87.8379381257615));
#150999=CARTESIAN_POINT('Ctrl Pts',(-12.7813665282732,77.1015759417694,
87.8409543222174));
#151000=CARTESIAN_POINT('Ctrl Pts',(-12.7783911023947,77.0804685064775,
87.8439257445653));
#151001=CARTESIAN_POINT('Ctrl Pts',(-12.7754467826672,77.059353615165,87.8468523252774));
#151002=CARTESIAN_POINT('Ctrl Pts',(-12.7750787427012,77.0567142537509,
87.8472181478665));
#151003=CARTESIAN_POINT('Ctrl Pts',(-12.7747111887689,77.0540747572995,
87.8475831355736));
#151004=CARTESIAN_POINT('Ctrl Pts',(-12.7744712246906,77.0523490281323,
87.8478214971566));
#151005=CARTESIAN_POINT('Ctrl Pts',(-12.7742312606124,77.050623298965,87.8480598587396));
#151006=CARTESIAN_POINT('Ctrl Pts',(-12.7741183995359,77.0498113824519,
87.8481717851012));
#151007=CARTESIAN_POINT('Ctrl Pts',(-12.7740743863699,77.0494940241591,
87.8482155572021));
#151008=CARTESIAN_POINT('Ctrl Pts',(-12.7739863600379,77.0488593075736,
87.8483031014039));
#151009=CARTESIAN_POINT('Ctrl Pts',(-12.7738970165722,77.0482133976243,
87.8483921480379));
#151010=CARTESIAN_POINT('Ctrl Pts',(-12.773806359778,77.0475562935894,87.8484826927436));
#151011=CARTESIAN_POINT('Ctrl Pts',(-12.7736250461896,77.0462420855196,
87.8486637821549));
#151012=CARTESIAN_POINT('Ctrl Pts',(-12.7734384792872,77.0448831011278,
87.8488508640047));
#151013=CARTESIAN_POINT('Ctrl Pts',(-12.7732466894325,77.0434793345013,
87.849043901573));
#151014=CARTESIAN_POINT('Ctrl Pts',(-12.7724795300137,77.0378642679956,
87.849816051846));
#151015=CARTESIAN_POINT('Ctrl Pts',(-12.7716288033574,77.0315326922741,
87.8506835421921));
#151016=CARTESIAN_POINT('Ctrl Pts',(-12.7706965594528,77.0244841615641,
87.8516436360311));
#151017=CARTESIAN_POINT('Ctrl Pts',(-12.7688320716436,77.0103871001443,
87.8535638237089));
#151018=CARTESIAN_POINT('Ctrl Pts',(-12.7666415148415,76.9934223030366,
87.8558550473182));
#151019=CARTESIAN_POINT('Ctrl Pts',(-12.7641489243869,76.9735853740015,
87.8584879276142));
#151020=CARTESIAN_POINT('Ctrl Pts',(-12.7603881763992,76.943655992376,87.8624603408348));
#151021=CARTESIAN_POINT('Ctrl Pts',(-12.7559136930925,76.9071891064106,
87.8672128741886));
#151022=CARTESIAN_POINT('Ctrl Pts',(-12.7508847778743,76.8641652564707,
87.872601554469));
#151023=CARTESIAN_POINT('Ctrl Pts',(-12.7458602599409,76.8211790265965,
87.8779855228859));
#151024=CARTESIAN_POINT('Ctrl Pts',(-12.740282279263,76.7716471452226,87.8840045375955));
#151025=CARTESIAN_POINT('Ctrl Pts',(-12.7343097217284,76.7155467348373,
87.8904631088614));
#151026=CARTESIAN_POINT('Ctrl Pts',(-12.7304119732769,76.678935067818,87.8946780345453));
#151027=CARTESIAN_POINT('Ctrl Pts',(-12.7263461748165,76.6395257987867,
87.8990791095172));
#151028=CARTESIAN_POINT('Ctrl Pts',(-12.7221564880409,76.5973122916239,
87.9036000255105));
#151029=CARTESIAN_POINT('Ctrl Pts',(-12.7157559154614,76.5328228367065,
87.9105066160246));
#151030=CARTESIAN_POINT('Ctrl Pts',(-12.7090596215634,76.4617886583938,
87.9176953647784));
#151031=CARTESIAN_POINT('Ctrl Pts',(-12.7023690004211,76.3841852195534,
87.9248872199345));
#151032=CARTESIAN_POINT('Ctrl Pts',(-12.6957025603321,76.3068622528613,
87.9320530824916));
#151033=CARTESIAN_POINT('Ctrl Pts',(-12.6890417520683,76.2230171639885,
87.939222012628));
#151034=CARTESIAN_POINT('Ctrl Pts',(-12.6826847136308,76.1326304096918,
87.9460665385376));
#151035=CARTESIAN_POINT('Ctrl Pts',(-12.6784412442731,76.0722951724632,
87.9506354169941));
#151036=CARTESIAN_POINT('Ctrl Pts',(-12.6743331307868,76.0090451519203,
87.9550586867079));
#151037=CARTESIAN_POINT('Ctrl Pts',(-12.6704490512014,75.9428766493832,
87.9592261771818));
#151038=CARTESIAN_POINT('Ctrl Pts',(-12.6646823510838,75.8446361517392,
87.9654136579679));
#151039=CARTESIAN_POINT('Ctrl Pts',(-12.6594351114857,75.7399612101461,
87.9710396191839));
#151040=CARTESIAN_POINT('Ctrl Pts',(-12.6551289588245,75.6288466423876,
87.9757019863411));
#151041=CARTESIAN_POINT('Ctrl Pts',(-12.6536321155254,75.590222582983,87.9773226518368));
#151042=CARTESIAN_POINT('Ctrl Pts',(-12.6522489835133,75.55082055245,87.9788264446894));
#151043=CARTESIAN_POINT('Ctrl Pts',(-12.6509972715651,75.5106407819581,
87.9801950666));
#151044=CARTESIAN_POINT('Ctrl Pts',(-12.6485709389679,75.43275586041,87.9828480187905));
#151045=CARTESIAN_POINT('Ctrl Pts',(-12.6466421085366,75.3519482421605,
87.9849937077908));
#151046=CARTESIAN_POINT('Ctrl Pts',(-12.6453635745304,75.2682216895248,
87.9864910990295));
#151047=CARTESIAN_POINT('Ctrl Pts',(-12.6447243075273,75.2263584132069,
87.9872397946489));
#151048=CARTESIAN_POINT('Ctrl Pts',(-12.6442478758664,75.1837654570326,
87.9878262556065));
#151049=CARTESIAN_POINT('Ctrl Pts',(-12.6439550112119,75.140443641486,87.9882318916222));
#151050=CARTESIAN_POINT('Ctrl Pts',(-12.6438085788846,75.1187827337127,
87.98843470963));
#151051=CARTESIAN_POINT('Ctrl Pts',(-12.643708038309,75.0969396106309,87.9885923114292));
#151052=CARTESIAN_POINT('Ctrl Pts',(-12.6436561075585,75.0749144037385,
87.9887023131505));
#151053=CARTESIAN_POINT('Ctrl Pts',(-12.6436301421833,75.0639018002923,
87.9887573140112));
#151054=CARTESIAN_POINT('Ctrl Pts',(-12.6436163292643,75.0528436758568,
87.9888004142306));
#151055=CARTESIAN_POINT('Ctrl Pts',(-12.6436150126618,75.0417400477704,
87.9888313120813));
#151056=CARTESIAN_POINT('Ctrl Pts',(-12.6436136960592,75.030636419684,87.988862209932));
#151057=CARTESIAN_POINT('Ctrl Pts',(-12.6436289425742,75.0175924670353,
87.9888819529564));
#151058=CARTESIAN_POINT('Ctrl Pts',(-12.643648897583,75.0082926704016,87.9888870943004));
#151059=CARTESIAN_POINT('Ctrl Pts',(-12.644195767988,74.7534301646491,87.9890279937058));
#151060=CARTESIAN_POINT('Ctrl Pts',(-12.6513772312014,74.4981090494674,
87.9826693314223));
#151061=CARTESIAN_POINT('Ctrl Pts',(-12.6647090533377,74.2428344994553,
87.9697672114868));
#151062=CARTESIAN_POINT('Ctrl Pts',(-12.6780337947826,73.9876955288341,
87.9568719440227));
#151063=CARTESIAN_POINT('Ctrl Pts',(-12.6975023638259,73.7326034297094,
87.9374401521479));
#151064=CARTESIAN_POINT('Ctrl Pts',(-12.72263129772,73.4780643757733,87.9114800448976));
#151065=CARTESIAN_POINT('Ctrl Pts',(-12.7310755086258,73.3925302474942,
87.9027565303353));
#151066=CARTESIAN_POINT('Ctrl Pts',(-12.7401588866746,73.3070585602922,
87.8932962750379));
#151067=CARTESIAN_POINT('Ctrl Pts',(-12.7498630868526,73.22166845818,87.8831009107718));
#151068=CARTESIAN_POINT('Ctrl Pts',(-12.7782149963072,72.9721916956449,
87.8533140103342));
#151069=CARTESIAN_POINT('Ctrl Pts',(-12.8118641852904,72.7234184043276,
87.8172493006473));
#151070=CARTESIAN_POINT('Ctrl Pts',(-12.8503429411276,72.4758397156348,
87.7749847081594));
#151071=CARTESIAN_POINT('Ctrl Pts',(-12.8576532368596,72.4288040620151,
87.7669551691747));
#151072=CARTESIAN_POINT('Ctrl Pts',(-12.8651378481022,72.3818115008075,
87.7587020044201));
#151073=CARTESIAN_POINT('Ctrl Pts',(-12.8727935676933,72.3348653610224,
87.7502259573693));
#151074=CARTESIAN_POINT('Ctrl Pts',(-12.8967698986114,72.1878385310274,
87.7236805090219));
#151075=CARTESIAN_POINT('Ctrl Pts',(-12.9224245102739,72.0412671229056,
87.6949484896749));
#151076=CARTESIAN_POINT('Ctrl Pts',(-12.9496575479537,71.8952524204115,
87.6640569313489));
#151077=CARTESIAN_POINT('Ctrl Pts',(-12.9632740667936,71.8222450691645,
87.6486111521859));
#151078=CARTESIAN_POINT('Ctrl Pts',(-12.9772851921378,71.7493768545001,
87.6326255846485));
#151079=CARTESIAN_POINT('Ctrl Pts',(-12.9916784023378,71.676660173943,87.6161041727429));
#151080=CARTESIAN_POINT('Ctrl Pts',(-12.9988750074377,71.6403018336645,
87.6078434667901));
#151081=CARTESIAN_POINT('Ctrl Pts',(-13.0061671337516,71.6039813737283,
87.599448805464));
#151082=CARTESIAN_POINT('Ctrl Pts',(-13.0135532114325,71.5677003261153,
87.5909207161125));
#151083=CARTESIAN_POINT('Ctrl Pts',(-13.0204776592583,71.533686843978,87.5829256323456));
#151084=CARTESIAN_POINT('Ctrl Pts',(-13.0274846815277,71.4997080014925,
87.5748132780719));
#151085=CARTESIAN_POINT('Ctrl Pts',(-13.0345729826817,71.4657650503592,
87.5665841055929));
#151086=CARTESIAN_POINT('Ctrl Pts',(-13.035045536092,71.4635021869503,87.5660354940943));
#151087=CARTESIAN_POINT('Ctrl Pts',(-13.0358533538668,71.4596384428753,
87.5650974157022));
#151088=CARTESIAN_POINT('Ctrl Pts',(-13.0359917262243,71.4589769390507,
87.5649367136788));
#151089=CARTESIAN_POINT('Ctrl Pts',(-13.040419641666,71.4378088166649,87.5597942489322));
#151090=CARTESIAN_POINT('Ctrl Pts',(-13.0461916289705,71.4097504302298,
87.5529342150623));
#151091=CARTESIAN_POINT('Ctrl Pts',(-13.0534262918525,71.3748480667611,
87.5442414421276));
#151092=CARTESIAN_POINT('Ctrl Pts',(-13.0604266942912,71.3410758517556,
87.5358301436547));
#151093=CARTESIAN_POINT('Ctrl Pts',(-13.0687965821947,71.3008956697415,
87.5257025281699));
#151094=CARTESIAN_POINT('Ctrl Pts',(-13.0786434070465,71.2543642514234,
87.5137030803588));
#151095=CARTESIAN_POINT('Ctrl Pts',(-13.0889845009582,71.2054971522406,
87.5011013108982));
#151096=CARTESIAN_POINT('Ctrl Pts',(-13.1009545251389,71.1496248624621,
87.4864354574992));
#151097=CARTESIAN_POINT('Ctrl Pts',(-13.114677937705,71.0868327997857,87.4694668081874));
#151098=CARTESIAN_POINT('Ctrl Pts',(-13.1284013502712,71.0240407371094,
87.4524981588757));
#151099=CARTESIAN_POINT('Ctrl Pts',(-13.1438781512227,70.9543286492023,
87.4332265983425));
#151100=CARTESIAN_POINT('Ctrl Pts',(-13.1612327986762,70.8778054772566,
87.4113549288049));
#151101=CARTESIAN_POINT('Ctrl Pts',(-13.1783109484543,70.8025014876197,
87.3898317230317));
#151102=CARTESIAN_POINT('Ctrl Pts',(-13.1972368931742,70.7206039818765,
87.3657911400615));
#151103=CARTESIAN_POINT('Ctrl Pts',(-13.2181516178511,70.6322258372372,
87.338891089127));
#151104=CARTESIAN_POINT('Ctrl Pts',(-13.239066342528,70.5438476925979,87.3119910381925));
#151105=CARTESIAN_POINT('Ctrl Pts',(-13.2619698471617,70.4489885678385,
87.2822313861059));
#151106=CARTESIAN_POINT('Ctrl Pts',(-13.2870031167675,70.347792376931,87.2492177219255));
#151107=CARTESIAN_POINT('Ctrl Pts',(-13.3106570501867,70.2521721083965,
87.2180231146391));
#151108=CARTESIAN_POINT('Ctrl Pts',(-13.3362102524477,70.1508910394946,
87.1839219449404));
#151109=CARTESIAN_POINT('Ctrl Pts',(-13.3637483457489,70.0440780364571,
87.1465317570904));
#151110=CARTESIAN_POINT('Ctrl Pts',(-13.3653541796678,70.0378494300906,
87.1443514161632));
#151111=CARTESIAN_POINT('Ctrl Pts',(-13.3669667630647,70.03160202198,87.142159879629));
#151112=CARTESIAN_POINT('Ctrl Pts',(-13.3685861129178,70.0253358411578,
87.1399570673852));
#151113=CARTESIAN_POINT('Ctrl Pts',(-13.3832807253887,69.9684740711821,
87.1199678895022));
#151114=CARTESIAN_POINT('Ctrl Pts',(-13.3985319081895,69.9100658854031,
87.0990503614127));
#151115=CARTESIAN_POINT('Ctrl Pts',(-13.4143477727133,69.8501321735506,
87.0771419883082));
#151116=CARTESIAN_POINT('Ctrl Pts',(-13.4222557049753,69.8201653176244,
87.0661878017559));
#151117=CARTESIAN_POINT('Ctrl Pts',(-13.4303048076679,69.7898171021899,
87.0549858456137));
#151118=CARTESIAN_POINT('Ctrl Pts',(-13.4384956724289,69.7590902424223,
87.0435279416239));
#151119=CARTESIAN_POINT('Ctrl Pts',(-13.4425911048093,69.7437268125385,
87.037798989629));
#151120=CARTESIAN_POINT('Ctrl Pts',(-13.4467219777069,69.7282687230002,
87.0320060469309));
#151121=CARTESIAN_POINT('Ctrl Pts',(-13.4508883493145,69.7127163209738,
87.0261480682993));
#151122=CARTESIAN_POINT('Ctrl Pts',(-13.4529715351183,69.7049401199606,
87.0232190789835));
#151123=CARTESIAN_POINT('Ctrl Pts',(-13.4550635955996,69.6971403409203,
87.0202738304489));
#151124=CARTESIAN_POINT('Ctrl Pts',(-13.4571645363573,69.6893170276936,
87.0173121905753));
#151125=CARTESIAN_POINT('Ctrl Pts',(-13.459265477115,69.6814937144669,87.0143505507017));
#151126=CARTESIAN_POINT('Ctrl Pts',(-13.4618074963028,69.6720413854221,
87.0107616557083));
#151127=CARTESIAN_POINT('Ctrl Pts',(-13.4634940045198,69.6657765296424,
87.0083779638529));
#151128=CARTESIAN_POINT('Ctrl Pts',(-13.5025360795504,69.5207473107225,
86.9531963315711));
#151129=CARTESIAN_POINT('Ctrl Pts',(-13.5406679975864,69.382336143713,86.8979602069376));
#151130=CARTESIAN_POINT('Ctrl Pts',(-13.5776553922134,69.250422107576,86.8432155722503));
#151131=CARTESIAN_POINT('Ctrl Pts',(-13.6150631200759,69.1170089700783,
86.7878488069789));
#151132=CARTESIAN_POINT('Ctrl Pts',(-13.6513001634661,68.9902410372982,
86.7329848247617));
#151133=CARTESIAN_POINT('Ctrl Pts',(-13.6861240746425,68.8699806916482,
86.6791363996632));
#151134=CARTESIAN_POINT('Ctrl Pts',(-13.7120606591743,68.780411699671,86.639030501667));
#151135=CARTESIAN_POINT('Ctrl Pts',(-13.737213357045,68.6944522788393,86.5994868643773));
#151136=CARTESIAN_POINT('Ctrl Pts',(-13.7614820014407,68.6120432588692,
86.5606987233428));
#151137=CARTESIAN_POINT('Ctrl Pts',(-13.7942709972546,68.5007016871368,
86.5082926567626));
#151138=CARTESIAN_POINT('Ctrl Pts',(-13.8254696763556,68.3958423297509,
86.4572683615289));
#151139=CARTESIAN_POINT('Ctrl Pts',(-13.8550187233594,68.2973101826394,
86.4080528930081));
#151140=CARTESIAN_POINT('Ctrl Pts',(-13.8847124904967,68.1982954620806,
86.358596385608));
#151141=CARTESIAN_POINT('Ctrl Pts',(-13.9127404274108,68.1056697133762,
86.3109664100483));
#151142=CARTESIAN_POINT('Ctrl Pts',(-13.9390423429289,68.0192804077862,
86.2655438588061));
#151143=CARTESIAN_POINT('Ctrl Pts',(-13.9576676956576,67.9581049664956,
86.2333784814158));
#151144=CARTESIAN_POINT('Ctrl Pts',(-13.9754275217645,67.9000569338153,
86.2023189351381));
#151145=CARTESIAN_POINT('Ctrl Pts',(-13.9923004473289,67.845085027017,86.1724849405017));
#151146=CARTESIAN_POINT('Origin',(-13.9922814997631,65.4601089523298,90.5670141932079));
#151147=CARTESIAN_POINT('Ctrl Pts',(-14.1113299480719,67.99729033203,86.25689542676));
#151148=CARTESIAN_POINT('Ctrl Pts',(-11.862640570514,67.63449740977,85.9811177666601));
#151149=CARTESIAN_POINT('Ctrl Pts',(-10.0162267656979,66.69382083775,86.9661594600301));
#151150=CARTESIAN_POINT('Ctrl Pts',(-9.30362299642391,65.54790245802,88.82184290376));
#151151=CARTESIAN_POINT('Ctrl Pts',(-14.6084235582589,66.3684868668701,
85.3977275067001));
#151152=CARTESIAN_POINT('Ctrl Pts',(-12.2761791919147,65.94373812164,85.01902796748));
#151153=CARTESIAN_POINT('Ctrl Pts',(-10.3874061607769,64.7718800752,85.94969573064));
#151154=CARTESIAN_POINT('Ctrl Pts',(-9.74725467144591,63.35238921989,87.79310189113));
#151155=CARTESIAN_POINT('Ctrl Pts',(-15.2202405059459,64.90419477503,84.23630032921));
#151156=CARTESIAN_POINT('Ctrl Pts',(-12.769810936217,64.5010541575,83.7487065063399));
#151157=CARTESIAN_POINT('Ctrl Pts',(-10.8264676087059,63.11180437274,84.60346776298));
#151158=CARTESIAN_POINT('Ctrl Pts',(-10.2937231765289,61.38225058552,86.4032922329301));
#151159=CARTESIAN_POINT('Ctrl Pts',(-15.7858253484379,63.70313319505,82.861956262162));
#151160=CARTESIAN_POINT('Ctrl Pts',(-13.2006025443827,63.38438634906,82.351027486016));
#151161=CARTESIAN_POINT('Ctrl Pts',(-11.2038824748619,61.8092972954501,
83.1115754237101));
#151162=CARTESIAN_POINT('Ctrl Pts',(-10.7993506281109,59.76948116378,84.76141092969));
#151163=CARTESIAN_POINT('',(-15.5675364833309,63.77502783968,82.938763757646));
#151164=CARTESIAN_POINT('Ctrl Pts',(-15.5675364833309,63.7750278396777,
82.938763757648));
#151165=CARTESIAN_POINT('Ctrl Pts',(-15.4656186766729,63.9946650181252,
83.186547912653));
#151166=CARTESIAN_POINT('Ctrl Pts',(-15.3632899217089,64.2226173284476,
83.4269525126868));
#151167=CARTESIAN_POINT('Ctrl Pts',(-15.2605507121745,64.4582711559872,
83.6595429156073));
#151168=CARTESIAN_POINT('Ctrl Pts',(-15.2286410871491,64.5314625432545,
83.7317828381775));
#151169=CARTESIAN_POINT('Ctrl Pts',(-15.1966921480705,64.6053970859381,
83.8032689508469));
#151170=CARTESIAN_POINT('Ctrl Pts',(-15.1647047257657,64.6800571258485,
83.8739882984837));
#151171=CARTESIAN_POINT('Ctrl Pts',(-15.0972161681521,64.8375783651946,
84.0231952812129));
#151172=CARTESIAN_POINT('Ctrl Pts',(-15.0295538846762,64.9983290816565,
84.1689893491265));
#151173=CARTESIAN_POINT('Ctrl Pts',(-14.961717781448,65.1621474989424,84.31124838789));
#151174=CARTESIAN_POINT('Ctrl Pts',(-14.9277997298339,65.2440567075854,
84.3823779072718));
#151175=CARTESIAN_POINT('Ctrl Pts',(-14.8938382230921,65.3267329248824,
84.4526236609836));
#151176=CARTESIAN_POINT('Ctrl Pts',(-14.8598332546457,65.4101563011331,
84.5219702946248));
#151177=CARTESIAN_POINT('Ctrl Pts',(-14.8428307704224,65.4518679892585,
84.5566436114454));
#151178=CARTESIAN_POINT('Ctrl Pts',(-14.8258174208648,65.4937664700047,
84.5910921470643));
#151179=CARTESIAN_POINT('Ctrl Pts',(-14.8087932058618,65.5358492776703,
84.6253139766023));
#151180=CARTESIAN_POINT('Ctrl Pts',(-14.8002810983603,65.5568906815031,
84.6424248913712));
#151181=CARTESIAN_POINT('Ctrl Pts',(-14.7917662745059,65.5779781671964,
84.6594791295602));
#151182=CARTESIAN_POINT('Ctrl Pts',(-14.7832487343406,65.59911142716,84.6764764501779));
#151183=CARTESIAN_POINT('Ctrl Pts',(-14.778989964258,65.6096780571419,84.6849751104868));
#151184=CARTESIAN_POINT('Ctrl Pts',(-14.7747305150982,65.6202561306973,
84.6934595413993));
#151185=CARTESIAN_POINT('Ctrl Pts',(-14.7704703868703,65.6308456094083,
84.70192971277));
#151186=CARTESIAN_POINT('Ctrl Pts',(-14.7662102586423,65.6414350881193,
84.7103998841407));
#151187=CARTESIAN_POINT('Ctrl Pts',(-14.7614474301979,65.6532861400737,
84.7198502548234));
#151188=CARTESIAN_POINT('Ctrl Pts',(-14.7576879649934,65.6626482226085,
84.7272974180975));
#151189=CARTESIAN_POINT('Ctrl Pts',(-14.7244750223662,65.7453574094699,
84.7930892776053));
#151190=CARTESIAN_POINT('Ctrl Pts',(-14.6899771016152,65.8331893986453,
84.8615430975335));
#151191=CARTESIAN_POINT('Ctrl Pts',(-14.654150529173,65.9263531473689,84.9323443142181));
#151192=CARTESIAN_POINT('Ctrl Pts',(-14.6190487988401,66.0176320099999,
85.0017130828691));
#151193=CARTESIAN_POINT('Ctrl Pts',(-14.5826713302042,66.1140292730603,
85.0733352782067));
#151194=CARTESIAN_POINT('Ctrl Pts',(-14.545005571114,66.215750145994,85.1468761711002));
#151195=CARTESIAN_POINT('Ctrl Pts',(-14.5085278025403,66.3142627089058,
85.2180975598754));
#151196=CARTESIAN_POINT('Ctrl Pts',(-14.4708415205441,66.4177685482323,
85.2911184942675));
#151197=CARTESIAN_POINT('Ctrl Pts',(-14.4319659731008,66.5264594367093,
85.3655980275366));
#151198=CARTESIAN_POINT('Ctrl Pts',(-14.4035514676782,66.6059026354073,
85.4200358230441));
#151199=CARTESIAN_POINT('Ctrl Pts',(-14.3745022236368,66.688115954453,85.4752521024859));
#151200=CARTESIAN_POINT('Ctrl Pts',(-14.3448376701008,66.7731753463617,
85.53110066904));
#151201=CARTESIAN_POINT('Ctrl Pts',(-14.325471304126,66.8287059752416,85.5675611462807));
#151202=CARTESIAN_POINT('Ctrl Pts',(-14.3058344006169,66.8854493524695,
85.604290692101));
#151203=CARTESIAN_POINT('Ctrl Pts',(-14.2859269601853,66.9434263337528,
85.6412457446482));
#151204=CARTESIAN_POINT('Ctrl Pts',(-14.2834385301313,66.9506734564132,
85.6458651262165));
#151205=CARTESIAN_POINT('Ctrl Pts',(-14.2809458729396,66.9579398553398,
85.6504880293378));
#151206=CARTESIAN_POINT('Ctrl Pts',(-14.2784489886125,66.9652255685214,
85.6551143648198));
#151207=CARTESIAN_POINT('Ctrl Pts',(-14.2759521042853,66.9725112817029,
85.6597407003019));
#151208=CARTESIAN_POINT('Ctrl Pts',(-14.274373726549,66.9771222966787,85.66266251223));
#151209=CARTESIAN_POINT('Ctrl Pts',(-14.2724661389012,66.982699104053,85.6661929182527));
#151210=CARTESIAN_POINT('Ctrl Pts',(-14.2686509636057,66.9938527188015,
85.6732537302981));
#151211=CARTESIAN_POINT('Ctrl Pts',(-14.2648489860863,67.0049889914759,
85.6802829154931));
#151212=CARTESIAN_POINT('Ctrl Pts',(-14.2610602063424,67.0161077555074,
85.6872806562372));
#151213=CARTESIAN_POINT('Ctrl Pts',(-14.2534826468546,67.0383452835705,
85.7012761377256));
#151214=CARTESIAN_POINT('Ctrl Pts',(-14.2459578784689,67.0605127766583,
85.7151458422875));
#151215=CARTESIAN_POINT('Ctrl Pts',(-14.2384859011777,67.0826088746059,
85.7288911974603));
#151216=CARTESIAN_POINT('Ctrl Pts',(-14.2085979920129,67.1709932663963,
85.7838726181511));
#151217=CARTESIAN_POINT('Ctrl Pts',(-14.1795547404069,67.2582351770003,
85.8368647362588));
#151218=CARTESIAN_POINT('Ctrl Pts',(-14.1513561454702,67.3442534426152,
85.8879594938722));
#151219=CARTESIAN_POINT('Ctrl Pts',(-14.1056923780582,67.4835482579436,
85.9707004649337));
#151220=CARTESIAN_POINT('Ctrl Pts',(-14.0622422564733,67.6196323210958,
86.0484664752182));
#151221=CARTESIAN_POINT('Ctrl Pts',(-14.0210093452371,67.7521944444359,
86.1216412289296));
#151222=CARTESIAN_POINT('Ctrl Pts',(-14.0113174104562,67.7833536183898,
86.1388412014592));
#151223=CARTESIAN_POINT('Ctrl Pts',(-14.0017478415776,67.814318384856,86.1557874692341));
#151224=CARTESIAN_POINT('Ctrl Pts',(-13.9923004473294,67.8450850269991,
86.1724849405349));
#151225=CARTESIAN_POINT('Origin',(-15.567536483327,60.0333704529112,86.2553885480113));
#151226=CARTESIAN_POINT('Ctrl Pts',(-10.7041478512869,60.09386358315,60.91310738057));
#151227=CARTESIAN_POINT('Ctrl Pts',(-10.7993782800729,60.52820765429,61.28143633235));
#151228=CARTESIAN_POINT('Ctrl Pts',(-11.1849148787759,61.42183746249,61.97975320377));
#151229=CARTESIAN_POINT('Ctrl Pts',(-12.3843078552048,62.66523363696,62.74337770198));
#151230=CARTESIAN_POINT('Ctrl Pts',(-14.0046199477159,63.57750343472,63.071352235562));
#151231=CARTESIAN_POINT('Ctrl Pts',(-15.1626528546819,63.86437128803,62.97100038631));
#151232=CARTESIAN_POINT('Ctrl Pts',(-15.7241364691869,63.93250661787,62.85729087165));
#151233=CARTESIAN_POINT('Ctrl Pts',(-10.9677003684249,59.23917692104,61.74432861127));
#151234=CARTESIAN_POINT('Ctrl Pts',(-11.0441856921679,59.69432284704,62.07811676378));
#151235=CARTESIAN_POINT('Ctrl Pts',(-11.3853725838149,60.62794654058,62.70918441869));
#151236=CARTESIAN_POINT('Ctrl Pts',(-12.4999814042143,61.92964160607,63.404910218528));
#151237=CARTESIAN_POINT('Ctrl Pts',(-14.0404250630359,62.89957197099,63.720140072344));
#151238=CARTESIAN_POINT('Ctrl Pts',(-15.1678421958939,63.22153762942,63.648738097669));
#151239=CARTESIAN_POINT('Ctrl Pts',(-15.7218484252699,63.30516960111,63.555460526342));
#151240=CARTESIAN_POINT('Ctrl Pts',(-11.3522936220299,58.14048279688,63.112571062291));
#151241=CARTESIAN_POINT('Ctrl Pts',(-11.4036986376439,58.61682481433,63.39382635559));
#151242=CARTESIAN_POINT('Ctrl Pts',(-11.6848368356725,59.58954811192,63.923065828625));
#151243=CARTESIAN_POINT('Ctrl Pts',(-12.6807018187541,60.95041422043,64.511351021118));
#151244=CARTESIAN_POINT('Ctrl Pts',(-14.1030936751889,61.9883845619,64.794328418875));
#151245=CARTESIAN_POINT('Ctrl Pts',(-15.1787465752669,62.36041090115,64.754643608369));
#151246=CARTESIAN_POINT('Ctrl Pts',(-15.7172649246479,62.4683826908,64.686581762677));
#151247=CARTESIAN_POINT('Ctrl Pts',(-11.7927722579713,57.02090553469,65.101174498226));
#151248=CARTESIAN_POINT('Ctrl Pts',(-11.8176818813148,57.5125830774,65.313181016537));
#151249=CARTESIAN_POINT('Ctrl Pts',(-12.0347761979639,58.51132096517,65.710392001923));
#151250=CARTESIAN_POINT('Ctrl Pts',(-12.9001966352731,59.91385972121,66.156294835457));
#151251=CARTESIAN_POINT('Ctrl Pts',(-14.1863686741549,61.01129527967,66.384105820796));
#151252=CARTESIAN_POINT('Ctrl Pts',(-15.1950629340269,61.43683394941,66.371138073743));
#151253=CARTESIAN_POINT('Ctrl Pts',(-15.7105937362879,61.57320926474,66.328753181307));
#151254=CARTESIAN_POINT('Ctrl Pts',(-12.0661314106483,56.37283617372,66.595423337916));
#151255=CARTESIAN_POINT('Ctrl Pts',(-12.075843484741,56.87031895129,66.759479358578));
#151256=CARTESIAN_POINT('Ctrl Pts',(-12.2555688846867,57.87753552955,67.065970272353));
#151257=CARTESIAN_POINT('Ctrl Pts',(-13.0422585423336,59.29546209927,67.41236946592));
#151258=CARTESIAN_POINT('Ctrl Pts',(-14.2430805630419,60.42240614722,67.596288679237));
#151259=CARTESIAN_POINT('Ctrl Pts',(-15.2068409041219,60.87953638865,67.595276586158));
#151260=CARTESIAN_POINT('Ctrl Pts',(-15.7058387404459,61.0336884742,67.567305919008));
#151261=CARTESIAN_POINT('Ctrl Pts',(-12.2840775879579,55.88110902615,68.139369567263));
#151262=CARTESIAN_POINT('Ctrl Pts',(-12.2827124321577,56.38084424396,68.259552190757));
#151263=CARTESIAN_POINT('Ctrl Pts',(-12.4345336551906,57.38982547879,68.483378307406));
#151264=CARTESIAN_POINT('Ctrl Pts',(-13.1600193818491,58.81285577352,68.737117882334));
#151265=CARTESIAN_POINT('Ctrl Pts',(-14.2920472090019,59.95780874927,68.875104868816));
#151266=CARTESIAN_POINT('Ctrl Pts',(-15.2174560511339,60.43844112166,68.878748123676));
#151267=CARTESIAN_POINT('Ctrl Pts',(-15.7015914388329,60.60654655031,68.86065654605));
#151268=CARTESIAN_POINT('Ctrl Pts',(-12.4455223641968,55.53147356831,69.729584462491));
#151269=CARTESIAN_POINT('Ctrl Pts',(-12.4364409723155,56.03153659582,69.808270714192));
#151270=CARTESIAN_POINT('Ctrl Pts',(-12.5684953465757,57.03906368193,69.954444991214));
#151271=CARTESIAN_POINT('Ctrl Pts',(-13.2494610073255,58.46199397327,70.120458107449));
#151272=CARTESIAN_POINT('Ctrl Pts',(-14.3302328652479,59.61727660643,70.212240577407));
#151273=CARTESIAN_POINT('Ctrl Pts',(-15.2259605578979,60.11434751671,70.216671992981));
#151274=CARTESIAN_POINT('Ctrl Pts',(-15.6982072375269,60.29264234042,70.205961262777));
#151275=CARTESIAN_POINT('Ctrl Pts',(-12.5457498999138,55.32390979008,71.345733821343));
#151276=CARTESIAN_POINT('Ctrl Pts',(-12.5323125837535,55.8230599579,71.384509154805));
#151277=CARTESIAN_POINT('Ctrl Pts',(-12.6528329390118,56.82750771549,71.456441367017));
#151278=CARTESIAN_POINT('Ctrl Pts',(-13.3066685414157,58.24764282185,71.538286506703));
#151279=CARTESIAN_POINT('Ctrl Pts',(-14.3552787532329,59.40754337175,71.584076966819));
#151280=CARTESIAN_POINT('Ctrl Pts',(-15.2316755631129,59.91449324558,71.586996148855));
#151281=CARTESIAN_POINT('Ctrl Pts',(-15.6959440082919,60.09919481949,71.582126108352));
#151282=CARTESIAN_POINT('Ctrl Pts',(-12.5810013147727,55.25465453145,72.9682049875124));
#151283=CARTESIAN_POINT('Ctrl Pts',(-12.5662393202886,55.75295766121,72.9686809528089));
#151284=CARTESIAN_POINT('Ctrl Pts',(-12.6830375165265,56.75533192763,72.9695652327033));
#151285=CARTESIAN_POINT('Ctrl Pts',(-13.3275136480546,58.17334349544,72.9705789955397));
#151286=CARTESIAN_POINT('Ctrl Pts',(-14.3646256854689,59.33424330126,72.9711581432487));
#151287=CARTESIAN_POINT('Ctrl Pts',(-15.2338545192429,59.84467210232,72.971209319932));
#151288=CARTESIAN_POINT('Ctrl Pts',(-15.6950847124779,60.03173379517,72.9711575988109));
#151289=CARTESIAN_POINT('Ctrl Pts',(-12.5475045162957,55.32017430334,74.590690933763));
#151290=CARTESIAN_POINT('Ctrl Pts',(-12.533981149037,55.81932730129,74.55291642949));
#151291=CARTESIAN_POINT('Ctrl Pts',(-12.6542839686069,56.82375706031,74.482838228714));
#151292=CARTESIAN_POINT('Ctrl Pts',(-13.3076377377342,58.2438840296,74.403081923287));
#151293=CARTESIAN_POINT('Ctrl Pts',(-14.3556951419809,59.4038845339,74.358425507288));
#151294=CARTESIAN_POINT('Ctrl Pts',(-15.2317691498149,59.91100278183,74.355537412367));
#151295=CARTESIAN_POINT('Ctrl Pts',(-15.6959068347229,60.09581045991,74.360258574239));
#151296=CARTESIAN_POINT('Ctrl Pts',(-12.415890569498,55.59282803409,76.748377568762));
#151297=CARTESIAN_POINT('Ctrl Pts',(-12.4081109279239,56.09315502217,76.657403775015));
#151298=CARTESIAN_POINT('Ctrl Pts',(-12.5435994725054,57.10157402003,76.488382653225));
#151299=CARTESIAN_POINT('Ctrl Pts',(-13.2325997356438,58.52529383771,76.296485974051));
#151300=CARTESIAN_POINT('Ctrl Pts',(-14.3228650735109,59.67918060652,76.190569027371));
#151301=CARTESIAN_POINT('Ctrl Pts',(-15.2242815937599,60.17332252705,76.185676184442));
#151302=CARTESIAN_POINT('Ctrl Pts',(-15.6988723085229,60.34972220064,76.198183493317));
#151303=CARTESIAN_POINT('Ctrl Pts',(-12.0984815213201,56.28453201345,79.379282177917));
#151304=CARTESIAN_POINT('Ctrl Pts',(-12.1059032952047,56.78383432926,79.217993773868));
#151305=CARTESIAN_POINT('Ctrl Pts',(-12.2803121570303,57.79442431143,78.916961042675));
#151306=CARTESIAN_POINT('Ctrl Pts',(-13.0569396205545,59.21756273984,78.575716119718));
#151307=CARTESIAN_POINT('Ctrl Pts',(-14.2480069695869,60.35063110239,78.391769330457));
#151308=CARTESIAN_POINT('Ctrl Pts',(-15.2076486671689,60.8123315191,78.389193997522));
#151309=CARTESIAN_POINT('Ctrl Pts',(-15.7054941595619,60.96870853934,78.414798392491));
#151310=CARTESIAN_POINT('Ctrl Pts',(-11.4801382308999,57.77429967397,82.410149750697));
#151311=CARTESIAN_POINT('Ctrl Pts',(-11.5230945717699,58.25793556694,82.146393216678));
#151312=CARTESIAN_POINT('Ctrl Pts',(-11.7841034131413,59.24408794519,81.651018262809));
#151313=CARTESIAN_POINT('Ctrl Pts',(-12.7404495534974,60.62500522955,81.098302707073));
#151314=CARTESIAN_POINT('Ctrl Pts',(-14.1237202044259,61.68566477043,80.825785486714));
#151315=CARTESIAN_POINT('Ctrl Pts',(-15.1823110544289,62.07418257557,80.85469887249));
#151316=CARTESIAN_POINT('Ctrl Pts',(-15.7157641330979,62.19013200718,80.914252246577));
#151317=CARTESIAN_POINT('Ctrl Pts',(-10.9713079387719,59.22776230562,84.2218583444));
#151318=CARTESIAN_POINT('Ctrl Pts',(-11.0475501095389,59.68314485841,83.88853398117));
#151319=CARTESIAN_POINT('Ctrl Pts',(-11.3881525214289,60.61722479436,83.25836777774));
#151320=CARTESIAN_POINT('Ctrl Pts',(-12.5016155027486,61.91961304936,82.56355185095));
#151321=CARTESIAN_POINT('Ctrl Pts',(-14.0409546878519,62.89027630592,82.248495693581));
#151322=CARTESIAN_POINT('Ctrl Pts',(-15.1679259362809,63.21272241284,82.319513523069));
#151323=CARTESIAN_POINT('Ctrl Pts',(-15.7218123616379,63.29657498626,82.412519105935));
#151324=CARTESIAN_POINT('Ctrl Pts',(-10.7040595554349,60.09411427919,85.06497750449));
#151325=CARTESIAN_POINT('Ctrl Pts',(-10.7992944412079,60.52845915508,84.69663916139));
#151326=CARTESIAN_POINT('Ctrl Pts',(-11.1848427857669,61.42209035944,83.99830481448));
#151327=CARTESIAN_POINT('Ctrl Pts',(-12.3842618607212,62.66548448627,83.23466499336));
#151328=CARTESIAN_POINT('Ctrl Pts',(-14.0046020364719,63.5777452831,82.906691022993));
#151329=CARTESIAN_POINT('Ctrl Pts',(-15.1626491571459,63.86460259476,83.00705348714));
#151330=CARTESIAN_POINT('Ctrl Pts',(-15.7241379640389,63.9327320353,83.12076992282));
#151331=CARTESIAN_POINT('Ctrl Pts',(-15.5675364833309,63.77502783968,63.039015015514));
#151332=CARTESIAN_POINT('Ctrl Pts',(-15.5675364833366,63.1966588570052,
63.6915032265959));
#151333=CARTESIAN_POINT('Ctrl Pts',(-15.5675364833221,62.4022926946241,
64.7657142192389));
#151334=CARTESIAN_POINT('Ctrl Pts',(-15.5675364833146,61.5332281582025,
66.3395724687636));
#151335=CARTESIAN_POINT('Ctrl Pts',(-15.5675364833362,60.9888173218726,
67.574344511651));
#151336=CARTESIAN_POINT('Ctrl Pts',(-15.5675364833589,60.5578543920014,
68.8651514730108));
#151337=CARTESIAN_POINT('Ctrl Pts',(-15.567536483356,60.2411695586609,70.2085918635667));
#151338=CARTESIAN_POINT('Ctrl Pts',(-15.5675364833459,60.0459797863666,
71.5833100686918));
#151339=CARTESIAN_POINT('Ctrl Pts',(-15.5675364833335,59.9778791011265,
72.9711699015529));
#151340=CARTESIAN_POINT('Ctrl Pts',(-15.5675364833356,60.0425665085272,
74.3591115894978));
#151341=CARTESIAN_POINT('Ctrl Pts',(-15.5675364833536,60.2987648763767,
76.1951078607713));
#151342=CARTESIAN_POINT('Ctrl Pts',(-15.5675364833368,60.9232171254913,
78.4084022555666));
#151343=CARTESIAN_POINT('Ctrl Pts',(-15.5675364833127,62.1248654345252,
80.8364426677163));
#151344=CARTESIAN_POINT('Ctrl Pts',(-15.5675364833367,63.188677426801,82.277271278915));
#151345=CARTESIAN_POINT('Ctrl Pts',(-15.5675364833309,63.77502783968,82.938763757646));
#151346=CARTESIAN_POINT('Origin',(-15.5675364833309,75.,72.98888938658));
#151347=CARTESIAN_POINT('Origin',(-15.5675364833309,75.,72.98888938658));
#151348=CARTESIAN_POINT('Origin',(-15.5675364833309,75.,72.98888938658));
#151349=CARTESIAN_POINT('Origin',(-15.5675364833309,75.,72.98888938658));
#151350=CARTESIAN_POINT('Origin',(-15.5675364833309,75.,72.98888938658));
#151351=CARTESIAN_POINT('Origin',(27.4324635166691,25.,72.98888938658));
#151352=CARTESIAN_POINT('Origin',(-2.02513312664091,-92.,60.48888938658));
#151353=CARTESIAN_POINT('',(1.02913961852909,-92.5,53.63896836527));
#151354=CARTESIAN_POINT('Origin',(-2.02513312664091,-92.5,60.48888938658));
#151355=CARTESIAN_POINT('Origin',(1.02913961852909,-92.,53.63896836527));
#151356=CARTESIAN_POINT('Origin',(-10.9843331791359,-92.,80.581991049076));
#151357=CARTESIAN_POINT('Origin',(-10.9843331791359,-92.5,80.581991049076));
#151358=CARTESIAN_POINT('Origin',(-10.9843331791359,-92.,80.581991049076));
#151359=CARTESIAN_POINT('Origin',(-10.9843331791359,-92.,65.395787724084));
#151360=CARTESIAN_POINT('Origin',(-10.9843331791359,-92.,65.395787724084));
#151361=CARTESIAN_POINT('',(1.02913961852909,-92.5,92.33881040789));
#151362=CARTESIAN_POINT('Origin',(1.02913961852909,-92.,92.33881040789));
#151363=CARTESIAN_POINT('Origin',(-10.9843331791359,-92.5,65.395787724084));
#151364=CARTESIAN_POINT('Origin',(-2.27593483123091,-92.5,69.192338555332));
#151365=CARTESIAN_POINT('Origin',(-2.02513312664091,-92.5,85.48888938658));
#151366=CARTESIAN_POINT('Origin',(-2.02513312664091,-92.,85.48888938658));
#151367=CARTESIAN_POINT('Origin',(-10.9843331791359,-92.5,65.395787724084));
#151368=CARTESIAN_POINT('Ctrl Pts',(16.5158721297058,-26.62691877498,77.3848956129786));
#151369=CARTESIAN_POINT('Ctrl Pts',(16.3820322875788,-26.7011776840352,
77.6918928617402));
#151370=CARTESIAN_POINT('Ctrl Pts',(16.2459288731422,-26.7722083172181,
77.990054798336));
#151371=CARTESIAN_POINT('Ctrl Pts',(16.1082781307409,-26.8400106745286,
78.2795143748608));
#151372=CARTESIAN_POINT('Ctrl Pts',(15.9688840103591,-26.9086717641257,
78.5726400228005));
#151373=CARTESIAN_POINT('Ctrl Pts',(15.8279032167025,-26.9740222863118,
78.8568417897912));
#151374=CARTESIAN_POINT('Ctrl Pts',(15.6860353899346,-27.0360622410872,
79.1322880203727));
#151375=CARTESIAN_POINT('Ctrl Pts',(15.5414909720178,-27.0992726909465,
79.4129310384115));
#151376=CARTESIAN_POINT('Ctrl Pts',(15.396025859127,-27.1590464753882,79.6844853256324));
#151377=CARTESIAN_POINT('Ctrl Pts',(15.2503327146554,-27.2153835944122,
79.9471555443661));
#151378=CARTESIAN_POINT('Ctrl Pts',(15.1031356263789,-27.2723022635252,
80.2125372238871));
#151379=CARTESIAN_POINT('Ctrl Pts',(14.9557058104529,-27.3257129498178,
80.4688508172432));
#151380=CARTESIAN_POINT('Ctrl Pts',(14.8087086118992,-27.3756156532902,
80.7163293321968));
#151381=CARTESIAN_POINT('Ctrl Pts',(14.6595141442981,-27.4262642870715,
80.9675070801029));
#151382=CARTESIAN_POINT('Ctrl Pts',(14.5107653761148,-27.4732992817285,
81.2095839839924));
#151383=CARTESIAN_POINT('Ctrl Pts',(14.3631070011745,-27.5167206372612,
81.4428209796608));
#151384=CARTESIAN_POINT('Ctrl Pts',(14.2912166810056,-27.5378611594474,
81.5563768975056));
#151385=CARTESIAN_POINT('Ctrl Pts',(14.2195840629412,-27.5581450986431,
81.667837615716));
#151386=CARTESIAN_POINT('Ctrl Pts',(14.148279236274,-27.5775724548482,81.7772343383726));
#151387=CARTESIAN_POINT('Ctrl Pts',(14.0923156340326,-27.5928200178265,
81.8630943700058));
#151388=CARTESIAN_POINT('Ctrl Pts',(14.0365538920273,-27.6075399344871,
81.9476830161932));
#151389=CARTESIAN_POINT('Ctrl Pts',(13.9810266940025,-27.62173220483,82.0310155976267));
#151390=CARTESIAN_POINT('Ctrl Pts',(13.9532630949901,-27.6288283400015,
82.0726818883434));
#151391=CARTESIAN_POINT('Ctrl Pts',(13.9255581219713,-27.6357925635935,
82.1140341561832));
#151392=CARTESIAN_POINT('Ctrl Pts',(13.8979157551414,-27.6426248756062,
82.1550743429307));
#151393=CARTESIAN_POINT('Ctrl Pts',(13.8840945717265,-27.6460410316125,
82.1755944363045));
#151394=CARTESIAN_POINT('Ctrl Pts',(13.8702890392204,-27.649424209724,82.196036508983));
#151395=CARTESIAN_POINT('Ctrl Pts',(13.8564996502144,-27.6527744099406,
82.2164008028118));
#151396=CARTESIAN_POINT('Ctrl Pts',(13.84615760846,-27.6552870601031,82.2316740231835));
#151397=CARTESIAN_POINT('Ctrl Pts',(13.8358246473727,-27.6577811601997,
82.2469034929172));
#151398=CARTESIAN_POINT('Ctrl Pts',(13.8255009733157,-27.6602567102304,
82.2620893141732));
#151399=CARTESIAN_POINT('Ctrl Pts',(13.8220597486301,-27.661081893574,82.2671512545919));
#151400=CARTESIAN_POINT('Ctrl Pts',(13.8196814399517,-27.6616515023092,
82.2706483977758));
#151401=CARTESIAN_POINT('Ctrl Pts',(13.8151804024935,-27.6627260769059,
82.2772605897607));
#151402=CARTESIAN_POINT('Ctrl Pts',(13.5932909459714,-27.7156998136198,
82.6032244813254));
#151403=CARTESIAN_POINT('Ctrl Pts',(13.3682551472339,-27.7624240386982,
82.9199960935799));
#151404=CARTESIAN_POINT('Ctrl Pts',(13.1407961930566,-27.8028987521411,
83.2277290871262));
#151405=CARTESIAN_POINT('Ctrl Pts',(12.9110186606534,-27.8437860401939,
83.5385989236287));
#151406=CARTESIAN_POINT('Ctrl Pts',(12.6787684254416,-27.8782957598135,
83.8402451995739));
#151407=CARTESIAN_POINT('Ctrl Pts',(12.4447515029891,-27.906427911,84.1328630283522));
#151408=CARTESIAN_POINT('Ctrl Pts',(12.2067799972796,-27.9350354591488,
84.4304257198962));
#151409=CARTESIAN_POINT('Ctrl Pts',(11.9669817217329,-27.9570480723335,
84.7186524906363));
#151410=CARTESIAN_POINT('Ctrl Pts',(11.7260565705287,-27.9724657505541,
84.9977824546804));
#151411=CARTESIAN_POINT('Ctrl Pts',(11.5250001554144,-27.9853320830931,
85.2307214801047));
#151412=CARTESIAN_POINT('Ctrl Pts',(11.3231581995199,-27.993605567279,85.4573259977147));
#151413=CARTESIAN_POINT('Ctrl Pts',(11.1209145922133,-27.9972862031118,
85.6777506706842));
#151414=CARTESIAN_POINT('Ctrl Pts',(10.9677766773297,-28.0000731633742,
85.8446552035739));
#151415=CARTESIAN_POINT('Ctrl Pts',(10.8144080517589,-28.0002268380673,
86.008016856321));
#151416=CARTESIAN_POINT('Ctrl Pts',(10.6609674346233,-27.9977472271911,
86.1679075326157));
#151417=CARTESIAN_POINT('Ctrl Pts',(10.5842471260555,-27.996507421753,86.247852870763));
#151418=CARTESIAN_POINT('Ctrl Pts',(10.5075087946992,-27.9946092949226,
86.3269304407219));
#151419=CARTESIAN_POINT('Ctrl Pts',(10.4307715507466,-27.9920528466999,
86.4051496708011));
#151420=CARTESIAN_POINT('Ctrl Pts',(10.3924029287703,-27.9907746225885,
86.4442592858407));
#151421=CARTESIAN_POINT('Ctrl Pts',(10.3540345768555,-27.9893318181291,
86.4831543142134));
#151422=CARTESIAN_POINT('Ctrl Pts',(10.3156688587493,-27.9877244333215,
86.5218359391688));
#151423=CARTESIAN_POINT('Ctrl Pts',(10.2964859996962,-27.9869207409178,
86.5411767516465));
#151424=CARTESIAN_POINT('Ctrl Pts',(10.27730379899,-27.986075903427,86.5604642131652));
#151425=CARTESIAN_POINT('Ctrl Pts',(10.258122549549,-27.9851899208492,86.5796984729251));
#151426=CARTESIAN_POINT('Ctrl Pts',(10.2485319248285,-27.9847469295603,
86.589315602805));
#151427=CARTESIAN_POINT('Ctrl Pts',(10.2389415379176,-27.9842936519996,
86.5989194322384));
#151428=CARTESIAN_POINT('Ctrl Pts',(10.2293514252671,-27.9838300881672,
86.6085099799595));
#151429=CARTESIAN_POINT('Ctrl Pts',(10.2197613126166,-27.9833665243348,
86.6181005276805));
#151430=CARTESIAN_POINT('Ctrl Pts',(10.2117549429593,-27.9829726171462,
86.6260985397174));
#151431=CARTESIAN_POINT('Ctrl Pts',(10.2005819464838,-27.9824085378547,
86.6372417967291));
#151432=CARTESIAN_POINT('Ctrl Pts',(9.90016413482943,-27.9672416605789,
86.9368599782508));
#151433=CARTESIAN_POINT('Ctrl Pts',(9.59694061001989,-27.9419657850838,
87.2265639041723));
#151434=CARTESIAN_POINT('Ctrl Pts',(9.29161323374535,-27.9065809113692,
87.5065542657932));
#151435=CARTESIAN_POINT('Ctrl Pts',(8.98304848127122,-27.8708208529943,
87.7895133560748));
#151436=CARTESIAN_POINT('Ctrl Pts',(8.67233513464827,-27.8247362891609,
88.0625520408413));
#151437=CARTESIAN_POINT('Ctrl Pts',(8.36015795388373,-27.7683272198691,
88.3259133845449));
#151438=CARTESIAN_POINT('Ctrl Pts',(8.03290934727259,-27.7091948089709,
88.6019894018603));
#151439=CARTESIAN_POINT('Ctrl Pts',(7.70405253396476,-27.6387169262424,
88.867431165492));
#151440=CARTESIAN_POINT('Ctrl Pts',(7.37432879336558,-27.5568935716835,
89.1225559528047));
#151441=CARTESIAN_POINT('Ctrl Pts',(7.05118518470879,-27.4767031249279,
89.3725893422118));
#151442=CARTESIAN_POINT('Ctrl Pts',(6.72720874293467,-27.3856155196975,
89.6127138586078));
#151443=CARTESIAN_POINT('Ctrl Pts',(6.40305184743187,-27.2836307559925,
89.8432587985712));
#151444=CARTESIAN_POINT('Ctrl Pts',(6.06899380386998,-27.1785309382527,
90.0808455741904));
#151445=CARTESIAN_POINT('Ctrl Pts',(5.73474432538952,-27.0618581031527,
90.3082588254074));
#151446=CARTESIAN_POINT('Ctrl Pts',(5.40096780733715,-26.9336122506926,
90.5258874370315));
#151447=CARTESIAN_POINT('Ctrl Pts',(5.06719128928478,-26.8053663982324,
90.7435160486557));
#151448=CARTESIAN_POINT('Ctrl Pts',(4.73388767236532,-26.665547528412,90.9513603482028));
#151449=CARTESIAN_POINT('Ctrl Pts',(4.40167170800331,-26.5141556412314,
91.1498331075365));
#151450=CARTESIAN_POINT('Ctrl Pts',(4.3554809349335,-26.4931063568637,91.177428440604));
#151451=CARTESIAN_POINT('Ctrl Pts',(4.30931424153723,-26.4718422337862,
91.2048467869842));
#151452=CARTESIAN_POINT('Ctrl Pts',(4.26073795147533,-26.4492073398415,
91.2335083321911));
#151453=CARTESIAN_POINT('Ctrl Pts',(4.21216166141343,-26.4265724458968,
91.2621698773981));
#151454=CARTESIAN_POINT('Ctrl Pts',(4.16359850258958,-26.403687164881,91.2906389948733));
#151455=CARTESIAN_POINT('Ctrl Pts',(4.11505021502293,-26.3805514967941,
91.3189168005709));
#151456=CARTESIAN_POINT('Ctrl Pts',(3.92085706475633,-26.2880088244464,
91.4320280233613));
#151457=CARTESIAN_POINT('Ctrl Pts',(3.72690188042819,-26.1914599589606,
91.542078301748));
#151458=CARTESIAN_POINT('Ctrl Pts',(3.53329053955223,-26.0909049003369,
91.6491418252762));
#151459=CARTESIAN_POINT('Ctrl Pts',(3.18566624854605,-25.9103608226863,
91.8413716879006));
#151460=CARTESIAN_POINT('Ctrl Pts',(2.83915323135102,-25.7169018604478,
92.0239720877067));
#151461=CARTESIAN_POINT('Ctrl Pts',(2.49432560190691,-25.5105280136215,
92.1973876290191));
#151462=CARTESIAN_POINT('Ctrl Pts',(2.14463366168432,-25.3012429542303,
92.3732494565764));
#151463=CARTESIAN_POINT('Ctrl Pts',(1.79667501169128,-25.0786760726497,
92.5396657319217));
#151464=CARTESIAN_POINT('Ctrl Pts',(1.45099749566678,-24.8428273688797,
92.6971164647939));
#151465=CARTESIAN_POINT('Ctrl Pts',(1.37814818263882,-24.7931237715912,
92.7302981939888));
#151466=CARTESIAN_POINT('Ctrl Pts',(1.30540000319713,-24.7428302907079,
92.7630817867072));
#151467=CARTESIAN_POINT('Ctrl Pts',(1.23275780153721,-24.69194692623,92.7954718093058));
#151468=CARTESIAN_POINT('Ctrl Pts',(21.0098527486291,-19.89566736418,80.408148930172));
#151469=CARTESIAN_POINT('Ctrl Pts',(20.6551365913091,-19.99124366319,80.237482208311));
#151470=CARTESIAN_POINT('Ctrl Pts',(19.9910149156791,-20.23867708484,79.904460322262));
#151471=CARTESIAN_POINT('Ctrl Pts',(19.0648609531091,-20.80248074526,79.396961278566));
#151472=CARTESIAN_POINT('Ctrl Pts',(18.2673560862191,-21.51326965896,78.915583888499));
#151473=CARTESIAN_POINT('Ctrl Pts',(17.5939479981591,-22.37888325624,78.456835314244));
#151474=CARTESIAN_POINT('Ctrl Pts',(17.0765716352991,-23.36518757691,78.041108570563));
#151475=CARTESIAN_POINT('Ctrl Pts',(16.7338537221591,-24.42774757018,77.685128810774));
#151476=CARTESIAN_POINT('Ctrl Pts',(16.5606913794591,-25.57344706162,77.385356055912));
#151477=CARTESIAN_POINT('Ctrl Pts',(16.5711618237791,-26.34223932515,77.238423393511));
#151478=CARTESIAN_POINT('Ctrl Pts',(16.6081249192391,-26.74041077153,77.175825765138));
#151479=CARTESIAN_POINT('Ctrl Pts',(20.3926287521091,-20.2277816629,82.564474719442));
#151480=CARTESIAN_POINT('Ctrl Pts',(20.0304495599191,-20.3062712552,82.36756185427));
#151481=CARTESIAN_POINT('Ctrl Pts',(19.3485196483991,-20.52646386931,81.983339277436));
#151482=CARTESIAN_POINT('Ctrl Pts',(18.3896783510891,-21.06856485919,81.399520311364));
#151483=CARTESIAN_POINT('Ctrl Pts',(17.5596258339291,-21.77713325838,80.849001012762));
#151484=CARTESIAN_POINT('Ctrl Pts',(16.8570714683491,-22.65858032904,80.329679945766));
#151485=CARTESIAN_POINT('Ctrl Pts',(16.3180571926391,-23.67552873337,79.866533429259));
#151486=CARTESIAN_POINT('Ctrl Pts',(15.9635459865691,-24.77815848302,79.479434494296));
#151487=CARTESIAN_POINT('Ctrl Pts',(15.7884768001891,-25.96937000168,79.165303624673));
#151488=CARTESIAN_POINT('Ctrl Pts',(15.8039654328291,-26.76746529055,79.021363678754));
#151489=CARTESIAN_POINT('Ctrl Pts',(15.8446902264591,-27.17980945688,78.963423318945));
#151490=CARTESIAN_POINT('Ctrl Pts',(18.8791778988491,-20.81222181939,86.54683680967));
#151491=CARTESIAN_POINT('Ctrl Pts',(18.5090651864891,-20.85157100999,86.29682420477));
#151492=CARTESIAN_POINT('Ctrl Pts',(17.8026752686791,-21.00753396259,85.80852977002));
#151493=CARTESIAN_POINT('Ctrl Pts',(16.7884714733291,-21.49368110695,85.06979054407));
#151494=CARTESIAN_POINT('Ctrl Pts',(15.8973287740491,-22.18943159807,84.38083918167));
#151495=CARTESIAN_POINT('Ctrl Pts',(15.1358035389891,-23.09873073241,83.74432372475));
#151496=CARTESIAN_POINT('Ctrl Pts',(14.5492421568691,-24.17733474,83.19601594835));
#151497=CARTESIAN_POINT('Ctrl Pts',(14.1640926878391,-25.36315201507,82.76265760696));
#151498=CARTESIAN_POINT('Ctrl Pts',(13.9751991718891,-26.64940096258,82.442431434339));
#151499=CARTESIAN_POINT('Ctrl Pts',(13.9919355575191,-27.50824023846,82.322766335322));
#151500=CARTESIAN_POINT('Ctrl Pts',(14.0349062209691,-27.94970483338,82.28413504845));
#151501=CARTESIAN_POINT('Ctrl Pts',(16.1824725435691,-21.09209438161,90.98689436045));
#151502=CARTESIAN_POINT('Ctrl Pts',(15.8353920940991,-21.07651442269,90.66407951446));
#151503=CARTESIAN_POINT('Ctrl Pts',(15.1562212037291,-21.13655542109,90.03216892887));
#151504=CARTESIAN_POINT('Ctrl Pts',(14.1357975968091,-21.52378539238,89.08090920936));
#151505=CARTESIAN_POINT('Ctrl Pts',(13.2024016538491,-22.17634380389,88.20804330743));
#151506=CARTESIAN_POINT('Ctrl Pts',(12.3725625246191,-23.09809302245,87.42817780739));
#151507=CARTESIAN_POINT('Ctrl Pts',(11.7042631277791,-24.23734882118,86.79534712921));
#151508=CARTESIAN_POINT('Ctrl Pts',(11.2345903778791,-25.51470352118,86.3450307177));
#151509=CARTESIAN_POINT('Ctrl Pts',(10.9601647413791,-26.90758355909,86.07493152895));
#151510=CARTESIAN_POINT('Ctrl Pts',(10.9217922244791,-27.83312706015,86.02981874014));
#151511=CARTESIAN_POINT('Ctrl Pts',(10.9358081186491,-28.30574486146,86.03831960593));
#151512=CARTESIAN_POINT('Ctrl Pts',(13.6800125517991,-20.85160484736,93.96864121737));
#151513=CARTESIAN_POINT('Ctrl Pts',(13.3756529423391,-20.80305713171,93.5913417542));
#151514=CARTESIAN_POINT('Ctrl Pts',(12.7642912235491,-20.80264803255,92.85220100697));
#151515=CARTESIAN_POINT('Ctrl Pts',(11.7975700778191,-21.1189877902,91.74412056314));
#151516=CARTESIAN_POINT('Ctrl Pts',(10.8695342697591,-21.72973149919,90.73881456859));
#151517=CARTESIAN_POINT('Ctrl Pts',(10.0003460674491,-22.64000762359,89.86134820672));
#151518=CARTESIAN_POINT('Ctrl Pts',(9.25501270070909,-23.79502260284,89.1797656491));
#151519=CARTESIAN_POINT('Ctrl Pts',(8.68104170661909,-25.10559524195,88.73467241033));
#151520=CARTESIAN_POINT('Ctrl Pts',(8.27959754217909,-26.5389182176,88.52152852489));
#151521=CARTESIAN_POINT('Ctrl Pts',(8.14849243932909,-27.48840466516,88.54361140251));
#151522=CARTESIAN_POINT('Ctrl Pts',(8.11278288879909,-27.97136651022,88.59242893348));
#151523=CARTESIAN_POINT('Ctrl Pts',(11.6467057389891,-20.40077118403,95.93019164297));
#151524=CARTESIAN_POINT('Ctrl Pts',(11.3836934115591,-20.33562680778,95.51624099247));
#151525=CARTESIAN_POINT('Ctrl Pts',(10.8414362027591,-20.30310783194,94.70537766303));
#151526=CARTESIAN_POINT('Ctrl Pts',(9.93982085948909,-20.57626855614,93.49370810764));
#151527=CARTESIAN_POINT('Ctrl Pts',(9.03357187753909,-21.154608245,92.40231734157));
#151528=CARTESIAN_POINT('Ctrl Pts',(8.14288801602909,-22.044239404,91.46324854709));
#151529=CARTESIAN_POINT('Ctrl Pts',(7.33588463937909,-23.18976034117,90.75351553684));
#151530=CARTESIAN_POINT('Ctrl Pts',(6.66829790515909,-24.49809298253,90.31643495592));
#151531=CARTESIAN_POINT('Ctrl Pts',(6.14617826714909,-25.93133038039,90.14535398219));
#151532=CARTESIAN_POINT('Ctrl Pts',(5.92435902304909,-26.87930744686,90.21408009388));
#151533=CARTESIAN_POINT('Ctrl Pts',(5.83988198614909,-27.36055233645,90.29044282441));
#151534=CARTESIAN_POINT('Ctrl Pts',(9.48566925591909,-19.63589615636,97.59555314433));
#151535=CARTESIAN_POINT('Ctrl Pts',(9.27098750755909,-19.56575558261,97.15206697347));
#151536=CARTESIAN_POINT('Ctrl Pts',(8.81191716525909,-19.52082184909,96.28422750364));
#151537=CARTESIAN_POINT('Ctrl Pts',(7.99590436653909,-19.76818182049,94.99225672571));
#151538=CARTESIAN_POINT('Ctrl Pts',(7.12739780805909,-20.31659507032,93.83549487305));
#151539=CARTESIAN_POINT('Ctrl Pts',(6.22388368237909,-21.1725135457,92.85056839143));
#151540=CARTESIAN_POINT('Ctrl Pts',(5.35392344615909,-22.28183405455,92.12050954926));
#151541=CARTESIAN_POINT('Ctrl Pts',(4.58102981613909,-23.55235799666,91.69007777815));
#151542=CARTESIAN_POINT('Ctrl Pts',(3.91698303326909,-24.94497669681,91.55079655694));
#151543=CARTESIAN_POINT('Ctrl Pts',(3.58588420224909,-25.86529397632,91.65444864575));
#151544=CARTESIAN_POINT('Ctrl Pts',(3.44241434770909,-26.33204745337,91.75144897014));
#151545=CARTESIAN_POINT('Ctrl Pts',(8.00926134120909,-18.89711948749,98.48664285459));
#151546=CARTESIAN_POINT('Ctrl Pts',(7.82700873851909,-18.8309347938,98.02954612217));
#151547=CARTESIAN_POINT('Ctrl Pts',(7.42454263933909,-18.79011314066,97.13635843924));
#151548=CARTESIAN_POINT('Ctrl Pts',(6.66936590663908,-19.03092176508,95.81070161864));
#151549=CARTESIAN_POINT('Ctrl Pts',(5.83078526668909,-19.5601301908,94.62764699397));
#151550=CARTESIAN_POINT('Ctrl Pts',(4.92330275591909,-20.38384396178,93.62454790876));
#151551=CARTESIAN_POINT('Ctrl Pts',(4.01417257721909,-21.45015830713,92.88584223434));
#151552=CARTESIAN_POINT('Ctrl Pts',(3.17092794726909,-22.67084984203,92.45640650951));
#151553=CARTESIAN_POINT('Ctrl Pts',(2.40874601918909,-24.00878867259,92.32715669325));
#151554=CARTESIAN_POINT('Ctrl Pts',(2.00040163275909,-24.89318394035,92.44279977495));
#151555=CARTESIAN_POINT('Ctrl Pts',(1.81495250691909,-25.34182018804,92.54714379559));
#151556=CARTESIAN_POINT('Ctrl Pts',(7.24274295347909,-18.44807871483,98.89217210658));
#151557=CARTESIAN_POINT('Ctrl Pts',(7.07635687067909,-18.3857964445,98.429970603));
#151558=CARTESIAN_POINT('Ctrl Pts',(6.70163711703909,-18.35020608194,97.52763951722));
#151559=CARTESIAN_POINT('Ctrl Pts',(5.97659597624909,-18.59015319315,96.19061261638));
#151560=CARTESIAN_POINT('Ctrl Pts',(5.15326941421909,-19.1093773468,94.99905242918));
#151561=CARTESIAN_POINT('Ctrl Pts',(4.24452036201909,-19.91366910359,93.98998241731));
#151562=CARTESIAN_POINT('Ctrl Pts',(3.31659813599909,-20.95258803845,93.247814414));
#151563=CARTESIAN_POINT('Ctrl Pts',(2.43861741667909,-22.14079466069,92.81729138984));
#151564=CARTESIAN_POINT('Ctrl Pts',(1.62712657436909,-23.44283258147,92.68923465246));
#151565=CARTESIAN_POINT('Ctrl Pts',(1.17940863797909,-24.30369856826,92.80726391985));
#151566=CARTESIAN_POINT('Ctrl Pts',(0.972428646019088,-24.74052533156,92.9132664501));
#151567=CARTESIAN_POINT('Ctrl Pts',(7.33390977282909,-18.51896019696,98.61558102691));
#151568=CARTESIAN_POINT('Ctrl Pts',(7.17927099155909,-18.47494133476,98.21269615893));
#151569=CARTESIAN_POINT('Ctrl Pts',(6.81839532782909,-18.45454687724,97.3773696126));
#151570=CARTESIAN_POINT('Ctrl Pts',(6.12341626982909,-18.68273930707,96.10938806091));
#151571=CARTESIAN_POINT('Ctrl Pts',(5.29685182923909,-19.20408022183,94.9197080813));
#151572=CARTESIAN_POINT('Ctrl Pts',(4.38838335134909,-20.01244945753,93.91195584547));
#151573=CARTESIAN_POINT('Ctrl Pts',(3.46446828778909,-21.05710096399,93.17053740908));
#151574=CARTESIAN_POINT('Ctrl Pts',(2.59387851028909,-22.2520961092,92.74022114186));
#151575=CARTESIAN_POINT('Ctrl Pts',(1.83141007716909,-23.49861933641,92.61802875499));
#151576=CARTESIAN_POINT('Ctrl Pts',(1.41597523797909,-24.30522867552,92.71377801739));
#151577=CARTESIAN_POINT('Ctrl Pts',(1.23275780153909,-24.69194692623,92.79547180931));
#151578=CARTESIAN_POINT('Ctrl Pts',(20.8003130810766,-19.9701890920257,
80.5583314865116));
#151579=CARTESIAN_POINT('Ctrl Pts',(20.5143567750622,-20.0538194850392,
80.417262464135));
#151580=CARTESIAN_POINT('Ctrl Pts',(20.2284979684703,-20.1617475291585,
80.2714704935566));
#151581=CARTESIAN_POINT('Ctrl Pts',(19.9480670705018,-20.2953208803297,
80.1230151286706));
#151582=CARTESIAN_POINT('Ctrl Pts',(19.9273554498031,-20.3051861291485,
80.1120507476752));
#151583=CARTESIAN_POINT('Ctrl Pts',(19.9066734348693,-20.3151912438291,
80.1010718420925));
#151584=CARTESIAN_POINT('Ctrl Pts',(19.8860231713586,-20.3253367559184,
80.0900792431011));
#151585=CARTESIAN_POINT('Ctrl Pts',(19.6187303069626,-20.4566582272256,
79.947793249024));
#151586=CARTESIAN_POINT('Ctrl Pts',(19.3567592096545,-20.6115057583191,
79.8032132308831));
#151587=CARTESIAN_POINT('Ctrl Pts',(19.1051659171744,-20.7894093407683,
79.6586356218779));
#151588=CARTESIAN_POINT('Ctrl Pts',(19.0728654827711,-20.8122492302517,
79.6400742384251));
#151589=CARTESIAN_POINT('Ctrl Pts',(19.0407360588875,-20.8354690788735,
79.6215128887285));
#151590=CARTESIAN_POINT('Ctrl Pts',(19.0087883050101,-20.8590678408783,
79.6029564250444));
#151591=CARTESIAN_POINT('Ctrl Pts',(19.0080136045072,-20.8596400868291,
79.6025064496939));
#151592=CARTESIAN_POINT('Ctrl Pts',(19.0072390108282,-20.8602125555853,
79.6020564772164));
#151593=CARTESIAN_POINT('Ctrl Pts',(19.0064645241169,-20.8607852470758,
79.6016065076885));
#151594=CARTESIAN_POINT('Ctrl Pts',(18.8067701111758,-21.0084485824678,
79.4855859234624));
#151595=CARTESIAN_POINT('Ctrl Pts',(18.6140280223814,-21.1710425202242,
79.3696679926295));
#151596=CARTESIAN_POINT('Ctrl Pts',(18.4307822608431,-21.3473573891257,
79.2551990600057));
#151597=CARTESIAN_POINT('Ctrl Pts',(18.3571849327144,-21.4181710502525,
79.2092246946281));
#151598=CARTESIAN_POINT('Ctrl Pts',(18.2851192504696,-21.4911974483095,
79.163484092077));
#151599=CARTESIAN_POINT('Ctrl Pts',(18.2147489810016,-21.5663560929115,
79.1180644352836));
#151600=CARTESIAN_POINT('Ctrl Pts',(18.0422175956949,-21.7506274502474,
79.0067060965142));
#151601=CARTESIAN_POINT('Ctrl Pts',(17.8798803400537,-21.9477182068604,
78.8972777885827));
#151602=CARTESIAN_POINT('Ctrl Pts',(17.7296386708767,-22.1555609120406,
78.7910139638691));
#151603=CARTESIAN_POINT('Ctrl Pts',(17.6654106032881,-22.2444133282129,
78.7455863527854));
#151604=CARTESIAN_POINT('Ctrl Pts',(17.6033925792008,-22.3352303260424,
78.700736931842));
#151605=CARTESIAN_POINT('Ctrl Pts',(17.5437307068886,-22.4278489395183,
78.6565613612389));
#151606=CARTESIAN_POINT('Ctrl Pts',(17.5431525540228,-22.4287464594037,
78.6561332782481));
#151607=CARTESIAN_POINT('Ctrl Pts',(17.5425746223999,-22.429644148466,78.6557052585308));
#151608=CARTESIAN_POINT('Ctrl Pts',(17.5419969120972,-22.4305420065136,
78.6552773021585));
#151609=CARTESIAN_POINT('Ctrl Pts',(17.402432433722,-22.6474484550983,78.5518906954236));
#151610=CARTESIAN_POINT('Ctrl Pts',(17.275623170277,-22.8744760912279,78.4520798562389));
#151611=CARTESIAN_POINT('Ctrl Pts',(17.1627326147873,-23.1089760714818,
78.3568715393448));
#151612=CARTESIAN_POINT('Ctrl Pts',(17.1150663766594,-23.2079899513524,
78.3166713446948));
#151613=CARTESIAN_POINT('Ctrl Pts',(17.069881152779,-23.3083355314165,78.2772915997086));
#151614=CARTESIAN_POINT('Ctrl Pts',(17.0272624613387,-23.4098116755575,
78.238809035761));
#151615=CARTESIAN_POINT('Ctrl Pts',(16.9247515091058,-23.6538927539119,
78.1462467317272));
#151616=CARTESIAN_POINT('Ctrl Pts',(16.8370925179916,-23.9045154058893,
78.0588763655667));
#151617=CARTESIAN_POINT('Ctrl Pts',(16.7645015768804,-24.1586334501126,
77.9773895868215));
#151618=CARTESIAN_POINT('Ctrl Pts',(16.7351538648562,-24.2613705557055,
77.9444453863498));
#151619=CARTESIAN_POINT('Ctrl Pts',(16.708268476164,-24.3646788587115,77.9124626431124));
#151620=CARTESIAN_POINT('Ctrl Pts',(16.6838574597094,-24.4683569221556,
77.8814861175022));
#151621=CARTESIAN_POINT('Ctrl Pts',(16.6835993597175,-24.4694531201524,
77.8811585997593));
#151622=CARTESIAN_POINT('Ctrl Pts',(16.6833415363243,-24.4705493594865,
77.8808311944963));
#151623=CARTESIAN_POINT('Ctrl Pts',(16.6830839894752,-24.4716456399339,
77.8805039017331));
#151624=CARTESIAN_POINT('Ctrl Pts',(16.6075775881359,-24.7930481021296,
77.7845497139153));
#151625=CARTESIAN_POINT('Ctrl Pts',(16.5557693472223,-25.1183063542804,
77.6981708478282));
#151626=CARTESIAN_POINT('Ctrl Pts',(16.5263676979949,-25.4419090629032,
77.6218851543626));
#151627=CARTESIAN_POINT('Ctrl Pts',(16.5229178833183,-25.4798786803543,
77.6129342447419));
#151628=CARTESIAN_POINT('Ctrl Pts',(16.5197764940058,-25.517825488518,77.6041222711108));
#151629=CARTESIAN_POINT('Ctrl Pts',(16.5169414026472,-25.555740574269,77.5954500541109));
#151630=CARTESIAN_POINT('Ctrl Pts',(16.491658739231,-25.8938581973755,77.5181133069824));
#151631=CARTESIAN_POINT('Ctrl Pts',(16.4907387445089,-26.2294522321289,
77.4518927603714));
#151632=CARTESIAN_POINT('Ctrl Pts',(16.5112006384634,-26.5573269539316,
77.3965079296405));
#151633=CARTESIAN_POINT('Ctrl Pts',(16.5126507836543,-26.5805636079823,
77.392582777545));
#151634=CARTESIAN_POINT('Ctrl Pts',(16.514208303769,-26.6037614969942,77.3887120400042));
#151635=CARTESIAN_POINT('Ctrl Pts',(16.5158721297067,-26.62691877498,77.384895612979));
#151636=CARTESIAN_POINT('Ctrl Pts',(20.2362883878691,-19.21905923456,65.991441278798));
#151637=CARTESIAN_POINT('Ctrl Pts',(19.6561718605991,-19.46975913513,66.282916919374));
#151638=CARTESIAN_POINT('Ctrl Pts',(18.5598661246491,-20.16689938673,66.859928238528));
#151639=CARTESIAN_POINT('Ctrl Pts',(17.2726781923991,-21.78307897052,67.63089597445));
#151640=CARTESIAN_POINT('Ctrl Pts',(16.5149844393091,-23.77214263969,68.206347704864));
#151641=CARTESIAN_POINT('Ctrl Pts',(16.4199777461291,-25.17488001869,68.413681499209));
#151642=CARTESIAN_POINT('Ctrl Pts',(16.4654068172991,-25.86638094596,68.474205480461));
#151643=CARTESIAN_POINT('Ctrl Pts',(20.7062170281991,-19.10951799103,67.232304771193));
#151644=CARTESIAN_POINT('Ctrl Pts',(20.1158188456291,-19.37047804022,67.469676518088));
#151645=CARTESIAN_POINT('Ctrl Pts',(19.0007409478491,-20.08064708151,67.935823409705));
#151646=CARTESIAN_POINT('Ctrl Pts',(17.6829174351891,-21.69045553846,68.550905928852));
#151647=CARTESIAN_POINT('Ctrl Pts',(16.8880896066391,-23.65469053605,69.005542901801));
#151648=CARTESIAN_POINT('Ctrl Pts',(16.7656461286091,-25.03809333799,69.166985238623));
#151649=CARTESIAN_POINT('Ctrl Pts',(16.7978573856091,-25.72137447255,69.213086010125));
#151650=CARTESIAN_POINT('Ctrl Pts',(21.4160457777491,-18.98907957194,69.727647073886));
#151651=CARTESIAN_POINT('Ctrl Pts',(20.8060147882291,-19.26131652568,69.860368865498));
#151652=CARTESIAN_POINT('Ctrl Pts',(19.6537267080291,-19.98557475556,70.114357140683));
#151653=CARTESIAN_POINT('Ctrl Pts',(18.2792491310391,-21.58857984457,70.429187446299));
#151654=CARTESIAN_POINT('Ctrl Pts',(17.4249804936691,-23.52609490909,70.640240430402));
#151655=CARTESIAN_POINT('Ctrl Pts',(17.2637426655391,-24.88806220984,70.696472147368));
#151656=CARTESIAN_POINT('Ctrl Pts',(17.2779315874191,-25.56194221315,70.704594103709));
#151657=CARTESIAN_POINT('Ctrl Pts',(21.8746811002291,-19.08221580172,73.5305053260389));
#151658=CARTESIAN_POINT('Ctrl Pts',(21.2390599349591,-19.34554237141,73.5093642872265));
#151659=CARTESIAN_POINT('Ctrl Pts',(20.0327821155791,-20.05868861321,73.4527172431424));
#151660=CARTESIAN_POINT('Ctrl Pts',(18.5835345216691,-21.66698079851,73.3247462356018));
#151661=CARTESIAN_POINT('Ctrl Pts',(17.6765663617291,-23.62538478012,73.1671620379613));
#151662=CARTESIAN_POINT('Ctrl Pts',(17.5004644929091,-25.00412250867,73.0545824673722));
#151663=CARTESIAN_POINT('Ctrl Pts',(17.5116592050391,-25.68535623987,72.9985767002431));
#151664=CARTESIAN_POINT('Ctrl Pts',(21.7364082859691,-19.43942007733,77.298248370054));
#151665=CARTESIAN_POINT('Ctrl Pts',(21.0739796168191,-19.66964195353,77.120649703139));
#151666=CARTESIAN_POINT('Ctrl Pts',(19.8067642895291,-20.34082664886,76.746337439781));
#151667=CARTESIAN_POINT('Ctrl Pts',(18.2875788718191,-21.96946629291,76.170375437408));
#151668=CARTESIAN_POINT('Ctrl Pts',(17.3699668233691,-24.00779371033,75.656203729192));
#151669=CARTESIAN_POINT('Ctrl Pts',(17.2329278425291,-25.44945423035,75.398807937707));
#151670=CARTESIAN_POINT('Ctrl Pts',(17.2714592832091,-26.15774963945,75.294337547645));
#151671=CARTESIAN_POINT('Ctrl Pts',(21.2442578173891,-19.78039759178,79.688891430801));
#151672=CARTESIAN_POINT('Ctrl Pts',(20.5752522699491,-19.97334520296,79.407696162325));
#151673=CARTESIAN_POINT('Ctrl Pts',(19.2831813460191,-20.59399037267,78.818398048164));
#151674=CARTESIAN_POINT('Ctrl Pts',(17.7329461897391,-22.23903620348,77.941493589672));
#151675=CARTESIAN_POINT('Ctrl Pts',(16.8277611948191,-24.36240202829,77.208327889628));
#151676=CARTESIAN_POINT('Ctrl Pts',(16.7322184029291,-25.871198608,76.886196845068));
#151677=CARTESIAN_POINT('Ctrl Pts',(16.7953681445091,-26.60785186972,76.768881260083));
#151678=CARTESIAN_POINT('Ctrl Pts',(20.8910485624391,-19.96034543716,80.846768517016));
#151679=CARTESIAN_POINT('Ctrl Pts',(20.2240002921291,-20.13083459838,80.511741733943));
#151680=CARTESIAN_POINT('Ctrl Pts',(18.9280022641691,-20.71954229589,79.809910826839));
#151681=CARTESIAN_POINT('Ctrl Pts',(17.3693373493691,-22.37162094307,78.779154983542));
#151682=CARTESIAN_POINT('Ctrl Pts',(16.4735851577291,-24.54434556066,77.944890187453));
#151683=CARTESIAN_POINT('Ctrl Pts',(16.3981512864091,-26.09221327059,77.60473604749));
#151684=CARTESIAN_POINT('Ctrl Pts',(16.4722738819291,-26.84515323639,77.489330396979));
#151685=CARTESIAN_POINT('Origin',(22.9325866828116,-25.680307646595,65.7954246374866));
#151686=CARTESIAN_POINT('Ctrl Pts',(13.2930694310391,-20.66237848365,53.68975486087));
#151687=CARTESIAN_POINT('Ctrl Pts',(10.7180091674091,-21.08563477736,56.49440478545));
#151688=CARTESIAN_POINT('Ctrl Pts',(9.21471621113909,-23.95935693907,58.53368317417));
#151689=CARTESIAN_POINT('Ctrl Pts',(9.57611457998908,-27.76823344487,58.73202601266));
#151690=CARTESIAN_POINT('Ctrl Pts',(16.2924369462091,-20.23943758692,57.37466452154));
#151691=CARTESIAN_POINT('Ctrl Pts',(13.5489454822691,-21.02431750442,59.50105713222));
#151692=CARTESIAN_POINT('Ctrl Pts',(12.1050665875791,-23.76578490842,61.15955582037));
#151693=CARTESIAN_POINT('Ctrl Pts',(12.6176757419791,-27.21702901157,61.59573606817));
#151694=CARTESIAN_POINT('Ctrl Pts',(18.6424662440091,-19.57781353748,61.59810028618));
#151695=CARTESIAN_POINT('Ctrl Pts',(16.0534824559291,-20.58287868644,63.230417443635));
#151696=CARTESIAN_POINT('Ctrl Pts',(14.6346786905991,-23.17657072105,64.508683836537));
#151697=CARTESIAN_POINT('Ctrl Pts',(14.9438417193691,-26.33949061197,64.930416329974));
#151698=CARTESIAN_POINT('Ctrl Pts',(20.3789122648491,-19.18654856391,66.379101644893));
#151699=CARTESIAN_POINT('Ctrl Pts',(17.8362433345891,-20.29589930151,67.594481304134));
#151700=CARTESIAN_POINT('Ctrl Pts',(16.3981408222991,-22.80740317579,68.487445675464));
#151701=CARTESIAN_POINT('Ctrl Pts',(16.5805176758491,-25.82029907338,68.737672797816));
#151702=CARTESIAN_POINT('',(9.66895531238909,-27.56162305116,58.82327613956));
#151703=CARTESIAN_POINT('Ctrl Pts',(9.66895531218067,-27.56162305116,58.8232761397796));
#151704=CARTESIAN_POINT('Ctrl Pts',(9.77608710290332,-27.5422216721081,
58.9249652233086));
#151705=CARTESIAN_POINT('Ctrl Pts',(9.88895321117128,-27.5209935825139,
59.0335358873943));
#151706=CARTESIAN_POINT('Ctrl Pts',(10.0072436822018,-27.4979159451008,
59.1492633874772));
#151707=CARTESIAN_POINT('Ctrl Pts',(10.1238338517625,-27.4751700245239,
59.2633274261098));
#151708=CARTESIAN_POINT('Ctrl Pts',(10.2456935170223,-27.4506269081709,
59.3843440639975));
#151709=CARTESIAN_POINT('Ctrl Pts',(10.3724860739076,-27.4242725941385,
59.5126066600382));
#151710=CARTESIAN_POINT('Ctrl Pts',(10.4977802711195,-27.3982297198494,
59.6393535243496));
#151711=CARTESIAN_POINT('Ctrl Pts',(10.6278914412047,-27.3704177419175,
59.773176135285));
#151712=CARTESIAN_POINT('Ctrl Pts',(10.7624560785538,-27.3408375150209,
59.9143864465665));
#151713=CARTESIAN_POINT('Ctrl Pts',(10.8939955750282,-27.3119222797242,
60.0524222159102));
#151714=CARTESIAN_POINT('Ctrl Pts',(11.0297904768344,-27.281316982425,60.1975173504776));
#151715=CARTESIAN_POINT('Ctrl Pts',(11.1694648606077,-27.2490426668715,
60.3499899515095));
#151716=CARTESIAN_POINT('Ctrl Pts',(11.2447490156163,-27.2316468888535,
60.4321723146642));
#151717=CARTESIAN_POINT('Ctrl Pts',(11.321159608222,-27.2137666170437,60.516498422091));
#151718=CARTESIAN_POINT('Ctrl Pts',(11.3986333366825,-27.1954083537372,
60.6030212674793));
#151719=CARTESIAN_POINT('Ctrl Pts',(11.5378144428915,-27.1624278396215,
60.7584590600419));
#151720=CARTESIAN_POINT('Ctrl Pts',(11.6804221980073,-27.1278911831314,
60.9209786202939));
#151721=CARTESIAN_POINT('Ctrl Pts',(11.8260325426628,-27.0917696931306,
61.0908661445346));
#151722=CARTESIAN_POINT('Ctrl Pts',(11.9672281693689,-27.0567433601439,
61.2556028980357));
#151723=CARTESIAN_POINT('Ctrl Pts',(12.1112469245432,-27.0202265326995,
61.4272677115551));
#151724=CARTESIAN_POINT('Ctrl Pts',(12.2576751072232,-26.9822296355385,
61.6061393856237));
#151725=CARTESIAN_POINT('Ctrl Pts',(12.3226316538668,-26.9653739512189,
61.6854880876783));
#151726=CARTESIAN_POINT('Ctrl Pts',(12.3880619947326,-26.9482275265822,
61.7662552377078));
#151727=CARTESIAN_POINT('Ctrl Pts',(12.4539283464614,-26.9307939267627,
61.8484662788217));
#151728=CARTESIAN_POINT('Ctrl Pts',(12.5960163946389,-26.8931858597292,
62.0258133773618));
#151729=CARTESIAN_POINT('Ctrl Pts',(12.7401308506418,-26.8542263500844,
62.20987421503));
#151730=CARTESIAN_POINT('Ctrl Pts',(12.8858554081658,-26.8139086882211,
62.4008856755935));
#151731=CARTESIAN_POINT('Ctrl Pts',(12.9285667161065,-26.8020917364283,
62.4568704008242));
#151732=CARTESIAN_POINT('Ctrl Pts',(12.9714162165931,-26.7901584148067,
62.5134523061076));
#151733=CARTESIAN_POINT('Ctrl Pts',(13.0143931242072,-26.7781093321009,
62.5706375669336));
#151734=CARTESIAN_POINT('Ctrl Pts',(13.1091969498418,-26.751529961939,62.6967839510545));
#151735=CARTESIAN_POINT('Ctrl Pts',(13.2046203502908,-26.7243846635722,
62.8258654302207));
#151736=CARTESIAN_POINT('Ctrl Pts',(13.3005416224173,-26.6966735094419,
62.9579447179794));
#151737=CARTESIAN_POINT('Ctrl Pts',(13.3485022584805,-26.6828179323767,
63.0239843618587));
#151738=CARTESIAN_POINT('Ctrl Pts',(13.3965873139316,-26.6688208915697,
63.0907734856094));
#151739=CARTESIAN_POINT('Ctrl Pts',(13.4447810230397,-26.6546823959435,
63.1583196951015));
#151740=CARTESIAN_POINT('Ctrl Pts',(13.4688778775937,-26.6476131481305,
63.1920927998475));
#151741=CARTESIAN_POINT('Ctrl Pts',(13.4930018929273,-26.6405085366125,
63.2260551775518));
#151742=CARTESIAN_POINT('Ctrl Pts',(13.5171510732691,-26.6333685624621,
63.2602077741688));
#151743=CARTESIAN_POINT('Ctrl Pts',(13.5393493205099,-26.6268054034133,
63.2916012944823));
#151744=CARTESIAN_POINT('Ctrl Pts',(13.562262411493,-26.6200058659919,63.324144014503));
#151745=CARTESIAN_POINT('Ctrl Pts',(13.5839760634089,-26.6135394010544,
63.3551108659612));
#151746=CARTESIAN_POINT('Ctrl Pts',(13.5858844069735,-26.6129710840897,
63.3578324437008));
#151747=CARTESIAN_POINT('Ctrl Pts',(13.5877835133376,-26.6124053393619,
63.360541830305));
#151748=CARTESIAN_POINT('Ctrl Pts',(13.5896720985665,-26.6118425531398,
63.3632371650776));
#151749=CARTESIAN_POINT('Ctrl Pts',(13.7434389940496,-26.5660210096465,
63.582688876301));
#151750=CARTESIAN_POINT('Ctrl Pts',(13.8905072688594,-26.5215528747677,
63.7989611004999));
#151751=CARTESIAN_POINT('Ctrl Pts',(14.0312770356143,-26.4785184816057,
64.011721612069));
#151752=CARTESIAN_POINT('Ctrl Pts',(14.1764604592964,-26.4341347998013,
64.2311529587712));
#151753=CARTESIAN_POINT('Ctrl Pts',(14.3149443160671,-26.3912760346578,
64.4468487802049));
#151754=CARTESIAN_POINT('Ctrl Pts',(14.447148206126,-26.3499796557284,64.658458625851));
#151755=CARTESIAN_POINT('Ctrl Pts',(14.5816957684308,-26.3079511865625,
64.8738198295093));
#151756=CARTESIAN_POINT('Ctrl Pts',(14.7097388113884,-26.2675407051138,
65.0849487873465));
#151757=CARTESIAN_POINT('Ctrl Pts',(14.8316986288703,-26.2287394799824,
65.2914923765872));
#151758=CARTESIAN_POINT('Ctrl Pts',(14.9570468693798,-26.188860236144,65.5037743890924));
#151759=CARTESIAN_POINT('Ctrl Pts',(15.0759693110088,-26.1506806600927,
65.7112125565739));
#151760=CARTESIAN_POINT('Ctrl Pts',(15.1888995598772,-26.1141447875305,
65.9134426219291));
#151761=CARTESIAN_POINT('Ctrl Pts',(15.2627229382154,-26.0902610046637,
66.0456419819382));
#151762=CARTESIAN_POINT('Ctrl Pts',(15.3339851579122,-26.0670786871891,
66.175616142649));
#151763=CARTESIAN_POINT('Ctrl Pts',(15.4028016457588,-26.0445727674571,
66.3032679929604));
#151764=CARTESIAN_POINT('Ctrl Pts',(15.5077431731565,-26.0102524226376,
66.4979303560947));
#151765=CARTESIAN_POINT('Ctrl Pts',(15.6070091098075,-25.9775458127129,
66.6872096404678));
#151766=CARTESIAN_POINT('Ctrl Pts',(15.7010249755036,-25.9464984904361,
66.870857023816));
#151767=CARTESIAN_POINT('Ctrl Pts',(15.7985675524621,-25.9142865249331,
67.0613933645796));
#151768=CARTESIAN_POINT('Ctrl Pts',(15.890458976969,-25.8838602604155,67.2458672631598));
#151769=CARTESIAN_POINT('Ctrl Pts',(15.9771369870681,-25.8552356095173,
67.4240241675736));
#151770=CARTESIAN_POINT('Ctrl Pts',(16.0654902566879,-25.8260577188888,
67.60562437958));
#151771=CARTESIAN_POINT('Ctrl Pts',(16.1484267094834,-25.7987512123656,
67.7806610205149));
#151772=CARTESIAN_POINT('Ctrl Pts',(16.226369910093,-25.7733047959622,67.9488891587593));
#151773=CARTESIAN_POINT('Ctrl Pts',(16.3060903466905,-25.7472781584921,
68.1209531813288));
#151774=CARTESIAN_POINT('Ctrl Pts',(16.3805873111834,-25.7231968526043,
68.285894603277));
#151775=CARTESIAN_POINT('Ctrl Pts',(16.450271297183,-25.7010280500849,68.4434777168875));
#151776=CARTESIAN_POINT('Ctrl Pts',(16.4726294312709,-25.6939151811497,
68.494038320354));
#151777=CARTESIAN_POINT('Ctrl Pts',(16.4944917657597,-25.6869990726531,
68.5438416263688));
#151778=CARTESIAN_POINT('Ctrl Pts',(16.5158709371514,-25.6802783436,68.5928804245897));
#151779=CARTESIAN_POINT('Ctrl Pts',(13.2733353341602,-20.6712011628671,
53.9604716641149));
#151780=CARTESIAN_POINT('Ctrl Pts',(13.0170347351402,-20.7250378132106,
54.2388016656023));
#151781=CARTESIAN_POINT('Ctrl Pts',(12.7582063428879,-20.8115059547408,
54.5248435686163));
#151782=CARTESIAN_POINT('Ctrl Pts',(12.5030245679339,-20.9342717895189,
54.8126593880525));
#151783=CARTESIAN_POINT('Ctrl Pts',(12.2478836190979,-21.0570179831903,
55.100429160303));
#151784=CARTESIAN_POINT('Ctrl Pts',(11.9963882360896,-21.2160503044088,
55.3899721645967));
#151785=CARTESIAN_POINT('Ctrl Pts',(11.7556603016108,-21.4120189338142,
55.6738855564106));
#151786=CARTESIAN_POINT('Ctrl Pts',(11.5149131061665,-21.6080032429329,
55.9578216645163));
#151787=CARTESIAN_POINT('Ctrl Pts',(11.2849328996215,-21.8409314181471,
56.2361298209099));
#151788=CARTESIAN_POINT('Ctrl Pts',(11.0727144271428,-22.107582157184,56.5009421516352));
#151789=CARTESIAN_POINT('Ctrl Pts',(10.860495954664,-22.3742328962209,56.7657544823605));
#151790=CARTESIAN_POINT('Ctrl Pts',(10.6660393405502,-22.6746064010369,
57.0170708879501));
#151791=CARTESIAN_POINT('Ctrl Pts',(10.4949554108468,-23.0016697749345,
57.2478918360827));
#151792=CARTESIAN_POINT('Ctrl Pts',(10.3238714811434,-23.3287331488321,
57.4787127842154));
#151793=CARTESIAN_POINT('Ctrl Pts',(10.1761603811614,-23.6824865561447,
57.6890381474577));
#151794=CARTESIAN_POINT('Ctrl Pts',(10.0550128727907,-24.0531337087021,
57.8739905639562));
#151795=CARTESIAN_POINT('Ctrl Pts',(9.93386536441998,-24.4237808612596,
58.0589429804546));
#151796=CARTESIAN_POINT('Ctrl Pts',(9.83928157859918,-24.8113218760576,
58.2185223304877));
#151797=CARTESIAN_POINT('Ctrl Pts',(9.77160709345427,-25.204943088974,58.3506914591221));
#151798=CARTESIAN_POINT('Ctrl Pts',(9.70392952498099,-25.5985822357313,
58.4828666095359));
#151799=CARTESIAN_POINT('Ctrl Pts',(9.66316383171567,-25.9983020993844,
58.5876289051968));
#151800=CARTESIAN_POINT('Ctrl Pts',(9.64708646826566,-26.3940853352116,
58.6657711555562));
#151801=CARTESIAN_POINT('Ctrl Pts',(9.63101056975571,-26.7898325079914,
58.7439062857361));
#151802=CARTESIAN_POINT('Ctrl Pts',(9.63961850007943,-27.181643774797,58.7954262256073));
#151803=CARTESIAN_POINT('Ctrl Pts',(9.66895531217942,-27.56162305116,58.8232761397809));
#151804=CARTESIAN_POINT('Ctrl Pts',(9.83370851895909,-27.80605867564,58.97339667448));
#151805=CARTESIAN_POINT('Ctrl Pts',(9.78042150163909,-27.34107630378,58.94776316344));
#151806=CARTESIAN_POINT('Ctrl Pts',(9.73957619330909,-26.46196602269,58.83698460444));
#151807=CARTESIAN_POINT('Ctrl Pts',(9.86285265310909,-25.16099225256,58.48191889848));
#151808=CARTESIAN_POINT('Ctrl Pts',(10.1423397371991,-23.99302628575,57.98753584959));
#151809=CARTESIAN_POINT('Ctrl Pts',(10.5855565583291,-22.9284853311,57.3408553055));
#151810=CARTESIAN_POINT('Ctrl Pts',(11.1731667914491,-22.02730607102,56.57244262719));
#151811=CARTESIAN_POINT('Ctrl Pts',(11.8706526240191,-21.3322492191,55.72566239936));
#151812=CARTESIAN_POINT('Ctrl Pts',(12.6953086638991,-20.82524464081,54.77937302147));
#151813=CARTESIAN_POINT('Ctrl Pts',(13.2841451199891,-20.65883849192,54.13779122735));
#151814=CARTESIAN_POINT('Ctrl Pts',(13.6035760583091,-20.61577618492,53.79797816226));
#151815=CARTESIAN_POINT('Ctrl Pts',(9.11717682860909,-27.94509497959,58.28335974554));
#151816=CARTESIAN_POINT('Ctrl Pts',(9.08937096593909,-27.48943650101,58.28325601136));
#151817=CARTESIAN_POINT('Ctrl Pts',(9.09152833544909,-26.63065417243,58.22256576765));
#151818=CARTESIAN_POINT('Ctrl Pts',(9.25956437210909,-25.3622681632,57.9493381346));
#151819=CARTESIAN_POINT('Ctrl Pts',(9.56072435519909,-24.22097731061,57.53587587343));
#151820=CARTESIAN_POINT('Ctrl Pts',(10.0031416783291,-23.17251910771,56.97022060426));
#151821=CARTESIAN_POINT('Ctrl Pts',(10.5684535699491,-22.2708802756,56.27615356594));
#151822=CARTESIAN_POINT('Ctrl Pts',(11.2265639643191,-21.55595641958,55.48995245848));
#151823=CARTESIAN_POINT('Ctrl Pts',(11.9972985087991,-21.00770518571,54.58814904501));
#151824=CARTESIAN_POINT('Ctrl Pts',(12.5456331782291,-20.80111230341,53.95883282879));
#151825=CARTESIAN_POINT('Ctrl Pts',(12.8433966925291,-20.73414220241,53.62023291165));
#151826=CARTESIAN_POINT('Ctrl Pts',(7.67397546574909,-27.95817851065,57.02941707911));
#151827=CARTESIAN_POINT('Ctrl Pts',(7.69368603541909,-27.52958047589,57.06769883325));
#151828=CARTESIAN_POINT('Ctrl Pts',(7.77522018889909,-26.72684409599,57.08322556095));
#151829=CARTESIAN_POINT('Ctrl Pts',(8.02617065688909,-25.5458747545,56.93925035408));
#151830=CARTESIAN_POINT('Ctrl Pts',(8.36984268079909,-24.47883173608,56.65894378471));
#151831=CARTESIAN_POINT('Ctrl Pts',(8.81690277762909,-23.48440306249,56.23363513379));
#151832=CARTESIAN_POINT('Ctrl Pts',(9.35082782543909,-22.60491801913,55.67727937557));
#151833=CARTESIAN_POINT('Ctrl Pts',(9.94832565112909,-21.87364104583,55.01448586002));
#151834=CARTESIAN_POINT('Ctrl Pts',(10.6327613513191,-21.2662171359,54.21867473302));
#151835=CARTESIAN_POINT('Ctrl Pts',(11.1140271747291,-20.99177940337,53.63518616128));
#151836=CARTESIAN_POINT('Ctrl Pts',(11.3752399880891,-20.8821982339,53.31253580915));
#151837=CARTESIAN_POINT('Ctrl Pts',(5.43454356140909,-27.31037712512,55.42201572643));
#151838=CARTESIAN_POINT('Ctrl Pts',(5.51448681552909,-26.94233731382,55.49057385725));
#151839=CARTESIAN_POINT('Ctrl Pts',(5.69390299566909,-26.25877334963,55.57050017209));
#151840=CARTESIAN_POINT('Ctrl Pts',(6.04460295007909,-25.25758388311,55.55120905308));
#151841=CARTESIAN_POINT('Ctrl Pts',(6.44021683080909,-24.34738618168,55.41345947614));
#151842=CARTESIAN_POINT('Ctrl Pts',(6.89728546114909,-23.48295592214,55.15425267772));
#151843=CARTESIAN_POINT('Ctrl Pts',(7.40253140983909,-22.6912641974,54.77930163254));
#151844=CARTESIAN_POINT('Ctrl Pts',(7.93992038432909,-21.99506265131,54.30127049136));
#151845=CARTESIAN_POINT('Ctrl Pts',(8.53600518809909,-21.36454828166,53.69386025715));
#151846=CARTESIAN_POINT('Ctrl Pts',(8.94653057408909,-21.02974712498,53.22152798187));
#151847=CARTESIAN_POINT('Ctrl Pts',(9.16848657809909,-20.87597367229,52.95148886331));
#151848=CARTESIAN_POINT('Ctrl Pts',(3.16862316927909,-26.0820046989,54.08896136514));
#151849=CARTESIAN_POINT('Ctrl Pts',(3.29227522776909,-25.78649730686,54.16665648107));
#151850=CARTESIAN_POINT('Ctrl Pts',(3.53973649723909,-25.24218736313,54.27316853242));
#151851=CARTESIAN_POINT('Ctrl Pts',(3.95473450660909,-24.44846538033,54.3262374297));
#151852=CARTESIAN_POINT('Ctrl Pts',(4.38029066318909,-23.7229939639,54.28628502759));
#151853=CARTESIAN_POINT('Ctrl Pts',(4.83896404899909,-23.02265304565,54.15509276207));
#151854=CARTESIAN_POINT('Ctrl Pts',(5.32122666807909,-22.36221887555,53.93421344229));
#151855=CARTESIAN_POINT('Ctrl Pts',(5.81665422799909,-21.75492892715,53.62885834605));
#151856=CARTESIAN_POINT('Ctrl Pts',(6.35405727128909,-21.16863778309,53.21732561724));
#151857=CARTESIAN_POINT('Ctrl Pts',(6.71912917933909,-20.82346967198,52.87878574479));
#151858=CARTESIAN_POINT('Ctrl Pts',(6.91624503764909,-20.65240575508,52.67904764169));
#151859=CARTESIAN_POINT('Ctrl Pts',(1.72141832568909,-24.85893421638,53.39227235504));
#151860=CARTESIAN_POINT('Ctrl Pts',(1.86138775815909,-24.6196947487,53.46571529331));
#151861=CARTESIAN_POINT('Ctrl Pts',(2.13156694140909,-24.18090919594,53.57170084919));
#151862=CARTESIAN_POINT('Ctrl Pts',(2.56163415524909,-23.54217452337,53.64706858042));
#151863=CARTESIAN_POINT('Ctrl Pts',(2.98733474422909,-22.95640933389,53.64868782902));
#151864=CARTESIAN_POINT('Ctrl Pts',(3.43416123779909,-22.38592628414,53.58043254411));
#151865=CARTESIAN_POINT('Ctrl Pts',(3.89513691238909,-21.83981625833,53.44278035182));
#151866=CARTESIAN_POINT('Ctrl Pts',(4.36284999481909,-21.32642311508,53.23837114653));
#151867=CARTESIAN_POINT('Ctrl Pts',(4.86681861189909,-20.81543581553,52.95074037956));
#151868=CARTESIAN_POINT('Ctrl Pts',(5.20856241979909,-20.50033960173,52.7054128393));
#151869=CARTESIAN_POINT('Ctrl Pts',(5.39352276268909,-20.3389852037,52.55789591871));
#151870=CARTESIAN_POINT('Ctrl Pts',(1.02430073505909,-24.12637036333,53.08835936746));
#151871=CARTESIAN_POINT('Ctrl Pts',(1.16810393818909,-23.91739391685,53.15797563719));
#151872=CARTESIAN_POINT('Ctrl Pts',(1.44218254462909,-23.53489557941,53.2607313398));
#151873=CARTESIAN_POINT('Ctrl Pts',(1.87042680159909,-22.97863212377,53.3428746214));
#151874=CARTESIAN_POINT('Ctrl Pts',(2.28892063595909,-22.46782016658,53.36102867422));
#151875=CARTESIAN_POINT('Ctrl Pts',(2.72399825596909,-21.96847658261,53.31982149989));
#151876=CARTESIAN_POINT('Ctrl Pts',(3.16990258487909,-21.48741537387,53.21940714362));
#151877=CARTESIAN_POINT('Ctrl Pts',(3.62058593277909,-21.03095975614,53.06152914518));
#151878=CARTESIAN_POINT('Ctrl Pts',(4.10556888538909,-20.57090981072,52.8326281048));
#151879=CARTESIAN_POINT('Ctrl Pts',(4.43482038252909,-20.28194513784,52.63297059822));
#151880=CARTESIAN_POINT('Ctrl Pts',(4.61342437641909,-20.13207988419,52.51162123628));
#151881=CARTESIAN_POINT('',(4.64910226411582,-20.256889925637,52.5918790595098));
#151882=CARTESIAN_POINT('Ctrl Pts',(13.2733140793291,-20.67108058276,53.96047540136));
#151883=CARTESIAN_POINT('Ctrl Pts',(12.2257002710903,-20.8471678309609,
53.716470749042));
#151884=CARTESIAN_POINT('Ctrl Pts',(10.9703341069513,-20.9769066735361,
53.4506422512973));
#151885=CARTESIAN_POINT('Ctrl Pts',(8.80304421585373,-20.9341539530389,
53.0822538172543));
#151886=CARTESIAN_POINT('Ctrl Pts',(8.03200170493279,-20.879883044699,52.9648770407774));
#151887=CARTESIAN_POINT('Ctrl Pts',(6.40018947062691,-20.6595239703279,
52.7558525862709));
#151888=CARTESIAN_POINT('Ctrl Pts',(5.54011073138219,-20.4932266343529,
52.6644263554667));
#151889=CARTESIAN_POINT('Ctrl Pts',(4.64910232197909,-20.25688994124,52.59187906431));
#151890=CARTESIAN_POINT('Ctrl Pts',(1.23275780153909,-24.13180332393,53.18230696385));
#151891=CARTESIAN_POINT('Ctrl Pts',(1.56529619659252,-24.4648844502913,
53.3305806378981));
#151892=CARTESIAN_POINT('Ctrl Pts',(1.91017087927006,-24.7772692564106,
53.4915985803787));
#151893=CARTESIAN_POINT('Ctrl Pts',(2.44441765738417,-25.2148019852262,
53.7546160241926));
#151894=CARTESIAN_POINT('Ctrl Pts',(2.7157702493135,-25.4258072295432,53.8914992340918));
#151895=CARTESIAN_POINT('Ctrl Pts',(3.03935596163509,-25.6583980544209,
54.0611380827515));
#151896=CARTESIAN_POINT('Ctrl Pts',(3.17949164949788,-25.7551694164772,
54.1360291895486));
#151897=CARTESIAN_POINT('Ctrl Pts',(3.2732338566531,-25.8190368978406,54.1864494810047));
#151898=CARTESIAN_POINT('Ctrl Pts',(3.32167141204987,-25.8515803170269,
54.2126726960811));
#151899=CARTESIAN_POINT('Ctrl Pts',(3.7336884124416,-26.1247656165185,54.4371296540365));
#151900=CARTESIAN_POINT('Ctrl Pts',(4.10147301394926,-26.3429261082056,
54.6473927299034));
#151901=CARTESIAN_POINT('Ctrl Pts',(4.65436136270961,-26.6331605172783,
54.9796968619355));
#151902=CARTESIAN_POINT('Ctrl Pts',(4.83885836952416,-26.7237375988929,
55.0932827520693));
#151903=CARTESIAN_POINT('Ctrl Pts',(5.20805692641525,-26.8925563193026,
55.3262165785686));
#151904=CARTESIAN_POINT('Ctrl Pts',(5.39398822008854,-26.9712778269078,
55.4463787381086));
#151905=CARTESIAN_POINT('Ctrl Pts',(7.04522995475302,-27.6156242640875,
56.5396614650258));
#151906=CARTESIAN_POINT('Ctrl Pts',(8.41433224598033,-27.7885413226464,
57.6323927517983));
#151907=CARTESIAN_POINT('Ctrl Pts',(9.66895531238909,-27.56162305116,58.82327613956));
#151908=CARTESIAN_POINT('Ctrl Pts',(4.64905724122965,-20.257198923201,52.5914164071972));
#151909=CARTESIAN_POINT('Ctrl Pts',(4.50275090268148,-20.3831082015137,
52.6897565959011));
#151910=CARTESIAN_POINT('Ctrl Pts',(4.35430396620251,-20.5157369186716,
52.7806356884754));
#151911=CARTESIAN_POINT('Ctrl Pts',(4.20464821630592,-20.6544868135792,
52.8630552368816));
#151912=CARTESIAN_POINT('Ctrl Pts',(4.05499508653927,-20.7932342792934,
52.9454733423099));
#151913=CARTESIAN_POINT('Ctrl Pts',(3.90413325971158,-20.93810265643,53.0194321268842));
#151914=CARTESIAN_POINT('Ctrl Pts',(3.75308161321061,-21.088286535986,53.0841158328481));
#151915=CARTESIAN_POINT('Ctrl Pts',(3.60203018546341,-21.238470198045,53.1487994451366));
#151916=CARTESIAN_POINT('Ctrl Pts',(3.4507846295339,-21.3939734096786,53.2042102799266));
#151917=CARTESIAN_POINT('Ctrl Pts',(3.30039658837663,-21.5538219581052,
53.2497670004603));
#151918=CARTESIAN_POINT('Ctrl Pts',(3.15000547702269,-21.7136737698662,
53.2953246510421));
#151919=CARTESIAN_POINT('Ctrl Pts',(3.00047190286233,-21.8778711070341,
53.3310277919671));
#151920=CARTESIAN_POINT('Ctrl Pts',(2.85284338538292,-22.0453003764685,
53.3565587080005));
#151921=CARTESIAN_POINT('Ctrl Pts',(2.70521775660114,-22.2127263697572,
53.3820891244617));
#151922=CARTESIAN_POINT('Ctrl Pts',(2.55950120823532,-22.3833824781628,
53.3974479391146));
#151923=CARTESIAN_POINT('Ctrl Pts',(2.41668848157172,-22.556065276394,53.4026001826463));
#151924=CARTESIAN_POINT('Ctrl Pts',(2.27387308141089,-22.7287513072992,
53.4077525226295));
#151925=CARTESIAN_POINT('Ctrl Pts',(2.13396160307715,-22.9034641166288,
53.4026979090517));
#151926=CARTESIAN_POINT('Ctrl Pts',(1.99785109332966,-23.0789669753365,
53.3876812805484));
#151927=CARTESIAN_POINT('Ctrl Pts',(1.86174244805379,-23.2544674299675,
53.3726648577461));
#151928=CARTESIAN_POINT('Ctrl Pts',(1.72943577324374,-23.4307564927545,
53.3476868010187));
#151929=CARTESIAN_POINT('Ctrl Pts',(1.6016934803756,-23.6066202710027,53.3132525943462));
#151930=CARTESIAN_POINT('Ctrl Pts',(1.4739500791378,-23.7824855751518,53.2788180889015));
#151931=CARTESIAN_POINT('Ctrl Pts',(1.35077113556768,-23.9579255954924,
53.2349272654012));
#151932=CARTESIAN_POINT('Ctrl Pts',(1.23275780153644,-24.13180332393,53.1823069638559));
#151933=CARTESIAN_POINT('Ctrl Pts',(-2.42455476508091,-16.92552468831,52.4988667111));
#151934=CARTESIAN_POINT('Ctrl Pts',(-2.42455476508091,-16.92552468831,52.4988667111));
#151935=CARTESIAN_POINT('Ctrl Pts',(-2.42455476508091,-16.92552468831,52.4988667111));
#151936=CARTESIAN_POINT('Ctrl Pts',(-2.42455476508091,-16.92552468831,52.4988667111));
#151937=CARTESIAN_POINT('Ctrl Pts',(0.0925700926990874,-18.66477847312,
52.37303551213));
#151938=CARTESIAN_POINT('Ctrl Pts',(-0.40352170620526,-19.01823830871,52.3978351662936));
#151939=CARTESIAN_POINT('Ctrl Pts',(-0.895515371595163,-19.3752846472,52.4224299545554));
#151940=CARTESIAN_POINT('Ctrl Pts',(-1.38380702798091,-19.73620495593,52.4468396792));
#151941=CARTESIAN_POINT('Ctrl Pts',(2.61806989089909,-19.62553369534,52.3800215797));
#151942=CARTESIAN_POINT('Ctrl Pts',(1.81091627060909,-20.56849142381,52.7494537592));
#151943=CARTESIAN_POINT('Ctrl Pts',(0.882002567539087,-21.47590869842,52.81681492777));
#151944=CARTESIAN_POINT('Ctrl Pts',(-0.118702425890913,-22.29896448428,
52.57846424995));
#151945=CARTESIAN_POINT('Ctrl Pts',(4.9224142687991,-20.20104612485,52.52308494659));
#151946=CARTESIAN_POINT('Ctrl Pts',(3.58550549598909,-21.31670369689,53.48424000451));
#151947=CARTESIAN_POINT('Ctrl Pts',(2.28444022049909,-22.80320843748,53.71713075241));
#151948=CARTESIAN_POINT('Ctrl Pts',(1.23910472621909,-24.40940586234,53.18227139459));
#151949=CARTESIAN_POINT('Ctrl Pts',(-2.42458295845305,-16.925539708287,
52.4988706296685));
#151950=CARTESIAN_POINT('Ctrl Pts',(-0.0053251185174313,-18.6527258434453,
52.3779300787027));
#151951=CARTESIAN_POINT('Ctrl Pts',(2.43348027117323,-19.659441558893,52.4080762030945));
#151952=CARTESIAN_POINT('Ctrl Pts',(4.64910226411582,-20.256889925637,52.5918790595098));
#151953=CARTESIAN_POINT('Ctrl Pts',(-3.40710623457991,16.74987807225,53.26489050321));
#151954=CARTESIAN_POINT('Ctrl Pts',(-3.44015780858091,16.7877187014,53.18678205605));
#151955=CARTESIAN_POINT('Ctrl Pts',(-3.47411659594991,16.81609088261,52.97739892932));
#151956=CARTESIAN_POINT('Ctrl Pts',(-3.39900274290291,16.69301953239,52.69930032793));
#151957=CARTESIAN_POINT('Ctrl Pts',(-3.25700159720791,16.48893470772,52.5247826245));
#151958=CARTESIAN_POINT('Ctrl Pts',(-3.13465059761291,16.32595396115,52.53248719305));
#151959=CARTESIAN_POINT('Ctrl Pts',(-3.08228869862991,16.25860810914,52.56532557876));
#151960=CARTESIAN_POINT('Ctrl Pts',(-1.68908392749091,18.03638543845,53.15637468044));
#151961=CARTESIAN_POINT('Ctrl Pts',(-1.71662850822091,18.07757909273,53.07756727486));
#151962=CARTESIAN_POINT('Ctrl Pts',(-1.74342672971091,18.10925496055,52.86678217038));
#151963=CARTESIAN_POINT('Ctrl Pts',(-1.67460039708091,17.97699686228,52.58972356196));
#151964=CARTESIAN_POINT('Ctrl Pts',(-1.54908851454091,17.75659770341,52.41886569374));
#151965=CARTESIAN_POINT('Ctrl Pts',(-1.44337391233091,17.58052643821,52.43072285259));
#151966=CARTESIAN_POINT('Ctrl Pts',(-1.39876593617091,17.50798340364,52.46536694065));
#151967=CARTESIAN_POINT('Ctrl Pts',(1.07693460833909,19.50311649761,53.0718773398));
#151968=CARTESIAN_POINT('Ctrl Pts',(1.05895121514909,19.54755046649,52.99188495825));
#151969=CARTESIAN_POINT('Ctrl Pts',(1.04578197976909,19.5815972729,52.7800824925));
#151970=CARTESIAN_POINT('Ctrl Pts',(1.10522958526909,19.43847226411,52.50633463755));
#151971=CARTESIAN_POINT('Ctrl Pts',(1.20316906527909,19.2002287929,52.34113102147));
#151972=CARTESIAN_POINT('Ctrl Pts',(1.28101030741909,19.01007425153,52.35751934278));
#151973=CARTESIAN_POINT('Ctrl Pts',(1.31310458513909,18.93178446037,52.39404246105));
#151974=CARTESIAN_POINT('Ctrl Pts',(5.06563032373909,20.59484478841,53.20623240665));
#151975=CARTESIAN_POINT('Ctrl Pts',(5.06183880814909,20.63957292805,53.12452214098));
#151976=CARTESIAN_POINT('Ctrl Pts',(5.06883951965909,20.66983858451,52.91500285754));
#151977=CARTESIAN_POINT('Ctrl Pts',(5.11505284373909,20.51752889178,52.65037067022));
#151978=CARTESIAN_POINT('Ctrl Pts',(5.17349613021909,20.26928325906,52.49244770842));
#151979=CARTESIAN_POINT('Ctrl Pts',(5.21143059488909,20.07103705068,52.50969456771));
#151980=CARTESIAN_POINT('Ctrl Pts',(5.22557289505909,19.98809984277,52.54636284127));
#151981=CARTESIAN_POINT('Ctrl Pts',(8.03610849690909,20.9874015617,53.42437431764));
#151982=CARTESIAN_POINT('Ctrl Pts',(8.04194577030909,21.02949187638,53.34171129579));
#151983=CARTESIAN_POINT('Ctrl Pts',(8.06158500465909,21.05225963239,53.13607983203));
#151984=CARTESIAN_POINT('Ctrl Pts',(8.09708351090909,20.8951095524,52.88025240482));
#151985=CARTESIAN_POINT('Ctrl Pts',(8.12753901812909,20.64660776267,52.72716979148));
#151986=CARTESIAN_POINT('Ctrl Pts',(8.13794707847909,20.44893917348,52.74223755693));
#151987=CARTESIAN_POINT('Ctrl Pts',(8.13954305478909,20.36490533889,52.77763238708));
#151988=CARTESIAN_POINT('Ctrl Pts',(11.0180886174491,20.97321204109,53.77155255328));
#151989=CARTESIAN_POINT('Ctrl Pts',(11.0335416724191,21.01102056917,53.68814340185));
#151990=CARTESIAN_POINT('Ctrl Pts',(11.0647526508891,21.02428219291,53.48823744763));
#151991=CARTESIAN_POINT('Ctrl Pts',(11.0893040268491,20.86530603859,53.24298148565));
#151992=CARTESIAN_POINT('Ctrl Pts',(11.0926876599891,20.62232524553,53.09440600867));
#151993=CARTESIAN_POINT('Ctrl Pts',(11.0761562910891,20.42936878983,53.10499311365));
#151994=CARTESIAN_POINT('Ctrl Pts',(11.0648480929591,20.34538349142,53.13787754361));
#151995=CARTESIAN_POINT('Ctrl Pts',(13.9644070623891,20.57916431854,54.23506456235));
#151996=CARTESIAN_POINT('Ctrl Pts',(13.9865267092991,20.6105729157,54.15122252992));
#151997=CARTESIAN_POINT('Ctrl Pts',(14.0231526773991,20.61201672497,53.95854525182));
#151998=CARTESIAN_POINT('Ctrl Pts',(14.0348030158591,20.4536887321,53.72503837394));
#151999=CARTESIAN_POINT('Ctrl Pts',(14.0145811381691,20.22163133078,53.58068290002));
#152000=CARTESIAN_POINT('Ctrl Pts',(13.9764484038391,20.03814293245,53.5851099017));
#152001=CARTESIAN_POINT('Ctrl Pts',(13.9544275408291,19.95608272267,53.6144092451));
#152002=CARTESIAN_POINT('Ctrl Pts',(16.8058284233791,19.81821401566,54.80384410726));
#152003=CARTESIAN_POINT('Ctrl Pts',(16.8340781940791,19.84189616667,54.72032170736));
#152004=CARTESIAN_POINT('Ctrl Pts',(16.8745289432991,19.83117104756,54.53653151378));
#152005=CARTESIAN_POINT('Ctrl Pts',(16.8736965349691,19.6764455665,54.31559597181));
#152006=CARTESIAN_POINT('Ctrl Pts',(16.8319008500691,19.45952204084,54.17500204704));
#152007=CARTESIAN_POINT('Ctrl Pts',(16.7734706797691,19.28889909667,54.17167264988));
#152008=CARTESIAN_POINT('Ctrl Pts',(16.7404857641791,19.21029645639,54.19614555997));
#152009=CARTESIAN_POINT('Ctrl Pts',(20.4359206765091,18.34298649127,55.67611292805));
#152010=CARTESIAN_POINT('Ctrl Pts',(20.4667388630091,18.3565819536,55.59285186564));
#152011=CARTESIAN_POINT('Ctrl Pts',(20.5029573525391,18.33245952273,55.42066915017));
#152012=CARTESIAN_POINT('Ctrl Pts',(20.4833180003491,18.18716761514,55.21617862709));
#152013=CARTESIAN_POINT('Ctrl Pts',(20.4184049676391,17.99415985211,55.08085560007));
#152014=CARTESIAN_POINT('Ctrl Pts',(20.3415140559391,17.84264224454,55.06763848037));
#152015=CARTESIAN_POINT('Ctrl Pts',(20.2980266000691,17.76951098269,55.08547709476));
#152016=CARTESIAN_POINT('Ctrl Pts',(23.7046130034791,16.23826005541,56.66962621578));
#152017=CARTESIAN_POINT('Ctrl Pts',(23.7384091580691,16.23740974354,56.59057333489));
#152018=CARTESIAN_POINT('Ctrl Pts',(23.7713882524891,16.19742240036,56.43482429516));
#152019=CARTESIAN_POINT('Ctrl Pts',(23.7362797661591,16.06486082624,56.24764430893));
#152020=CARTESIAN_POINT('Ctrl Pts',(23.6513044671591,15.90303658722,56.11563173389));
#152021=CARTESIAN_POINT('Ctrl Pts',(23.5556796510791,15.7805203603,56.0886553188));
#152022=CARTESIAN_POINT('Ctrl Pts',(23.4996641483091,15.71978669272,56.09627230119));
#152023=CARTESIAN_POINT('Ctrl Pts',(26.5074730295191,13.55520149323,57.66170186843));
#152024=CARTESIAN_POINT('Ctrl Pts',(26.5345305319991,13.54877802608,57.58393577616));
#152025=CARTESIAN_POINT('Ctrl Pts',(26.5521243712991,13.50849899519,57.43829414488));
#152026=CARTESIAN_POINT('Ctrl Pts',(26.4999080877691,13.39758649353,57.26420353995));
#152027=CARTESIAN_POINT('Ctrl Pts',(26.4031994683291,13.26626054144,57.13712372676));
#152028=CARTESIAN_POINT('Ctrl Pts',(26.3023331084391,13.16639120647,57.10285417391));
#152029=CARTESIAN_POINT('Ctrl Pts',(26.2421213057291,13.11480416125,57.10387121501));
#152030=CARTESIAN_POINT('Ctrl Pts',(28.0260365809591,11.66012040095,58.24862470654));
#152031=CARTESIAN_POINT('Ctrl Pts',(28.0476816641691,11.65292670417,58.1714936895));
#152032=CARTESIAN_POINT('Ctrl Pts',(28.0551995851891,11.61658071257,58.03118300585));
#152033=CARTESIAN_POINT('Ctrl Pts',(27.9934517031191,11.5216568794,57.86408561232));
#152034=CARTESIAN_POINT('Ctrl Pts',(27.8911848302791,11.40987079221,57.73990245967));
#152035=CARTESIAN_POINT('Ctrl Pts',(27.7887895379791,11.32361591897,57.70211559891));
#152036=CARTESIAN_POINT('Ctrl Pts',(27.7271521339691,11.27764565271,57.69964977519));
#152037=CARTESIAN_POINT('Ctrl Pts',(29.0847447463191,10.01576377267,58.6800910282));
#152038=CARTESIAN_POINT('Ctrl Pts',(29.1032139923391,10.00691673868,58.60442319409));
#152039=CARTESIAN_POINT('Ctrl Pts',(29.1047538730291,9.97257820357701,58.46908444647));
#152040=CARTESIAN_POINT('Ctrl Pts',(29.0369066999691,9.89056585094001,58.30730489342));
#152041=CARTESIAN_POINT('Ctrl Pts',(28.9304374574991,9.79604558653101,58.18476641947));
#152042=CARTESIAN_POINT('Ctrl Pts',(28.8258605611791,9.72374971286802,58.14350537075));
#152043=CARTESIAN_POINT('Ctrl Pts',(28.7623207753191,9.68480362226701,58.13771481948));
#152044=CARTESIAN_POINT('Ctrl Pts',(30.0344103243391,8.28039375792901,59.07930366752));
#152045=CARTESIAN_POINT('Ctrl Pts',(30.0494068162891,8.27099728743901,59.00486237631));
#152046=CARTESIAN_POINT('Ctrl Pts',(30.0449146508391,8.24027854369101,58.87380147701));
#152047=CARTESIAN_POINT('Ctrl Pts',(29.9714373510291,8.17217495521601,58.71670125264));
#152048=CARTESIAN_POINT('Ctrl Pts',(29.8614874735291,8.09516504455002,58.59575014517));
#152049=CARTESIAN_POINT('Ctrl Pts',(29.7555116330291,8.03666664573201,58.55162412187));
#152050=CARTESIAN_POINT('Ctrl Pts',(29.6906397264391,8.00479089321601,58.54295901742));
#152051=CARTESIAN_POINT('Ctrl Pts',(30.9865852142591,5.98897834251701,59.49800326924));
#152052=CARTESIAN_POINT('Ctrl Pts',(30.9977138336291,5.98144064890401,59.42489819269));
#152053=CARTESIAN_POINT('Ctrl Pts',(30.9869121544591,5.95858128531701,59.29817025603));
#152054=CARTESIAN_POINT('Ctrl Pts',(30.9078234541491,5.90949647884401,59.14574880578));
#152055=CARTESIAN_POINT('Ctrl Pts',(30.7945343219091,5.85422246716001,59.02644072744));
#152056=CARTESIAN_POINT('Ctrl Pts',(30.6873012573491,5.81183682443201,58.97952488484));
#152057=CARTESIAN_POINT('Ctrl Pts',(30.6211478216291,5.78824194237301,58.96792696849));
#152058=CARTESIAN_POINT('Ctrl Pts',(31.6985560499091,3.05950795606701,59.82186454665));
#152059=CARTESIAN_POINT('Ctrl Pts',(31.7058639729391,3.05463005644801,59.74964937203));
#152060=CARTESIAN_POINT('Ctrl Pts',(31.6893593933991,3.04179231445501,59.62595519273));
#152061=CARTESIAN_POINT('Ctrl Pts',(31.6058009611491,3.01644898656901,59.47692924067));
#152062=CARTESIAN_POINT('Ctrl Pts',(31.4904078016391,2.98871223998301,59.35895991202));
#152063=CARTESIAN_POINT('Ctrl Pts',(31.3831023081891,2.96791198367201,59.31023304863));
#152064=CARTESIAN_POINT('Ctrl Pts',(31.3166485767291,2.95635194048101,59.29658677628));
#152065=CARTESIAN_POINT('Ctrl Pts',(31.9528697870491,0.0317595130754642,
59.94136526076));
#152066=CARTESIAN_POINT('Ctrl Pts',(31.9595118395691,0.0317214715852542,
59.86982005549));
#152067=CARTESIAN_POINT('Ctrl Pts',(31.9418703744391,0.0316044173649042,
59.7476393923));
#152068=CARTESIAN_POINT('Ctrl Pts',(31.8570592176591,0.0313477725403642,
59.59998716507));
#152069=CARTESIAN_POINT('Ctrl Pts',(31.7405930043491,0.0310540693394842,
59.48235757363));
#152070=CARTESIAN_POINT('Ctrl Pts',(31.6324015555691,0.0308217453532442,
59.43260160338));
#152071=CARTESIAN_POINT('Ctrl Pts',(31.5651520458091,0.0306880972146742,
59.41790430726));
#152072=CARTESIAN_POINT('Ctrl Pts',(31.7096390339091,-2.99439664410999,
59.8269624593));
#152073=CARTESIAN_POINT('Ctrl Pts',(31.7168773774691,-2.98964919846099,
59.75475691015));
#152074=CARTESIAN_POINT('Ctrl Pts',(31.7002725349691,-2.97711986729099,
59.63110422964));
#152075=CARTESIAN_POINT('Ctrl Pts',(31.6166408408991,-2.95233086026699,
59.48212883459));
#152076=CARTESIAN_POINT('Ctrl Pts',(31.5012193086591,-2.92517228349799,
59.36418257283));
#152077=CARTESIAN_POINT('Ctrl Pts',(31.3939231685891,-2.90477741108599,
59.31543332717));
#152078=CARTESIAN_POINT('Ctrl Pts',(31.3274729253591,-2.89343129713299,
59.30175933843));
#152079=CARTESIAN_POINT('Ctrl Pts',(31.0044106669691,-5.93536919510399,
59.50603336636));
#152080=CARTESIAN_POINT('Ctrl Pts',(31.0154731923991,-5.92785021371099,
59.43296090614));
#152081=CARTESIAN_POINT('Ctrl Pts',(31.0045638706991,-5.90513994487099,
59.30632287634));
#152082=CARTESIAN_POINT('Ctrl Pts',(30.9253751969791,-5.85648208176699,
59.15399206733));
#152083=CARTESIAN_POINT('Ctrl Pts',(30.8120201776491,-5.80172712439799,
59.0347122833));
#152084=CARTESIAN_POINT('Ctrl Pts',(30.7047528103491,-5.75976080252899,
58.98773724997));
#152085=CARTESIAN_POINT('Ctrl Pts',(30.6385665932191,-5.73639908315999,
58.97607793401));
#152086=CARTESIAN_POINT('Ctrl Pts',(30.0557145698791,-8.23704896139899,
59.08843189482));
#152087=CARTESIAN_POINT('Ctrl Pts',(30.0705985394091,-8.22770398536199,
59.01400704745));
#152088=CARTESIAN_POINT('Ctrl Pts',(30.0659296562591,-8.19715733411999,
58.88302652709));
#152089=CARTESIAN_POINT('Ctrl Pts',(29.9923124410791,-8.12942617515799,
58.72602481875));
#152090=CARTESIAN_POINT('Ctrl Pts',(29.8823004329491,-8.05282051051399,
58.60511553591));
#152091=CARTESIAN_POINT('Ctrl Pts',(29.7763309397791,-7.99459750740499,
58.56094125343));
#152092=CARTESIAN_POINT('Ctrl Pts',(29.7114575444091,-7.96285095315699,
58.5522226205));
#152093=CARTESIAN_POINT('Ctrl Pts',(29.1078599310991,-9.97750665916399,
58.68964302613));
#152094=CARTESIAN_POINT('Ctrl Pts',(29.1262401562691,-9.96865880744899,
58.61399984743));
#152095=CARTESIAN_POINT('Ctrl Pts',(29.1276254743691,-9.93441589189099,
58.47875913071));
#152096=CARTESIAN_POINT('Ctrl Pts',(29.0596373139691,-9.85271906620799,
58.31709135142));
#152097=CARTESIAN_POINT('Ctrl Pts',(28.9530857827691,-9.75858037769199,
58.19459310768));
#152098=CARTESIAN_POINT('Ctrl Pts',(28.8484829788591,-9.68656808159099,
58.15326699513));
#152099=CARTESIAN_POINT('Ctrl Pts',(28.7849174247891,-9.64775830644099,
58.14741097197));
#152100=CARTESIAN_POINT('Ctrl Pts',(28.0475935276391,-11.63113612008,58.25712100103));
#152101=CARTESIAN_POINT('Ctrl Pts',(28.0691745203191,-11.62390612933,58.18001298797));
#152102=CARTESIAN_POINT('Ctrl Pts',(28.0765679313191,-11.58758738077,58.0397958346));
#152103=CARTESIAN_POINT('Ctrl Pts',(28.0146927415291,-11.49289309856,57.8728042192));
#152104=CARTESIAN_POINT('Ctrl Pts',(27.9123405097291,-11.38141696717,57.74865628821));
#152105=CARTESIAN_POINT('Ctrl Pts',(27.8099051124691,-11.29540682901,57.71080399278));
#152106=CARTESIAN_POINT('Ctrl Pts',(27.7482330766891,-11.24955318315,57.70827617846));
#152107=CARTESIAN_POINT('Ctrl Pts',(26.5214437291491,-13.54032966652,57.66695703587));
#152108=CARTESIAN_POINT('Ctrl Pts',(26.5485508020591,-13.53380889766,57.58923687734));
#152109=CARTESIAN_POINT('Ctrl Pts',(26.5661819088591,-13.49343887783,57.44369998587));
#152110=CARTESIAN_POINT('Ctrl Pts',(26.5139245004491,-13.38261131029,57.26969608568));
#152111=CARTESIAN_POINT('Ctrl Pts',(26.4171148585491,-13.25148782603,57.14262203634));
#152112=CARTESIAN_POINT('Ctrl Pts',(26.3161138823091,-13.15183237676,57.10826642317));
#152113=CARTESIAN_POINT('Ctrl Pts',(26.2558011253391,-13.10036270574,57.10921336507));
#152114=CARTESIAN_POINT('Ctrl Pts',(23.7055625057091,-16.23941370425,56.66968418131));
#152115=CARTESIAN_POINT('Ctrl Pts',(23.7395296243291,-16.23843525767,56.59069809116));
#152116=CARTESIAN_POINT('Ctrl Pts',(23.7727467150091,-16.19825706731,56.43505039964));
#152117=CARTESIAN_POINT('Ctrl Pts',(23.7377218800291,-16.06561772276,56.24791478528));
#152118=CARTESIAN_POINT('Ctrl Pts',(23.6526468582291,-15.90385847186,56.11586590366));
#152119=CARTESIAN_POINT('Ctrl Pts',(23.5567952192891,-15.78150421852,56.08879317878));
#152120=CARTESIAN_POINT('Ctrl Pts',(23.5006236139291,-15.72087914736,56.09634553719));
#152121=CARTESIAN_POINT('Ctrl Pts',(20.4063581786991,-18.35659770911,55.66857977841));
#152122=CARTESIAN_POINT('Ctrl Pts',(20.4372924338591,-18.37025081134,55.58533314885));
#152123=CARTESIAN_POINT('Ctrl Pts',(20.4737750944691,-18.34617970186,55.41308873976));
#152124=CARTESIAN_POINT('Ctrl Pts',(20.4543781545091,-18.20077654436,55.20848050105));
#152125=CARTESIAN_POINT('Ctrl Pts',(20.3895554076191,-18.00758317946,55.07309921297));
#152126=CARTESIAN_POINT('Ctrl Pts',(20.3126053147691,-17.85594411037,55.05992821344));
#152127=CARTESIAN_POINT('Ctrl Pts',(20.2690822741291,-17.78278504154,55.07780473431));
#152128=CARTESIAN_POINT('Ctrl Pts',(16.7993745713591,-19.82194976627,54.80194949585));
#152129=CARTESIAN_POINT('Ctrl Pts',(16.8273405443191,-19.84574005463,54.71836633499));
#152130=CARTESIAN_POINT('Ctrl Pts',(16.8673426669891,-19.83518836646,54.53445056239));
#152131=CARTESIAN_POINT('Ctrl Pts',(16.8663605573891,-19.68049552455,54.31343739281));
#152132=CARTESIAN_POINT('Ctrl Pts',(16.8247934988291,-19.46345295172,54.17287454728));
#152133=CARTESIAN_POINT('Ctrl Pts',(16.7668216086291,-19.29265043197,54.16966394249));
#152134=CARTESIAN_POINT('Ctrl Pts',(16.7341161278291,-19.21395367916,54.19420937311));
#152135=CARTESIAN_POINT('Ctrl Pts',(13.9657231564391,-20.57828465165,54.23548724589));
#152136=CARTESIAN_POINT('Ctrl Pts',(13.9879455534891,-20.60966085868,54.15166605761));
#152137=CARTESIAN_POINT('Ctrl Pts',(14.0247403784291,-20.61105128252,53.95902957051));
#152138=CARTESIAN_POINT('Ctrl Pts',(14.0364529343591,-20.45271034974,53.72554558312));
#152139=CARTESIAN_POINT('Ctrl Pts',(14.0161518533491,-20.22068637473,53.5811777803));
#152140=CARTESIAN_POINT('Ctrl Pts',(13.9778536334091,-20.03725207962,53.58556593897));
#152141=CARTESIAN_POINT('Ctrl Pts',(13.9557336715891,-19.95522093542,53.61484203308));
#152142=CARTESIAN_POINT('Ctrl Pts',(11.0113131159191,-20.97458758877,53.77033478716));
#152143=CARTESIAN_POINT('Ctrl Pts',(11.0266214897391,-21.0124365846,53.68690337854));
#152144=CARTESIAN_POINT('Ctrl Pts',(11.0575930742591,-21.02577068253,53.48693796005));
#152145=CARTESIAN_POINT('Ctrl Pts',(11.0820802461291,-20.86680750785,53.24163470357));
#152146=CARTESIAN_POINT('Ctrl Pts',(11.0856142047891,-20.62377642666,53.09306635909));
#152147=CARTESIAN_POINT('Ctrl Pts',(11.0693440424891,-20.43075299565,53.10370892621));
#152148=CARTESIAN_POINT('Ctrl Pts',(11.0581825160391,-20.34673852124,53.13662523048));
#152149=CARTESIAN_POINT('Ctrl Pts',(8.04813110016909,-20.98752038782,53.42572108627));
#152150=CARTESIAN_POINT('Ctrl Pts',(8.05403136395909,-21.02958615157,53.34306054731));
#152151=CARTESIAN_POINT('Ctrl Pts',(8.07375925218909,-21.05230244721,53.13746098213));
#152152=CARTESIAN_POINT('Ctrl Pts',(8.10923075950909,-20.89513781208,52.88167951425));
#152153=CARTESIAN_POINT('Ctrl Pts',(8.13955926130909,-20.64666172642,52.728611378));
#152154=CARTESIAN_POINT('Ctrl Pts',(8.14981954849909,-20.44902373923,52.74365318103));
#152155=CARTESIAN_POINT('Ctrl Pts',(8.15134070741909,-20.36499744938,52.77903315124));
#152156=CARTESIAN_POINT('Ctrl Pts',(5.07309482417909,-20.59608243382,53.20669897951));
#152157=CARTESIAN_POINT('Ctrl Pts',(5.06935091329909,-20.64081249018,53.12498643087));
#152158=CARTESIAN_POINT('Ctrl Pts',(5.07642996605909,-20.6710738593,52.91547662321));
#152159=CARTESIAN_POINT('Ctrl Pts',(5.12263597221909,-20.51875562994,52.65086622165));
#152160=CARTESIAN_POINT('Ctrl Pts',(5.18098777968909,-20.27050002442,52.49295530845));
#152161=CARTESIAN_POINT('Ctrl Pts',(5.21881036298909,-20.07224017422,52.51019701694));
#152162=CARTESIAN_POINT('Ctrl Pts',(5.23289940429909,-19.98929249306,52.5468624545));
#152163=CARTESIAN_POINT('Ctrl Pts',(1.08063148447909,-19.50530743072,53.07169077902));
#152164=CARTESIAN_POINT('Ctrl Pts',(1.06264699612909,-19.54974310474,52.99169611687));
#152165=CARTESIAN_POINT('Ctrl Pts',(1.04946942829909,-19.58378828415,52.77988994916));
#152166=CARTESIAN_POINT('Ctrl Pts',(1.10889319615909,-19.44064471873,52.50614477021));
#152167=CARTESIAN_POINT('Ctrl Pts',(1.20680757944909,-19.20237679195,52.34094946877));
#152168=CARTESIAN_POINT('Ctrl Pts',(1.28463643807909,-19.01220687809,52.35734645449));
#152169=CARTESIAN_POINT('Ctrl Pts',(1.31672726259909,-18.93391206485,52.39387330581));
#152170=CARTESIAN_POINT('Ctrl Pts',(-1.69053559703091,-18.03599000716,53.15636154203));
#152171=CARTESIAN_POINT('Ctrl Pts',(-1.71808399435091,-18.07718359794,53.07755602641));
#152172=CARTESIAN_POINT('Ctrl Pts',(-1.74488816840091,-18.10886086129,52.8667717657));
#152173=CARTESIAN_POINT('Ctrl Pts',(-1.67605689913091,-17.97660542263,52.5897100818));
#152174=CARTESIAN_POINT('Ctrl Pts',(-1.55053199647091,-17.75620898753,52.41884899955));
#152175=CARTESIAN_POINT('Ctrl Pts',(-1.44480576140091,-17.58014026888,52.43070527192));
#152176=CARTESIAN_POINT('Ctrl Pts',(-1.40019337549091,-17.50759891703,52.4653489107));
#152177=CARTESIAN_POINT('Ctrl Pts',(-3.41135153547391,-16.74669685633,53.26515925386));
#152178=CARTESIAN_POINT('Ctrl Pts',(-3.44441691723091,-16.78452916259,53.18705230737));
#152179=CARTESIAN_POINT('Ctrl Pts',(-3.47839365781991,-16.8128930659,52.97767245609));
#152180=CARTESIAN_POINT('Ctrl Pts',(-3.40326426680091,-16.68984456638,52.6995713555));
#152181=CARTESIAN_POINT('Ctrl Pts',(-3.26122207631491,-16.48580033262,52.52504467785));
#152182=CARTESIAN_POINT('Ctrl Pts',(-3.13882947022291,-16.32285201154,52.53273894012));
#152183=CARTESIAN_POINT('Ctrl Pts',(-3.08644810130291,-16.25551893355,52.56557287499));
#152184=CARTESIAN_POINT('Ctrl Pts',(28.7709983219891,10.49234437565,58.41163725334));
#152185=CARTESIAN_POINT('Ctrl Pts',(29.3461221071324,9.56300210468609,58.5927697031041));
#152186=CARTESIAN_POINT('Ctrl Pts',(29.8057154407229,8.63828625185421,58.7510834555065));
#152187=CARTESIAN_POINT('Ctrl Pts',(30.3555567806281,7.32278537807955,58.9515072191109));
#152188=CARTESIAN_POINT('Ctrl Pts',(30.5159033093088,6.89496887683618,59.0121909318143));
#152189=CARTESIAN_POINT('Ctrl Pts',(30.7271988464659,6.27166620909241,59.0941761584547));
#152190=CARTESIAN_POINT('Ctrl Pts',(30.7927562218314,6.06695929915259,59.1200015382421));
#152191=CARTESIAN_POINT('Ctrl Pts',(30.8843957051587,5.76472441168283,59.1565412167044));
#152192=CARTESIAN_POINT('Ctrl Pts',(30.9285417571211,5.6148146654431,59.174262504219));
#152193=CARTESIAN_POINT('Ctrl Pts',(30.9772641233391,5.44211882506228,59.1940072984711));
#152194=CARTESIAN_POINT('Ctrl Pts',(30.9975645193261,5.36858589133721,59.2022733859752));
#152195=CARTESIAN_POINT('Ctrl Pts',(31.0109707890621,5.31967141993883,59.207740935901));
#152196=CARTESIAN_POINT('Ctrl Pts',(31.0172412021778,5.29663432717222,59.2103021252824));
#152197=CARTESIAN_POINT('Ctrl Pts',(31.2464496779949,4.44801620230947,59.3040810454547));
#152198=CARTESIAN_POINT('Ctrl Pts',(31.422068609294,3.59228160990379,59.3800803609666));
#152199=CARTESIAN_POINT('Ctrl Pts',(31.6042594119283,2.26851847251972,59.4602965423362));
#152200=CARTESIAN_POINT('Ctrl Pts',(31.6513458307658,1.8206038811692,59.4813869362216));
#152201=CARTESIAN_POINT('Ctrl Pts',(31.7151442513319,0.91351085499764,59.510151984243));
#152202=CARTESIAN_POINT('Ctrl Pts',(31.7318541630843,0.452133816180361,
59.5178257421016));
#152203=CARTESIAN_POINT('Ctrl Pts',(31.7312760050765,-0.932164512008769,
59.5175336001747));
#152204=CARTESIAN_POINT('Ctrl Pts',(31.6642947229183,-1.8377192754502,59.4867196198187));
#152205=CARTESIAN_POINT('Ctrl Pts',(31.4817290686544,-3.15982924914525,
59.4064276877234));
#152206=CARTESIAN_POINT('Ctrl Pts',(31.4071817438355,-3.59455586282469,
59.3739951040488));
#152207=CARTESIAN_POINT('Ctrl Pts',(31.2763107521092,-4.23624383665348,
59.3182294737973));
#152208=CARTESIAN_POINT('Ctrl Pts',(31.20610676927,-4.55448733964118,59.2885671381903));
#152209=CARTESIAN_POINT('Ctrl Pts',(31.1161324157846,-4.92091881738991,
59.2511517616297));
#152210=CARTESIAN_POINT('Ctrl Pts',(31.0691585581828,-5.10288463135961,
59.2317800728514));
#152211=CARTESIAN_POINT('Ctrl Pts',(31.0486044725996,-5.18059821864631,
59.2233396726097));
#152212=CARTESIAN_POINT('Ctrl Pts',(31.0348082285965,-5.23234645161641,
59.2176824672922));
#152213=CARTESIAN_POINT('Ctrl Pts',(31.0275426096999,-5.2593743437665,59.2147075866874));
#152214=CARTESIAN_POINT('Ctrl Pts',(30.8074085273367,-6.07212759538227,
59.124699826665));
#152215=CARTESIAN_POINT('Ctrl Pts',(30.5296965601241,-6.9095815185838,59.0148863513764));
#152216=CARTESIAN_POINT('Ctrl Pts',(29.7963024629428,-8.65873560151838,
58.7476516372334));
#152217=CARTESIAN_POINT('Ctrl Pts',(29.3397689438772,-9.57385470219907,
58.5906228748175));
#152218=CARTESIAN_POINT('Ctrl Pts',(28.7710188797691,-10.4923807534,58.41162797882));
#152219=CARTESIAN_POINT('',(31.3508441160571,-2.89782725707868,59.2994353999759));
#152220=CARTESIAN_POINT('Ctrl Pts',(-2.42458242200845,-16.9255392716443,
52.4988706032414));
#152221=CARTESIAN_POINT('Ctrl Pts',(-2.16632614325253,-17.0988665935668,
52.4859654166524));
#152222=CARTESIAN_POINT('Ctrl Pts',(-1.77248405024906,-17.3574983428894,
52.4672011127588));
#152223=CARTESIAN_POINT('Ctrl Pts',(-0.683856029902338,-17.9865695496037,
52.4313748176118));
#152224=CARTESIAN_POINT('Ctrl Pts',(0.0112588477405891,-18.3570638684891,
52.4140653025779));
#152225=CARTESIAN_POINT('Ctrl Pts',(1.74522869355982,-19.1099025180147,
52.4092811029507));
#152226=CARTESIAN_POINT('Ctrl Pts',(2.78684201670358,-19.4924676991997,
52.4220745510272));
#152227=CARTESIAN_POINT('Ctrl Pts',(4.62995700479528,-19.9672626057456,
52.5002241852911));
#152228=CARTESIAN_POINT('Ctrl Pts',(5.29041794170216,-20.1085904800991,
52.5361613138869));
#152229=CARTESIAN_POINT('Ctrl Pts',(6.34669362641008,-20.2783653160647,
52.6104108949246));
#152230=CARTESIAN_POINT('Ctrl Pts',(6.70968283517132,-20.3279138961736,
52.6385567608978));
#152231=CARTESIAN_POINT('Ctrl Pts',(7.26966232137013,-20.3894369756384,
52.6866276868625));
#152232=CARTESIAN_POINT('Ctrl Pts',(7.45890139848648,-20.4078101042906,
52.703627261911));
#152233=CARTESIAN_POINT('Ctrl Pts',(7.7464903526402,-20.4318771574289,52.7306905966657));
#152234=CARTESIAN_POINT('Ctrl Pts',(7.8912170624135,-20.4430374054714,52.7446133131957));
#152235=CARTESIAN_POINT('Ctrl Pts',(8.03731286798729,-20.4528321403702,
52.7591418792631));
#152236=CARTESIAN_POINT('Ctrl Pts',(8.13501083043728,-20.4590522649648,
52.7689644007653));
#152237=CARTESIAN_POINT('Ctrl Pts',(8.18277051725864,-20.4619368764897,
52.7738167642272));
#152238=CARTESIAN_POINT('Ctrl Pts',(9.03936739200707,-20.5106917172357,
52.8618159068938));
#152239=CARTESIAN_POINT('Ctrl Pts',(9.80729514858892,-20.5097894221079,
52.9551892516658));
#152240=CARTESIAN_POINT('Ctrl Pts',(11.2671631570161,-20.4406463677333,
53.1547980920525));
#152241=CARTESIAN_POINT('Ctrl Pts',(11.9598251615053,-20.372355709591,53.2611368412179));
#152242=CARTESIAN_POINT('Ctrl Pts',(13.2615957830399,-20.1912275376119,
53.4784379682602));
#152243=CARTESIAN_POINT('Ctrl Pts',(13.8702498411828,-20.0784030226057,
53.5893650768242));
#152244=CARTESIAN_POINT('Ctrl Pts',(15.0001057677037,-19.8273770812652,
53.8090163975912));
#152245=CARTESIAN_POINT('Ctrl Pts',(15.5220355823112,-19.6891188015656,
53.917755928775));
#152246=CARTESIAN_POINT('Ctrl Pts',(16.9657920465214,-19.2595772205367,
54.2330585459834));
#152247=CARTESIAN_POINT('Ctrl Pts',(17.7658807493745,-18.9547675909247,
54.4281742547284));
#152248=CARTESIAN_POINT('Ctrl Pts',(18.7466149156235,-18.5395730455278,
54.6790754654745));
#152249=CARTESIAN_POINT('Ctrl Pts',(19.0369211658129,-18.4078755443859,
54.7558732415921));
#152250=CARTESIAN_POINT('Ctrl Pts',(19.4200611720369,-18.2266064375923,
54.8593141333102));
#152251=CARTESIAN_POINT('Ctrl Pts',(19.5390521798461,-18.1688795566976,
54.8918415325469));
#152252=CARTESIAN_POINT('Ctrl Pts',(19.7047275048477,-18.0869728282722,
54.9375482806614));
#152253=CARTESIAN_POINT('Ctrl Pts',(19.7843617015479,-18.0471889741464,
54.9596307963868));
#152254=CARTESIAN_POINT('Ctrl Pts',(19.8717173989075,-18.0029455223164,
54.9840156643012));
#152255=CARTESIAN_POINT('Ctrl Pts',(19.9140141553603,-17.9813809461242,
54.9958603571947));
#152256=CARTESIAN_POINT('Ctrl Pts',(19.9370470702791,-17.9695995807222,
55.0023205552476));
#152257=CARTESIAN_POINT('Ctrl Pts',(19.9480768337365,-17.963946438888,55.0054171538287));
#152258=CARTESIAN_POINT('Ctrl Pts',(19.9539307327573,-17.9609433195311,
55.0070613659337));
#152259=CARTESIAN_POINT('Ctrl Pts',(19.9532979363362,-17.9612680880685,
55.0068835935327));
#152260=CARTESIAN_POINT('Ctrl Pts',(21.0278979566056,-17.4098385978704,
55.3087502062728));
#152261=CARTESIAN_POINT('Ctrl Pts',(21.9872307161722,-16.8135812747035,
55.6059399606889));
#152262=CARTESIAN_POINT('Ctrl Pts',(23.6910635202309,-15.5993991122065,
56.1641237827156));
#152263=CARTESIAN_POINT('Ctrl Pts',(24.435605244222,-14.9813640950237,56.4252882101671));
#152264=CARTESIAN_POINT('Ctrl Pts',(25.247874111132,-14.2286703298098,56.7215268452324));
#152265=CARTESIAN_POINT('Ctrl Pts',(25.4044436438363,-14.0790877401365,
56.7792954404312));
#152266=CARTESIAN_POINT('Ctrl Pts',(25.5742363860013,-13.912277103095,56.8425741476889));
#152267=CARTESIAN_POINT('Ctrl Pts',(25.5930140841894,-13.8937629692774,
56.8495813745036));
#152268=CARTESIAN_POINT('Ctrl Pts',(25.6163765984874,-13.8706465997973,
56.8583106542445));
#152269=CARTESIAN_POINT('Ctrl Pts',(25.6203716430044,-13.8666893334539,
56.8598039775691));
#152270=CARTESIAN_POINT('Ctrl Pts',(25.6250546777405,-13.8620488471939,
56.8615546475305));
#152271=CARTESIAN_POINT('Ctrl Pts',(25.6321124084277,-13.8550515852847,
56.8641934725242));
#152272=CARTESIAN_POINT('Ctrl Pts',(25.6583551719979,-13.8289925783274,
56.87401011471));
#152273=CARTESIAN_POINT('Ctrl Pts',(25.7232460854031,-13.7642200861319,
56.8983224964411));
#152274=CARTESIAN_POINT('Ctrl Pts',(25.7894094547597,-13.6973144323053,
56.9232125149742));
#152275=CARTESIAN_POINT('Ctrl Pts',(26.0234759713672,-13.4581110773956,
57.011563091923));
#152276=CARTESIAN_POINT('Ctrl Pts',(26.2542570915582,-13.2151383992763,
57.0995489930895));
#152277=CARTESIAN_POINT('Ctrl Pts',(26.6550819662342,-12.76395485381,57.2556012621352));
#152278=CARTESIAN_POINT('Ctrl Pts',(26.7977477960912,-12.5990667370465,
57.3116159859511));
#152279=CARTESIAN_POINT('Ctrl Pts',(27.0234979757553,-12.3284864287904,
57.4012178390993));
#152280=CARTESIAN_POINT('Ctrl Pts',(27.1007028704835,-12.2344160295773,
57.4320135793588));
#152281=CARTESIAN_POINT('Ctrl Pts',(27.2191777995056,-12.0872864063817,
57.4795325384023));
#152282=CARTESIAN_POINT('Ctrl Pts',(27.2572852694891,-12.039567521655,57.4948544239221));
#152283=CARTESIAN_POINT('Ctrl Pts',(27.3445926257812,-11.9290532178486,
57.5300656388903));
#152284=CARTESIAN_POINT('Ctrl Pts',(27.5604418089713,-11.6529181842193,
57.6173801481391));
#152285=CARTESIAN_POINT('Ctrl Pts',(27.7643266128138,-11.3777193887521,
57.7011000161376));
#152286=CARTESIAN_POINT('Ctrl Pts',(27.9980297334884,-11.0490467215497,
57.7980621647422));
#152287=CARTESIAN_POINT('Ctrl Pts',(28.0741046541145,-10.9397499691282,
57.829800052545));
#152288=CARTESIAN_POINT('Ctrl Pts',(28.1855445418666,-10.7762761581739,
57.8765286440429));
#152289=CARTESIAN_POINT('Ctrl Pts',(28.2405962231963,-10.6946569176132,
57.8996730544128));
#152290=CARTESIAN_POINT('Ctrl Pts',(28.3036677385792,-10.5996568939419,
57.926287847214));
#152291=CARTESIAN_POINT('Ctrl Pts',(28.3382644776577,-10.5471314185549,
57.9409136599995));
#152292=CARTESIAN_POINT('Ctrl Pts',(28.354909008582,-10.5217355082056,57.9479581567594));
#152293=CARTESIAN_POINT('Ctrl Pts',(28.3637623064331,-10.5081959854576,
57.9517071228317));
#152294=CARTESIAN_POINT('Ctrl Pts',(28.3642504980367,-10.5074494502633,
57.9519138455112));
#152295=CARTESIAN_POINT('Ctrl Pts',(28.8072822136622,-9.82946303269992,
58.1395456803965));
#152296=CARTESIAN_POINT('Ctrl Pts',(29.1403891456331,-9.23551770479662,
58.2856110436817));
#152297=CARTESIAN_POINT('Ctrl Pts',(29.4261543259507,-8.688189577794,58.4120568897489));
#152298=CARTESIAN_POINT('Ctrl Pts',(29.4604742612531,-8.62164741825242,
58.4272743459153));
#152299=CARTESIAN_POINT('Ctrl Pts',(29.4932810185291,-8.55725794934168,
58.4418500563432));
#152300=CARTESIAN_POINT('Ctrl Pts',(29.5005342269758,-8.54300244064415,
58.4450733190014));
#152301=CARTESIAN_POINT('Ctrl Pts',(29.5065481546985,-8.53116535843972,
58.4477464851833));
#152302=CARTESIAN_POINT('Ctrl Pts',(29.5219173193004,-8.50083863653641,
58.4545807132889));
#152303=CARTESIAN_POINT('Ctrl Pts',(29.5524550061442,-8.44032846541405,
58.468168930256));
#152304=CARTESIAN_POINT('Ctrl Pts',(29.6622351103387,-8.22005640629188,
58.5171135902792));
#152305=CARTESIAN_POINT('Ctrl Pts',(29.7555017141154,-8.02473479822831,
58.5589693357939));
#152306=CARTESIAN_POINT('Ctrl Pts',(29.9676270401634,-7.56596255809928,
58.6545706892795));
#152307=CARTESIAN_POINT('Ctrl Pts',(30.0934291407565,-7.27346040122188,
58.7118290030969));
#152308=CARTESIAN_POINT('Ctrl Pts',(30.4305361920918,-6.43983351878229,
58.8661833811409));
#152309=CARTESIAN_POINT('Ctrl Pts',(30.6017015221323,-5.94273501237737,
58.9458453456209));
#152310=CARTESIAN_POINT('Ctrl Pts',(30.8690696439402,-5.08181461271089,
59.0707799223984));
#152311=CARTESIAN_POINT('Ctrl Pts',(30.9654862405048,-4.71824198664394,
59.1162478879745));
#152312=CARTESIAN_POINT('Ctrl Pts',(31.1092511104897,-4.13547169174936,
59.1842138846025));
#152313=CARTESIAN_POINT('Ctrl Pts',(31.1566306792003,-3.91615800091589,
59.2067439642156));
#152314=CARTESIAN_POINT('Ctrl Pts',(31.1882788539873,-3.76670242305925,
59.2217970147776));
#152315=CARTESIAN_POINT('Ctrl Pts',(31.1899279068987,-3.75890358193124,
59.22258140472));
#152316=CARTESIAN_POINT('Ctrl Pts',(31.191526235068,-3.75132682256149,59.2233417271164));
#152317=CARTESIAN_POINT('Ctrl Pts',(31.1924272284903,-3.74705165499355,
59.2237703419836));
#152318=CARTESIAN_POINT('Ctrl Pts',(31.192451412363,-3.74693784764103,59.2237818430606));
#152319=CARTESIAN_POINT('Ctrl Pts',(31.1979880818164,-3.72064228839014,
59.2264157979236));
#152320=CARTESIAN_POINT('Ctrl Pts',(31.2126539379119,-3.65031692538155,
59.2333953052197));
#152321=CARTESIAN_POINT('Ctrl Pts',(31.246169304696,-3.4847989670745,59.2493626506961));
#152322=CARTESIAN_POINT('Ctrl Pts',(31.2950308030585,-3.22808531019791,
59.2726919096464));
#152323=CARTESIAN_POINT('Ctrl Pts',(31.3318892564873,-3.01441384823045,
59.2903439354106));
#152324=CARTESIAN_POINT('Ctrl Pts',(31.3508441160571,-2.89782725707868,
59.2994353999759));
#152325=CARTESIAN_POINT('Ctrl Pts',(31.3508441160571,-2.89782725707868,
59.2994353999759));
#152326=CARTESIAN_POINT('Ctrl Pts',(31.3643364183393,-2.8148394868934,59.3059068163245));
#152327=CARTESIAN_POINT('Ctrl Pts',(31.3773700640756,-2.7311139651831,59.3121655266745));
#152328=CARTESIAN_POINT('Ctrl Pts',(31.4502627075308,-2.24043316614677,
59.3472058793744));
#152329=CARTESIAN_POINT('Ctrl Pts',(31.4993601963515,-1.81721685765294,
59.37096887932));
#152330=CARTESIAN_POINT('Ctrl Pts',(31.5507955538991,-1.15800595548692,
59.3959648098905));
#152331=CARTESIAN_POINT('Ctrl Pts',(31.5642321680799,-0.934211156047476,
59.4025178792687));
#152332=CARTESIAN_POINT('Ctrl Pts',(31.5780945074336,-0.592634550543183,
59.4092925482075));
#152333=CARTESIAN_POINT('Ctrl Pts',(31.5834518610784,-0.420375857261311,
59.4119157264788));
#152334=CARTESIAN_POINT('Ctrl Pts',(31.5867810664521,-0.216886265457119,
59.4135496999944));
#152335=CARTESIAN_POINT('Ctrl Pts',(31.5876940015959,-0.114518307268904,
59.4139985958855));
#152336=CARTESIAN_POINT('Ctrl Pts',(31.587988345412,-0.0576788530393498,
59.4141436080728));
#152337=CARTESIAN_POINT('Ctrl Pts',(31.5880664968281,-0.030124188040783,
59.4141822360037));
#152338=CARTESIAN_POINT('Ctrl Pts',(31.5880920817686,-0.0154155323770532,
59.4141949345244));
#152339=CARTESIAN_POINT('Ctrl Pts',(31.5880975749401,-0.0117660961253776,
59.4141976654743));
#152340=CARTESIAN_POINT('Ctrl Pts',(31.5881079907109,-0.00446340954013271,
59.4142028472302));
#152341=CARTESIAN_POINT('Ctrl Pts',(31.5895013220746,0.0964852093340877,
59.4148793415132));
#152342=CARTESIAN_POINT('Ctrl Pts',(31.5855029882768,0.48579525851113,59.4129096994819));
#152343=CARTESIAN_POINT('Ctrl Pts',(31.5800613279519,0.774270040535324,
59.4102263740453));
#152344=CARTESIAN_POINT('Ctrl Pts',(31.5523869457887,1.25116702736311,59.3967794752227));
#152345=CARTESIAN_POINT('Ctrl Pts',(31.5457695059732,1.35235209954351,59.3935675439545));
#152346=CARTESIAN_POINT('Ctrl Pts',(31.5367893723556,1.47267497284401,59.389216101337));
#152347=CARTESIAN_POINT('Ctrl Pts',(31.5357702172396,1.48613429659454,59.3887223420515));
#152348=CARTESIAN_POINT('Ctrl Pts',(31.5336880180921,1.51323299734914,59.3877137448108));
#152349=CARTESIAN_POINT('Ctrl Pts',(31.5331308836647,1.52036036184975,59.3874439247427));
#152350=CARTESIAN_POINT('Ctrl Pts',(31.5309008599961,1.54873986803599,59.3863639530715));
#152351=CARTESIAN_POINT('Ctrl Pts',(31.5263460591525,1.60550490001567,59.3841585276368));
#152352=CARTESIAN_POINT('Ctrl Pts',(31.5086031540121,1.81370488806439,59.3755720940963));
#152353=CARTESIAN_POINT('Ctrl Pts',(31.4584603244844,2.30622542292442,59.3513450096757));
#152354=CARTESIAN_POINT('Ctrl Pts',(31.3940473453495,2.76111324379761,59.3203351614487));
#152355=CARTESIAN_POINT('Ctrl Pts',(31.3176164948346,3.21526317021081,59.2836744519205));
#152356=CARTESIAN_POINT('Ctrl Pts',(31.2901345172591,3.36652440870389,59.2705120269015));
#152357=CARTESIAN_POINT('Ctrl Pts',(31.2458949964513,3.59312731575648,59.2493663033884));
#152358=CARTESIAN_POINT('Ctrl Pts',(31.2316141424242,3.6638916111659,59.2425462348826));
#152359=CARTESIAN_POINT('Ctrl Pts',(31.1995969954496,3.81740185029469,59.2272723803715));
#152360=CARTESIAN_POINT('Ctrl Pts',(31.1822274256952,3.89816656063337,59.2189941580727));
#152361=CARTESIAN_POINT('Ctrl Pts',(31.1255610878174,4.15232744849929,59.1920240911793));
#152362=CARTESIAN_POINT('Ctrl Pts',(31.081720998449,4.33760261137644,59.1712019338395));
#152363=CARTESIAN_POINT('Ctrl Pts',(31.017540391408,4.58828507862619,59.1408341645621));
#152364=CARTESIAN_POINT('Ctrl Pts',(30.9975809933864,4.66492003209589,59.1313977297925));
#152365=CARTESIAN_POINT('Ctrl Pts',(30.9765080995779,4.74367597221363,59.1214482661628));
#152366=CARTESIAN_POINT('Ctrl Pts',(30.9657812798762,4.78340525731003,59.1163859910534));
#152367=CARTESIAN_POINT('Ctrl Pts',(30.9630586863305,4.79346825522217,59.1151012495784));
#152368=CARTESIAN_POINT('Ctrl Pts',(30.9526717350889,4.83157822333907,59.1102017551008));
#152369=CARTESIAN_POINT('Ctrl Pts',(30.9061209306105,5.00130319864553,59.0882512240363));
#152370=CARTESIAN_POINT('Ctrl Pts',(30.8614554891954,5.15514021531874,59.0672545751894));
#152371=CARTESIAN_POINT('Ctrl Pts',(30.7492445259733,5.5284675154164,59.0146181758072));
#152372=CARTESIAN_POINT('Ctrl Pts',(30.6837752421392,5.72818023448767,58.9840654380761));
#152373=CARTESIAN_POINT('Ctrl Pts',(30.606644414273,5.95664803870136,58.9481511252953));
#152374=CARTESIAN_POINT('Ctrl Pts',(30.5844111552921,6.02094849677282,58.9378160443542));
#152375=CARTESIAN_POINT('Ctrl Pts',(30.5614367333558,6.08670460389163,58.9271457506316));
#152376=CARTESIAN_POINT('Ctrl Pts',(30.5570820158569,6.09912457315758,58.9251238088587));
#152377=CARTESIAN_POINT('Ctrl Pts',(30.5488619467414,6.12250588503938,58.9213080151338));
#152378=CARTESIAN_POINT('Ctrl Pts',(30.5449355619366,6.13363443630184,58.9194859040566));
#152379=CARTESIAN_POINT('Ctrl Pts',(30.5377098658508,6.1540971245753,58.9161331050368));
#152380=CARTESIAN_POINT('Ctrl Pts',(30.5320633787142,6.17005993453924,58.9135137320084));
#152381=CARTESIAN_POINT('Ctrl Pts',(30.4736147764047,6.33454315250574,58.8864116497724));
#152382=CARTESIAN_POINT('Ctrl Pts',(30.3690557537706,6.62958573704077,58.837855810521));
#152383=CARTESIAN_POINT('Ctrl Pts',(30.0125509583764,7.49842179310155,58.674749828271));
#152384=CARTESIAN_POINT('Ctrl Pts',(29.7600841387613,8.07251657893688,58.5597410349833));
#152385=CARTESIAN_POINT('Ctrl Pts',(29.3503334012256,8.85243318681241,58.378441064234));
#152386=CARTESIAN_POINT('Ctrl Pts',(29.3030494993425,8.94091740462205,58.3575776543996));
#152387=CARTESIAN_POINT('Ctrl Pts',(29.2477935313922,9.04242225112039,58.333274656692));
#152388=CARTESIAN_POINT('Ctrl Pts',(29.2416253470245,9.05372777660621,58.3305627752559));
#152389=CARTESIAN_POINT('Ctrl Pts',(29.2292314161529,9.07639289084225,58.3251158408468));
#152390=CARTESIAN_POINT('Ctrl Pts',(29.2252417118537,9.08367104141893,58.3233631745203));
#152391=CARTESIAN_POINT('Ctrl Pts',(29.2108420365903,9.10990865382669,58.3170387280041));
#152392=CARTESIAN_POINT('Ctrl Pts',(29.1819685788639,9.16233624221613,58.3043649315334));
#152393=CARTESIAN_POINT('Ctrl Pts',(29.0752885191553,9.35403928379102,58.2576234899208));
#152394=CARTESIAN_POINT('Ctrl Pts',(28.9758769922251,9.52665917566663,58.2143291862738));
#152395=CARTESIAN_POINT('Ctrl Pts',(28.7328322034821,9.93742152356835,58.109026362923));
#152396=CARTESIAN_POINT('Ctrl Pts',(28.5648839810477,10.2064838036535,58.0369688930087));
#152397=CARTESIAN_POINT('Ctrl Pts',(27.6967660476423,11.5282928587391,57.6689109432536));
#152398=CARTESIAN_POINT('Ctrl Pts',(26.9118841789333,12.5113512549311,57.3502372469519));
#152399=CARTESIAN_POINT('Ctrl Pts',(25.1829115933319,14.3312194690257,56.6913254711783));
#152400=CARTESIAN_POINT('Ctrl Pts',(24.2395124014287,15.1668846914999,56.351198049462));
#152401=CARTESIAN_POINT('Ctrl Pts',(22.7280041048116,16.2961287838868,55.8461256319013));
#152402=CARTESIAN_POINT('Ctrl Pts',(21.9478953609756,16.8298442996705,55.5947874736229));
#152403=CARTESIAN_POINT('Ctrl Pts',(20.9988547315172,17.3962858871967,55.3079261156194));
#152404=CARTESIAN_POINT('Ctrl Pts',(20.5150692586934,17.6651808024177,55.1666215132978));
#152405=CARTESIAN_POINT('Ctrl Pts',(20.2534788527478,17.8053581616721,55.0915637613476));
#152406=CARTESIAN_POINT('Ctrl Pts',(20.1307531149892,17.8697148753435,55.0567211022284));
#152407=CARTESIAN_POINT('Ctrl Pts',(20.060466439718,17.9062297903841,55.0368579370139));
#152408=CARTESIAN_POINT('Ctrl Pts',(20.0445922393146,17.9144536834225,55.032377992028));
#152409=CARTESIAN_POINT('Ctrl Pts',(18.7895387906621,18.5624030433635,54.6787873298313));
#152410=CARTESIAN_POINT('Ctrl Pts',(17.4880542508462,19.0929939467329,54.350792426133));
#152411=CARTESIAN_POINT('Ctrl Pts',(14.8049250018864,19.9130716628939,53.7585639997161));
#152412=CARTESIAN_POINT('Ctrl Pts',(13.4189225674684,20.2021071066721,53.49482150861));
#152413=CARTESIAN_POINT('Ctrl Pts',(10.5989297874419,20.5186536225354,53.0493074876692));
#152414=CARTESIAN_POINT('Ctrl Pts',(9.16879510167067,20.5474535819967,52.8667463358057));
#152415=CARTESIAN_POINT('Ctrl Pts',(7.03429655982645,20.378623757791,52.6625784528267));
#152416=CARTESIAN_POINT('Ctrl Pts',(6.32454994165452,20.2872254257206,52.605939889171));
#152417=CARTESIAN_POINT('Ctrl Pts',(5.26781972066546,20.0977345353649,52.5373095039074));
#152418=CARTESIAN_POINT('Ctrl Pts',(4.91685036642107,20.0258308076223,52.5171513356887));
#152419=CARTESIAN_POINT('Ctrl Pts',(4.39324422595082,19.9049582444335,52.4909091926348));
#152420=CARTESIAN_POINT('Ctrl Pts',(4.13216299115475,19.8412696819295,52.4787875127944));
#152421=CARTESIAN_POINT('Ctrl Pts',(3.78847452803686,19.7505915309332,52.4647163644973));
#152422=CARTESIAN_POINT('Ctrl Pts',(3.61858047887794,19.7035232752188,52.4583728317327));
#152423=CARTESIAN_POINT('Ctrl Pts',(3.53244486979829,19.6790953700934,52.4553091168919));
#152424=CARTESIAN_POINT('Ctrl Pts',(3.52828977296109,19.6779158019158,52.4551616476577));
#152425=CARTESIAN_POINT('Ctrl Pts',(2.26969720044624,19.3204479785115,52.410539354288));
#152426=CARTESIAN_POINT('Ctrl Pts',(1.15098086607544,18.8794025892053,52.4044756295119));
#152427=CARTESIAN_POINT('Ctrl Pts',(-0.823365706586399,17.9315764407793,
52.4301705412463));
#152428=CARTESIAN_POINT('Ctrl Pts',(-1.68085508940634,17.4246104337525,
52.4616915003746));
#152429=CARTESIAN_POINT('Ctrl Pts',(-2.42457349465642,16.925539184609,52.4988700952682));
#152430=CARTESIAN_POINT('',(4.64902170753621,20.2569043834612,52.5918015797662));
#152431=CARTESIAN_POINT('Ctrl Pts',(4.64902170753621,20.2569043834612,52.5918015797661));
#152432=CARTESIAN_POINT('Ctrl Pts',(2.44080379989214,19.6604809726091,52.4080693694926));
#152433=CARTESIAN_POINT('Ctrl Pts',(0.0111762509740697,18.6631588814877,
52.3771048369357));
#152434=CARTESIAN_POINT('Ctrl Pts',(-2.42457387236482,16.9255393804567,
52.4988701141421));
#152435=CARTESIAN_POINT('Ctrl Pts',(4.64902175036909,20.25690439503,52.59180158333));
#152436=CARTESIAN_POINT('Ctrl Pts',(5.53077500234378,20.4910577162601,52.6634099038893));
#152437=CARTESIAN_POINT('Ctrl Pts',(6.38264026146891,20.6568280351203,52.7536679026443));
#152438=CARTESIAN_POINT('Ctrl Pts',(8.00564535770169,20.8773654563953,52.9611269937213));
#152439=CARTESIAN_POINT('Ctrl Pts',(8.77692842067965,20.9322329149705,53.0782432829553));
#152440=CARTESIAN_POINT('Ctrl Pts',(10.951160880708,20.9769467088012,53.4469728543927));
#152441=CARTESIAN_POINT('Ctrl Pts',(12.2123332559162,20.8495653778833,53.7134261489691));
#152442=CARTESIAN_POINT('Ctrl Pts',(13.2725929185091,20.67124111202,53.96044066964));
#152443=CARTESIAN_POINT('Ctrl Pts',(7.76490383693909,-18.74690283777,98.56218991496));
#152444=CARTESIAN_POINT('Ctrl Pts',(7.58087064334909,-18.68099734404,98.11407719773));
#152445=CARTESIAN_POINT('Ctrl Pts',(7.17186061948909,-18.63711019633,97.23171771039));
#152446=CARTESIAN_POINT('Ctrl Pts',(6.40257597231909,-18.86761696116,95.91866414515));
#152447=CARTESIAN_POINT('Ctrl Pts',(5.54113344588909,-19.38926508363,94.74000227609));
#152448=CARTESIAN_POINT('Ctrl Pts',(4.60850716178909,-20.20664112972,93.74354915989));
#152449=CARTESIAN_POINT('Ctrl Pts',(3.67444280643909,-21.26785788722,93.01404174921));
#152450=CARTESIAN_POINT('Ctrl Pts',(2.80889919598909,-22.48420896871,92.59591077148));
#152451=CARTESIAN_POINT('Ctrl Pts',(2.03364908499909,-23.80773656447,92.48047031176));
#152452=CARTESIAN_POINT('Ctrl Pts',(1.61949372405909,-24.67952653565,92.60114010393));
#152453=CARTESIAN_POINT('Ctrl Pts',(1.43267983846909,-25.11816111829,92.70581998851));
#152454=CARTESIAN_POINT('Ctrl Pts',(6.84591093522909,-18.24106815967,99.10973240698));
#152455=CARTESIAN_POINT('Ctrl Pts',(6.70261001385909,-18.18978059281,98.64887935225));
#152456=CARTESIAN_POINT('Ctrl Pts',(6.37155078055909,-18.17079665846,97.74322717855));
#152457=CARTESIAN_POINT('Ctrl Pts',(5.71034935076909,-18.42237686917,96.39856329425));
#152458=CARTESIAN_POINT('Ctrl Pts',(4.93649968105909,-18.94461540664,95.19135919012));
#152459=CARTESIAN_POINT('Ctrl Pts',(4.06467328216909,-19.74072638946,94.16679995292));
#152460=CARTESIAN_POINT('Ctrl Pts',(3.15626401104909,-20.76149483123,93.40873771827));
#152461=CARTESIAN_POINT('Ctrl Pts',(2.27820018257909,-21.92509472165,92.9622122916));
#152462=CARTESIAN_POINT('Ctrl Pts',(1.45346803662909,-23.18955465286,92.81955761915));
#152463=CARTESIAN_POINT('Ctrl Pts',(0.985339306749088,-24.02354685244,92.92544468146));
#152464=CARTESIAN_POINT('Ctrl Pts',(0.766573969559087,-24.4438355265,93.02381020086));
#152465=CARTESIAN_POINT('Ctrl Pts',(5.15603146102909,-17.16231939458,99.73756536437));
#152466=CARTESIAN_POINT('Ctrl Pts',(5.07656232213909,-17.14519507788,99.27362141278));
#152467=CARTESIAN_POINT('Ctrl Pts',(4.86817723096909,-17.18438724036,98.36643775416));
#152468=CARTESIAN_POINT('Ctrl Pts',(4.38100554644909,-17.48578263476,97.02636012813));
#152469=CARTESIAN_POINT('Ctrl Pts',(3.75396200163909,-18.01131189391,95.82123531016));
#152470=CARTESIAN_POINT('Ctrl Pts',(2.99214101344909,-18.76168546006,94.78583662497));
#152471=CARTESIAN_POINT('Ctrl Pts',(2.14179705642909,-19.69395915499,93.9959895059));
#152472=CARTESIAN_POINT('Ctrl Pts',(1.26131915930909,-20.74169706882,93.4954768101));
#152473=CARTESIAN_POINT('Ctrl Pts',(0.372093247579088,-21.87630201657,93.27979108267));
#152474=CARTESIAN_POINT('Ctrl Pts',(-0.177301220500912,-22.62731794107,
93.33173363611));
#152475=CARTESIAN_POINT('Ctrl Pts',(-0.446098143760912,-23.00743325026,
93.40275143284));
#152476=CARTESIAN_POINT('Ctrl Pts',(2.01811505418909,-14.54776816726,99.9277716794));
#152477=CARTESIAN_POINT('Ctrl Pts',(2.01023554995909,-14.59632979974,99.50291917014));
#152478=CARTESIAN_POINT('Ctrl Pts',(1.94159672944909,-14.74161505002,98.68214416067));
#152479=CARTESIAN_POINT('Ctrl Pts',(1.66792258261909,-15.11758854345,97.48221302774));
#152480=CARTESIAN_POINT('Ctrl Pts',(1.24264558750909,-15.62293131579,96.39555993001));
#152481=CARTESIAN_POINT('Ctrl Pts',(0.662401506139089,-16.25798036424,95.43134765319));
#152482=CARTESIAN_POINT('Ctrl Pts',(-0.0485908112209128,-16.99447857602,
94.64062974799));
#152483=CARTESIAN_POINT('Ctrl Pts',(-0.852845516220913,-17.79509455314,
94.05825027106));
#152484=CARTESIAN_POINT('Ctrl Pts',(-1.74211739427091,-18.65432063726,93.68272059274));
#152485=CARTESIAN_POINT('Ctrl Pts',(-2.35020149985091,-19.22776358223,93.58953241735));
#152486=CARTESIAN_POINT('Ctrl Pts',(-2.66433753136591,-19.52121356586,93.5800352882));
#152487=CARTESIAN_POINT('Ctrl Pts',(-0.500978249740913,-11.56191239416,
99.08684515167));
#152488=CARTESIAN_POINT('Ctrl Pts',(-0.502039037980913,-11.64481246331,
98.72685538008));
#152489=CARTESIAN_POINT('Ctrl Pts',(-0.550354078040912,-11.83448920176,
98.03869925544));
#152490=CARTESIAN_POINT('Ctrl Pts',(-0.763358486380913,-12.20569664454,
97.03885362909));
#152491=CARTESIAN_POINT('Ctrl Pts',(-1.09904393458091,-12.63925516577,96.12438509733));
#152492=CARTESIAN_POINT('Ctrl Pts',(-1.56136469190091,-13.13963119611,95.28732914327));
#152493=CARTESIAN_POINT('Ctrl Pts',(-2.13667832435091,-13.69111153729,94.55765981838));
#152494=CARTESIAN_POINT('Ctrl Pts',(-2.80383775034391,-14.27476406571,93.9584167065));
#152495=CARTESIAN_POINT('Ctrl Pts',(-3.56787214556291,-14.89589555266,93.48403838359));
#152496=CARTESIAN_POINT('Ctrl Pts',(-4.11575259146291,-15.31302927099,93.2731503106));
#152497=CARTESIAN_POINT('Ctrl Pts',(-4.40751537919091,-15.52864660289,93.19152480061));
#152498=CARTESIAN_POINT('Ctrl Pts',(-2.40385438927091,-8.27513353230999,
97.91549930542));
#152499=CARTESIAN_POINT('Ctrl Pts',(-2.41705892460091,-8.35576375550799,
97.61350798042));
#152500=CARTESIAN_POINT('Ctrl Pts',(-2.47850833858091,-8.52577604133099,
97.04016580438));
#152501=CARTESIAN_POINT('Ctrl Pts',(-2.67662882390191,-8.82289719190299,
96.2090842562));
#152502=CARTESIAN_POINT('Ctrl Pts',(-2.96472720229591,-9.14598820546499,
95.44224967854));
#152503=CARTESIAN_POINT('Ctrl Pts',(-3.34766214760091,-9.50115635602199,
94.72434974774));
#152504=CARTESIAN_POINT('Ctrl Pts',(-3.81750557776291,-9.88052715685699,
94.07294332057));
#152505=CARTESIAN_POINT('Ctrl Pts',(-4.36228735193491,-10.27515198003,93.5025467691));
#152506=CARTESIAN_POINT('Ctrl Pts',(-4.99278044581591,-10.69277817964,93.00315604594));
#152507=CARTESIAN_POINT('Ctrl Pts',(-5.45419991380291,-10.9745024863,92.73682245074));
#152508=CARTESIAN_POINT('Ctrl Pts',(-5.70378986383891,-11.12121270698,92.61655057154));
#152509=CARTESIAN_POINT('Ctrl Pts',(-3.48946853730791,-5.66270952226699,
97.03465353091));
#152510=CARTESIAN_POINT('Ctrl Pts',(-3.51536059911091,-5.72718798709899,
96.77001431597));
#152511=CARTESIAN_POINT('Ctrl Pts',(-3.59361606472291,-5.85816473999899,
96.26934622152));
#152512=CARTESIAN_POINT('Ctrl Pts',(-3.79317244891691,-6.07452079650099,
95.5436014807));
#152513=CARTESIAN_POINT('Ctrl Pts',(-4.06044298827191,-6.30075292131999,
94.86955024439));
#152514=CARTESIAN_POINT('Ctrl Pts',(-4.40098234935791,-6.54248518883199,
94.22941353888));
#152515=CARTESIAN_POINT('Ctrl Pts',(-4.80945351933091,-6.79576625556499,
93.63469864769));
#152516=CARTESIAN_POINT('Ctrl Pts',(-5.27818789952991,-7.05626892909499,
93.09537001614));
#152517=CARTESIAN_POINT('Ctrl Pts',(-5.81982158017491,-7.33076614359399,
92.59899144013));
#152518=CARTESIAN_POINT('Ctrl Pts',(-6.21841979583891,-7.51629614060999,
92.313172261));
#152519=CARTESIAN_POINT('Ctrl Pts',(-6.43544364235691,-7.61333585955899,
92.17693035492));
#152520=CARTESIAN_POINT('Ctrl Pts',(-4.08125864136291,-3.34963677957899,
96.4640360546));
#152521=CARTESIAN_POINT('Ctrl Pts',(-4.11495573449391,-3.38996690520999,
96.22103118722));
#152522=CARTESIAN_POINT('Ctrl Pts',(-4.20360591321791,-3.47078065240599,
95.76198955656));
#152523=CARTESIAN_POINT('Ctrl Pts',(-4.40510898824891,-3.60154101220899,
95.09616413785));
#152524=CARTESIAN_POINT('Ctrl Pts',(-4.66186458946291,-3.73629411992999,
94.4753371721));
#152525=CARTESIAN_POINT('Ctrl Pts',(-4.97991493535491,-3.87877956301499,
93.88117499892));
#152526=CARTESIAN_POINT('Ctrl Pts',(-5.35511778786991,-4.02705282314199,
93.32243209734));
#152527=CARTESIAN_POINT('Ctrl Pts',(-5.78169641327591,-4.17900780868299,
92.80685149873));
#152528=CARTESIAN_POINT('Ctrl Pts',(-6.27263192495991,-4.33902725749599,
92.3209175153));
#152529=CARTESIAN_POINT('Ctrl Pts',(-6.63392144579591,-4.44742362454599,
92.03132075072));
#152530=CARTESIAN_POINT('Ctrl Pts',(-6.83104608699891,-4.50427380216299,
91.89005190681));
#152531=CARTESIAN_POINT('Ctrl Pts',(-4.32563828462991,-1.45531027820599,
96.20932054197));
#152532=CARTESIAN_POINT('Ctrl Pts',(-4.36303811445691,-1.47327684969999,
95.97550868925));
#152533=CARTESIAN_POINT('Ctrl Pts',(-4.45674571338191,-1.50907333094899,
95.53411677963));
#152534=CARTESIAN_POINT('Ctrl Pts',(-4.65983797573291,-1.56647815097599,
94.89371248405));
#152535=CARTESIAN_POINT('Ctrl Pts',(-4.91271757859291,-1.62524988581899,
94.2955919798));
#152536=CARTESIAN_POINT('Ctrl Pts',(-5.22165458228691,-1.68708854078499,
93.72129734803));
#152537=CARTESIAN_POINT('Ctrl Pts',(-5.58297014235291,-1.75121737845499,
93.17850775416));
#152538=CARTESIAN_POINT('Ctrl Pts',(-5.99162063487591,-1.81680109518699,
92.67408166894));
#152539=CARTESIAN_POINT('Ctrl Pts',(-6.46063249209491,-1.88580703178699,
92.19412061021));
#152540=CARTESIAN_POINT('Ctrl Pts',(-6.80547994037391,-1.93256605067699,
91.90424269924));
#152541=CARTESIAN_POINT('Ctrl Pts',(-6.99372679758291,-1.95710965956499,
91.76159800597));
#152542=CARTESIAN_POINT('Ctrl Pts',(-4.38971615456091,-0.00834582542081779,
96.13767933788));
#152543=CARTESIAN_POINT('Ctrl Pts',(-4.42824857521291,-0.00845141752385579,
95.90627280969));
#152544=CARTESIAN_POINT('Ctrl Pts',(-4.52354494822991,-0.00866085690577179,
95.46951686637));
#152545=CARTESIAN_POINT('Ctrl Pts',(-4.72732393892391,-0.00899423329457679,
94.83585426025));
#152546=CARTESIAN_POINT('Ctrl Pts',(-4.97934129871291,-0.00933351887315879,
94.2438310054));
#152547=CARTESIAN_POINT('Ctrl Pts',(-5.28593578059191,-0.00968867480289279,
93.67497113172));
#152548=CARTESIAN_POINT('Ctrl Pts',(-5.64354565335191,-0.0100553448513358,
93.13667952072));
#152549=CARTESIAN_POINT('Ctrl Pts',(-6.04731363736391,-0.0104288918987758,
92.6355846836));
#152550=CARTESIAN_POINT('Ctrl Pts',(-6.51025910053291,-0.0108206286907258,
92.15770391467));
#152551=CARTESIAN_POINT('Ctrl Pts',(-6.85048297649391,-0.0110852664431558,
91.86815847988));
#152552=CARTESIAN_POINT('Ctrl Pts',(-7.03620933377191,-0.0112239861470658,
91.72537995813));
#152553=CARTESIAN_POINT('Ctrl Pts',(-4.32713170324291,1.43866748068201,
96.20779519047));
#152554=CARTESIAN_POINT('Ctrl Pts',(-4.36455171328791,1.45643608224001,
95.97404039411));
#152555=CARTESIAN_POINT('Ctrl Pts',(-4.45828600907391,1.49183529502801,
95.53275739702));
#152556=CARTESIAN_POINT('Ctrl Pts',(-4.66138340529791,1.54859559587301,
94.89250848788));
#152557=CARTESIAN_POINT('Ctrl Pts',(-4.91423671646991,1.60670145769501,
94.29452563453));
#152558=CARTESIAN_POINT('Ctrl Pts',(-5.22311740864891,1.66783413833301,
93.72035042235));
#152559=CARTESIAN_POINT('Ctrl Pts',(-5.58434947881591,1.73122617606901,
93.17765569491));
#152560=CARTESIAN_POINT('Ctrl Pts',(-5.99289358065391,1.79605238890401,
92.67329470011));
#152561=CARTESIAN_POINT('Ctrl Pts',(-6.46177625288291,1.86425784562201,
92.19336654142));
#152562=CARTESIAN_POINT('Ctrl Pts',(-6.80652723416991,1.91047243766801,
91.90348413557));
#152563=CARTESIAN_POINT('Ctrl Pts',(-6.99472208375591,1.93472985067201,
91.76082943399));
#152564=CARTESIAN_POINT('Ctrl Pts',(-4.08466637979291,3.33351684098901,
96.46069423489));
#152565=CARTESIAN_POINT('Ctrl Pts',(-4.11840899567191,3.37367820166701,
96.2178178536));
#152566=CARTESIAN_POINT('Ctrl Pts',(-4.20712022633291,3.45414316234301,
95.75902244189));
#152567=CARTESIAN_POINT('Ctrl Pts',(-4.40863651739491,3.58431165906801,
95.09354947048));
#152568=CARTESIAN_POINT('Ctrl Pts',(-4.66533330758691,3.71843350521601,
94.47303426014));
#152569=CARTESIAN_POINT('Ctrl Pts',(-4.98325513816091,3.86023366340401,
93.87914038642));
#152570=CARTESIAN_POINT('Ctrl Pts',(-5.35826621411991,4.00777956126601,
93.32060660702));
#152571=CARTESIAN_POINT('Ctrl Pts',(-5.78460058356491,4.15897831435901,
92.80516330061));
#152572=CARTESIAN_POINT('Ctrl Pts',(-6.27524140749091,4.31819349568901,
92.31928870611));
#152573=CARTESIAN_POINT('Ctrl Pts',(-6.63631352672891,4.42604158474401,
92.02966887888));
#152574=CARTESIAN_POINT('Ctrl Pts',(-6.83332202411891,4.48260385956001,
91.8883702024));
#152575=CARTESIAN_POINT('Ctrl Pts',(-3.49366057865791,5.65170562487801,
97.03121358409));
#152576=CARTESIAN_POINT('Ctrl Pts',(-3.51959060155191,5.71610818987201,
96.76672008513));
#152577=CARTESIAN_POINT('Ctrl Pts',(-3.59788812876691,5.84690863477801,
96.26633081383));
#152578=CARTESIAN_POINT('Ctrl Pts',(-3.79741910388591,6.06291747560601,
95.54098130515));
#152579=CARTESIAN_POINT('Ctrl Pts',(-4.06458925483091,6.28874343571801,
94.86727462891));
#152580=CARTESIAN_POINT('Ctrl Pts',(-4.40496019109691,6.53000524676001,
94.22742782932));
#152581=CARTESIAN_POINT('Ctrl Pts',(-4.81320613037991,6.78276433667501,
93.63292996755));
#152582=CARTESIAN_POINT('Ctrl Pts',(-5.28167093282291,7.04270951258801,
93.09373074917));
#152583=CARTESIAN_POINT('Ctrl Pts',(-5.82299093728491,7.31660676789101,
92.59738480008));
#152584=CARTESIAN_POINT('Ctrl Pts',(-6.22136312270091,7.50172825322501,
92.31150938393));
#152585=CARTESIAN_POINT('Ctrl Pts',(-6.43826758672891,7.59855515253601,
92.17521557127));
#152586=CARTESIAN_POINT('Ctrl Pts',(-2.40566532396091,8.27093850373701,
97.913483192));
#152587=CARTESIAN_POINT('Ctrl Pts',(-2.41893979818091,8.35151331732401,
97.61155021493));
#152588=CARTESIAN_POINT('Ctrl Pts',(-2.48051296884091,8.52141215550501,
97.03833798277));
#152589=CARTESIAN_POINT('Ctrl Pts',(-2.67876057350391,8.81833919218701,
96.20748045575));
#152590=CARTESIAN_POINT('Ctrl Pts',(-2.96690463677591,9.14122590023601,
95.44086436563));
#152591=CARTESIAN_POINT('Ctrl Pts',(-3.34979049398491,9.49618416298601,
94.72315811491));
#152592=CARTESIAN_POINT('Ctrl Pts',(-3.81948858118091,9.87535335871601,
94.07189534027));
#152593=CARTESIAN_POINT('Ctrl Pts',(-4.36404809004391,10.26979652667,93.50157597282));
#152594=CARTESIAN_POINT('Ctrl Pts',(-4.99426574517891,10.68726364368,93.00219312889));
#152595=CARTESIAN_POINT('Ctrl Pts',(-5.45549518861091,10.96890692798,92.73582111251));
#152596=CARTESIAN_POINT('Ctrl Pts',(-5.70499060313391,11.11558274903,92.61552178529));
#152597=CARTESIAN_POINT('Ctrl Pts',(-0.986861114710913,10.72477427286,98.78960368345));
#152598=CARTESIAN_POINT('Ctrl Pts',(-0.990891422970911,10.80721848264,98.4444406356));
#152599=CARTESIAN_POINT('Ctrl Pts',(-1.04229030476091,10.99209348129,97.78557907002));
#152600=CARTESIAN_POINT('Ctrl Pts',(-1.25112303813091,11.34467819767,96.82867121273));
#152601=CARTESIAN_POINT('Ctrl Pts',(-1.57441029605091,11.75027336749,95.95168997202));
#152602=CARTESIAN_POINT('Ctrl Pts',(-2.01639196031091,12.21374866258,95.14484570844));
#152603=CARTESIAN_POINT('Ctrl Pts',(-2.56490724892091,12.72136740625,94.4349931982));
#152604=CARTESIAN_POINT('Ctrl Pts',(-3.20111188233091,13.2567343196,93.84302552526));
#152605=CARTESIAN_POINT('Ctrl Pts',(-3.93142853957191,13.82577205484,93.3622420885));
#152606=CARTESIAN_POINT('Ctrl Pts',(-4.45747219799491,14.20816411588,93.13720689211));
#152607=CARTESIAN_POINT('Ctrl Pts',(-4.73857333104691,14.40607930072,93.04570973776));
#152608=CARTESIAN_POINT('Ctrl Pts',(0.752803273019088,13.04777395438,99.50267990176));
#152609=CARTESIAN_POINT('Ctrl Pts',(0.748001440679089,13.11333574627,99.11026889267));
#152610=CARTESIAN_POINT('Ctrl Pts',(0.688801803489089,13.28050113826,98.35606433508));
#152611=CARTESIAN_POINT('Ctrl Pts',(0.444478148969087,13.65351217911,97.25704934952));
#152612=CARTESIAN_POINT('Ctrl Pts',(0.0634478276490876,14.12231339896,96.25750483054));
#152613=CARTESIAN_POINT('Ctrl Pts',(-0.457745008220911,14.68938538907,95.35776322763));
#152614=CARTESIAN_POINT('Ctrl Pts',(-1.10012730427091,15.33287565161,94.59807905016));
#152615=CARTESIAN_POINT('Ctrl Pts',(-1.83459092072091,16.0247678547,94.00725484854));
#152616=CARTESIAN_POINT('Ctrl Pts',(-2.65985793962991,16.76505394477,93.58178296922));
#152617=CARTESIAN_POINT('Ctrl Pts',(-3.23713241969691,17.2607200173,93.42919782937));
#152618=CARTESIAN_POINT('Ctrl Pts',(-3.53983067401091,17.51554255463,93.3833719997));
#152619=CARTESIAN_POINT('Ctrl Pts',(2.76127419102909,15.1656997103,99.8818256134));
#152620=CARTESIAN_POINT('Ctrl Pts',(2.73645150366909,15.19875100305,99.44781306681));
#152621=CARTESIAN_POINT('Ctrl Pts',(2.63477302079909,15.31897349528,98.60670232739));
#152622=CARTESIAN_POINT('Ctrl Pts',(2.31065481307909,15.67735269961,97.37363418217));
#152623=CARTESIAN_POINT('Ctrl Pts',(1.83767642022909,16.1875285794,96.25890102547));
#152624=CARTESIAN_POINT('Ctrl Pts',(1.21443386181909,16.84991538689,95.27779332052));
#152625=CARTESIAN_POINT('Ctrl Pts',(0.470358250379088,17.63275208932,94.48728208583));
#152626=CARTESIAN_POINT('Ctrl Pts',(-0.352070020950912,18.49178896765,93.92434986784));
#152627=CARTESIAN_POINT('Ctrl Pts',(-1.24142138326091,19.41602173204,93.58677668322));
#152628=CARTESIAN_POINT('Ctrl Pts',(-1.83558875622091,20.03129423533,93.5280107824));
#152629=CARTESIAN_POINT('Ctrl Pts',(-2.13894907756091,20.34512812081,93.53758527922));
#152630=CARTESIAN_POINT('Ctrl Pts',(5.15251803294909,17.16074206836,99.7395436905));
#152631=CARTESIAN_POINT('Ctrl Pts',(5.07319338924909,17.14367080395,99.27554213802));
#152632=CARTESIAN_POINT('Ctrl Pts',(4.86507307407909,17.18296054942,98.36827711269));
#152633=CARTESIAN_POINT('Ctrl Pts',(4.37825821066909,17.48443955237,97.02814196662));
#152634=CARTESIAN_POINT('Ctrl Pts',(3.75151422181909,18.00996471582,95.82298786203));
#152635=CARTESIAN_POINT('Ctrl Pts',(2.98992757208909,18.76024383142,94.78754665466));
#152636=CARTESIAN_POINT('Ctrl Pts',(2.13972143248909,19.69235387311,93.99761263896));
#152637=CARTESIAN_POINT('Ctrl Pts',(1.25925323305909,20.73989979774,93.49696073771));
#152638=CARTESIAN_POINT('Ctrl Pts',(0.369883529649088,21.8743228404,93.28109681334));
#152639=CARTESIAN_POINT('Ctrl Pts',(-0.179717950130911,22.62525541673,93.33292570464));
#152640=CARTESIAN_POINT('Ctrl Pts',(-0.448648786890913,23.00534209725,93.40389634347));
#152641=CARTESIAN_POINT('Ctrl Pts',(6.85073007253909,18.24407708458,99.10786428624));
#152642=CARTESIAN_POINT('Ctrl Pts',(6.70724910919909,18.19269701524,98.64702681991));
#152643=CARTESIAN_POINT('Ctrl Pts',(6.37584548782909,18.17355521153,97.74138873472));
#152644=CARTESIAN_POINT('Ctrl Pts',(5.71415695023908,18.42500317992,96.39671839293));
#152645=CARTESIAN_POINT('Ctrl Pts',(4.93989507319909,18.94723983301,95.18950999885));
#152646=CARTESIAN_POINT('Ctrl Pts',(4.06775656452909,19.7434855041,94.16498151748));
#152647=CARTESIAN_POINT('Ctrl Pts',(3.15917820969909,20.76450555988,93.40701054919));
#152648=CARTESIAN_POINT('Ctrl Pts',(2.28111507590909,21.92842864054,92.96064173443));
#152649=CARTESIAN_POINT('Ctrl Pts',(1.45656181868909,23.19324375474,92.81819939069));
#152650=CARTESIAN_POINT('Ctrl Pts',(0.988665265629088,24.0274567351,92.92424183273));
#152651=CARTESIAN_POINT('Ctrl Pts',(0.770044302759088,24.44785020645,93.02268489469));
#152652=CARTESIAN_POINT('Ctrl Pts',(7.76977665654909,18.74956759114,98.55922121492));
#152653=CARTESIAN_POINT('Ctrl Pts',(7.58552417775909,18.68358470833,98.11117902881));
#152654=CARTESIAN_POINT('Ctrl Pts',(7.17609427717909,18.63956574254,97.22895015673));
#152655=CARTESIAN_POINT('Ctrl Pts',(6.40622811537909,18.86995998959,95.91607715674));
#152656=CARTESIAN_POINT('Ctrl Pts',(5.54431599616909,19.39160284285,94.73757900216));
#152657=CARTESIAN_POINT('Ctrl Pts',(4.61136636581909,20.20908841369,93.7412845361));
#152658=CARTESIAN_POINT('Ctrl Pts',(3.67716922131909,21.27051618285,93.01193319476));
#152659=CARTESIAN_POINT('Ctrl Pts',(2.81169810886909,22.48714439168,92.59395157678));
#152660=CARTESIAN_POINT('Ctrl Pts',(2.03671749476909,23.81098447627,92.47864881967));
#152661=CARTESIAN_POINT('Ctrl Pts',(1.62285219573909,24.68297630121,92.59939017677));
#152662=CARTESIAN_POINT('Ctrl Pts',(1.43620923990909,25.12170949067,92.70409987748));
#152663=CARTESIAN_POINT('Ctrl Pts',(7.33390977334909,18.51896019671,98.61558102776));
#152664=CARTESIAN_POINT('Ctrl Pts',(7.17868839516909,18.47477382474,98.21117617597));
#152665=CARTESIAN_POINT('Ctrl Pts',(6.81702728821909,18.45460915649,97.37438079512));
#152666=CARTESIAN_POINT('Ctrl Pts',(6.12091536944909,18.68399519172,96.10537895283));
#152667=CARTESIAN_POINT('Ctrl Pts',(5.29447661592909,19.2059342101,94.91674272034));
#152668=CARTESIAN_POINT('Ctrl Pts',(4.38638383960909,20.01451204523,93.91009879714));
#152669=CARTESIAN_POINT('Ctrl Pts',(3.46301295419909,21.05896146255,93.16964338637));
#152670=CARTESIAN_POINT('Ctrl Pts',(2.59301206463909,22.25343591018,92.73998457345));
#152671=CARTESIAN_POINT('Ctrl Pts',(1.83106111871909,23.49927992091,92.61808758665));
#152672=CARTESIAN_POINT('Ctrl Pts',(1.41587669048909,24.30543668035,92.71382195817));
#152673=CARTESIAN_POINT('Ctrl Pts',(1.23275780153909,24.69194692623,92.79547180931));
#152674=CARTESIAN_POINT('Ctrl Pts',(7.24327301076909,18.44841292379,98.89152713403));
#152675=CARTESIAN_POINT('Ctrl Pts',(7.07686380614909,18.38614815484,98.4293351801));
#152676=CARTESIAN_POINT('Ctrl Pts',(6.70210515371909,18.35059385064,97.52702995238));
#152677=CARTESIAN_POINT('Ctrl Pts',(5.97702939368908,18.59059437363,96.19006143074));
#152678=CARTESIAN_POINT('Ctrl Pts',(5.15369661933909,19.10986144225,94.99856944475));
#152679=CARTESIAN_POINT('Ctrl Pts',(4.24496997515909,19.91418147426,93.9895692329));
#152680=CARTESIAN_POINT('Ctrl Pts',(3.31709496123909,20.95311160024,93.2474603871));
#152681=CARTESIAN_POINT('Ctrl Pts',(2.43917773245909,22.14131525181,92.81697663142));
#152682=CARTESIAN_POINT('Ctrl Pts',(1.62775941032909,23.44334321557,92.68893680414));
#152683=CARTESIAN_POINT('Ctrl Pts',(1.18008954667909,24.30420194899,92.80696251476));
#152684=CARTESIAN_POINT('Ctrl Pts',(0.973133455769088,24.74102620381,92.9129604542));
#152685=CARTESIAN_POINT('Ctrl Pts',(8.00953233305909,18.89726647515,98.48609646253));
#152686=CARTESIAN_POINT('Ctrl Pts',(7.82726256922909,18.83110259375,98.02900834109));
#152687=CARTESIAN_POINT('Ctrl Pts',(7.42476847736909,18.79032238758,97.13584503445));
#152688=CARTESIAN_POINT('Ctrl Pts',(6.66957047162909,19.03118815527,95.81024525772));
#152689=CARTESIAN_POINT('Ctrl Pts',(5.83099218217909,19.56043801888,94.6272581298));
#152690=CARTESIAN_POINT('Ctrl Pts',(4.92353481037909,20.38417296558,93.62422832877));
#152691=CARTESIAN_POINT('Ctrl Pts',(4.01444774807909,21.45048632645,92.88558108514));
#152692=CARTESIAN_POINT('Ctrl Pts',(3.17125581513909,22.67115923528,92.45618350511));
#152693=CARTESIAN_POINT('Ctrl Pts',(2.40912940075909,24.00907021716,92.32694912102));
#152694=CARTESIAN_POINT('Ctrl Pts',(2.00081881447909,24.89344637271,92.44258765142));
#152695=CARTESIAN_POINT('Ctrl Pts',(1.81538572080909,25.34207419056,92.54692663014));
#152696=CARTESIAN_POINT('Ctrl Pts',(9.48574240951909,19.63597267403,97.59516207783));
#152697=CARTESIAN_POINT('Ctrl Pts',(9.27104903689909,19.56585320366,97.15168124725));
#152698=CARTESIAN_POINT('Ctrl Pts',(8.81196101849909,19.5209615512,96.28385992272));
#152699=CARTESIAN_POINT('Ctrl Pts',(7.99594013996909,19.76837911278,94.99193752219));
#152700=CARTESIAN_POINT('Ctrl Pts',(7.12744499441909,20.31683308929,93.8352360129));
#152701=CARTESIAN_POINT('Ctrl Pts',(6.22395983921909,21.17277039945,92.85037342522));
#152702=CARTESIAN_POINT('Ctrl Pts',(5.35404037564909,22.28208598191,92.12036988641));
#152703=CARTESIAN_POINT('Ctrl Pts',(4.58119122970909,23.55258633343,91.68997564786));
#152704=CARTESIAN_POINT('Ctrl Pts',(3.91718676034909,24.94517181348,91.55071182088));
#152705=CARTESIAN_POINT('Ctrl Pts',(3.58611082929909,25.86546670108,91.65436237848));
#152706=CARTESIAN_POINT('Ctrl Pts',(3.44265110932909,26.33221020789,91.75135962898));
#152707=CARTESIAN_POINT('Ctrl Pts',(11.6479277035891,20.40116728954,95.92876188531));
#152708=CARTESIAN_POINT('Ctrl Pts',(11.3848777392391,20.33605104043,95.51483955623));
#152709=CARTESIAN_POINT('Ctrl Pts',(10.8425601258091,20.30358730125,94.70403709746));
#152710=CARTESIAN_POINT('Ctrl Pts',(9.94089745124909,20.5768235546,93.49247187146));
#152711=CARTESIAN_POINT('Ctrl Pts',(9.03464754236909,21.15521919782,92.4011837042));
#152712=CARTESIAN_POINT('Ctrl Pts',(8.14400714704909,22.04488243193,91.46220571441));
#152713=CARTESIAN_POINT('Ctrl Pts',(7.33708442288909,23.19040987993,90.75253698504));
#152714=CARTESIAN_POINT('Ctrl Pts',(6.66960293537909,24.49872891802,90.3154847248));
#152715=CARTESIAN_POINT('Ctrl Pts',(6.14760493758909,25.93194257256,90.14439432218));
#152716=CARTESIAN_POINT('Ctrl Pts',(5.92586915515909,26.87990332949,90.21309060207));
#152717=CARTESIAN_POINT('Ctrl Pts',(5.84143517901909,27.36114151081,90.28943327589));
#152718=CARTESIAN_POINT('Ctrl Pts',(13.6809074185791,20.85170333419,93.96716093539));
#152719=CARTESIAN_POINT('Ctrl Pts',(13.3765394460391,20.80319375581,93.5898761014));
#152720=CARTESIAN_POINT('Ctrl Pts',(12.7651707336891,20.80285913764,92.85077521182));
#152721=CARTESIAN_POINT('Ctrl Pts',(11.7984701037891,21.11929473493,91.74278239443));
#152722=CARTESIAN_POINT('Ctrl Pts',(10.8704808523091,21.7300990431,90.73757408298));
#152723=CARTESIAN_POINT('Ctrl Pts',(10.0013578369191,22.64039295908,89.86020117914));
#152724=CARTESIAN_POINT('Ctrl Pts',(9.25609538950909,23.79538319067,89.17868977515));
#152725=CARTESIAN_POINT('Ctrl Pts',(8.68218874229909,25.10590136429,88.73363476746));
#152726=CARTESIAN_POINT('Ctrl Pts',(8.28079699504909,26.53915697395,88.52049654022));
#152727=CARTESIAN_POINT('Ctrl Pts',(8.14971560437909,27.48860192212,88.5425653416));
#152728=CARTESIAN_POINT('Ctrl Pts',(8.11401571270909,27.97154561276,88.59137325496));
#152729=CARTESIAN_POINT('Ctrl Pts',(15.5534522998791,21.03171586279,91.73576692756));
#152730=CARTESIAN_POINT('Ctrl Pts',(15.2170648098991,21.00785881936,91.39930513927));
#152731=CARTESIAN_POINT('Ctrl Pts',(14.5548673242691,21.0527148989,90.74052347661));
#152732=CARTESIAN_POINT('Ctrl Pts',(13.5478771793591,21.4221254335,89.74993758817));
#152733=CARTESIAN_POINT('Ctrl Pts',(12.6158039357191,22.06417039289,88.84384557423));
#152734=CARTESIAN_POINT('Ctrl Pts',(11.7760903471591,22.98303944533,88.03949202247));
#152735=CARTESIAN_POINT('Ctrl Pts',(11.0884865829691,24.12626750567,87.39443634879));
#152736=CARTESIAN_POINT('Ctrl Pts',(10.5926947637791,25.41198318725,86.94544353959));
#152737=CARTESIAN_POINT('Ctrl Pts',(10.2864742437991,26.81503393584,86.68964252342));
#152738=CARTESIAN_POINT('Ctrl Pts',(10.2248975625791,27.74659100247,86.66137917484));
#152739=CARTESIAN_POINT('Ctrl Pts',(10.2264729148191,28.22180509888,86.67998303916));
#152740=CARTESIAN_POINT('Ctrl Pts',(17.2430554107691,20.98202291482,89.2412331004));
#152741=CARTESIAN_POINT('Ctrl Pts',(16.8870711991091,20.98811724776,88.94690397629));
#152742=CARTESIAN_POINT('Ctrl Pts',(16.1974641026791,21.08604958705,88.3712592249));
#152743=CARTESIAN_POINT('Ctrl Pts',(15.1798276002791,21.51243494163,87.50343557567));
#152744=CARTESIAN_POINT('Ctrl Pts',(14.2633095441191,22.18214566721,86.70288959624));
#152745=CARTESIAN_POINT('Ctrl Pts',(13.4604932260391,23.09902889153,85.97946359338));
#152746=CARTESIAN_POINT('Ctrl Pts',(12.8243493470991,24.21432352264,85.37995749348));
#152747=CARTESIAN_POINT('Ctrl Pts',(12.3877610938491,25.45548507477,84.93639608553));
#152748=CARTESIAN_POINT('Ctrl Pts',(12.1466467109391,26.80621472776,84.64669984466));
#152749=CARTESIAN_POINT('Ctrl Pts',(12.1296311867691,27.7054105439,84.57240108835));
#152750=CARTESIAN_POINT('Ctrl Pts',(12.1548476689691,28.16572967293,84.56246164962));
#152751=CARTESIAN_POINT('Ctrl Pts',(19.2495989492791,20.66912552818,85.57069919532));
#152752=CARTESIAN_POINT('Ctrl Pts',(18.8813413248491,20.71804850918,85.33379157953));
#152753=CARTESIAN_POINT('Ctrl Pts',(18.1807999501791,20.88969632127,84.87114381612));
#152754=CARTESIAN_POINT('Ctrl Pts',(17.1800032533291,21.38945414672,84.17048672317));
#152755=CARTESIAN_POINT('Ctrl Pts',(16.3037323185991,22.08827360986,83.51550270559));
#152756=CARTESIAN_POINT('Ctrl Pts',(15.5566288286191,22.99073213886,82.907709313505));
#152757=CARTESIAN_POINT('Ctrl Pts',(14.9817758260491,24.05427124838,82.380258430425));
#152758=CARTESIAN_POINT('Ctrl Pts',(14.6042814360791,25.21977981858,81.958213960619));
#152759=CARTESIAN_POINT('Ctrl Pts',(14.4190122273291,26.48281801567,81.63942835036));
#152760=CARTESIAN_POINT('Ctrl Pts',(14.4356493819991,27.32680522234,81.513735365478));
#152761=CARTESIAN_POINT('Ctrl Pts',(14.4781882928991,27.76114514435,81.470312737204));
#152762=CARTESIAN_POINT('Ctrl Pts',(20.3925977909591,20.2277535595,82.563826718236));
#152763=CARTESIAN_POINT('Ctrl Pts',(20.0304340562991,20.30626477584,82.366918248488));
#152764=CARTESIAN_POINT('Ctrl Pts',(19.3485382185991,20.52649526466,81.982708898295));
#152765=CARTESIAN_POINT('Ctrl Pts',(18.3897565831791,21.06863508853,81.398921431952));
#152766=CARTESIAN_POINT('Ctrl Pts',(17.5597638046891,21.77721885701,80.848439464904));
#152767=CARTESIAN_POINT('Ctrl Pts',(16.8572640880491,22.65865690252,80.329157482003));
#152768=CARTESIAN_POINT('Ctrl Pts',(16.3182918298191,23.67557410625,79.866046158033));
#152769=CARTESIAN_POINT('Ctrl Pts',(15.9638049917991,24.77815737146,79.47897454881));
#152770=CARTESIAN_POINT('Ctrl Pts',(15.7887413289391,25.96931466839,79.164862427794));
#152771=CARTESIAN_POINT('Ctrl Pts',(15.8042210389591,26.76737479866,79.020929073105));
#152772=CARTESIAN_POINT('Ctrl Pts',(15.8449385154191,27.17970245025,78.962990978534));
#152773=CARTESIAN_POINT('Ctrl Pts',(21.0097926924391,19.89563600971,80.40741922018));
#152774=CARTESIAN_POINT('Ctrl Pts',(20.6550889131691,19.99123032158,80.236762155004));
#152775=CARTESIAN_POINT('Ctrl Pts',(19.9909956425891,20.23869347959,79.903761107118));
#152776=CARTESIAN_POINT('Ctrl Pts',(19.0648929430391,20.80252378355,79.396298271413));
#152777=CARTESIAN_POINT('Ctrl Pts',(18.2674404295791,21.51331951319,78.914958065391));
#152778=CARTESIAN_POINT('Ctrl Pts',(17.5940818891591,22.37892089328,78.456246002549));
#152779=CARTESIAN_POINT('Ctrl Pts',(17.0767465562291,23.3651962814,78.040551621815));
#152780=CARTESIAN_POINT('Ctrl Pts',(16.7340571199191,24.42771547795,77.684597081619));
#152781=CARTESIAN_POINT('Ctrl Pts',(16.5609096844291,25.5733672766,77.384841020182));
#152782=CARTESIAN_POINT('Ctrl Pts',(16.5713804283391,26.34212759319,77.237912445421));
#152783=CARTESIAN_POINT('Ctrl Pts',(16.6083416058691,26.74028365911,77.175315062579));
#152784=CARTESIAN_POINT('Ctrl Pts',(20.8003130807923,19.9701890936878,80.5583314860603));
#152785=CARTESIAN_POINT('Ctrl Pts',(20.6335820361414,20.0189518422149,80.4760789509608));
#152786=CARTESIAN_POINT('Ctrl Pts',(20.4669496987559,20.0760850758162,80.3922277537374));
#152787=CARTESIAN_POINT('Ctrl Pts',(20.3014025923107,20.1417112308046,80.3071839810886));
#152788=CARTESIAN_POINT('Ctrl Pts',(20.1619570128364,20.1969902230355,80.2355489135098));
#152789=CARTESIAN_POINT('Ctrl Pts',(20.0232809114241,20.2582959630628,80.1630672985196));
#152790=CARTESIAN_POINT('Ctrl Pts',(19.8859672107522,20.3257298729312,80.089977743185));
#152791=CARTESIAN_POINT('Ctrl Pts',(19.7194382428212,20.4075112200145,80.0013374388537));
#152792=CARTESIAN_POINT('Ctrl Pts',(19.554896435378,20.4983220718029,79.9117925166094));
#152793=CARTESIAN_POINT('Ctrl Pts',(19.3936514485524,20.5982275367535,79.8219011751989));
#152794=CARTESIAN_POINT('Ctrl Pts',(19.2629129348508,20.6792315558888,79.7490166744028));
#152795=CARTESIAN_POINT('Ctrl Pts',(19.1343420084579,20.7662135553124,79.675904710384));
#152796=CARTESIAN_POINT('Ctrl Pts',(19.0086290342816,20.8591842185031,79.6028641638261));
#152797=CARTESIAN_POINT('Ctrl Pts',(19.0081406208618,20.8595454232224,79.6025803905453));
#152798=CARTESIAN_POINT('Ctrl Pts',(19.0076522508267,20.8599067181176,79.602296618492));
#152799=CARTESIAN_POINT('Ctrl Pts',(19.0071639242108,20.8602681031926,79.6020128476805));
#152800=CARTESIAN_POINT('Ctrl Pts',(18.8391759142115,20.984587273217,79.5043935650917));
#152801=CARTESIAN_POINT('Ctrl Pts',(18.6763247663055,21.1195741449237,79.4069214661285));
#152802=CARTESIAN_POINT('Ctrl Pts',(18.5198692521112,21.2642924660863,79.310329056666));
#152803=CARTESIAN_POINT('Ctrl Pts',(18.415340634275,21.3609794135845,79.2457952426512));
#152804=CARTESIAN_POINT('Ctrl Pts',(18.3136670380584,21.4620112568094,79.1816539740263));
#152805=CARTESIAN_POINT('Ctrl Pts',(18.2152299323709,21.567120184169,79.1181241093975));
#152806=CARTESIAN_POINT('Ctrl Pts',(18.0246947079353,21.7705694112136,78.9951554693622));
#152807=CARTESIAN_POINT('Ctrl Pts',(17.8462319408475,21.9893610467865,78.8744409174966));
#152808=CARTESIAN_POINT('Ctrl Pts',(17.6828842429067,22.2213279990028,78.7577319097057));
#152809=CARTESIAN_POINT('Ctrl Pts',(17.635159449823,22.2891010679615,78.7236333988724));
#152810=CARTESIAN_POINT('Ctrl Pts',(17.5887247601207,22.3579984909406,78.6898768065634));
#152811=CARTESIAN_POINT('Ctrl Pts',(17.5436556307801,22.4279655044851,78.6565057690561));
#152812=CARTESIAN_POINT('Ctrl Pts',(17.5433331744752,22.4284660977953,78.6562670091422));
#152813=CARTESIAN_POINT('Ctrl Pts',(17.5430107883002,22.4289667455025,78.6560282691331));
#152814=CARTESIAN_POINT('Ctrl Pts',(17.5426884722822,22.4294674475864,78.6557895490448));
#152815=CARTESIAN_POINT('Ctrl Pts',(17.3892006190096,22.6679032797583,78.5421103278949));
#152816=CARTESIAN_POINT('Ctrl Pts',(17.2516260865013,22.91867136202,78.4329499479108));
#152817=CARTESIAN_POINT('Ctrl Pts',(17.1308164024521,23.1779493409036,78.3294294576132));
#152818=CARTESIAN_POINT('Ctrl Pts',(17.0950583166704,23.2546922302106,78.2987887469669));
#152819=CARTESIAN_POINT('Ctrl Pts',(17.0607686562475,23.3321805774696,78.2686420158084));
#152820=CARTESIAN_POINT('Ctrl Pts',(17.0279686886132,23.4103151652504,78.2390179986263));
#152821=CARTESIAN_POINT('Ctrl Pts',(16.9418410159583,23.6154845810995,78.1612298836188));
#152822=CARTESIAN_POINT('Ctrl Pts',(16.8659609336768,23.8251558422008,78.0870264878607));
#152823=CARTESIAN_POINT('Ctrl Pts',(16.8006819883727,24.0377033797527,78.0168806813474));
#152824=CARTESIAN_POINT('Ctrl Pts',(16.7569336799293,24.1801473973206,77.9698707248437));
#152825=CARTESIAN_POINT('Ctrl Pts',(16.7179476188404,24.3238837428768,77.924683472366));
#152826=CARTESIAN_POINT('Ctrl Pts',(16.6838422822653,24.468425051943,77.8814661384565));
#152827=CARTESIAN_POINT('Ctrl Pts',(16.6837151459022,24.4689638666331,77.8813050347933));
#152828=CARTESIAN_POINT('Ctrl Pts',(16.6835880774277,24.4695026922809,77.881143958578));
#152829=CARTESIAN_POINT('Ctrl Pts',(16.6834610768493,24.4700415288566,77.8809829098195));
#152830=CARTESIAN_POINT('Ctrl Pts',(16.6366722700736,24.6685565335379,77.8216502726667));
#152831=CARTESIAN_POINT('Ctrl Pts',(16.5991031763914,24.868555425736,77.7660460631051));
#152832=CARTESIAN_POINT('Ctrl Pts',(16.57030512461,25.0687079639017,77.7142355762191));
#152833=CARTESIAN_POINT('Ctrl Pts',(16.5469232938871,25.2312166225316,77.6721693960747));
#152834=CARTESIAN_POINT('Ctrl Pts',(16.5293224072309,25.3938260497807,77.6326037348469));
#152835=CARTESIAN_POINT('Ctrl Pts',(16.5172392852194,25.5558247763328,77.5955633957734));
#152836=CARTESIAN_POINT('Ctrl Pts',(16.5026188695806,25.7518410635896,77.5507450820837));
#152837=CARTESIAN_POINT('Ctrl Pts',(16.4960688129371,25.9469850810175,77.5096162455846));
#152838=CARTESIAN_POINT('Ctrl Pts',(16.4971157343381,26.140278270034,77.4721624214652));
#152839=CARTESIAN_POINT('Ctrl Pts',(16.4980025980298,26.3040199903037,77.4404346941551));
#152840=CARTESIAN_POINT('Ctrl Pts',(16.5043421206547,26.4664339872537,77.4113445365776));
#152841=CARTESIAN_POINT('Ctrl Pts',(16.5158721328963,26.62691877866,77.3848956136509));
#152842=CARTESIAN_POINT('Ctrl Pts',(1.23275780153909,24.69194692623,92.79547180931));
#152843=CARTESIAN_POINT('Ctrl Pts',(1.99037470125288,25.2226352445827,92.4576622723953));
#152844=CARTESIAN_POINT('Ctrl Pts',(2.75938293298785,25.6890597071317,92.0771176746582));
#152845=CARTESIAN_POINT('Ctrl Pts',(3.92098936528719,26.2923006172496,91.4347419076188));
#152846=CARTESIAN_POINT('Ctrl Pts',(4.30952220315875,26.4773149566713,91.2086956120099));
#152847=CARTESIAN_POINT('Ctrl Pts',(4.8930242498354,26.7307375198775,90.8508771482829));
#152848=CARTESIAN_POINT('Ctrl Pts',(5.18494917491221,26.851424064999,90.6672814614646));
#152849=CARTESIAN_POINT('Ctrl Pts',(5.52553055718069,26.9816817454645,90.4447048347504));
#152850=CARTESIAN_POINT('Ctrl Pts',(5.69578263189675,27.0441747634866,90.3312993469999));
#152851=CARTESIAN_POINT('Ctrl Pts',(5.76873529807879,27.070392666451,90.2822410057258));
#152852=CARTESIAN_POINT('Ctrl Pts',(5.81736715483406,27.0877457530838,90.2494338595921));
#152853=CARTESIAN_POINT('Ctrl Pts',(5.84317307001101,27.0968841603482,90.2319668635416));
#152854=CARTESIAN_POINT('Ctrl Pts',(6.59626022173228,27.3617555700107,89.7207092547717));
#152855=CARTESIAN_POINT('Ctrl Pts',(7.32748827641959,27.5632869808104,89.177216366884));
#152856=CARTESIAN_POINT('Ctrl Pts',(8.41450607645436,27.7826137082458,88.2847550197912));
#152857=CARTESIAN_POINT('Ctrl Pts',(8.77518981053865,27.8418942192636,87.9744085087981));
#152858=CARTESIAN_POINT('Ctrl Pts',(9.31216035509837,27.9100723885993,87.4890121728745));
#152859=CARTESIAN_POINT('Ctrl Pts',(9.57963016181105,27.9389758239694,87.2413462190352));
#152860=CARTESIAN_POINT('Ctrl Pts',(9.88953951596442,27.9636216122967,86.9435958459439));
#152861=CARTESIAN_POINT('Ctrl Pts',(10.0439129722782,27.9736757848926,86.7925060680695));
#152862=CARTESIAN_POINT('Ctrl Pts',(10.12094854271,27.9781356907987,86.7164059576889));
#152863=CARTESIAN_POINT('Ctrl Pts',(10.1539307653767,27.9799255403887,86.6836724838006));
#152864=CARTESIAN_POINT('Ctrl Pts',(10.1759115053255,27.9810917648586,86.6618236740342));
#152865=CARTESIAN_POINT('Ctrl Pts',(10.1882885335909,27.9817317716749,86.6494997130189));
#152866=CARTESIAN_POINT('Ctrl Pts',(10.8118051772457,28.0133025816265,86.0278008089336));
#152867=CARTESIAN_POINT('Ctrl Pts',(11.4271146397258,28.0022536845851,85.3612777556491));
#152868=CARTESIAN_POINT('Ctrl Pts',(12.3365974155725,27.9224793356862,84.2732251185324));
#152869=CARTESIAN_POINT('Ctrl Pts',(12.6374842751345,27.8853543854972,83.8958448105857));
#152870=CARTESIAN_POINT('Ctrl Pts',(13.0832130151965,27.8138667093793,83.3070638705607));
#152871=CARTESIAN_POINT('Ctrl Pts',(13.3046744335626,27.7741728086118,83.0069978057266));
#152872=CARTESIAN_POINT('Ctrl Pts',(13.56008482604,27.7209506479765,82.6468659740776));
#152873=CARTESIAN_POINT('Ctrl Pts',(13.6869844531481,27.6926114152238,82.4642729700953));
#152874=CARTESIAN_POINT('Ctrl Pts',(13.7547418214793,27.6769667854183,82.3657766620698));
#152875=CARTESIAN_POINT('Ctrl Pts',(13.7862995872375,27.6695399470608,82.3196267535338));
#152876=CARTESIAN_POINT('Ctrl Pts',(13.8043171073331,27.665265179563,82.2932100387377));
#152877=CARTESIAN_POINT('Ctrl Pts',(13.8098802979734,27.6639410447168,82.2850451218363));
#152878=CARTESIAN_POINT('Ctrl Pts',(14.2538584320099,27.5580367056132,81.6329789913368));
#152879=CARTESIAN_POINT('Ctrl Pts',(14.7117977987722,27.4191449094803,80.9064250815115));
#152880=CARTESIAN_POINT('Ctrl Pts',(15.6262304717903,27.0737444754176,79.2791922290114));
#152881=CARTESIAN_POINT('Ctrl Pts',(16.0827382847579,26.867235837488,78.3784032011472));
#152882=CARTESIAN_POINT('Ctrl Pts',(16.5158721306991,26.62691877866,77.384895612693));
#152883=CARTESIAN_POINT('Origin',(-10.9843331791359,-92.5,65.395787724084));
#152884=CARTESIAN_POINT('Origin',(-10.9843331791359,92.,65.395787724084));
#152885=CARTESIAN_POINT('Origin',(-10.9843331791359,-92.5,80.581991049076));
#152886=CARTESIAN_POINT('Origin',(-10.9843331791359,92.,80.581991049076));
#152887=CARTESIAN_POINT('',(9.66896668869965,27.5617702389202,58.8232869212091));
#152888=CARTESIAN_POINT('Ctrl Pts',(16.5158747359332,25.68037166863,68.59288913751));
#152889=CARTESIAN_POINT('Ctrl Pts',(16.4459098082595,25.7023664947635,68.4324058857396));
#152890=CARTESIAN_POINT('Ctrl Pts',(16.3708016848024,25.7264355825049,68.2638291090571));
#152891=CARTESIAN_POINT('Ctrl Pts',(16.2900924916398,25.7526220639059,68.087416378764));
#152892=CARTESIAN_POINT('Ctrl Pts',(16.2145217776279,25.777141341319,67.9222352455293));
#152893=CARTESIAN_POINT('Ctrl Pts',(16.1340400901703,25.8035174070722,67.7501844193478));
#152894=CARTESIAN_POINT('Ctrl Pts',(16.0482330249535,25.8317680994321,67.5715021767688));
#152895=CARTESIAN_POINT('Ctrl Pts',(15.9641112558687,25.8594639332562,67.3963293479136));
#152896=CARTESIAN_POINT('Ctrl Pts',(15.8748711423744,25.8889619931436,67.2147830510035));
#152897=CARTESIAN_POINT('Ctrl Pts',(15.7800870845148,25.9202546953833,67.0271128863405));
#152898=CARTESIAN_POINT('Ctrl Pts',(15.6882391434718,25.9505780465384,66.84525616266));
#152899=CARTESIAN_POINT('Ctrl Pts',(15.5911852428945,25.9825869923839,66.6576491436249));
#152900=CARTESIAN_POINT('Ctrl Pts',(15.4885068102668,26.0162448440536,66.4645421677599));
#152901=CARTESIAN_POINT('Ctrl Pts',(15.4589311972375,26.0259396900978,66.4089194138352));
#152902=CARTESIAN_POINT('Ctrl Pts',(15.4288887343077,26.0357711263778,66.3528404898641));
#152903=CARTESIAN_POINT('Ctrl Pts',(15.3983689445526,26.0457377209224,66.2963117436976));
#152904=CARTESIAN_POINT('Ctrl Pts',(15.2935013134504,26.0799834732175,66.1020759462948));
#152905=CARTESIAN_POINT('Ctrl Pts',(15.1830052612199,26.1158519036328,65.9025373029214));
#152906=CARTESIAN_POINT('Ctrl Pts',(15.0664620478353,26.1533704672762,65.6980085872791));
#152907=CARTESIAN_POINT('Ctrl Pts',(14.9532564079349,26.1898145714161,65.4993371806836));
#152908=CARTESIAN_POINT('Ctrl Pts',(14.8343448523761,26.2278159253131,65.2959575066244));
#152909=CARTESIAN_POINT('Ctrl Pts',(14.7093219885693,26.2673607483818,65.0881773775743));
#152910=CARTESIAN_POINT('Ctrl Pts',(14.6706560100771,26.2795908255989,65.0239169554696));
#152911=CARTESIAN_POINT('Ctrl Pts',(14.6314053420285,26.2919682299591,64.9592357867873));
#152912=CARTESIAN_POINT('Ctrl Pts',(14.5915575904957,26.3044917041774,64.8941433845765));
#152913=CARTESIAN_POINT('Ctrl Pts',(14.4642369251658,26.3445064354577,64.6861615628025));
#152914=CARTESIAN_POINT('Ctrl Pts',(14.330824459311,26.3860287580984,64.4739844034523));
#152915=CARTESIAN_POINT('Ctrl Pts',(14.1909215845456,26.429062909699,64.2579613569774));
#152916=CARTESIAN_POINT('Ctrl Pts',(14.1652678660448,26.4369539985199,64.2183496303904));
#152917=CARTESIAN_POINT('Ctrl Pts',(14.1393958721347,26.4448957968062,64.1786086419067));
#152918=CARTESIAN_POINT('Ctrl Pts',(14.1133030877435,26.4528881597977,64.1387406151485));
#152919=CARTESIAN_POINT('Ctrl Pts',(14.0291080325024,26.4786775670719,64.0100962104369));
#152920=CARTESIAN_POINT('Ctrl Pts',(13.9426145712807,26.5049953038812,63.8801294315358));
#152921=CARTESIAN_POINT('Ctrl Pts',(13.8537392943827,26.5318413543076,63.7489197144917));
#152922=CARTESIAN_POINT('Ctrl Pts',(13.8093016559336,26.5452643795209,63.6833148559696));
#152923=CARTESIAN_POINT('Ctrl Pts',(13.7642685318244,26.5588194830634,63.6173992890108));
#152924=CARTESIAN_POINT('Ctrl Pts',(13.7186295371029,26.5725066620024,63.5511834160091));
#152925=CARTESIAN_POINT('Ctrl Pts',(13.6958100397421,26.5793502514719,63.5180754795082));
#152926=CARTESIAN_POINT('Ctrl Pts',(13.6728390729451,26.5862268597882,63.4848924679298));
#152927=CARTESIAN_POINT('Ctrl Pts',(13.6497153358115,26.5931364865593,63.4516357011427));
#152928=CARTESIAN_POINT('Ctrl Pts',(13.6282808843813,26.5995413361981,63.4208084802527));
#152929=CARTESIAN_POINT('Ctrl Pts',(13.6074099997462,26.6057675296784,63.3909096946062));
#152930=CARTESIAN_POINT('Ctrl Pts',(13.5851694912851,26.6123907729804,63.3591823036636));
#152931=CARTESIAN_POINT('Ctrl Pts',(13.5834166788512,26.6129127620902,63.3566818138283));
#152932=CARTESIAN_POINT('Ctrl Pts',(13.5816553376048,26.6134372177213,63.3541699818618));
#152933=CARTESIAN_POINT('Ctrl Pts',(13.5798845098451,26.6139644218352,63.3516454664426));
#152934=CARTESIAN_POINT('Ctrl Pts',(13.4348263677831,26.6571505808716,63.144848665166));
#152935=CARTESIAN_POINT('Ctrl Pts',(13.2906713269679,26.6991517299152,62.9449804241607));
#152936=CARTESIAN_POINT('Ctrl Pts',(13.1478211692805,26.7398786761325,62.7518015164918));
#152937=CARTESIAN_POINT('Ctrl Pts',(13.0019686553813,26.7814616018036,62.5545624670433));
#152938=CARTESIAN_POINT('Ctrl Pts',(12.8574765519758,26.8217164212871,62.3642968595557));
#152939=CARTESIAN_POINT('Ctrl Pts',(12.7147524235516,26.8605974413362,62.1807611240509));
#152940=CARTESIAN_POINT('Ctrl Pts',(12.5673203685204,26.9007609984785,61.9911712421167));
#152941=CARTESIAN_POINT('Ctrl Pts',(12.4217750071565,26.9394588097394,61.8087624702855));
#152942=CARTESIAN_POINT('Ctrl Pts',(12.278542312745,26.9766895356588,61.6332788391071));
#152943=CARTESIAN_POINT('Ctrl Pts',(12.1323852990195,27.0146803850356,61.4542124353357));
#152944=CARTESIAN_POINT('Ctrl Pts',(11.9886364670197,27.0511439628675,61.2823567753943));
#152945=CARTESIAN_POINT('Ctrl Pts',(11.8477225193739,27.0861249741561,61.1174536620441));
#152946=CARTESIAN_POINT('Ctrl Pts',(11.7027389237983,27.1221162502378,60.9477880846151));
#152947=CARTESIAN_POINT('Ctrl Pts',(11.5607564832687,27.1565384199676,60.7854823417614));
#152948=CARTESIAN_POINT('Ctrl Pts',(11.4222105981809,27.1894834912378,60.6302708610468));
#152949=CARTESIAN_POINT('Ctrl Pts',(11.4111877277838,27.1921046391023,60.6179220566419));
#152950=CARTESIAN_POINT('Ctrl Pts',(11.4001865949999,27.1947164574398,60.6056181671864));
#152951=CARTESIAN_POINT('Ctrl Pts',(11.3892074109533,27.1973190029251,60.5933590633205));
#152952=CARTESIAN_POINT('Ctrl Pts',(11.2465292019462,27.2311399614894,60.4340478634905));
#152953=CARTESIAN_POINT('Ctrl Pts',(11.1075447488207,27.2633192232488,60.2822800986382));
#152954=CARTESIAN_POINT('Ctrl Pts',(10.9726453414288,27.2938212954465,60.1377288074397));
#152955=CARTESIAN_POINT('Ctrl Pts',(10.8339787621069,27.3251751619732,59.9891408078731));
#152956=CARTESIAN_POINT('Ctrl Pts',(10.6996286506066,27.3547572947639,59.848177795414));
#152957=CARTESIAN_POINT('Ctrl Pts',(10.5699800376746,27.3825557890386,59.7145119675845));
#152958=CARTESIAN_POINT('Ctrl Pts',(10.4387257766684,27.4106985569448,59.5791907400234));
#152959=CARTESIAN_POINT('Ctrl Pts',(10.3122901776469,27.4370137383686,59.4513484768771));
#152960=CARTESIAN_POINT('Ctrl Pts',(10.1910319724966,27.4615085851807,59.3306744916551));
#152961=CARTESIAN_POINT('Ctrl Pts',(10.0681689845437,27.4863276072424,59.2084034554462));
#152962=CARTESIAN_POINT('Ctrl Pts',(9.95062134681771,27.509278282649,59.0934916163665));
#152963=CARTESIAN_POINT('Ctrl Pts',(9.83872060946937,27.5303805812036,58.985647044844));
#152964=CARTESIAN_POINT('Ctrl Pts',(9.78059920408066,27.5413411457002,58.9296324178723));
#152965=CARTESIAN_POINT('Ctrl Pts',(9.72400052762142,27.5518032151801,58.8755249005202));
#152966=CARTESIAN_POINT('Ctrl Pts',(9.66896668055068,27.5617702389205,58.8232869297943));
#152967=CARTESIAN_POINT('Ctrl Pts',(1.23275780212867,24.13180332306,53.1823069641179));
#152968=CARTESIAN_POINT('Ctrl Pts',(1.24922759706115,24.1480653974204,53.1896505883185));
#152969=CARTESIAN_POINT('Ctrl Pts',(1.27440967752685,24.1734031842924,53.2008913260592));
#152970=CARTESIAN_POINT('Ctrl Pts',(1.3085221121756,24.2072241748601,53.2162148169485));
#152971=CARTESIAN_POINT('Ctrl Pts',(1.34067084263351,24.2390982384025,53.2306562012515));
#152972=CARTESIAN_POINT('Ctrl Pts',(1.38075131620029,24.2785069351784,53.2487240377262));
#152973=CARTESIAN_POINT('Ctrl Pts',(1.42892482678689,24.3249543034778,53.2706193208307));
#152974=CARTESIAN_POINT('Ctrl Pts',(1.47640302832188,24.3707312768816,53.2921985798726));
#152975=CARTESIAN_POINT('Ctrl Pts',(1.53174246303046,24.4233452037699,53.317495505027));
#152976=CARTESIAN_POINT('Ctrl Pts',(1.5950753971386,24.4823212892496,53.3467477075681));
#152977=CARTESIAN_POINT('Ctrl Pts',(1.65719135552206,24.5401641181484,53.3754378136125));
#152978=CARTESIAN_POINT('Ctrl Pts',(1.7269966919911,24.6041269503153,53.4079326235042));
#152979=CARTESIAN_POINT('Ctrl Pts',(1.80459287974523,24.6737618385938,53.4445009245182));
#152980=CARTESIAN_POINT('Ctrl Pts',(1.82314049055782,24.6904064811227,53.4532417484545));
#152981=CARTESIAN_POINT('Ctrl Pts',(1.84213311292883,24.7073751913143,53.4622155123241));
#152982=CARTESIAN_POINT('Ctrl Pts',(1.86157191681418,24.7246618517312,53.4714262769093));
#152983=CARTESIAN_POINT('Ctrl Pts',(1.93892890328496,24.7934543537738,53.50808064081));
#152984=CARTESIAN_POINT('Ctrl Pts',(2.02341605629018,24.8671314325845,53.5485142421835));
#152985=CARTESIAN_POINT('Ctrl Pts',(2.11519799494867,24.9449326669951,53.5930621518562));
#152986=CARTESIAN_POINT('Ctrl Pts',(2.20469853691352,25.0208000189715,53.6365027472214));
#152987=CARTESIAN_POINT('Ctrl Pts',(2.30113587746158,25.1005890488324,53.6838556337299));
#152988=CARTESIAN_POINT('Ctrl Pts',(2.40463675923085,25.183594642293,53.7354738822346));
#152989=CARTESIAN_POINT('Ctrl Pts',(2.43996923889309,25.2119305694142,53.7530949950629));
#152990=CARTESIAN_POINT('Ctrl Pts',(2.47612463805057,25.2406413420158,53.7712135484868));
#152991=CARTESIAN_POINT('Ctrl Pts',(2.51310722943784,25.2696989090092,53.7898447666857));
#152992=CARTESIAN_POINT('Ctrl Pts',(2.61818119077468,25.3522565004673,53.8427792914785));
#152993=CARTESIAN_POINT('Ctrl Pts',(2.72993999096494,25.4375824234251,53.8998518017394));
#152994=CARTESIAN_POINT('Ctrl Pts',(2.84847168809193,25.5248859158878,53.9614442946384));
#152995=CARTESIAN_POINT('Ctrl Pts',(2.87456719151849,25.5441063323834,53.9750042718298));
#152996=CARTESIAN_POINT('Ctrl Pts',(2.90099085274009,25.5634225993189,53.9887834894792));
#152997=CARTESIAN_POINT('Ctrl Pts',(2.92774340859437,25.5828262786981,54.002786301433));
#152998=CARTESIAN_POINT('Ctrl Pts',(3.00187777568457,25.6365960754173,54.0415896818401));
#152999=CARTESIAN_POINT('Ctrl Pts',(3.07853802377204,25.6910344099707,54.0821095823487));
#153000=CARTESIAN_POINT('Ctrl Pts',(3.15773517204983,25.7459457441527,54.1244419798521));
#153001=CARTESIAN_POINT('Ctrl Pts',(3.19733374618873,25.7734014112436,54.1456081786038));
#153002=CARTESIAN_POINT('Ctrl Pts',(3.23756648761963,25.8009753282418,54.1672276054822));
#153003=CARTESIAN_POINT('Ctrl Pts',(3.27843408473616,25.8286418990266,54.1893127087366));
#153004=CARTESIAN_POINT('Ctrl Pts',(3.29886788329442,25.842475184419,54.2003552603638));
#153005=CARTESIAN_POINT('Ctrl Pts',(3.31946039210981,25.8563316332581,54.2115142377327));
#153006=CARTESIAN_POINT('Ctrl Pts',(3.34021167400882,25.8702079929798,54.2227912366719));
#153007=CARTESIAN_POINT('Ctrl Pts',(3.35058731495833,25.8771461728407,54.2284297361415));
#153008=CARTESIAN_POINT('Ctrl Pts',(3.36100264894217,25.8840893304222,54.2340977414226));
#153009=CARTESIAN_POINT('Ctrl Pts',(3.37145768859112,25.8910370435328,54.239795457932));
#153010=CARTESIAN_POINT('Ctrl Pts',(3.37668520841559,25.8945109000882,54.2426443161867));
#153011=CARTESIAN_POINT('Ctrl Pts',(3.3819226546413,25.8979858955258,54.2455006022758));
#153012=CARTESIAN_POINT('Ctrl Pts',(3.3871700281858,25.9014619775766,54.2483643417282));
#153013=CARTESIAN_POINT('Ctrl Pts',(3.38979371495805,25.903200018602,54.2497962114543));
#153014=CARTESIAN_POINT('Ctrl Pts',(3.39241988355906,25.9049383312807,54.251229944523));
#153015=CARTESIAN_POINT('Ctrl Pts',(3.39504853411381,25.9066769090288,54.2526655441441));
#153016=CARTESIAN_POINT('Ctrl Pts',(3.39767718466856,25.908415486777,54.2541011437651));
#153017=CARTESIAN_POINT('Ctrl Pts',(3.40151786624113,25.9109530525223,54.2561996586179));
#153018=CARTESIAN_POINT('Ctrl Pts',(3.40294193175905,25.9118934308925,54.2569779458803));
#153019=CARTESIAN_POINT('Ctrl Pts',(3.65218015250606,26.0764773133412,54.3931928391448));
#153020=CARTESIAN_POINT('Ctrl Pts',(3.90334231127312,26.2298342139882,54.535060473175));
#153021=CARTESIAN_POINT('Ctrl Pts',(4.15573981610667,26.371901834692,54.6826051548366));
#153022=CARTESIAN_POINT('Ctrl Pts',(4.27252416903728,26.4376365382392,54.7508740950845));
#153023=CARTESIAN_POINT('Ctrl Pts',(4.38957306574967,26.5009543041443,54.8203577276091));
#153024=CARTESIAN_POINT('Ctrl Pts',(4.5068187742771,26.5618489611465,54.8910546870773));
#153025=CARTESIAN_POINT('Ctrl Pts',(4.69213892805981,26.6580998801944,55.0027992580741));
#153026=CARTESIAN_POINT('Ctrl Pts',(4.87795159594536,26.748297190703,55.1175764440731));
#153027=CARTESIAN_POINT('Ctrl Pts',(5.06399849957787,26.8324173905609,55.2353729249555));
#153028=CARTESIAN_POINT('Ctrl Pts',(5.15702195139412,26.8744774904898,55.2942711653967));
#153029=CARTESIAN_POINT('Ctrl Pts',(5.25010413704565,26.915018312756,55.3539240772649));
#153030=CARTESIAN_POINT('Ctrl Pts',(5.34321355468929,26.9540369872704,55.4143289078529));
#153031=CARTESIAN_POINT('Ctrl Pts',(5.38976826351112,26.9735463245276,55.4445313231469));
#153032=CARTESIAN_POINT('Ctrl Pts',(5.43632979261359,26.9926751248468,55.474921709351));
#153033=CARTESIAN_POINT('Ctrl Pts',(5.48289426716108,27.0114230236912,55.5054996630802));
#153034=CARTESIAN_POINT('Ctrl Pts',(5.50617650443482,27.0207969731135,55.5207886399447));
#153035=CARTESIAN_POINT('Ctrl Pts',(5.52945947903618,27.030075697167,55.5361245084827));
#153036=CARTESIAN_POINT('Ctrl Pts',(5.55274255826553,27.0392587624797,55.5515071133737));
#153037=CARTESIAN_POINT('Ctrl Pts',(5.57444917700966,27.0478200569581,55.5658481864068));
#153038=CARTESIAN_POINT('Ctrl Pts',(5.59767411521259,27.0568843890177,55.581238267158));
#153039=CARTESIAN_POINT('Ctrl Pts',(5.61817054560409,27.0648119703249,55.5948569583085));
#153040=CARTESIAN_POINT('Ctrl Pts',(5.61965911519574,27.0653877172352,55.5958460266066));
#153041=CARTESIAN_POINT('Ctrl Pts',(5.6211333058231,27.0659574683464,55.5968257327792));
#153042=CARTESIAN_POINT('Ctrl Pts',(5.62259149634526,27.0665205955125,55.5977949879077));
#153043=CARTESIAN_POINT('Ctrl Pts',(5.84891017131741,27.1539208303596,55.7482283730251));
#153044=CARTESIAN_POINT('Ctrl Pts',(6.07562464989286,27.2324148761963,55.9033636707012));
#153045=CARTESIAN_POINT('Ctrl Pts',(6.3021361807368,27.3015027510538,56.0630600554502));
#153046=CARTESIAN_POINT('Ctrl Pts',(6.53375524878111,27.3721484666517,56.2263573837045));
#153047=CARTESIAN_POINT('Ctrl Pts',(6.76516172690714,27.4329590351902,56.3944240383909));
#153048=CARTESIAN_POINT('Ctrl Pts',(6.9957374952623,27.4833998845232,56.5670569758031));
#153049=CARTESIAN_POINT('Ctrl Pts',(7.22631326361745,27.5338407338561,56.7396899132153));
#153050=CARTESIAN_POINT('Ctrl Pts',(7.45605801145856,27.5739118639835,56.9168891151683));
#153051=CARTESIAN_POINT('Ctrl Pts',(7.6843805945019,27.6030787027589,57.0983983503856));
#153052=CARTESIAN_POINT('Ctrl Pts',(7.89040519895813,27.6293971086821,57.2621813975653));
#153053=CARTESIAN_POINT('Ctrl Pts',(8.09526409678687,27.6468405362001,57.4294678871763));
#153054=CARTESIAN_POINT('Ctrl Pts',(8.29846844405858,27.655078180412,57.5999641245306));
#153055=CARTESIAN_POINT('Ctrl Pts',(8.5012141214738,27.6632972307349,57.7700755202919));
#153056=CARTESIAN_POINT('Ctrl Pts',(8.70231251363328,27.662352009166,57.9433820782813));
#153057=CARTESIAN_POINT('Ctrl Pts',(8.90130878651381,27.6519139458157,58.1195503176241));
#153058=CARTESIAN_POINT('Ctrl Pts',(9.1000757923728,27.6414879083373,58.2955155905145));
#153059=CARTESIAN_POINT('Ctrl Pts',(9.29674534304399,27.6215908902089,58.4743358168237));
#153060=CARTESIAN_POINT('Ctrl Pts',(9.4908976461116,27.591895455886,58.6556388067892));
#153061=CARTESIAN_POINT('Ctrl Pts',(9.55049475305616,27.5827801276249,58.7112916809072));
#153062=CARTESIAN_POINT('Ctrl Pts',(9.60985492117232,27.5727415454755,58.7671782174972));
#153063=CARTESIAN_POINT('Ctrl Pts',(9.66896668003918,27.56177023892,58.8232869303331));
#153064=CARTESIAN_POINT('Ctrl Pts',(1.02018651496909,24.12736861615,53.08644276134));
#153065=CARTESIAN_POINT('Ctrl Pts',(1.28010839926909,23.74963944379,53.21264495039));
#153066=CARTESIAN_POINT('Ctrl Pts',(1.69372155058909,23.19034260218,53.33423556322));
#153067=CARTESIAN_POINT('Ctrl Pts',(2.28532636027909,22.4683497999,53.36025868992));
#153068=CARTESIAN_POINT('Ctrl Pts',(2.72064084369909,21.96878201391,53.31931450845));
#153069=CARTESIAN_POINT('Ctrl Pts',(3.16680680853909,21.48749253734,53.21907255652));
#153070=CARTESIAN_POINT('Ctrl Pts',(3.80379334035909,20.84237217285,52.99629044043));
#153071=CARTESIAN_POINT('Ctrl Pts',(4.28807530375909,20.4025094424,52.73095649241));
#153072=CARTESIAN_POINT('Ctrl Pts',(4.61113719324909,20.13148505149,52.51146626848));
#153073=CARTESIAN_POINT('Ctrl Pts',(1.72739619405909,24.87088028168,53.3946519969));
#153074=CARTESIAN_POINT('Ctrl Pts',(1.98016437202909,24.43764203493,53.52791146856));
#153075=CARTESIAN_POINT('Ctrl Pts',(2.39170334478909,23.79368517934,53.64972059236));
#153076=CARTESIAN_POINT('Ctrl Pts',(2.99363132225909,22.96415595654,53.65205971503));
#153077=CARTESIAN_POINT('Ctrl Pts',(3.44088690595909,22.39235728434,53.58369970474));
#153078=CARTESIAN_POINT('Ctrl Pts',(3.90240318107909,21.84503415371,53.44568945113));
#153079=CARTESIAN_POINT('Ctrl Pts',(4.56392990621909,21.11826512872,53.15625082403));
#153080=CARTESIAN_POINT('Ctrl Pts',(5.06794995464909,20.63347851478,52.82593298942));
#153081=CARTESIAN_POINT('Ctrl Pts',(5.40276176874909,20.34145978504,52.55843576862));
#153082=CARTESIAN_POINT('Ctrl Pts',(3.17914527510909,26.09640831234,54.09413185087));
#153083=CARTESIAN_POINT('Ctrl Pts',(3.40222081686909,25.56141982058,54.23518571775));
#153084=CARTESIAN_POINT('Ctrl Pts',(3.78905928284909,24.75971584166,54.348934864));
#153085=CARTESIAN_POINT('Ctrl Pts',(4.39075430025909,23.73217540148,54.29225680523));
#153086=CARTESIAN_POINT('Ctrl Pts',(4.84985111793909,23.03008574148,54.16070223457));
#153087=CARTESIAN_POINT('Ctrl Pts',(5.33269502402909,22.36806245594,53.93909869207));
#153088=CARTESIAN_POINT('Ctrl Pts',(6.03347108353909,21.50817639152,53.50650311147));
#153089=CARTESIAN_POINT('Ctrl Pts',(6.57305116340909,20.96447914599,53.04243066886));
#153090=CARTESIAN_POINT('Ctrl Pts',(6.92979819842909,20.65505525241,52.68021892232));
#153091=CARTESIAN_POINT('Ctrl Pts',(5.43493315155909,27.31689412349,55.42149232346));
#153092=CARTESIAN_POINT('Ctrl Pts',(5.57886835666909,26.65149635406,55.54636262511));
#153093=CARTESIAN_POINT('Ctrl Pts',(5.88091137179909,25.6387335644,55.60927396635));
#153094=CARTESIAN_POINT('Ctrl Pts',(6.44001219137909,24.35121556071,55.41502290768));
#153095=CARTESIAN_POINT('Ctrl Pts',(6.89713355269909,23.48579054893,55.15603975691));
#153096=CARTESIAN_POINT('Ctrl Pts',(7.40256384026909,22.69322035286,54.78097445767));
#153097=CARTESIAN_POINT('Ctrl Pts',(8.16206876439909,21.708389665,54.1053488272));
#153098=CARTESIAN_POINT('Ctrl Pts',(8.76799204153909,21.15393359669,53.44033099395));
#153099=CARTESIAN_POINT('Ctrl Pts',(9.16935658079909,20.87624188168,52.95149370635));
#153100=CARTESIAN_POINT('Ctrl Pts',(7.68979117344909,27.96384357157,57.042983249));
#153101=CARTESIAN_POINT('Ctrl Pts',(7.72330678673909,27.18890190058,57.11221136924));
#153102=CARTESIAN_POINT('Ctrl Pts',(7.89618292747909,25.99000196864,57.067606522));
#153103=CARTESIAN_POINT('Ctrl Pts',(8.38110448977909,24.47966951747,56.66954723005));
#153104=CARTESIAN_POINT('Ctrl Pts',(8.82812186513909,23.48367508624,56.24292428671));
#153105=CARTESIAN_POINT('Ctrl Pts',(9.36273061159909,22.60305442893,55.68503473905));
#153106=CARTESIAN_POINT('Ctrl Pts',(10.2085995213291,21.56855669904,54.74658540708));
#153107=CARTESIAN_POINT('Ctrl Pts',(10.9188216964491,21.07709473119,53.90000039928));
#153108=CARTESIAN_POINT('Ctrl Pts',(11.3923064424291,20.88050279146,53.31616956596));
#153109=CARTESIAN_POINT('Ctrl Pts',(9.13342233188909,27.94957487251,58.2979440507));
#153110=CARTESIAN_POINT('Ctrl Pts',(9.08106830642909,27.12604219688,58.29819803193));
#153111=CARTESIAN_POINT('Ctrl Pts',(9.14758840929909,25.83611398064,58.13417901149));
#153112=CARTESIAN_POINT('Ctrl Pts',(9.57241865212909,24.22058009908,57.54766571695));
#153113=CARTESIAN_POINT('Ctrl Pts',(10.0146980747891,23.17051685142,56.98046127077));
#153114=CARTESIAN_POINT('Ctrl Pts',(10.5806282235291,22.26779541216,56.28459372418));
#153115=CARTESIAN_POINT('Ctrl Pts',(11.5120991780291,21.25642831637,55.17124635962));
#153116=CARTESIAN_POINT('Ctrl Pts',(12.3210049830591,20.85107620434,54.23646469467));
#153117=CARTESIAN_POINT('Ctrl Pts',(12.8602418793091,20.73195002337,53.62410434214));
#153118=CARTESIAN_POINT('Ctrl Pts',(9.83727978500909,27.81219977272,58.97626003861));
#153119=CARTESIAN_POINT('Ctrl Pts',(9.73949458818909,26.97238804509,58.93119606197));
#153120=CARTESIAN_POINT('Ctrl Pts',(9.74858544025909,25.64882808166,58.69043954903));
#153121=CARTESIAN_POINT('Ctrl Pts',(10.1431268412991,23.99629606828,57.99131379478));
#153122=CARTESIAN_POINT('Ctrl Pts',(10.5860577947591,22.93050615594,57.34439895311));
#153123=CARTESIAN_POINT('Ctrl Pts',(11.1738219636591,22.02828425791,56.57543834793));
#153124=CARTESIAN_POINT('Ctrl Pts',(12.1599880660491,21.0444542549,55.37786778629));
#153125=CARTESIAN_POINT('Ctrl Pts',(13.0285934306291,20.6920670675,54.41291434299));
#153126=CARTESIAN_POINT('Ctrl Pts',(13.6062929436291,20.61550204861,53.7987131345));
#153127=CARTESIAN_POINT('Ctrl Pts',(4.64898302763928,20.2571697908605,52.5914041824882));
#153128=CARTESIAN_POINT('Ctrl Pts',(4.37640638855581,20.4917590865083,52.7746243664382));
#153129=CARTESIAN_POINT('Ctrl Pts',(4.09631448667638,20.7498815758729,52.9317573917127));
#153130=CARTESIAN_POINT('Ctrl Pts',(3.81504798690012,21.0269126271465,53.0570185057454));
#153131=CARTESIAN_POINT('Ctrl Pts',(3.79438846371867,21.0472610491246,53.066219156698));
#153132=CARTESIAN_POINT('Ctrl Pts',(3.77372260637565,21.0677114719799,53.0752478720827));
#153133=CARTESIAN_POINT('Ctrl Pts',(3.75305292839587,21.0882620568661,53.0841023688874));
#153134=CARTESIAN_POINT('Ctrl Pts',(3.75282391110331,21.0884897546229,53.0842004755385));
#153135=CARTESIAN_POINT('Ctrl Pts',(3.7525948933306,21.0887174646872,53.0842985608067));
#153136=CARTESIAN_POINT('Ctrl Pts',(3.75236587508114,21.0889451870564,53.084396624689));
#153137=CARTESIAN_POINT('Ctrl Pts',(3.60121378324409,21.2392419976695,53.1491188072116));
#153138=CARTESIAN_POINT('Ctrl Pts',(3.44985401812235,21.3948988306987,53.2045252912585));
#153139=CARTESIAN_POINT('Ctrl Pts',(3.29935834752775,21.5548974467013,53.2500701259441));
#153140=CARTESIAN_POINT('Ctrl Pts',(3.14931819963736,21.7144117763325,53.2954771047951));
#153141=CARTESIAN_POINT('Ctrl Pts',(3.00013691813682,21.8782416497902,53.331082045352));
#153142=CARTESIAN_POINT('Ctrl Pts',(2.85285330004476,22.0452897893958,53.3565571956255));
#153143=CARTESIAN_POINT('Ctrl Pts',(2.85240650238333,22.0457965444517,53.3566344767088));
#153144=CARTESIAN_POINT('Ctrl Pts',(2.85195972219237,22.0463033291172,53.3567116645701));
#153145=CARTESIAN_POINT('Ctrl Pts',(2.85151295950087,22.0468101433616,53.3567887592001));
#153146=CARTESIAN_POINT('Ctrl Pts',(2.70379463414956,22.2143840094626,53.3822794500264));
#153147=CARTESIAN_POINT('Ctrl Pts',(2.55798942099489,22.3851915508815,53.3975777418528));
#153148=CARTESIAN_POINT('Ctrl Pts',(2.41508772742532,22.5580263962415,53.4026635334286));
#153149=CARTESIAN_POINT('Ctrl Pts',(2.27218603385641,22.7308612416006,53.4077493250044));
#153150=CARTESIAN_POINT('Ctrl Pts',(2.13218785948827,22.905723390667,53.4026226173359));
#153151=CARTESIAN_POINT('Ctrl Pts',(1.99602497078142,23.0813571917986,53.3874847959142));
#153152=CARTESIAN_POINT('Ctrl Pts',(1.72451941585065,23.4315668054,53.3573003407768));
#153153=CARTESIAN_POINT('Ctrl Pts',(1.468262734854,23.7848444098977,53.2873123215654));
#153154=CARTESIAN_POINT('Ctrl Pts',(1.23275780652318,24.13180332306,53.1823069542621));
#153155=CARTESIAN_POINT('Ctrl Pts',(13.2725929185091,20.67124111202,53.96044066964));
#153156=CARTESIAN_POINT('Ctrl Pts',(12.7601005265309,20.7790383531423,54.5170917113046));
#153157=CARTESIAN_POINT('Ctrl Pts',(12.2365830640386,21.0202700835715,55.1059943501782));
#153158=CARTESIAN_POINT('Ctrl Pts',(11.5144024001356,21.6082528697978,55.9578487963725));
#153159=CARTESIAN_POINT('Ctrl Pts',(11.284484943989,21.8411904407848,56.2361257836112));
#153160=CARTESIAN_POINT('Ctrl Pts',(10.8600882151825,22.3745190753888,56.7657768656355));
#153161=CARTESIAN_POINT('Ctrl Pts',(10.6656891171808,22.6748728094781,57.017060721281));
#153162=CARTESIAN_POINT('Ctrl Pts',(10.3235697698876,23.3290339756505,57.4787180816328));
#153163=CARTESIAN_POINT('Ctrl Pts',(10.1759004486617,23.6827440137225,57.6890228698567));
#153164=CARTESIAN_POINT('Ctrl Pts',(9.93366676041426,24.4240678546045,58.0589285287306));
#153165=CARTESIAN_POINT('Ctrl Pts',(9.83910660616593,24.8115576094456,58.2185057763796));
#153166=CARTESIAN_POINT('Ctrl Pts',(9.63618653282326,25.9924390190698,58.6150020729616));
#153167=CARTESIAN_POINT('Ctrl Pts',(9.61024456763422,26.8018116088772,58.7675633910135));
#153168=CARTESIAN_POINT('Ctrl Pts',(9.66896670550909,27.56177023892,58.8232869035));
#153169=CARTESIAN_POINT('Ctrl Pts',(20.3787275855491,19.18666345688,66.379741082483));
#153170=CARTESIAN_POINT('Ctrl Pts',(17.8361393017991,20.29619101201,67.595084209341));
#153171=CARTESIAN_POINT('Ctrl Pts',(16.3981991143491,22.80777792279,68.487957490196));
#153172=CARTESIAN_POINT('Ctrl Pts',(16.5807046766691,25.82061478888,68.738094180426));
#153173=CARTESIAN_POINT('Ctrl Pts',(18.6376929650191,19.57899817903,61.58547060068));
#153174=CARTESIAN_POINT('Ctrl Pts',(16.0482537547891,20.58406629994,63.2181484680071));
#153175=CARTESIAN_POINT('Ctrl Pts',(14.6296236331391,23.17807550392,64.49719057205));
#153176=CARTESIAN_POINT('Ctrl Pts',(14.9395338453091,26.34133394336,64.919770175413));
#153177=CARTESIAN_POINT('Ctrl Pts',(16.2689157983691,20.24291980593,57.34617439044));
#153178=CARTESIAN_POINT('Ctrl Pts',(13.5272592236191,21.02524550693,59.47841963262));
#153179=CARTESIAN_POINT('Ctrl Pts',(12.0834247294191,23.76779590644,61.13994925363));
#153180=CARTESIAN_POINT('Ctrl Pts',(12.5949792953091,27.2217169096,61.57409469908));
#153181=CARTESIAN_POINT('Ctrl Pts',(13.2927090274791,20.66243511217,53.69009205466));
#153182=CARTESIAN_POINT('Ctrl Pts',(10.7176832624191,21.08595805766,56.49475584674));
#153183=CARTESIAN_POINT('Ctrl Pts',(9.21456506056909,23.95986757545,58.53385767307));
#153184=CARTESIAN_POINT('Ctrl Pts',(9.57610311105909,27.76867765135,58.7320035412201));
#153185=CARTESIAN_POINT('Origin',(22.932586701957,25.6803076522557,65.7954246532035));
#153186=CARTESIAN_POINT('Ctrl Pts',(20.8911511744791,19.9604224465,80.848282833327));
#153187=CARTESIAN_POINT('Ctrl Pts',(20.2241964889591,20.13080330299,80.513263521276));
#153188=CARTESIAN_POINT('Ctrl Pts',(18.9283646791091,20.71921193457,79.811448093371));
#153189=CARTESIAN_POINT('Ctrl Pts',(17.3696955150691,22.37067833873,78.780633438867));
#153190=CARTESIAN_POINT('Ctrl Pts',(16.4736258696191,24.54284688986,77.9461870487));
#153191=CARTESIAN_POINT('Ctrl Pts',(16.3978381440991,26.09054287903,77.605843233037));
#153192=CARTESIAN_POINT('Ctrl Pts',(16.4717809815391,26.84345587847,77.490338917542));
#153193=CARTESIAN_POINT('Ctrl Pts',(21.2489006219491,19.77806662564,79.674997080701));
#153194=CARTESIAN_POINT('Ctrl Pts',(20.5800208574191,19.9711851103,79.394482109607));
#153195=CARTESIAN_POINT('Ctrl Pts',(19.2882260173591,20.59194413007,78.806627701594));
#153196=CARTESIAN_POINT('Ctrl Pts',(17.7380604811591,22.23637549275,77.931740551844));
#153197=CARTESIAN_POINT('Ctrl Pts',(16.8323403731591,24.35865510143,77.199951533994));
#153198=CARTESIAN_POINT('Ctrl Pts',(16.7360936623891,25.86678725123,76.878121802014));
#153199=CARTESIAN_POINT('Ctrl Pts',(16.7988664925391,26.60318525589,76.760821350634));
#153200=CARTESIAN_POINT('Ctrl Pts',(21.7404719851691,19.4367501038,77.27768430253));
#153201=CARTESIAN_POINT('Ctrl Pts',(21.0781718769291,19.66719172332,77.10117478113));
#153202=CARTESIAN_POINT('Ctrl Pts',(19.8112633217491,20.33854901363,76.729024104145));
#153203=CARTESIAN_POINT('Ctrl Pts',(18.2922620430691,21.96660458151,76.155867660549));
#153204=CARTESIAN_POINT('Ctrl Pts',(17.3742768987591,24.00382143215,75.643605268245));
#153205=CARTESIAN_POINT('Ctrl Pts',(17.2366271868691,25.44474146273,75.386690727847));
#153206=CARTESIAN_POINT('Ctrl Pts',(17.2748132426991,26.1527308176,75.282273549274));
#153207=CARTESIAN_POINT('Ctrl Pts',(21.8755966897991,19.08135358495,73.526845056723));
#153208=CARTESIAN_POINT('Ctrl Pts',(21.2401175084091,19.34463071198,73.5057660894959));
#153209=CARTESIAN_POINT('Ctrl Pts',(20.0340922790191,20.05757741651,73.4492763332938));
#153210=CARTESIAN_POINT('Ctrl Pts',(18.5849356991691,21.66533371693,73.321641233911));
#153211=CARTESIAN_POINT('Ctrl Pts',(17.6776840505191,23.62313410685,73.1644554192328));
#153212=CARTESIAN_POINT('Ctrl Pts',(17.5011681902691,25.00156958332,73.0521458729575));
#153213=CARTESIAN_POINT('Ctrl Pts',(17.5121252768591,25.6826957763,72.9962696634154));
#153214=CARTESIAN_POINT('Ctrl Pts',(21.4080075944791,18.99041968019,69.698937793342));
#153215=CARTESIAN_POINT('Ctrl Pts',(20.7982638491291,19.26244640202,69.832985568099));
#153216=CARTESIAN_POINT('Ctrl Pts',(19.6465587797891,19.986295941,70.089606824027));
#153217=CARTESIAN_POINT('Ctrl Pts',(18.2728403102091,21.58882896434,70.408052707636));
#153218=CARTESIAN_POINT('Ctrl Pts',(17.4191062600591,23.52613108719,70.621969420302));
#153219=CARTESIAN_POINT('Ctrl Pts',(17.2580474576791,24.88819990756,70.679396362023));
#153220=CARTESIAN_POINT('Ctrl Pts',(17.2722927312391,25.56219068901,70.687933105918));
#153221=CARTESIAN_POINT('Ctrl Pts',(20.6971812658991,19.11140694679,67.205408224001));
#153222=CARTESIAN_POINT('Ctrl Pts',(20.1070383963591,19.37210896923,67.443938609233));
#153223=CARTESIAN_POINT('Ctrl Pts',(18.9924858732291,20.08180195792,67.912437713137));
#153224=CARTESIAN_POINT('Ctrl Pts',(17.6753991076991,21.69114765413,68.5308846882));
#153225=CARTESIAN_POINT('Ctrl Pts',(16.8811751422491,23.65527078503,68.988289141191));
#153226=CARTESIAN_POINT('Ctrl Pts',(16.7590148989391,25.03886729217,69.150951498051));
#153227=CARTESIAN_POINT('Ctrl Pts',(16.7913432132991,25.72230139667,69.197497579931));
#153228=CARTESIAN_POINT('Ctrl Pts',(20.2354688957591,19.21917800851,65.988118467194));
#153229=CARTESIAN_POINT('Ctrl Pts',(19.6554686558991,19.46975735037,66.279674422239));
#153230=CARTESIAN_POINT('Ctrl Pts',(18.5593496213791,20.16661372345,66.85686112244));
#153231=CARTESIAN_POINT('Ctrl Pts',(17.2722126901491,21.78232033032,67.628148426319));
#153232=CARTESIAN_POINT('Ctrl Pts',(16.5143337230091,23.77097449246,68.203940042059));
#153233=CARTESIAN_POINT('Ctrl Pts',(16.4190832870791,25.17355603177,68.411481313033));
#153234=CARTESIAN_POINT('Ctrl Pts',(16.4643772039691,25.86501026269,68.472097080547));
#153235=CARTESIAN_POINT('Ctrl Pts',(-2.42455476507091,16.92552468832,52.4988667111));
#153236=CARTESIAN_POINT('Ctrl Pts',(-2.42455476507091,16.92552468832,52.4988667111));
#153237=CARTESIAN_POINT('Ctrl Pts',(-2.42455476507091,16.92552468832,52.4988667111));
#153238=CARTESIAN_POINT('Ctrl Pts',(-2.42455476507091,16.92552468832,52.4988667111));
#153239=CARTESIAN_POINT('Ctrl Pts',(-1.37593350884091,19.75605503409,52.44644608116));
#153240=CARTESIAN_POINT('Ctrl Pts',(-0.884501579890127,19.39180151254,52.4218793741253));
#153241=CARTESIAN_POINT('Ctrl Pts',(-0.389267231970226,19.03168229686,52.3971225839732));
#153242=CARTESIAN_POINT('Ctrl Pts',(0.110004993249088,18.67552617523,52.37216394013));
#153243=CARTESIAN_POINT('Ctrl Pts',(-0.11447139326091,22.30361770189,52.58018366622));
#153244=CARTESIAN_POINT('Ctrl Pts',(0.887603277609087,21.4786617599,52.8198982923901));
#153245=CARTESIAN_POINT('Ctrl Pts',(1.81796826660909,20.56952055347,52.75185713948));
#153246=CARTESIAN_POINT('Ctrl Pts',(2.62639801664909,19.62528980623,52.37976571339));
#153247=CARTESIAN_POINT('Ctrl Pts',(1.24014776487909,24.40863425477,53.18278579188));
#153248=CARTESIAN_POINT('Ctrl Pts',(2.28602424783909,22.80161860487,53.71749108626));
#153249=CARTESIAN_POINT('Ctrl Pts',(3.58775731907909,21.31467159053,53.48378241936));
#153250=CARTESIAN_POINT('Ctrl Pts',(4.9251348840291,20.1992043079,52.52142955503));
#153251=CARTESIAN_POINT('Origin',(-10.9843331791359,92.,80.581991049076));
#153252=CARTESIAN_POINT('',(1.02913961852909,92.5,53.63896836527));
#153253=CARTESIAN_POINT('Origin',(1.02913961852909,92.,53.63896836527));
#153254=CARTESIAN_POINT('Origin',(-10.9843331791359,92.5,80.581991049076));
#153255=CARTESIAN_POINT('Origin',(-10.9843331791359,92.,65.395787724084));
#153256=CARTESIAN_POINT('',(1.02913961852909,92.5,92.33881040789));
#153257=CARTESIAN_POINT('Origin',(-10.9843331791359,92.5,65.395787724084));
#153258=CARTESIAN_POINT('Origin',(1.02913961852909,92.,92.33881040789));
#153259=CARTESIAN_POINT('Origin',(-2.02513312664091,92.,85.48888938658));
#153260=CARTESIAN_POINT('Origin',(-2.02513312664091,92.5,85.48888938658));
#153261=CARTESIAN_POINT('Origin',(-2.27593483123091,92.5,69.192338555332));
#153262=CARTESIAN_POINT('Origin',(-2.02513312664091,92.5,60.48888938658));
#153263=CARTESIAN_POINT('Origin',(-2.02513312664091,92.,60.48888938658));
#153264=CARTESIAN_POINT('Origin',(20.5162416486691,1.4210854715202E-14,
116.353388269));
#153265=CARTESIAN_POINT('Ctrl Pts',(37.1148577576791,-11.38315600667,64.424614458756));
#153266=CARTESIAN_POINT('Ctrl Pts',(33.3746924839791,-9.55480085092099,
64.424638317428));
#153267=CARTESIAN_POINT('Ctrl Pts',(30.0554397785991,-9.17281283206899,
61.94094919385));
#153268=CARTESIAN_POINT('Ctrl Pts',(28.7731848187491,-10.42324480072,58.18267172033));
#153269=CARTESIAN_POINT('Ctrl Pts',(36.7247317035591,-11.99143530332,64.746736687142));
#153270=CARTESIAN_POINT('Ctrl Pts',(33.0869920335091,-10.11930380944,64.661644695515));
#153271=CARTESIAN_POINT('Ctrl Pts',(29.8376575084291,-9.718933522376,62.2086132886801));
#153272=CARTESIAN_POINT('Ctrl Pts',(28.5145010531591,-10.97987178426,58.54842980974));
#153273=CARTESIAN_POINT('Ctrl Pts',(36.3045657794791,-12.5809663284,65.090039586453));
#153274=CARTESIAN_POINT('Ctrl Pts',(32.7708362104291,-10.68071449823,64.92189605369));
#153275=CARTESIAN_POINT('Ctrl Pts',(29.5952467863491,-10.26284018231,62.50069738269));
#153276=CARTESIAN_POINT('Ctrl Pts',(28.2357619232591,-11.51926368214,58.9379362879));
#153277=CARTESIAN_POINT('Ctrl Pts',(35.8540738479291,-13.15242231248,65.452547555325));
#153278=CARTESIAN_POINT('Ctrl Pts',(32.4235807876891,-11.23800283895,65.206103155874));
#153279=CARTESIAN_POINT('Ctrl Pts',(29.3251926934191,-10.80344668515,62.81749475457));
#153280=CARTESIAN_POINT('Ctrl Pts',(27.9366338055491,-12.04204812536,59.3487279449101));
#153281=CARTESIAN_POINT('',(36.8798279596591,-11.43907953387,64.491475339616));
#153282=CARTESIAN_POINT('Ctrl Pts',(35.8057502945591,-12.95453430026,65.365954576197));
#153283=CARTESIAN_POINT('Ctrl Pts',(36.1860516598291,-12.46249651106,65.059698667609));
#153284=CARTESIAN_POINT('Ctrl Pts',(36.5439947228891,-11.95743270971,64.76779286742));
#153285=CARTESIAN_POINT('Ctrl Pts',(36.8798279596591,-11.43907953387,64.491475339616));
#153286=CARTESIAN_POINT('Ctrl Pts',(36.8798279596681,-11.4390795338486,
64.4914753396672));
#153287=CARTESIAN_POINT('Ctrl Pts',(36.7441750018997,-11.3735279686372,
64.4879383408179));
#153288=CARTESIAN_POINT('Ctrl Pts',(36.6064460983526,-11.3089290560052,
64.4804862516236));
#153289=CARTESIAN_POINT('Ctrl Pts',(36.4669094342276,-11.2455257133135,
64.4689019673217));
#153290=CARTESIAN_POINT('Ctrl Pts',(36.3287823623725,-11.1827628679584,
64.4574347068695));
#153291=CARTESIAN_POINT('Ctrl Pts',(36.1888840383274,-11.1211718375744,
64.4419179324151));
#153292=CARTESIAN_POINT('Ctrl Pts',(36.047515073403,-11.0609928153098,64.4221717313969));
#153293=CARTESIAN_POINT('Ctrl Pts',(35.9080299464162,-11.0016157195872,
64.4026886619836));
#153294=CARTESIAN_POINT('Ctrl Pts',(35.7671133724119,-10.94361353859,64.3790878219158));
#153295=CARTESIAN_POINT('Ctrl Pts',(35.6250904880056,-10.8872172610078,
64.3512315440085));
#153296=CARTESIAN_POINT('Ctrl Pts',(35.4840672423464,-10.8312179328644,
64.3235713346072));
#153297=CARTESIAN_POINT('Ctrl Pts',(35.3419534965111,-10.7768022748865,
64.2917150865606));
#153298=CARTESIAN_POINT('Ctrl Pts',(35.1990996420043,-10.7241923799527,
64.2555674775194));
#153299=CARTESIAN_POINT('Ctrl Pts',(35.0575694076834,-10.6720699448718,
64.2197547961228));
#153300=CARTESIAN_POINT('Ctrl Pts',(34.9153130778802,-10.6217202516276,
64.1797296977471));
#153301=CARTESIAN_POINT('Ctrl Pts',(34.7726981088167,-10.5733509706476,
64.1354420899077));
#153302=CARTESIAN_POINT('Ctrl Pts',(34.6643414532593,-10.5366007364112,
64.101793048018));
#153303=CARTESIAN_POINT('Ctrl Pts',(34.5557783568399,-10.5009936047222,
64.0656842235702));
#153304=CARTESIAN_POINT('Ctrl Pts',(34.4471783750911,-10.4666158673459,
64.0271113390586));
#153305=CARTESIAN_POINT('Ctrl Pts',(34.3077698634826,-10.4224855726357,
63.9775957836081));
#153306=CARTESIAN_POINT('Ctrl Pts',(34.1682336268683,-10.3803607477818,
63.9239944308088));
#153307=CARTESIAN_POINT('Ctrl Pts',(34.0289521150137,-10.3404196067234,
63.8663302586336));
#153308=CARTESIAN_POINT('Ctrl Pts',(33.8903294409197,-10.3006673976459,
63.808938852984));
#153309=CARTESIAN_POINT('Ctrl Pts',(33.7519595460037,-10.2630785115483,
63.7475229310178));
#153310=CARTESIAN_POINT('Ctrl Pts',(33.6142299740126,-10.2278100923352,
63.6821520759947));
#153311=CARTESIAN_POINT('Ctrl Pts',(33.4754483971942,-10.1922722861872,
63.6162819058713));
#153312=CARTESIAN_POINT('Ctrl Pts',(33.3373174532717,-10.1590908011647,
63.5463961017914));
#153313=CARTESIAN_POINT('Ctrl Pts',(33.2002371867619,-10.128403545685,63.4726144903044));
#153314=CARTESIAN_POINT('Ctrl Pts',(33.0652012554393,-10.0981739420452,
63.3999332147619));
#153315=CARTESIAN_POINT('Ctrl Pts',(32.9311853795762,-10.0703648598007,
63.3234716773683));
#153316=CARTESIAN_POINT('Ctrl Pts',(32.7985681278943,-10.0450831627581,
63.2433899608591));
#153317=CARTESIAN_POINT('Ctrl Pts',(32.6629392987228,-10.0192273489339,
63.1614896853637));
#153318=CARTESIAN_POINT('Ctrl Pts',(32.5287739002282,-9.99601527822984,
63.0758029691421));
#153319=CARTESIAN_POINT('Ctrl Pts',(32.3964648510167,-9.97553168804268,
62.9865476599149));
#153320=CARTESIAN_POINT('Ctrl Pts',(32.2641558018052,-9.95504809785552,
62.8972923506877));
#153321=CARTESIAN_POINT('Ctrl Pts',(32.1337036138356,-9.93729309243784,
62.8044687444746));
#153322=CARTESIAN_POINT('Ctrl Pts',(32.0054812102974,-9.92231950953623,
62.7083380847189));
#153323=CARTESIAN_POINT('Ctrl Pts',(31.8803697597832,-9.90770921816341,
62.6145397628262));
#153324=CARTESIAN_POINT('Ctrl Pts',(31.7572899979802,-9.89573625457834,
62.5175247549684));
#153325=CARTESIAN_POINT('Ctrl Pts',(31.6365737639664,-9.88643109912129,
62.4175581834101));
#153326=CARTESIAN_POINT('Ctrl Pts',(31.5157672166093,-9.87711898205128,
62.3175168222813));
#153327=CARTESIAN_POINT('Ctrl Pts',(31.3973281256053,-9.87047867724871,
62.2145198410588));
#153328=CARTESIAN_POINT('Ctrl Pts',(31.2815608813011,-9.86651055480352,
62.1088649167814));
#153329=CARTESIAN_POINT('Ctrl Pts',(31.163210651863,-9.86245389607721,62.0008526322647));
#153330=CARTESIAN_POINT('Ctrl Pts',(31.0476533098122,-9.86119005685629,
61.8900628208581));
#153331=CARTESIAN_POINT('Ctrl Pts',(30.935177785853,-9.8626871641774,61.7768416797537));
#153332=CARTESIAN_POINT('Ctrl Pts',(30.824489314776,-9.86416048490157,61.6654194381735));
#153333=CARTESIAN_POINT('Ctrl Pts',(30.7167856681417,-9.86830752697171,
61.5516430401091));
#153334=CARTESIAN_POINT('Ctrl Pts',(30.6123030211769,-9.87506826147692,
61.4358625684621));
#153335=CARTESIAN_POINT('Ctrl Pts',(30.5052900833844,-9.8819927229263,61.3172782028294));
#153336=CARTESIAN_POINT('Ctrl Pts',(30.4016564107195,-9.89165895151477,
61.1965919844559));
#153337=CARTESIAN_POINT('Ctrl Pts',(30.3016099115775,-9.90397263019706,
61.0741939994848));
#153338=CARTESIAN_POINT('Ctrl Pts',(30.2015634124355,-9.91628630887936,
60.9517960145137));
#153339=CARTESIAN_POINT('Ctrl Pts',(30.1051041820874,-9.93124721616769,
60.8276867937595));
#153340=CARTESIAN_POINT('Ctrl Pts',(30.0123915794226,-9.94873382237174,
60.702262569282));
#153341=CARTESIAN_POINT('Ctrl Pts',(29.9190203204585,-9.96634465832449,
60.5759472959808));
#153342=CARTESIAN_POINT('Ctrl Pts',(29.8294030814699,-9.98652556792445,
60.4482366205373));
#153343=CARTESIAN_POINT('Ctrl Pts',(29.7436578355946,-10.0091373557639,
60.3195209980263));
#153344=CARTESIAN_POINT('Ctrl Pts',(29.6573497459522,-10.0318975705363,
60.1899604681958));
#153345=CARTESIAN_POINT('Ctrl Pts',(29.5749646284969,-10.0571204355003,
60.0593822207725));
#153346=CARTESIAN_POINT('Ctrl Pts',(29.4965744788422,-10.0846437655168,
59.9281770342848));
#153347=CARTESIAN_POINT('Ctrl Pts',(29.4172168052186,-10.1125067999684,
59.7953524585837));
#153348=CARTESIAN_POINT('Ctrl Pts',(29.3419532620603,-10.1427271751237,
59.6618858288828));
#153349=CARTESIAN_POINT('Ctrl Pts',(29.270809736117,-10.1751197943674,59.5281679608396));
#153350=CARTESIAN_POINT('Ctrl Pts',(29.1991491694168,-10.2077478293309,
59.3934782884501));
#153351=CARTESIAN_POINT('Ctrl Pts',(29.1316685385326,-10.2425795025469,
59.2585341137898));
#153352=CARTESIAN_POINT('Ctrl Pts',(29.0683470046054,-10.2794129266527,
59.1237135976406));
#153353=CARTESIAN_POINT('Ctrl Pts',(29.0041776407885,-10.3167395238698,
58.9870879315487));
#153354=CARTESIAN_POINT('Ctrl Pts',(28.9442792778791,-10.3561215368744,
58.8505896339998));
#153355=CARTESIAN_POINT('Ctrl Pts',(28.8885848131186,-10.3973403349861,
58.7145845665897));
#153356=CARTESIAN_POINT('Ctrl Pts',(28.8470986002056,-10.4280437781709,
58.6132758421396));
#153357=CARTESIAN_POINT('Ctrl Pts',(28.8079439853351,-10.4597661809439,
58.5122402265492));
#153358=CARTESIAN_POINT('Ctrl Pts',(28.7710784579419,-10.4924156480374,
58.4116174733487));
#153359=CARTESIAN_POINT('Ctrl Pts',(28.6318099234291,-10.68337721174,58.2360960239));
#153360=CARTESIAN_POINT('Ctrl Pts',(28.9036687620591,-10.40410957799,59.04777775718));
#153361=CARTESIAN_POINT('Ctrl Pts',(29.7282443214291,-9.97887814526099,
60.69655454236));
#153362=CARTESIAN_POINT('Ctrl Pts',(31.8102465520291,-9.94192586985999,
62.86109705332));
#153363=CARTESIAN_POINT('Ctrl Pts',(34.3891486420691,-10.55131574029,64.279269257528));
#153364=CARTESIAN_POINT('Ctrl Pts',(36.1064545847691,-11.2894506228,64.582977897741));
#153365=CARTESIAN_POINT('Ctrl Pts',(36.9086854560691,-11.70132943018,64.595573649679));
#153366=CARTESIAN_POINT('Ctrl Pts',(29.0456292725091,-10.01132377404,58.37055718011));
#153367=CARTESIAN_POINT('Ctrl Pts',(29.3498254657591,-9.77458649748099,
59.16172491632));
#153368=CARTESIAN_POINT('Ctrl Pts',(30.2325487222691,-9.41554285765999,
60.73612952655));
#153369=CARTESIAN_POINT('Ctrl Pts',(32.3627339107191,-9.37345866626899,
62.71704601845));
#153370=CARTESIAN_POINT('Ctrl Pts',(34.9609073760491,-9.86290539232099,
63.941641260975));
#153371=CARTESIAN_POINT('Ctrl Pts',(36.6922503471391,-10.4709131891,64.141295131879));
#153372=CARTESIAN_POINT('Ctrl Pts',(37.5052929747491,-10.81476301663,64.108748322606));
#153373=CARTESIAN_POINT('Ctrl Pts',(29.8074106496591,-8.60875283793899,
58.64000348532));
#153374=CARTESIAN_POINT('Ctrl Pts',(30.1723381639891,-8.44024965538699,
59.37231809656));
#153375=CARTESIAN_POINT('Ctrl Pts',(31.1487519819791,-8.18096902990299,
60.77590041796));
#153376=CARTESIAN_POINT('Ctrl Pts',(33.3031956985291,-8.10811512607799,
62.41397188693));
#153377=CARTESIAN_POINT('Ctrl Pts',(35.8461147163691,-8.37510901302899,
63.319546372377));
#153378=CARTESIAN_POINT('Ctrl Pts',(37.5408772930491,-8.74778122122199,
63.36692565601));
#153379=CARTESIAN_POINT('Ctrl Pts',(38.3453292531191,-8.96717590778899,
63.271322697011));
#153380=CARTESIAN_POINT('Ctrl Pts',(30.7659404102391,-6.12843955931699,
59.02640618789));
#153381=CARTESIAN_POINT('Ctrl Pts',(31.1943400875191,-6.03067355048699,
59.64444010852));
#153382=CARTESIAN_POINT('Ctrl Pts',(32.2374024575391,-5.86859656993499,
60.77872899668));
#153383=CARTESIAN_POINT('Ctrl Pts',(34.2962640644291,-5.75551569888499,
61.99917441976));
#153384=CARTESIAN_POINT('Ctrl Pts',(36.6198739262991,-5.78832739818299,
62.58745827192));
#153385=CARTESIAN_POINT('Ctrl Pts',(38.1639558208391,-5.90433866667599,
62.52263971893));
#153386=CARTESIAN_POINT('Ctrl Pts',(38.9069661676791,-5.98184811597299,
62.3893519671));
#153387=CARTESIAN_POINT('Ctrl Pts',(31.4628040362191,-3.27451591220699,
59.34145203332));
#153388=CARTESIAN_POINT('Ctrl Pts',(31.9148547160891,-3.22399603912999,
59.85552151593));
#153389=CARTESIAN_POINT('Ctrl Pts',(32.9537808151091,-3.13354949579399,
60.77329930901));
#153390=CARTESIAN_POINT('Ctrl Pts',(34.8624033916191,-3.03865186609699,
61.7164874873));
#153391=CARTESIAN_POINT('Ctrl Pts',(36.9515785646591,-2.99298517160899,
62.13709043757));
#153392=CARTESIAN_POINT('Ctrl Pts',(38.3374590596191,-2.99798405108899,
62.04637567703));
#153393=CARTESIAN_POINT('Ctrl Pts',(39.0114873686691,-3.00876121641099,
61.9161681279));
#153394=CARTESIAN_POINT('Ctrl Pts',(31.6941891349691,-0.559164177511486,
59.45203956376));
#153395=CARTESIAN_POINT('Ctrl Pts',(32.1483274996991,-0.550463064146686,
59.929061278));
#153396=CARTESIAN_POINT('Ctrl Pts',(33.1744137845191,-0.534881944430286,
60.77391018355));
#153397=CARTESIAN_POINT('Ctrl Pts',(35.0195538481991,-0.518480218034586,
61.63166634532));
#153398=CARTESIAN_POINT('Ctrl Pts',(37.0205148723291,-0.510451987175386,
62.00677298972));
#153399=CARTESIAN_POINT('Ctrl Pts',(38.3472726057891,-0.511094758103086,
61.91535197825));
#153400=CARTESIAN_POINT('Ctrl Pts',(38.9948370647791,-0.512805555018386,
61.79060918495));
#153401=CARTESIAN_POINT('Ctrl Pts',(31.6030449881391,1.63342335677401,59.40849392115));
#153402=CARTESIAN_POINT('Ctrl Pts',(32.0562402583091,1.60809110369101,59.90010929421));
#153403=CARTESIAN_POINT('Ctrl Pts',(33.0871862210291,1.56273341258401,60.77377016236));
#153404=CARTESIAN_POINT('Ctrl Pts',(34.9572779373091,1.51505187528801,61.66534608043));
#153405=CARTESIAN_POINT('Ctrl Pts',(36.9930942606091,1.49187208211601,62.05839402226));
#153406=CARTESIAN_POINT('Ctrl Pts',(38.3431995755691,1.49399892537301,61.96714783356));
#153407=CARTESIAN_POINT('Ctrl Pts',(39.0011940413591,1.49914916427001,61.84019219338));
#153408=CARTESIAN_POINT('Ctrl Pts',(31.3474186477091,3.74625791698601,59.28928090803));
#153409=CARTESIAN_POINT('Ctrl Pts',(31.7956253642391,3.68797075177601,59.82056228684));
#153410=CARTESIAN_POINT('Ctrl Pts',(32.8353535505091,3.58576207768401,60.77413589135));
#153411=CARTESIAN_POINT('Ctrl Pts',(34.7688811807491,3.48797809126401,61.76313013829));
#153412=CARTESIAN_POINT('Ctrl Pts',(36.8968037579091,3.45543334845601,62.21148594642));
#153413=CARTESIAN_POINT('Ctrl Pts',(38.3088386424591,3.47892537809701,62.12512240935));
#153414=CARTESIAN_POINT('Ctrl Pts',(38.9942825908291,3.50082164918001,61.99444197964));
#153415=CARTESIAN_POINT('Ctrl Pts',(30.7683829701991,6.12095524445701,59.02743346636));
#153416=CARTESIAN_POINT('Ctrl Pts',(31.1968671386991,6.02337634604401,59.64515039934));
#153417=CARTESIAN_POINT('Ctrl Pts',(32.2399479399591,5.86157111726001,60.77875998162));
#153418=CARTESIAN_POINT('Ctrl Pts',(34.2984250721691,5.74848170063101,61.99825790957));
#153419=CARTESIAN_POINT('Ctrl Pts',(36.6214127992191,5.78083057602201,62.58585616545));
#153420=CARTESIAN_POINT('Ctrl Pts',(38.1650763376391,5.89625980071201,62.52080797117));
#153421=CARTESIAN_POINT('Ctrl Pts',(38.9079073284191,5.97342694265101,62.3874504358));
#153422=CARTESIAN_POINT('Ctrl Pts',(29.8089157326691,8.60405889048601,58.64067146398));
#153423=CARTESIAN_POINT('Ctrl Pts',(30.1740149579691,8.43552829169101,59.37277486795));
#153424=CARTESIAN_POINT('Ctrl Pts',(31.1506497978491,8.17616183997101,60.77583536541));
#153425=CARTESIAN_POINT('Ctrl Pts',(33.3049462375891,8.10299652459701,62.41308396893));
#153426=CARTESIAN_POINT('Ctrl Pts',(35.8473775190891,8.36951394256301,63.318103430771));
#153427=CARTESIAN_POINT('Ctrl Pts',(37.5417814200891,8.74184941723802,63.365377186793));
#153428=CARTESIAN_POINT('Ctrl Pts',(38.3460819705591,8.96109715611501,63.269768790418));
#153429=CARTESIAN_POINT('Ctrl Pts',(29.0444408655791,10.01352551446,58.37014632461));
#153430=CARTESIAN_POINT('Ctrl Pts',(29.3485833929991,9.77666292162801,59.16139737026));
#153431=CARTESIAN_POINT('Ctrl Pts',(30.2312412513191,9.41739555567501,60.73602919927));
#153432=CARTESIAN_POINT('Ctrl Pts',(32.3614928437391,9.37516348482501,62.71737336154));
#153433=CARTESIAN_POINT('Ctrl Pts',(34.9598381149091,9.86469977852602,63.942339691534));
#153434=CARTESIAN_POINT('Ctrl Pts',(36.6912888370791,10.47289336349,64.142147541472));
#153435=CARTESIAN_POINT('Ctrl Pts',(37.5043705412191,10.81685010051,64.10965815328));
#153436=CARTESIAN_POINT('Ctrl Pts',(28.6314686688091,10.68390667014,58.23598693286));
#153437=CARTESIAN_POINT('Ctrl Pts',(28.9032909729591,10.40460748413,59.04768337326));
#153438=CARTESIAN_POINT('Ctrl Pts',(29.7277959815891,9.97933481861901,60.69652425927));
#153439=CARTESIAN_POINT('Ctrl Pts',(31.8097200738291,9.94243017287101,62.86124366858));
#153440=CARTESIAN_POINT('Ctrl Pts',(34.3885675638091,10.55197967391,64.279613731913));
#153441=CARTESIAN_POINT('Ctrl Pts',(36.1058374833391,11.29026451401,64.583435617639));
#153442=CARTESIAN_POINT('Ctrl Pts',(36.9080477180991,11.70221929791,64.596082014895));
#153443=CARTESIAN_POINT('',(36.8798265045291,11.43907883074,64.491475301679));
#153444=CARTESIAN_POINT('Ctrl Pts',(36.8798279595137,-11.4390795342153,
64.4914753387916));
#153445=CARTESIAN_POINT('Ctrl Pts',(37.0098305129696,-11.2382074865074,
64.3844217348773));
#153446=CARTESIAN_POINT('Ctrl Pts',(37.1330559421466,-11.032180459589,64.2791469343491));
#153447=CARTESIAN_POINT('Ctrl Pts',(37.2495510317378,-10.8209394872084,
64.1758610837496));
#153448=CARTESIAN_POINT('Ctrl Pts',(37.3649491417382,-10.6116876719354,
64.0735478275362));
#153449=CARTESIAN_POINT('Ctrl Pts',(37.4737424415873,-10.3973193963561,
63.9731862588846));
#153450=CARTESIAN_POINT('Ctrl Pts',(37.5759730006416,-10.1778039241941,
63.8750238873));
#153451=CARTESIAN_POINT('Ctrl Pts',(37.6761385330716,-9.96272259871627,
63.7788443661731));
#153452=CARTESIAN_POINT('Ctrl Pts',(37.7700032180155,-9.74269975563697,
63.684776174574));
#153453=CARTESIAN_POINT('Ctrl Pts',(37.857612056372,-9.51773506712692,63.5930929761144));
#153454=CARTESIAN_POINT('Ctrl Pts',(37.8719863351407,-9.4808243489116,63.5780502032871));
#153455=CARTESIAN_POINT('Ctrl Pts',(37.8861922287029,-9.44378066252948,
63.5630717240933));
#153456=CARTESIAN_POINT('Ctrl Pts',(37.9002299660476,-9.40660408663557,
63.5481588530175));
#153457=CARTESIAN_POINT('Ctrl Pts',(37.9733622814116,-9.21292550399318,
63.4704673587465));
#153458=CARTESIAN_POINT('Ctrl Pts',(38.041938023627,-9.01564124523459,63.3945535346591));
#153459=CARTESIAN_POINT('Ctrl Pts',(38.1059762093653,-8.81469346733212,
63.3205966744608));
#153460=CARTESIAN_POINT('Ctrl Pts',(38.1623696876838,-8.63773429796041,
63.2554685865234));
#153461=CARTESIAN_POINT('Ctrl Pts',(38.2152438827478,-8.45793386216728,
63.1918586472492));
#153462=CARTESIAN_POINT('Ctrl Pts',(38.264633349399,-8.27532061150791,63.1298994651875));
#153463=CARTESIAN_POINT('Ctrl Pts',(38.3173704373835,-8.08032982257757,
63.0637406856462));
#153464=CARTESIAN_POINT('Ctrl Pts',(38.3661269542761,-7.88211198822048,
62.9994587855359));
#153465=CARTESIAN_POINT('Ctrl Pts',(38.4109334817639,-7.68066015104794,
62.9372275318957));
#153466=CARTESIAN_POINT('Ctrl Pts',(38.4333367455077,-7.57993423246166,
62.9061119050756));
#153467=CARTESIAN_POINT('Ctrl Pts',(38.45475257401,-7.47839970899487,62.875509289796));
#153468=CARTESIAN_POINT('Ctrl Pts',(38.475185232764,-7.37605590671984,62.8454438875471));
#153469=CARTESIAN_POINT('Ctrl Pts',(38.485401562141,-7.32488400558233,62.8304111864227));
#153470=CARTESIAN_POINT('Ctrl Pts',(38.495372103593,-7.273509779017,62.8155128136895));
#153471=CARTESIAN_POINT('Ctrl Pts',(38.5050974197184,-7.22193313447018,
62.8007519582672));
#153472=CARTESIAN_POINT('Ctrl Pts',(38.5099600777811,-7.19614481219677,
62.7933715305561));
#153473=CARTESIAN_POINT('Ctrl Pts',(38.5147614298181,-7.17030588510649,
62.7860254838728));
#153474=CARTESIAN_POINT('Ctrl Pts',(38.5195015481513,-7.14441634262704,
62.7787142279474));
#153475=CARTESIAN_POINT('Ctrl Pts',(38.5232683013994,-7.12384311821073,
62.7729043103315));
#153476=CARTESIAN_POINT('Ctrl Pts',(38.5267948165354,-7.10436051932523,
62.7674306943907));
#153477=CARTESIAN_POINT('Ctrl Pts',(38.5305622170623,-7.08329247922146,
62.7615438485301));
#153478=CARTESIAN_POINT('Ctrl Pts',(38.5315357494103,-7.07784829604959,
62.760022631226));
#153479=CARTESIAN_POINT('Ctrl Pts',(38.5325251554163,-7.07229818822057,
62.758473968008));
#153480=CARTESIAN_POINT('Ctrl Pts',(38.5335382756798,-7.06659585814249,
62.7568852495087));
#153481=CARTESIAN_POINT('Ctrl Pts',(38.5648627577464,-6.89028654648589,
62.707763949759));
#153482=CARTESIAN_POINT('Ctrl Pts',(38.5938540547229,-6.70862617273319,
62.6594277140837));
#153483=CARTESIAN_POINT('Ctrl Pts',(38.6205403121146,-6.52158307912809,
62.6121931288261));
#153484=CARTESIAN_POINT('Ctrl Pts',(38.6467448942024,-6.33791603176428,
62.5658111072261));
#153485=CARTESIAN_POINT('Ctrl Pts',(38.6707265414135,-6.14905802435774,
62.5204908743574));
#153486=CARTESIAN_POINT('Ctrl Pts',(38.6925239461544,-5.95500045380756,
62.476574435171));
#153487=CARTESIAN_POINT('Ctrl Pts',(38.7044688916416,-5.84865719280242,
62.4525082915954));
#153488=CARTESIAN_POINT('Ctrl Pts',(38.7157577867499,-5.74075329648307,
62.4288648219717));
#153489=CARTESIAN_POINT('Ctrl Pts',(38.726426943577,-5.63126269288935,62.4056808771417));
#153490=CARTESIAN_POINT('Ctrl Pts',(38.742129208159,-5.47012058440449,62.371560051881));
#153491=CARTESIAN_POINT('Ctrl Pts',(38.7564526971244,-5.30557682948906,
62.3384478461317));
#153492=CARTESIAN_POINT('Ctrl Pts',(38.7694094634675,-5.13762681718977,
62.306498937974));
#153493=CARTESIAN_POINT('Ctrl Pts',(38.7770673484422,-5.03836270748577,
62.2876160579976));
#153494=CARTESIAN_POINT('Ctrl Pts',(38.7842487191847,-4.93790890283837,
62.2691395020168));
#153495=CARTESIAN_POINT('Ctrl Pts',(38.7909645338487,-4.83626607811927,
62.2511007189063));
#153496=CARTESIAN_POINT('Ctrl Pts',(38.8000038559376,-4.69945732495441,
62.2268209585515));
#153497=CARTESIAN_POINT('Ctrl Pts',(38.8081938994977,-4.56049375710199,
62.2033351283924));
#153498=CARTESIAN_POINT('Ctrl Pts',(38.8155488598102,-4.41937717082027,
62.1807237168028));
#153499=CARTESIAN_POINT('Ctrl Pts',(38.8192263399665,-4.3488188776794,62.1694180110079));
#153500=CARTESIAN_POINT('Ctrl Pts',(38.8226950540342,-4.27772232198402,
62.1583309366808));
#153501=CARTESIAN_POINT('Ctrl Pts',(38.8259568116944,-4.20608794889965,
62.1474727558722));
#153502=CARTESIAN_POINT('Ctrl Pts',(38.8275876905245,-4.17027076235747,
62.1420436654678));
#153503=CARTESIAN_POINT('Ctrl Pts',(38.829166830545,-4.13431912091543,62.1366718001178));
#153504=CARTESIAN_POINT('Ctrl Pts',(38.8306944599535,-4.09823308540843,
62.1313584539612));
#153505=CARTESIAN_POINT('Ctrl Pts',(38.8314582746578,-4.08019006765494,
62.1287017808829));
#153506=CARTESIAN_POINT('Ctrl Pts',(38.8322092117279,-4.0621134513515,62.1260597377108));
#153507=CARTESIAN_POINT('Ctrl Pts',(38.8329472998241,-4.04400324484754,
62.1234324869897));
#153508=CARTESIAN_POINT('Ctrl Pts',(38.8333163438723,-4.03494814159556,
62.1221188616292));
#153509=CARTESIAN_POINT('Ctrl Pts',(38.8336821756781,-4.02588464079131,
62.1208089343882));
#153510=CARTESIAN_POINT('Ctrl Pts',(38.8340447988329,-4.01681274352909,
62.1195027256339));
#153511=CARTESIAN_POINT('Ctrl Pts',(38.8344074219876,-4.00774084626686,
62.1181965168797));
#153512=CARTESIAN_POINT('Ctrl Pts',(38.8348372704066,-3.99686343020025,
62.1166372222354));
#153513=CARTESIAN_POINT('Ctrl Pts',(38.83512304594,-3.9895718634735,62.1155952752285));
#153514=CARTESIAN_POINT('Ctrl Pts',(38.83987727857,-3.86826755149894,62.0982611864758));
#153515=CARTESIAN_POINT('Ctrl Pts',(38.8441419459198,-3.74026219392216,
62.0808688446545));
#153516=CARTESIAN_POINT('Ctrl Pts',(38.8479129797729,-3.60554370191226,
62.0636772334747));
#153517=CARTESIAN_POINT('Ctrl Pts',(38.8514022624339,-3.48089064479584,
62.0477700862202));
#153518=CARTESIAN_POINT('Ctrl Pts',(38.854468577654,-3.3504900244013,62.0320351127797));
#153519=CARTESIAN_POINT('Ctrl Pts',(38.8571515577449,-3.21433521685374,
62.0166888938196));
#153520=CARTESIAN_POINT('Ctrl Pts',(38.8585208767362,-3.14484556079837,
62.0088566072004));
#153521=CARTESIAN_POINT('Ctrl Pts',(38.8597910854502,-3.07385711093731,
62.0011257453176));
#153522=CARTESIAN_POINT('Ctrl Pts',(38.8609727143632,-3.00136944360957,
61.993526002045));
#153523=CARTESIAN_POINT('Ctrl Pts',(38.8635089936615,-2.84578001278042,
61.9772137137095));
#153524=CARTESIAN_POINT('Ctrl Pts',(38.8656351315966,-2.68328395752332,
61.9615038043529));
#153525=CARTESIAN_POINT('Ctrl Pts',(38.8673988961025,-2.51385124300707,
61.9467287260682));
#153526=CARTESIAN_POINT('Ctrl Pts',(38.8681573266244,-2.44099404371637,
61.9403753436875));
#153527=CARTESIAN_POINT('Ctrl Pts',(38.8688493000898,-2.3668541654991,61.9341951035091));
#153528=CARTESIAN_POINT('Ctrl Pts',(38.8694813648467,-2.29142901485335,
61.9282157050522));
#153529=CARTESIAN_POINT('Ctrl Pts',(38.8708760369027,-2.125000893707,61.9150219620867));
#153530=CARTESIAN_POINT('Ctrl Pts',(38.8719833550435,-1.95232991211532,
61.9028050003795));
#153531=CARTESIAN_POINT('Ctrl Pts',(38.8728321120811,-1.77342523308076,
61.8918890344145));
#153532=CARTESIAN_POINT('Ctrl Pts',(38.8736321201952,-1.60479606296729,
61.881600034196));
#153533=CARTESIAN_POINT('Ctrl Pts',(38.87420235681,-1.43062871772306,61.8724670776073));
#153534=CARTESIAN_POINT('Ctrl Pts',(38.8746155555018,-1.2509307177607,61.8647716416033));
#153535=CARTESIAN_POINT('Ctrl Pts',(38.8746407339857,-1.23998072375628,
61.8643027160831));
#153536=CARTESIAN_POINT('Ctrl Pts',(38.8746653453594,-1.22901019357011,
61.863839130996));
#153537=CARTESIAN_POINT('Ctrl Pts',(38.8746894124171,-1.21801912886532,
61.8633809510676));
#153538=CARTESIAN_POINT('Ctrl Pts',(38.8750698351621,-1.04428576062759,
61.8561386006349));
#153539=CARTESIAN_POINT('Ctrl Pts',(38.8752990052889,-0.865423956850033,
61.8502483396648));
#153540=CARTESIAN_POINT('Ctrl Pts',(38.8754222231277,-0.681454298511442,
61.8459818319775));
#153541=CARTESIAN_POINT('Ctrl Pts',(38.8754347267326,-0.662785865894718,
61.8455488855232));
#153542=CARTESIAN_POINT('Ctrl Pts',(38.8754461835269,-0.644064836495899,
61.8451326637247));
#153543=CARTESIAN_POINT('Ctrl Pts',(38.8754566711061,-0.625291232005114,
61.8447334533453));
#153544=CARTESIAN_POINT('Ctrl Pts',(38.875524466503,-0.503932056618734,
61.8421528171939));
#153545=CARTESIAN_POINT('Ctrl Pts',(38.8755516014932,-0.380917881018939,
61.8402903434325));
#153546=CARTESIAN_POINT('Ctrl Pts',(38.8755477611405,-0.255289580951591,
61.8392102481073));
#153547=CARTESIAN_POINT('Ctrl Pts',(38.8755452828126,-0.174216784067554,
61.8385132208542));
#153548=CARTESIAN_POINT('Ctrl Pts',(38.8755300542589,-0.0920552103720104,
61.8381429881062));
#153549=CARTESIAN_POINT('Ctrl Pts',(38.8755077513205,-0.00854601869039584,
61.8381279487094));
#153550=CARTESIAN_POINT('Ctrl Pts',(38.875506582961,-0.00417131427553062,
61.838127160857));
#153551=CARTESIAN_POINT('Ctrl Pts',(38.8755053959128,0.000207088582348095,
61.8381273498256));
#153552=CARTESIAN_POINT('Ctrl Pts',(38.8755041868924,0.00458922532672068,
61.8381285210023));
#153553=CARTESIAN_POINT('Ctrl Pts',(38.8754551810142,0.182212749011649,
61.8381759929426));
#153554=CARTESIAN_POINT('Ctrl Pts',(38.8754435586669,0.355643354741394,
61.8398207203825));
#153555=CARTESIAN_POINT('Ctrl Pts',(38.8753693043867,0.524797406056961,
61.842849969035));
#153556=CARTESIAN_POINT('Ctrl Pts',(38.8752921578751,0.70054006989275,61.8459972080368));
#153557=CARTESIAN_POINT('Ctrl Pts',(38.8751474499859,0.871666670567132,
61.8506388441163));
#153558=CARTESIAN_POINT('Ctrl Pts',(38.8748656192459,1.03812127927734,61.856545897734));
#153559=CARTESIAN_POINT('Ctrl Pts',(38.8745997571531,1.19514450039705,61.8621182552288));
#153560=CARTESIAN_POINT('Ctrl Pts',(38.8742124586965,1.34801070455855,61.8688167552262));
#153561=CARTESIAN_POINT('Ctrl Pts',(38.8736767940754,1.4967002041647,61.8764574414583));
#153562=CARTESIAN_POINT('Ctrl Pts',(38.8730494572866,1.6708360151668,61.8854057336857));
#153563=CARTESIAN_POINT('Ctrl Pts',(38.8722176733478,1.83924498920277,61.8956455149775));
#153564=CARTESIAN_POINT('Ctrl Pts',(38.8711772778275,2.00200098431962,61.9068852202791));
#153565=CARTESIAN_POINT('Ctrl Pts',(38.8705113478883,2.10617683649829,61.9140794614326));
#153566=CARTESIAN_POINT('Ctrl Pts',(38.8697610056539,2.20803694311787,61.9216837821204));
#153567=CARTESIAN_POINT('Ctrl Pts',(38.868935031263,2.30760310302302,61.9296261375732));
#153568=CARTESIAN_POINT('Ctrl Pts',(38.8675127054407,2.47905577977653,61.9433028536724));
#153569=CARTESIAN_POINT('Ctrl Pts',(38.8657829944992,2.64360896180348,61.9579874501031));
#153570=CARTESIAN_POINT('Ctrl Pts',(38.8636834250032,2.80126596185201,61.9733446717352));
#153571=CARTESIAN_POINT('Ctrl Pts',(38.8628086667356,2.86695169624411,61.979743057984));
#153572=CARTESIAN_POINT('Ctrl Pts',(38.8618702826237,2.93144046537901,61.9862584852745));
#153573=CARTESIAN_POINT('Ctrl Pts',(38.8608660096394,2.9947329449184,61.9928679340296));
#153574=CARTESIAN_POINT('Ctrl Pts',(38.859611295864,3.07380900012709,62.0011256154865));
#153575=CARTESIAN_POINT('Ctrl Pts',(38.8582534042406,3.15101777476518,62.0095300980127));
#153576=CARTESIAN_POINT('Ctrl Pts',(38.8567796333586,3.22636338050231,62.0180418815993));
#153577=CARTESIAN_POINT('Ctrl Pts',(38.8540373162935,3.36656260882913,62.0338801707583));
#153578=CARTESIAN_POINT('Ctrl Pts',(38.8509044609947,3.50030572704103,62.0500863045402));
#153579=CARTESIAN_POINT('Ctrl Pts',(38.8473375827046,3.62760922988561,62.0664136645151));
#153580=CARTESIAN_POINT('Ctrl Pts',(38.8455541435595,3.6912609813079,62.0745773445025));
#153581=CARTESIAN_POINT('Ctrl Pts',(38.8436622557374,3.75330289609045,62.0827716535668));
#153582=CARTESIAN_POINT('Ctrl Pts',(38.8416568331374,3.81373738325631,62.09096774022));
#153583=CARTESIAN_POINT('Ctrl Pts',(38.8406541218374,3.84395462683924,62.0950657835467));
#153584=CARTESIAN_POINT('Ctrl Pts',(38.8396230304044,3.873770010651,62.099164291412));
#153585=CARTESIAN_POINT('Ctrl Pts',(38.8385629455729,3.90318385970171,62.103259784658));
#153586=CARTESIAN_POINT('Ctrl Pts',(38.8380329031572,3.91789078422705,62.1053075312811));
#153587=CARTESIAN_POINT('Ctrl Pts',(38.8374956126186,3.93249732489038,62.1073545255331));
#153588=CARTESIAN_POINT('Ctrl Pts',(38.8369509986835,3.94700352213919,62.1094003403576));
#153589=CARTESIAN_POINT('Ctrl Pts',(38.8366786917159,3.9542566207636,62.1104232477698));
#153590=CARTESIAN_POINT('Ctrl Pts',(38.8364045539135,3.96148463352306,62.1114458604058));
#153591=CARTESIAN_POINT('Ctrl Pts',(38.8361285759556,3.96868756554229,62.112468125386));
#153592=CARTESIAN_POINT('Ctrl Pts',(38.8358525979978,3.97589049756151,62.1134903903662));
#153593=CARTESIAN_POINT('Ctrl Pts',(38.8356492511492,3.98116367204593,62.1142402930151));
#153594=CARTESIAN_POINT('Ctrl Pts',(38.8352951123537,3.99022112449758,62.1155338248086));
#153595=CARTESIAN_POINT('Ctrl Pts',(38.8285328412474,4.16317294389909,62.1402337808219));
#153596=CARTESIAN_POINT('Ctrl Pts',(38.8206410998247,4.33311250091768,62.1662914189214));
#153597=CARTESIAN_POINT('Ctrl Pts',(38.8115378492565,4.50003137234844,62.1935808853104));
#153598=CARTESIAN_POINT('Ctrl Pts',(38.8023180837981,4.66908668216695,62.2212196367328));
#153599=CARTESIAN_POINT('Ctrl Pts',(38.7918557192814,4.83504340502254,62.2501218691348));
#153600=CARTESIAN_POINT('Ctrl Pts',(38.7801187157006,4.99789823554354,62.2801498303958));
#153601=CARTESIAN_POINT('Ctrl Pts',(38.7681210309875,5.1643701035261,62.3108447185169));
#153602=CARTESIAN_POINT('Ctrl Pts',(38.7547915533566,5.32760067385293,62.3427158038281));
#153603=CARTESIAN_POINT('Ctrl Pts',(38.7401497505278,5.48759338691093,62.3756100036374));
#153604=CARTESIAN_POINT('Ctrl Pts',(38.7358564036623,5.53450729643028,62.3852554148819));
#153605=CARTESIAN_POINT('Ctrl Pts',(38.7314505608984,5.58114286099023,62.3949887615589));
#153606=CARTESIAN_POINT('Ctrl Pts',(38.7269335390551,5.62750029347685,62.4048061087723));
#153607=CARTESIAN_POINT('Ctrl Pts',(38.7163775057703,5.73583508071256,62.4277487128928));
#153608=CARTESIAN_POINT('Ctrl Pts',(38.7052028854674,5.84263827108527,62.4511494917308));
#153609=CARTESIAN_POINT('Ctrl Pts',(38.693382204351,5.94793326722577,62.4749706034504));
#153610=CARTESIAN_POINT('Ctrl Pts',(38.6772800292229,6.09136649677287,62.5074198091162));
#153611=CARTESIAN_POINT('Ctrl Pts',(38.6599794071874,6.23199997192202,62.5406479392232));
#153612=CARTESIAN_POINT('Ctrl Pts',(38.6414863883519,6.36981442588874,62.5745062423265));
#153613=CARTESIAN_POINT('Ctrl Pts',(38.6254519736731,6.48930676639268,62.6038631622058));
#153614=CARTESIAN_POINT('Ctrl Pts',(38.6085106387425,6.60669129998388,62.6336983904886));
#153615=CARTESIAN_POINT('Ctrl Pts',(38.5906480604823,6.72197766351148,62.6639307691723));
#153616=CARTESIAN_POINT('Ctrl Pts',(38.5817167713523,6.77962084527528,62.6790469585141));
#153617=CARTESIAN_POINT('Ctrl Pts',(38.5725551888408,6.83673946970737,62.694262535642));
#153618=CARTESIAN_POINT('Ctrl Pts',(38.5631616284874,6.89333483604516,62.7095679634777));
#153619=CARTESIAN_POINT('Ctrl Pts',(38.5584648483107,6.92163251921405,62.7172206773955));
#153620=CARTESIAN_POINT('Ctrl Pts',(38.5537100746504,6.94979938687568,62.7248958595933));
#153621=CARTESIAN_POINT('Ctrl Pts',(38.5488971028194,6.97783560032803,62.7325923515764));
#153622=CARTESIAN_POINT('Ctrl Pts',(38.5450906465819,7.00000872398614,62.7386793101011));
#153623=CARTESIAN_POINT('Ctrl Pts',(38.541055129008,7.02319790002491,62.7450838174653));
#153624=CARTESIAN_POINT('Ctrl Pts',(38.5372469778334,7.04479846112864,62.75108392236));
#153625=CARTESIAN_POINT('Ctrl Pts',(38.5362400140591,7.05051015206178,62.7526704896978));
#153626=CARTESIAN_POINT('Ctrl Pts',(38.5352491794564,7.0561108238743,62.7542286171872));
#153627=CARTESIAN_POINT('Ctrl Pts',(38.534283391879,7.06155243825886,62.7557446198548));
#153628=CARTESIAN_POINT('Ctrl Pts',(38.4950678675933,7.28250761105259,62.8173014681913));
#153629=CARTESIAN_POINT('Ctrl Pts',(38.4514677808959,7.49993410311113,62.8814236534411));
#153630=CARTESIAN_POINT('Ctrl Pts',(38.4034120046589,7.71374537848964,62.9478547481597));
#153631=CARTESIAN_POINT('Ctrl Pts',(38.353854388085,7.93423868926519,63.0163619491341));
#153632=CARTESIAN_POINT('Ctrl Pts',(38.2995586747863,8.15088734571122,63.0873245284362));
#153633=CARTESIAN_POINT('Ctrl Pts',(38.2404641286669,8.3636343684669,63.1604989037323));
#153634=CARTESIAN_POINT('Ctrl Pts',(38.1985944857594,8.5143697993545,63.2123443812733));
#153635=CARTESIAN_POINT('Ctrl Pts',(38.1543162113558,8.66314742523656,63.2653009763042));
#153636=CARTESIAN_POINT('Ctrl Pts',(38.1076107402353,8.80995754172659,63.3192933263533));
#153637=CARTESIAN_POINT('Ctrl Pts',(38.040477762247,9.0209777944362,63.3969002353602));
#153638=CARTESIAN_POINT('Ctrl Pts',(37.9683308415603,9.22793205243882,63.476645035497));
#153639=CARTESIAN_POINT('Ctrl Pts',(37.8911667027997,9.43083440096504,63.5582971365134));
#153640=CARTESIAN_POINT('Ctrl Pts',(37.8131087081171,9.63608713490014,63.6408950812237));
#153641=CARTESIAN_POINT('Ctrl Pts',(37.7299171586969,9.8371938291356,63.7254447963416));
#153642=CARTESIAN_POINT('Ctrl Pts',(37.6415778233655,10.0341968982806,63.8117514604914));
#153643=CARTESIAN_POINT('Ctrl Pts',(37.5533472488685,10.2309574229453,63.8979518663727));
#153644=CARTESIAN_POINT('Ctrl Pts',(37.4599821147105,10.4236247681885,63.9859049945857));
#153645=CARTESIAN_POINT('Ctrl Pts',(37.3614490022685,10.6122639308637,64.0754591935364));
#153646=CARTESIAN_POINT('Ctrl Pts',(37.2641660718243,10.7985096515844,64.163877134385));
#153647=CARTESIAN_POINT('Ctrl Pts',(37.1618459602365,10.980829119707,64.2538559225466));
#153648=CARTESIAN_POINT('Ctrl Pts',(37.0544300457932,11.1593017562432,64.3452890788976));
#153649=CARTESIAN_POINT('Ctrl Pts',(36.9976569986222,11.2536307526987,64.3936146824677));
#153650=CARTESIAN_POINT('Ctrl Pts',(36.9394599539417,11.3468853923056,64.4423472142503));
#153651=CARTESIAN_POINT('Ctrl Pts',(36.8798265043843,11.4390788310839,64.491475300858));
#153652=CARTESIAN_POINT('Origin',(35.5956616019292,14.4895299089392,57.2082295467003));
#153653=CARTESIAN_POINT('Ctrl Pts',(35.8543614565591,13.15204220094,65.45231182744));
#153654=CARTESIAN_POINT('Ctrl Pts',(32.4237988913791,11.23764088211,65.205920002004));
#153655=CARTESIAN_POINT('Ctrl Pts',(29.3253632443791,10.80309640319,62.81729045488));
#153656=CARTESIAN_POINT('Ctrl Pts',(27.9368279710891,12.04170148852,59.34846031169));
#153657=CARTESIAN_POINT('Ctrl Pts',(36.3019357589691,12.58434307729,65.092157074978));
#153658=CARTESIAN_POINT('Ctrl Pts',(32.7688116514491,10.68400218145,64.923549223214));
#153659=CARTESIAN_POINT('Ctrl Pts',(29.5936770628891,10.26603134238,62.50254428216));
#153660=CARTESIAN_POINT('Ctrl Pts',(28.2340161075791,11.52235912053,58.94033961831));
#153661=CARTESIAN_POINT('Ctrl Pts',(36.7244351862591,11.99194848018,64.746982746171));
#153662=CARTESIAN_POINT('Ctrl Pts',(33.0867885711591,10.11975548635,64.661809058638));
#153663=CARTESIAN_POINT('Ctrl Pts',(29.8375082935191,9.71937111787702,62.20880149968));
#153664=CARTESIAN_POINT('Ctrl Pts',(28.5143069408691,10.98034479711,58.54871055167));
#153665=CARTESIAN_POINT('Ctrl Pts',(37.1146182133191,11.38351121538,64.4248079792711));
#153666=CARTESIAN_POINT('Ctrl Pts',(33.3745126141391,9.55513834427301,64.424781466774));
#153667=CARTESIAN_POINT('Ctrl Pts',(30.0553047540791,9.17314039863302,61.94111101675));
#153668=CARTESIAN_POINT('Ctrl Pts',(28.7730289746491,10.42357140722,58.18289110879));
#153669=CARTESIAN_POINT('Ctrl Pts',(36.8798265045291,11.43907883074,64.491475301679));
#153670=CARTESIAN_POINT('Ctrl Pts',(36.5447601595308,11.9562440716563,64.7671593619721));
#153671=CARTESIAN_POINT('Ctrl Pts',(36.1868105242993,12.4615090948357,65.059084102699));
#153672=CARTESIAN_POINT('Ctrl Pts',(35.8057492437391,12.9545337474,65.365954457758));
#153673=CARTESIAN_POINT('Origin',(62.4468966735091,1.4210854715202E-14,
88.14465325204));
#153674=CARTESIAN_POINT('',(59.2279850657691,10.8294941091,60.30347098134));
#153675=CARTESIAN_POINT('Ctrl Pts',(62.2792373804993,12.9545454545494,60.6979699644412));
#153676=CARTESIAN_POINT('Ctrl Pts',(61.8897073835902,12.7338209487284,60.6593514763456));
#153677=CARTESIAN_POINT('Ctrl Pts',(61.5099484134262,12.5022554868387,60.6170931465005));
#153678=CARTESIAN_POINT('Ctrl Pts',(61.1401151554292,12.2595992725174,60.5719752910757));
#153679=CARTESIAN_POINT('Ctrl Pts',(60.7728430689499,12.0186235024809,60.5271698860965));
#153680=CARTESIAN_POINT('Ctrl Pts',(60.4153597015435,11.7667100689689,60.47954440569));
#153681=CARTESIAN_POINT('Ctrl Pts',(60.0678070782513,11.5036136977798,60.429913403337));
#153682=CARTESIAN_POINT('Ctrl Pts',(59.7810828472561,11.2865642507285,60.3889687807691));
#153683=CARTESIAN_POINT('Ctrl Pts',(59.5011172473088,11.061903765029,60.3466601017626));
#153684=CARTESIAN_POINT('Ctrl Pts',(59.2279850656438,10.8294941093792,60.3034709806296));
#153685=CARTESIAN_POINT('',(59.2279850657991,-10.82949410913,60.30347098135));
#153686=CARTESIAN_POINT('Ctrl Pts',(59.2279850656426,10.8294941093819,60.3034709806228));
#153687=CARTESIAN_POINT('Ctrl Pts',(59.0590795829281,10.6857595475055,60.2767580663414));
#153688=CARTESIAN_POINT('Ctrl Pts',(58.8934066931531,10.5376026455191,60.2491609098041));
#153689=CARTESIAN_POINT('Ctrl Pts',(58.7309616758768,10.3850122881246,60.2208262862206));
#153690=CARTESIAN_POINT('Ctrl Pts',(58.570753726094,10.2345232874479,60.1928818652202));
#153691=CARTESIAN_POINT('Ctrl Pts',(58.4136850934738,10.0797216908457,60.1642198447616));
#153692=CARTESIAN_POINT('Ctrl Pts',(58.2597950174985,9.92057176318211,60.1349835210994));
#153693=CARTESIAN_POINT('Ctrl Pts',(58.2038786422741,9.86274420662415,60.1243604238418));
#153694=CARTESIAN_POINT('Ctrl Pts',(58.1483823586069,9.80434234877015,60.1136615506583));
#153695=CARTESIAN_POINT('Ctrl Pts',(58.0933096167251,9.74536380024524,60.1028939810487));
#153696=CARTESIAN_POINT('Ctrl Pts',(57.9458021331067,9.58739495789036,60.0740539951769));
#153697=CARTESIAN_POINT('Ctrl Pts',(57.8013160487736,9.42529668230862,60.0447253867283));
#153698=CARTESIAN_POINT('Ctrl Pts',(57.6598752169046,9.25904163467008,60.0150721757949));
#153699=CARTESIAN_POINT('Ctrl Pts',(57.628562885117,9.22223590365005,60.0085075143244));
#153700=CARTESIAN_POINT('Ctrl Pts',(57.5973999739887,9.18522635045155,60.0019269632268));
#153701=CARTESIAN_POINT('Ctrl Pts',(57.5663870484643,9.14801251292571,59.9953323409695));
#153702=CARTESIAN_POINT('Ctrl Pts',(57.4808363932956,9.04535634205985,59.9771407564877));
#153703=CARTESIAN_POINT('Ctrl Pts',(57.3964251327715,8.9411467102242,59.9588425419686));
#153704=CARTESIAN_POINT('Ctrl Pts',(57.3131606483973,8.83537641227296,59.9404797170312));
#153705=CARTESIAN_POINT('Ctrl Pts',(57.2715284062101,8.78249126329734,59.9312983045624));
#153706=CARTESIAN_POINT('Ctrl Pts',(57.2301828662008,8.72921592957571,59.9221007847856));
#153707=CARTESIAN_POINT('Ctrl Pts',(57.1891250082528,8.67554951902579,59.9128927285279));
#153708=CARTESIAN_POINT('Ctrl Pts',(57.1634523238683,8.64199295058918,59.9071351090632));
#153709=CARTESIAN_POINT('Ctrl Pts',(57.1374312224451,8.60767483826395,59.9012695327338));
#153710=CARTESIAN_POINT('Ctrl Pts',(57.1119290737584,8.57373520574596,59.8954922629261));
#153711=CARTESIAN_POINT('Ctrl Pts',(57.0976552888904,8.55473888433728,59.8922586724011));
#153712=CARTESIAN_POINT('Ctrl Pts',(57.0835432510979,8.5358616141826,59.8890527294345));
#153713=CARTESIAN_POINT('Ctrl Pts',(57.0697388483035,8.51730679825192,59.8859086612033));
#153714=CARTESIAN_POINT('Ctrl Pts',(57.0687628449579,8.51599492966228,59.8856863682756));
#153715=CARTESIAN_POINT('Ctrl Pts',(57.0677883776336,8.51468467394813,59.8854643845792));
#153716=CARTESIAN_POINT('Ctrl Pts',(57.0668154970974,8.513376103457,59.8852427221799));
#153717=CARTESIAN_POINT('Ctrl Pts',(56.9398671014472,8.34262448671979,59.8563186303476));
#153718=CARTESIAN_POINT('Ctrl Pts',(56.8175157456154,8.17037242182476,59.8277440127108));
#153719=CARTESIAN_POINT('Ctrl Pts',(56.6997399809284,7.9966358962389,59.7995971606568));
#153720=CARTESIAN_POINT('Ctrl Pts',(56.5812815801934,7.82189238236865,59.7712871676042));
#153721=CARTESIAN_POINT('Ctrl Pts',(56.4674518916248,7.64564667420447,59.7434096701134));
#153722=CARTESIAN_POINT('Ctrl Pts',(56.358279023726,7.46789973214102,59.7160500410813));
#153723=CARTESIAN_POINT('Ctrl Pts',(56.3085945078996,7.38700719055972,59.7035986880317));
#153724=CARTESIAN_POINT('Ctrl Pts',(56.2598751796783,7.30580355524723,59.691254693885));
#153725=CARTESIAN_POINT('Ctrl Pts',(56.2121271546688,7.22428827363687,59.6790266927907));
#153726=CARTESIAN_POINT('Ctrl Pts',(56.2106478891286,7.22176287605111,59.6786478611921));
#153727=CARTESIAN_POINT('Ctrl Pts',(56.2091695560213,7.21923717932473,59.6782691409578));
#153728=CARTESIAN_POINT('Ctrl Pts',(56.2076921551256,7.21671118302507,59.6778905323204));
#153729=CARTESIAN_POINT('Ctrl Pts',(56.0786259342956,6.99603932802176,59.6448151591173));
#153730=CARTESIAN_POINT('Ctrl Pts',(55.9566410081673,6.77309191637419,59.6125985100089));
#153731=CARTESIAN_POINT('Ctrl Pts',(55.8417738725684,6.54788192837225,59.5814482300864));
#153732=CARTESIAN_POINT('Ctrl Pts',(55.784340304769,6.43527693437129,59.5658730901252));
#153733=CARTESIAN_POINT('Ctrl Pts',(55.7286862328209,6.32210634815834,59.5505648401431));
#153734=CARTESIAN_POINT('Ctrl Pts',(55.6748165509668,6.20837284521694,59.5355513624588));
#153735=CARTESIAN_POINT('Ctrl Pts',(55.6462508535993,6.14806291366084,59.5275901040069));
#153736=CARTESIAN_POINT('Ctrl Pts',(55.6179612615491,6.08710656462898,59.519648101766));
#153737=CARTESIAN_POINT('Ctrl Pts',(55.5903126041415,6.02627911558751,59.5118318947263));
#153738=CARTESIAN_POINT('Ctrl Pts',(55.5658209493739,5.97239711834083,59.5049081645218));
#153739=CARTESIAN_POINT('Ctrl Pts',(55.5418314797697,5.9186165509691,59.4980830580316));
#153740=CARTESIAN_POINT('Ctrl Pts',(55.5185657968262,5.86548670373654,59.4914243363906));
#153741=CARTESIAN_POINT('Ctrl Pts',(55.4156138859168,5.63038424350782,59.4619591314012));
#153742=CARTESIAN_POINT('Ctrl Pts',(55.3194484791371,5.39295812998054,59.4339787906589));
#153743=CARTESIAN_POINT('Ctrl Pts',(55.2298705468524,5.15304981258439,59.4075238454497));
#153744=CARTESIAN_POINT('Ctrl Pts',(55.1435432835686,4.9218474622776,59.3820289164869));
#153745=CARTESIAN_POINT('Ctrl Pts',(55.0633348246565,4.68833991247754,59.3579508911544));
#153746=CARTESIAN_POINT('Ctrl Pts',(54.9891061163647,4.4523992880887,59.3353451301884));
#153747=CARTESIAN_POINT('Ctrl Pts',(54.9143193404503,4.21468481061334,59.3125694141799));
#153748=CARTESIAN_POINT('Ctrl Pts',(54.8456021618042,3.97449950281697,59.2912881697926));
#153749=CARTESIAN_POINT('Ctrl Pts',(54.7831355984502,3.732100756132,59.2715977724828));
#153750=CARTESIAN_POINT('Ctrl Pts',(54.724323975159,3.50388484331681,59.2530594670783));
#153751=CARTESIAN_POINT('Ctrl Pts',(54.671053301148,3.27370683043166,59.2359314995989));
#153752=CARTESIAN_POINT('Ctrl Pts',(54.6235060357775,3.04180580456216,59.2203087503871));
#153753=CARTESIAN_POINT('Ctrl Pts',(54.6202808930024,3.02607590059592,59.2192490554424));
#153754=CARTESIAN_POINT('Ctrl Pts',(54.6170815819542,3.01033757179436,59.2181963285862));
#153755=CARTESIAN_POINT('Ctrl Pts',(54.6139081016492,2.99459087982342,59.2171506133393));
#153756=CARTESIAN_POINT('Ctrl Pts',(54.5654562732485,2.75417469824556,59.2011849192656));
#153757=CARTESIAN_POINT('Ctrl Pts',(54.523021719713,2.51180993797416,59.1868522684903));
#153758=CARTESIAN_POINT('Ctrl Pts',(54.4865661577128,2.26747671758865,59.1743098336218));
#153759=CARTESIAN_POINT('Ctrl Pts',(54.4504614062033,2.02549470651829,59.1618880941284));
#153760=CARTESIAN_POINT('Ctrl Pts',(54.420221143089,1.78158156531106,59.1512220156086));
#153761=CARTESIAN_POINT('Ctrl Pts',(54.3958549336375,1.53571073982857,59.1424830742769));
#153762=CARTESIAN_POINT('Ctrl Pts',(54.3711335941183,1.28625642208994,59.1336167655419));
#153763=CARTESIAN_POINT('Ctrl Pts',(54.3524586267359,1.03478658610385,59.1267338002371));
#153764=CARTESIAN_POINT('Ctrl Pts',(54.339889719583,0.781271445267059,59.122037673447));
#153765=CARTESIAN_POINT('Ctrl Pts',(54.3273208124301,0.527756304430266,
59.117341546657));
#153766=CARTESIAN_POINT('Ctrl Pts',(54.3208579646841,0.2721955082923,59.1148319135422));
#153767=CARTESIAN_POINT('Ctrl Pts',(54.320611205963,0.0145625469582074,
59.114741865325));
#153768=CARTESIAN_POINT('Ctrl Pts',(54.3203494715567,-0.258706052728112,
59.1146463521185));
#153769=CARTESIAN_POINT('Ctrl Pts',(54.3270837351186,-0.529930243673467,
59.1172754622834));
#153770=CARTESIAN_POINT('Ctrl Pts',(54.3407128965343,-0.799028173290029,
59.1223642792772));
#153771=CARTESIAN_POINT('Ctrl Pts',(54.3545066696695,-1.07137624218956,
59.1275145585203));
#153772=CARTESIAN_POINT('Ctrl Pts',(54.3753628104337,-1.34154672703684,
59.1351846587339));
#153773=CARTESIAN_POINT('Ctrl Pts',(54.4032218321361,-1.60945722250699,
59.1451294739156));
#153774=CARTESIAN_POINT('Ctrl Pts',(54.4315877950223,-1.88224279453792,
59.1552552515315));
#153775=CARTESIAN_POINT('Ctrl Pts',(54.4672137438209,-2.15268581224499,
59.1677396219718));
#153776=CARTESIAN_POINT('Ctrl Pts',(54.5100848851986,-2.42069585734544,
59.1823491365729));
#153777=CARTESIAN_POINT('Ctrl Pts',(54.5394027880972,-2.60397748283012,
59.1923400142753));
#153778=CARTESIAN_POINT('Ctrl Pts',(54.5721100330777,-2.78612122246499,
59.2033252772472));
#153779=CARTESIAN_POINT('Ctrl Pts',(54.6082145668267,-2.96709559377786,
59.2152355980989));
#153780=CARTESIAN_POINT('Ctrl Pts',(54.6116595092352,-2.98436340537522,
59.2163720307056));
#153781=CARTESIAN_POINT('Ctrl Pts',(54.6151353887236,-3.00162056868052,
59.217516887937));
#153782=CARTESIAN_POINT('Ctrl Pts',(54.6186422447928,-3.01886702602003,
59.2186701098161));
#153783=CARTESIAN_POINT('Ctrl Pts',(54.6685109495927,-3.26411760743095,
59.2350693233336));
#153784=CARTESIAN_POINT('Ctrl Pts',(54.7246069067787,-3.50723131290814,
59.2531671796548));
#153785=CARTESIAN_POINT('Ctrl Pts',(54.7868883723096,-3.74814573278264,
59.272844922212));
#153786=CARTESIAN_POINT('Ctrl Pts',(54.848836712347,-3.98777157130564,59.2924174142321));
#153787=CARTESIAN_POINT('Ctrl Pts',(54.9169044303602,-4.22522200340054,
59.3135530070516));
#153788=CARTESIAN_POINT('Ctrl Pts',(54.9910949979195,-4.46045128752221,
59.3361544451959));
#153789=CARTESIAN_POINT('Ctrl Pts',(55.0654850443464,-4.69631304114448,
59.3588166526459));
#153790=CARTESIAN_POINT('Ctrl Pts',(55.146020717095,-4.92993807118413,59.3829539452067));
#153791=CARTESIAN_POINT('Ctrl Pts',(55.2326893264597,-5.16127026167754,
59.4084942759323));
#153792=CARTESIAN_POINT('Ctrl Pts',(55.276023631142,-5.27693635692425,59.421264441295));
#153793=CARTESIAN_POINT('Ctrl Pts',(55.3208912335958,-5.39202908955734,
59.4343857088369));
#153794=CARTESIAN_POINT('Ctrl Pts',(55.3672909336742,-5.50654108903935,
59.4478512005941));
#153795=CARTESIAN_POINT('Ctrl Pts',(55.3904907837134,-5.56379708878036,
59.4545839464727));
#153796=CARTESIAN_POINT('Ctrl Pts',(55.4140736618391,-5.62090789344703,
59.4614027690403));
#153797=CARTESIAN_POINT('Ctrl Pts',(55.4380394395861,-5.67787252503938,
59.4683069334854));
#153798=CARTESIAN_POINT('Ctrl Pts',(55.4500223284596,-5.70635484083555,
59.471759015708));
#153799=CARTESIAN_POINT('Ctrl Pts',(55.4621009424477,-5.73480061255788,
59.4752324346489));
#153800=CARTESIAN_POINT('Ctrl Pts',(55.4742752667805,-5.76320971526244,
59.4787271063192));
#153801=CARTESIAN_POINT('Ctrl Pts',(55.4803624289469,-5.77741426661473,
59.4804744421543));
#153802=CARTESIAN_POINT('Ctrl Pts',(55.4864735187118,-5.79160965066008,
59.4822270912488));
#153803=CARTESIAN_POINT('Ctrl Pts',(55.4926085343061,-5.8057958516082,59.4839850435921));
#153804=CARTESIAN_POINT('Ctrl Pts',(55.4987435499005,-5.81998205255631,
59.4857429959354));
#153805=CARTESIAN_POINT('Ctrl Pts',(55.5044550657775,-5.83313381049701,
59.4873782697557));
#153806=CARTESIAN_POINT('Ctrl Pts',(55.5110853568569,-5.84832688919887,
59.4892748006713));
#153807=CARTESIAN_POINT('Ctrl Pts',(55.6016461484042,-6.05584375637715,
59.5151788430206));
#153808=CARTESIAN_POINT('Ctrl Pts',(55.6969727210893,-6.25997357036908,
59.5419952418224));
#153809=CARTESIAN_POINT('Ctrl Pts',(55.7968887123826,-6.46077599426773,
59.5695027589807));
#153810=CARTESIAN_POINT('Ctrl Pts',(55.8993092391477,-6.66661181459251,
59.5976997909161));
#153811=CARTESIAN_POINT('Ctrl Pts',(56.0065521001706,-6.86895162215178,
59.6266232452781));
#153812=CARTESIAN_POINT('Ctrl Pts',(56.1184762778283,-7.06786023839376,
59.656059786709));
#153813=CARTESIAN_POINT('Ctrl Pts',(56.2317422028379,-7.26915337167839,
59.68584921348));
#153814=CARTESIAN_POINT('Ctrl Pts',(56.3498024034668,-7.46693284995802,
59.7161643869244));
#153815=CARTESIAN_POINT('Ctrl Pts',(56.4725600911692,-7.66126201797403,
59.7468055032499));
#153816=CARTESIAN_POINT('Ctrl Pts',(56.5969927808993,-7.85824276534574,
59.777864710963));
#153817=CARTESIAN_POINT('Ctrl Pts',(56.7262520472292,-8.05167871602991,
59.8092591046023));
#153818=CARTESIAN_POINT('Ctrl Pts',(56.8602869895031,-8.24162728614395,
59.8407979957789));
#153819=CARTESIAN_POINT('Ctrl Pts',(56.9239377896736,-8.33183046953685,
59.855775251902));
#153820=CARTESIAN_POINT('Ctrl Pts',(56.9886662855614,-8.42124704991932,
59.8707853182742));
#153821=CARTESIAN_POINT('Ctrl Pts',(57.0544708651079,-8.50988220134331,
59.8858088337675));
#153822=CARTESIAN_POINT('Ctrl Pts',(57.1933423107988,-8.69693440503645,
59.9175138812017));
#153823=CARTESIAN_POINT('Ctrl Pts',(57.3370030268218,-8.88050745517193,
59.9492783279215));
#153824=CARTESIAN_POINT('Ctrl Pts',(57.4854155525887,-9.06060085278201,
59.9809314046518));
#153825=CARTESIAN_POINT('Ctrl Pts',(57.6345467173149,-9.24156629357823,
60.0127377510201));
#153826=CARTESIAN_POINT('Ctrl Pts',(57.7884759610297,-9.41901866773446,
60.0444319421711));
#153827=CARTESIAN_POINT('Ctrl Pts',(57.9472137328405,-9.59293834494708,
60.0758466724522));
#153828=CARTESIAN_POINT('Ctrl Pts',(58.1056349933134,-9.76651123922892,
60.1071987640921));
#153829=CARTESIAN_POINT('Ctrl Pts',(58.2688457995564,-9.93656585419427,
60.1382728031));
#153830=CARTESIAN_POINT('Ctrl Pts',(58.4369022484652,-10.1030583892898,
60.1689039612922));
#153831=CARTESIAN_POINT('Ctrl Pts',(58.6034090924211,-10.2680157398762,
60.1992526775147));
#153832=CARTESIAN_POINT('Ctrl Pts',(58.7746728320292,-10.4294766998782,
60.2291669206477));
#153833=CARTESIAN_POINT('Ctrl Pts',(58.95079006548,-10.5873700501157,60.2584835746801));
#153834=CARTESIAN_POINT('Ctrl Pts',(59.0418834198168,-10.669037440744,60.2736470672095));
#153835=CARTESIAN_POINT('Ctrl Pts',(59.1342758914813,-10.749749898048,60.2886506162358));
#153836=CARTESIAN_POINT('Ctrl Pts',(59.2279850656721,-10.8294941094132,
60.3034709806296));
#153837=CARTESIAN_POINT('Ctrl Pts',(59.2279850656726,-10.8294941094118,
60.303470980633));
#153838=CARTESIAN_POINT('Ctrl Pts',(59.5767424389413,-11.1262539191291,
60.3586184675425));
#153839=CARTESIAN_POINT('Ctrl Pts',(59.9366440777721,-11.4103793077849,
60.4123224458978));
#153840=CARTESIAN_POINT('Ctrl Pts',(60.3075303353131,-11.6821583996076,
60.4635928169708));
#153841=CARTESIAN_POINT('Ctrl Pts',(60.6796998531796,-11.9548778425992,
60.5150405826809));
#153842=CARTESIAN_POINT('Ctrl Pts',(61.0629301323383,-12.2151653842106,
60.564037881877));
#153843=CARTESIAN_POINT('Ctrl Pts',(61.4570510653701,-12.4633103583552,
60.6096360877662));
#153844=CARTESIAN_POINT('Ctrl Pts',(61.7260584762589,-12.6326818162633,
60.6407591626383));
#153845=CARTESIAN_POINT('Ctrl Pts',(62.0001393885515,-12.7963963183867,
60.6702997600123));
#153846=CARTESIAN_POINT('Ctrl Pts',(62.2792373805004,-12.9545454545462,
60.6979699644477));
#153847=CARTESIAN_POINT('Ctrl Pts',(62.3623725079491,-13.1649643715,60.78391287288));
#153848=CARTESIAN_POINT('Ctrl Pts',(63.8217099690391,-11.20483377633,59.6461334374101));
#153849=CARTESIAN_POINT('Ctrl Pts',(64.7770536940892,-10.27834225011,57.30189869769));
#153850=CARTESIAN_POINT('Ctrl Pts',(64.8631085247691,-10.73979194701,54.64739874676));
#153851=CARTESIAN_POINT('Ctrl Pts',(61.1174740105891,-12.47994051503,60.66365145323));
#153852=CARTESIAN_POINT('Ctrl Pts',(62.7940792459991,-10.52306401831,59.5562432799201));
#153853=CARTESIAN_POINT('Ctrl Pts',(63.9019099705191,-9.63724577769599,
57.1388720445));
#153854=CARTESIAN_POINT('Ctrl Pts',(63.9901546224391,-10.18300062512,54.3950475618301));
#153855=CARTESIAN_POINT('Ctrl Pts',(59.9844193641791,-11.69588976856,60.50709666618));
#153856=CARTESIAN_POINT('Ctrl Pts',(61.8920759066391,-9.76298109347099,
59.44379451149));
#153857=CARTESIAN_POINT('Ctrl Pts',(63.1412817937692,-8.92499334381699,
56.95138240988));
#153858=CARTESIAN_POINT('Ctrl Pts',(63.1903745247891,-9.54533591150498,
54.11035997021));
#153859=CARTESIAN_POINT('Ctrl Pts',(58.9593897563791,-10.81129024408,60.3407081496501));
#153860=CARTESIAN_POINT('Ctrl Pts',(61.1067038788591,-8.94679575810299,
59.33391888342));
#153861=CARTESIAN_POINT('Ctrl Pts',(62.4867262093291,-8.16465088582199,
56.76779162634));
#153862=CARTESIAN_POINT('Ctrl Pts',(62.4637164412891,-8.82522553066699,
53.82421532476));
#153863=CARTESIAN_POINT('',(62.5668976793491,-8.89165927519551,54.0330209494394));
#153864=CARTESIAN_POINT('Ctrl Pts',(59.2279850657991,-10.82949410913,60.30347098135));
#153865=CARTESIAN_POINT('Ctrl Pts',(59.6576037928366,-10.4528243853097,
60.0796572311861));
#153866=CARTESIAN_POINT('Ctrl Pts',(60.0954495905067,-10.0900443262501,
59.7549266261475));
#153867=CARTESIAN_POINT('Ctrl Pts',(60.91252465905,-9.46575246404225,58.9076269594709));
#153868=CARTESIAN_POINT('Ctrl Pts',(61.2902828898919,-9.20568070081324,
58.385136210451));
#153869=CARTESIAN_POINT('Ctrl Pts',(61.9121932750885,-8.84473536319556,
57.2171883668237));
#153870=CARTESIAN_POINT('Ctrl Pts',(62.155331367146,-8.74445034487759,56.5736358012396));
#153871=CARTESIAN_POINT('Ctrl Pts',(62.4775613443828,-8.70751278667245,
55.2813284955923));
#153872=CARTESIAN_POINT('Ctrl Pts',(62.5571152908332,-8.77000581973829,
54.6343903912162));
#153873=CARTESIAN_POINT('Ctrl Pts',(62.5668978279891,-8.89165927519899,
54.03302179244));
#153874=CARTESIAN_POINT('',(64.7368422444091,-10.63636346571,54.76937978503));
#153875=CARTESIAN_POINT('Ctrl Pts',(64.7368422444113,-10.6363634657067,
54.7693797850296));
#153876=CARTESIAN_POINT('Ctrl Pts',(64.4705013672014,-10.4618582038463,
54.6889341849824));
#153877=CARTESIAN_POINT('Ctrl Pts',(64.2101814201152,-10.2786530461274,
54.6074269325054));
#153878=CARTESIAN_POINT('Ctrl Pts',(63.9564670518738,-10.0871970340218,
54.5247549382549));
#153879=CARTESIAN_POINT('Ctrl Pts',(63.7027404475878,-9.89573178844495,
54.4420789569294));
#153880=CARTESIAN_POINT('Ctrl Pts',(63.4556202456009,-9.69601504587226,
54.3582380886331));
#153881=CARTESIAN_POINT('Ctrl Pts',(63.2156587923114,-9.48853636535973,
54.2731349397934));
#153882=CARTESIAN_POINT('Ctrl Pts',(62.9931099547497,-9.29611321349957,
54.1942072345829));
#153883=CARTESIAN_POINT('Ctrl Pts',(62.776718406385,-9.09701424058528,54.1141938331589));
#153884=CARTESIAN_POINT('Ctrl Pts',(62.5668978279935,-8.89165927519479,
54.0330217924392));
#153885=CARTESIAN_POINT('Origin',(61.3394944160718,-15.5454545454696,55.368422775105));
#153886=CARTESIAN_POINT('Ctrl Pts',(84.0800519726791,-12.99512036682,56.87009645751));
#153887=CARTESIAN_POINT('Ctrl Pts',(83.6661946429091,-12.5469383764,56.75027017985));
#153888=CARTESIAN_POINT('Ctrl Pts',(82.7965369015191,-11.71844316471,56.33665948385));
#153889=CARTESIAN_POINT('Ctrl Pts',(81.4695020430691,-10.82009029684,55.18295003764));
#153890=CARTESIAN_POINT('Ctrl Pts',(80.3036938147791,-10.39648861976,53.64722176789));
#153891=CARTESIAN_POINT('Ctrl Pts',(79.7378359864291,-10.4635207436,52.51240603953));
#153892=CARTESIAN_POINT('Ctrl Pts',(79.5131204023091,-10.57285133752,51.94360802037));
#153893=CARTESIAN_POINT('Ctrl Pts',(83.2651276943291,-13.34120049562,57.18470057318));
#153894=CARTESIAN_POINT('Ctrl Pts',(82.8829401304591,-12.90294209031,57.0362090282));
#153895=CARTESIAN_POINT('Ctrl Pts',(82.0847138805391,-12.10130574004,56.58227996675));
#153896=CARTESIAN_POINT('Ctrl Pts',(80.8653217669191,-11.23972064159,55.43357173692));
#153897=CARTESIAN_POINT('Ctrl Pts',(79.7738747741391,-10.82877473082,53.95609666109));
#153898=CARTESIAN_POINT('Ctrl Pts',(79.2196176577691,-10.88586704929,52.87448522791));
#153899=CARTESIAN_POINT('Ctrl Pts',(78.9913181074791,-10.98810527869,52.33051917722));
#153900=CARTESIAN_POINT('Ctrl Pts',(81.6394458735691,-13.91964486991,57.81578810632));
#153901=CARTESIAN_POINT('Ctrl Pts',(81.3170669355891,-13.50761079111,57.62192240622));
#153902=CARTESIAN_POINT('Ctrl Pts',(80.6510324482591,-12.76589073325,57.1089812309));
#153903=CARTESIAN_POINT('Ctrl Pts',(79.6315581494091,-11.97266212853,55.97951292672));
#153904=CARTESIAN_POINT('Ctrl Pts',(78.6903991156591,-11.57564099902,54.60435686025));
#153905=CARTESIAN_POINT('Ctrl Pts',(78.1765730446491,-11.60238669821,53.61372744078));
#153906=CARTESIAN_POINT('Ctrl Pts',(77.9523738165591,-11.68373610129,53.11270985383));
#153907=CARTESIAN_POINT('Ctrl Pts',(79.4388619220891,-14.43965128122,58.6008316937));
#153908=CARTESIAN_POINT('Ctrl Pts',(79.1924362457891,-14.06465275778,58.36868006312));
#153909=CARTESIAN_POINT('Ctrl Pts',(78.6866339965491,-13.39597478952,57.81107313064));
#153910=CARTESIAN_POINT('Ctrl Pts',(77.9069917824891,-12.6721700663,56.70787752612));
#153911=CARTESIAN_POINT('Ctrl Pts',(77.1657033515691,-12.2788510491,55.42701703778));
#153912=CARTESIAN_POINT('Ctrl Pts',(76.7353144646191,-12.2605680305,54.51917695659));
#153913=CARTESIAN_POINT('Ctrl Pts',(76.5382941560091,-12.31045564282,54.05817220228));
#153914=CARTESIAN_POINT('Ctrl Pts',(77.6162987730291,-14.73391373999,59.17156261559));
#153915=CARTESIAN_POINT('Ctrl Pts',(77.4292728693391,-14.38230171041,58.91782585669));
#153916=CARTESIAN_POINT('Ctrl Pts',(77.0457870997091,-13.757827987,58.33523259925));
#153917=CARTESIAN_POINT('Ctrl Pts',(76.4492311625191,-13.07397037488,57.24426156275));
#153918=CARTESIAN_POINT('Ctrl Pts',(75.8697775008791,-12.68142066445,56.01101958947));
#153919=CARTESIAN_POINT('Ctrl Pts',(75.5201084752091,-12.63506048891,55.14560797757));
#153920=CARTESIAN_POINT('Ctrl Pts',(75.3554576632691,-12.66496377676,54.70525314943));
#153921=CARTESIAN_POINT('Ctrl Pts',(76.2071628757491,-14.8934563637,59.56388257989));
#153922=CARTESIAN_POINT('Ctrl Pts',(76.0650224041191,-14.55550964164,59.29702655635));
#153923=CARTESIAN_POINT('Ctrl Pts',(75.7724199604191,-13.95625819436,58.69824636597));
#153924=CARTESIAN_POINT('Ctrl Pts',(75.3109369339791,-13.29449480621,57.60945441332));
#153925=CARTESIAN_POINT('Ctrl Pts',(74.8536355956291,-12.90182964091,56.39722064014));
#153926=CARTESIAN_POINT('Ctrl Pts',(74.5692627635191,-12.83911853561,55.55187457973));
#153927=CARTESIAN_POINT('Ctrl Pts',(74.4326271289791,-12.85728762685,55.12140910176));
#153928=CARTESIAN_POINT('Ctrl Pts',(74.7602603369891,-14.99086818853,59.91232469828));
#153929=CARTESIAN_POINT('Ctrl Pts',(74.6637866458491,-14.66200007839,59.6349011036));
#153930=CARTESIAN_POINT('Ctrl Pts',(74.4621882103191,-14.07915129287,59.02122513388));
#153931=CARTESIAN_POINT('Ctrl Pts',(74.1342948725691,-13.431302473,57.92606828431));
#153932=CARTESIAN_POINT('Ctrl Pts',(73.7988562189591,-13.03810819612,56.71909544721));
#153933=CARTESIAN_POINT('Ctrl Pts',(73.5820799877991,-12.96445387057,55.88141223042));
#153934=CARTESIAN_POINT('Ctrl Pts',(73.4755239802991,-12.97474890777,55.45483672956));
#153935=CARTESIAN_POINT('Ctrl Pts',(73.2774620481891,-15.02379049898,60.20753715318));
#153936=CARTESIAN_POINT('Ctrl Pts',(73.2272578267591,-14.69834531273,59.92141206142));
#153937=CARTESIAN_POINT('Ctrl Pts',(73.1168676334091,-14.1215596745,59.29259789444));
#153938=CARTESIAN_POINT('Ctrl Pts',(72.9214777686291,-13.47866908886,58.18047859039));
#153939=CARTESIAN_POINT('Ctrl Pts',(72.7071889548991,-13.08505255241,56.9615075124));
#153940=CARTESIAN_POINT('Ctrl Pts',(72.5588984830791,-13.00718824553,56.11840724491));
#153941=CARTESIAN_POINT('Ctrl Pts',(72.4834297908491,-13.01446680747,55.68943757256));
#153942=CARTESIAN_POINT('Ctrl Pts',(71.7826488958691,-14.99006392632,60.43659409979));
#153943=CARTESIAN_POINT('Ctrl Pts',(71.7789295473791,-14.6611250522,60.1428335071));
#153944=CARTESIAN_POINT('Ctrl Pts',(71.7594710721691,-14.07814838366,59.49702773573));
#153945=CARTESIAN_POINT('Ctrl Pts',(71.6944226714991,-13.43019013293,58.35538254833));
#153946=CARTESIAN_POINT('Ctrl Pts',(71.5980645007491,-13.03699746572,57.10603814888));
#153947=CARTESIAN_POINT('Ctrl Pts',(71.5159400922591,-12.96342646928,56.24445554096));
#153948=CARTESIAN_POINT('Ctrl Pts',(71.4704731886791,-12.97378221592,55.80703477539));
#153949=CARTESIAN_POINT('Ctrl Pts',(69.8115991120691,-14.85944831896,60.65919191265));
#153950=CARTESIAN_POINT('Ctrl Pts',(69.8699356568591,-14.51834940535,60.35791581069));
#153951=CARTESIAN_POINT('Ctrl Pts',(69.9713126105991,-13.91339295952,59.6893510355));
#153952=CARTESIAN_POINT('Ctrl Pts',(70.0764973366891,-13.24677567487,58.49470358249));
#153953=CARTESIAN_POINT('Ctrl Pts',(70.1302881609591,-12.85427967805,57.18301095558));
#153954=CARTESIAN_POINT('Ctrl Pts',(70.1292194872591,-12.79536407084,56.28083629208));
#153955=CARTESIAN_POINT('Ctrl Pts',(70.1195867559491,-12.81626401359,55.82474063768));
#153956=CARTESIAN_POINT('Ctrl Pts',(67.3973149529291,-14.53891337949,60.79998145237));
#153957=CARTESIAN_POINT('Ctrl Pts',(67.5334496752791,-14.17098221515,60.49568646605));
#153958=CARTESIAN_POINT('Ctrl Pts',(67.7865544822591,-13.51623522621,59.80123462312));
#153959=CARTESIAN_POINT('Ctrl Pts',(68.1007762587091,-12.80566305584,58.51830879814));
#153960=CARTESIAN_POINT('Ctrl Pts',(68.3297419833491,-12.41304472226,57.09105979811));
#153961=CARTESIAN_POINT('Ctrl Pts',(68.4141870978591,-12.38616952145,56.1109805838));
#153962=CARTESIAN_POINT('Ctrl Pts',(68.4394260012791,-12.43005186544,55.61929350187));
#153963=CARTESIAN_POINT('Ctrl Pts',(64.6154734129691,-13.91879763618,60.81696389427));
#153964=CARTESIAN_POINT('Ctrl Pts',(64.8521749835191,-13.50671310406,60.52453930129));
#153965=CARTESIAN_POINT('Ctrl Pts',(65.3027548701191,-12.76489017189,59.81471204003));
#153966=CARTESIAN_POINT('Ctrl Pts',(65.8746443789191,-11.9715608226,58.40452801752));
#153967=CARTESIAN_POINT('Ctrl Pts',(66.2888358550891,-11.57453512393,56.79020205016));
#153968=CARTESIAN_POINT('Ctrl Pts',(66.4328674667591,-11.60134676736,55.68345421607));
#153969=CARTESIAN_POINT('Ctrl Pts',(66.4721728268491,-11.68274103778,55.13592509803));
#153970=CARTESIAN_POINT('Ctrl Pts',(62.8734648869491,-13.34106036443,60.78023802665));
#153971=CARTESIAN_POINT('Ctrl Pts',(63.1818395710891,-12.9028007288,60.50999302207));
#153972=CARTESIAN_POINT('Ctrl Pts',(63.7767189561991,-12.10115904569,59.81043707638));
#153973=CARTESIAN_POINT('Ctrl Pts',(64.5297446150191,-11.23956517827,58.31393457948));
#153974=CARTESIAN_POINT('Ctrl Pts',(65.0500707627491,-10.8286161971,56.55223549403));
#153975=CARTESIAN_POINT('Ctrl Pts',(65.2009676842291,-10.88571082207,55.34626375257));
#153976=CARTESIAN_POINT('Ctrl Pts',(65.2294469649091,-10.98795046753,54.75700975733));
#153977=CARTESIAN_POINT('Ctrl Pts',(62.0002612841991,-12.99502442972,60.76331046995));
#153978=CARTESIAN_POINT('Ctrl Pts',(62.3481866604191,-12.54683897575,60.50916749016));
#153979=CARTESIAN_POINT('Ctrl Pts',(63.0239546412991,-11.7183348805,59.8230635593));
#153980=CARTESIAN_POINT('Ctrl Pts',(63.8763929217491,-10.81997022647,58.28504622256));
#153981=CARTESIAN_POINT('Ctrl Pts',(64.4466570060491,-10.39636449694,56.44318062693));
#153982=CARTESIAN_POINT('Ctrl Pts',(64.5902575303291,-10.46339979819,55.18325268157));
#153983=CARTESIAN_POINT('Ctrl Pts',(64.6068775615691,-10.57273271432,54.57189404607));
#153984=CARTESIAN_POINT('',(79.4586834778791,-10.63636348946,52.17352181749));
#153985=CARTESIAN_POINT('Ctrl Pts',(79.4586834778791,-10.63636348946,52.17352181749));
#153986=CARTESIAN_POINT('Ctrl Pts',(79.2182665366338,-10.8242034905193,
52.3493746776794));
#153987=CARTESIAN_POINT('Ctrl Pts',(78.9712303380147,-11.0019622800485,
52.5284827748445));
#153988=CARTESIAN_POINT('Ctrl Pts',(78.5918981391498,-11.2527215428637,
52.801824826324));
#153989=CARTESIAN_POINT('Ctrl Pts',(78.4000384533495,-11.3741328145895,
52.9396656717656));
#153990=CARTESIAN_POINT('Ctrl Pts',(78.1726240478271,-11.5086838386425,
53.1024812126444));
#153991=CARTESIAN_POINT('Ctrl Pts',(78.058055521351,-11.5741677613258,53.1843834338617));
#153992=CARTESIAN_POINT('Ctrl Pts',(78.0005600925498,-11.6064596423588,
53.2254574226984));
#153993=CARTESIAN_POINT('Ctrl Pts',(77.9758743927393,-11.6202023435904,
53.2430868128239));
#153994=CARTESIAN_POINT('Ctrl Pts',(77.9594073534643,-11.6293426353525,
53.2548455645689));
#153995=CARTESIAN_POINT('Ctrl Pts',(77.9496365045884,-11.6347475761949,
53.2618218595603));
#153996=CARTESIAN_POINT('Ctrl Pts',(77.835549087271,-11.6976998452158,53.3432720869405));
#153997=CARTESIAN_POINT('Ctrl Pts',(77.7080672130804,-11.7655718912864,
53.43126058736));
#153998=CARTESIAN_POINT('Ctrl Pts',(77.4852219956203,-11.8768312897897,
53.5804957074688));
#153999=CARTESIAN_POINT('Ctrl Pts',(77.4056671923129,-11.9154812671034,
53.6331166119991));
#154000=CARTESIAN_POINT('Ctrl Pts',(77.2782272168703,-11.9752576397277,
53.7163967090028));
#154001=CARTESIAN_POINT('Ctrl Pts',(77.2124802010098,-12.0055950223212,
53.7591239576359));
#154002=CARTESIAN_POINT('Ctrl Pts',(77.1321843721096,-12.0416433896302,
53.8108827161825));
#154003=CARTESIAN_POINT('Ctrl Pts',(77.091133281944,-12.0598139074465,53.8372406286189));
#154004=CARTESIAN_POINT('Ctrl Pts',(77.07334584094,-12.0676307473141,53.8486395217188));
#154005=CARTESIAN_POINT('Ctrl Pts',(77.0614443457364,-12.0728483122197,
53.8562616050807));
#154006=CARTESIAN_POINT('Ctrl Pts',(77.0538147825992,-12.0761832627605,
53.8611440448338));
#154007=CARTESIAN_POINT('Ctrl Pts',(76.9107015072919,-12.1386197783156,
53.9526821245316));
#154008=CARTESIAN_POINT('Ctrl Pts',(76.7773043815819,-12.1933590011967,
54.0360049530036));
#154009=CARTESIAN_POINT('Ctrl Pts',(76.585863466879,-12.267908338182,54.1527238662569));
#154010=CARTESIAN_POINT('Ctrl Pts',(76.4923046622753,-12.3032918237924,
54.2090173503535));
#154011=CARTESIAN_POINT('Ctrl Pts',(76.3870436154587,-12.3414994558542,
54.2710585866321));
#154012=CARTESIAN_POINT('Ctrl Pts',(76.3353979394004,-12.359863377654,54.3011684431247));
#154013=CARTESIAN_POINT('Ctrl Pts',(76.3098227963269,-12.3688638765705,
54.3159954194455));
#154014=CARTESIAN_POINT('Ctrl Pts',(76.2989152533216,-12.3726827212548,
54.322300963678));
#154015=CARTESIAN_POINT('Ctrl Pts',(76.2916554044697,-12.3752201006942,
54.3264937959008));
#154016=CARTESIAN_POINT('Ctrl Pts',(76.2893266900199,-12.3760333765106,
54.3278381426087));
#154017=CARTESIAN_POINT('Ctrl Pts',(75.9699585372172,-12.4872710399339,
54.5119303705281));
#154018=CARTESIAN_POINT('Ctrl Pts',(75.6597207636066,-12.5790030369484,
54.6767940136471));
#154019=CARTESIAN_POINT('Ctrl Pts',(75.2034047424673,-12.6936455014327,
54.8990161370789));
#154020=CARTESIAN_POINT('Ctrl Pts',(75.0527987684558,-12.7280340649545,
54.9689125940415));
#154021=CARTESIAN_POINT('Ctrl Pts',(74.8294150922816,-12.7743438611341,
55.0674421954789));
#154022=CARTESIAN_POINT('Ctrl Pts',(74.7183539461519,-12.7961804425788,
55.1151283361502));
#154023=CARTESIAN_POINT('Ctrl Pts',(74.5899403028197,-12.8194503967565,
55.16798999321));
#154024=CARTESIAN_POINT('Ctrl Pts',(74.5260291900002,-12.8305464055966,
55.1937266700248));
#154025=CARTESIAN_POINT('Ctrl Pts',(74.4987027424523,-12.8351876863875,
55.2046078106391));
#154026=CARTESIAN_POINT('Ctrl Pts',(74.4804994119687,-12.8382566553966,
55.2118288107744));
#154027=CARTESIAN_POINT('Ctrl Pts',(74.4726914094744,-12.8395648502973,
55.2149163039946));
#154028=CARTESIAN_POINT('Ctrl Pts',(73.7983918019866,-12.9515612288076,
55.4803672135456));
#154029=CARTESIAN_POINT('Ctrl Pts',(73.1425581831981,-13.0002712185578,
55.6679582563767));
#154030=CARTESIAN_POINT('Ctrl Pts',(72.1779457721873,-12.999862694313,55.8374422870987));
#154031=CARTESIAN_POINT('Ctrl Pts',(71.8467331756462,-12.9874245983009,
55.8775652700784));
#154032=CARTESIAN_POINT('Ctrl Pts',(71.3369427421527,-12.9480664787371,
55.9129204572201));
#154033=CARTESIAN_POINT('Ctrl Pts',(71.1648542801795,-12.9314972524444,
55.9205666692747));
#154034=CARTESIAN_POINT('Ctrl Pts',(70.9037101836172,-12.9011924710973,
55.9257878491668));
#154035=CARTESIAN_POINT('Ctrl Pts',(70.7723856405246,-12.88467741229,55.9268363417773));
#154036=CARTESIAN_POINT('Ctrl Pts',(70.6179100696195,-12.8629655994262,
55.9253165212991));
#154037=CARTESIAN_POINT('Ctrl Pts',(70.5403633290349,-12.8514912585476,
55.9238696208533));
#154038=CARTESIAN_POINT('Ctrl Pts',(70.5070635581712,-12.8464403744297,
55.9231021760181));
#154039=CARTESIAN_POINT('Ctrl Pts',(70.4848492499652,-12.8430434067123,
55.9225577880179));
#154040=CARTESIAN_POINT('Ctrl Pts',(70.4723440122104,-12.8411139351123,
55.9222310770215));
#154041=CARTESIAN_POINT('Ctrl Pts',(70.1512302636805,-12.7912143975556,
55.9134259636291));
#154042=CARTESIAN_POINT('Ctrl Pts',(69.8268858491848,-12.7300263417389,
55.8916180724123));
#154043=CARTESIAN_POINT('Ctrl Pts',(69.3229872617733,-12.6152727351453,
55.8386385829609));
#154044=CARTESIAN_POINT('Ctrl Pts',(69.1521305333145,-12.5731918441631,
55.8175996716809));
#154045=CARTESIAN_POINT('Ctrl Pts',(68.8918290846557,-12.503849098367,55.7809163561449));
#154046=CARTESIAN_POINT('Ctrl Pts',(68.7606749469699,-12.4676223509791,
55.76129334209));
#154047=CARTESIAN_POINT('Ctrl Pts',(68.6059830259655,-12.4225316334654,
55.7361438374548));
#154048=CARTESIAN_POINT('Ctrl Pts',(68.5282275913894,-12.3992667242409,
55.723003286718));
#154049=CARTESIAN_POINT('Ctrl Pts',(68.4892487990756,-12.3874527583474,
55.7162913336671));
#154050=CARTESIAN_POINT('Ctrl Pts',(68.4725220836888,-12.3823505609953,
55.7133843981258));
#154051=CARTESIAN_POINT('Ctrl Pts',(68.46136617385,-12.3789403947625,55.7114396862813));
#154052=CARTESIAN_POINT('Ctrl Pts',(68.454265362147,-12.3767642024997,55.7101972879607));
#154053=CARTESIAN_POINT('Ctrl Pts',(68.1902197847981,-12.2957068872524,
55.6638882242063));
#154054=CARTESIAN_POINT('Ctrl Pts',(67.898439597219,-12.1984333668864,55.6054520038334));
#154055=CARTESIAN_POINT('Ctrl Pts',(67.4173577167285,-12.017215557559,55.4977829400417));
#154056=CARTESIAN_POINT('Ctrl Pts',(67.2497818096774,-11.9509078132217,
55.4585539391153));
#154057=CARTESIAN_POINT('Ctrl Pts',(66.9883390582529,-11.8413193460853,
55.3945702757593));
#154058=CARTESIAN_POINT('Ctrl Pts',(66.8551003665473,-11.7839921569833,
55.3612929792204));
#154059=CARTESIAN_POINT('Ctrl Pts',(66.6954397661749,-11.7123873444338,
55.3201864286527));
#154060=CARTESIAN_POINT('Ctrl Pts',(66.6145814998515,-11.6753671227974,
55.2990578272136));
#154061=CARTESIAN_POINT('Ctrl Pts',(66.5695398063386,-11.6545315704221,
55.2872017499201));
#154062=CARTESIAN_POINT('Ctrl Pts',(66.5476610622123,-11.6443455785527,
55.2814164859836));
#154063=CARTESIAN_POINT('Ctrl Pts',(66.5359715222561,-11.6388869268952,
55.2783189307872));
#154064=CARTESIAN_POINT('Ctrl Pts',(66.5331097796484,-11.6375497290343,
55.2775602702098));
#154065=CARTESIAN_POINT('Ctrl Pts',(66.5251426860014,-11.6338261539074,
55.2754478327547));
#154066=CARTESIAN_POINT('Ctrl Pts',(66.4433421804196,-11.5963633136154,
55.2536349773092));
#154067=CARTESIAN_POINT('Ctrl Pts',(66.2128815524225,-11.4834360363897,
55.1907969074375));
#154068=CARTESIAN_POINT('Ctrl Pts',(66.1181588471154,-11.436223321606,55.1648209506834));
#154069=CARTESIAN_POINT('Ctrl Pts',(65.9501947904545,-11.3492951706169,
55.1181404177946));
#154070=CARTESIAN_POINT('Ctrl Pts',(65.8898979274334,-11.3176275957972,
55.10129334901));
#154071=CARTESIAN_POINT('Ctrl Pts',(65.793155058743,-11.2658118802046,55.0740631931231));
#154072=CARTESIAN_POINT('Ctrl Pts',(65.7432097182676,-11.2388248497899,
55.0599581410588));
#154073=CARTESIAN_POINT('Ctrl Pts',(65.6822274432277,-11.2053848067082,
55.0426374527362));
#154074=CARTESIAN_POINT('Ctrl Pts',(65.6510637532451,-11.188167229931,55.0337599181163));
#154075=CARTESIAN_POINT('Ctrl Pts',(65.6375643813724,-11.1806807010638,
55.029908611407));
#154076=CARTESIAN_POINT('Ctrl Pts',(65.6285329795425,-11.1756656714266,
55.0273306949228));
#154077=CARTESIAN_POINT('Ctrl Pts',(65.6222654085081,-11.1721797453671,
55.0255405354853));
#154078=CARTESIAN_POINT('Ctrl Pts',(65.2595784503797,-10.9702724799302,
54.9219108093643));
#154079=CARTESIAN_POINT('Ctrl Pts',(64.9677068724542,-10.7879579602342,
54.8363804219922));
#154080=CARTESIAN_POINT('Ctrl Pts',(64.7368422444091,-10.63636346571,54.76937978503));
#154081=CARTESIAN_POINT('Origin',(82.8560309931588,-15.5454545439394,51.5744768443685));
#154082=CARTESIAN_POINT('Ctrl Pts',(86.7935017742691,-10.81101501757,55.43269565713));
#154083=CARTESIAN_POINT('Ctrl Pts',(84.4312816407391,-8.94654054056199,
55.22108905121));
#154084=CARTESIAN_POINT('Ctrl Pts',(82.2567709278791,-8.16441345063199,
53.28170593214));
#154085=CARTESIAN_POINT('Ctrl Pts',(81.2716395534891,-8.82500194251199,
50.50774237648));
#154086=CARTESIAN_POINT('Ctrl Pts',(85.8893229942491,-11.69357781737,55.93843994818));
#154087=CARTESIAN_POINT('Ctrl Pts',(83.7324870031991,-9.76084628208499,
55.59207959555));
#154088=CARTESIAN_POINT('Ctrl Pts',(81.7057729806091,-8.92300163973699,
53.6771661408401));
#154089=CARTESIAN_POINT('Ctrl Pts',(80.6880453874592,-9.54345189092599,
51.02394478223));
#154090=CARTESIAN_POINT('Ctrl Pts',(84.8783621295491,-12.47844490921,56.4731990882401));
#154091=CARTESIAN_POINT('Ctrl Pts',(82.9237074454691,-10.52153477369,56.0062179350201));
#154092=CARTESIAN_POINT('Ctrl Pts',(81.0555047860191,-9.63580488196199,
54.1134952895101));
#154093=CARTESIAN_POINT('Ctrl Pts',(80.0340224569391,-10.18178345265,51.56516199695));
#154094=CARTESIAN_POINT('Ctrl Pts',(83.7460546069791,-13.16556661825,57.01369190147));
#154095=CARTESIAN_POINT('Ctrl Pts',(81.9857604089391,-11.20542779044,56.44355765246));
#154096=CARTESIAN_POINT('Ctrl Pts',(80.2864018783391,-10.27890102988,54.56745883809));
#154097=CARTESIAN_POINT('Ctrl Pts',(79.2976663793691,-10.74028182249,52.1025541699701));
#154098=CARTESIAN_POINT('',(81.2459147097291,-8.89165945462999,50.73940625853));
#154099=CARTESIAN_POINT('Ctrl Pts',(81.2459147097291,-8.89165945462999,
50.73940625853));
#154100=CARTESIAN_POINT('Ctrl Pts',(81.2202959565912,-8.92270890598236,
50.7617613799387));
#154101=CARTESIAN_POINT('Ctrl Pts',(81.1414335151752,-9.01946891462081,
50.8313298801056));
#154102=CARTESIAN_POINT('Ctrl Pts',(80.9346684136756,-9.25459974075488,
51.0080212942601));
#154103=CARTESIAN_POINT('Ctrl Pts',(80.8508805959602,-9.34785307260811,
51.0789961902285));
#154104=CARTESIAN_POINT('Ctrl Pts',(80.7008468650282,-9.50777103164881,
51.2039371401138));
#154105=CARTESIAN_POINT('Ctrl Pts',(80.6467707885678,-9.56440771321901,
51.2486649781948));
#154106=CARTESIAN_POINT('Ctrl Pts',(80.5592530342723,-9.65398878461894,
51.3204320423859));
#154107=CARTESIAN_POINT('Ctrl Pts',(80.5138927754486,-9.69993490407142,
51.3574844844354));
#154108=CARTESIAN_POINT('Ctrl Pts',(80.4580984353019,-9.75546994883981,
51.4027705544957));
#154109=CARTESIAN_POINT('Ctrl Pts',(80.4294734957991,-9.78370812276213,
51.4259297775437));
#154110=CARTESIAN_POINT('Ctrl Pts',(80.4170487161119,-9.79590972894298,
51.4359659465212));
#154111=CARTESIAN_POINT('Ctrl Pts',(80.408730540569,-9.80406610213962,51.4426813650083));
#154112=CARTESIAN_POINT('Ctrl Pts',(80.4031747110217,-9.80950359146663,
51.4471636877465));
#154113=CARTESIAN_POINT('Ctrl Pts',(80.0400544742734,-10.1644809698603,
51.7400019907965));
#154114=CARTESIAN_POINT('Ctrl Pts',(79.7198700088378,-10.4322956649842,
51.982474190258));
#154115=CARTESIAN_POINT('Ctrl Pts',(79.4586834778791,-10.63636348946,52.17352181749));
#154116=CARTESIAN_POINT('',(86.5280866410491,-10.82949410857,55.48972649733));
#154117=CARTESIAN_POINT('Origin',(85.5564956930185,-12.9954571590635,49.979316792856));
#154118=CARTESIAN_POINT('Ctrl Pts',(83.7957739555189,-12.9545454545505,
56.904024034869));
#154119=CARTESIAN_POINT('Ctrl Pts',(84.1486041138588,-12.7338209515203,
56.7345074233581));
#154120=CARTESIAN_POINT('Ctrl Pts',(84.4910076116214,-12.5022554926068,
56.5649123673248));
#154121=CARTESIAN_POINT('Ctrl Pts',(84.8231059758929,-12.2595992814565,
56.3960250296263));
#154122=CARTESIAN_POINT('Ctrl Pts',(85.1529044919244,-12.018623513573,56.2283072708483));
#154123=CARTESIAN_POINT('Ctrl Pts',(85.4725400985228,-11.7667100823158,
56.0612874470315));
#154124=CARTESIAN_POINT('Ctrl Pts',(85.7821579295011,-11.5036137134864,
55.895779563482));
#154125=CARTESIAN_POINT('Ctrl Pts',(86.0375866944652,-11.2865642614432,
55.7592387378025));
#154126=CARTESIAN_POINT('Ctrl Pts',(86.2861978886604,-11.0619037703368,
55.6237277063215));
#154127=CARTESIAN_POINT('Ctrl Pts',(86.5280866409232,-10.8294941088507,
55.4897264966159));
#154128=CARTESIAN_POINT('Origin',(62.4468966735091,1.4210854715202E-14,
88.14465325204));
#154129=CARTESIAN_POINT('Ctrl Pts',(86.5280866409241,-10.8294941088486,
55.4897264966211));
#154130=CARTESIAN_POINT('Ctrl Pts',(86.6918895241715,-10.6720900181015,
55.3989752596312));
#154131=CARTESIAN_POINT('Ctrl Pts',(86.8511035029772,-10.5104540155873,
55.3091182403179));
#154132=CARTESIAN_POINT('Ctrl Pts',(87.005791366162,-10.34458109779,55.2202729032426));
#154133=CARTESIAN_POINT('Ctrl Pts',(87.1610704384634,-10.1780742221685,
55.1310880038245));
#154134=CARTESIAN_POINT('Ctrl Pts',(87.3117886541035,-10.0072976322616,
55.04292228975));
#154135=CARTESIAN_POINT('Ctrl Pts',(87.4579649906633,-9.83223355314167,
54.9559191917343));
#154136=CARTESIAN_POINT('Ctrl Pts',(87.5660229298694,-9.70282092683066,
54.891603888058));
#154137=CARTESIAN_POINT('Ctrl Pts',(87.6715979854452,-9.57106506431779,
54.8279243985957));
#154138=CARTESIAN_POINT('Ctrl Pts',(87.774682602461,-9.43695606495881,54.764948471155));
#154139=CARTESIAN_POINT('Ctrl Pts',(87.9118857825905,-9.25846016781429,
54.6811290054907));
#154140=CARTESIAN_POINT('Ctrl Pts',(88.0447000283536,-9.07579752707207,
54.5985516421133));
#154141=CARTESIAN_POINT('Ctrl Pts',(88.1731648010593,-8.88894992129916,
54.5173877183289));
#154142=CARTESIAN_POINT('Ctrl Pts',(88.2232782819917,-8.81606158209185,
54.4857260677355));
#154143=CARTESIAN_POINT('Ctrl Pts',(88.2727294362972,-8.74253621078332,
54.4542797745651));
#154144=CARTESIAN_POINT('Ctrl Pts',(88.3215188668516,-8.6683720702075,54.423060113666));
#154145=CARTESIAN_POINT('Ctrl Pts',(88.4084488819124,-8.53623095308506,
54.3674348366068));
#154146=CARTESIAN_POINT('Ctrl Pts',(88.4932814398042,-8.4020630321285,54.3125284166921));
#154147=CARTESIAN_POINT('Ctrl Pts',(88.5760284980551,-8.26586071196768,
54.2584085335309));
#154148=CARTESIAN_POINT('Ctrl Pts',(88.6174020271806,-8.19775955188727,
54.2313485919503));
#154149=CARTESIAN_POINT('Ctrl Pts',(88.6582541958196,-8.12914975782779,
54.2044853684469));
#154150=CARTESIAN_POINT('Ctrl Pts',(88.6985866007877,-8.0600304155922,54.1778279138681));
#154151=CARTESIAN_POINT('Ctrl Pts',(88.7187528032718,-8.02547074447441,
54.1644991865787));
#154152=CARTESIAN_POINT('Ctrl Pts',(88.7387890658019,-7.99078368424058,
54.1512219071426));
#154153=CARTESIAN_POINT('Ctrl Pts',(88.7586955942985,-7.95596911635383,
54.1379972436758));
#154154=CARTESIAN_POINT('Ctrl Pts',(88.7732907992623,-7.93044353291926,
54.1283010942991));
#154155=CARTESIAN_POINT('Ctrl Pts',(88.7882361273448,-7.9041070941112,54.1183535710719));
#154156=CARTESIAN_POINT('Ctrl Pts',(88.8026071008764,-7.878591952754,54.1087707359372));
#154157=CARTESIAN_POINT('Ctrl Pts',(88.8078368246176,-7.86930676826568,
54.1052834578971));
#154158=CARTESIAN_POINT('Ctrl Pts',(88.8129909059121,-7.86013057299354,
54.1018442892881));
#154159=CARTESIAN_POINT('Ctrl Pts',(88.8180261878799,-7.85114276745102,
54.098482294191));
#154160=CARTESIAN_POINT('Ctrl Pts',(88.9278621585223,-7.65508932853309,
54.0251461836907));
#154161=CARTESIAN_POINT('Ctrl Pts',(89.03273547922,-7.45644993021727,53.9540375170907));
#154162=CARTESIAN_POINT('Ctrl Pts',(89.1327764104183,-7.25526270336443,
53.8852876975004));
#154163=CARTESIAN_POINT('Ctrl Pts',(89.2328176800074,-7.05407479599094,
53.8165376453622));
#154164=CARTESIAN_POINT('Ctrl Pts',(89.3280265081163,-6.8503386692998,53.7501461482649));
#154165=CARTESIAN_POINT('Ctrl Pts',(89.4184903579054,-6.64407409498235,
53.6862677950503));
#154166=CARTESIAN_POINT('Ctrl Pts',(89.5081546318131,-6.43963261551638,
53.6229540385303));
#154167=CARTESIAN_POINT('Ctrl Pts',(89.5931573688675,-6.23270680663967,
53.5621089256275));
#154168=CARTESIAN_POINT('Ctrl Pts',(89.6735424179408,-6.02330353211724,
53.5039100144859));
#154169=CARTESIAN_POINT('Ctrl Pts',(89.7531863679052,-5.81583082281737,
53.4462476603493));
#154170=CARTESIAN_POINT('Ctrl Pts',(89.8282973284865,-5.60592575728841,
53.3911826739128));
#154171=CARTESIAN_POINT('Ctrl Pts',(89.8988780945993,-5.39358828939796,
53.3389183812801));
#154172=CARTESIAN_POINT('Ctrl Pts',(89.9681322724845,-5.18524177259375,
53.2876364128577));
#154173=CARTESIAN_POINT('Ctrl Pts',(90.0330248486349,-4.97455309164704,
53.2390506443791));
#154174=CARTESIAN_POINT('Ctrl Pts',(90.0935211386558,-4.76152085442564,
53.1933861560868));
#154175=CARTESIAN_POINT('Ctrl Pts',(90.1287711912425,-4.63739096873988,
53.1667783159517));
#154176=CARTESIAN_POINT('Ctrl Pts',(90.1625279362402,-4.51246540473219,
53.1411629347915));
#154177=CARTESIAN_POINT('Ctrl Pts',(90.1947786764252,-4.3867443600625,53.116590296774));
#154178=CARTESIAN_POINT('Ctrl Pts',(81.0890185711991,-9.03398009659499,
50.59499624711));
#154179=CARTESIAN_POINT('Ctrl Pts',(82.066389392229,-8.36205842516198,53.36445303819));
#154180=CARTESIAN_POINT('Ctrl Pts',(84.2070509463491,-9.16260829370599,
55.32747811058));
#154181=CARTESIAN_POINT('Ctrl Pts',(86.5272072002091,-11.06780283748,55.58175683397));
#154182=CARTESIAN_POINT('Ctrl Pts',(82.487240909939,-7.53053025822599,50.35332743294));
#154183=CARTESIAN_POINT('Ctrl Pts',(83.5976153297791,-7.11372210236199,
52.98684050843));
#154184=CARTESIAN_POINT('Ctrl Pts',(85.9352162978791,-7.76899575474999,
54.59298316059));
#154185=CARTESIAN_POINT('Ctrl Pts',(88.5027323665692,-9.21684229213699,
54.4863678699901));
#154186=CARTESIAN_POINT('Ctrl Pts',(83.5727435711491,-5.62937756856198,
50.17140339387));
#154187=CARTESIAN_POINT('Ctrl Pts',(84.8299194058891,-5.40125583473699,
52.58820136205));
#154188=CARTESIAN_POINT('Ctrl Pts',(87.2071109645591,-5.85034243553598,
53.8781499741101));
#154189=CARTESIAN_POINT('Ctrl Pts',(89.7749977603691,-6.80110798966,53.53684402454));
#154190=CARTESIAN_POINT('Ctrl Pts',(84.1481896945291,-3.52973739894199,
50.07613844788));
#154191=CARTESIAN_POINT('Ctrl Pts',(85.4754380405791,-3.38512521217299,
52.35995335757));
#154192=CARTESIAN_POINT('Ctrl Pts',(87.8501898806692,-3.65538595374999,
53.49389491214));
#154193=CARTESIAN_POINT('Ctrl Pts',(90.3929854306691,-4.24045176432299,
53.05791123413));
#154194=CARTESIAN_POINT('',(84.1879278549181,-3.6707688494137,50.2206500166039));
#154195=CARTESIAN_POINT('Ctrl Pts',(84.1879274881912,-3.67076874249921,
50.2206500280999));
#154196=CARTESIAN_POINT('Ctrl Pts',(83.9030415620743,-4.65335590647006,
50.2708831032984));
#154197=CARTESIAN_POINT('Ctrl Pts',(83.501679882298,-5.60034065948235,50.3416539964655));
#154198=CARTESIAN_POINT('Ctrl Pts',(82.5073581548077,-7.353093032406,50.5169797445266));
#154199=CARTESIAN_POINT('Ctrl Pts',(81.9183583627455,-8.16338650643592,
50.6208362994988));
#154200=CARTESIAN_POINT('Ctrl Pts',(81.2459147097293,-8.89165945462988,
50.7394062585317));
#154201=CARTESIAN_POINT('Origin',(89.1641836723275,-5.263693750641,47.2711935873025));
#154202=CARTESIAN_POINT('Ctrl Pts',(84.0667906462691,-3.82236309078299,
50.0943346407));
#154203=CARTESIAN_POINT('Ctrl Pts',(84.6854064384891,-3.74742101924199,
51.1753351273));
#154204=CARTESIAN_POINT('Ctrl Pts',(86.5900487858291,-3.81967065678199,
52.94802757545));
#154205=CARTESIAN_POINT('Ctrl Pts',(89.1175620006691,-4.30049088340399,
53.32409278569));
#154206=CARTESIAN_POINT('Ctrl Pts',(90.2986082780691,-4.59747416179299,
53.12858445196));
#154207=CARTESIAN_POINT('Ctrl Pts',(84.4477663971991,-2.54890099283399,
50.03137520846));
#154208=CARTESIAN_POINT('Ctrl Pts',(85.0876027608091,-2.50648289723299,
51.07540225952));
#154209=CARTESIAN_POINT('Ctrl Pts',(87.0114302617491,-2.55714551410099,
52.7497662106));
#154210=CARTESIAN_POINT('Ctrl Pts',(89.5316085984691,-2.85585336077299,
53.03803083282));
#154211=CARTESIAN_POINT('Ctrl Pts',(90.7113645633691,-3.04045842633399,
52.81088733089));
#154212=CARTESIAN_POINT('Ctrl Pts',(84.6410736300791,-1.21419340158199,
49.99988982678));
#154213=CARTESIAN_POINT('Ctrl Pts',(85.2906386456891,-1.19339881491799,
51.02156561606));
#154214=CARTESIAN_POINT('Ctrl Pts',(87.2173778492491,-1.21624717379899,
52.64366771246));
#154215=CARTESIAN_POINT('Ctrl Pts',(89.7219899406691,-1.35749773631899,
52.89343266706));
#154216=CARTESIAN_POINT('Ctrl Pts',(90.8953710962691,-1.44502606200399,
52.65421569171));
#154217=CARTESIAN_POINT('Ctrl Pts',(84.6255050281691,0.153010053497514,
50.00242696498));
#154218=CARTESIAN_POINT('Ctrl Pts',(85.2742834368191,0.150394585033814,
51.02589223615));
#154219=CARTESIAN_POINT('Ctrl Pts',(87.2007679081091,0.153286082122214,
52.6521963776));
#154220=CARTESIAN_POINT('Ctrl Pts',(89.7065985576691,0.171098155476114,
52.90507996211));
#154221=CARTESIAN_POINT('Ctrl Pts',(90.8804761688691,0.182133423763114,
52.66684715676));
#154222=CARTESIAN_POINT('',(84.7089070649894,1.43647443565002E-14,50.1287872718967));
#154223=CARTESIAN_POINT('Ctrl Pts',(84.7089070652226,1.4432899320127E-14,
50.1287872722712));
#154224=CARTESIAN_POINT('Ctrl Pts',(84.7089070652227,-0.620790188952753,
50.1287872722712));
#154225=CARTESIAN_POINT('Ctrl Pts',(84.6654155304985,-1.23992630038833,
50.1364560032405));
#154226=CARTESIAN_POINT('Ctrl Pts',(84.4910143635045,-2.4687340790315,50.1672076344486));
#154227=CARTESIAN_POINT('Ctrl Pts',(84.3605401866984,-3.07529560408347,
50.1902137521402));
#154228=CARTESIAN_POINT('Ctrl Pts',(84.187928507386,-3.67076904714443,50.2206498483884));
#154229=CARTESIAN_POINT('Ctrl Pts',(84.7089070650127,1.42110872006939E-14,
50.1287872718807));
#154230=CARTESIAN_POINT('Ctrl Pts',(85.3559684191721,2.23742947452393E-14,
51.0930107907251));
#154231=CARTESIAN_POINT('Ctrl Pts',(87.2135596094279,-5.0029901016169E-14,
52.6236276843951));
#154232=CARTESIAN_POINT('Ctrl Pts',(89.6030123367996,7.09023504723426E-15,
52.8932693059995));
#154233=CARTESIAN_POINT('Ctrl Pts',(90.7329496419691,1.4210854715202E-14,
52.69425954596));
#154234=CARTESIAN_POINT('Ctrl Pts',(84.6207906093291,-0.152011227331786,
49.99508307661));
#154235=CARTESIAN_POINT('Ctrl Pts',(85.9974652801591,-0.146440090307486,
52.16989344765));
#154236=CARTESIAN_POINT('Ctrl Pts',(88.3653709583691,-0.157188198121986,
53.17894399659));
#154237=CARTESIAN_POINT('Ctrl Pts',(90.8875370260691,-0.180457446103386,
52.6654408377301));
#154238=CARTESIAN_POINT('Ctrl Pts',(84.6361601793791,1.20741070204101,49.9925779501701));
#154239=CARTESIAN_POINT('Ctrl Pts',(86.0144572373891,1.16275390045801,52.1633314201001));
#154240=CARTESIAN_POINT('Ctrl Pts',(88.3816214943691,1.24781582637001,53.16836818009));
#154241=CARTESIAN_POINT('Ctrl Pts',(90.9023154006691,1.43258709002601,52.65289559471));
#154242=CARTESIAN_POINT('Ctrl Pts',(84.4452429771191,2.54236893826101,50.02365025392));
#154243=CARTESIAN_POINT('Ctrl Pts',(85.8028873051391,2.45960847280301,52.24550138407));
#154244=CARTESIAN_POINT('Ctrl Pts',(88.1793852807691,2.64702290766801,53.30037093943));
#154245=CARTESIAN_POINT('Ctrl Pts',(90.7196837319691,3.03719723761501,52.80858638915));
#154246=CARTESIAN_POINT('Ctrl Pts',(84.0625947609391,3.82278043910101,50.08710134634));
#154247=CARTESIAN_POINT('Ctrl Pts',(85.3805449859791,3.66255118679801,52.39269601302));
#154248=CARTESIAN_POINT('Ctrl Pts',(87.7577840179691,3.95799738650802,53.55053860319));
#154249=CARTESIAN_POINT('Ctrl Pts',(90.3052323644691,4.59865127728601,53.12745538062));
#154250=CARTESIAN_POINT('',(84.1879285286622,3.67076919515978,50.2206498311393));
#154251=CARTESIAN_POINT('Ctrl Pts',(84.1879285683743,3.67076920633965,50.2206498376345));
#154252=CARTESIAN_POINT('Ctrl Pts',(84.3605360711567,3.07533070753628,50.1902144778213));
#154253=CARTESIAN_POINT('Ctrl Pts',(84.4909881059739,2.46873053153842,50.1672122643816));
#154254=CARTESIAN_POINT('Ctrl Pts',(84.6653784517624,1.23999491019598,50.136462541244));
#154255=CARTESIAN_POINT('Ctrl Pts',(84.7089070652242,0.620754149608006,
50.1287872722709));
#154256=CARTESIAN_POINT('Ctrl Pts',(84.7089070652245,1.30451205393456E-14,
50.1287872722709));
#154257=CARTESIAN_POINT('Ctrl Pts',(84.187928567227,3.67076914922564,50.2206498048453));
#154258=CARTESIAN_POINT('Ctrl Pts',(84.2524098516593,3.6645515876862,50.3260846691099));
#154259=CARTESIAN_POINT('Ctrl Pts',(84.3206795773437,3.65929251149661,50.4306354818293));
#154260=CARTESIAN_POINT('Ctrl Pts',(84.3927259892234,3.6550621788536,50.5339131962136));
#154261=CARTESIAN_POINT('Ctrl Pts',(84.464074555574,3.65087282144648,50.6361905569458));
#154262=CARTESIAN_POINT('Ctrl Pts',(84.5391271491909,3.64769249978238,50.7372188628749));
#154263=CARTESIAN_POINT('Ctrl Pts',(84.6178234087269,3.64558114180426,50.8366098849484));
#154264=CARTESIAN_POINT('Ctrl Pts',(84.695845306457,3.64348787641641,50.9351492082304));
#154265=CARTESIAN_POINT('Ctrl Pts',(84.7774487528274,3.64244544419323,51.0320786615377));
#154266=CARTESIAN_POINT('Ctrl Pts',(84.8625250016019,3.64250228307859,51.1270172861643));
#154267=CARTESIAN_POINT('Ctrl Pts',(84.9469679163454,3.64255869883762,51.2212491581695));
#154268=CARTESIAN_POINT('Ctrl Pts',(85.0348320906405,3.64369817408329,51.3135191948001));
#154269=CARTESIAN_POINT('Ctrl Pts',(85.125961546269,3.6459566841249,51.4034602027465));
#154270=CARTESIAN_POINT('Ctrl Pts',(85.2165158259445,3.64820093927323,51.492833535789));
#154271=CARTESIAN_POINT('Ctrl Pts',(85.310294175703,3.65155022151192,51.5799066160371));
#154272=CARTESIAN_POINT('Ctrl Pts',(85.4070954772706,3.65602728794667,51.6643324012192));
#154273=CARTESIAN_POINT('Ctrl Pts',(85.5033958194257,3.66048118497632,51.7483212719069));
#154274=CARTESIAN_POINT('Ctrl Pts',(85.6026876928605,3.6660512739478,51.829689668403));
#154275=CARTESIAN_POINT('Ctrl Pts',(85.7047278508454,3.67274657976675,51.9081168229286));
#154276=CARTESIAN_POINT('Ctrl Pts',(85.8062983199339,3.67941106722102,51.9861829787612));
#154277=CARTESIAN_POINT('Ctrl Pts',(85.910591529777,3.68719046054209,52.0613344418456));
#154278=CARTESIAN_POINT('Ctrl Pts',(86.0173264830788,3.69607981140521,52.1332829125085));
#154279=CARTESIAN_POINT('Ctrl Pts',(86.1237629157328,3.70494430017116,52.2050301547695));
#154280=CARTESIAN_POINT('Ctrl Pts',(86.2326270796844,3.71491254565264,52.2735918823881));
#154281=CARTESIAN_POINT('Ctrl Pts',(86.3436044015489,3.72596565800079,52.3387167704167));
#154282=CARTESIAN_POINT('Ctrl Pts',(86.4544400082225,3.73700465580824,52.4037584956353));
#154283=CARTESIAN_POINT('Ctrl Pts',(86.5673829426877,3.74912572526539,52.4653718046733));
#154284=CARTESIAN_POINT('Ctrl Pts',(86.6820900106887,3.76229627959937,52.5233465895402));
#154285=CARTESIAN_POINT('Ctrl Pts',(86.796767633063,3.77546345301504,52.5813064921169));
#154286=CARTESIAN_POINT('Ctrl Pts',(86.9132079937252,3.78967952021909,52.635629469868));
#154287=CARTESIAN_POINT('Ctrl Pts',(87.0310452881542,3.8048987359492,52.6861504842319));
#154288=CARTESIAN_POINT('Ctrl Pts',(87.1497257202048,3.82022684668929,52.7370329815041));
#154289=CARTESIAN_POINT('Ctrl Pts',(87.2698226260638,3.83657244725239,52.78405867872));
#154290=CARTESIAN_POINT('Ctrl Pts',(87.3909466918256,3.85387629261818,52.8271084253288));
#154291=CARTESIAN_POINT('Ctrl Pts',(87.5116929092281,3.87112615837604,52.8700238776003));
#154292=CARTESIAN_POINT('Ctrl Pts',(87.6334593284,3.88932819055397,52.9089881038916));
#154293=CARTESIAN_POINT('Ctrl Pts',(87.7558530000194,3.90841265468426,52.9439339994195));
#154294=CARTESIAN_POINT('Ctrl Pts',(87.878902380451,3.92759936144802,52.9790671132189));
#154295=CARTESIAN_POINT('Ctrl Pts',(88.0025851964464,3.94767786548767,53.0101387184408));
#154296=CARTESIAN_POINT('Ctrl Pts',(88.1265031900006,3.96856779516172,53.0371326720082));
#154297=CARTESIAN_POINT('Ctrl Pts',(88.2502576305924,3.98943015329604,53.0640909976498));
#154298=CARTESIAN_POINT('Ctrl Pts',(88.374246106134,4.0111016583654,53.0869825826451));
#154299=CARTESIAN_POINT('Ctrl Pts',(88.4980810843336,4.03349472027891,53.105841917296));
#154300=CARTESIAN_POINT('Ctrl Pts',(88.6231846835399,4.05611718675291,53.1248944554218));
#154301=CARTESIAN_POINT('Ctrl Pts',(88.7481309294624,4.0794758611196,53.1398318319754));
#154302=CARTESIAN_POINT('Ctrl Pts',(88.872537677615,4.1034745768986,53.1507390052145));
#154303=CARTESIAN_POINT('Ctrl Pts',(88.9982633132582,4.12772771300853,53.161761809917));
#154304=CARTESIAN_POINT('Ctrl Pts',(89.1234374712175,4.15263438431025,53.1686687657082));
#154305=CARTESIAN_POINT('Ctrl Pts',(89.2476908452341,4.17809178994324,53.1715945389227));
#154306=CARTESIAN_POINT('Ctrl Pts',(89.3727499613135,4.20371427843767,53.1745392848095));
#154307=CARTESIAN_POINT('Ctrl Pts',(89.4968759177392,4.22989451437176,53.1734514224341));
#154308=CARTESIAN_POINT('Ctrl Pts',(89.6197241169299,4.25652640758112,53.1685107305081));
#154309=CARTESIAN_POINT('Ctrl Pts',(89.7440298219647,4.28347426911763,53.1635114208131));
#154310=CARTESIAN_POINT('Ctrl Pts',(89.8670269216465,4.31088441821633,53.1545677316536));
#154311=CARTESIAN_POINT('Ctrl Pts',(89.9883967134665,4.33864794789005,53.1419033128201));
#154312=CARTESIAN_POINT('Ctrl Pts',(90.0577546357967,4.35451368108318,53.1346661101798));
#154313=CARTESIAN_POINT('Ctrl Pts',(90.1265818674342,4.3704948477379,53.1262144940036));
#154314=CARTESIAN_POINT('Ctrl Pts',(90.1948250300408,4.38657154635619,53.1165947501917));
#154315=CARTESIAN_POINT('Ctrl Pts',(84.1478916908791,3.53084617379201,50.07617289185));
#154316=CARTESIAN_POINT('Ctrl Pts',(85.4750404242492,3.38611454775601,52.35990944625));
#154317=CARTESIAN_POINT('Ctrl Pts',(87.8496043814691,3.65643304604401,53.49395859461));
#154318=CARTESIAN_POINT('Ctrl Pts',(90.3922895163691,4.24172967370401,53.05823942373));
#154319=CARTESIAN_POINT('Ctrl Pts',(83.5684103616991,5.64263664564902,50.17212144973));
#154320=CARTESIAN_POINT('Ctrl Pts',(84.8253303192091,5.41333805546702,52.58956324423));
#154321=CARTESIAN_POINT('Ctrl Pts',(87.2025717175191,5.86327918692001,53.88058185588));
#154322=CARTESIAN_POINT('Ctrl Pts',(89.7702498546691,6.81650413436202,53.5400188389));
#154323=CARTESIAN_POINT('Ctrl Pts',(82.4965671836292,7.51960021670801,50.3516900304801));
#154324=CARTESIAN_POINT('Ctrl Pts',(83.6066894758891,7.10528059197901,52.9844159722199));
#154325=CARTESIAN_POINT('Ctrl Pts',(85.9445157806491,7.76009296512003,54.5885582561201));
#154326=CARTESIAN_POINT('Ctrl Pts',(88.5134190995691,9.20496137042702,54.4800726227));
#154327=CARTESIAN_POINT('Ctrl Pts',(81.0891963680291,9.033815381809,50.59494971387));
#154328=CARTESIAN_POINT('Ctrl Pts',(82.0665861402791,8.36191540094801,53.36419282181));
#154329=CARTESIAN_POINT('Ctrl Pts',(84.2071635732892,9.16226600288201,55.32711634851));
#154330=CARTESIAN_POINT('Ctrl Pts',(86.5272818095892,11.0672006189,55.58150421395));
#154331=CARTESIAN_POINT('',(81.2459147097091,8.89165945465101,50.73940625854));
#154332=CARTESIAN_POINT('Ctrl Pts',(81.2459147097075,8.89165945465026,50.7394062585356));
#154333=CARTESIAN_POINT('Ctrl Pts',(81.9196419748508,8.16199632308235,50.6206099640519));
#154334=CARTESIAN_POINT('Ctrl Pts',(82.508629049238,7.35516112537247,50.5167556515489));
#154335=CARTESIAN_POINT('Ctrl Pts',(83.5044460856509,5.5997346190605,50.3411662401802));
#154336=CARTESIAN_POINT('Ctrl Pts',(83.902684616162,4.65479953785456,50.2709460424934));
#154337=CARTESIAN_POINT('Ctrl Pts',(84.1879284697861,3.67076917687268,50.2206498550183));
#154338=CARTESIAN_POINT('',(86.5280866410291,10.82949410859,55.48972649734));
#154339=CARTESIAN_POINT('Origin',(85.5564936082272,12.9954596346064,49.979318101201));
#154340=CARTESIAN_POINT('Ctrl Pts',(90.1948181095954,4.38657743647023,53.1165555002035));
#154341=CARTESIAN_POINT('Ctrl Pts',(90.1359031779921,4.61710858188133,53.1615437195885));
#154342=CARTESIAN_POINT('Ctrl Pts',(90.0722973819612,4.84441445094358,53.2098399585012));
#154343=CARTESIAN_POINT('Ctrl Pts',(90.0040341246653,5.06851243131367,53.261143072422));
#154344=CARTESIAN_POINT('Ctrl Pts',(89.9344459738422,5.2969598373542,53.3134419074121));
#154345=CARTESIAN_POINT('Ctrl Pts',(89.8600178886679,5.52207399296512,53.3688657860787));
#154346=CARTESIAN_POINT('Ctrl Pts',(89.7807494466665,5.74386776536395,53.4271359386309));
#154347=CARTESIAN_POINT('Ctrl Pts',(89.6995809044398,5.97097803429376,53.4868028529611));
#154348=CARTESIAN_POINT('Ctrl Pts',(89.6133372662829,6.19460721382888,53.5494544411179));
#154349=CARTESIAN_POINT('Ctrl Pts',(89.5219795893552,6.41475756038536,53.6148284024007));
#154350=CARTESIAN_POINT('Ctrl Pts',(89.4296437898062,6.63726495061136,53.680902291183));
#154351=CARTESIAN_POINT('Ctrl Pts',(89.3320838593223,6.85621896990238,53.7497575573331));
#154352=CARTESIAN_POINT('Ctrl Pts',(89.2292201379769,7.07160469119592,53.8211552001164));
#154353=CARTESIAN_POINT('Ctrl Pts',(89.1252501823817,7.28930674966545,53.8933206793805));
#154354=CARTESIAN_POINT('Ctrl Pts',(89.0158617365942,7.50336369899101,53.9680839167634));
#154355=CARTESIAN_POINT('Ctrl Pts',(88.900932501327,7.71373724533197,54.0452243608646));
#154356=CARTESIAN_POINT('Ctrl Pts',(88.867122648076,7.77562488178179,54.0679175171248));
#154357=CARTESIAN_POINT('Ctrl Pts',(88.8328330245806,7.83719358179163,54.0908165501825));
#154358=CARTESIAN_POINT('Ctrl Pts',(88.7980598701763,7.89844193170923,54.1139161922911));
#154359=CARTESIAN_POINT('Ctrl Pts',(88.6794829077388,8.10729969603818,54.1926863079607));
#154360=CARTESIAN_POINT('Ctrl Pts',(88.555284664877,8.31251142837422,54.273809043917));
#154361=CARTESIAN_POINT('Ctrl Pts',(88.4255283010071,8.51406415544969,54.3570702991699));
#154362=CARTESIAN_POINT('Ctrl Pts',(88.2912330438266,8.72266722130921,54.4432440432073));
#154363=CARTESIAN_POINT('Ctrl Pts',(88.1509845932116,8.92735105379942,54.531708338956));
#154364=CARTESIAN_POINT('Ctrl Pts',(88.004809584826,9.12811582839587,54.6222639722302));
#154365=CARTESIAN_POINT('Ctrl Pts',(87.8675534157416,9.31663097987456,54.7072943714037));
#154366=CARTESIAN_POINT('Ctrl Pts',(87.7250717523547,9.50169110207378,54.7941690553451));
#154367=CARTESIAN_POINT('Ctrl Pts',(87.5773466870284,9.68330413920943,54.8827538765666));
#154368=CARTESIAN_POINT('Ctrl Pts',(87.4318396847443,9.86219029201598,54.970008613976));
#154369=CARTESIAN_POINT('Ctrl Pts',(87.2812458092384,10.0377323720386,55.0589226290465));
#154370=CARTESIAN_POINT('Ctrl Pts',(87.1255062609115,10.2099411783719,55.1493954830942));
#154371=CARTESIAN_POINT('Ctrl Pts',(86.9737396511167,10.3777569130057,55.2375603614748));
#154372=CARTESIAN_POINT('Ctrl Pts',(86.8170867506117,10.5424075120072,55.3272057084067));
#154373=CARTESIAN_POINT('Ctrl Pts',(86.6554500841697,10.7039022560808,55.4182631789919));
#154374=CARTESIAN_POINT('Ctrl Pts',(86.6133349353838,10.7459804263656,55.4419886059397));
#154375=CARTESIAN_POINT('Ctrl Pts',(86.5708812042372,10.7878443356175,55.4658100262816));
#154376=CARTESIAN_POINT('Ctrl Pts',(86.5280866409046,10.8294941088676,55.4897264966337));
#154377=CARTESIAN_POINT('Origin',(62.4468966735091,1.4210854715202E-14,
88.14465325204));
#154378=CARTESIAN_POINT('Ctrl Pts',(86.5280866409038,10.8294941088694,55.4897264966292));
#154379=CARTESIAN_POINT('Ctrl Pts',(86.2192234645901,11.1262539163102,55.6608302285934));
#154380=CARTESIAN_POINT('Ctrl Pts',(85.8993943954668,11.4103793028112,55.834389069437));
#154381=CARTESIAN_POINT('Ctrl Pts',(85.5684108187881,11.6821583926022,56.0094180282724));
#154382=CARTESIAN_POINT('Ctrl Pts',(85.236282045607,11.9548778325644,56.1850525837767));
#154383=CARTESIAN_POINT('Ctrl Pts',(84.8929214481348,12.2151653713604,56.3621674570628));
#154384=CARTESIAN_POINT('Ctrl Pts',(84.5381644255921,12.4633103428954,56.5398130503948));
#154385=CARTESIAN_POINT('Ctrl Pts',(84.2960248581174,12.632681806349,56.6610651311145));
#154386=CARTESIAN_POINT('Ctrl Pts',(84.0485765193537,12.7963963136241,56.7825654090797));
#154387=CARTESIAN_POINT('Ctrl Pts',(83.7957739555192,12.9545454545498,56.9040240348704));
#154388=CARTESIAN_POINT('Ctrl Pts',(83.7470466955891,13.16496437151,57.01321783994));
#154389=CARTESIAN_POINT('Ctrl Pts',(81.9865745665792,11.20483377632,56.44317770796));
#154390=CARTESIAN_POINT('Ctrl Pts',(80.2870696161591,10.2783422501,54.56706441941));
#154391=CARTESIAN_POINT('Ctrl Pts',(79.2983120731091,10.73979194701,52.10208288917));
#154392=CARTESIAN_POINT('Ctrl Pts',(84.8757367991591,12.47994051502,56.47442870884));
#154393=CARTESIAN_POINT('Ctrl Pts',(82.9214873293092,10.52306401839,56.00723818309));
#154394=CARTESIAN_POINT('Ctrl Pts',(81.0536773160091,9.63724577777001,54.11455269465));
#154395=CARTESIAN_POINT('Ctrl Pts',(80.0323112249891,10.18300062511,51.56638252406));
#154396=CARTESIAN_POINT('Ctrl Pts',(85.8869149987391,11.69588976861,55.93978781814));
#154397=CARTESIAN_POINT('Ctrl Pts',(83.7306334675291,9.76298109352201,55.59306759372));
#154398=CARTESIAN_POINT('Ctrl Pts',(81.7043087692891,8.92499334384901,53.67821991044));
#154399=CARTESIAN_POINT('Ctrl Pts',(80.6864897900991,9.54533591150901,51.02532279134));
#154400=CARTESIAN_POINT('Ctrl Pts',(86.7932195329291,10.81129024407,55.4328529836));
#154401=CARTESIAN_POINT('Ctrl Pts',(84.4310620883791,8.94679575809301,55.2212052233701));
#154402=CARTESIAN_POINT('Ctrl Pts',(82.2565980756691,8.16465088581602,53.28182981116));
#154403=CARTESIAN_POINT('Ctrl Pts',(81.2714577963691,8.82522553066502,50.50790307768));
#154404=CARTESIAN_POINT('',(79.4586835372191,10.63636346571,52.1735219594));
#154405=CARTESIAN_POINT('Ctrl Pts',(79.4586835372178,10.636363465708,52.1735219594002));
#154406=CARTESIAN_POINT('Ctrl Pts',(79.6814480592509,10.4618582038496,52.0068337685839));
#154407=CARTESIAN_POINT('Ctrl Pts',(79.8981916511604,10.2786530461329,51.8412072301974));
#154408=CARTESIAN_POINT('Ctrl Pts',(80.1083296642254,10.0871970340296,51.6767454335844));
#154409=CARTESIAN_POINT('Ctrl Pts',(80.3184778117459,9.89573178845914,51.5122757053708));
#154410=CARTESIAN_POINT('Ctrl Pts',(80.5220195569677,9.69601504589331,51.3489708641279));
#154411=CARTESIAN_POINT('Ctrl Pts',(80.7184025534926,9.48853636538811,51.1869283034285));
#154412=CARTESIAN_POINT('Ctrl Pts',(80.9005351179808,9.29611326957157,51.036644278545));
#154413=CARTESIAN_POINT('Ctrl Pts',(81.0765103968599,9.09701435659084,50.8874459492423));
#154414=CARTESIAN_POINT('Ctrl Pts',(81.2459147097113,8.89165945465309,50.7394062585396));
#154415=CARTESIAN_POINT('Origin',(82.8560309932748,15.5454545438535,51.5744768443036));
#154416=CARTESIAN_POINT('Ctrl Pts',(62.0004995106591,12.99512036681,60.76331727853));
#154417=CARTESIAN_POINT('Ctrl Pts',(62.3484151888391,12.54693837639,60.50916986639));
#154418=CARTESIAN_POINT('Ctrl Pts',(63.0241629615191,11.7184431647,59.82306248213));
#154419=CARTESIAN_POINT('Ctrl Pts',(63.8765759553791,10.82009029682,58.28505757651));
#154420=CARTESIAN_POINT('Ctrl Pts',(64.4468273418191,10.39648861975,56.44321515656));
#154421=CARTESIAN_POINT('Ctrl Pts',(64.5904299294691,10.4635207436,55.18330241512));
#154422=CARTESIAN_POINT('Ctrl Pts',(64.6070531255991,10.57285133752,54.5719498575));
#154423=CARTESIAN_POINT('Ctrl Pts',(62.8738787862491,13.34120049567,60.78022792604));
#154424=CARTESIAN_POINT('Ctrl Pts',(63.1822305202591,12.90294209037,60.5099756716));
#154425=CARTESIAN_POINT('Ctrl Pts',(63.7770649543591,12.1013057401,59.81041242578));
#154426=CARTESIAN_POINT('Ctrl Pts',(64.5300373719591,11.23972064165,58.3139231133));
#154427=CARTESIAN_POINT('Ctrl Pts',(65.0503358198691,10.82877473085,56.55225383024));
#154428=CARTESIAN_POINT('Ctrl Pts',(65.2012342447591,10.8858670493,55.34630444955));
#154429=CARTESIAN_POINT('Ctrl Pts',(65.2297183008891,10.98810527869,54.75706052086));
#154430=CARTESIAN_POINT('Ctrl Pts',(64.6173646454791,13.91964486995,60.81724029466));
#154431=CARTESIAN_POINT('Ctrl Pts',(64.8539957800591,13.50761079116,60.52480603628));
#154432=CARTESIAN_POINT('Ctrl Pts',(65.3044272586691,12.7658907333,59.81500178811));
#154433=CARTESIAN_POINT('Ctrl Pts',(65.8761188231091,11.97266212857,58.40496801144));
#154434=CARTESIAN_POINT('Ctrl Pts',(66.2901879471691,11.57564099905,56.79084865574));
#154435=CARTESIAN_POINT('Ctrl Pts',(66.4342112984491,11.60238669822,55.68422263389));
#154436=CARTESIAN_POINT('Ctrl Pts',(66.4735315517891,11.68373610128,55.13673945242));
#154437=CARTESIAN_POINT('Ctrl Pts',(66.9537378663991,14.43965128121,60.80229592221));
#154438=CARTESIAN_POINT('Ctrl Pts',(67.1059017220291,14.06465275777,60.49986220292));
#154439=CARTESIAN_POINT('Ctrl Pts',(67.3904875602491,13.39597478951,59.8028885254));
#154440=CARTESIAN_POINT('Ctrl Pts',(67.7457964768791,12.67217006629,58.49957041475));
#154441=CARTESIAN_POINT('Ctrl Pts',(68.0042996574791,12.27885104909,57.04241969021));
#154442=CARTESIAN_POINT('Ctrl Pts',(68.0982333239291,12.2605680305,56.04212739625));
#154443=CARTESIAN_POINT('Ctrl Pts',(68.1256989419291,12.31045564282,55.5415397163));
#154444=CARTESIAN_POINT('Ctrl Pts',(68.8615884801891,14.73391374,60.71525424851));
#154445=CARTESIAN_POINT('Ctrl Pts',(68.9505522591391,14.38230171041,60.41285306216));
#154446=CARTESIAN_POINT('Ctrl Pts',(69.1116523776291,13.757827987,59.73423461933));
#154447=CARTESIAN_POINT('Ctrl Pts',(69.2990975194291,13.07397037489,58.5050230397));
#154448=CARTESIAN_POINT('Ctrl Pts',(69.4218122528991,12.68142066446,57.14796983335));
#154449=CARTESIAN_POINT('Ctrl Pts',(69.4544054525091,12.63506048891,56.21515507744));
#154450=CARTESIAN_POINT('Ctrl Pts',(69.4585163840591,12.66496377676,55.74504300061));
#154451=CARTESIAN_POINT('Ctrl Pts',(70.3199244149591,14.8934563637,60.60196156239));
#154452=CARTESIAN_POINT('Ctrl Pts',(70.3622226318591,14.55550964164,60.30258402178));
#154453=CARTESIAN_POINT('Ctrl Pts',(70.4323841024791,13.95625819437,59.63983876568));
#154454=CARTESIAN_POINT('Ctrl Pts',(70.4936475173591,13.29449480622,58.45887251135));
#154455=CARTESIAN_POINT('Ctrl Pts',(70.5087618416291,12.90182964092,57.16333911074));
#154456=CARTESIAN_POINT('Ctrl Pts',(70.4868595127791,12.83911853561,56.27171241897));
#154457=CARTESIAN_POINT('Ctrl Pts',(70.4680271458191,12.85728762685,55.82047504651));
#154458=CARTESIAN_POINT('Ctrl Pts',(71.7987422768891,14.99086818853,60.43452023613));
#154459=CARTESIAN_POINT('Ctrl Pts',(71.7945134349491,14.66200007839,60.1408313857));
#154460=CARTESIAN_POINT('Ctrl Pts',(71.7740644540591,14.07915129287,59.4952138796));
#154461=CARTESIAN_POINT('Ctrl Pts',(71.7076177012891,13.431302473,58.35395694307));
#154462=CARTESIAN_POINT('Ctrl Pts',(71.6100179060791,13.03810819612,57.10504669817));
#154463=CARTESIAN_POINT('Ctrl Pts',(71.5272163969991,12.96445387057,56.24374012316));
#154464=CARTESIAN_POINT('Ctrl Pts',(71.4814488769991,12.97474890777,55.80644597183));
#154465=CARTESIAN_POINT('Ctrl Pts',(73.2930854931491,15.02379049898,60.2047823183));
#154466=CARTESIAN_POINT('Ctrl Pts',(73.2424014846691,14.69834531273,59.91874182595));
#154467=CARTESIAN_POINT('Ctrl Pts',(73.1310672232491,14.1215596745,59.29009412364));
#154468=CARTESIAN_POINT('Ctrl Pts',(72.9343064335891,13.47866908886,58.17821655064));
#154469=CARTESIAN_POINT('Ctrl Pts',(72.7187593877691,13.0850525524,56.95946733291));
#154470=CARTESIAN_POINT('Ctrl Pts',(72.5697495755391,13.00718824553,56.11649390454));
#154471=CARTESIAN_POINT('Ctrl Pts',(72.4939506799091,13.01446680747,55.68758245596));
#154472=CARTESIAN_POINT('Ctrl Pts',(74.7760924715591,14.99006392631,59.90876923216));
#154473=CARTESIAN_POINT('Ctrl Pts',(74.6791154758791,14.6611250522,59.63145247883));
#154474=CARTESIAN_POINT('Ctrl Pts',(74.4765218789691,14.07814838366,59.01793837054));
#154475=CARTESIAN_POINT('Ctrl Pts',(74.1471817304391,13.43019013293,57.92289494906));
#154476=CARTESIAN_POINT('Ctrl Pts',(73.8104278418891,13.03699746573,56.71593880071));
#154477=CARTESIAN_POINT('Ctrl Pts',(73.5929209354791,12.96342646928,55.87822777989));
#154478=CARTESIAN_POINT('Ctrl Pts',(73.4860391363291,12.97378221592,55.45163611742));
#154479=CARTESIAN_POINT('Ctrl Pts',(76.7044063444491,14.85944831897,59.44380402476));
#154480=CARTESIAN_POINT('Ctrl Pts',(76.5465454282191,14.51834940535,59.18064936834));
#154481=CARTESIAN_POINT('Ctrl Pts',(76.2226196326491,13.91339295952,58.58707694282));
#154482=CARTESIAN_POINT('Ctrl Pts',(75.7151848286191,13.24677567487,57.50045084188));
#154483=CARTESIAN_POINT('Ctrl Pts',(75.2160126877391,12.85427967805,56.28626050506));
#154484=CARTESIAN_POINT('Ctrl Pts',(74.9084550047991,12.79536407084,55.43812812318));
#154485=CARTESIAN_POINT('Ctrl Pts',(74.7615129102391,12.81626401359,55.00624381423));
#154486=CARTESIAN_POINT('Ctrl Pts',(79.0212442118191,14.53891337949,58.75036910218));
#154487=CARTESIAN_POINT('Ctrl Pts',(78.7892444029591,14.17098221515,58.51098616624));
#154488=CARTESIAN_POINT('Ctrl Pts',(78.3138871646991,13.51623522621,57.94498183631));
#154489=CARTESIAN_POINT('Ctrl Pts',(77.5798288055491,12.80566305584,56.84689608258));
#154490=CARTESIAN_POINT('Ctrl Pts',(76.8765234961291,12.41304472226,55.58403161918));
#154491=CARTESIAN_POINT('Ctrl Pts',(76.4619642118191,12.38616952145,54.69194034387));
#154492=CARTESIAN_POINT('Ctrl Pts',(76.2700805142791,12.43005186544,54.23853783461));
#154493=CARTESIAN_POINT('Ctrl Pts',(81.6411285163391,13.91879763618,57.81488153531));
#154494=CARTESIAN_POINT('Ctrl Pts',(81.3186866959591,13.50671310406,57.62104900824));
#154495=CARTESIAN_POINT('Ctrl Pts',(80.6525048798091,12.76489017188,57.10813696619));
#154496=CARTESIAN_POINT('Ctrl Pts',(79.6327931869791,11.97156082259,55.97859517806));
#154497=CARTESIAN_POINT('Ctrl Pts',(78.6914485145091,11.57453512392,54.60328680704));
#154498=CARTESIAN_POINT('Ctrl Pts',(78.1775730190191,11.60134676736,53.61254574674));
#154499=CARTESIAN_POINT('Ctrl Pts',(77.9533720747691,11.68274103777,53.11147989974));
#154500=CARTESIAN_POINT('Ctrl Pts',(83.2655200870691,13.34106036443,57.18456850277));
#154501=CARTESIAN_POINT('Ctrl Pts',(82.8833134367491,12.9028007288,57.03609161983));
#154502=CARTESIAN_POINT('Ctrl Pts',(82.0850474434891,12.10115904569,56.5821847924));
#154503=CARTESIAN_POINT('Ctrl Pts',(80.8656007901591,11.23956517827,55.43348238283));
#154504=CARTESIAN_POINT('Ctrl Pts',(79.7741175750391,10.82861619709,53.95598877582));
#154505=CARTESIAN_POINT('Ctrl Pts',(79.2198542235591,10.88571082207,52.87435581621));
#154506=CARTESIAN_POINT('Ctrl Pts',(78.9915557177591,10.98795046753,52.33037867278));
#154507=CARTESIAN_POINT('Ctrl Pts',(84.0802735036491,12.99502442972,56.87000858129));
#154508=CARTESIAN_POINT('Ctrl Pts',(83.6664085766591,12.54683897575,56.7501897856));
#154509=CARTESIAN_POINT('Ctrl Pts',(82.7967330268891,11.7183348805,56.33658924635));
#154510=CARTESIAN_POINT('Ctrl Pts',(81.4696701551291,10.81997022647,55.18287676723));
#154511=CARTESIAN_POINT('Ctrl Pts',(80.3038420682091,10.39636449694,53.64713106238));
#154512=CARTESIAN_POINT('Ctrl Pts',(79.7379809787491,10.46339979819,52.5123003413));
#154513=CARTESIAN_POINT('Ctrl Pts',(79.5132662898991,10.57273271432,51.94349552833));
#154514=CARTESIAN_POINT('',(64.7368422516391,10.63636348946,54.76937963139));
#154515=CARTESIAN_POINT('Ctrl Pts',(64.7368422516391,10.63636348946,54.76937963139));
#154516=CARTESIAN_POINT('Ctrl Pts',(65.022905497685,10.8242034905186,54.8523998297597));
#154517=CARTESIAN_POINT('Ctrl Pts',(65.3163021676567,11.0019622800467,54.9362150309343));
#154518=CARTESIAN_POINT('Ctrl Pts',(65.7662463233778,11.2527215428607,55.0633332866357));
#154519=CARTESIAN_POINT('Ctrl Pts',(65.9936798000631,11.3741328145859,55.1272414347024));
#154520=CARTESIAN_POINT('Ctrl Pts',(66.2630656334176,11.5086838386383,55.2024576894393));
#154521=CARTESIAN_POINT('Ctrl Pts',(66.3987370417595,11.5741677613214,55.240235858494));
#154522=CARTESIAN_POINT('Ctrl Pts',(66.4668132034811,11.6064596423542,55.2591681879092));
#154523=CARTESIAN_POINT('Ctrl Pts',(66.4960397799691,11.6202023435858,55.2672913891309));
#154524=CARTESIAN_POINT('Ctrl Pts',(66.5155354652189,11.6293426353479,55.2727089422419));
#154525=CARTESIAN_POINT('Ctrl Pts',(66.5271030932093,11.6347475761856,55.2759226880298));
#154526=CARTESIAN_POINT('Ctrl Pts',(66.6621678159956,11.6976998452844,55.3134406708803));
#154527=CARTESIAN_POINT('Ctrl Pts',(66.8120554320327,11.765571891373,55.3525214465694));
#154528=CARTESIAN_POINT('Ctrl Pts',(67.0725028555396,11.876831289836,55.4165390344623));
#154529=CARTESIAN_POINT('Ctrl Pts',(67.1652573264087,11.9154812671251,55.4387771649057));
#154530=CARTESIAN_POINT('Ctrl Pts',(67.313495201512,11.9752576396986,55.4734478188224));
#154531=CARTESIAN_POINT('Ctrl Pts',(67.3898907667822,12.0055950222634,55.4911114952644));
#154532=CARTESIAN_POINT('Ctrl Pts',(67.483046702591,12.0416433895335,55.5122860277984));
#154533=CARTESIAN_POINT('Ctrl Pts',(67.5306370460269,12.0598139073292,55.5230140638589));
#154534=CARTESIAN_POINT('Ctrl Pts',(67.5512504241072,12.0676307471877,55.5276418564625));
#154535=CARTESIAN_POINT('Ctrl Pts',(67.5650410773529,12.0728483120871,55.5307337208534));
#154536=CARTESIAN_POINT('Ctrl Pts',(67.5738804142658,12.076183262624,55.5327122491806));
#154537=CARTESIAN_POINT('Ctrl Pts',(67.7396707699348,12.1386197781047,55.5697822842124));
#154538=CARTESIAN_POINT('Ctrl Pts',(67.893521150259,12.1933590009703,55.602455627199));
#154539=CARTESIAN_POINT('Ctrl Pts',(68.1133369846499,12.2679083379962,55.6466588796227));
#154540=CARTESIAN_POINT('Ctrl Pts',(68.2205070085393,12.303291823643,55.6675584554868));
#154541=CARTESIAN_POINT('Ctrl Pts',(68.3406393902131,12.3414994557714,55.6898567491261));
#154542=CARTESIAN_POINT('Ctrl Pts',(68.3994686284563,12.3598633776101,55.7004868975834));
#154543=CARTESIAN_POINT('Ctrl Pts',(68.4285725263113,12.3688638765474,55.7056724837353));
#154544=CARTESIAN_POINT('Ctrl Pts',(68.4409788871562,12.3726827212409,55.7078671577049));
#154545=CARTESIAN_POINT('Ctrl Pts',(68.4492349466484,12.3752201006865,55.7093241166643));
#154546=CARTESIAN_POINT('Ctrl Pts',(68.4518830161046,12.3760333765084,55.709790922099));
#154547=CARTESIAN_POINT('Ctrl Pts',(68.8149541629483,12.4872710399799,55.7735506888852));
#154548=CARTESIAN_POINT('Ctrl Pts',(69.162868996431,12.5790030370059,55.8223642699944));
#154549=CARTESIAN_POINT('Ctrl Pts',(69.6676702367486,12.6936455014814,55.8751154886068));
#154550=CARTESIAN_POINT('Ctrl Pts',(69.8330995553812,12.7280340649958,55.8892863966092));
#154551=CARTESIAN_POINT('Ctrl Pts',(70.0767106558291,12.774343861161,55.9054722190449));
#154552=CARTESIAN_POINT('Ctrl Pts',(70.1973836159313,12.7961804425978,55.9122973844165));
#154553=CARTESIAN_POINT('Ctrl Pts',(70.3361327204431,12.8194503967652,55.9180510407596));
#154554=CARTESIAN_POINT('Ctrl Pts',(70.4049919834056,12.8305464056001,55.9203767180677));
#154555=CARTESIAN_POINT('Ctrl Pts',(70.4343920137761,12.8351876863888,55.9212554500965));
#154556=CARTESIAN_POINT('Ctrl Pts',(70.4539672765963,12.8382566553964,55.9218150649338));
#154557=CARTESIAN_POINT('Ctrl Pts',(70.4623603837728,12.8395648502933,55.9220458653953));
#154558=CARTESIAN_POINT('Ctrl Pts',(71.1867843081602,12.9515612289472,55.9408640777805));
#154559=CARTESIAN_POINT('Ctrl Pts',(71.8672262336773,13.0002712185582,55.8928336884898));
#154560=CARTESIAN_POINT('Ctrl Pts',(72.8316323522009,12.9998626943128,55.7221797060804));
#154561=CARTESIAN_POINT('Ctrl Pts',(73.156593253721,12.9874245982617,55.6466015973117));
#154562=CARTESIAN_POINT('Ctrl Pts',(73.6477317483949,12.9480664786676,55.5054660086465));
#154563=CARTESIAN_POINT('Ctrl Pts',(73.8120571647138,12.9314972523697,55.4537933772774));
#154564=CARTESIAN_POINT('Ctrl Pts',(74.059238093724,12.9011924710334,55.3693831402032));
#154565=CARTESIAN_POINT('Ctrl Pts',(74.183001403273,12.8846774122361,55.3254527619492));
#154566=CARTESIAN_POINT('Ctrl Pts',(74.327641147951,12.8629655993948,55.2711908410012));
#154567=CARTESIAN_POINT('Ctrl Pts',(74.4000163786488,12.8514912585304,55.2433086520233));
#154568=CARTESIAN_POINT('Ctrl Pts',(74.4310454459668,12.8464403744192,55.2311982973818));
#154569=CARTESIAN_POINT('Ctrl Pts',(74.4517338757724,12.8430434067065,55.2230889991257));
#154570=CARTESIAN_POINT('Ctrl Pts',(74.4633732136143,12.8411139351156,55.2185049480234));
#154571=CARTESIAN_POINT('Ctrl Pts',(74.7621099082225,12.7912143974189,55.1004034772508));
#154572=CARTESIAN_POINT('Ctrl Pts',(75.0594352234263,12.7300263414723,54.9689784394765));
#154573=CARTESIAN_POINT('Ctrl Pts',(75.5148249550515,12.6152727348306,54.7468505371001));
#154574=CARTESIAN_POINT('Ctrl Pts',(75.6681820304404,12.5731918438571,54.668643984714));
#154575=CARTESIAN_POINT('Ctrl Pts',(75.9002389477876,12.5038490981298,54.5451446051645));
#154576=CARTESIAN_POINT('Ctrl Pts',(76.0167720568909,12.4676223507902,54.4818476467801));
#154577=CARTESIAN_POINT('Ctrl Pts',(76.1535332760956,12.4225316333616,54.4053070900001));
#154578=CARTESIAN_POINT('Ctrl Pts',(76.222105150992,12.3992667241873,54.366365086637));
#154579=CARTESIAN_POINT('Ctrl Pts',(76.256437611271,12.387452758321,54.3467263817898));
#154580=CARTESIAN_POINT('Ctrl Pts',(76.271161351744,12.382350560981,54.3382738823359));
#154581=CARTESIAN_POINT('Ctrl Pts',(76.2809793472499,12.3789403947562,54.3326309050957));
#154582=CARTESIAN_POINT('Ctrl Pts',(76.2872270023928,12.3767642024809,54.3290348119035));
#154583=CARTESIAN_POINT('Ctrl Pts',(76.5195100464752,12.2957068885854,54.1952096223952));
#154584=CARTESIAN_POINT('Ctrl Pts',(76.7737073693445,12.1984333691483,54.0405028368108));
#154585=CARTESIAN_POINT('Ctrl Pts',(77.1889514738957,12.0172155600492,53.7747873183489));
#154586=CARTESIAN_POINT('Ctrl Pts',(77.333004209153,11.9509078155911,53.6806097796382));
#154587=CARTESIAN_POINT('Ctrl Pts',(77.5567963331259,11.841319347885,53.5310661152164));
#154588=CARTESIAN_POINT('Ctrl Pts',(77.6706182436651,11.7839921584008,53.4542253682861));
#154589=CARTESIAN_POINT('Ctrl Pts',(77.8065908646447,11.7123873452126,53.3609907038759));
#154590=CARTESIAN_POINT('Ctrl Pts',(77.875346374262,11.6753671232057,53.3134811567604));
#154591=CARTESIAN_POINT('Ctrl Pts',(77.9136167044436,11.6545315706107,53.2869349217018));
#154592=CARTESIAN_POINT('Ctrl Pts',(77.9321973222568,11.6443455786305,53.2740155805481));
#154593=CARTESIAN_POINT('Ctrl Pts',(77.9421224705332,11.6388869269128,53.2671067725909));
#154594=CARTESIAN_POINT('Ctrl Pts',(77.944552151737,11.6375497290564,53.2654150912361));
#154595=CARTESIAN_POINT('Ctrl Pts',(77.9513162792979,11.633826151391,53.2607051396328));
#154596=CARTESIAN_POINT('Ctrl Pts',(78.0207231770864,11.5963633097845,53.2122303381047));
#154597=CARTESIAN_POINT('Ctrl Pts',(78.2157934428615,11.4834360324175,53.0743596905367));
#154598=CARTESIAN_POINT('Ctrl Pts',(78.2959193690099,11.4362233179004,53.0175532028137));
#154599=CARTESIAN_POINT('Ctrl Pts',(78.4377882693462,11.3492951678592,52.9162407609837));
#154600=CARTESIAN_POINT('Ctrl Pts',(78.4886867489951,11.3176275934474,52.8797869535281));
#154601=CARTESIAN_POINT('Ctrl Pts',(78.5702820457391,11.2658118786183,52.8211109680525));
#154602=CARTESIAN_POINT('Ctrl Pts',(78.6123911010194,11.2388248486234,52.7907742426851));
#154603=CARTESIAN_POINT('Ctrl Pts',(78.6637716696953,11.2053848061015,52.7536409538566));
#154604=CARTESIAN_POINT('Ctrl Pts',(78.6900196630872,11.1881672296221,52.7346401906974));
#154605=CARTESIAN_POINT('Ctrl Pts',(78.7013876985477,11.1806807008864,52.7264040892436));
#154606=CARTESIAN_POINT('Ctrl Pts',(78.7089927407024,11.1756656713378,52.7208927188949));
#154607=CARTESIAN_POINT('Ctrl Pts',(78.7142700602418,11.1721797453604,52.7170668838275));
#154608=CARTESIAN_POINT('Ctrl Pts',(79.0196408631394,10.9702724809317,52.4956405505701));
#154609=CARTESIAN_POINT('Ctrl Pts',(79.264657315864,10.7879579613599,52.3154423177719));
#154610=CARTESIAN_POINT('Ctrl Pts',(79.4586835372191,10.63636346571,52.1735219594));
#154611=CARTESIAN_POINT('Origin',(61.3394944137234,15.5454545439464,55.3684227747178));
#154612=CARTESIAN_POINT('Ctrl Pts',(58.9590707274591,10.81101501758,60.34065684336));
#154613=CARTESIAN_POINT('Ctrl Pts',(61.1064578339192,8.94654054057203,59.33388480863));
#154614=CARTESIAN_POINT('Ctrl Pts',(62.4865214122591,8.16441345063902,56.76773433708));
#154615=CARTESIAN_POINT('Ctrl Pts',(62.4634906824092,8.82500194251101,53.82412647963));
#154616=CARTESIAN_POINT('Ctrl Pts',(59.9816955898691,11.69357781733,60.50665366569));
#154617=CARTESIAN_POINT('Ctrl Pts',(61.8899962375191,9.76084628201802,59.44350004341));
#154618=CARTESIAN_POINT('Ctrl Pts',(63.1395454747391,8.92300163969001,56.9508929801001));
#154619=CARTESIAN_POINT('Ctrl Pts',(63.1884414345591,9.54345189093102,54.10959711083));
#154620=CARTESIAN_POINT('Ctrl Pts',(61.1145864519892,12.47844490925,60.66339390371));
#154621=CARTESIAN_POINT('Ctrl Pts',(62.7916440738191,10.52153477373,59.55604388476));
#154622=CARTESIAN_POINT('Ctrl Pts',(63.8998310565591,9.63580488197901,57.13850344022));
#154623=CARTESIAN_POINT('Ctrl Pts',(63.9881291455391,10.18178345265,54.39448591732));
#154624=CARTESIAN_POINT('Ctrl Pts',(62.3634669048891,13.16556661825,60.78401903071));
#154625=CARTESIAN_POINT('Ctrl Pts',(63.8226049756391,11.20542779043,59.64621201015));
#154626=CARTESIAN_POINT('Ctrl Pts',(64.7778160615291,10.27890102988,57.30204095023));
#154627=CARTESIAN_POINT('Ctrl Pts',(64.8638764659491,10.74028182249,54.64762076559));
#154628=CARTESIAN_POINT('',(62.5668978423991,8.89165945463101,54.03302090535));
#154629=CARTESIAN_POINT('Ctrl Pts',(62.5668978423991,8.89165945463101,54.03302090535));
#154630=CARTESIAN_POINT('Ctrl Pts',(62.5986175218308,8.92270892978409,54.0452657277444));
#154631=CARTESIAN_POINT('Ctrl Pts',(62.6965178171167,9.01946894987616,54.0836661950859));
#154632=CARTESIAN_POINT('Ctrl Pts',(62.9512454808967,9.25459977512765,54.1789839833193));
#154633=CARTESIAN_POINT('Ctrl Pts',(63.054255116238,9.34785310371798,54.2170214466761));
#154634=CARTESIAN_POINT('Ctrl Pts',(63.2379730184545,9.50777105388192,54.2831129736518));
#154635=CARTESIAN_POINT('Ctrl Pts',(63.3040857261481,9.56440773183257,54.3066482841705));
#154636=CARTESIAN_POINT('Ctrl Pts',(63.4108712884247,9.65398879690074,54.3441544273615));
#154637=CARTESIAN_POINT('Ctrl Pts',(63.4661686665216,9.69993491296207,54.3634582101237));
#154638=CARTESIAN_POINT('Ctrl Pts',(63.5340869392131,9.75546995340281,54.3869304059749));
#154639=CARTESIAN_POINT('Ctrl Pts',(63.5689065016673,9.78370812507163,54.3989026501242));
#154640=CARTESIAN_POINT('Ctrl Pts',(63.5840145461932,9.79590973026782,54.4040840387116));
#154641=CARTESIAN_POINT('Ctrl Pts',(63.5941278819465,9.80406610280387,54.4075494840412));
#154642=CARTESIAN_POINT('Ctrl Pts',(63.6008816978809,9.80950359151928,54.4098612837665));
#154643=CARTESIAN_POINT('Ctrl Pts',(64.0422596943631,10.1644809627909,54.5608448379334));
#154644=CARTESIAN_POINT('Ctrl Pts',(64.4260650495644,10.4322956587886,54.6791846378752));
#154645=CARTESIAN_POINT('Ctrl Pts',(64.7368422516391,10.63636348946,54.76937963139));
#154646=CARTESIAN_POINT('Ctrl Pts',(59.2279850656438,10.8294941093792,60.3034709806296));
#154647=CARTESIAN_POINT('Ctrl Pts',(59.3134256343538,10.7545915723124,60.258963004405));
#154648=CARTESIAN_POINT('Ctrl Pts',(59.3991652882675,10.680240728207,60.2105626520754));
#154649=CARTESIAN_POINT('Ctrl Pts',(59.4849397019862,10.6067220037401,60.1581869063918));
#154650=CARTESIAN_POINT('Ctrl Pts',(59.5713228657953,10.5326815091063,60.1054394444988));
#154651=CARTESIAN_POINT('Ctrl Pts',(59.6577410378865,10.4594853307763,60.0486595080926));
#154652=CARTESIAN_POINT('Ctrl Pts',(59.7439023723681,10.3874309241517,59.9878108477117));
#154653=CARTESIAN_POINT('Ctrl Pts',(59.8274742292158,10.3175420280255,59.9287909222971));
#154654=CARTESIAN_POINT('Ctrl Pts',(59.9108040573564,10.2487277080708,59.8659431171087));
#154655=CARTESIAN_POINT('Ctrl Pts',(59.993610017306,10.1812641227691,59.7992830131684));
#154656=CARTESIAN_POINT('Ctrl Pts',(60.0758344999377,10.1142742780612,59.7330910076413));
#154657=CARTESIAN_POINT('Ctrl Pts',(60.1575420809736,10.048616654725,59.6631399245928));
#154658=CARTESIAN_POINT('Ctrl Pts',(60.2384468059363,9.98456054389281,59.5894953010128));
#154659=CARTESIAN_POINT('Ctrl Pts',(60.3186969195305,9.92102271995163,59.5164465463125));
#154660=CARTESIAN_POINT('Ctrl Pts',(60.3981567261616,9.85906098815908,59.4397637592995));
#154661=CARTESIAN_POINT('Ctrl Pts',(60.4765429014928,9.79893126053567,59.3595616608662));
#154662=CARTESIAN_POINT('Ctrl Pts',(60.4856978007711,9.79190857320978,59.3501946758084));
#154663=CARTESIAN_POINT('Ctrl Pts',(60.4948380543894,9.78491086352201,59.3407797431561));
#154664=CARTESIAN_POINT('Ctrl Pts',(60.5039632110606,9.77793852912787,59.3313170911929));
#154665=CARTESIAN_POINT('Ctrl Pts',(60.580499202148,9.71945903751137,59.2519504049623));
#154666=CARTESIAN_POINT('Ctrl Pts',(60.6560082058958,9.66273886911162,59.1691860498569));
#154667=CARTESIAN_POINT('Ctrl Pts',(60.7302169784138,9.60801399981514,59.0831828485741));
#154668=CARTESIAN_POINT('Ctrl Pts',(60.8040691333626,9.55355211627086,58.9975929441502));
#154669=CARTESIAN_POINT('Ctrl Pts',(60.876633123015,9.50106676290267,58.9087954073986));
#154670=CARTESIAN_POINT('Ctrl Pts',(60.9476470270386,9.45077273985678,58.816994662647));
#154671=CARTESIAN_POINT('Ctrl Pts',(61.0183254973686,9.40071628028738,58.7256275380902));
#154672=CARTESIAN_POINT('Ctrl Pts',(61.087468108101,9.35283082106235,58.6312857698978));
#154673=CARTESIAN_POINT('Ctrl Pts',(61.1548298447628,9.30730534780568,58.534215305236));
#154674=CARTESIAN_POINT('Ctrl Pts',(61.2220446102576,9.26187920292532,58.4373566308303));
#154675=CARTESIAN_POINT('Ctrl Pts',(61.2874859051142,9.21880303954255,58.3377814899491));
#154676=CARTESIAN_POINT('Ctrl Pts',(61.3509290700527,9.17823732169581,58.2357741030116));
#154677=CARTESIAN_POINT('Ctrl Pts',(61.4142893140245,9.13772462372195,58.133900040935));
#154678=CARTESIAN_POINT('Ctrl Pts',(61.4756563286036,9.09971603908283,58.0296005002065));
#154679=CARTESIAN_POINT('Ctrl Pts',(61.5348301573818,9.06434033599487,57.9231927895167));
#154680=CARTESIAN_POINT('Ctrl Pts',(61.557278527314,9.05092009792798,57.8828256254759));
#154681=CARTESIAN_POINT('Ctrl Pts',(61.5794115312215,9.03787843829657,57.8421553797251));
#154682=CARTESIAN_POINT('Ctrl Pts',(61.6012192890004,9.025221122758,57.8012004642127));
#154683=CARTESIAN_POINT('Ctrl Pts',(61.658703143616,8.99185724859815,57.6932459265211));
#154684=CARTESIAN_POINT('Ctrl Pts',(61.7139641673336,8.96114362320618,57.5832381541095));
#154685=CARTESIAN_POINT('Ctrl Pts',(61.7668325938444,8.93317273510113,57.4715236451438));
#154686=CARTESIAN_POINT('Ctrl Pts',(61.8197461278394,8.90517798215884,57.3597138210575));
#154687=CARTESIAN_POINT('Ctrl Pts',(61.8702627698071,8.87993074294189,57.2461948693806));
#154688=CARTESIAN_POINT('Ctrl Pts',(61.9182443233936,8.85748767537645,57.1313341626496));
#154689=CARTESIAN_POINT('Ctrl Pts',(61.9664028183663,8.83496184459917,57.0160498845428));
#154690=CARTESIAN_POINT('Ctrl Pts',(62.012007338638,8.815260938074,56.8994144889776));
#154691=CARTESIAN_POINT('Ctrl Pts',(62.054953159131,8.79840493994763,56.7818114600221));
#154692=CARTESIAN_POINT('Ctrl Pts',(62.0980138971958,8.78150383730693,56.6638937402684));
#154693=CARTESIAN_POINT('Ctrl Pts',(62.1384016172103,8.7674628347838,56.5450037683519));
#154694=CARTESIAN_POINT('Ctrl Pts',(62.1760475714549,8.75626481291633,56.4255317414049));
#154695=CARTESIAN_POINT('Ctrl Pts',(62.2139110231855,8.7450020950768,56.3053694712159));
#154696=CARTESIAN_POINT('Ctrl Pts',(62.2490009275031,8.73661518966188,56.1846189627729));
#154697=CARTESIAN_POINT('Ctrl Pts',(62.281285169705,8.73105026857484,56.063672343902));
#154698=CARTESIAN_POINT('Ctrl Pts',(62.2933952537888,8.72896282102498,56.0183042750153));
#154699=CARTESIAN_POINT('Ctrl Pts',(62.3051109433974,8.72727208828487,55.9729085200835));
#154700=CARTESIAN_POINT('Ctrl Pts',(62.3164318955331,8.72597398141135,55.9275053573406));
#154701=CARTESIAN_POINT('Ctrl Pts',(62.3472724494424,8.7224376768203,55.8038179968227));
#154702=CARTESIAN_POINT('Ctrl Pts',(62.3751954603565,8.72181580791975,55.6800186717206));
#154703=CARTESIAN_POINT('Ctrl Pts',(62.4002141666283,8.7240106844509,55.5564958095557));
#154704=CARTESIAN_POINT('Ctrl Pts',(62.4266203901146,8.72632728705925,55.4261224693609));
#154705=CARTESIAN_POINT('Ctrl Pts',(62.4497910931516,8.73178169992798,55.296057876902));
#154706=CARTESIAN_POINT('Ctrl Pts',(62.4697845242374,8.74022267695791,55.1667317285681));
#154707=CARTESIAN_POINT('Ctrl Pts',(62.4890937538867,8.74837479268213,55.041831290663));
#154708=CARTESIAN_POINT('Ctrl Pts',(62.5054399441388,8.75931202454087,54.9176198452025));
#154709=CARTESIAN_POINT('Ctrl Pts',(62.5189106525707,8.77287020927075,54.7944531757696));
#154710=CARTESIAN_POINT('Ctrl Pts',(62.5330973407356,8.78714902317408,54.6647400919784));
#154711=CARTESIAN_POINT('Ctrl Pts',(62.5440948296285,8.80433457894131,54.5361864972875));
#154712=CARTESIAN_POINT('Ctrl Pts',(62.5520413132412,8.82420895134365,54.4091649177086));
#154713=CARTESIAN_POINT('Ctrl Pts',(62.5599877968539,8.84408332374599,54.2821433381296));
#154714=CARTESIAN_POINT('Ctrl Pts',(62.5648837133173,8.86664602936165,54.156653998794));
#154715=CARTESIAN_POINT('Ctrl Pts',(62.5668978424016,8.89165945462865,54.0330209053496));
#154716=CARTESIAN_POINT('Ctrl Pts',(62.6875707163291,9.05486984706101,53.85409719576));
#154717=CARTESIAN_POINT('Ctrl Pts',(62.6936927437891,8.90708944577401,54.49996789171));
#154718=CARTESIAN_POINT('Ctrl Pts',(62.5519594607091,8.75508983733901,55.85643113434));
#154719=CARTESIAN_POINT('Ctrl Pts',(61.8187473138591,9.06713176397001,57.86053638825));
#154720=CARTESIAN_POINT('Ctrl Pts',(60.6706513748291,9.88591711331501,59.49166260962));
#154721=CARTESIAN_POINT('Ctrl Pts',(59.7641049370091,10.66790050512,60.16132571301));
#154722=CARTESIAN_POINT('Ctrl Pts',(59.3056604462691,11.08744520415,60.39001266332));
#154723=CARTESIAN_POINT('Ctrl Pts',(62.1213330553091,8.44949510325101,53.95571996686));
#154724=CARTESIAN_POINT('Ctrl Pts',(62.1108200502591,8.32237104745601,54.59787120527));
#154725=CARTESIAN_POINT('Ctrl Pts',(61.9267980790491,8.19927673930601,55.93250107089));
#154726=CARTESIAN_POINT('Ctrl Pts',(61.1093761573991,8.49914365747801,57.86858052973));
#154727=CARTESIAN_POINT('Ctrl Pts',(59.8669990431491,9.25045145190902,59.41928559907));
#154728=CARTESIAN_POINT('Ctrl Pts',(58.8963896387191,9.96331635072501,60.04138849839));
#154729=CARTESIAN_POINT('Ctrl Pts',(58.4060688283291,10.34643938379,60.24891883476));
#154730=CARTESIAN_POINT('Ctrl Pts',(61.3620176577091,7.46083974632801,54.09323968618));
#154731=CARTESIAN_POINT('Ctrl Pts',(61.3251626795591,7.36129509255801,54.72601497373));
#154732=CARTESIAN_POINT('Ctrl Pts',(61.0803190466291,7.27338783305801,56.02131835236));
#154733=CARTESIAN_POINT('Ctrl Pts',(60.1582507453391,7.54259435678201,57.85121399405));
#154734=CARTESIAN_POINT('Ctrl Pts',(58.8087038077091,8.18268645878101,59.28224135853));
#154735=CARTESIAN_POINT('Ctrl Pts',(57.7674952770791,8.78618585702401,59.83536073368));
#154736=CARTESIAN_POINT('Ctrl Pts',(57.2415921764891,9.11164773419301,60.0124212846));
#154737=CARTESIAN_POINT('Ctrl Pts',(60.5437715759391,6.00793348176301,54.24295470498));
#154738=CARTESIAN_POINT('Ctrl Pts',(60.4753647636491,5.93916618444801,54.85989885246));
#154739=CARTESIAN_POINT('Ctrl Pts',(60.1636338904891,5.88576846827101,56.10101490775));
#154740=CARTESIAN_POINT('Ctrl Pts',(59.1425671318791,6.10203393089201,57.80204415533));
#154741=CARTESIAN_POINT('Ctrl Pts',(57.7021490370491,6.59039605304901,59.0946682543));
#154742=CARTESIAN_POINT('Ctrl Pts',(56.6033067699491,7.04779466755601,59.57002403801));
#154743=CARTESIAN_POINT('Ctrl Pts',(56.0476476565391,7.29537012181901,59.71293770471));
#154744=CARTESIAN_POINT('Ctrl Pts',(60.0471342481991,4.90275765822201,54.33449450703));
#154745=CARTESIAN_POINT('Ctrl Pts',(59.9584867813191,4.85293774611401,54.9392420524));
#154746=CARTESIAN_POINT('Ctrl Pts',(59.6062054947891,4.81843036106501,56.14248407187));
#154747=CARTESIAN_POINT('Ctrl Pts',(58.5319771100791,4.99247752985201,57.76014880143));
#154748=CARTESIAN_POINT('Ctrl Pts',(57.0481181060591,5.37294144456601,58.96651117554));
#154749=CARTESIAN_POINT('Ctrl Pts',(55.9232080096891,5.72782341665301,59.39476748319));
#154750=CARTESIAN_POINT('Ctrl Pts',(55.3537576252991,5.92042931459201,59.51724032973));
#154751=CARTESIAN_POINT('Ctrl Pts',(59.6514918396991,3.73992698433501,54.40789230405));
#154752=CARTESIAN_POINT('Ctrl Pts',(59.5463847958691,3.70514679147901,55.00100479065));
#154753=CARTESIAN_POINT('Ctrl Pts',(59.1627398857991,3.68320799693501,56.17068044341));
#154754=CARTESIAN_POINT('Ctrl Pts',(58.0522452014191,3.81340119389101,57.71933487698));
#154755=CARTESIAN_POINT('Ctrl Pts',(56.5429763649491,4.09236446003801,58.85701018477));
#154756=CARTESIAN_POINT('Ctrl Pts',(55.4041011816691,4.35221319071501,59.24912253076));
#154757=CARTESIAN_POINT('Ctrl Pts',(54.8269328357791,4.49364817466901,59.35619700334));
#154758=CARTESIAN_POINT('Ctrl Pts',(59.2623296266291,2.11847170632401,54.48042667407));
#154759=CARTESIAN_POINT('Ctrl Pts',(59.1408541116391,2.10082097206001,55.06070972073));
#154760=CARTESIAN_POINT('Ctrl Pts',(58.7271787855591,2.09107712759001,56.19493379311));
#154761=CARTESIAN_POINT('Ctrl Pts',(57.5854988517191,2.16271678317001,57.67379941492));
#154762=CARTESIAN_POINT('Ctrl Pts',(56.0578341057191,2.31287231939801,58.74373047707));
#154763=CARTESIAN_POINT('Ctrl Pts',(54.9100779263991,2.45260917966401,59.10101280316));
#154764=CARTESIAN_POINT('Ctrl Pts',(54.3276575839291,2.52896184850001,59.19342098219));
#154765=CARTESIAN_POINT('Ctrl Pts',(59.0540952976791,0.0127975999524342,
54.5196572809));
#154766=CARTESIAN_POINT('Ctrl Pts',(58.9232560182391,0.0126887045292242,
55.09143455285));
#154767=CARTESIAN_POINT('Ctrl Pts',(58.4938016584491,0.0126145908767642,
56.2037448358));
#154768=CARTESIAN_POINT('Ctrl Pts',(57.3403850018491,0.0129921919657642,
57.64274508359));
#154769=CARTESIAN_POINT('Ctrl Pts',(55.8112488908891,0.0138214067188142,
58.6760997592));
#154770=CARTESIAN_POINT('Ctrl Pts',(54.6655311374391,0.0146072936320442,
59.01584458769));
#154771=CARTESIAN_POINT('Ctrl Pts',(54.0837499761391,0.0150396948250942,
59.10118989083));
#154772=CARTESIAN_POINT('Ctrl Pts',(59.2989189396391,-2.51693002856899,
54.47354239089));
#154773=CARTESIAN_POINT('Ctrl Pts',(59.1790755060991,-2.49593417718599,
55.05528462409));
#154774=CARTESIAN_POINT('Ctrl Pts',(58.7681731074591,-2.48428118923299,
56.19329870897));
#154775=CARTESIAN_POINT('Ctrl Pts',(57.6286544560291,-2.56920952549099,
57.67914147466));
#154776=CARTESIAN_POINT('Ctrl Pts',(56.1014244201991,-2.74738422816499,
58.75555153277));
#154777=CARTESIAN_POINT('Ctrl Pts',(54.9534490419391,-2.91325666836699,
59.11599776679));
#154778=CARTESIAN_POINT('Ctrl Pts',(54.3709846642191,-3.00390208172399,
59.20969563797));
#154779=CARTESIAN_POINT('Ctrl Pts',(59.9917126604991,-4.91906267884899,
54.34448351142));
#154780=CARTESIAN_POINT('Ctrl Pts',(59.9009297075891,-4.87125340189799,
54.94879468213));
#154781=CARTESIAN_POINT('Ctrl Pts',(59.5435979960591,-4.83987319128399,
56.14942539199));
#154782=CARTESIAN_POINT('Ctrl Pts',(58.4604560798591,-5.01415296934599,
57.75897301872));
#154783=CARTESIAN_POINT('Ctrl Pts',(56.9673297784391,-5.39038447606399,
58.95563343562));
#154784=CARTESIAN_POINT('Ctrl Pts',(55.8362600566191,-5.74067651648499,
59.37795261339));
#154785=CARTESIAN_POINT('Ctrl Pts',(55.2637085671291,-5.93095636015299,
59.49771519496));
#154786=CARTESIAN_POINT('Ctrl Pts',(61.1125443538391,-7.13614956716599,
54.13839204096));
#154787=CARTESIAN_POINT('Ctrl Pts',(61.0671680892591,-7.04576412768599,
54.76818692763));
#154788=CARTESIAN_POINT('Ctrl Pts',(60.8025094853891,-6.96962720623199,
56.0507627613));
#154789=CARTESIAN_POINT('Ctrl Pts',(59.8459446485991,-7.22911178542799,
57.84598152538));
#154790=CARTESIAN_POINT('Ctrl Pts',(58.4607058835591,-7.83300648254199,
59.2377399736));
#154791=CARTESIAN_POINT('Ctrl Pts',(57.3957858977891,-8.40075126025699,
59.76809594155));
#154792=CARTESIAN_POINT('Ctrl Pts',(56.8579036864491,-8.70733922026899,
59.93506871694));
#154793=CARTESIAN_POINT('Ctrl Pts',(62.1145143757991,-8.44196653416099,
53.95694727695));
#154794=CARTESIAN_POINT('Ctrl Pts',(62.1038084651091,-8.31509888071599,
54.59903739218));
#154795=CARTESIAN_POINT('Ctrl Pts',(61.9193139144091,-8.19237189993399,
55.93337680427));
#154796=CARTESIAN_POINT('Ctrl Pts',(61.1010004648091,-8.49213444877799,
57.86861879038));
#154797=CARTESIAN_POINT('Ctrl Pts',(59.8576583382091,-9.24267821450499,
59.41836213069));
#154798=CARTESIAN_POINT('Ctrl Pts',(58.8864033693091,-9.95473954319099,
60.03991099606));
#154799=CARTESIAN_POINT('Ctrl Pts',(58.3957609560291,-10.33743603438,60.24719828988));
#154800=CARTESIAN_POINT('Ctrl Pts',(62.6879642021691,-9.05532397487499,
53.8540261509));
#154801=CARTESIAN_POINT('Ctrl Pts',(62.6940943763991,-8.90752652229099,
54.49990186792));
#154802=CARTESIAN_POINT('Ctrl Pts',(62.5523798635391,-8.75549999478799,
55.85638386176));
#154803=CARTESIAN_POINT('Ctrl Pts',(61.8191993941091,-9.06753559913399,
57.86053706941));
#154804=CARTESIAN_POINT('Ctrl Pts',(60.6711354527091,-9.88635090107299,
59.49171575596));
#154805=CARTESIAN_POINT('Ctrl Pts',(59.7646103295491,-10.6683719995,60.16140778771));
#154806=CARTESIAN_POINT('Ctrl Pts',(59.3061767685891,-11.08793749998,60.39010712379));
#154807=CARTESIAN_POINT('Ctrl Pts',(62.5668978424019,8.89165945462829,54.0330209053495));
#154808=CARTESIAN_POINT('Ctrl Pts',(61.5307357207086,7.76947049531924,54.2157242437921));
#154809=CARTESIAN_POINT('Ctrl Pts',(60.6061882911196,6.35847891159746,54.3787469007418));
#154810=CARTESIAN_POINT('Ctrl Pts',(59.406833177869,3.23205943624151,54.5902255666585));
#154811=CARTESIAN_POINT('Ctrl Pts',(59.1039820610764,1.60347731142046,54.6436263895163));
#154812=CARTESIAN_POINT('Ctrl Pts',(59.1038271015103,-1.60757587207886,
54.6436537130687));
#154813=CARTESIAN_POINT('Ctrl Pts',(59.4077654184968,-3.23446213873761,
54.5900611874711));
#154814=CARTESIAN_POINT('Ctrl Pts',(60.6369613386987,-6.4381888767319,54.3733207821628));
#154815=CARTESIAN_POINT('Ctrl Pts',(61.58246960519,-7.82549951850307,54.2066021641412));
#154816=CARTESIAN_POINT('Ctrl Pts',(62.5668976767239,-8.89165927519747,
54.033020934563));
#154817=CARTESIAN_POINT('Origin',(71.9064062760691,1.4210854715202E-14,
52.38621358194));
#154818=CARTESIAN_POINT('Origin',(71.9064062760691,1.4210854715202E-14,
52.38621358194));
#154819=CARTESIAN_POINT('Origin',(71.9064062760691,1.4210854715202E-14,
52.38621358194));
#154820=CARTESIAN_POINT('Origin',(71.9064062760691,1.4210854715202E-14,
52.38621358194));
#154821=CARTESIAN_POINT('Origin',(71.9064062760691,1.4210854715202E-14,
52.38621358194));
#154822=CARTESIAN_POINT('Origin',(72.0800544537291,1.4210854715202E-14,
53.37102133495));
#154823=CARTESIAN_POINT('Origin',(72.4273508090691,1.4210854715202E-14,
55.34063684098));
#154824=CARTESIAN_POINT('Origin',(72.4273508090703,1.25011112572802E-13,
55.3406368409798));
#154825=CARTESIAN_POINT('Origin',(72.4794268116891,1.25011112572802E-13,
55.63597452787));
#154826=CARTESIAN_POINT('Origin',(82.1588614745091,11.44983787884,58.70184200704));
#154827=CARTESIAN_POINT('',(81.8983972201781,-8.53716763907585,57.2246289649024));
#154828=CARTESIAN_POINT('',(81.8983892080091,-3.04138126515099,57.22463037752));
#154829=CARTESIAN_POINT('Origin',(82.1588614745091,-8.53720311761699,58.70184200704));
#154830=CARTESIAN_POINT('',(81.8983915604129,8.53714783790647,57.2246299627624));
#154831=CARTESIAN_POINT('Origin',(82.1588614745091,8.53714874844301,58.70184200704));
#154832=CARTESIAN_POINT('',(81.8983892078791,8.53712721536902,57.22463037754));
#154833=CARTESIAN_POINT('Origin',(83.3756008375291,111.0724296188,56.96415811102));
#154834=CARTESIAN_POINT('',(81.3676282287758,8.73788135389827,57.3182179348277));
#154835=CARTESIAN_POINT('Ctrl Pts',(81.8983892080091,8.53714874844301,57.22463037752));
#154836=CARTESIAN_POINT('Ctrl Pts',(81.8095766714547,8.57150267943434,57.2402904239405));
#154837=CARTESIAN_POINT('Ctrl Pts',(81.6321992954396,8.63903130243991,57.2715668124596));
#154838=CARTESIAN_POINT('Ctrl Pts',(81.4557926517591,8.70548579598501,57.30267214923));
#154839=CARTESIAN_POINT('Ctrl Pts',(81.3676282255091,8.73788135389401,57.31821791631));
#154840=CARTESIAN_POINT('',(64.7026068549496,8.73787995439493,60.2567108302939));
#154841=CARTESIAN_POINT('Ctrl Pts',(81.3676282316625,8.73788135390567,57.318217951183));
#154842=CARTESIAN_POINT('Ctrl Pts',(81.2087098997806,8.79636286454771,57.346239540823));
#154843=CARTESIAN_POINT('Ctrl Pts',(81.0460194198263,8.85311144861849,57.3749262452573));
#154844=CARTESIAN_POINT('Ctrl Pts',(80.879564119114,8.90817525433878,57.404276787864));
#154845=CARTESIAN_POINT('Ctrl Pts',(80.7218084076859,8.96036121542369,57.4320933590991));
#154846=CARTESIAN_POINT('Ctrl Pts',(80.5606711114645,9.01103370167497,57.4605061948796));
#154847=CARTESIAN_POINT('Ctrl Pts',(80.3961944404702,9.06026076227427,57.489507859617));
#154848=CARTESIAN_POINT('Ctrl Pts',(80.2448213934373,9.10556597251676,57.5161990027061));
#154849=CARTESIAN_POINT('Ctrl Pts',(80.090620016467,9.14964691300423,57.5433888623393));
#154850=CARTESIAN_POINT('Ctrl Pts',(79.9336532193732,9.19258112448351,57.5710663427408));
#154851=CARTESIAN_POINT('Ctrl Pts',(79.8707917540675,9.20977525404021,57.58215051472));
#154852=CARTESIAN_POINT('Ctrl Pts',(79.8074871650171,9.22678582049492,57.5933128217162));
#154853=CARTESIAN_POINT('Ctrl Pts',(79.7437354288369,9.24360804525351,57.6045539728719));
#154854=CARTESIAN_POINT('Ctrl Pts',(79.4985200072644,9.30831324676067,57.6477920677814));
#154855=CARTESIAN_POINT('Ctrl Pts',(79.246746324175,9.3702979433272,57.6921865627655));
#154856=CARTESIAN_POINT('Ctrl Pts',(78.9881445367556,9.42934575710402,57.7377850365787));
#154857=CARTESIAN_POINT('Ctrl Pts',(78.7466393188292,9.48448982736184,57.780368923818));
#154858=CARTESIAN_POINT('Ctrl Pts',(78.4991787716111,9.53707191423088,57.8240028948914));
#154859=CARTESIAN_POINT('Ctrl Pts',(78.2455882533844,9.58691893897613,57.8687177431983));
#154860=CARTESIAN_POINT('Ctrl Pts',(78.1786342973979,9.60007974453066,57.8805235315473));
#154861=CARTESIAN_POINT('Ctrl Pts',(78.1112532983418,9.61304993661468,57.8924046190412));
#154862=CARTESIAN_POINT('Ctrl Pts',(78.0434426503664,9.62582644832172,57.9043614653979));
#154863=CARTESIAN_POINT('Ctrl Pts',(77.9943883457167,9.63506899232256,57.9130110624944));
#154864=CARTESIAN_POINT('Ctrl Pts',(77.9451092107804,9.64421018988931,57.9217003033261));
#154865=CARTESIAN_POINT('Ctrl Pts',(77.895603477672,9.65324711977084,57.9304294997728));
#154866=CARTESIAN_POINT('Ctrl Pts',(77.6104542861935,9.70529913652465,57.9807089957573));
#154867=CARTESIAN_POINT('Ctrl Pts',(77.3177944791281,9.7539232726487,58.0323128302488));
#154868=CARTESIAN_POINT('Ctrl Pts',(77.017571009771,9.79862093414819,58.0852503400246));
#154869=CARTESIAN_POINT('Ctrl Pts',(76.7258995738197,9.8420453577655,58.1366798952325));
#154870=CARTESIAN_POINT('Ctrl Pts',(76.4270889872002,9.88176373028796,58.1893682585896));
#154871=CARTESIAN_POINT('Ctrl Pts',(76.1211255271846,9.9172842206695,58.2433178523359));
#154872=CARTESIAN_POINT('Ctrl Pts',(76.0487109490709,9.92569111123492,58.2560864916706));
#154873=CARTESIAN_POINT('Ctrl Pts',(75.9758958620973,9.93386269940829,58.2689257514992));
#154874=CARTESIAN_POINT('Ctrl Pts',(75.9026804047984,9.94179217756508,58.2818356096016));
#154875=CARTESIAN_POINT('Ctrl Pts',(75.8725910730752,9.94505095252126,58.2871411696196));
#154876=CARTESIAN_POINT('Ctrl Pts',(75.8424341220151,9.94826883511575,58.2924586531357));
#154877=CARTESIAN_POINT('Ctrl Pts',(75.8122095038501,9.95144517225851,58.2977880687998));
#154878=CARTESIAN_POINT('Ctrl Pts',(75.6129449749411,9.97238609270137,58.3329237815446));
#154879=CARTESIAN_POINT('Ctrl Pts',(75.4107482586051,9.99147803552478,58.3685765513916));
#154880=CARTESIAN_POINT('Ctrl Pts',(75.2052376707838,10.008466872973,58.40481366752));
#154881=CARTESIAN_POINT('Ctrl Pts',(75.0035537627652,10.0251393722616,58.4403760357346));
#154882=CARTESIAN_POINT('Ctrl Pts',(74.7986780933736,10.039786500644,58.4765012135102));
#154883=CARTESIAN_POINT('Ctrl Pts',(74.5902601914052,10.0521200015532,58.5132509362234));
#154884=CARTESIAN_POINT('Ctrl Pts',(74.3880141962563,10.0640882688733,58.548912384551));
#154885=CARTESIAN_POINT('Ctrl Pts',(74.1824325273812,10.07387795741,58.5851619478052));
#154886=CARTESIAN_POINT('Ctrl Pts',(73.9732067158383,10.0811787248403,58.6220540275996));
#154887=CARTESIAN_POINT('Ctrl Pts',(73.8131362535894,10.0867642556537,58.6502787108855));
#154888=CARTESIAN_POINT('Ctrl Pts',(73.6509330157534,10.0908920808399,58.6788794326511));
#154889=CARTESIAN_POINT('Ctrl Pts',(73.4864645224222,10.0934033427859,58.7078796595598));
#154890=CARTESIAN_POINT('Ctrl Pts',(73.4812596380798,10.0934828159283,58.7087974209128));
#154891=CARTESIAN_POINT('Ctrl Pts',(73.4760524855103,10.0935606685529,58.7097155823065));
#154892=CARTESIAN_POINT('Ctrl Pts',(73.4708430605507,10.0936368963972,58.7106341444809));
#154893=CARTESIAN_POINT('Ctrl Pts',(73.313719697043,10.0959360321715,58.738339232767));
#154894=CARTESIAN_POINT('Ctrl Pts',(73.1545210835498,10.0969060906889,58.7664103272364));
#154895=CARTESIAN_POINT('Ctrl Pts',(72.9939823965101,10.0964561168859,58.7947177107984));
#154896=CARTESIAN_POINT('Ctrl Pts',(72.8341151294458,10.0960080250055,58.8229067045621));
#154897=CARTESIAN_POINT('Ctrl Pts',(72.6729190852784,10.0941517127178,58.851329996284));
#154898=CARTESIAN_POINT('Ctrl Pts',(72.5111223893388,10.0908490929896,58.8798591609756));
#154899=CARTESIAN_POINT('Ctrl Pts',(72.349012790577,10.0875400862395,58.908443498958));
#154900=CARTESIAN_POINT('Ctrl Pts',(72.1863003330493,10.0827791597301,58.9371340995332));
#154901=CARTESIAN_POINT('Ctrl Pts',(72.0237177999578,10.0765805260161,58.9658017542732));
#154902=CARTESIAN_POINT('Ctrl Pts',(71.8603464080213,10.0703518162113,58.9946085059542));
#154903=CARTESIAN_POINT('Ctrl Pts',(71.6971063286149,10.0626714542577,59.0233920672517));
#154904=CARTESIAN_POINT('Ctrl Pts',(71.5347396565587,10.0536066711788,59.0520216173761));
#154905=CARTESIAN_POINT('Ctrl Pts',(71.3703135220802,10.0444269101929,59.0810143053409));
#154906=CARTESIAN_POINT('Ctrl Pts',(71.2067832228854,10.0338274401187,59.1098490278532));
#154907=CARTESIAN_POINT('Ctrl Pts',(71.0449160659144,10.0219314966988,59.1383905417107));
#154908=CARTESIAN_POINT('Ctrl Pts',(70.9990218191482,10.0185586360577,59.1464829262596));
#154909=CARTESIAN_POINT('Ctrl Pts',(70.9532612441384,10.0150818744564,59.1545517448528));
#154910=CARTESIAN_POINT('Ctrl Pts',(70.9076517592672,10.011504773392,59.1625939276118));
#154911=CARTESIAN_POINT('Ctrl Pts',(70.8844280704287,10.0096833653604,59.1666888905456));
#154912=CARTESIAN_POINT('Ctrl Pts',(70.8612434278685,10.0078331957779,59.1707769699724));
#154913=CARTESIAN_POINT('Ctrl Pts',(70.8380978782737,10.0059546557708,59.174858157267));
#154914=CARTESIAN_POINT('Ctrl Pts',(70.5639884063584,9.98370737202299,59.2231910814659));
#154915=CARTESIAN_POINT('Ctrl Pts',(70.2953657364984,9.95748310183114,59.2705566163134));
#154916=CARTESIAN_POINT('Ctrl Pts',(70.0323257265772,9.92788208337571,59.3169376710089));
#154917=CARTESIAN_POINT('Ctrl Pts',(69.7622598959452,9.89749041923642,59.3645575675625));
#154918=CARTESIAN_POINT('Ctrl Pts',(69.4980787513188,9.86353935820031,59.4111397681367));
#154919=CARTESIAN_POINT('Ctrl Pts',(69.2398383678665,9.82665089058296,59.4566744756763));
#154920=CARTESIAN_POINT('Ctrl Pts',(69.0030022172092,9.79281992054897,59.4984350427527));
#154921=CARTESIAN_POINT('Ctrl Pts',(68.7711621228901,9.75651798925938,59.5393146945093));
#154922=CARTESIAN_POINT('Ctrl Pts',(68.5443295182875,9.71820398339368,59.5793114028052));
#154923=CARTESIAN_POINT('Ctrl Pts',(68.4979540337069,9.71037075945588,59.5874886519803));
#154924=CARTESIAN_POINT('Ctrl Pts',(68.451788756776,9.70245224538409,59.595628836128));
#154925=CARTESIAN_POINT('Ctrl Pts',(68.4058309666273,9.69445075333064,59.6037324348464));
#154926=CARTESIAN_POINT('Ctrl Pts',(68.1335570607557,9.64704643978242,59.6517416726167));
#154927=CARTESIAN_POINT('Ctrl Pts',(67.8685694281125,9.59673179975426,59.6984661438657));
#154928=CARTESIAN_POINT('Ctrl Pts',(67.610388088832,9.54366699229344,59.7439904786632));
#154929=CARTESIAN_POINT('Ctrl Pts',(67.346491205237,9.48942745137039,59.7905226181054));
#154930=CARTESIAN_POINT('Ctrl Pts',(67.089704291705,9.43231545711566,59.8358010774));
#154931=CARTESIAN_POINT('Ctrl Pts',(66.8394768016439,9.372464570161,59.8799229349657));
#154932=CARTESIAN_POINT('Ctrl Pts',(66.7205692919111,9.34402357064757,59.9008895370231));
#154933=CARTESIAN_POINT('Ctrl Pts',(66.6031425341752,9.31496347614318,59.9215950427055));
#154934=CARTESIAN_POINT('Ctrl Pts',(66.4871355313901,9.28529498604309,59.9420502072477));
#154935=CARTESIAN_POINT('Ctrl Pts',(66.4248180118144,9.26935744203104,59.9530384673198));
#154936=CARTESIAN_POINT('Ctrl Pts',(66.3629127008068,9.25324277664608,59.9639540438851));
#154937=CARTESIAN_POINT('Ctrl Pts',(66.30141756641,9.23695619266647,59.9747972953772));
#154938=CARTESIAN_POINT('Ctrl Pts',(66.131765985172,9.19202508141341,60.0047114467883));
#154939=CARTESIAN_POINT('Ctrl Pts',(65.9652394658963,9.14578249704889,60.0340745667036));
#154940=CARTESIAN_POINT('Ctrl Pts',(65.801950109141,9.09815126322316,60.0628668933248));
#154941=CARTESIAN_POINT('Ctrl Pts',(65.6347159065267,9.04936932442035,60.0923548028837));
#154942=CARTESIAN_POINT('Ctrl Pts',(65.4708770287103,8.99913104760663,60.1212440317185));
#154943=CARTESIAN_POINT('Ctrl Pts',(65.3105126467954,8.94738991497825,60.1495206156003));
#154944=CARTESIAN_POINT('Ctrl Pts',(65.1443606514881,8.89378142459526,60.1788177124765));
#154945=CARTESIAN_POINT('Ctrl Pts',(64.981938417273,8.83855984079847,60.2074571537367));
#154946=CARTESIAN_POINT('Ctrl Pts',(64.8232916151915,8.78170889653389,60.2354308722771));
#154947=CARTESIAN_POINT('Ctrl Pts',(64.7828177266181,8.76720511358165,60.2425675126148));
#154948=CARTESIAN_POINT('Ctrl Pts',(64.7425893597467,8.75259544747843,60.2496608600567));
#154949=CARTESIAN_POINT('Ctrl Pts',(64.7026068590706,8.73787995440276,60.2567108536817));
#154950=CARTESIAN_POINT('',(61.8548446843784,7.54727709634001,60.7588480660759));
#154951=CARTESIAN_POINT('Ctrl Pts',(64.7026068528891,8.73787995439101,60.2567108186));
#154952=CARTESIAN_POINT('Ctrl Pts',(64.3947973318191,8.62477534901001,60.31098594208));
#154953=CARTESIAN_POINT('Ctrl Pts',(63.7735190092491,8.38547959455801,60.42053398858));
#154954=CARTESIAN_POINT('Ctrl Pts',(62.8261686619491,7.98775290683101,60.58757744947));
#154955=CARTESIAN_POINT('Ctrl Pts',(62.1799654461091,7.69932044348701,60.7015205038));
#154956=CARTESIAN_POINT('Ctrl Pts',(61.8548446843791,7.54727709634001,60.75884806608));
#154957=CARTESIAN_POINT('',(61.7095776082786,7.4812853662219,60.7844468788789));
#154958=CARTESIAN_POINT('Ctrl Pts',(61.8548446843769,7.54727709634,60.7588480660678));
#154959=CARTESIAN_POINT('Ctrl Pts',(61.830610270908,7.535950846149,60.763121247024));
#154960=CARTESIAN_POINT('Ctrl Pts',(61.8059568191555,7.5263062771995,60.7674683157356));
#154961=CARTESIAN_POINT('Ctrl Pts',(61.7817268381449,7.51550163332151,60.7717407151298));
#154962=CARTESIAN_POINT('Ctrl Pts',(61.7574968571344,7.50469698944351,60.776013114524));
#154963=CARTESIAN_POINT('Ctrl Pts',(61.7336903468659,7.49273227063699,60.7802108446008));
#154964=CARTESIAN_POINT('Ctrl Pts',(61.709580295825,7.48128536884799,60.7844620971056));
#154965=CARTESIAN_POINT('',(61.7095727627346,-7.48130385739646,60.7844478028312));
#154966=CARTESIAN_POINT('',(61.7095747601691,-7.48130386006799,60.78445910689));
#154967=CARTESIAN_POINT('Ctrl Pts',(61.7095754384465,-7.48130386006801,
60.7844629535925));
#154968=CARTESIAN_POINT('Ctrl Pts',(61.7337023565672,-7.49275138904401,
60.7802087269665));
#154969=CARTESIAN_POINT('Ctrl Pts',(61.7573216977192,-7.5046239858585,60.7760439998548));
#154970=CARTESIAN_POINT('Ctrl Pts',(61.7817452684442,-7.51551609139476,
60.7717374653708));
#154971=CARTESIAN_POINT('Ctrl Pts',(61.8061688391693,-7.526408196931,60.7674309308867));
#154972=CARTESIAN_POINT('Ctrl Pts',(61.8313966394674,-7.536319811189,60.7629825890302));
#154973=CARTESIAN_POINT('Ctrl Pts',(61.8556180259576,-7.547638577278,60.7587117050818));
#154974=CARTESIAN_POINT('Ctrl Pts',(81.3676320519491,-8.73787997305799,
57.31821724176));
#154975=CARTESIAN_POINT('Ctrl Pts',(81.4558177302491,-8.70547663004399,
57.30266772736));
#154976=CARTESIAN_POINT('Ctrl Pts',(81.6322430735685,-8.63901488156727,
57.2715590931222));
#154977=CARTESIAN_POINT('Ctrl Pts',(81.8095955022414,-8.57149553463792,
57.2402871035593));
#154978=CARTESIAN_POINT('Ctrl Pts',(81.898376792049,-8.53713216053471,57.2246325667929));
#154979=CARTESIAN_POINT('Ctrl Pts',(81.7702420948291,-9.98581821596098,
57.96180292846));
#154980=CARTESIAN_POINT('Ctrl Pts',(81.8773200986491,-9.94703058694397,
57.94292218735));
#154981=CARTESIAN_POINT('Ctrl Pts',(82.1129399024391,-9.86032094569297,
57.90137605875));
#154982=CARTESIAN_POINT('Ctrl Pts',(82.3927019950691,-9.75384394443899,
57.85204645364));
#154983=CARTESIAN_POINT('Ctrl Pts',(82.5654880401691,-9.68649744342697,
57.821579612));
#154984=CARTESIAN_POINT('Ctrl Pts',(82.6104698889891,-9.668857973788,57.81364809841));
#154985=CARTESIAN_POINT('Ctrl Pts',(81.5614869693291,-9.66248792385799,
57.44212653776));
#154986=CARTESIAN_POINT('Ctrl Pts',(81.6674971093891,-9.62408711525799,
57.42343408984));
#154987=CARTESIAN_POINT('Ctrl Pts',(81.9007846866091,-9.53823585217798,
57.38229919571));
#154988=CARTESIAN_POINT('Ctrl Pts',(82.1778276085491,-9.43279395884399,
57.33344905376));
#154989=CARTESIAN_POINT('Ctrl Pts',(82.3489593127491,-9.36609228455299,
57.30327391705));
#154990=CARTESIAN_POINT('Ctrl Pts',(82.3935122424591,-9.34862101415597,
57.29541803347));
#154991=CARTESIAN_POINT('Ctrl Pts',(81.3205762370191,-9.10265723476799,
57.22594062351));
#154992=CARTESIAN_POINT('Ctrl Pts',(81.4247374228791,-9.06492618692099,
57.2075741961001));
#154993=CARTESIAN_POINT('Ctrl Pts',(81.6539868631391,-8.98056116393499,
57.16715133447));
#154994=CARTESIAN_POINT('Ctrl Pts',(81.9263216731591,-8.87691150966299,
57.11913135968));
#154995=CARTESIAN_POINT('Ctrl Pts',(82.0945889664591,-8.81132632150599,
57.0894612959));
#154996=CARTESIAN_POINT('Ctrl Pts',(82.1383992435791,-8.79414627992399,
57.08173636201));
#154997=CARTESIAN_POINT('Ctrl Pts',(81.1333888323891,-8.50589244697699,
57.39031031181));
#154998=CARTESIAN_POINT('Ctrl Pts',(81.2355790816991,-8.46887534647299,
57.3722914136901));
#154999=CARTESIAN_POINT('Ctrl Pts',(81.4605239741791,-8.38609461632999,
57.33262755997));
#155000=CARTESIAN_POINT('Ctrl Pts',(81.7278400607391,-8.28435544175299,
57.28549252153));
#155001=CARTESIAN_POINT('Ctrl Pts',(81.8930539673891,-8.21996039844499,
57.2563608522));
#155002=CARTESIAN_POINT('Ctrl Pts',(81.9360725963791,-8.20309079911799,
57.24877550724));
#155003=CARTESIAN_POINT('',(82.3445054699596,-9.52426778569044,57.5877997674927));
#155004=CARTESIAN_POINT('Origin',(82.1588614745391,-8.53712735499399,58.70184200703));
#155005=CARTESIAN_POINT('Origin',(70.1868938445538,19.4102088531332,61.5764747906095));
#155006=CARTESIAN_POINT('Ctrl Pts',(84.0442680918191,-11.95582982209,59.18935354422));
#155007=CARTESIAN_POINT('Ctrl Pts',(81.8918266601391,-9.61525107327999,
58.42149541083));
#155008=CARTESIAN_POINT('Ctrl Pts',(79.7745014548291,-8.34407927290099,
56.24909744227));
#155009=CARTESIAN_POINT('Ctrl Pts',(78.3288817485491,-8.55554395195999,
53.28264952));
#155010=CARTESIAN_POINT('Ctrl Pts',(85.1121236298391,-11.35883600978,58.70841656241));
#155011=CARTESIAN_POINT('Ctrl Pts',(82.7330218046191,-9.02815085113,58.0565061079401));
#155012=CARTESIAN_POINT('Ctrl Pts',(80.4127135380691,-7.79958765931899,
55.8783245343));
#155013=CARTESIAN_POINT('Ctrl Pts',(78.8938373461991,-8.10009195420299,
52.8212125382));
#155014=CARTESIAN_POINT('Ctrl Pts',(86.0708998648091,-10.68228981744,58.23459657962));
#155015=CARTESIAN_POINT('Ctrl Pts',(83.4615653605592,-8.38274450323699,
57.714890811));
#155016=CARTESIAN_POINT('Ctrl Pts',(80.9478736525491,-7.20591802747199,
55.5272558574701));
#155017=CARTESIAN_POINT('Ctrl Pts',(79.3875877710191,-7.58953754562799,
52.35946311877));
#155018=CARTESIAN_POINT('Ctrl Pts',(86.9329409753991,-9.92711979710299,
57.7857695233));
#155019=CARTESIAN_POINT('Ctrl Pts',(84.0933088102791,-7.69990047563699,
57.41104593754));
#155020=CARTESIAN_POINT('Ctrl Pts',(81.3965784204191,-6.58687843436799,
55.21311191527));
#155021=CARTESIAN_POINT('Ctrl Pts',(79.8215157765292,-7.02960519182299,
51.92060906181));
#155022=CARTESIAN_POINT('Ctrl Pts',(82.3445054687794,-9.52426777936283,
57.5877997772795));
#155023=CARTESIAN_POINT('Ctrl Pts',(82.346531728505,-9.68011068266613,57.7262280958423));
#155024=CARTESIAN_POINT('Ctrl Pts',(82.3485329827188,-9.83740635046138,
57.8622242865471));
#155025=CARTESIAN_POINT('Ctrl Pts',(82.3504900740855,-9.9963050532987,57.9955223328722));
#155026=CARTESIAN_POINT('Ctrl Pts',(82.3511858079024,-10.0527925545503,
58.0429089598501));
#155027=CARTESIAN_POINT('Ctrl Pts',(82.3518761372479,-10.1094822257348,
58.0899544567353));
#155028=CARTESIAN_POINT('Ctrl Pts',(82.3525607872356,-10.1663794243756,
58.1366463490096));
#155029=CARTESIAN_POINT('Ctrl Pts',(82.043884088149,-9.44562267741599,57.50371656119));
#155030=CARTESIAN_POINT('Ctrl Pts',(82.044039598059,-9.45922946787,57.51651606553));
#155031=CARTESIAN_POINT('Ctrl Pts',(82.0459853009791,-9.62874435123598,
57.67559019143));
#155032=CARTESIAN_POINT('Ctrl Pts',(82.049394194429,-9.91110503789099,57.93262616537));
#155033=CARTESIAN_POINT('Ctrl Pts',(82.0528541451991,-10.18503707275,58.1689905444));
#155034=CARTESIAN_POINT('Ctrl Pts',(82.0543047412092,-10.29908415109,58.26507845926));
#155035=CARTESIAN_POINT('Ctrl Pts',(83.0663576928291,-9.40090354793498,
57.3716525166401));
#155036=CARTESIAN_POINT('Ctrl Pts',(83.0664294579292,-9.41553184202599,
57.38345779192));
#155037=CARTESIAN_POINT('Ctrl Pts',(83.0672929144891,-9.59770268033198,
57.53015586066));
#155038=CARTESIAN_POINT('Ctrl Pts',(83.0681107121791,-9.899697052152,57.76678515028));
#155039=CARTESIAN_POINT('Ctrl Pts',(83.0680607108091,-10.19037421172,57.9837057944601));
#155040=CARTESIAN_POINT('Ctrl Pts',(83.0679027349291,-10.31099202241,58.07176439365));
#155041=CARTESIAN_POINT('Ctrl Pts',(83.7612238213791,-8.82417024784398,
57.87108493871));
#155042=CARTESIAN_POINT('Ctrl Pts',(83.7624324745491,-8.83995187633898,
57.8826402837801));
#155043=CARTESIAN_POINT('Ctrl Pts',(83.7773932391891,-9.03649860696499,
58.02622515743));
#155044=CARTESIAN_POINT('Ctrl Pts',(83.8003368389191,-9.36257781544699,
58.25767378284));
#155045=CARTESIAN_POINT('Ctrl Pts',(83.8197704260491,-9.67659535880799,
58.46952040891));
#155046=CARTESIAN_POINT('Ctrl Pts',(83.8273975284591,-9.80690123912098,
58.55545143395));
#155047=CARTESIAN_POINT('Ctrl Pts',(83.613542411989,-8.14281888841199,58.63190259055));
#155048=CARTESIAN_POINT('Ctrl Pts',(83.616266079629,-8.15903098781899,58.64413751846));
#155049=CARTESIAN_POINT('Ctrl Pts',(83.650056703569,-8.36102009624099,58.79617913494));
#155050=CARTESIAN_POINT('Ctrl Pts',(83.7034463744892,-8.69778689479599,
59.04151231842));
#155051=CARTESIAN_POINT('Ctrl Pts',(83.7509185106491,-9.02444336993198,
59.26641481374));
#155052=CARTESIAN_POINT('Ctrl Pts',(83.7699551026291,-9.16037518045798,
59.35769667413));
#155053=CARTESIAN_POINT('Origin',(82.1588614726791,-8.53712737026499,58.70184199665));
#155054=CARTESIAN_POINT('Origin',(82.1588614745091,-8.53712735484699,58.70184200704));
#155055=CARTESIAN_POINT('Ctrl Pts',(61.3269057219591,-8.495578707918,61.36288605057));
#155056=CARTESIAN_POINT('Ctrl Pts',(61.3647221303192,-8.51352689253799,
61.35621799746));
#155057=CARTESIAN_POINT('Ctrl Pts',(61.4169935891791,-8.53819570856299,
61.34700112894));
#155058=CARTESIAN_POINT('Ctrl Pts',(61.4693484792691,-8.56270798360799,
61.33776954924));
#155059=CARTESIAN_POINT('Ctrl Pts',(61.4837887359291,-8.56945389890299,
61.33522334239));
#155060=CARTESIAN_POINT('Ctrl Pts',(61.4076467126991,-8.16570792682499,
60.93289001715));
#155061=CARTESIAN_POINT('Ctrl Pts',(61.4449938331991,-8.18343338001699,
60.92630471215));
#155062=CARTESIAN_POINT('Ctrl Pts',(61.4966121580391,-8.20779394370498,
60.91720300878));
#155063=CARTESIAN_POINT('Ctrl Pts',(61.5483071585291,-8.23199726141499,
60.90808778543));
#155064=CARTESIAN_POINT('Ctrl Pts',(61.5625649852991,-8.23865795307699,
60.90557374588));
#155065=CARTESIAN_POINT('Ctrl Pts',(61.5943982728691,-7.69471886378999,
60.72426695352));
#155066=CARTESIAN_POINT('Ctrl Pts',(61.6310753447891,-7.712126301345,60.71779979617));
#155067=CARTESIAN_POINT('Ctrl Pts',(61.6817611257391,-7.73604674275599,
60.70886252545));
#155068=CARTESIAN_POINT('Ctrl Pts',(61.7325139367491,-7.75980893159299,
60.6999134355201));
#155069=CARTESIAN_POINT('Ctrl Pts',(61.7465112903491,-7.76634794106699,
60.69744532442));
#155070=CARTESIAN_POINT('Ctrl Pts',(61.8372995538392,-7.20836101379599,
60.79271718683));
#155071=CARTESIAN_POINT('Ctrl Pts',(61.8732847128991,-7.22544005858399,
60.78637203238));
#155072=CARTESIAN_POINT('Ctrl Pts',(61.9230075202292,-7.24890601614099,
60.77760455989));
#155073=CARTESIAN_POINT('Ctrl Pts',(61.9727873972891,-7.27221268168199,
60.76882702447));
#155074=CARTESIAN_POINT('Ctrl Pts',(61.9865157782691,-7.27862603836998,
60.7664063405));
#155075=CARTESIAN_POINT('',(61.3905222458867,-8.28493716412695,61.1354064364425));
#155076=CARTESIAN_POINT('Ctrl Pts',(61.3905294889791,-8.28492712720199,
61.13542050615));
#155077=CARTESIAN_POINT('Ctrl Pts',(61.4674394663872,-8.04432492131577,
60.924176948769));
#155078=CARTESIAN_POINT('Ctrl Pts',(61.5789829799692,-7.76585888253086,
60.8074607170329));
#155079=CARTESIAN_POINT('Ctrl Pts',(61.7095747601691,-7.48130386006799,
60.78445910689));
#155080=CARTESIAN_POINT('Ctrl Pts',(61.3905222458867,-8.28493716412695,
61.1354064364425));
#155081=CARTESIAN_POINT('Ctrl Pts',(61.439093656703,-8.31187513499146,61.1296186241446));
#155082=CARTESIAN_POINT('Ctrl Pts',(61.4877657995991,-8.3386626725425,61.1238255489273));
#155083=CARTESIAN_POINT('Ctrl Pts',(61.5365392768834,-8.36530895132786,
61.1180360527177));
#155084=CARTESIAN_POINT('Ctrl Pts',(62.6424555061691,-7.77604012554399,
59.87323994982));
#155085=CARTESIAN_POINT('Ctrl Pts',(61.8379543617991,-8.32413368283999,
61.12832290559));
#155086=CARTESIAN_POINT('Ctrl Pts',(60.8091181018691,-9.16035193985399,
62.11581956026));
#155087=CARTESIAN_POINT('Ctrl Pts',(59.7096837229991,-10.16199998466,62.67784534094));
#155088=CARTESIAN_POINT('Ctrl Pts',(61.9505428605791,-7.28867726858799,
59.92779417502));
#155089=CARTESIAN_POINT('Ctrl Pts',(61.0752928453991,-7.79388560581099,
61.12485983068));
#155090=CARTESIAN_POINT('Ctrl Pts',(59.9706799034791,-8.55606341233799,
62.04936186926));
#155091=CARTESIAN_POINT('Ctrl Pts',(58.7973007554591,-9.46702852828699,
62.55790618144));
#155092=CARTESIAN_POINT('Ctrl Pts',(61.0397767654491,-6.48728583724199,
59.97697348357));
#155093=CARTESIAN_POINT('Ctrl Pts',(60.0827831329091,-6.92037734173899,
61.08879812396));
#155094=CARTESIAN_POINT('Ctrl Pts',(58.8947164971891,-7.56515213793899,
61.92331331462));
#155095=CARTESIAN_POINT('Ctrl Pts',(57.6405715268691,-8.33435433040299,
62.35656344383));
#155096=CARTESIAN_POINT('Ctrl Pts',(60.0688746546991,-5.27194363025099,
60.00234697595));
#155097=CARTESIAN_POINT('Ctrl Pts',(59.0408262773091,-5.60461176273999,
61.0151475571));
#155098=CARTESIAN_POINT('Ctrl Pts',(57.7857638448791,-6.09372256888499,
61.74863088935));
#155099=CARTESIAN_POINT('Ctrl Pts',(56.4678784022591,-6.67671573941599,
62.09945975638));
#155100=CARTESIAN_POINT('Ctrl Pts',(59.4770560102391,-4.32125532974499,
60.00642490582));
#155101=CARTESIAN_POINT('Ctrl Pts',(58.4136231286291,-4.58127352118499,
60.95656721084));
#155102=CARTESIAN_POINT('Ctrl Pts',(57.1281453354791,-4.96056460946199,
61.62786539327));
#155103=CARTESIAN_POINT('Ctrl Pts',(55.7820195624491,-5.41264480586399,
61.92925370837));
#155104=CARTESIAN_POINT('Ctrl Pts',(59.0055325931291,-3.29999083432499,
60.00206093384));
#155105=CARTESIAN_POINT('Ctrl Pts',(57.9201032021691,-3.49064234678699,
60.90165448937));
#155106=CARTESIAN_POINT('Ctrl Pts',(56.6182263543491,-3.76707829037499,
61.52424896709));
#155107=CARTESIAN_POINT('Ctrl Pts',(55.2575867634991,-4.09661278804299,
61.78816659785));
#155108=CARTESIAN_POINT('Ctrl Pts',(58.5486233310291,-1.86656057990399,
59.99197481201));
#155109=CARTESIAN_POINT('Ctrl Pts',(57.4463566197091,-1.96891264366899,
60.84184399687));
#155110=CARTESIAN_POINT('Ctrl Pts',(56.1342847286391,-2.11626651270099,
61.41753985169));
#155111=CARTESIAN_POINT('Ctrl Pts',(54.7653910149991,-2.29199771900499,
61.64625014668));
#155112=CARTESIAN_POINT('Ctrl Pts',(58.3582172880991,-0.364152247367286,
59.98205701354));
#155113=CARTESIAN_POINT('Ctrl Pts',(57.2534029238191,-0.383925391423086,
60.81057084221));
#155114=CARTESIAN_POINT('Ctrl Pts',(55.9427550000591,-0.412412157066686,
61.36713327766));
#155115=CARTESIAN_POINT('Ctrl Pts',(54.5762064592391,-0.446400905279986,
61.58237710042));
#155116=CARTESIAN_POINT('Ctrl Pts',(58.4563178714691,1.13682553069601,59.98708278791));
#155117=CARTESIAN_POINT('Ctrl Pts',(57.3528856763591,1.19880013307101,60.82659338268));
#155118=CARTESIAN_POINT('Ctrl Pts',(56.0415920647091,1.28805985484101,61.39302436016));
#155119=CARTESIAN_POINT('Ctrl Pts',(54.6739248975291,1.39453885209001,61.61522897311));
#155120=CARTESIAN_POINT('Ctrl Pts',(58.6684090262891,2.24546507681701,59.99462082065));
#155121=CARTESIAN_POINT('Ctrl Pts',(57.5705549788991,2.37120525228701,60.85752631199));
#155122=CARTESIAN_POINT('Ctrl Pts',(56.2611536705391,2.55273821128001,61.44551740073));
#155123=CARTESIAN_POINT('Ctrl Pts',(54.8944216917291,2.76918920966101,61.68345776097));
#155124=CARTESIAN_POINT('Ctrl Pts',(59.0129434444591,3.31779743315801,60.00214865606));
#155125=CARTESIAN_POINT('Ctrl Pts',(57.9278466186591,3.50960883722001,60.90254051803));
#155126=CARTESIAN_POINT('Ctrl Pts',(56.6262103281791,3.78775995029701,61.52590143521));
#155127=CARTESIAN_POINT('Ctrl Pts',(55.2657813302291,4.11933921369801,61.79040654324));
#155128=CARTESIAN_POINT('Ctrl Pts',(59.4834197823591,4.33310144087101,60.00646456182));
#155129=CARTESIAN_POINT('Ctrl Pts',(58.4203057347191,4.59398713221801,60.95729393492));
#155130=CARTESIAN_POINT('Ctrl Pts',(57.1350750964291,4.97457145865601,61.62926036187));
#155131=CARTESIAN_POINT('Ctrl Pts',(55.7891716005991,5.42819059581601,61.93116907861));
#155132=CARTESIAN_POINT('Ctrl Pts',(60.0753871131491,5.27952185925301,60.00213395257));
#155133=CARTESIAN_POINT('Ctrl Pts',(59.0478312209291,5.61281571356601,61.01557669505));
#155134=CARTESIAN_POINT('Ctrl Pts',(57.7932429430791,6.10290620065401,61.74971718187));
#155135=CARTESIAN_POINT('Ctrl Pts',(56.4758102450491,6.68707454965501,62.10108184812));
#155136=CARTESIAN_POINT('Ctrl Pts',(61.0501979198291,6.49523278975501,59.97628350722));
#155137=CARTESIAN_POINT('Ctrl Pts',(60.0942006841991,6.92904513194801,61.08903090901));
#155138=CARTESIAN_POINT('Ctrl Pts',(58.9071773606691,7.57502746814901,61.9245323559));
#155139=CARTESIAN_POINT('Ctrl Pts',(57.6540464565791,8.34569757739901,62.35861252668));
#155140=CARTESIAN_POINT('Ctrl Pts',(61.9597595856491,7.29558295991301,59.92711980225));
#155141=CARTESIAN_POINT('Ctrl Pts',(61.0854258026491,7.80140074479901,61.12497890819));
#155142=CARTESIAN_POINT('Ctrl Pts',(59.9817847430291,8.56461376917001,62.05033656025));
#155143=CARTESIAN_POINT('Ctrl Pts',(58.8093524363191,9.47684203488101,62.5596047531));
#155144=CARTESIAN_POINT('Ctrl Pts',(62.6430578172491,7.77642528815001,59.87318767161));
#155145=CARTESIAN_POINT('Ctrl Pts',(61.8386206584491,8.32455263239701,61.12831924649));
#155146=CARTESIAN_POINT('Ctrl Pts',(60.8098537966191,9.16083079049501,62.11586923259));
#155147=CARTESIAN_POINT('Ctrl Pts',(59.7104872797291,10.16255263743,62.67794052264));
#155148=CARTESIAN_POINT('',(61.5365898356002,8.36429289895023,61.1191118314549));
#155149=CARTESIAN_POINT('Ctrl Pts',(59.6330698027491,9.92669722269101,62.60067754791));
#155150=CARTESIAN_POINT('Ctrl Pts',(60.2754754017191,9.36357130994093,62.26469288354));
#155151=CARTESIAN_POINT('Ctrl Pts',(60.931205048551,8.82195183547381,61.7699139266904));
#155152=CARTESIAN_POINT('Ctrl Pts',(61.5365886724991,8.36429728100001,61.11911541945));
#155153=CARTESIAN_POINT('',(61.3903529552591,8.28473912510079,61.1353684361582));
#155154=CARTESIAN_POINT('Ctrl Pts',(61.3903529552591,8.28473912510079,61.1353684361582));
#155155=CARTESIAN_POINT('Ctrl Pts',(61.3377118247909,8.25526241917844,61.141452580646));
#155156=CARTESIAN_POINT('Ctrl Pts',(61.2829644597506,8.22251248314273,61.1464748137686));
#155157=CARTESIAN_POINT('Ctrl Pts',(61.2264763926447,8.18609043811816,61.1501335755795));
#155158=CARTESIAN_POINT('Ctrl Pts',(61.1699883255388,8.14966839309358,61.1537923373904));
#155159=CARTESIAN_POINT('Ctrl Pts',(61.1117592919253,8.1095735985994,61.156087549914));
#155160=CARTESIAN_POINT('Ctrl Pts',(61.0522097613923,8.06541900563375,61.1567389103051));
#155161=CARTESIAN_POINT('Ctrl Pts',(60.9926602308594,8.02126441266811,61.1573902706961));
#155162=CARTESIAN_POINT('Ctrl Pts',(60.9317867017939,7.97308795619621,61.1564284489814));
#155163=CARTESIAN_POINT('Ctrl Pts',(60.8701400495052,7.92096701354577,61.1538370019321));
#155164=CARTESIAN_POINT('Ctrl Pts',(60.8393167233608,7.89490654222055,61.1525412784074));
#155165=CARTESIAN_POINT('Ctrl Pts',(60.808308205484,7.86788034015697,61.1508473165268));
#155166=CARTESIAN_POINT('Ctrl Pts',(60.7771694695725,7.83988606021754,61.1487516800523));
#155167=CARTESIAN_POINT('Ctrl Pts',(60.7616001016168,7.82588892024782,61.1477038618151));
#155168=CARTESIAN_POINT('Ctrl Pts',(60.7459972413712,7.81164787313224,61.1465548862943));
#155169=CARTESIAN_POINT('Ctrl Pts',(60.7303658056483,7.79715985209986,61.1453036153926));
#155170=CARTESIAN_POINT('Ctrl Pts',(60.7225500877868,7.78991584158367,61.1446779799418));
#155171=CARTESIAN_POINT('Ctrl Pts',(60.7147272264663,7.78261008726788,61.1440267714112));
#155172=CARTESIAN_POINT('Ctrl Pts',(60.7068978067353,7.77524228743362,61.1433499213563));
#155173=CARTESIAN_POINT('Ctrl Pts',(60.7029830968699,7.77155838751649,61.1430114963289));
#155174=CARTESIAN_POINT('Ctrl Pts',(60.6990667474229,7.76785897620417,61.1426666609589));
#155175=CARTESIAN_POINT('Ctrl Pts',(60.6951488303989,7.76414401835922,61.1423154092602));
#155176=CARTESIAN_POINT('Ctrl Pts',(60.6931898718869,7.76228653943675,61.1421397834109));
#155177=CARTESIAN_POINT('Ctrl Pts',(60.6912305214819,7.7604251738802,61.1419625534816));
#155178=CARTESIAN_POINT('Ctrl Pts',(60.6892707880624,7.75855991760359,61.1417837190025));
#155179=CARTESIAN_POINT('Ctrl Pts',(60.6873110546429,7.75669466132698,61.1416048845235));
#155180=CARTESIAN_POINT('Ctrl Pts',(60.6843542242277,7.75387325937131,61.1413318942811));
#155181=CARTESIAN_POINT('Ctrl Pts',(60.6833904476014,7.75295247262085,61.1412424015378));
#155182=CARTESIAN_POINT('Ctrl Pts',(60.6612792552886,7.73182756425257,61.1391892377623));
#155183=CARTESIAN_POINT('Ctrl Pts',(60.6355310995566,7.70686995188823,61.1366539398549));
#155184=CARTESIAN_POINT('Ctrl Pts',(60.6064952106979,7.67781946348534,61.1334020559537));
#155185=CARTESIAN_POINT('Ctrl Pts',(60.5781297503531,7.64943974069468,61.1302252569138));
#155186=CARTESIAN_POINT('Ctrl Pts',(60.5466265144245,7.61715345693505,61.1263643604354));
#155187=CARTESIAN_POINT('Ctrl Pts',(60.5123592417978,7.58071060291756,61.1216072593446));
#155188=CARTESIAN_POINT('Ctrl Pts',(60.4838518594743,7.55039332661272,61.1176497661111));
#155189=CARTESIAN_POINT('Ctrl Pts',(60.4534323333134,7.51719909725086,61.1130720895418));
#155190=CARTESIAN_POINT('Ctrl Pts',(60.4213429520122,7.48098377967267,61.107757168389));
#155191=CARTESIAN_POINT('Ctrl Pts',(60.3827970733818,7.43748181175304,61.1013728662498));
#155192=CARTESIAN_POINT('Ctrl Pts',(60.3418254808226,7.3896587533634,61.0939557525152));
#155193=CARTESIAN_POINT('Ctrl Pts',(60.2988462550389,7.337327249333,61.0853726381127));
#155194=CARTESIAN_POINT('Ctrl Pts',(60.2804176612785,7.31488859412073,61.0816923780419));
#155195=CARTESIAN_POINT('Ctrl Pts',(60.261620588273,7.29162113177491,61.077797883836));
#155196=CARTESIAN_POINT('Ctrl Pts',(60.2424908302629,7.2675105725611,61.0736793075588));
#155197=CARTESIAN_POINT('Ctrl Pts',(60.204597019692,7.21975037804492,61.0655208902285));
#155198=CARTESIAN_POINT('Ctrl Pts',(60.1651082495433,7.16825318712065,61.0563860736495));
#155199=CARTESIAN_POINT('Ctrl Pts',(60.1248164208882,7.11365044413259,61.0463747624552));
#155200=CARTESIAN_POINT('Ctrl Pts',(60.0973301082003,7.07640150017828,61.0395452379811));
#155201=CARTESIAN_POINT('Ctrl Pts',(60.0694694898623,7.03770787784243,61.0323079317492));
#155202=CARTESIAN_POINT('Ctrl Pts',(60.0414742272431,6.9977780246817,61.0246955120611));
#155203=CARTESIAN_POINT('Ctrl Pts',(59.9785441792343,6.90802042495623,61.0075836905736));
#155204=CARTESIAN_POINT('Ctrl Pts',(59.919583248113,6.81893395325138,60.989999556601));
#155205=CARTESIAN_POINT('Ctrl Pts',(59.8641613855649,6.73082734281785,60.9721977538004));
#155206=CARTESIAN_POINT('Ctrl Pts',(59.8367010755203,6.68717246136417,60.9633773532981));
#155207=CARTESIAN_POINT('Ctrl Pts',(59.8101093729386,6.64375740387163,60.954503165352));
#155208=CARTESIAN_POINT('Ctrl Pts',(59.7843328970857,6.60061556171698,60.9456043143883));
#155209=CARTESIAN_POINT('Ctrl Pts',(59.7300536100411,6.5097688359153,60.9268653956711));
#155210=CARTESIAN_POINT('Ctrl Pts',(59.6793896697743,6.42013687583715,60.9080181947062));
#155211=CARTESIAN_POINT('Ctrl Pts',(59.6318393284069,6.33199972875507,60.8893192919711));
#155212=CARTESIAN_POINT('Ctrl Pts',(59.5820720232687,6.23975331859895,60.8697485807753));
#155213=CARTESIAN_POINT('Ctrl Pts',(59.5357149928056,6.14914430700615,60.8503400762022));
#155214=CARTESIAN_POINT('Ctrl Pts',(59.4921887892894,6.0604382288152,60.8313706804393));
#155215=CARTESIAN_POINT('Ctrl Pts',(59.462012291282,5.99893875090234,60.8182192937527));
#155216=CARTESIAN_POINT('Ctrl Pts',(59.433196375619,5.9383527406437,60.8052786098179));
#155217=CARTESIAN_POINT('Ctrl Pts',(59.4055483710978,5.87875459662487,60.7926372591075));
#155218=CARTESIAN_POINT('Ctrl Pts',(59.3539010331536,5.76742339792561,60.769022820253));
#155219=CARTESIAN_POINT('Ctrl Pts',(59.3066122933732,5.65943881126518,60.7462375435995));
#155220=CARTESIAN_POINT('Ctrl Pts',(59.2630491139327,5.55506525212866,60.7244065722365));
#155221=CARTESIAN_POINT('Ctrl Pts',(59.2390317590691,5.49752177526686,60.7123706696009));
#155222=CARTESIAN_POINT('Ctrl Pts',(59.2161471056752,5.44107491983873,60.7006246744183));
#155223=CARTESIAN_POINT('Ctrl Pts',(59.1942897531849,5.38575787591432,60.6891897472044));
#155224=CARTESIAN_POINT('Ctrl Pts',(59.163538415909,5.30793174964514,60.6731018287965));
#155225=CARTESIAN_POINT('Ctrl Pts',(59.1348229842282,5.23234056849942,60.6576274853771));
#155226=CARTESIAN_POINT('Ctrl Pts',(59.107944785793,5.15908438941234,60.6427766703575));
#155227=CARTESIAN_POINT('Ctrl Pts',(59.0945056865755,5.1224562998688,60.6353512628477));
#155228=CARTESIAN_POINT('Ctrl Pts',(59.0815269848548,5.08641198790164,60.6280811498728));
#155229=CARTESIAN_POINT('Ctrl Pts',(59.0689869744624,5.05096271344002,60.6209655664145));
#155230=CARTESIAN_POINT('Ctrl Pts',(59.0627169692662,5.03323807620921,60.6174077746854));
#155231=CARTESIAN_POINT('Ctrl Pts',(59.0565566388387,5.01566219686254,60.613888618575));
#155232=CARTESIAN_POINT('Ctrl Pts',(59.0505034032855,4.99823635968953,60.6104079010811));
#155233=CARTESIAN_POINT('Ctrl Pts',(59.0474767855088,4.98952344110303,60.6086675423341));
#155234=CARTESIAN_POINT('Ctrl Pts',(59.0444769415938,4.98084803295673,60.606936793476));
#155235=CARTESIAN_POINT('Ctrl Pts',(59.0415035532834,4.97221029268076,60.605215628219));
#155236=CARTESIAN_POINT('Ctrl Pts',(59.0400168591282,4.96789142254277,60.6043550455905));
#155237=CARTESIAN_POINT('Ctrl Pts',(59.0385367788836,4.96358196936576,60.6034968588777));
#155238=CARTESIAN_POINT('Ctrl Pts',(59.0370632732322,4.95928195242892,60.6026410644859));
#155239=CARTESIAN_POINT('Ctrl Pts',(59.0363265204065,4.9571319439605,60.6022131672901));
#155240=CARTESIAN_POINT('Ctrl Pts',(59.0355914112297,4.95498429455169,60.6017858681754));
#155241=CARTESIAN_POINT('Ctrl Pts',(59.0348579408175,4.95283900658724,60.6013591666728));
#155242=CARTESIAN_POINT('Ctrl Pts',(59.0341244704053,4.95069371862278,60.6009324651701));
#155243=CARTESIAN_POINT('Ctrl Pts',(59.0338010189301,4.94974795186889,60.6007443358881));
#155244=CARTESIAN_POINT('Ctrl Pts',(59.0326624410009,4.94641022940329,60.6000808545276));
#155245=CARTESIAN_POINT('Ctrl Pts',(58.9796566010893,4.79102448184745,60.5691928618161));
#155246=CARTESIAN_POINT('Ctrl Pts',(58.930736484917,4.6357662566957,60.5392009258538));
#155247=CARTESIAN_POINT('Ctrl Pts',(58.8855150366211,4.48081331346773,60.5103268074466));
#155248=CARTESIAN_POINT('Ctrl Pts',(58.8268216235003,4.27969819102264,60.4728507728649));
#155249=CARTESIAN_POINT('Ctrl Pts',(58.7743573384257,4.07909742038663,60.4372557182607));
#155250=CARTESIAN_POINT('Ctrl Pts',(58.7271135166555,3.87967446387876,60.4039585698523));
#155251=CARTESIAN_POINT('Ctrl Pts',(58.7106768093691,3.81029276190213,60.3923740819479));
#155252=CARTESIAN_POINT('Ctrl Pts',(58.694871899034,3.74105316775628,60.3810676975273));
#155253=CARTESIAN_POINT('Ctrl Pts',(58.6796559307865,3.67198222607764,60.3700569153105));
#155254=CARTESIAN_POINT('Ctrl Pts',(58.6584438516869,3.57569270611219,60.3547071472557));
#155255=CARTESIAN_POINT('Ctrl Pts',(58.6383919111362,3.47973088583468,60.3399209525927));
#155256=CARTESIAN_POINT('Ctrl Pts',(58.619413783502,3.38410156360109,60.3257074772219));
#155257=CARTESIAN_POINT('Ctrl Pts',(58.5835603943274,3.20343909928238,60.2988554466203));
#155258=CARTESIAN_POINT('Ctrl Pts',(58.5515377751492,3.02396572657779,60.2740463222185));
#155259=CARTESIAN_POINT('Ctrl Pts',(58.5228608625712,2.84586567714671,60.2513143089754));
#155260=CARTESIAN_POINT('Ctrl Pts',(58.5004183251908,2.70648466791441,60.2335242468286));
#155261=CARTESIAN_POINT('Ctrl Pts',(58.4800258712364,2.56794413817846,60.21700666853));
#155262=CARTESIAN_POINT('Ctrl Pts',(58.4614664842412,2.43031879908165,60.2017861458073));
#155263=CARTESIAN_POINT('Ctrl Pts',(58.4541828756914,2.37630790439186,60.1958128704257));
#155264=CARTESIAN_POINT('Ctrl Pts',(58.4471815755868,2.32243511427534,60.1900389850738));
#155265=CARTESIAN_POINT('Ctrl Pts',(58.4404544275918,2.2687030578129,60.1844629675555));
#155266=CARTESIAN_POINT('Ctrl Pts',(58.4166125164259,2.07826947170898,60.1647008165773));
#155267=CARTESIAN_POINT('Ctrl Pts',(58.3962108898787,1.88960528727602,60.1474217544783));
#155268=CARTESIAN_POINT('Ctrl Pts',(58.3789027294227,1.70278520533782,60.1325898188454));
#155269=CARTESIAN_POINT('Ctrl Pts',(58.3643330923764,1.54552408023421,60.1201046145735));
#155270=CARTESIAN_POINT('Ctrl Pts',(58.3519565393527,1.38956933060372,60.1093539633021));
#155271=CARTESIAN_POINT('Ctrl Pts',(58.3415860474452,1.23495332602257,60.100332773935));
#155272=CARTESIAN_POINT('Ctrl Pts',(58.3395087708272,1.20398274006014,60.0985257713447));
#155273=CARTESIAN_POINT('Ctrl Pts',(58.3375123669455,1.17306470608009,60.0967878453344));
#155274=CARTESIAN_POINT('Ctrl Pts',(58.3355961354574,1.14220024887804,60.095118592652));
#155275=CARTESIAN_POINT('Ctrl Pts',(58.3254435033222,0.978673304477079,
60.0862745106455));
#155276=CARTESIAN_POINT('Ctrl Pts',(58.3175425203729,0.81665010430814,60.0793568043996));
#155277=CARTESIAN_POINT('Ctrl Pts',(58.311776746117,0.65624044993948,60.074314670715));
#155278=CARTESIAN_POINT('Ctrl Pts',(58.3083497361431,0.560897576452767,
60.0713177718321));
#155279=CARTESIAN_POINT('Ctrl Pts',(58.3056802608143,0.466130684709749,
60.0689816791386));
#155280=CARTESIAN_POINT('Ctrl Pts',(58.3037515412153,0.371970297407789,
60.0672905342075));
#155281=CARTESIAN_POINT('Ctrl Pts',(58.3027837784396,0.324723969935379,
60.0664419779354));
#155282=CARTESIAN_POINT('Ctrl Pts',(58.3020180653192,0.278177922856337,
60.0657590562465));
#155283=CARTESIAN_POINT('Ctrl Pts',(58.3014227085939,0.231511507082222,
60.06523424694));
#155284=CARTESIAN_POINT('Ctrl Pts',(58.3008315388136,0.185173280625659,
60.0647131284421));
#155285=CARTESIAN_POINT('Ctrl Pts',(58.3004083166453,0.138716286073158,
60.0643478840615));
#155286=CARTESIAN_POINT('Ctrl Pts',(58.3001726215235,0.091336347976081,
60.0641342783048));
#155287=CARTESIAN_POINT('Ctrl Pts',(58.3000397137522,0.0646189431954746,
60.0640138266602));
#155288=CARTESIAN_POINT('Ctrl Pts',(58.2999634391186,0.0378503959760054,
60.0639468458643));
#155289=CARTESIAN_POINT('Ctrl Pts',(58.2999452270056,0.0110309761453676,
60.0639338298282));
#155290=CARTESIAN_POINT('Ctrl Pts',(58.2998110086453,-0.186620913474732,
60.0638379051531));
#155291=CARTESIAN_POINT('Ctrl Pts',(58.302832431568,-0.387038543163136,
60.0666698817325));
#155292=CARTESIAN_POINT('Ctrl Pts',(58.3093125342766,-0.590061378700564,
60.072468905283));
#155293=CARTESIAN_POINT('Ctrl Pts',(58.3159292651874,-0.797364801485306,
60.0783901969824));
#155294=CARTESIAN_POINT('Ctrl Pts',(58.3261512202964,-1.00738343278767,
60.0874044096972));
#155295=CARTESIAN_POINT('Ctrl Pts',(58.340281980589,-1.2199202386454,60.0995982247504));
#155296=CARTESIAN_POINT('Ctrl Pts',(58.3540988771689,-1.42773630835026,
60.1115211983213));
#155297=CARTESIAN_POINT('Ctrl Pts',(58.3716517175546,-1.63795850118814,
60.1264839986969));
#155298=CARTESIAN_POINT('Ctrl Pts',(58.393221283897,-1.85039632962378,60.1446146025748));
#155299=CARTESIAN_POINT('Ctrl Pts',(58.4065868933095,-1.98203370212521,
60.1558492544912));
#155300=CARTESIAN_POINT('Ctrl Pts',(58.4214947794622,-2.11452173605364,
60.1683011786858));
#155301=CARTESIAN_POINT('Ctrl Pts',(58.4380143589673,-2.24781785929611,
60.1820103398356));
#155302=CARTESIAN_POINT('Ctrl Pts',(58.4404138660129,-2.26717942880672,
60.1840016271295));
#155303=CARTESIAN_POINT('Ctrl Pts',(58.4428473830314,-2.28655805460061,
60.1860194527049));
#155304=CARTESIAN_POINT('Ctrl Pts',(58.4453151528025,-2.3059535689316,60.1880639619441));
#155305=CARTESIAN_POINT('Ctrl Pts',(58.4690615709735,-2.49258929132516,
60.2077375035832));
#155306=CARTESIAN_POINT('Ctrl Pts',(58.4960924330805,-2.68091509646556,
60.2298223783291));
#155307=CARTESIAN_POINT('Ctrl Pts',(58.5269446035756,-2.87072609599083,
60.2542598726009));
#155308=CARTESIAN_POINT('Ctrl Pts',(58.5535927944882,-3.03467306216784,
60.2753674641359));
#155309=CARTESIAN_POINT('Ctrl Pts',(58.583091938661,-3.19972753045303,60.2982306841269));
#155310=CARTESIAN_POINT('Ctrl Pts',(58.6158096951469,-3.36574064915635,
60.322826922696));
#155311=CARTESIAN_POINT('Ctrl Pts',(58.6298388921635,-3.43692617652021,
60.3333736567576));
#155312=CARTESIAN_POINT('Ctrl Pts',(58.6444601564802,-3.50828776656749,
60.3442392130297));
#155313=CARTESIAN_POINT('Ctrl Pts',(58.6596998748985,-3.57981586985723,
60.3554201094352));
#155314=CARTESIAN_POINT('Ctrl Pts',(58.6965915521465,-3.7529681308318,60.3824863589691));
#155315=CARTESIAN_POINT('Ctrl Pts',(58.7371370372468,-3.92707067059017,
60.4113704999466));
#155316=CARTESIAN_POINT('Ctrl Pts',(58.7819106933059,-4.10185860030788,
60.4418732050604));
#155317=CARTESIAN_POINT('Ctrl Pts',(58.7929214942294,-4.14484269558513,
60.4493744735115));
#155318=CARTESIAN_POINT('Ctrl Pts',(58.8041881504347,-4.187868046168,60.4569736423612));
#155319=CARTESIAN_POINT('Ctrl Pts',(58.8157195053545,-4.23093031976178,
60.4646677664296));
#155320=CARTESIAN_POINT('Ctrl Pts',(58.836795293484,-4.30963497857667,60.4787302707785));
#155321=CARTESIAN_POINT('Ctrl Pts',(58.8587520838187,-4.38846373130315,
60.493112292388));
#155322=CARTESIAN_POINT('Ctrl Pts',(58.8816491331759,-4.46737832075861,
60.5077891134032));
#155323=CARTESIAN_POINT('Ctrl Pts',(58.8904872180244,-4.49783874500423,
60.5134542533702));
#155324=CARTESIAN_POINT('Ctrl Pts',(58.8994653992315,-4.52831193526029,
60.519163314747));
#155325=CARTESIAN_POINT('Ctrl Pts',(58.9085869514967,-4.55879700219545,
60.5249146864526));
#155326=CARTESIAN_POINT('Ctrl Pts',(58.9249634454014,-4.61352875160944,
60.5352404841831));
#155327=CARTESIAN_POINT('Ctrl Pts',(58.9418038125052,-4.6682965230225,60.5457007137537));
#155328=CARTESIAN_POINT('Ctrl Pts',(58.9591302413778,-4.72308788085057,
60.5562809970971));
#155329=CARTESIAN_POINT('Ctrl Pts',(58.9677934558141,-4.75048355976461,
60.5615711387687));
#155330=CARTESIAN_POINT('Ctrl Pts',(58.9765781842021,-4.77788513687593,
60.5668912911526));
#155331=CARTESIAN_POINT('Ctrl Pts',(58.9854871327347,-4.80529091555044,
60.5722396150746));
#155332=CARTESIAN_POINT('Ctrl Pts',(58.9899416070011,-4.81899380488769,
60.5749137770356));
#155333=CARTESIAN_POINT('Ctrl Pts',(58.9944271361751,-4.83269774470628,
60.5775949816723));
#155334=CARTESIAN_POINT('Ctrl Pts',(58.9989440554225,-4.84640251863526,
60.5802829973539));
#155335=CARTESIAN_POINT('Ctrl Pts',(59.0012025150462,-4.85325490559974,
60.5816270051946));
#155336=CARTESIAN_POINT('Ctrl Pts',(59.0034688221802,-4.86010750109739,
60.5829727157835));
#155337=CARTESIAN_POINT('Ctrl Pts',(59.0057430184444,-4.86696027757705,
60.5843201000103));
#155338=CARTESIAN_POINT('Ctrl Pts',(59.0068801165765,-4.87038666581687,
60.5849937921237));
#155339=CARTESIAN_POINT('Ctrl Pts',(59.0080191869907,-4.87381309930254,
60.5856679026457));
#155340=CARTESIAN_POINT('Ctrl Pts',(59.0091602348704,-4.87723957455611,
60.5863424279278));
#155341=CARTESIAN_POINT('Ctrl Pts',(59.01030128275,-4.88066604980967,60.5870169532098));
#155342=CARTESIAN_POINT('Ctrl Pts',(59.0118496790891,-4.8853056816243,60.5879309900696));
#155343=CARTESIAN_POINT('Ctrl Pts',(59.0125893160822,-4.88751912213284,
60.5883672444004));
#155344=CARTESIAN_POINT('Ctrl Pts',(59.0466683952197,-4.98950430534963,
60.6084678424014));
#155345=CARTESIAN_POINT('Ctrl Pts',(59.084110335281,-5.09640993499694,60.6299095208549));
#155346=CARTESIAN_POINT('Ctrl Pts',(59.1255979348175,-5.20796002104424,
60.6526112582718));
#155347=CARTESIAN_POINT('Ctrl Pts',(59.165827699191,-5.3161280936172,60.6746247166873));
#155348=CARTESIAN_POINT('Ctrl Pts',(59.2098617926801,-5.42866360276206,
60.6978233217053));
#155349=CARTESIAN_POINT('Ctrl Pts',(59.2583639538129,-5.54529390482577,
60.7221259849945));
#155350=CARTESIAN_POINT('Ctrl Pts',(59.2987976607154,-5.6425224682432,60.7423858402553));
#155351=CARTESIAN_POINT('Ctrl Pts',(59.3423371250503,-5.74259666554944,
60.7634127529908));
#155352=CARTESIAN_POINT('Ctrl Pts',(59.3893976796749,-5.84533900592405,
60.7851613181427));
#155353=CARTESIAN_POINT('Ctrl Pts',(59.4334172168723,-5.9414422140131,60.8055045074726));
#155354=CARTESIAN_POINT('Ctrl Pts',(59.4805056426105,-6.03988847527971,
60.826490027304));
#155355=CARTESIAN_POINT('Ctrl Pts',(59.5312764880216,-6.14041774579453,
60.8478786261836));
#155356=CARTESIAN_POINT('Ctrl Pts',(59.5737720098771,-6.22456138724261,
60.8657810200434));
#155357=CARTESIAN_POINT('Ctrl Pts',(59.6188477085341,-6.3101637636052,60.883965731171));
#155358=CARTESIAN_POINT('Ctrl Pts',(59.666867193762,-6.39704577233237,60.9022838917411));
#155359=CARTESIAN_POINT('Ctrl Pts',(59.7022865976223,-6.46113036092596,
60.9157954553103));
#155360=CARTESIAN_POINT('Ctrl Pts',(59.7393264044079,-6.52590512609024,
60.9293660785788));
#155361=CARTESIAN_POINT('Ctrl Pts',(59.7781648402363,-6.59126771537316,
60.9429035856504));
#155362=CARTESIAN_POINT('Ctrl Pts',(59.7971080468353,-6.62314791358959,
60.9495064209042));
#155363=CARTESIAN_POINT('Ctrl Pts',(59.8164791148336,-6.65516778169856,
60.9561013135051));
#155364=CARTESIAN_POINT('Ctrl Pts',(59.8362984871501,-6.68731447842764,
60.9626770974503));
#155365=CARTESIAN_POINT('Ctrl Pts',(59.8665255735293,-6.73634231661122,
60.9727060118956));
#155366=CARTESIAN_POINT('Ctrl Pts',(59.8977906010286,-6.78566703466396,
60.9826941806909));
#155367=CARTESIAN_POINT('Ctrl Pts',(59.930185682024,-6.83522716113299,60.9925823374755));
#155368=CARTESIAN_POINT('Ctrl Pts',(59.9517635487066,-6.86823840138494,
60.9991686870779));
#155369=CARTESIAN_POINT('Ctrl Pts',(59.973545298576,-6.90091096020029,61.0056234497311));
#155370=CARTESIAN_POINT('Ctrl Pts',(59.9961709624893,-6.93410116671089,
61.012085605819));
#155371=CARTESIAN_POINT('Ctrl Pts',(60.0075134487101,-6.95073977061893,
61.0153251534701));
#155372=CARTESIAN_POINT('Ctrl Pts',(60.0190687714284,-6.96750821772436,
61.0185665818014));
#155373=CARTESIAN_POINT('Ctrl Pts',(60.0309222556114,-6.98451278948907,
61.0218275075584));
#155374=CARTESIAN_POINT('Ctrl Pts',(60.0795079257767,-7.05421200216824,
61.0351935576426));
#155375=CARTESIAN_POINT('Ctrl Pts',(60.1269746556736,-7.11911555985469,
61.0472183111237));
#155376=CARTESIAN_POINT('Ctrl Pts',(60.1728493085623,-7.17939944829445,
61.0579965072052));
#155377=CARTESIAN_POINT('Ctrl Pts',(60.2188885679778,-7.23989964619653,
61.0688133773978));
#155378=CARTESIAN_POINT('Ctrl Pts',(60.2633242216992,-7.29574725332997,
61.0783747962133));
#155379=CARTESIAN_POINT('Ctrl Pts',(60.3057283855415,-7.34712996019628,
61.0867886051467));
#155380=CARTESIAN_POINT('Ctrl Pts',(60.3445567285779,-7.39417971162545,
61.0944929018456));
#155381=CARTESIAN_POINT('Ctrl Pts',(60.3816823380303,-7.43748612756068,
61.1012351771947));
#155382=CARTESIAN_POINT('Ctrl Pts',(60.4168140181179,-7.47719724058691,
61.1071061410174));
#155383=CARTESIAN_POINT('Ctrl Pts',(60.4552298300096,-7.52062057372167,
61.1135259262732));
#155384=CARTESIAN_POINT('Ctrl Pts',(60.4912460540125,-7.55971785059863,
61.1188948231495));
#155385=CARTESIAN_POINT('Ctrl Pts',(60.5244579042493,-7.59471761046306,
61.1233979425645));
#155386=CARTESIAN_POINT('Ctrl Pts',(60.5395427633062,-7.61061454004744,
61.1254432643761));
#155387=CARTESIAN_POINT('Ctrl Pts',(60.5540497928784,-7.6256661838935,61.1273101159803));
#155388=CARTESIAN_POINT('Ctrl Pts',(60.5679445416861,-7.63989391794987,
61.129016460982));
#155389=CARTESIAN_POINT('Ctrl Pts',(60.590187727431,-7.66267015778862,61.1317480360066));
#155390=CARTESIAN_POINT('Ctrl Pts',(60.6108585027185,-7.68333953919245,
61.1340723320172));
#155391=CARTESIAN_POINT('Ctrl Pts',(60.6298219773043,-7.70200106833081,
61.1360750499524));
#155392=CARTESIAN_POINT('Ctrl Pts',(60.6393037145972,-7.71133183289999,
61.13707640892));
#155393=CARTESIAN_POINT('Ctrl Pts',(60.6483588771974,-7.72016062410416,
61.1379973961989));
#155394=CARTESIAN_POINT('Ctrl Pts',(60.6569723142693,-7.72849936884094,
61.1388484909094));
#155395=CARTESIAN_POINT('Ctrl Pts',(60.6612790328052,-7.73266874120932,
61.1392740382647));
#155396=CARTESIAN_POINT('Ctrl Pts',(60.6654753229127,-7.73671559834878,
61.1396821182107));
#155397=CARTESIAN_POINT('Ctrl Pts',(60.6695594308556,-7.74064136924075,
61.1400739857034));
#155398=CARTESIAN_POINT('Ctrl Pts',(60.671601484827,-7.74260425468674,61.1402699194497));
#155399=CARTESIAN_POINT('Ctrl Pts',(60.673615493437,-7.74453686835117,61.1404618004314));
#155400=CARTESIAN_POINT('Ctrl Pts',(60.6756012425935,-7.74643938498901,
61.14064978388));
#155401=CARTESIAN_POINT('Ctrl Pts',(60.6765941171717,-7.74739064330793,
61.1407437756042));
#155402=CARTESIAN_POINT('Ctrl Pts',(60.6775799268976,-7.74833437735662,
61.1408367929666));
#155403=CARTESIAN_POINT('Ctrl Pts',(60.6785586455364,-7.74927060869726,
61.1409288551345));
#155404=CARTESIAN_POINT('Ctrl Pts',(60.6790480048557,-7.74973872436758,
61.1409748862185));
#155405=CARTESIAN_POINT('Ctrl Pts',(60.6792845347018,-7.74996512345502,
61.1409972458477));
#155406=CARTESIAN_POINT('Ctrl Pts',(60.6796448082126,-7.75030958071681,
61.1410310685549));
#155407=CARTESIAN_POINT('Ctrl Pts',(60.6800050817235,-7.75065403797859,
61.1410648912622));
#155408=CARTESIAN_POINT('Ctrl Pts',(60.6804890921598,-7.75111656176834,
61.1411101639344));
#155409=CARTESIAN_POINT('Ctrl Pts',(60.6814735021436,-7.7520568160311,61.141202195187));
#155410=CARTESIAN_POINT('Ctrl Pts',(60.7528816833991,-7.82026198250822,
61.1478780563335));
#155411=CARTESIAN_POINT('Ctrl Pts',(60.8238848687323,-7.88340841251751,
61.1524435095519));
#155412=CARTESIAN_POINT('Ctrl Pts',(60.8937477621502,-7.9414195808411,61.1549060387511));
#155413=CARTESIAN_POINT('Ctrl Pts',(60.9471625836398,-7.98577297144389,
61.1567888058561));
#155414=CARTESIAN_POINT('Ctrl Pts',(60.9999109579355,-8.02712549905052,
61.1574426075799));
#155415=CARTESIAN_POINT('Ctrl Pts',(61.0516739198898,-8.06545973778738,
61.1568778797576));
#155416=CARTESIAN_POINT('Ctrl Pts',(61.1080967748886,-8.10724496629978,
61.1562623130506));
#155417=CARTESIAN_POINT('Ctrl Pts',(61.1633153009485,-8.14537779070647,
61.1541689353691));
#155418=CARTESIAN_POINT('Ctrl Pts',(61.2169696534685,-8.18019173053023,
61.1508389703513));
#155419=CARTESIAN_POINT('Ctrl Pts',(61.2718447722498,-8.2157977716684,61.1474332405771));
#155420=CARTESIAN_POINT('Ctrl Pts',(61.3250837590809,-8.24793265307407,
61.142734006002));
#155421=CARTESIAN_POINT('Ctrl Pts',(61.3763514670402,-8.27696343931164,
61.1370178861163));
#155422=CARTESIAN_POINT('Ctrl Pts',(61.3810919615122,-8.27964778560205,
61.1364893422083));
#155423=CARTESIAN_POINT('Ctrl Pts',(61.3858156359089,-8.28230559643327,
61.1359521168453));
#155424=CARTESIAN_POINT('Ctrl Pts',(61.3905222458867,-8.28493716412695,
61.1354064364425));
#155425=CARTESIAN_POINT('Ctrl Pts',(61.5360580239853,8.3650447551965,61.1180922520029));
#155426=CARTESIAN_POINT('Ctrl Pts',(61.4873816218952,8.33842428962667,61.1238514036551));
#155427=CARTESIAN_POINT('Ctrl Pts',(61.4388137622094,8.31165854192863,61.1296130433924));
#155428=CARTESIAN_POINT('Ctrl Pts',(61.3903529552591,8.28473912510079,61.1353684361582));
#155429=CARTESIAN_POINT('Ctrl Pts',(61.4825779928491,8.56882230360101,61.3353622561));
#155430=CARTESIAN_POINT('Ctrl Pts',(61.4672316263191,8.56165228818601,61.33806823458));
#155431=CARTESIAN_POINT('Ctrl Pts',(61.4152057427591,8.53728542810601,61.34724180155));
#155432=CARTESIAN_POINT('Ctrl Pts',(61.3632704362791,8.51275974164101,61.35639939733));
#155433=CARTESIAN_POINT('Ctrl Pts',(61.3266920462791,8.49538778255501,61.3628491544));
#155434=CARTESIAN_POINT('Ctrl Pts',(61.5613777885692,8.23803123183401,60.90576138986));
#155435=CARTESIAN_POINT('Ctrl Pts',(61.5462338697091,8.23095580226301,60.90843167135));
#155436=CARTESIAN_POINT('Ctrl Pts',(61.4948919947391,8.20690930668701,60.91748462915));
#155437=CARTESIAN_POINT('Ctrl Pts',(61.4436315449591,8.18270232868401,60.92652322949));
#155438=CARTESIAN_POINT('Ctrl Pts',(61.4075243290991,8.16555414216201,60.9328899058401));
#155439=CARTESIAN_POINT('Ctrl Pts',(61.7453363893891,7.76575783100901,60.69766018174));
#155440=CARTESIAN_POINT('Ctrl Pts',(61.7304815069191,7.75881744250201,60.70027949832));
#155441=CARTESIAN_POINT('Ctrl Pts',(61.6801161971691,7.73522833422001,60.70916026132));
#155442=CARTESIAN_POINT('Ctrl Pts',(61.629819246419,7.71147637916701,60.71802897078));
#155443=CARTESIAN_POINT('Ctrl Pts',(61.5943847301191,7.69464767475702,60.72427703205));
#155444=CARTESIAN_POINT('Ctrl Pts',(61.9853446639591,7.27807903569201,60.76661281361));
#155445=CARTESIAN_POINT('Ctrl Pts',(61.9707882461391,7.27127809324201,60.76917950281));
#155446=CARTESIAN_POINT('Ctrl Pts',(61.9214313568291,7.24816129207001,60.77788245408));
#155447=CARTESIAN_POINT('Ctrl Pts',(61.8721293341091,7.22487920265801,60.78657573089));
#155448=CARTESIAN_POINT('Ctrl Pts',(61.8373894605991,7.20838040175501,60.79270130789));
#155449=CARTESIAN_POINT('Ctrl Pts',(61.3903603269491,8.28472891518701,61.13538275197));
#155450=CARTESIAN_POINT('Ctrl Pts',(61.4655545379308,8.04965156496637,60.9289822447848));
#155451=CARTESIAN_POINT('Ctrl Pts',(61.5757173213241,7.77270711240031,60.8080469803564));
#155452=CARTESIAN_POINT('Ctrl Pts',(61.7095796149691,7.48128536884801,60.78445823578));
#155453=CARTESIAN_POINT('Ctrl Pts',(61.536589981978,8.36429305416126,61.1191117063875));
#155454=CARTESIAN_POINT('Ctrl Pts',(61.5728698807379,8.24718616881929,61.0162396390448));
#155455=CARTESIAN_POINT('Ctrl Pts',(61.6197151052205,8.11435345893999,60.9298413020711));
#155456=CARTESIAN_POINT('Ctrl Pts',(61.7286246545714,7.83494047062615,60.8068890704171));
#155457=CARTESIAN_POINT('Ctrl Pts',(61.79052732657,7.68874228281837,60.7704317967065));
#155458=CARTESIAN_POINT('Ctrl Pts',(61.8548446843791,7.54727709634001,60.75884806608));
#155459=CARTESIAN_POINT('Ctrl Pts',(64.5445770840491,9.98588384555501,60.99915285191));
#155460=CARTESIAN_POINT('Ctrl Pts',(64.1994083728391,9.86085233672401,61.06001540859));
#155461=CARTESIAN_POINT('Ctrl Pts',(63.4820912895591,9.587604127095,61.18649776409));
#155462=CARTESIAN_POINT('Ctrl Pts',(62.4046333853091,9.13665291821101,61.37648266319));
#155463=CARTESIAN_POINT('Ctrl Pts',(61.6766080692791,8.80504019941101,61.50485316905));
#155464=CARTESIAN_POINT('Ctrl Pts',(61.3149677140191,8.63437250107801,61.56862012099));
#155465=CARTESIAN_POINT('Ctrl Pts',(64.5630006955291,9.66255945666802,60.43942959882));
#155466=CARTESIAN_POINT('Ctrl Pts',(64.2212742212191,9.53877485330901,60.4996851962601));
#155467=CARTESIAN_POINT('Ctrl Pts',(63.5109376432391,9.26818929731802,60.6249367003401));
#155468=CARTESIAN_POINT('Ctrl Pts',(62.4432659544991,8.82134180562501,60.81319602561));
#155469=CARTESIAN_POINT('Ctrl Pts',(61.7212021268391,8.49245145827502,60.94051536022));
#155470=CARTESIAN_POINT('Ctrl Pts',(61.3622879725491,8.32307031229001,61.00380160938));
#155471=CARTESIAN_POINT('Ctrl Pts',(64.7154346237891,9.10274130524401,60.15388495627));
#155472=CARTESIAN_POINT('Ctrl Pts',(64.3796681907591,8.98111564918601,60.21308963763));
#155473=CARTESIAN_POINT('Ctrl Pts',(63.6814179684591,8.71514032950402,60.33620999111));
#155474=CARTESIAN_POINT('Ctrl Pts',(62.6306905662491,8.27539819531201,60.52148158149));
#155475=CARTESIAN_POINT('Ctrl Pts',(61.9189487232691,7.95122148233401,60.6469808717));
#155476=CARTESIAN_POINT('Ctrl Pts',(61.5647548339591,7.78406793000301,60.70943481079));
#155477=CARTESIAN_POINT('Ctrl Pts',(64.9475416382091,8.50598449258701,60.24430535246));
#155478=CARTESIAN_POINT('Ctrl Pts',(64.6181285097791,8.38666023834401,60.3023897748));
#155479=CARTESIAN_POINT('Ctrl Pts',(63.9327621410791,8.12559935367801,60.42323835727));
#155480=CARTESIAN_POINT('Ctrl Pts',(62.9000970656791,7.69343141207701,60.6053250721));
#155481=CARTESIAN_POINT('Ctrl Pts',(62.1993582862391,7.37427935472601,60.72888422534));
#155482=CARTESIAN_POINT('Ctrl Pts',(61.8501961206591,7.20950038007601,60.79045093578));
#155483=CARTESIAN_POINT('',(64.4193726617333,9.7592596408602,60.7791711866962));
#155484=CARTESIAN_POINT('Origin',(64.963170393819,8.73683398597385,61.7327853056315));
#155485=CARTESIAN_POINT('Ctrl Pts',(64.4195454322906,9.75893531368795,60.7794745133828));
#155486=CARTESIAN_POINT('Ctrl Pts',(64.1788703740164,9.6579680563156,60.8084988936834));
#155487=CARTESIAN_POINT('Ctrl Pts',(63.9381154510292,9.55304684809677,60.8372628737177));
#155488=CARTESIAN_POINT('Ctrl Pts',(63.697456498012,9.44426471655492,60.8658538895038));
#155489=CARTESIAN_POINT('Ctrl Pts',(63.4577439202741,9.33591036348895,60.8943324730275));
#155490=CARTESIAN_POINT('Ctrl Pts',(63.2181262646531,9.22372625169533,60.9226400368081));
#155491=CARTESIAN_POINT('Ctrl Pts',(62.9787286335067,9.10780870892131,60.9508448865463));
#155492=CARTESIAN_POINT('Ctrl Pts',(62.7379133045354,8.99120470969623,60.9792167636437));
#155493=CARTESIAN_POINT('Ctrl Pts',(62.4973203663039,8.87082394515049,61.0074853213969));
#155494=CARTESIAN_POINT('Ctrl Pts',(62.2570317776485,8.7467548208856,61.0356926206112));
#155495=CARTESIAN_POINT('Ctrl Pts',(62.0298535183495,8.62945500302505,61.0623609079855));
#155496=CARTESIAN_POINT('Ctrl Pts',(61.8029467202873,8.50885904290689,61.088974601359));
#155497=CARTESIAN_POINT('Ctrl Pts',(61.5763469233615,8.38502077013121,61.1155396989721));
#155498=CARTESIAN_POINT('Ctrl Pts',(61.5632699767427,8.37787413317734,61.1170727557891));
#155499=CARTESIAN_POINT('Ctrl Pts',(61.5501940441027,8.37071669029369,61.1186056418031));
#155500=CARTESIAN_POINT('Ctrl Pts',(61.5371191292109,8.36354844880146,61.1201383548072));
#155501=CARTESIAN_POINT('Ctrl Pts',(62.7515737541991,12.07774640868,63.001901751759));
#155502=CARTESIAN_POINT('Ctrl Pts',(64.5503514671391,9.66775772102602,61.57390007131));
#155503=CARTESIAN_POINT('Ctrl Pts',(65.8339234114092,8.34497068419502,58.77515659908));
#155504=CARTESIAN_POINT('Ctrl Pts',(66.1844451731991,8.55990068685403,55.42750337263));
#155505=CARTESIAN_POINT('Ctrl Pts',(61.5063898405791,11.44707601721,62.90835246028));
#155506=CARTESIAN_POINT('Ctrl Pts',(63.5763627523891,9.04690003902301,61.51844654984));
#155507=CARTESIAN_POINT('Ctrl Pts',(65.0655865226491,7.76869735204601,58.6407671082601));
#155508=CARTESIAN_POINT('Ctrl Pts',(65.4573779299991,8.07974756896001,55.17405404619));
#155509=CARTESIAN_POINT('Ctrl Pts',(60.3778000932491,10.72664715258,62.77986335145));
#155510=CARTESIAN_POINT('Ctrl Pts',(62.7295784718991,8.36060988985802,61.4444601686601));
#155511=CARTESIAN_POINT('Ctrl Pts',(64.4134291656991,7.13761983681501,58.48792002224));
#155512=CARTESIAN_POINT('Ctrl Pts',(64.8046720640391,7.53823008741401,54.89307383022));
#155513=CARTESIAN_POINT('Ctrl Pts',(59.3595858619191,9.916504400752,62.64129573267));
#155514=CARTESIAN_POINT('Ctrl Pts',(61.9983452479491,7.63333056293401,61.37410196926));
#155515=CARTESIAN_POINT('Ctrl Pts',(63.8659652165791,6.48021923494602,58.34220507549));
#155516=CARTESIAN_POINT('Ctrl Pts',(64.2231019555691,6.94207966240701,54.6147516902));
#155517=CARTESIAN_POINT('Ctrl Pts',(62.6708095529579,11.8749837583452,62.9186045084915));
#155518=CARTESIAN_POINT('Ctrl Pts',(62.7578181479658,11.7616266579273,62.8481545770921));
#155519=CARTESIAN_POINT('Ctrl Pts',(62.8449003046356,11.6491939411928,62.7730948511703));
#155520=CARTESIAN_POINT('Ctrl Pts',(62.9318200968733,11.5380437482938,62.6933908725665));
#155521=CARTESIAN_POINT('Ctrl Pts',(63.0199125448919,11.4253940014626,62.6126115884555));
#155522=CARTESIAN_POINT('Ctrl Pts',(63.1078380140172,11.314062011975,62.5270614846297));
#155523=CARTESIAN_POINT('Ctrl Pts',(63.1953366462701,11.2044299246556,62.4367574345381));
#155524=CARTESIAN_POINT('Ctrl Pts',(63.2799927685102,11.0983593822187,62.3493870322072));
#155525=CARTESIAN_POINT('Ctrl Pts',(63.3642490279793,10.9938805260787,62.2575666328219));
#155526=CARTESIAN_POINT('Ctrl Pts',(63.4478607751725,10.8913418736331,62.1613622370055));
#155527=CARTESIAN_POINT('Ctrl Pts',(63.530982892732,10.7894036866067,62.065721213259));
#155528=CARTESIAN_POINT('Ctrl Pts',(63.6134677475192,10.6893834687848,61.9657473366532));
#155529=CARTESIAN_POINT('Ctrl Pts',(63.6950698661447,10.5916197585739,61.8615564717354));
#155530=CARTESIAN_POINT('Ctrl Pts',(63.7761228081869,10.4945139913338,61.7580668040926));
#155531=CARTESIAN_POINT('Ctrl Pts',(63.856304567228,10.3996348795351,61.6504167624718));
#155532=CARTESIAN_POINT('Ctrl Pts',(63.9353737663347,10.3073040540845,61.5387704012505));
#155533=CARTESIAN_POINT('Ctrl Pts',(63.9449132764184,10.2961645604464,61.5253005343401));
#155534=CARTESIAN_POINT('Ctrl Pts',(63.9544365943459,10.2850621426659,61.511772557708));
#155535=CARTESIAN_POINT('Ctrl Pts',(63.9639432985778,10.2739973509954,61.4981868088115));
#155536=CARTESIAN_POINT('Ctrl Pts',(64.042387156448,10.1826970513345,61.3860850194318));
#155537=CARTESIAN_POINT('Ctrl Pts',(64.1197402632482,10.0939126076095,61.2699867480628));
#155538=CARTESIAN_POINT('Ctrl Pts',(64.1957551375657,10.0079657234468,61.150117356748));
#155539=CARTESIAN_POINT('Ctrl Pts',(64.2717700118831,9.92201883928409,61.0302479654333));
#155540=CARTESIAN_POINT('Ctrl Pts',(64.3464463024524,9.83890998680352,60.9066076599331));
#155541=CARTESIAN_POINT('Ctrl Pts',(64.4195454322906,9.75893531368794,60.7794745133828));
#155542=CARTESIAN_POINT('Ctrl Pts',(84.4901667991491,11.93708079303,59.09834125997));
#155543=CARTESIAN_POINT('Ctrl Pts',(83.9147835748191,11.31851875633,58.92696924491));
#155544=CARTESIAN_POINT('Ctrl Pts',(82.8290630913291,10.28891810155,58.40666372177));
#155545=CARTESIAN_POINT('Ctrl Pts',(81.7119670519691,9.50097580768701,57.48286963236));
#155546=CARTESIAN_POINT('Ctrl Pts',(81.2581645020491,9.22984081121201,57.03752908385));
#155547=CARTESIAN_POINT('Ctrl Pts',(83.6617321185691,12.17586092735,59.3644367066));
#155548=CARTESIAN_POINT('Ctrl Pts',(83.1307067314591,11.57135929148,59.15364085641));
#155549=CARTESIAN_POINT('Ctrl Pts',(82.1344977737191,10.57540906728,58.58332876952));
#155550=CARTESIAN_POINT('Ctrl Pts',(81.1085173115291,9.81898400595401,57.65781121812));
#155551=CARTESIAN_POINT('Ctrl Pts',(80.6895279691791,9.55843631046701,57.21938802614));
#155552=CARTESIAN_POINT('Ctrl Pts',(82.0144069406191,12.57231964261,59.89501020394));
#155553=CARTESIAN_POINT('Ctrl Pts',(81.5669966029291,12.00452484203,59.62213429887));
#155554=CARTESIAN_POINT('Ctrl Pts',(80.7361758999491,11.08327377401,58.97893486564));
#155555=CARTESIAN_POINT('Ctrl Pts',(79.8788943064191,10.38652959513,58.05985965617));
#155556=CARTESIAN_POINT('Ctrl Pts',(79.5256597583991,10.1446658366,57.63620001424));
#155557=CARTESIAN_POINT('Ctrl Pts',(79.7945501172291,12.9266341776,60.56116805791));
#155558=CARTESIAN_POINT('Ctrl Pts',(79.4523719769991,12.40990839757,60.23657063794));
#155559=CARTESIAN_POINT('Ctrl Pts',(78.8208983604991,11.57901923841,59.53893424688));
#155560=CARTESIAN_POINT('Ctrl Pts',(78.1654256105091,10.94422155279,58.63373828109));
#155561=CARTESIAN_POINT('Ctrl Pts',(77.8929235677491,10.7202982577,58.22585805));
#155562=CARTESIAN_POINT('Ctrl Pts',(77.9640422107791,13.12680188932,61.05599713268));
#155563=CARTESIAN_POINT('Ctrl Pts',(77.7041168382291,12.64242377406,60.70217368394));
#155564=CARTESIAN_POINT('Ctrl Pts',(77.2248237057191,11.86642305288,59.97395619231));
#155565=CARTESIAN_POINT('Ctrl Pts',(76.7232189414891,11.26765541666,59.07462987159));
#155566=CARTESIAN_POINT('Ctrl Pts',(76.5132178516091,11.05395427136,58.67443825277));
#155567=CARTESIAN_POINT('Ctrl Pts',(76.5484058674291,13.23564492474,61.40514351714));
#155568=CARTESIAN_POINT('Ctrl Pts',(76.3506939226291,12.77022591026,61.03351673584));
#155569=CARTESIAN_POINT('Ctrl Pts',(75.9846773751891,12.02566337689,60.28544751858));
#155570=CARTESIAN_POINT('Ctrl Pts',(75.5969071603691,11.44700487058,59.38566747742));
#155571=CARTESIAN_POINT('Ctrl Pts',(75.4334154616191,11.23893043935,58.98806501362));
#155572=CARTESIAN_POINT('Ctrl Pts',(75.0966676773891,13.30237781364,61.72591085587));
#155573=CARTESIAN_POINT('Ctrl Pts',(74.9621214288391,12.84950608055,61.33981339755));
#155574=CARTESIAN_POINT('Ctrl Pts',(74.7094237279791,12.12535075536,60.57331429327));
#155575=CARTESIAN_POINT('Ctrl Pts',(74.4343965495091,11.55943344353,59.66681793516));
#155576=CARTESIAN_POINT('Ctrl Pts',(74.3170517761591,11.35486892705,59.26810663539));
#155577=CARTESIAN_POINT('Ctrl Pts',(73.6116764726791,13.32524436449,62.01148422652));
#155578=CARTESIAN_POINT('Ctrl Pts',(73.5411274561791,12.87708681798,61.61332948466));
#155579=CARTESIAN_POINT('Ctrl Pts',(73.4020349067191,12.16047212512,60.82794870269));
#155580=CARTESIAN_POINT('Ctrl Pts',(73.2389962138791,11.59914480222,59.90671015597));
#155581=CARTESIAN_POINT('Ctrl Pts',(73.1674788426691,11.39581940583,59.50250721111));
#155582=CARTESIAN_POINT('Ctrl Pts',(72.1188799015491,13.30289486689,62.25146683139));
#155583=CARTESIAN_POINT('Ctrl Pts',(72.1125583805291,12.85011658359,61.84273092877));
#155584=CARTESIAN_POINT('Ctrl Pts',(72.0866318414391,12.12611361488,61.03625300543));
#155585=CARTESIAN_POINT('Ctrl Pts',(72.0338540971691,11.56029225914,60.09066585512));
#155586=CARTESIAN_POINT('Ctrl Pts',(72.0072775324691,11.35575444167,59.67600260266));
#155587=CARTESIAN_POINT('Ctrl Pts',(70.6447970428891,13.23668446295,62.44705203254));
#155588=CARTESIAN_POINT('Ctrl Pts',(70.7027629578791,12.77144316539,62.03027350808));
#155589=CARTESIAN_POINT('Ctrl Pts',(70.7896012143391,12.0271746967,61.20234985571));
#155590=CARTESIAN_POINT('Ctrl Pts',(70.8450707564591,11.4487047659,60.22459753681));
#155591=CARTESIAN_POINT('Ctrl Pts',(70.8622468154291,11.24068339608,59.79523992369));
#155592=CARTESIAN_POINT('Ctrl Pts',(69.1938422725591,13.12817992329,62.60363053547));
#155593=CARTESIAN_POINT('Ctrl Pts',(69.3164050956391,12.64403066823,62.18226630755));
#155594=CARTESIAN_POINT('Ctrl Pts',(69.5165533775491,11.86841436887,61.3342268008));
#155595=CARTESIAN_POINT('Ctrl Pts',(69.6792300687291,11.26989645149,60.31800299092));
#155596=CARTESIAN_POINT('Ctrl Pts',(69.7392629655691,11.05626582625,59.87032822369));
#155597=CARTESIAN_POINT('Ctrl Pts',(67.2987925196791,12.9278854165,62.76551241559));
#155598=CARTESIAN_POINT('Ctrl Pts',(67.5088893277491,12.41134714893,62.34342713161));
#155599=CARTESIAN_POINT('Ctrl Pts',(67.8629193001691,11.58078531893,61.47196925136));
#155600=CARTESIAN_POINT('Ctrl Pts',(68.1685781880491,10.94620890791,60.39748653351));
#155601=CARTESIAN_POINT('Ctrl Pts',(68.2848774985691,10.72234926957,59.92116013881));
#155602=CARTESIAN_POINT('Ctrl Pts',(64.9776135133791,12.57277215386,62.89933853185));
#155603=CARTESIAN_POINT('Ctrl Pts',(65.3046216182191,12.00502373315,62.48986053372));
#155604=CARTESIAN_POINT('Ctrl Pts',(65.8651825116391,11.08386469307,61.60127612814));
#155605=CARTESIAN_POINT('Ctrl Pts',(66.3562770791491,10.3871904121,60.44448875357));
#155606=CARTESIAN_POINT('Ctrl Pts',(66.5432577288191,10.14534757908,59.92560503161));
#155607=CARTESIAN_POINT('Ctrl Pts',(63.2468791157191,12.17590577892,62.96414316285));
#155608=CARTESIAN_POINT('Ctrl Pts',(63.6737672946891,11.57140227548,62.58443568663));
#155609=CARTESIAN_POINT('Ctrl Pts',(64.4148112944791,10.57545021812,61.70779142165));
#155610=CARTESIAN_POINT('Ctrl Pts',(65.0623489581691,9.81902510121501,60.48718610584));
#155611=CARTESIAN_POINT('Ctrl Pts',(65.3061124827291,9.55847754437801,59.93190217482));
#155612=CARTESIAN_POINT('Ctrl Pts',(62.3770790606791,11.93704232306,62.997456388872));
#155613=CARTESIAN_POINT('Ctrl Pts',(62.8591600596191,11.3184788717,62.63962976268));
#155614=CARTESIAN_POINT('Ctrl Pts',(63.7014671428791,10.28887446589,61.77936646535));
#155615=CARTESIAN_POINT('Ctrl Pts',(64.4352534501791,9.50092849403001,60.52921035483));
#155616=CARTESIAN_POINT('Ctrl Pts',(64.7093784324491,9.22979226124701,59.95551485634));
#155617=CARTESIAN_POINT('',(81.8125288217999,9.75922027029902,57.7122994775726));
#155618=CARTESIAN_POINT('Ctrl Pts',(81.8125638933902,9.75941427559586,57.7120937184908));
#155619=CARTESIAN_POINT('Ctrl Pts',(81.6439092695413,9.83352396075257,57.7531647795599));
#155620=CARTESIAN_POINT('Ctrl Pts',(81.4758410035563,9.90338403709679,57.7939788425709));
#155621=CARTESIAN_POINT('Ctrl Pts',(81.3085563965148,9.96953432483138,57.8344710069339));
#155622=CARTESIAN_POINT('Ctrl Pts',(81.1350609420459,10.0381406026996,57.876466541268));
#155623=CARTESIAN_POINT('Ctrl Pts',(80.9624080034726,10.1027570084598,57.9181158985582));
#155624=CARTESIAN_POINT('Ctrl Pts',(80.7907683120586,10.16396002248,57.9593597431247));
#155625=CARTESIAN_POINT('Ctrl Pts',(80.6363540335763,10.2190208255672,57.9964644387118));
#155626=CARTESIAN_POINT('Ctrl Pts',(80.4827588716633,10.2713187822153,58.0332411691658));
#155627=CARTESIAN_POINT('Ctrl Pts',(80.3300792674316,10.3212522825865,58.0696544850922));
#155628=CARTESIAN_POINT('Ctrl Pts',(80.1076282946657,10.3940043426084,58.1227079206851));
#155629=CARTESIAN_POINT('Ctrl Pts',(79.8871203429479,10.4617356301858,58.1749895696072));
#155630=CARTESIAN_POINT('Ctrl Pts',(79.6686891674991,10.5249660905481,58.2264280517326));
#155631=CARTESIAN_POINT('Ctrl Pts',(79.6236763044412,10.5379962088338,58.2370281565348));
#155632=CARTESIAN_POINT('Ctrl Pts',(79.5787514980179,10.5508350969496,58.2475925140022));
#155633=CARTESIAN_POINT('Ctrl Pts',(79.5339157184396,10.5634871501206,58.2581205875384));
#155634=CARTESIAN_POINT('Ctrl Pts',(79.3054702511054,10.6279513844124,58.3117628059123));
#155635=CARTESIAN_POINT('Ctrl Pts',(79.0793396002763,10.6875671033886,58.3644602054702));
#155636=CARTESIAN_POINT('Ctrl Pts',(78.8556312477068,10.7428916622159,58.4161506350891));
#155637=CARTESIAN_POINT('Ctrl Pts',(78.6974177155852,10.782018917701,58.452707720924));
#155638=CARTESIAN_POINT('Ctrl Pts',(78.5404149375569,10.8189990491118,58.4887615270575));
#155639=CARTESIAN_POINT('Ctrl Pts',(78.384652376787,10.8540168851848,58.5242945022815));
#155640=CARTESIAN_POINT('Ctrl Pts',(78.1161060568885,10.9143902570768,58.5855560126488));
#155641=CARTESIAN_POINT('Ctrl Pts',(77.8512481119559,10.9689305735653,58.6452681998748));
#155642=CARTESIAN_POINT('Ctrl Pts',(77.5902789029177,11.0181836520086,58.7033465791699));
#155643=CARTESIAN_POINT('Ctrl Pts',(77.3203166773425,11.0691339948555,58.7634263433308));
#155644=CARTESIAN_POINT('Ctrl Pts',(77.0545153684036,11.1144268661446,58.8217580301841));
#155645=CARTESIAN_POINT('Ctrl Pts',(76.7930581821983,11.1546321196916,58.8782711045304));
#155646=CARTESIAN_POINT('Ctrl Pts',(76.5829449901012,11.1869420144183,58.9236863505921));
#155647=CARTESIAN_POINT('Ctrl Pts',(76.3756364373161,11.21596562502,58.9679276240705));
#155648=CARTESIAN_POINT('Ctrl Pts',(76.1712133147876,11.2419809454017,59.0109667460181));
#155649=CARTESIAN_POINT('Ctrl Pts',(75.8815787661272,11.2788404527011,59.0719462306568));
#155650=CARTESIAN_POINT('Ctrl Pts',(75.59773925635,11.3096601531848,59.1305115677576));
#155651=CARTESIAN_POINT('Ctrl Pts',(75.3199685850635,11.3350228954986,59.1865883387752));
#155652=CARTESIAN_POINT('Ctrl Pts',(75.0421979137771,11.3603856378124,59.2426651097928));
#155653=CARTESIAN_POINT('Ctrl Pts',(74.7704955719418,11.3802917690579,59.2962536749412));
#155654=CARTESIAN_POINT('Ctrl Pts',(74.5050850915348,11.3952985645584,59.3472999044669));
#155655=CARTESIAN_POINT('Ctrl Pts',(74.3558761444026,11.4037351121771,59.3759971667262));
#155656=CARTESIAN_POINT('Ctrl Pts',(74.2086548676872,11.4106227413642,59.4038912591849));
#155657=CARTESIAN_POINT('Ctrl Pts',(74.0634548838674,11.4160563271302,59.4309748116691));
#155658=CARTESIAN_POINT('Ctrl Pts',(73.9908548919575,11.4187731200132,59.4445165879112));
#155659=CARTESIAN_POINT('Ctrl Pts',(73.9187602260095,11.4211263570358,59.4578557522274));
#155660=CARTESIAN_POINT('Ctrl Pts',(73.8471746436691,11.4231275886736,59.4709915147018));
#155661=CARTESIAN_POINT('Ctrl Pts',(73.8113818524989,11.4241282044924,59.477559395939));
#155662=CARTESIAN_POINT('Ctrl Pts',(73.7757163323885,11.4250408160184,59.4840764282361));
#155663=CARTESIAN_POINT('Ctrl Pts',(73.7401785436256,11.4258668478509,59.4905425203682));
#155664=CARTESIAN_POINT('Ctrl Pts',(73.7224096492442,11.4262798637672,59.4937755664343));
#155665=CARTESIAN_POINT('Ctrl Pts',(73.7046726877126,11.4266712345755,59.496995877553));
#155666=CARTESIAN_POINT('Ctrl Pts',(73.6869677151652,11.4270411370982,59.5002034428149));
#155667=CARTESIAN_POINT('Ctrl Pts',(73.6781152288915,11.4272260883595,59.5018072254458));
#155668=CARTESIAN_POINT('Ctrl Pts',(73.6692707398647,11.4274056725378,59.5034078216184));
#155669=CARTESIAN_POINT('Ctrl Pts',(73.6604342550126,11.4275799116558,59.5050052299982));
#155670=CARTESIAN_POINT('Ctrl Pts',(73.6569248990391,11.427649109657,59.5056396309771));
#155671=CARTESIAN_POINT('Ctrl Pts',(73.6536221489607,11.427713488097,59.5062364894203));
#155672=CARTESIAN_POINT('Ctrl Pts',(73.6502813551559,11.4277778705353,59.5068399351009));
#155673=CARTESIAN_POINT('Ctrl Pts',(73.6452101001197,11.4278756017284,59.5077559530074));
#155674=CARTESIAN_POINT('Ctrl Pts',(73.6400511856228,11.4279734504925,59.5086871490538));
#155675=CARTESIAN_POINT('Ctrl Pts',(73.6339488202455,11.4280866170063,59.5097878903822));
#155676=CARTESIAN_POINT('Ctrl Pts',(73.37269285973,11.4329315295009,59.5569130976182));
#155677=CARTESIAN_POINT('Ctrl Pts',(73.1057310345403,11.4334108565222,59.6036608241303));
#155678=CARTESIAN_POINT('Ctrl Pts',(72.8332623814959,11.4291105690191,59.6499966677035));
#155679=CARTESIAN_POINT('Ctrl Pts',(72.5643617687005,11.424866594779,59.6957257326511));
#155680=CARTESIAN_POINT('Ctrl Pts',(72.2900973328511,11.4159671805462,59.7410536382019));
#155681=CARTESIAN_POINT('Ctrl Pts',(72.0107020881292,11.401986105176,59.785945913169));
#155682=CARTESIAN_POINT('Ctrl Pts',(71.7361080183772,11.3882452829611,59.8300667517177));
#155683=CARTESIAN_POINT('Ctrl Pts',(71.4565577601902,11.3695957390455,59.8737667243901));
#155684=CARTESIAN_POINT('Ctrl Pts',(71.1723165576537,11.3456083098175,59.9170122883105));
#155685=CARTESIAN_POINT('Ctrl Pts',(71.071551075223,11.3371045993883,59.9323431413767));
#155686=CARTESIAN_POINT('Ctrl Pts',(70.9701964803605,11.3279298363987,59.9476168852996));
#155687=CARTESIAN_POINT('Ctrl Pts',(70.8682660213638,11.3180642193791,59.9628320401611));
#155688=CARTESIAN_POINT('Ctrl Pts',(70.5736199088582,11.2895460930907,60.0068138516356));
#155689=CARTESIAN_POINT('Ctrl Pts',(70.2741594485926,11.2552578328754,60.0503055208331));
#155690=CARTESIAN_POINT('Ctrl Pts',(69.9700900940868,11.2146418474901,60.0932999798448));
#155691=CARTESIAN_POINT('Ctrl Pts',(69.6814145157921,11.1760820817808,60.1341178068791));
#155692=CARTESIAN_POINT('Ctrl Pts',(69.3885844713174,11.1318185857853,60.1744873762341));
#155693=CARTESIAN_POINT('Ctrl Pts',(69.0918121909477,11.0813480683395,60.2144100787492));
#155694=CARTESIAN_POINT('Ctrl Pts',(68.8359392920326,11.0378330958746,60.2488308730779));
#155695=CARTESIAN_POINT('Ctrl Pts',(68.5771361023818,10.98970350295,60.2829195155496));
#155696=CARTESIAN_POINT('Ctrl Pts',(68.31556650976,10.9366239300422,60.3166828761457));
#155697=CARTESIAN_POINT('Ctrl Pts',(68.070794472209,10.886953037173,60.3482780110574));
#155698=CARTESIAN_POINT('Ctrl Pts',(67.8235995869013,10.83294997116,60.3795883191861));
#155699=CARTESIAN_POINT('Ctrl Pts',(67.5740910332913,10.7740690469024,60.4106341420548));
#155700=CARTESIAN_POINT('Ctrl Pts',(67.368988937872,10.7256674960509,60.4361545630275));
#155701=CARTESIAN_POINT('Ctrl Pts',(67.1623236686854,10.6739690496663,60.4614963651982));
#155702=CARTESIAN_POINT('Ctrl Pts',(66.9541747351594,10.6186522329261,60.4866736678413));
#155703=CARTESIAN_POINT('Ctrl Pts',(66.7160785369694,10.5553767525348,60.5154733351682));
#155704=CARTESIAN_POINT('Ctrl Pts',(66.4760408660556,10.4873682802982,60.5440587719272));
#155705=CARTESIAN_POINT('Ctrl Pts',(66.2342168073654,10.4141216201386,60.5724541257979));
#155706=CARTESIAN_POINT('Ctrl Pts',(66.1921685668518,10.4013855292803,60.5773914950386));
#155707=CARTESIAN_POINT('Ctrl Pts',(66.1500664311417,10.388491012227,60.5823231272746));
#155708=CARTESIAN_POINT('Ctrl Pts',(66.1079113675261,10.3754353472268,60.5872491617598));
#155709=CARTESIAN_POINT('Ctrl Pts',(65.922908563467,10.3181389176469,60.6088676842928));
#155710=CARTESIAN_POINT('Ctrl Pts',(65.7368830571003,10.2577411616242,60.6303785991209));
#155711=CARTESIAN_POINT('Ctrl Pts',(65.5499853458738,10.1936438301779,60.6517844360448));
#155712=CARTESIAN_POINT('Ctrl Pts',(65.3630079214085,10.1295191607516,60.6731994027144));
#155713=CARTESIAN_POINT('Ctrl Pts',(65.1751567898374,10.0616913764202,60.694509302885));
#155714=CARTESIAN_POINT('Ctrl Pts',(64.9866299076625,9.98953569199477,60.715713410289));
#155715=CARTESIAN_POINT('Ctrl Pts',(64.8105237072252,9.9221338271916,60.7355205314035));
#155716=CARTESIAN_POINT('Ctrl Pts',(64.6338277155173,9.85095498689637,60.7552353944469));
#155717=CARTESIAN_POINT('Ctrl Pts',(64.4567500380413,9.77547459984062,60.77485352459));
#155718=CARTESIAN_POINT('Ctrl Pts',(64.4442608385168,9.77015100610725,60.7762371814414));
#155719=CARTESIAN_POINT('Ctrl Pts',(64.4317697614463,9.76480600997884,60.7776203551962));
#155720=CARTESIAN_POINT('Ctrl Pts',(64.4192768896971,9.75943942539138,60.7790030433804));
#155721=CARTESIAN_POINT('',(82.3525679182791,10.16626321309,58.13646557658));
#155722=CARTESIAN_POINT('Origin',(81.9836889860522,12.2828710982502,54.5138910326886));
#155723=CARTESIAN_POINT('Ctrl Pts',(82.3362552021099,12.3439667359304,59.7078933720934));
#155724=CARTESIAN_POINT('Ctrl Pts',(82.3367845506579,12.2021321891277,59.6209578472421));
#155725=CARTESIAN_POINT('Ctrl Pts',(82.3372717809877,12.0612843448791,59.5313433954501));
#155726=CARTESIAN_POINT('Ctrl Pts',(82.337812429342,11.9214102682619,59.439326167785));
#155727=CARTESIAN_POINT('Ctrl Pts',(82.3383767331593,11.7754161581178,59.3432828294067));
#155728=CARTESIAN_POINT('Ctrl Pts',(82.3389990879528,11.6304827840835,59.2446219115626));
#155729=CARTESIAN_POINT('Ctrl Pts',(82.3397609195431,11.4865638643117,59.1436177040391));
#155730=CARTESIAN_POINT('Ctrl Pts',(82.3405408397536,11.3392277920845,59.040215293581));
#155731=CARTESIAN_POINT('Ctrl Pts',(82.3414666358905,11.1929548302125,58.934356881012));
#155732=CARTESIAN_POINT('Ctrl Pts',(82.3426013441794,11.0476647255788,58.8262966308537));
#155733=CARTESIAN_POINT('Ctrl Pts',(82.3437673590602,10.8983660682135,58.7152549993272));
#155734=CARTESIAN_POINT('Ctrl Pts',(82.3451535991453,10.7501054127086,58.6018882076245));
#155735=CARTESIAN_POINT('Ctrl Pts',(82.3468082689014,10.6027633116616,58.4864321494171));
#155736=CARTESIAN_POINT('Ctrl Pts',(82.3478307597478,10.511714358207,58.4150869385433));
#155737=CARTESIAN_POINT('Ctrl Pts',(82.3489553753137,10.4210155333556,58.3429431568581));
#155738=CARTESIAN_POINT('Ctrl Pts',(82.3501908087954,10.3306320160889,58.2700496333164));
#155739=CARTESIAN_POINT('Ctrl Pts',(82.3509411230878,10.2757395060469,58.2257792995873));
#155740=CARTESIAN_POINT('Ctrl Pts',(82.3517322491779,10.2209631609564,58.1812322687692));
#155741=CARTESIAN_POINT('Ctrl Pts',(82.3525703921353,10.1662894370835,58.1364336318516));
#155742=CARTESIAN_POINT('Ctrl Pts',(82.0452144420091,12.45482652165,59.86552067071));
#155743=CARTESIAN_POINT('Ctrl Pts',(82.0448125353891,12.19986367057,59.70650410144));
#155744=CARTESIAN_POINT('Ctrl Pts',(82.0434374412991,11.64996340841,59.33864434196));
#155745=CARTESIAN_POINT('Ctrl Pts',(82.044184166809,10.85475243719,58.73582375429));
#155746=CARTESIAN_POINT('Ctrl Pts',(82.050838531519,10.32113499472,58.28707361965));
#155747=CARTESIAN_POINT('Ctrl Pts',(82.0553498143791,10.06894173163,58.06730239371));
#155748=CARTESIAN_POINT('Ctrl Pts',(83.1546990049091,12.5811772786,59.45168536214));
#155749=CARTESIAN_POINT('Ctrl Pts',(83.1625905359392,12.3201036028,59.31301191251));
#155750=CARTESIAN_POINT('Ctrl Pts',(83.1785169251191,11.75185687135,58.99008621727));
#155751=CARTESIAN_POINT('Ctrl Pts',(83.2017396508492,10.91386727203,58.4569794520501));
#155752=CARTESIAN_POINT('Ctrl Pts',(83.2201733202791,10.3389558953,58.05991259092));
#155753=CARTESIAN_POINT('Ctrl Pts',(83.2289698749091,10.06468241539,57.86541024147));
#155754=CARTESIAN_POINT('Ctrl Pts',(84.1164142591292,12.15828071422,60.01243626984));
#155755=CARTESIAN_POINT('Ctrl Pts',(84.1097704475691,11.87300708618,59.8804567433001));
#155756=CARTESIAN_POINT('Ctrl Pts',(84.0914149436691,11.25298218243,59.57233536711));
#155757=CARTESIAN_POINT('Ctrl Pts',(84.0535452913891,10.34012090282,59.0630977159));
#155758=CARTESIAN_POINT('Ctrl Pts',(84.0197048302691,9.71338194995202,58.6835306883801));
#155759=CARTESIAN_POINT('Ctrl Pts',(84.0013859811391,9.41587228684303,58.4983271796601));
#155760=CARTESIAN_POINT('Ctrl Pts',(84.0668739372791,11.5658390057,61.0442972286));
#155761=CARTESIAN_POINT('Ctrl Pts',(84.0359167148192,11.26000448237,60.89935221856));
#155762=CARTESIAN_POINT('Ctrl Pts',(83.962476303709,10.60125928587,60.56261320096));
#155763=CARTESIAN_POINT('Ctrl Pts',(83.834798336399,9.64865760807302,60.00996881749));
#155764=CARTESIAN_POINT('Ctrl Pts',(83.7315651934492,9.00609137754301,59.598005772));
#155765=CARTESIAN_POINT('Ctrl Pts',(83.6790761186291,8.70505241902901,59.39778200523));
#155766=CARTESIAN_POINT('Ctrl Pts',(82.3525733640486,10.1663210820827,58.136395020841));
#155767=CARTESIAN_POINT('Ctrl Pts',(82.3945030555095,10.1610405216675,58.1352972562638));
#155768=CARTESIAN_POINT('Ctrl Pts',(82.4370648290974,10.1545449462471,58.1355697300673));
#155769=CARTESIAN_POINT('Ctrl Pts',(82.4800399725421,10.146745735236,58.1373517678428));
#155770=CARTESIAN_POINT('Ctrl Pts',(82.5223769279141,10.1390623438138,58.1391073420591));
#155771=CARTESIAN_POINT('Ctrl Pts',(82.5651147310881,10.1301133570611,58.1423285092547));
#155772=CARTESIAN_POINT('Ctrl Pts',(82.6080053073103,10.1198371253139,58.1471276135581));
#155773=CARTESIAN_POINT('Ctrl Pts',(82.6500717961769,10.1097583381663,58.1518345092339));
#155774=CARTESIAN_POINT('Ctrl Pts',(82.6922847229005,10.0984025311023,58.1580597278645));
#155775=CARTESIAN_POINT('Ctrl Pts',(82.7343786504432,10.085738880054,58.1658819132491));
#155776=CARTESIAN_POINT('Ctrl Pts',(82.7638801760669,10.0768635612682,58.1713640912264));
#155777=CARTESIAN_POINT('Ctrl Pts',(82.7933225677532,10.0673464110393,58.1776301200527));
#155778=CARTESIAN_POINT('Ctrl Pts',(82.8226073273802,10.0571861011029,58.1846971565664));
#155779=CARTESIAN_POINT('Ctrl Pts',(82.8634086546753,10.0430301327284,58.1945433862596));
#155780=CARTESIAN_POINT('Ctrl Pts',(82.9039035584235,10.0276244794202,58.20594605374));
#155781=CARTESIAN_POINT('Ctrl Pts',(82.9438134541426,10.0109956210118,58.2189224676888));
#155782=CARTESIAN_POINT('Ctrl Pts',(82.9833775840859,9.99451082938244,58.2317864583964));
#155783=CARTESIAN_POINT('Ctrl Pts',(83.0223660486267,9.97682391605406,58.2461972008307));
#155784=CARTESIAN_POINT('Ctrl Pts',(83.0605032866594,9.95799336401192,58.2621329958283));
#155785=CARTESIAN_POINT('Ctrl Pts',(83.0983865723687,9.93928820286564,58.2779626758481));
#155786=CARTESIAN_POINT('Ctrl Pts',(83.1354291604188,9.91945468696171,58.2952971765887));
#155787=CARTESIAN_POINT('Ctrl Pts',(83.1713681958996,9.89858191831988,58.3140757469682));
#155788=CARTESIAN_POINT('Ctrl Pts',(83.2071405652668,9.87780594646696,58.3327672323355));
#155789=CARTESIAN_POINT('Ctrl Pts',(83.2418188546337,9.85600056275274,58.3528892855549));
#155790=CARTESIAN_POINT('Ctrl Pts',(83.2751623523267,9.83328278451351,58.3743436893457));
#155791=CARTESIAN_POINT('Ctrl Pts',(83.3084391276747,9.81061046591531,58.3957551615838));
#155792=CARTESIAN_POINT('Ctrl Pts',(83.3403857854015,9.78702973087887,58.4184933773822));
#155793=CARTESIAN_POINT('Ctrl Pts',(83.3707920740686,9.76268184976974,58.4424255889604));
#155794=CARTESIAN_POINT('Ctrl Pts',(83.4011928153647,9.73833841072618,58.4663534343083));
#155795=CARTESIAN_POINT('Ctrl Pts',(83.4300532122819,9.71322852495286,58.4914744303251));
#155796=CARTESIAN_POINT('Ctrl Pts',(83.4572012202667,9.68751271914462,58.517625939285));
#155797=CARTESIAN_POINT('Ctrl Pts',(83.4844664171747,9.66168590675377,58.5438903356131));
#155798=CARTESIAN_POINT('Ctrl Pts',(83.5100040116657,9.63524841096765,58.5711936551417));
#155799=CARTESIAN_POINT('Ctrl Pts',(83.5336852727824,9.60837557320823,58.5993478091022));
#155800=CARTESIAN_POINT('Ctrl Pts',(83.5529022951893,9.5865686296163,58.6221945234237));
#155801=CARTESIAN_POINT('Ctrl Pts',(83.5708977465699,9.56447536479424,58.6456009442468));
#155802=CARTESIAN_POINT('Ctrl Pts',(83.587626795633,9.54219220342424,58.6694590571945));
#155803=CARTESIAN_POINT('Ctrl Pts',(83.6085204360661,9.51436178941662,58.6992564970528));
#155804=CARTESIAN_POINT('Ctrl Pts',(83.6274371272222,9.48623551281498,58.7297583097961));
#155805=CARTESIAN_POINT('Ctrl Pts',(83.6443373015206,9.45799892415152,58.7607462965735));
#155806=CARTESIAN_POINT('Ctrl Pts',(83.6613600541117,9.42955753329083,58.7919590416549));
#155807=CARTESIAN_POINT('Ctrl Pts',(83.6763371024946,9.40100471560584,58.8236644181987));
#155808=CARTESIAN_POINT('Ctrl Pts',(83.6892807472202,9.37252131819323,58.855640635855));
#155809=CARTESIAN_POINT('Ctrl Pts',(83.7024340725541,9.34357650390593,58.8881348523371));
#155810=CARTESIAN_POINT('Ctrl Pts',(83.7134878859966,9.31470383090157,58.9209081565808));
#155811=CARTESIAN_POINT('Ctrl Pts',(83.7225058357604,9.28607678906234,58.9537383854738));
#155812=CARTESIAN_POINT('Ctrl Pts',(83.7298397047622,9.26279577949186,58.9804376468697));
#155813=CARTESIAN_POINT('Ctrl Pts',(83.7358281994042,9.23967697175823,59.0071746660718));
#155814=CARTESIAN_POINT('Ctrl Pts',(83.7405269386778,9.21680318453082,59.0338387719999));
#155815=CARTESIAN_POINT('Ctrl Pts',(82.3362558180773,12.3439659630715,59.7078953260468));
#155816=CARTESIAN_POINT('Ctrl Pts',(82.3898752941292,12.3438789835486,59.6983874893455));
#155817=CARTESIAN_POINT('Ctrl Pts',(82.4439640504566,12.3422887500421,59.6913976293074));
#155818=CARTESIAN_POINT('Ctrl Pts',(82.4981679796218,12.3391948370408,59.6869681324302));
#155819=CARTESIAN_POINT('Ctrl Pts',(82.5544403024617,12.3359828619324,59.6823696082616));
#155820=CARTESIAN_POINT('Ctrl Pts',(82.6108361599016,12.3311506991394,59.6805299615381));
#155821=CARTESIAN_POINT('Ctrl Pts',(82.666987223834,12.3247219659808,59.6814514375097));
#155822=CARTESIAN_POINT('Ctrl Pts',(82.7278805300929,12.3177502936799,59.6824507368037));
#155823=CARTESIAN_POINT('Ctrl Pts',(82.7884855316095,12.3089014340018,59.6866965834116));
#155824=CARTESIAN_POINT('Ctrl Pts',(82.8483737227941,12.2982262594063,59.6941495979233));
#155825=CARTESIAN_POINT('Ctrl Pts',(82.8720255849641,12.2940102736973,59.697093044177));
#155826=CARTESIAN_POINT('Ctrl Pts',(82.895566099159,12.2895096078843,59.7005363430759));
#155827=CARTESIAN_POINT('Ctrl Pts',(82.9189705088584,12.284727957392,59.7044758164529));
#155828=CARTESIAN_POINT('Ctrl Pts',(82.9752836654168,12.2732228677,59.713954550755));
#155829=CARTESIAN_POINT('Ctrl Pts',(83.0307890218355,12.2600930370941,59.7263059761169));
#155830=CARTESIAN_POINT('Ctrl Pts',(83.0850974846959,12.2454304953023,59.7414438060835));
#155831=CARTESIAN_POINT('Ctrl Pts',(83.1407614781443,12.2304019788013,59.7569594738763));
#155832=CARTESIAN_POINT('Ctrl Pts',(83.1951680326611,12.2137634772824,59.7754020615918));
#155833=CARTESIAN_POINT('Ctrl Pts',(83.247930350291,12.1956346723825,59.7966382691706));
#155834=CARTESIAN_POINT('Ctrl Pts',(83.3020507591139,12.1770392357768,59.8184210923603));
#155835=CARTESIAN_POINT('Ctrl Pts',(83.3544412763208,12.1568758451657,59.8431430904216));
#155836=CARTESIAN_POINT('Ctrl Pts',(83.4047175566575,12.1352930555086,59.8706218643776));
#155837=CARTESIAN_POINT('Ctrl Pts',(83.4189110912545,12.1292000018927,59.8783794177649));
#155838=CARTESIAN_POINT('Ctrl Pts',(83.4329363158177,12.1229939375054,59.8863564573931));
#155839=CARTESIAN_POINT('Ctrl Pts',(83.4467850288678,12.1166784743217,59.8945483461906));
#155840=CARTESIAN_POINT('Ctrl Pts',(83.495707214561,12.0943683678522,59.9234871438592));
#155841=CARTESIAN_POINT('Ctrl Pts',(83.5424118751783,12.0706973089624,59.9551025709805));
#155842=CARTESIAN_POINT('Ctrl Pts',(83.5865601147,12.0458386524717,59.9891628621646));
#155843=CARTESIAN_POINT('Ctrl Pts',(83.6299686621919,12.0213964961693,60.0226524822144));
#155844=CARTESIAN_POINT('Ctrl Pts',(83.6709057018179,11.9958061379543,60.0585058438186));
#155845=CARTESIAN_POINT('Ctrl Pts',(83.7090783845161,11.9692506337432,60.0964667024375));
#155846=CARTESIAN_POINT('Ctrl Pts',(83.7459394155726,11.9436076032759,60.1331231879024));
#155847=CARTESIAN_POINT('Ctrl Pts',(83.7802225929091,11.9170646238981,60.1717448460995));
#155848=CARTESIAN_POINT('Ctrl Pts',(83.8116934622586,11.8898040988633,60.2120662059309));
#155849=CARTESIAN_POINT('Ctrl Pts',(83.8211194575485,11.8816391645641,60.2241430552747));
#155850=CARTESIAN_POINT('Ctrl Pts',(83.8302933815406,11.8734099819859,60.2363721393201));
#155851=CARTESIAN_POINT('Ctrl Pts',(83.839209531085,11.8651217677242,60.2487456887995));
#155852=CARTESIAN_POINT('Ctrl Pts',(83.8704799058314,11.8360536633086,60.2921417228425));
#155853=CARTESIAN_POINT('Ctrl Pts',(83.8985682120131,11.8062674363767,60.3373029827861));
#155854=CARTESIAN_POINT('Ctrl Pts',(83.9232890453394,11.7759607036118,60.383921015016));
#155855=CARTESIAN_POINT('Ctrl Pts',(83.9465788636436,11.7474083368621,60.427840468944));
#155856=CARTESIAN_POINT('Ctrl Pts',(83.9668790442298,11.7183939124342,60.4730531648616));
#155857=CARTESIAN_POINT('Ctrl Pts',(83.9840549989384,11.6891014111649,60.5192657007433));
#155858=CARTESIAN_POINT('Ctrl Pts',(84.0002429493343,11.661493888581,60.5628199747976));
#155859=CARTESIAN_POINT('Ctrl Pts',(84.0136550708351,11.6336395430904,60.6072621814493));
#155860=CARTESIAN_POINT('Ctrl Pts',(84.0242076731205,11.6057085713668,60.6523140983562));
#155861=CARTESIAN_POINT('Ctrl Pts',(84.028908909982,11.5932651843904,60.6723849516602));
#155862=CARTESIAN_POINT('Ctrl Pts',(84.0330430642595,11.5808067950523,60.6925763859497));
#155863=CARTESIAN_POINT('Ctrl Pts',(84.0366053096489,11.5683493738914,60.7128617804331));
#155864=CARTESIAN_POINT('Origin',(83.1537660643691,9.5,64.344226319776));
#155865=CARTESIAN_POINT('Origin',(82.8534541851791,13.10501209624,62.64107301909));
#155866=CARTESIAN_POINT('Origin',(82.8534541851791,13.10501209624,62.64107301909));
#155867=CARTESIAN_POINT('Origin',(82.8534541851791,13.10500472878,62.64107301909));
#155868=CARTESIAN_POINT('Origin',(82.8534541851791,13.10501209624,62.64107301909));
#155869=CARTESIAN_POINT('Origin',(65.7305865146691,13.10501209624,65.660296576497));
#155870=CARTESIAN_POINT('Ctrl Pts',(65.9990597670353,14.4574398737497,64.9541505386852));
#155871=CARTESIAN_POINT('Ctrl Pts',(66.0057594746386,14.4759573978632,64.9921646720018));
#155872=CARTESIAN_POINT('Ctrl Pts',(66.0127624332916,14.4932775623909,65.031898108079));
#155873=CARTESIAN_POINT('Ctrl Pts',(66.0200516207235,14.5090651792659,65.0732541692221));
#155874=CARTESIAN_POINT('Ctrl Pts',(66.0272350688423,14.5246237758588,65.114010305952));
#155875=CARTESIAN_POINT('Ctrl Pts',(66.0346965123793,14.5386934153553,65.1563423930204));
#155876=CARTESIAN_POINT('Ctrl Pts',(66.0424108685044,14.5509579784476,65.2001080450176));
#155877=CARTESIAN_POINT('Ctrl Pts',(66.0499758944906,14.5629851310703,65.2430265062983));
#155878=CARTESIAN_POINT('Ctrl Pts',(66.0577841207212,14.5732758890196,65.2873234807316));
#155879=CARTESIAN_POINT('Ctrl Pts',(66.0658034282234,14.5815445851561,65.3328166865689));
#155880=CARTESIAN_POINT('Ctrl Pts',(66.0740601818967,14.5900581116894,65.3796569148937));
#155881=CARTESIAN_POINT('Ctrl Pts',(66.0825407385727,14.5964273023246,65.4277654708633));
#155882=CARTESIAN_POINT('Ctrl Pts',(66.0912007151699,14.6003635820811,65.4768905079869));
#155883=CARTESIAN_POINT('Ctrl Pts',(66.0994190005942,14.6040990968583,65.5235099846134));
#155884=CARTESIAN_POINT('Ctrl Pts',(66.1077987754103,14.6056432230592,65.5710443586578));
#155885=CARTESIAN_POINT('Ctrl Pts',(66.1162944712471,14.6047772907763,65.6192350815045));
#155886=CARTESIAN_POINT('Ctrl Pts',(66.1167510718232,14.6047307513066,65.6218250885193));
#155887=CARTESIAN_POINT('Ctrl Pts',(66.1172080055183,14.6046772580499,65.6244169816493));
#155888=CARTESIAN_POINT('Ctrl Pts',(66.1176652646771,14.6046167797623,65.6270107174613));
#155889=CARTESIAN_POINT('Ctrl Pts',(66.1254536827152,14.6035866633016,65.6711893815637));
#155890=CARTESIAN_POINT('Ctrl Pts',(66.1333324490441,14.6005268101228,65.7158795335643));
#155891=CARTESIAN_POINT('Ctrl Pts',(66.141252533839,14.5953144080035,65.7608030751315));
#155892=CARTESIAN_POINT('Ctrl Pts',(66.1491233289967,14.5901344446036,65.80544704077));
#155893=CARTESIAN_POINT('Ctrl Pts',(66.157034833932,14.5828284021327,65.8503209555839));
#155894=CARTESIAN_POINT('Ctrl Pts',(66.1649357618761,14.5733237250958,65.8951339221507));
#155895=CARTESIAN_POINT('Ctrl Pts',(66.1718110009962,14.5650529336328,65.9341293240847));
#155896=CARTESIAN_POINT('Ctrl Pts',(66.1786781405354,14.5551179750657,65.9730780617015));
#155897=CARTESIAN_POINT('Ctrl Pts',(66.1855023102385,14.543502605895,66.0117823524318));
#155898=CARTESIAN_POINT('Ctrl Pts',(66.1930281223036,14.5306929764088,66.0544661118965));
#155899=CARTESIAN_POINT('Ctrl Pts',(66.200501021359,14.5158392733046,66.0968488687635));
#155900=CARTESIAN_POINT('Ctrl Pts',(66.2078710231428,14.4989722922697,66.1386471816904));
#155901=CARTESIAN_POINT('Ctrl Pts',(66.2152313904599,14.4821273606688,66.1803908535916));
#155902=CARTESIAN_POINT('Ctrl Pts',(66.222489021452,14.4632745153903,66.2215509966373));
#155903=CARTESIAN_POINT('Ctrl Pts',(66.2295958760183,14.4424954357575,66.2618551952368));
#155904=CARTESIAN_POINT('Ctrl Pts',(66.2367027305846,14.4217163561247,66.3021593938362));
#155905=CARTESIAN_POINT('Ctrl Pts',(66.2436587050356,14.3990112627432,66.3416070599376));
#155906=CARTESIAN_POINT('Ctrl Pts',(66.250419100565,14.3745104500712,66.3799447273744));
#155907=CARTESIAN_POINT('Ctrl Pts',(66.257172054931,14.3500366054296,66.4182401965627));
#155908=CARTESIAN_POINT('Ctrl Pts',(66.263729127918,14.3237736558815,66.4554239584199));
#155909=CARTESIAN_POINT('Ctrl Pts',(66.2700506925101,14.2958966587661,66.4912713686282));
#155910=CARTESIAN_POINT('Ctrl Pts',(66.2763868477308,14.267955319524,66.5272015172535));
#155911=CARTESIAN_POINT('Ctrl Pts',(66.2824863241572,14.238392902661,66.5617886732506));
#155912=CARTESIAN_POINT('Ctrl Pts',(66.2883154073236,14.2074242124426,66.5948417246754));
#155913=CARTESIAN_POINT('Ctrl Pts',(66.29414449049,14.1764555222241,66.6278947761001));
#155914=CARTESIAN_POINT('Ctrl Pts',(66.2997031187361,14.1440810828274,66.6594133732594));
#155915=CARTESIAN_POINT('Ctrl Pts',(66.3049648364074,14.1105469821226,66.6892475709747));
#155916=CARTESIAN_POINT('Ctrl Pts',(66.3104409944182,14.0756462052884,66.7202976559509));
#155917=CARTESIAN_POINT('Ctrl Pts',(66.3155951249781,14.0394928311997,66.7495208615145));
#155918=CARTESIAN_POINT('Ctrl Pts',(66.3204087928235,14.0023722391874,66.7768127657061));
#155919=CARTESIAN_POINT('Ctrl Pts',(66.3252538533421,13.965009562626,66.8042826559685));
#155920=CARTESIAN_POINT('Ctrl Pts',(66.3297539717965,13.9266676208806,66.8297958354293));
#155921=CARTESIAN_POINT('Ctrl Pts',(66.3338993005816,13.8876498893092,66.8532965877114));
#155922=CARTESIAN_POINT('Ctrl Pts',(66.3374979748372,13.8537775203377,66.8736982389697));
#155923=CARTESIAN_POINT('Ctrl Pts',(66.3408294076461,13.8193962776764,66.892584051289));
#155924=CARTESIAN_POINT('Ctrl Pts',(66.3438926774567,13.784706883934,66.9099488847624));
#155925=CARTESIAN_POINT('Ctrl Pts',(66.3477567273563,13.7409492142877,66.9318531201676));
#155926=CARTESIAN_POINT('Ctrl Pts',(66.351191691087,13.6967299211875,66.9513236913815));
#155927=CARTESIAN_POINT('Ctrl Pts',(66.3542127318989,13.6523830947144,66.9684405122135));
#155928=CARTESIAN_POINT('Ctrl Pts',(66.3574047870039,13.6055258946137,66.9865262775906));
#155929=CARTESIAN_POINT('Ctrl Pts',(66.3601347360615,13.5585270469719,67.0019843017333));
#155930=CARTESIAN_POINT('Ctrl Pts',(66.36242967166,13.5117483031678,67.0149610607877));
#155931=CARTESIAN_POINT('Ctrl Pts',(66.3646648452017,13.4661877172684,67.027599894102));
#155932=CARTESIAN_POINT('Ctrl Pts',(66.3664874938195,13.4208360801918,67.0378857301113));
#155933=CARTESIAN_POINT('Ctrl Pts',(66.3679299384219,13.375991750249,67.0459952421882));
#155934=CARTESIAN_POINT('Ctrl Pts',(66.3694302332009,13.3293489093591,67.0544299915084));
#155935=CARTESIAN_POINT('Ctrl Pts',(66.3705192816255,13.2832553871896,67.0605107241182));
#155936=CARTESIAN_POINT('Ctrl Pts',(66.371240074511,13.2380019494673,67.0644737956167));
#155937=CARTESIAN_POINT('Ctrl Pts',(66.3719608673965,13.1927485117449,67.0684368671152));
#155938=CARTESIAN_POINT('Ctrl Pts',(66.3723135188225,13.1483352462663,67.0702829244797));
#155939=CARTESIAN_POINT('Ctrl Pts',(66.3723460706922,13.1050047578645,67.0702769694531));
#155940=CARTESIAN_POINT('Ctrl Pts',(62.7470145624991,14.67260333684,68.1339161337049));
#155941=CARTESIAN_POINT('Ctrl Pts',(62.7479150825191,14.67317930239,68.1258209755479));
#155942=CARTESIAN_POINT('Ctrl Pts',(62.7947126550891,14.70165222008,67.716427844428));
#155943=CARTESIAN_POINT('Ctrl Pts',(63.0238969208491,14.69415619541,66.887022874744));
#155944=CARTESIAN_POINT('Ctrl Pts',(63.6771079958591,14.55782369561,65.90062340207));
#155945=CARTESIAN_POINT('Ctrl Pts',(64.4836385318891,14.4067499227,65.232530091334));
#155946=CARTESIAN_POINT('Ctrl Pts',(65.2857897757591,14.31390318541,64.849693565196));
#155947=CARTESIAN_POINT('Ctrl Pts',(65.8917919259791,14.29551720364,64.700120545389));
#155948=CARTESIAN_POINT('Ctrl Pts',(66.2321603836891,14.30404532187,64.660713883658));
#155949=CARTESIAN_POINT('Ctrl Pts',(66.3183572158991,14.30731400122,64.653570092238));
#155950=CARTESIAN_POINT('Ctrl Pts',(64.0360609143291,15.66352209507,68.392852817656));
#155951=CARTESIAN_POINT('Ctrl Pts',(64.0366778488791,15.66420500743,68.3857663296231));
#155952=CARTESIAN_POINT('Ctrl Pts',(64.0691151217491,15.6979376344,68.027533940496));
#155953=CARTESIAN_POINT('Ctrl Pts',(64.2700051029891,15.68776125165,67.319166073428));
#155954=CARTESIAN_POINT('Ctrl Pts',(64.8256825409091,15.53611715734,66.5858944691141));
#155955=CARTESIAN_POINT('Ctrl Pts',(65.4124246610891,15.38571278724,66.2020900065669));
#155956=CARTESIAN_POINT('Ctrl Pts',(65.8737717372191,15.30532374558,66.050089008981));
#155957=CARTESIAN_POINT('Ctrl Pts',(66.1527177053691,15.29122946637,65.995932476021));
#155958=CARTESIAN_POINT('Ctrl Pts',(66.311070658609,15.2979482611,65.9716179772301));
#155959=CARTESIAN_POINT('Ctrl Pts',(66.3518513255091,15.30058162146,65.966078449576));
#155960=CARTESIAN_POINT('Ctrl Pts',(65.4272503875291,14.78981337192,68.501643204624));
#155961=CARTESIAN_POINT('Ctrl Pts',(65.4275400140691,14.79040198758,68.4979963080879));
#155962=CARTESIAN_POINT('Ctrl Pts',(65.4428463358591,14.81949704579,68.313664662612));
#155963=CARTESIAN_POINT('Ctrl Pts',(65.5462723729991,14.8116839771,67.951996102549));
#155964=CARTESIAN_POINT('Ctrl Pts',(65.8296142676391,14.67354035755,67.595807470617));
#155965=CARTESIAN_POINT('Ctrl Pts',(66.1121715994391,14.52254576442,67.430978993379));
#155966=CARTESIAN_POINT('Ctrl Pts',(66.3104326447591,14.43117257572,67.382530829545));
#155967=CARTESIAN_POINT('Ctrl Pts',(66.4130867013791,14.41329423457,67.367143975852));
#155968=CARTESIAN_POINT('Ctrl Pts',(66.4718810278291,14.42160833841,67.356286576696));
#155969=CARTESIAN_POINT('Ctrl Pts',(66.4872299064291,14.42480186956,67.353551898505));
#155970=CARTESIAN_POINT('Ctrl Pts',(65.1192019616691,13.18279848744,68.3194201143539));
#155971=CARTESIAN_POINT('Ctrl Pts',(65.1195443722891,13.18321366293,68.317189977293));
#155972=CARTESIAN_POINT('Ctrl Pts',(65.1371310953791,13.20377882802,68.204323782827));
#155973=CARTESIAN_POINT('Ctrl Pts',(65.2001246699891,13.20031260946,67.9660933031889));
#155974=CARTESIAN_POINT('Ctrl Pts',(65.3889626624191,13.08700045068,67.62267704219));
#155975=CARTESIAN_POINT('Ctrl Pts',(65.6768123602791,12.93492025868,67.327970738096));
#155976=CARTESIAN_POINT('Ctrl Pts',(66.0303623322191,12.8233438978,67.121707376222));
#155977=CARTESIAN_POINT('Ctrl Pts',(66.3357602447291,12.79850552099,67.038242493658));
#155978=CARTESIAN_POINT('Ctrl Pts',(66.5063662620891,12.80975388131,67.021782211843));
#155979=CARTESIAN_POINT('Ctrl Pts',(66.5491980682491,12.81397773617,67.019421110833));
#155980=CARTESIAN_POINT('',(65.1767302637191,13.4988189915,68.186796166063));
#155981=CARTESIAN_POINT('Ctrl Pts',(65.1767302637191,13.4988189915,68.186796166063));
#155982=CARTESIAN_POINT('Ctrl Pts',(65.1929684679118,13.5004670413057,68.1210750045845));
#155983=CARTESIAN_POINT('Ctrl Pts',(65.2147225439506,13.4958913458165,68.0522988453429));
#155984=CARTESIAN_POINT('Ctrl Pts',(65.257832004244,13.4796921846402,67.9464492805757));
#155985=CARTESIAN_POINT('Ctrl Pts',(65.2739476083543,13.4727365279243,67.9107267924136));
#155986=CARTESIAN_POINT('Ctrl Pts',(65.3010060673154,13.4599691383649,67.8568027520571));
#155987=CARTESIAN_POINT('Ctrl Pts',(65.3152562865387,13.4530019674638,67.8297565255));
#155988=CARTESIAN_POINT('Ctrl Pts',(65.3331978895328,13.4438525182,67.7981343309232));
#155989=CARTESIAN_POINT('Ctrl Pts',(65.3425042620514,13.4390225227651,67.7823167711229));
#155990=CARTESIAN_POINT('Ctrl Pts',(65.3465652990597,13.4368978238351,67.7755375856623));
#155991=CARTESIAN_POINT('Ctrl Pts',(65.3492888634492,13.4354692021293,67.7710182074229));
#155992=CARTESIAN_POINT('Ctrl Pts',(65.3513344277367,13.4343926095366,67.7676506489246));
#155993=CARTESIAN_POINT('Ctrl Pts',(65.3745118775289,13.4221739390526,67.7296466516154));
#155994=CARTESIAN_POINT('Ctrl Pts',(65.4075181681876,13.4032698716892,67.678533313575));
#155995=CARTESIAN_POINT('Ctrl Pts',(65.480294248736,13.3643302812121,67.5864913548544));
#155996=CARTESIAN_POINT('Ctrl Pts',(65.5084675799845,13.3495865028143,67.5532979674494));
#155997=CARTESIAN_POINT('Ctrl Pts',(65.5577359449127,13.3248249628597,67.5010467284812));
#155998=CARTESIAN_POINT('Ctrl Pts',(65.5753274880599,13.3161301374819,67.4832239345388));
#155999=CARTESIAN_POINT('Ctrl Pts',(65.603610088605,13.3024264313256,67.456088371081));
#156000=CARTESIAN_POINT('Ctrl Pts',(65.6182251610257,13.2954092112251,67.4424207290154));
#156001=CARTESIAN_POINT('Ctrl Pts',(65.6335767514054,13.2881439405909,67.4286466505924));
#156002=CARTESIAN_POINT('Ctrl Pts',(65.6439776049505,13.2832453044941,67.4194454183518));
#156003=CARTESIAN_POINT('Ctrl Pts',(65.6503894617934,13.2802420914402,67.413865319445));
#156004=CARTESIAN_POINT('Ctrl Pts',(65.7224706740662,13.2466142800192,67.3518778494876));
#156005=CARTESIAN_POINT('Ctrl Pts',(65.7890943453541,13.2197701629759,67.3050628077342));
#156006=CARTESIAN_POINT('Ctrl Pts',(65.8823332755805,13.1867123691467,67.2481596329767));
#156007=CARTESIAN_POINT('Ctrl Pts',(65.9123200873604,13.1768945014928,67.2314072951406));
#156008=CARTESIAN_POINT('Ctrl Pts',(65.9552393776427,13.163969795446,67.2091013539741));
#156009=CARTESIAN_POINT('Ctrl Pts',(65.9692034964649,13.159961909336,67.2021366296084));
#156010=CARTESIAN_POINT('Ctrl Pts',(65.9963899372814,13.152546835594,67.1890679943413));
#156011=CARTESIAN_POINT('Ctrl Pts',(66.0083992161454,13.1494334715406,67.1835042839346));
#156012=CARTESIAN_POINT('Ctrl Pts',(66.1347577280693,13.1188275137962,67.1272322695939));
#156013=CARTESIAN_POINT('Ctrl Pts',(66.2526057819523,13.1051514965565,67.091377765781));
#156014=CARTESIAN_POINT('Ctrl Pts',(66.3723465844291,13.10500475785,67.070279883));
#156015=CARTESIAN_POINT('Ctrl Pts',(63.7242537617786,14.9985402150431,67.8461554916125));
#156016=CARTESIAN_POINT('Ctrl Pts',(63.8955981567397,14.9984281505454,67.8886462156272));
#156017=CARTESIAN_POINT('Ctrl Pts',(64.0802735483646,14.9652747214087,67.9339609061182));
#156018=CARTESIAN_POINT('Ctrl Pts',(64.437577712981,14.8177553154702,68.0205666754888));
#156019=CARTESIAN_POINT('Ctrl Pts',(64.6091063807268,14.7029155066426,68.0615791088498));
#156020=CARTESIAN_POINT('Ctrl Pts',(64.8923141882571,14.410075514194,68.1279665869427));
#156021=CARTESIAN_POINT('Ctrl Pts',(65.0030535557672,14.233058864924,68.1531213529668));
#156022=CARTESIAN_POINT('Ctrl Pts',(65.1448299480447,13.8649342455952,68.1835019232699));
#156023=CARTESIAN_POINT('Ctrl Pts',(65.1763418945754,13.6749482756929,68.188859754286));
#156024=CARTESIAN_POINT('Ctrl Pts',(65.1767302637191,13.4988189915,68.186796166063));
#156025=CARTESIAN_POINT('Ctrl Pts',(63.5004917476991,14.85683282676,69.6013899904));
#156026=CARTESIAN_POINT('Ctrl Pts',(63.4875111720091,14.86142859631,69.562289012902));
#156027=CARTESIAN_POINT('Ctrl Pts',(63.3667162203191,14.90537723046,69.174553074221));
#156028=CARTESIAN_POINT('Ctrl Pts',(63.2779512911692,14.96073620167,68.428956249786));
#156029=CARTESIAN_POINT('Ctrl Pts',(63.4176540715092,14.97167354225,67.736399611083));
#156030=CARTESIAN_POINT('Ctrl Pts',(63.5272467061291,14.97036663875,67.431122989516));
#156031=CARTESIAN_POINT('Ctrl Pts',(64.632194658559,15.09322707693,69.316831401601));
#156032=CARTESIAN_POINT('Ctrl Pts',(64.6223300227891,15.09789088302,69.2901568971791));
#156033=CARTESIAN_POINT('Ctrl Pts',(64.5301655221991,15.14249513828,69.025170748245));
#156034=CARTESIAN_POINT('Ctrl Pts',(64.4569578919491,15.19876233977,68.5077214005671));
#156035=CARTESIAN_POINT('Ctrl Pts',(64.5513828811191,15.20980533273,68.0300280414471));
#156036=CARTESIAN_POINT('Ctrl Pts',(64.6262734480091,15.20849566901,67.822349915333));
#156037=CARTESIAN_POINT('Ctrl Pts',(65.4160083966392,14.25724551843,68.99376188389));
#156038=CARTESIAN_POINT('Ctrl Pts',(65.4103628908792,14.26166872097,68.977921457425));
#156039=CARTESIAN_POINT('Ctrl Pts',(65.3576865499092,14.30395444625,68.8206616065041));
#156040=CARTESIAN_POINT('Ctrl Pts',(65.3168769034091,14.35700979395,68.515233029078));
#156041=CARTESIAN_POINT('Ctrl Pts',(65.3731355800791,14.36767915922,68.232661054128));
#156042=CARTESIAN_POINT('Ctrl Pts',(65.4175819661791,14.36637925674,68.109211017786));
#156043=CARTESIAN_POINT('Ctrl Pts',(65.1483470279191,13.09930223189,68.922182948247));
#156044=CARTESIAN_POINT('Ctrl Pts',(65.1442365642691,13.10339216721,68.9058590563));
#156045=CARTESIAN_POINT('Ctrl Pts',(65.1064597700491,13.14246642663,68.744602114318));
#156046=CARTESIAN_POINT('Ctrl Pts',(65.0858069266991,13.19107293871,68.444748364805));
#156047=CARTESIAN_POINT('Ctrl Pts',(65.1452705423991,13.201224781,68.1624062803621));
#156048=CARTESIAN_POINT('Ctrl Pts',(65.1908586799991,13.1999383991,68.034207063451));
#156049=CARTESIAN_POINT('Ctrl Pts',(65.1554518235812,13.43008177675,68.8079679196157));
#156050=CARTESIAN_POINT('Ctrl Pts',(65.1461881102573,13.4408321527727,68.7554267047025));
#156051=CARTESIAN_POINT('Ctrl Pts',(65.1396268661127,13.4503444917441,68.7018053079805));
#156052=CARTESIAN_POINT('Ctrl Pts',(65.1359957247053,13.4586188334764,68.6473919336038));
#156053=CARTESIAN_POINT('Ctrl Pts',(65.132407771396,13.4667947617781,68.5936257414467));
#156054=CARTESIAN_POINT('Ctrl Pts',(65.1316810761034,13.4737619667128,68.5390864487085));
#156055=CARTESIAN_POINT('Ctrl Pts',(65.1340082530278,13.479520486689,68.4840944107843));
#156056=CARTESIAN_POINT('Ctrl Pts',(65.1362929772285,13.4851739588475,68.4301055461744));
#156057=CARTESIAN_POINT('Ctrl Pts',(65.1415215476525,13.4896624418642,68.375680553896));
#156058=CARTESIAN_POINT('Ctrl Pts',(65.149844087735,13.4929859720836,68.3211605832403));
#156059=CARTESIAN_POINT('Ctrl Pts',(65.1566824461639,13.4957168079419,68.2763633101505));
#156060=CARTESIAN_POINT('Ctrl Pts',(65.1656091946349,13.4976611410268,68.2315026619847));
#156061=CARTESIAN_POINT('Ctrl Pts',(65.1766881467414,13.4988189915,68.1867857312686));
#156062=CARTESIAN_POINT('Origin',(66.6326669169691,-15.387431115,68.54751529846));
#156063=CARTESIAN_POINT('Ctrl Pts',(65.1554729113358,6.92820316501672,68.8079843794271));
#156064=CARTESIAN_POINT('Ctrl Pts',(65.152422383041,6.92817587206967,68.7907276719249));
#156065=CARTESIAN_POINT('Ctrl Pts',(65.1496737586822,6.92912017635131,68.7734202159333));
#156066=CARTESIAN_POINT('Ctrl Pts',(65.1472414203523,6.93105915649169,68.7561084383063));
#156067=CARTESIAN_POINT('Ctrl Pts',(65.1359547055815,6.94005655439528,68.6757770576567));
#156068=CARTESIAN_POINT('Ctrl Pts',(65.1314783371817,6.97047158444587,68.5953526581359));
#156069=CARTESIAN_POINT('Ctrl Pts',(65.132953575682,7.01677570366725,68.5181912974979));
#156070=CARTESIAN_POINT('Ctrl Pts',(65.1334410218994,7.03207544521049,68.4926957499151));
#156071=CARTESIAN_POINT('Ctrl Pts',(65.1345782401243,7.04910988856502,68.467556444226));
#156072=CARTESIAN_POINT('Ctrl Pts',(65.1363109483351,7.06765272021812,68.4427928220101));
#156073=CARTESIAN_POINT('Ctrl Pts',(65.140437744398,7.11181623498945,68.3838132327012));
#156074=CARTESIAN_POINT('Ctrl Pts',(65.1479424717781,7.16453628519599,68.3269644385079));
#156075=CARTESIAN_POINT('Ctrl Pts',(65.1580919268926,7.22275584259291,68.2725087516098));
#156076=CARTESIAN_POINT('Ctrl Pts',(65.174020876945,7.31412788290298,68.1870438762168));
#156077=CARTESIAN_POINT('Ctrl Pts',(65.1964641614873,7.41904598491702,68.1074735321002));
#156078=CARTESIAN_POINT('Ctrl Pts',(65.2237077236684,7.53099885535992,68.0328950571003));
#156079=CARTESIAN_POINT('Ctrl Pts',(65.2538259358793,7.65476462017449,67.9504473095745));
#156080=CARTESIAN_POINT('Ctrl Pts',(65.2898109036682,7.7871280561005,67.874100474813));
#156081=CARTESIAN_POINT('Ctrl Pts',(65.3305707565767,7.9237476928918,67.802837119998));
#156082=CARTESIAN_POINT('Ctrl Pts',(65.3756768202716,8.07493504022901,67.7239749752151));
#156083=CARTESIAN_POINT('Ctrl Pts',(65.4266303535699,8.23133465583079,67.6513382216725));
#156084=CARTESIAN_POINT('Ctrl Pts',(65.4828074420408,8.38987577335587,67.5842795080536));
#156085=CARTESIAN_POINT('Ctrl Pts',(65.5453260651721,8.5663137598585,67.5096508906131));
#156086=CARTESIAN_POINT('Ctrl Pts',(65.6143141261707,8.74540402040174,67.4419307527597));
#156087=CARTESIAN_POINT('Ctrl Pts',(65.6894671929274,8.92454600486117,67.3811644589306));
#156088=CARTESIAN_POINT('Ctrl Pts',(65.740845476658,9.04701615947804,67.3396216713859));
#156089=CARTESIAN_POINT('Ctrl Pts',(65.7951051325205,9.1695104865657,67.3013289431462));
#156090=CARTESIAN_POINT('Ctrl Pts',(65.8521790298628,9.29134610700093,67.2665592059008));
#156091=CARTESIAN_POINT('Ctrl Pts',(65.8881718169189,9.36817989173203,67.2446321988636));
#156092=CARTESIAN_POINT('Ctrl Pts',(65.925284050671,9.44475190004438,67.2241061885447));
#156093=CARTESIAN_POINT('Ctrl Pts',(65.9634978877863,9.52089124203153,67.2050500989013));
#156094=CARTESIAN_POINT('Ctrl Pts',(66.076365450387,9.74577475535619,67.1487664447826));
#156095=CARTESIAN_POINT('Ctrl Pts',(66.1988426116163,9.96688292982532,67.105308130441));
#156096=CARTESIAN_POINT('Ctrl Pts',(66.3301387866529,10.1797418696686,67.0783397637765));
#156097=CARTESIAN_POINT('Ctrl Pts',(66.3439710393069,10.2021668842187,67.0754986051421));
#156098=CARTESIAN_POINT('Ctrl Pts',(66.3579011816857,10.2245003535534,67.0728404391239));
#156099=CARTESIAN_POINT('Ctrl Pts',(66.3719238214764,10.2467337087739,67.0703710012959));
#156100=CARTESIAN_POINT('Ctrl Pts',(65.1354671986791,7.23332581609401,68.864928317118));
#156101=CARTESIAN_POINT('Ctrl Pts',(65.1294770804791,7.22770562585001,68.835657331627));
#156102=CARTESIAN_POINT('Ctrl Pts',(65.1139917221791,7.22505393909401,68.750209130564));
#156103=CARTESIAN_POINT('Ctrl Pts',(65.0969965161891,7.29236458022901,68.598587674286));
#156104=CARTESIAN_POINT('Ctrl Pts',(65.0980562425391,7.48320689487401,68.396834377415));
#156105=CARTESIAN_POINT('Ctrl Pts',(65.1318622502191,7.77841338606401,68.17529511025));
#156106=CARTESIAN_POINT('Ctrl Pts',(65.2058415077292,8.162694802716,67.943290382012));
#156107=CARTESIAN_POINT('Ctrl Pts',(65.3281701944691,8.62651876980101,67.706454494588));
#156108=CARTESIAN_POINT('Ctrl Pts',(65.5107146763692,9.164189148054,67.471184229534));
#156109=CARTESIAN_POINT('Ctrl Pts',(65.7734920352691,9.77549192354001,67.247471406371));
#156110=CARTESIAN_POINT('Ctrl Pts',(66.0530479496791,10.28489480299,67.107115610461));
#156111=CARTESIAN_POINT('Ctrl Pts',(66.2497491622091,10.58326737122,67.053678484145));
#156112=CARTESIAN_POINT('Ctrl Pts',(66.3066656472291,10.6654284307,67.041691621389));
#156113=CARTESIAN_POINT('Ctrl Pts',(65.3531725036091,6.23131392019301,68.896248006187));
#156114=CARTESIAN_POINT('Ctrl Pts',(65.3364173605091,6.22224999202201,68.829802444975));
#156115=CARTESIAN_POINT('Ctrl Pts',(65.2987026046291,6.21733947843101,68.629745175412));
#156116=CARTESIAN_POINT('Ctrl Pts',(65.2998749919591,6.32804692909301,68.289669040376));
#156117=CARTESIAN_POINT('Ctrl Pts',(65.3867416400291,6.59893950037902,67.955205029451));
#156118=CARTESIAN_POINT('Ctrl Pts',(65.5289413574991,6.963178463889,67.689963037335));
#156119=CARTESIAN_POINT('Ctrl Pts',(65.7105984378291,7.39528975498902,67.480895256793));
#156120=CARTESIAN_POINT('Ctrl Pts',(65.9274201532491,7.88574182335501,67.318555940622));
#156121=CARTESIAN_POINT('Ctrl Pts',(66.1805132539291,8.43004104598201,67.201907098975));
#156122=CARTESIAN_POINT('Ctrl Pts',(66.4748259827891,9.02738931413101,67.1383118873611));
#156123=CARTESIAN_POINT('Ctrl Pts',(66.7283333062591,9.50831205247101,67.145082394149));
#156124=CARTESIAN_POINT('Ctrl Pts',(66.8808520355891,9.78320319603901,67.176998428673));
#156125=CARTESIAN_POINT('Ctrl Pts',(66.9231537246591,9.85837183611702,67.188078156507));
#156126=CARTESIAN_POINT('Ctrl Pts',(64.7343817516392,5.43913593756802,69.101455710263));
#156127=CARTESIAN_POINT('Ctrl Pts',(64.7040334588792,5.42734943357101,68.98332816162));
#156128=CARTESIAN_POINT('Ctrl Pts',(64.6365286033291,5.42065311994001,68.626582976925));
#156129=CARTESIAN_POINT('Ctrl Pts',(64.6456736852991,5.56566954154801,68.022721853925));
#156130=CARTESIAN_POINT('Ctrl Pts',(64.8151082091391,5.89984883734601,67.450048284848));
#156131=CARTESIAN_POINT('Ctrl Pts',(65.0795393031391,6.31866400387401,67.020711466353));
#156132=CARTESIAN_POINT('Ctrl Pts',(65.4049285112791,6.78858899120402,66.7054392210471));
#156133=CARTESIAN_POINT('Ctrl Pts',(65.7795850174191,7.30009290101001,66.483489253098));
#156134=CARTESIAN_POINT('Ctrl Pts',(66.2008884135791,7.84963280449501,66.350252627375));
#156135=CARTESIAN_POINT('Ctrl Pts',(66.6704436566291,8.43594881492901,66.316098737405));
#156136=CARTESIAN_POINT('Ctrl Pts',(67.0534415061091,8.89435551247002,66.38593021354));
#156137=CARTESIAN_POINT('Ctrl Pts',(67.2723705023591,9.15068253749601,66.469885980898));
#156138=CARTESIAN_POINT('Ctrl Pts',(67.3321395401491,9.22032305887401,66.49638480121));
#156139=CARTESIAN_POINT('Ctrl Pts',(63.7340191659991,5.43918737470401,69.329686286193));
#156140=CARTESIAN_POINT('Ctrl Pts',(63.6972430465491,5.42740104748701,69.183365038754));
#156141=CARTESIAN_POINT('Ctrl Pts',(63.6142885536191,5.42070484981102,68.743047328557));
#156142=CARTESIAN_POINT('Ctrl Pts',(63.6153500447691,5.56571904369301,67.994001054187));
#156143=CARTESIAN_POINT('Ctrl Pts',(63.8034109289491,5.89989423020201,67.252746616459));
#156144=CARTESIAN_POINT('Ctrl Pts',(64.1140486792091,6.31870585302701,66.659562539042));
#156145=CARTESIAN_POINT('Ctrl Pts',(64.5135549538991,6.78862838506501,66.187024096085));
#156146=CARTESIAN_POINT('Ctrl Pts',(64.9933506135291,7.30013092794801,65.815180970113));
#156147=CARTESIAN_POINT('Ctrl Pts',(65.5568606915191,7.84967049114902,65.542342403844));
#156148=CARTESIAN_POINT('Ctrl Pts',(66.2165303374391,8.435987217921,65.385308796823));
#156149=CARTESIAN_POINT('Ctrl Pts',(66.7893586421791,8.89439537745801,65.387774578562));
#156150=CARTESIAN_POINT('Ctrl Pts',(67.1364669795991,9.150723607877,65.452197942192));
#156151=CARTESIAN_POINT('Ctrl Pts',(67.2329438191191,9.22036448820301,65.475132507639));
#156152=CARTESIAN_POINT('Ctrl Pts',(66.371936433707,10.2467129746685,67.0703492004296));
#156153=CARTESIAN_POINT('Ctrl Pts',(66.8232876390597,9.66024242196376,66.9907827752467));
#156154=CARTESIAN_POINT('Ctrl Pts',(67.0909397415809,9.20580207491112,66.4655776203965));
#156155=CARTESIAN_POINT('Ctrl Pts',(67.0545035358591,9.08849833454501,65.731481575833));
#156156=CARTESIAN_POINT('Ctrl Pts',(65.1202128309596,6.80865448650755,68.513745885506));
#156157=CARTESIAN_POINT('Ctrl Pts',(65.1130248862952,6.77887522935553,68.4292572074512));
#156158=CARTESIAN_POINT('Ctrl Pts',(65.1062988116738,6.74993122712072,68.33221079615));
#156159=CARTESIAN_POINT('Ctrl Pts',(65.0995328946409,6.72719707959995,68.2212988484916));
#156160=CARTESIAN_POINT('Ctrl Pts',(65.1274618024618,6.68337652285334,68.6491891342771));
#156161=CARTESIAN_POINT('Ctrl Pts',(65.126315892328,6.67628535290415,68.642690355055));
#156162=CARTESIAN_POINT('Ctrl Pts',(65.1220591440704,6.65062009337786,68.6185491365772));
#156163=CARTESIAN_POINT('Ctrl Pts',(65.1140119965792,6.60634594809702,68.5729114948953));
#156164=CARTESIAN_POINT('Ctrl Pts',(65.1025845774915,6.55116777440088,68.5081033809057));
#156165=CARTESIAN_POINT('Ctrl Pts',(65.0894146357107,6.4956542873541,68.4334129294739));
#156166=CARTESIAN_POINT('Ctrl Pts',(65.0743938717168,6.44075786056385,68.3482259437502));
#156167=CARTESIAN_POINT('Ctrl Pts',(65.0573886353781,6.38738124122978,68.2517844560535));
#156168=CARTESIAN_POINT('Ctrl Pts',(65.0382437566995,6.33645081793974,68.1432084536717));
#156169=CARTESIAN_POINT('Ctrl Pts',(65.0167679466859,6.28886673138934,68.0214130827762));
#156170=CARTESIAN_POINT('Ctrl Pts',(64.9927178237894,6.24591318747231,67.8850180580309));
#156171=CARTESIAN_POINT('Ctrl Pts',(64.9659407425506,6.20937832800507,67.7331576840355));
#156172=CARTESIAN_POINT('Ctrl Pts',(64.9362912819956,6.18123465571579,67.5650072374273));
#156173=CARTESIAN_POINT('Ctrl Pts',(64.9046232778813,6.16401422306796,67.3854090614244));
#156174=CARTESIAN_POINT('Ctrl Pts',(64.8827743055232,6.16046240900282,67.2614973817191));
#156175=CARTESIAN_POINT('Ctrl Pts',(64.8718037269095,6.16067826099719,67.1992801386775));
#156176=CARTESIAN_POINT('Ctrl Pts',(65.1139076006613,6.75398795634377,68.5745299318079));
#156177=CARTESIAN_POINT('Ctrl Pts',(65.1128680951615,6.74755527937897,68.5686346008803));
#156178=CARTESIAN_POINT('Ctrl Pts',(65.1089989141607,6.72422559008582,68.5466913710057));
#156179=CARTESIAN_POINT('Ctrl Pts',(65.1016377391522,6.68371527314676,68.5049440839871));
#156180=CARTESIAN_POINT('Ctrl Pts',(65.0911145206383,6.63289255144576,68.4452639420414));
#156181=CARTESIAN_POINT('Ctrl Pts',(65.078906346136,6.58142138067483,68.3760279451778));
#156182=CARTESIAN_POINT('Ctrl Pts',(65.0648965972843,6.53020896520135,68.2965747108642));
#156183=CARTESIAN_POINT('Ctrl Pts',(65.0489433373531,6.4801225724662,68.2060992779522));
#156184=CARTESIAN_POINT('Ctrl Pts',(65.030876566461,6.43204858405808,68.103637528625));
#156185=CARTESIAN_POINT('Ctrl Pts',(65.0105047539925,6.38690098578241,67.9881032389442));
#156186=CARTESIAN_POINT('Ctrl Pts',(64.9876158486021,6.34601386199286,67.8582938059316));
#156187=CARTESIAN_POINT('Ctrl Pts',(64.9620427523565,6.31111285615102,67.713261570135));
#156188=CARTESIAN_POINT('Ctrl Pts',(64.9336316898486,6.28413266453705,67.5521344278609));
#156189=CARTESIAN_POINT('Ctrl Pts',(64.9031552466415,6.26755013237094,67.3792939295652));
#156190=CARTESIAN_POINT('Ctrl Pts',(64.8820795473119,6.26412038407241,67.2597676991259));
#156191=CARTESIAN_POINT('Ctrl Pts',(64.8714878273221,6.26432875241371,67.1996990701106));
#156192=CARTESIAN_POINT('Ctrl Pts',(65.1161939756686,6.82410170851579,68.4976206638588));
#156193=CARTESIAN_POINT('Ctrl Pts',(65.1152601248451,6.81832288336551,68.4923245280203));
#156194=CARTESIAN_POINT('Ctrl Pts',(65.1117757794614,6.79731230281174,68.4725637949535));
#156195=CARTESIAN_POINT('Ctrl Pts',(65.1050957420854,6.7605392861161,68.4346794427211));
#156196=CARTESIAN_POINT('Ctrl Pts',(65.0954703511864,6.71404131844838,68.3800911300056));
#156197=CARTESIAN_POINT('Ctrl Pts',(65.0842171652642,6.66658397302499,68.3162711437924));
#156198=CARTESIAN_POINT('Ctrl Pts',(65.0712113057501,6.61902960333383,68.2425112484398));
#156199=CARTESIAN_POINT('Ctrl Pts',(65.056302607718,6.57221024712437,68.1579598205501));
#156200=CARTESIAN_POINT('Ctrl Pts',(65.0393063459266,6.52697256096236,68.0615692299884));
#156201=CARTESIAN_POINT('Ctrl Pts',(65.0200307498421,6.48424427818018,67.9522518923636));
#156202=CARTESIAN_POINT('Ctrl Pts',(64.9982948775005,6.44540901003979,67.8289816347201));
#156203=CARTESIAN_POINT('Ctrl Pts',(64.9739172803584,6.41213034214683,67.69072941125));
#156204=CARTESIAN_POINT('Ctrl Pts',(64.9467358874593,6.38630543079974,67.536576071874));
#156205=CARTESIAN_POINT('Ctrl Pts',(64.9174426068361,6.37035630308492,67.3704456220308));
#156206=CARTESIAN_POINT('Ctrl Pts',(64.8971347303756,6.36704776021286,67.2552739314699));
#156207=CARTESIAN_POINT('Ctrl Pts',(64.8869191987505,6.36724869764713,67.1973387726862));
#156208=CARTESIAN_POINT('Ctrl Pts',(65.1346705530482,6.8919798904543,68.4202960166216));
#156209=CARTESIAN_POINT('Ctrl Pts',(65.1338389881117,6.88683406911642,68.4155799705943));
#156210=CARTESIAN_POINT('Ctrl Pts',(65.1307272078985,6.86806865274327,68.3979321456351));
#156211=CARTESIAN_POINT('Ctrl Pts',(65.1247065901473,6.83491377283282,68.3637875588852));
#156212=CARTESIAN_POINT('Ctrl Pts',(65.1159503997161,6.79260266483268,68.3141287229154));
#156213=CARTESIAN_POINT('Ctrl Pts',(65.1056217526552,6.74903116432229,68.2555520583749));
#156214=CARTESIAN_POINT('Ctrl Pts',(65.0935877735642,6.70501820397611,68.187303970419));
#156215=CARTESIAN_POINT('Ctrl Pts',(65.0796903316755,6.66136171514741,68.1084876612219));
#156216=CARTESIAN_POINT('Ctrl Pts',(65.0637304459047,6.61886989600768,68.0179746511137));
#156217=CARTESIAN_POINT('Ctrl Pts',(65.0455161134506,6.57848378907752,67.9146760386274));
#156218=CARTESIAN_POINT('Ctrl Pts',(65.0248965098102,6.54163495336659,67.7977364553764));
#156219=CARTESIAN_POINT('Ctrl Pts',(65.0016762933978,6.5099268953333,67.6660480641928));
#156220=CARTESIAN_POINT('Ctrl Pts',(64.9756853622109,6.48522042825308,67.5186461686814));
#156221=CARTESIAN_POINT('Ctrl Pts',(64.9475375191463,6.46988450894962,67.3590118180421));
#156222=CARTESIAN_POINT('Ctrl Pts',(64.9279729835967,6.46669330688071,67.248055823275));
#156223=CARTESIAN_POINT('Ctrl Pts',(64.9181216456063,6.4668870503417,67.1921861092301));
#156224=CARTESIAN_POINT('Origin',(73.9901844080691,1.4210854715202E-14,
64.203906618088));
#156225=CARTESIAN_POINT('Origin',(82.8534541851791,15.33010667085,62.64107301909));
#156226=CARTESIAN_POINT('Ctrl Pts',(82.0542997835692,10.29865851118,58.26471983769));
#156227=CARTESIAN_POINT('Ctrl Pts',(82.0527395465391,10.17603905197,58.16140352547));
#156228=CARTESIAN_POINT('Ctrl Pts',(82.0492308291891,9.89812303372602,57.92115839559));
#156229=CARTESIAN_POINT('Ctrl Pts',(82.0458365166991,9.61603810345401,57.66377166706));
#156230=CARTESIAN_POINT('Ctrl Pts',(82.043988738869,9.45484011582801,57.51238781076));
#156231=CARTESIAN_POINT('Ctrl Pts',(82.0438796852591,9.44529764517503,57.50341116586));
#156232=CARTESIAN_POINT('Ctrl Pts',(83.0679041040991,10.31054165842,58.07143591329));
#156233=CARTESIAN_POINT('Ctrl Pts',(83.0680728911292,10.18085680913,57.97675228206));
#156234=CARTESIAN_POINT('Ctrl Pts',(83.0680970000191,9.88587567699001,57.7562458923));
#156235=CARTESIAN_POINT('Ctrl Pts',(83.0672361907791,9.58406728388101,57.51926185832));
#156236=CARTESIAN_POINT('Ctrl Pts',(83.066405906709,9.41081340331201,57.37964988205));
#156237=CARTESIAN_POINT('Ctrl Pts',(83.0663555479991,9.40055449126001,57.37137050065));
#156238=CARTESIAN_POINT('Ctrl Pts',(83.8273697495491,9.80641462172301,58.55513154362));
#156239=CARTESIAN_POINT('Ctrl Pts',(83.8191676863491,9.66631332335401,58.46273485692));
#156240=CARTESIAN_POINT('Ctrl Pts',(83.7993625846091,9.34764672538402,58.24737311026));
#156241=CARTESIAN_POINT('Ctrl Pts',(83.7762983997391,9.02178381289601,58.01556464493));
#156242=CARTESIAN_POINT('Ctrl Pts',(83.7620427416892,8.83486184555501,57.87891342746));
#156243=CARTESIAN_POINT('Ctrl Pts',(83.7611950253791,8.82379411820401,57.87080933309));
#156244=CARTESIAN_POINT('Ctrl Pts',(83.769884078649,9.15986779421601,59.35735731505));
#156245=CARTESIAN_POINT('Ctrl Pts',(83.749414626619,9.013718243092,59.25920706419));
#156246=CARTESIAN_POINT('Ctrl Pts',(83.701112991309,8.68229827316202,59.03058335385));
#156247=CARTESIAN_POINT('Ctrl Pts',(83.6475626740491,8.345875722854,58.7848879037501));
#156248=CARTESIAN_POINT('Ctrl Pts',(83.615387835479,8.15380240182902,58.64019221211));
#156249=CARTESIAN_POINT('Ctrl Pts',(83.6134776020891,8.14243286917001,58.63161152939));
#156250=CARTESIAN_POINT('',(82.344504931983,9.5242671557599,57.5877992215605));
#156251=CARTESIAN_POINT('Origin',(82.1588614728291,8.53712723764301,58.70184199751));
#156252=CARTESIAN_POINT('Ctrl Pts',(82.3525639851769,10.1662213565488,58.1365166381844));
#156253=CARTESIAN_POINT('Ctrl Pts',(82.3515337760017,10.0806860329839,58.0663217283825));
#156254=CARTESIAN_POINT('Ctrl Pts',(82.3504894170264,9.99561838305282,57.9953267882541));
#156255=CARTESIAN_POINT('Ctrl Pts',(82.3494344128164,9.91100184699888,57.9235752783107));
#156256=CARTESIAN_POINT('Ctrl Pts',(82.3478142322361,9.78105538119467,57.8133857625485));
#156257=CARTESIAN_POINT('Ctrl Pts',(82.3461689438681,9.65217281892513,57.7014119551773));
#156258=CARTESIAN_POINT('Ctrl Pts',(82.3445049357179,9.52426717547808,57.5877992022325));
#156259=CARTESIAN_POINT('Ctrl Pts',(86.9329409753791,9.92711979712301,57.78576952332));
#156260=CARTESIAN_POINT('Ctrl Pts',(84.0933088102591,7.69990047565403,57.4110459375501));
#156261=CARTESIAN_POINT('Ctrl Pts',(81.3965784204092,6.58687843438301,55.21311191528));
#156262=CARTESIAN_POINT('Ctrl Pts',(79.8215157765191,7.02960519183701,51.92060906182));
#156263=CARTESIAN_POINT('Ctrl Pts',(86.0676469660691,10.68513943961,58.23629022148));
#156264=CARTESIAN_POINT('Ctrl Pts',(83.4591950453992,8.38530844920902,57.7160304338599));
#156265=CARTESIAN_POINT('Ctrl Pts',(80.9461889541891,7.20824339431001,55.52843468871));
#156266=CARTESIAN_POINT('Ctrl Pts',(79.3859501752991,7.59165105783701,52.36111905021));
#156267=CARTESIAN_POINT('Ctrl Pts',(85.1070801027791,11.36198787766,58.71079233602));
#156268=CARTESIAN_POINT('Ctrl Pts',(82.7291098543491,9.03120774616101,58.05826770049));
#156269=CARTESIAN_POINT('Ctrl Pts',(80.4097867402391,7.80241333656101,55.88012561213));
#156270=CARTESIAN_POINT('Ctrl Pts',(78.8911987758591,8.10248660419701,52.82351298253));
#156271=CARTESIAN_POINT('Ctrl Pts',(84.0404926560891,11.95793977738,59.19105334214));
#156272=CARTESIAN_POINT('Ctrl Pts',(81.888874467589,9.61731046456401,58.42277593509));
#156273=CARTESIAN_POINT('Ctrl Pts',(79.7722632969191,8.34598753659601,56.2503969924101));
#156274=CARTESIAN_POINT('Ctrl Pts',(78.3268882647691,8.55715030996601,53.28427687186));
#156275=CARTESIAN_POINT('Origin',(70.1855769158814,-19.4157022285867,61.5812032484374));
#156276=CARTESIAN_POINT('Ctrl Pts',(82.6104235887092,9.668870107941,57.81364808779));
#156277=CARTESIAN_POINT('Ctrl Pts',(82.5689416191891,9.68513702138402,57.82096247823));
#156278=CARTESIAN_POINT('Ctrl Pts',(82.4031385785191,9.74979208676402,57.8501980277801));
#156279=CARTESIAN_POINT('Ctrl Pts',(82.1234598163291,9.85639317719102,57.89951293949));
#156280=CARTESIAN_POINT('Ctrl Pts',(81.8843680682591,9.94447157893201,57.94167126554));
#156281=CARTESIAN_POINT('Ctrl Pts',(81.7702786897492,9.98579912464201,57.9617883011801));
#156282=CARTESIAN_POINT('Ctrl Pts',(82.3934669688891,9.34863157848701,57.29542335185));
#156283=CARTESIAN_POINT('Ctrl Pts',(82.3523805149492,9.36474339264802,57.30266800222));
#156284=CARTESIAN_POINT('Ctrl Pts',(82.1881643280692,9.42877964864201,57.33162374664));
#156285=CARTESIAN_POINT('Ctrl Pts',(81.9112013668991,9.53434541009101,57.38045978935));
#156286=CARTESIAN_POINT('Ctrl Pts',(81.6744751240489,9.62155226794001,57.42220101301));
#156287=CARTESIAN_POINT('Ctrl Pts',(81.5615236720891,9.66246761273101,57.4421174015));
#156288=CARTESIAN_POINT('Ctrl Pts',(82.1383565513191,8.79415897984801,57.08174467046));
#156289=CARTESIAN_POINT('Ctrl Pts',(82.0979549073891,8.81000224948801,57.08886857035));
#156290=CARTESIAN_POINT('Ctrl Pts',(81.9364862566791,8.87296707647901,57.11733985001));
#156291=CARTESIAN_POINT('Ctrl Pts',(81.6642255318591,8.97674023180402,57.16534676158));
#156292=CARTESIAN_POINT('Ctrl Pts',(81.4315950105091,9.06243806696601,57.20636579903));
#156293=CARTESIAN_POINT('Ctrl Pts',(81.3206138058091,9.10263971214401,57.22593477977));
#156294=CARTESIAN_POINT('Ctrl Pts',(81.9360321987691,8.20310657683102,57.24878262946));
#156295=CARTESIAN_POINT('Ctrl Pts',(81.8963605433192,8.21866358546402,57.25577781268));
#156296=CARTESIAN_POINT('Ctrl Pts',(81.7378206899191,8.28048629887201,57.28373266636));
#156297=CARTESIAN_POINT('Ctrl Pts',(81.4705724185491,8.38234858581402,57.33085574715));
#156298=CARTESIAN_POINT('Ctrl Pts',(81.2423078226591,8.46643784466801,57.37110495414));
#156299=CARTESIAN_POINT('Ctrl Pts',(81.1334268468591,8.50587870586502,57.39030360786));
#156300=CARTESIAN_POINT('Origin',(81.6278425866092,8.7374636884277,58.7954749599595));
#156301=CARTESIAN_POINT('Origin',(82.1588614744491,8.53712721516301,58.70184200705));
#156302=CARTESIAN_POINT('Origin',(82.1588614745091,8.53712721530601,58.70184200704));
#156303=CARTESIAN_POINT('Ctrl Pts',(82.2180760363191,10.03116305045,58.28208546212));
#156304=CARTESIAN_POINT('Ctrl Pts',(81.6448173157991,10.2499782811,58.38316644148));
#156305=CARTESIAN_POINT('Ctrl Pts',(80.4077005984991,10.6384119469,58.60130349702));
#156306=CARTESIAN_POINT('Ctrl Pts',(78.4208211301491,11.08801271783,58.95164395471));
#156307=CARTESIAN_POINT('Ctrl Pts',(76.1569665443491,11.42116381224,59.35082259858));
#156308=CARTESIAN_POINT('Ctrl Pts',(73.6216993183591,11.58264138134,59.79785861383));
#156309=CARTESIAN_POINT('Ctrl Pts',(70.9781759552091,11.49327700734,60.26398310689));
#156310=CARTESIAN_POINT('Ctrl Pts',(68.4543146920692,11.16992459859,60.70900794314));
#156311=CARTESIAN_POINT('Ctrl Pts',(66.2334199597191,10.69349906036,61.10061160577));
#156312=CARTESIAN_POINT('Ctrl Pts',(64.8647467245591,10.27221430314,61.3419456249));
#156313=CARTESIAN_POINT('Ctrl Pts',(64.2333895001991,10.03126768975,61.45327093802));
#156314=CARTESIAN_POINT('Ctrl Pts',(82.0018799307291,9.82226387024801,57.50799734594));
#156315=CARTESIAN_POINT('Ctrl Pts',(81.436977430279,10.03788714144,57.60760489824));
#156316=CARTESIAN_POINT('Ctrl Pts',(80.2133909429991,10.4222367679,57.8233562091799));
#156317=CARTESIAN_POINT('Ctrl Pts',(78.2425568897692,10.86825463521,58.1708674272599));
#156318=CARTESIAN_POINT('Ctrl Pts',(75.9954429246891,11.19894300459,58.56709424803));
#156319=CARTESIAN_POINT('Ctrl Pts',(73.4796033119692,11.3591631631,59.01070465089));
#156320=CARTESIAN_POINT('Ctrl Pts',(70.8569091407191,11.27051736571,59.47315639543));
#156321=CARTESIAN_POINT('Ctrl Pts',(68.3515547785591,10.94955172405,59.9149179657099));
#156322=CARTESIAN_POINT('Ctrl Pts',(66.1481091383991,10.47682179375,60.3034448826));
#156323=CARTESIAN_POINT('Ctrl Pts',(64.7939462302891,10.05980065435,60.54222033957));
#156324=CARTESIAN_POINT('Ctrl Pts',(64.1717857210691,9.82236564017501,60.65192402368));
#156325=CARTESIAN_POINT('Ctrl Pts',(81.6812403517491,9.15894488521401,57.12486504907));
#156326=CARTESIAN_POINT('Ctrl Pts',(81.142871413649,9.36443270586001,57.21979401843));
#156327=CARTESIAN_POINT('Ctrl Pts',(79.9622475576091,9.73581425448101,57.42796985832));
#156328=CARTESIAN_POINT('Ctrl Pts',(78.0423626199291,10.17045530359,57.76649737269));
#156329=CARTESIAN_POINT('Ctrl Pts',(75.8484052614891,10.49332376545,58.1533512495));
#156330=CARTESIAN_POINT('Ctrl Pts',(73.3942542810591,10.64955125961,58.58608428209));
#156331=CARTESIAN_POINT('Ctrl Pts',(70.8376991842391,10.56318716341,59.03687392332));
#156332=CARTESIAN_POINT('Ctrl Pts',(68.3911099103691,10.24980023947,59.46827362302));
#156333=CARTESIAN_POINT('Ctrl Pts',(66.2430704911391,9.78880499814102,59.84703092825));
#156334=CARTESIAN_POINT('Ctrl Pts',(64.9349823229891,9.38532215333301,60.07768216544));
#156335=CARTESIAN_POINT('Ctrl Pts',(64.3420242057991,9.15903754398101,60.18223667994));
#156336=CARTESIAN_POINT('Ctrl Pts',(81.4283134430791,8.39735189262101,57.33839798192));
#156337=CARTESIAN_POINT('Ctrl Pts',(80.9204091465791,8.59120264529501,57.427955213));
#156338=CARTESIAN_POINT('Ctrl Pts',(79.7891130493291,8.94769483083601,57.62743323812));
#156339=CARTESIAN_POINT('Ctrl Pts',(77.9277255921291,9.36927352953802,57.95564606838));
#156340=CARTESIAN_POINT('Ctrl Pts',(75.7948002560491,9.68316352566601,58.33173835296));
#156341=CARTESIAN_POINT('Ctrl Pts',(73.4114773856891,9.83480682238501,58.75198247875));
#156342=CARTESIAN_POINT('Ctrl Pts',(70.9308601961991,9.75106247277001,59.18938221806));
#156343=CARTESIAN_POINT('Ctrl Pts',(68.5517423507991,9.44637709127401,59.60888488449));
#156344=CARTESIAN_POINT('Ctrl Pts',(66.4673178597791,8.99885509146401,59.97642516151));
#156345=CARTESIAN_POINT('Ctrl Pts',(65.2121306335291,8.61091630694802,60.19774853534));
#156346=CARTESIAN_POINT('Ctrl Pts',(64.6527013880191,8.39743409036201,60.29639100512));
#156347=CARTESIAN_POINT('Ctrl Pts',(61.7087960388091,8.96199616764401,62.51282737052));
#156348=CARTESIAN_POINT('Ctrl Pts',(61.5698609821491,8.91295132180802,62.53238444947));
#156349=CARTESIAN_POINT('Ctrl Pts',(61.1109287379191,8.72474172236301,62.56944688524));
#156350=CARTESIAN_POINT('Ctrl Pts',(60.4269254807791,8.28965318991802,62.48943246867));
#156351=CARTESIAN_POINT('Ctrl Pts',(59.7821496029791,7.65995478656001,62.25896894211));
#156352=CARTESIAN_POINT('Ctrl Pts',(59.2815963525391,6.95212687654301,61.95938522881));
#156353=CARTESIAN_POINT('Ctrl Pts',(58.9002308413891,6.18282381217201,61.63205504275));
#156354=CARTESIAN_POINT('Ctrl Pts',(58.6155144813491,5.36332168350501,61.30598232287));
#156355=CARTESIAN_POINT('Ctrl Pts',(58.4087775349091,4.50277795774501,61.00312960765));
#156356=CARTESIAN_POINT('Ctrl Pts',(58.2676967409091,3.62424267013002,60.74495621511));
#156357=CARTESIAN_POINT('Ctrl Pts',(58.1753682422591,2.74535586735901,60.54030188331));
#156358=CARTESIAN_POINT('Ctrl Pts',(58.1174070039491,1.87206366585901,60.39022014666));
#156359=CARTESIAN_POINT('Ctrl Pts',(58.0841999562791,0.989209384080914,
60.29379447098));
#156360=CARTESIAN_POINT('Ctrl Pts',(58.0717192608791,0.0853586380197842,
60.2552299176));
#156361=CARTESIAN_POINT('Ctrl Pts',(58.0803412997091,-0.831619754236286,
60.28202412771));
#156362=CARTESIAN_POINT('Ctrl Pts',(58.1108074737091,-1.74388438871099,
60.37189799022));
#156363=CARTESIAN_POINT('Ctrl Pts',(58.1669615502191,-2.64765037633299,
60.5200731035));
#156364=CARTESIAN_POINT('Ctrl Pts',(58.2577587898791,-3.54868473576899,
60.72473754248));
#156365=CARTESIAN_POINT('Ctrl Pts',(58.3963509815491,-4.43903040165999,
60.98262707975));
#156366=CARTESIAN_POINT('Ctrl Pts',(58.5992125823491,-5.30768633024999,
61.28480916086));
#156367=CARTESIAN_POINT('Ctrl Pts',(58.8815263867091,-6.14095307104199,
61.61377902874));
#156368=CARTESIAN_POINT('Ctrl Pts',(59.2649866104491,-6.92834051674799,
61.94813791472));
#156369=CARTESIAN_POINT('Ctrl Pts',(59.773271127289,-7.65220305320499,62.25525822907));
#156370=CARTESIAN_POINT('Ctrl Pts',(60.4252820987391,-8.28925777980099,
62.48909095077));
#156371=CARTESIAN_POINT('Ctrl Pts',(61.1127782067391,-8.72598511128199,
62.56959587775));
#156372=CARTESIAN_POINT('Ctrl Pts',(61.5738723051191,-8.91455013048699,
62.53200605257));
#156373=CARTESIAN_POINT('Ctrl Pts',(61.7139245147291,-8.96379447908499,
62.51210995553));
#156374=CARTESIAN_POINT('Ctrl Pts',(61.4014954127191,9.08520596155202,61.44355402681));
#156375=CARTESIAN_POINT('Ctrl Pts',(61.2874245509091,9.03447923019001,61.4557756009));
#156376=CARTESIAN_POINT('Ctrl Pts',(60.9113316065891,8.83990361344802,61.47142631459));
#156377=CARTESIAN_POINT('Ctrl Pts',(60.3635251517091,8.39116201973901,61.3726104982501));
#156378=CARTESIAN_POINT('Ctrl Pts',(59.8745335491291,7.74580293368701,61.1432506871));
#156379=CARTESIAN_POINT('Ctrl Pts',(59.5187165013191,7.02447848409401,60.86473236401));
#156380=CARTESIAN_POINT('Ctrl Pts',(59.2664503582991,6.24374560589701,60.57342906056));
#156381=CARTESIAN_POINT('Ctrl Pts',(59.0925079293791,5.41430300349301,60.29253180843));
#156382=CARTESIAN_POINT('Ctrl Pts',(58.9765709581791,4.54438927710501,60.03779198931));
#156383=CARTESIAN_POINT('Ctrl Pts',(58.9055501263191,3.65710613517001,59.82467118793));
#156384=CARTESIAN_POINT('Ctrl Pts',(58.8647365117791,2.77013317747901,59.65814889886));
#156385=CARTESIAN_POINT('Ctrl Pts',(58.8424267403291,1.88911579779101,59.53724171955));
#156386=CARTESIAN_POINT('Ctrl Pts',(58.8311370770591,0.998433591798714,
59.46001421541));
#156387=CARTESIAN_POINT('Ctrl Pts',(58.8271635470091,0.0861862617952542,
59.42918292181));
#156388=CARTESIAN_POINT('Ctrl Pts',(58.8298939128291,-0.839419159311286,
59.45060263904));
#156389=CARTESIAN_POINT('Ctrl Pts',(58.8400687909492,-1.75979619587999,
59.52253773544));
#156390=CARTESIAN_POINT('Ctrl Pts',(58.8612623367191,-2.67154027375999,
59.6417775984));
#156391=CARTESIAN_POINT('Ctrl Pts',(58.9009231731791,-3.58087193680299,
59.80813714535));
#156392=CARTESIAN_POINT('Ctrl Pts',(58.9699394424191,-4.47995913630899,
60.02071203588));
#156393=CARTESIAN_POINT('Ctrl Pts',(59.0828230394891,-5.35795511875899,
60.27448991099));
#156394=CARTESIAN_POINT('Ctrl Pts',(59.2543775458091,-6.20124022696799,
60.55739034192));
#156395=CARTESIAN_POINT('Ctrl Pts',(59.5072378683591,-7.00026261349998,
60.85443640342));
#156396=CARTESIAN_POINT('Ctrl Pts',(59.8681473241091,-7.73789838758098,
61.13963055899));
#156397=CARTESIAN_POINT('Ctrl Pts',(60.3625395629591,-8.39079064494998,
61.37219504624));
#156398=CARTESIAN_POINT('Ctrl Pts',(60.9130033575691,-8.84120300394399,
61.4715825305));
#156399=CARTESIAN_POINT('Ctrl Pts',(61.2907349696091,-9.03613393057798,
61.45558231608));
#156400=CARTESIAN_POINT('Ctrl Pts',(61.4056779384191,-9.08706366640399,
61.44311667414));
#156401=CARTESIAN_POINT('Ctrl Pts',(61.4950703228691,8.31092208497201,60.64082694368));
#156402=CARTESIAN_POINT('Ctrl Pts',(61.4312159626292,8.27076477997901,60.6487343305501));
#156403=CARTESIAN_POINT('Ctrl Pts',(61.2204907529791,8.11619494844401,60.66160281426));
#156404=CARTESIAN_POINT('Ctrl Pts',(60.9100092313592,7.75325290741801,60.6154933257301));
#156405=CARTESIAN_POINT('Ctrl Pts',(60.6250557980591,7.20630981348502,60.49825917921));
#156406=CARTESIAN_POINT('Ctrl Pts',(60.4105475875591,6.56980129168201,60.35139718058));
#156407=CARTESIAN_POINT('Ctrl Pts',(60.2524225307591,5.86089647420301,60.1946002338601));
#156408=CARTESIAN_POINT('Ctrl Pts',(60.1384273166791,5.09392251407701,60.04102312208));
#156409=CARTESIAN_POINT('Ctrl Pts',(60.0585750382691,4.28289242169001,59.90011699997));
#156410=CARTESIAN_POINT('Ctrl Pts',(60.0063644514191,3.45058317703301,59.78113651281));
#156411=CARTESIAN_POINT('Ctrl Pts',(59.9737925723191,2.61442581751901,59.68750227682));
#156412=CARTESIAN_POINT('Ctrl Pts',(59.9542782938691,1.78195555997801,59.61917753525));
#156413=CARTESIAN_POINT('Ctrl Pts',(59.9435187238791,0.940466160123215,
59.5754076490299));
#156414=CARTESIAN_POINT('Ctrl Pts',(59.9395507897191,0.0809852487515842,
59.5579178275));
#156415=CARTESIAN_POINT('Ctrl Pts',(59.9422878235992,-0.790405575204286,
59.57006912894));
#156416=CARTESIAN_POINT('Ctrl Pts',(59.9521077472891,-1.65980206921799,
59.61085229615));
#156417=CARTESIAN_POINT('Ctrl Pts',(59.9708950406291,-2.52140965667399,
59.67827203419));
#156418=CARTESIAN_POINT('Ctrl Pts',(60.0027925917991,-3.37859880572699,
59.7718627086));
#156419=CARTESIAN_POINT('Ctrl Pts',(60.0538703201391,-4.22275182898199,
59.89062455975));
#156420=CARTESIAN_POINT('Ctrl Pts',(60.1319776920891,-5.04205237106898,
60.03110652867));
#156421=CARTESIAN_POINT('Ctrl Pts',(60.2447516350391,-5.82237933191699,
60.1859093365));
#156422=CARTESIAN_POINT('Ctrl Pts',(60.4035221583791,-6.54828458384299,
60.3459287535699));
#156423=CARTESIAN_POINT('Ctrl Pts',(60.6212298628391,-7.19936558429799,
60.49639210435));
#156424=CARTESIAN_POINT('Ctrl Pts',(60.9093564390591,-7.75273048808598,
60.61529830059));
#156425=CARTESIAN_POINT('Ctrl Pts',(61.2213839640791,-8.11714240979298,
60.66168084203));
#156426=CARTESIAN_POINT('Ctrl Pts',(61.4330643448691,-8.27206824165498,
60.64859350648));
#156427=CARTESIAN_POINT('Ctrl Pts',(61.4974194310191,-8.31240654545798,
60.64053996861));
#156428=CARTESIAN_POINT('Ctrl Pts',(61.9120241061091,7.28038925473501,60.76944687017));
#156429=CARTESIAN_POINT('Ctrl Pts',(61.8821503623991,7.25429932373901,60.77963430154));
#156430=CARTESIAN_POINT('Ctrl Pts',(61.7823674356291,7.15297517676501,60.81065422848));
#156431=CARTESIAN_POINT('Ctrl Pts',(61.6137917373691,6.90422801766101,60.84510858475));
#156432=CARTESIAN_POINT('Ctrl Pts',(61.4121504854391,6.48827165090601,60.85816206592));
#156433=CARTESIAN_POINT('Ctrl Pts',(61.2184949050291,5.96464885584601,60.84451248097));
#156434=CARTESIAN_POINT('Ctrl Pts',(61.0415870949391,5.35134356838701,60.8093061866));
#156435=CARTESIAN_POINT('Ctrl Pts',(60.8870654269791,4.66751222387701,60.75975017414));
#156436=CARTESIAN_POINT('Ctrl Pts',(60.7586980174391,3.93485328170701,60.70412400929));
#156437=CARTESIAN_POINT('Ctrl Pts',(60.6584697311591,3.17571152466401,60.65040664119));
#156438=CARTESIAN_POINT('Ctrl Pts',(60.5840408165191,2.40718716616401,60.60405220122));
#156439=CARTESIAN_POINT('Ctrl Pts',(60.5321508919591,1.63933068233101,60.56817017024));
#156440=CARTESIAN_POINT('Ctrl Pts',(60.5000951126591,0.863314429042514,
60.54440849196));
#156441=CARTESIAN_POINT('Ctrl Pts',(60.4876265705191,0.0740629624246842,
60.5348192438));
#156442=CARTESIAN_POINT('Ctrl Pts',(60.4962630912091,-0.725170964130086,
60.54148410271));
#156443=CARTESIAN_POINT('Ctrl Pts',(60.5259583672891,-1.52671492447299,
60.56370151384));
#156444=CARTESIAN_POINT('Ctrl Pts',(60.5768864913491,-2.32159336911999,
60.59933252936));
#156445=CARTESIAN_POINT('Ctrl Pts',(60.6508232556691,-3.10938345906399,
60.64595591541));
#156446=CARTESIAN_POINT('Ctrl Pts',(60.7504561259491,-3.88042186138999,
60.70010021104));
#156447=CARTESIAN_POINT('Ctrl Pts',(60.8777899489991,-4.62160172951099,
60.75622372783));
#156448=CARTESIAN_POINT('Ctrl Pts',(61.0324428208391,-5.31813456813899,
60.80698833398));
#156449=CARTESIAN_POINT('Ctrl Pts',(61.2115567297791,-5.94672459764799,
60.84374971148));
#156450=CARTESIAN_POINT('Ctrl Pts',(61.4088325039591,-6.48260555515498,
60.85825867285));
#156451=CARTESIAN_POINT('Ctrl Pts',(61.6128711300591,-6.90350456565199,
60.84524579483));
#156452=CARTESIAN_POINT('Ctrl Pts',(61.7825260542691,-7.15345423815299,
60.81063341023));
#156453=CARTESIAN_POINT('Ctrl Pts',(61.8829864021391,-7.25513530438499,
60.77936984004));
#156454=CARTESIAN_POINT('Ctrl Pts',(61.9131707250991,-7.28137694577499,
60.76905604858));
#156455=CARTESIAN_POINT('Ctrl Pts',(61.7095776082786,7.4812853662219,60.7844468788789));
#156456=CARTESIAN_POINT('Ctrl Pts',(61.7024296496402,7.47450503376971,60.7857109678101));
#156457=CARTESIAN_POINT('Ctrl Pts',(61.695272550974,7.46752133842146,60.7869235202457));
#156458=CARTESIAN_POINT('Ctrl Pts',(61.6881101684676,7.46033339730234,60.7880836318459));
#156459=CARTESIAN_POINT('Ctrl Pts',(61.6590245873343,7.43114402569089,60.7927947066929));
#156460=CARTESIAN_POINT('Ctrl Pts',(61.6298535312315,7.39858369876268,60.7966388545209));
#156461=CARTESIAN_POINT('Ctrl Pts',(61.6006617256375,7.36260348904996,60.7996058924316));
#156462=CARTESIAN_POINT('Ctrl Pts',(61.574030746394,7.32977961267307,60.8023126494617));
#156463=CARTESIAN_POINT('Ctrl Pts',(61.5473819531278,7.29410881954576,60.8042896853198));
#156464=CARTESIAN_POINT('Ctrl Pts',(61.5207555108983,7.2555898731445,60.8055486610889));
#156465=CARTESIAN_POINT('Ctrl Pts',(61.4962099300207,7.22008118948105,60.8067092476704));
#156466=CARTESIAN_POINT('Ctrl Pts',(61.4716829270121,7.18215149477169,60.8072596358207));
#156467=CARTESIAN_POINT('Ctrl Pts',(61.4472044231664,7.14184100557662,60.8072246296821));
#156468=CARTESIAN_POINT('Ctrl Pts',(61.4451292482964,7.13842366787081,60.8072216620228));
#156469=CARTESIAN_POINT('Ctrl Pts',(61.4430544231896,7.13498924959679,60.8072144974086));
#156470=CARTESIAN_POINT('Ctrl Pts',(61.4409799670258,7.13153779272376,60.8072031568315));
#156471=CARTESIAN_POINT('Ctrl Pts',(61.422576200912,7.10091781330252,60.8071025476531));
#156472=CARTESIAN_POINT('Ctrl Pts',(61.4042017000976,7.06895632298682,60.8066731820066));
#156473=CARTESIAN_POINT('Ctrl Pts',(61.3858482097925,7.03562826129724,60.8059072099783));
#156474=CARTESIAN_POINT('Ctrl Pts',(61.3612550949187,6.99096967941299,60.8048808309207));
#156475=CARTESIAN_POINT('Ctrl Pts',(61.3367290240724,6.94388825664927,60.8032499783446));
#156476=CARTESIAN_POINT('Ctrl Pts',(61.3123007852604,6.89435212608218,60.8010138805843));
#156477=CARTESIAN_POINT('Ctrl Pts',(61.2895289115423,6.84817480980348,60.798929402198));
#156478=CARTESIAN_POINT('Ctrl Pts',(61.2668420760223,6.79986414868234,60.7963188407643));
#156479=CARTESIAN_POINT('Ctrl Pts',(61.2442627728364,6.74943669867008,60.7931994062268));
#156480=CARTESIAN_POINT('Ctrl Pts',(61.2381450042524,6.7357735901624,60.7923542083721));
#156481=CARTESIAN_POINT('Ctrl Pts',(61.2320351136504,6.72195535069831,60.7914717671107));
#156482=CARTESIAN_POINT('Ctrl Pts',(61.225933508814,6.70798293461504,60.7905526945646));
#156483=CARTESIAN_POINT('Ctrl Pts',(61.2225114659508,6.70014660171226,60.790037239085));
#156484=CARTESIAN_POINT('Ctrl Pts',(61.2190919756263,6.69226105550839,60.7895102588224));
#156485=CARTESIAN_POINT('Ctrl Pts',(61.2156751295169,6.68432665296964,60.7889718818205));
#156486=CARTESIAN_POINT('Ctrl Pts',(61.1927425927241,6.63107404154833,60.785358505622));
#156487=CARTESIAN_POINT('Ctrl Pts',(61.169929987531,6.5756185258231,60.7812308129325));
#156488=CARTESIAN_POINT('Ctrl Pts',(61.1472630227814,6.51795609966164,60.7765797129808));
#156489=CARTESIAN_POINT('Ctrl Pts',(61.1342409018793,6.48482916390821,60.7739076663893));
#156490=CARTESIAN_POINT('Ctrl Pts',(61.1212670116287,6.45097431756662,60.7710631438124));
#156491=CARTESIAN_POINT('Ctrl Pts',(61.1083461984573,6.41639155685069,60.7680468976458));
#156492=CARTESIAN_POINT('Ctrl Pts',(61.1010131485361,6.39676453280979,60.7663350639228));
#156493=CARTESIAN_POINT('Ctrl Pts',(61.0934723320082,6.37629434955248,60.7645133489496));
#156494=CARTESIAN_POINT('Ctrl Pts',(61.0861103999751,6.35601441142343,60.7626738785569));
#156495=CARTESIAN_POINT('Ctrl Pts',(61.0805006286375,6.34056115606429,60.7612722073327));
#156496=CARTESIAN_POINT('Ctrl Pts',(61.07499388939,6.32521926176865,60.7598606323473));
#156497=CARTESIAN_POINT('Ctrl Pts',(61.0697473939376,6.31045954207386,60.7584858287314));
#156498=CARTESIAN_POINT('Ctrl Pts',(61.0495490913118,6.2536366042155,60.7531930195149));
#156499=CARTESIAN_POINT('Ctrl Pts',(61.029836906676,6.19598986728747,60.7475701238141));
#156500=CARTESIAN_POINT('Ctrl Pts',(61.0105904367975,6.13756557585011,60.7416749309707));
#156501=CARTESIAN_POINT('Ctrl Pts',(60.9813866365199,6.04891496359373,60.7327298082814));
#156502=CARTESIAN_POINT('Ctrl Pts',(60.9532547519052,5.95847333458106,60.723156234998));
#156503=CARTESIAN_POINT('Ctrl Pts',(60.9261963970484,5.86620260640735,60.7130815267755));
#156504=CARTESIAN_POINT('Ctrl Pts',(60.8991842623493,5.77408949194066,60.7030240278255));
#156505=CARTESIAN_POINT('Ctrl Pts',(60.8732428931832,5.68015349713977,60.6924671186045));
#156506=CARTESIAN_POINT('Ctrl Pts',(60.8483758680909,5.58438882133169,60.6815773773706));
#156507=CARTESIAN_POINT('Ctrl Pts',(60.8407944642082,5.55519229773041,60.6782573370293));
#156508=CARTESIAN_POINT('Ctrl Pts',(60.8333128853196,5.52582602612187,60.6749066403099));
#156509=CARTESIAN_POINT('Ctrl Pts',(60.8259310896484,5.49629045537718,60.6715307480661));
#156510=CARTESIAN_POINT('Ctrl Pts',(60.8209586139193,5.4763949021522,60.6692567021572));
#156511=CARTESIAN_POINT('Ctrl Pts',(60.8160314121518,5.4564225363887,60.6669712318813));
#156512=CARTESIAN_POINT('Ctrl Pts',(60.8111499698825,5.43637268458336,60.6646756052872));
#156513=CARTESIAN_POINT('Ctrl Pts',(60.7817493882788,5.31561384495521,60.6508492086425));
#156514=CARTESIAN_POINT('Ctrl Pts',(60.7539658830283,5.1920701708242,60.6366304267703));
#156515=CARTESIAN_POINT('Ctrl Pts',(60.7277506051091,5.06573719469669,60.6222409987507));
#156516=CARTESIAN_POINT('Ctrl Pts',(60.7203510690741,5.03007839252234,60.6181794323816));
#156517=CARTESIAN_POINT('Ctrl Pts',(60.7130763615802,4.99419754902143,60.6141044942699));
#156518=CARTESIAN_POINT('Ctrl Pts',(60.705925092349,4.95809503409377,60.610021715977));
#156519=CARTESIAN_POINT('Ctrl Pts',(60.6949873250782,4.90287673739608,60.6037771631092));
#156520=CARTESIAN_POINT('Ctrl Pts',(60.6843380832632,4.84713761316821,60.5975140635554));
#156521=CARTESIAN_POINT('Ctrl Pts',(60.6739694062406,4.790881130188,60.591251886166));
#156522=CARTESIAN_POINT('Ctrl Pts',(60.6689397390439,4.76359207620045,60.588214211434));
#156523=CARTESIAN_POINT('Ctrl Pts',(60.6639760762559,4.73618130800553,60.5851767731987));
#156524=CARTESIAN_POINT('Ctrl Pts',(60.6590780591191,4.70864760020753,60.5821412859459));
#156525=CARTESIAN_POINT('Ctrl Pts',(60.649274758987,4.65353934032295,60.5760658085118));
#156526=CARTESIAN_POINT('Ctrl Pts',(60.6396348571544,4.59735327204642,60.5699343033299));
#156527=CARTESIAN_POINT('Ctrl Pts',(60.6303500662329,4.54124210717251,60.5638847935891));
#156528=CARTESIAN_POINT('Ctrl Pts',(60.6254326807053,4.51152466577588,60.5606808688158));
#156529=CARTESIAN_POINT('Ctrl Pts',(60.6206140780844,4.48182863351887,60.5574998761221));
#156530=CARTESIAN_POINT('Ctrl Pts',(60.6159174747203,4.45232775894101,60.5543615921095));
#156531=CARTESIAN_POINT('Ctrl Pts',(60.5940061631212,4.31469577147727,60.5397203900414));
#156532=CARTESIAN_POINT('Ctrl Pts',(60.5736003025058,4.17611355577954,60.5252416566678));
#156533=CARTESIAN_POINT('Ctrl Pts',(60.5545755779023,4.03658419471692,60.5111020096261));
#156534=CARTESIAN_POINT('Ctrl Pts',(60.5293617251934,3.85166310746189,60.4923624491176));
#156535=CARTESIAN_POINT('Ctrl Pts',(60.5065743736299,3.66507755205774,60.4742174111081));
#156536=CARTESIAN_POINT('Ctrl Pts',(60.4859793913249,3.4767966879087,60.456955865348));
#156537=CARTESIAN_POINT('Ctrl Pts',(60.4774468298483,3.39879137455563,60.4498043563932));
#156538=CARTESIAN_POINT('Ctrl Pts',(60.4692904665321,3.32049537884637,60.4428050363997));
#156539=CARTESIAN_POINT('Ctrl Pts',(60.4614930446832,3.24190782947751,60.4359805891655));
#156540=CARTESIAN_POINT('Ctrl Pts',(60.4416275428167,3.04169022692585,60.4185939360006));
#156541=CARTESIAN_POINT('Ctrl Pts',(60.424092686678,2.83957778210097,60.4023397510308));
#156542=CARTESIAN_POINT('Ctrl Pts',(60.4087338989989,2.63560418090611,60.3875429756916));
#156543=CARTESIAN_POINT('Ctrl Pts',(60.4043124393325,2.57688463418718,60.3832833071083));
#156544=CARTESIAN_POINT('Ctrl Pts',(60.400071235891,2.51801106594078,60.3791446537451));
#156545=CARTESIAN_POINT('Ctrl Pts',(60.39600639891,2.45898482913597,60.3751353034089));
#156546=CARTESIAN_POINT('Ctrl Pts',(60.3932155221246,2.41845799994142,60.3723825232038));
#156547=CARTESIAN_POINT('Ctrl Pts',(60.3905077826995,2.37785920718455,60.3696907021608));
#156548=CARTESIAN_POINT('Ctrl Pts',(60.3878828126484,2.33718887814358,60.3670623245156));
#156549=CARTESIAN_POINT('Ctrl Pts',(60.3739061773947,2.12063998669542,60.3530675455505));
#156550=CARTESIAN_POINT('Ctrl Pts',(60.3622162362926,1.90202463683472,60.3408126922032));
#156551=CARTESIAN_POINT('Ctrl Pts',(60.3525787012096,1.68133585233899,60.3304806711094));
#156552=CARTESIAN_POINT('Ctrl Pts',(60.3460059668921,1.53082758078909,60.3234343019883));
#156553=CARTESIAN_POINT('Ctrl Pts',(60.3403881456358,1.37935474928527,60.3172824889154));
#156554=CARTESIAN_POINT('Ctrl Pts',(60.3356972804706,1.22692157740655,60.3120816036346));
#156555=CARTESIAN_POINT('Ctrl Pts',(60.3322532820412,1.11500627265237,60.3082631522174));
#156556=CARTESIAN_POINT('Ctrl Pts',(60.3293057405566,1.00256704992089,60.3049537472116));
#156557=CARTESIAN_POINT('Ctrl Pts',(60.3268350319213,0.889614900065707,
60.3021659554015));
#156558=CARTESIAN_POINT('Ctrl Pts',(60.3251559545933,0.812853362403946,
60.3002713904349));
#156559=CARTESIAN_POINT('Ctrl Pts',(60.3236971188136,0.735854947945547,
60.2986177588588));
#156560=CARTESIAN_POINT('Ctrl Pts',(60.3224579481672,0.658613460198747,
60.2972083801014));
#156561=CARTESIAN_POINT('Ctrl Pts',(60.3209266628389,0.563163525790775,
60.2954667628195));
#156562=CARTESIAN_POINT('Ctrl Pts',(60.3197296564896,0.46734763396879,60.2940967785737));
#156563=CARTESIAN_POINT('Ctrl Pts',(60.3188631184893,0.371165784773678,
60.2931017944797));
#156564=CARTESIAN_POINT('Ctrl Pts',(60.3182849037355,0.306986528656438,
60.2924378715094));
#156565=CARTESIAN_POINT('Ctrl Pts',(60.3178591568679,0.243471706970596,
60.2919470610062));
#156566=CARTESIAN_POINT('Ctrl Pts',(60.3175725545398,0.178965076606698,
60.2916165290168));
#156567=CARTESIAN_POINT('Ctrl Pts',(60.3174296420437,0.146799240365323,
60.2914517112643));
#156568=CARTESIAN_POINT('Ctrl Pts',(60.3173218438238,0.114386787195183,
60.2913273379523));
#156569=CARTESIAN_POINT('Ctrl Pts',(60.3172506780976,0.0815223650375594,
60.2912455157613));
#156570=CARTESIAN_POINT('Ctrl Pts',(60.3172503297988,0.0813615201835923,
60.2912451153076));
#156571=CARTESIAN_POINT('Ctrl Pts',(60.3172499824342,0.0812006763251198,
60.2912447159388));
#156572=CARTESIAN_POINT('Ctrl Pts',(60.317249636004,0.0810398334620816,
60.2912443176547));
#156573=CARTESIAN_POINT('Ctrl Pts',(60.3167718356663,-0.140796408850023,
60.2906949999507));
#156574=CARTESIAN_POINT('Ctrl Pts',(60.3180703536722,-0.360742013675031,
60.2922059588602));
#156575=CARTESIAN_POINT('Ctrl Pts',(60.3211269691535,-0.579049577315057,
60.2956904127889));
#156576=CARTESIAN_POINT('Ctrl Pts',(60.3218918879312,-0.633681098928665,
60.2965623982435));
#156577=CARTESIAN_POINT('Ctrl Pts',(60.3227669758375,-0.68820986561593,
60.2975581540585));
#156578=CARTESIAN_POINT('Ctrl Pts',(60.3237521056527,-0.74263949039439,
60.2986766416983));
#156579=CARTESIAN_POINT('Ctrl Pts',(60.3284060612508,-0.999776217996843,
60.3039606070528));
#156580=CARTESIAN_POINT('Ctrl Pts',(60.3355132095719,-1.25470074694503,
60.311980556618));
#156581=CARTESIAN_POINT('Ctrl Pts',(60.3452494162381,-1.50725414925296,
60.3225677543551));
#156582=CARTESIAN_POINT('Ctrl Pts',(60.3460161107382,-1.52714190545754,
60.3234014616248));
#156583=CARTESIAN_POINT('Ctrl Pts',(60.3467991282248,-1.5470149527718,60.3242511050648));
#156584=CARTESIAN_POINT('Ctrl Pts',(60.3475985655576,-1.56687321040098,
60.3251166094454));
#156585=CARTESIAN_POINT('Ctrl Pts',(60.3564916635564,-1.78778037090632,
60.3347446502675));
#156586=CARTESIAN_POINT('Ctrl Pts',(60.3674147954383,-2.00685857303107,
60.3463353301896));
#156587=CARTESIAN_POINT('Ctrl Pts',(60.380647663187,-2.22400159825584,60.3597674794863));
#156588=CARTESIAN_POINT('Ctrl Pts',(60.3837181096662,-2.27438569110276,
60.3628841656272));
#156589=CARTESIAN_POINT('Ctrl Pts',(60.3869109222145,-2.3246719574547,60.3660978702397));
#156590=CARTESIAN_POINT('Ctrl Pts',(60.3902275060726,-2.37485945220486,
60.3694049280582));
#156591=CARTESIAN_POINT('Ctrl Pts',(60.4060853424734,-2.61482476445802,
60.3852172168766));
#156592=CARTESIAN_POINT('Ctrl Pts',(60.424773147128,-2.85252956131487,60.4031603549941));
#156593=CARTESIAN_POINT('Ctrl Pts',(60.4466410345141,-3.0879812331881,60.4228099521189));
#156594=CARTESIAN_POINT('Ctrl Pts',(60.4494095158189,-3.11778948765049,
60.4252975971906));
#156595=CARTESIAN_POINT('Ctrl Pts',(60.4522289621883,-3.14756166853934,
60.4278126490277));
#156596=CARTESIAN_POINT('Ctrl Pts',(60.4551000813933,-3.17729782317844,
60.4303542964061));
#156597=CARTESIAN_POINT('Ctrl Pts',(60.4599606519324,-3.22763870660009,
60.4346570980267));
#156598=CARTESIAN_POINT('Ctrl Pts',(60.4649693168118,-3.2778763364631,60.4390361153204));
#156599=CARTESIAN_POINT('Ctrl Pts',(60.4701313186931,-3.32801012367678,
60.4434860043842));
#156600=CARTESIAN_POINT('Ctrl Pts',(60.4887980564844,-3.50930301777317,
60.4595776126911));
#156601=CARTESIAN_POINT('Ctrl Pts',(60.5094620301379,-3.68924165233354,
60.4765856585227));
#156602=CARTESIAN_POINT('Ctrl Pts',(60.5323041457749,-3.86782602254368,
60.4942268967716));
#156603=CARTESIAN_POINT('Ctrl Pts',(60.5371864013529,-3.90599650339826,
60.4979975209647));
#156604=CARTESIAN_POINT('Ctrl Pts',(60.5421679901616,-3.94410501957805,
60.5017970980832));
#156605=CARTESIAN_POINT('Ctrl Pts',(60.5472503730506,-3.98215175049627,
60.5056229160797));
#156606=CARTESIAN_POINT('Ctrl Pts',(60.5540572056899,-4.03310771652428,
60.5107468320417));
#156607=CARTESIAN_POINT('Ctrl Pts',(60.5610448370004,-4.08395284819393,
60.5159178009482));
#156608=CARTESIAN_POINT('Ctrl Pts',(60.5682184982992,-4.13468687987222,
60.5211266905536));
#156609=CARTESIAN_POINT('Ctrl Pts',(60.5744834683542,-4.17899440653005,
60.5256757675225));
#156610=CARTESIAN_POINT('Ctrl Pts',(60.5808903363372,-4.22321729183196,
60.5302537784216));
#156611=CARTESIAN_POINT('Ctrl Pts',(60.5874421641437,-4.26735553575933,
60.5348546200745));
#156612=CARTESIAN_POINT('Ctrl Pts',(60.5926973823719,-4.30275880197777,
60.5385449531591));
#156613=CARTESIAN_POINT('Ctrl Pts',(60.5979225873047,-4.33730075434144,
60.5421653199955));
#156614=CARTESIAN_POINT('Ctrl Pts',(60.6034153254535,-4.37292320597405,
60.5459162536311));
#156615=CARTESIAN_POINT('Ctrl Pts',(60.604770537851,-4.38171226286584,60.5468417140531));
#156616=CARTESIAN_POINT('Ctrl Pts',(60.6061422543349,-4.39056699089614,
60.5477751634014));
#156617=CARTESIAN_POINT('Ctrl Pts',(60.6075353869347,-4.39951634329599,
60.5487196897732));
#156618=CARTESIAN_POINT('Ctrl Pts',(60.6256697600186,-4.51600984527997,
60.5610145665249));
#156619=CARTESIAN_POINT('Ctrl Pts',(60.644794645044,-4.63022759689235,60.57339439645));
#156620=CARTESIAN_POINT('Ctrl Pts',(60.6649277275938,-4.74223674371549,
60.5857482471537));
#156621=CARTESIAN_POINT('Ctrl Pts',(60.6883341692675,-4.87245701950087,
60.6001106621106));
#156622=CARTESIAN_POINT('Ctrl Pts',(60.713104510655,-4.99968962535541,60.6144367085336));
#156623=CARTESIAN_POINT('Ctrl Pts',(60.7393115847284,-5.12389259812989,
60.6285186139536));
#156624=CARTESIAN_POINT('Ctrl Pts',(60.7605670573277,-5.22462848635463,
60.6399398643367));
#156625=CARTESIAN_POINT('Ctrl Pts',(60.7827670219855,-5.32337236172495,
60.6512013180985));
#156626=CARTESIAN_POINT('Ctrl Pts',(60.8059386129769,-5.42011754924029,
60.6622075350583));
#156627=CARTESIAN_POINT('Ctrl Pts',(60.8089240145654,-5.43258208983175,
60.6636255636092));
#156628=CARTESIAN_POINT('Ctrl Pts',(60.8119255029196,-5.44501355984374,
60.6650393579304));
#156629=CARTESIAN_POINT('Ctrl Pts',(60.8149430121899,-5.45741210818994,
60.6664486765836));
#156630=CARTESIAN_POINT('Ctrl Pts',(60.8393451527445,-5.55767729126446,
60.6778456231317));
#156631=CARTESIAN_POINT('Ctrl Pts',(60.8647961665854,-5.6557865365155,60.6889466944976));
#156632=CARTESIAN_POINT('Ctrl Pts',(60.8913187722302,-5.75173231434,60.6995837830937));
#156633=CARTESIAN_POINT('Ctrl Pts',(60.9034359144587,-5.7955661914367,60.7044434532612));
#156634=CARTESIAN_POINT('Ctrl Pts',(60.9157765342813,-5.83894899354787,
60.7092068094858));
#156635=CARTESIAN_POINT('Ctrl Pts',(60.9283421344644,-5.88188235016986,
60.713860427064));
#156636=CARTESIAN_POINT('Ctrl Pts',(60.9500775929391,-5.95614670495086,
60.7219100633849));
#156637=CARTESIAN_POINT('Ctrl Pts',(60.9724838128451,-6.02906282046898,
60.7296294861063));
#156638=CARTESIAN_POINT('Ctrl Pts',(60.9955541308482,-6.1006307460953,60.7369568347596));
#156639=CARTESIAN_POINT('Ctrl Pts',(60.9978757070085,-6.1078326576577,60.7376941890496));
#156640=CARTESIAN_POINT('Ctrl Pts',(61.000204018296,-6.11502084322828,60.7384275901662));
#156641=CARTESIAN_POINT('Ctrl Pts',(61.0025390361617,-6.12219540860419,
60.7391569766818));
#156642=CARTESIAN_POINT('Ctrl Pts',(61.0118059647722,-6.15066893170974,
60.7420516752059));
#156643=CARTESIAN_POINT('Ctrl Pts',(61.0211785101258,-6.17892787314475,
60.7448830833879));
#156644=CARTESIAN_POINT('Ctrl Pts',(61.0306570702488,-6.20697150151012,
60.7476440444355));
#156645=CARTESIAN_POINT('Ctrl Pts',(61.0381576299283,-6.22916294255784,
60.749828843903));
#156646=CARTESIAN_POINT('Ctrl Pts',(61.0455411532524,-6.25068477398866,
60.7519180674648));
#156647=CARTESIAN_POINT('Ctrl Pts',(61.0531533692364,-6.27255314702256,
60.7540067349002));
#156648=CARTESIAN_POINT('Ctrl Pts',(61.0575847121439,-6.28528350831903,
60.755222622842));
#156649=CARTESIAN_POINT('Ctrl Pts',(61.062094186921,-6.29813075474211,60.7564380996644));
#156650=CARTESIAN_POINT('Ctrl Pts',(61.0667557827805,-6.31128995373525,
60.7576696460975));
#156651=CARTESIAN_POINT('Ctrl Pts',(61.0928128619575,-6.38484637098175,
60.7645536626201));
#156652=CARTESIAN_POINT('Ctrl Pts',(61.1190916473322,-6.45534327866974,
60.7707317505738));
#156653=CARTESIAN_POINT('Ctrl Pts',(61.1455952625239,-6.52281934308269,
60.7762000466415));
#156654=CARTESIAN_POINT('Ctrl Pts',(61.167445218974,-6.57844756806917,60.7807081875147));
#156655=CARTESIAN_POINT('Ctrl Pts',(61.189447687566,-6.63202403649182,60.7847346252518));
#156656=CARTESIAN_POINT('Ctrl Pts',(61.2115992402602,-6.6835937174199,60.788288103955));
#156657=CARTESIAN_POINT('Ctrl Pts',(61.2348668728669,-6.73776167602956,
60.7920206205006));
#156658=CARTESIAN_POINT('Ctrl Pts',(61.2582990475287,-6.78971265842065,
60.7952301642865));
#156659=CARTESIAN_POINT('Ctrl Pts',(61.2818913036666,-6.83939922853566,
60.7978832027763));
#156660=CARTESIAN_POINT('Ctrl Pts',(61.3078113879601,-6.89398833091362,
60.8007980143521));
#156661=CARTESIAN_POINT('Ctrl Pts',(61.3339248025162,-6.94584436954833,
60.8030412191049));
#156662=CARTESIAN_POINT('Ctrl Pts',(61.3602187632956,-6.99496701511857,
60.8045939876081));
#156663=CARTESIAN_POINT('Ctrl Pts',(61.3862767718842,-7.04364885240078,
60.8061328221462));
#156664=CARTESIAN_POINT('Ctrl Pts',(61.4125121580285,-7.08964728722199,
60.8069939889131));
#156665=CARTESIAN_POINT('Ctrl Pts',(61.4389049804967,-7.13300804515157,
60.8071780886852));
#156666=CARTESIAN_POINT('Ctrl Pts',(61.4630245950937,-7.17263415073987,
60.8073463319853));
#156667=CARTESIAN_POINT('Ctrl Pts',(61.4872746627032,-7.21005544093054,
60.8069483336587));
#156668=CARTESIAN_POINT('Ctrl Pts',(61.5115944597208,-7.2452196605957,60.805949935138));
#156669=CARTESIAN_POINT('Ctrl Pts',(61.537167996932,-7.28219667481437,60.8049000669298));
#156670=CARTESIAN_POINT('Ctrl Pts',(61.5628187966211,-7.31667846300659,
60.8031863964706));
#156671=CARTESIAN_POINT('Ctrl Pts',(61.5884809504075,-7.34865871299229,
60.8007929533979));
#156672=CARTESIAN_POINT('Ctrl Pts',(61.6161756530536,-7.38317193122326,
60.7982099397214));
#156673=CARTESIAN_POINT('Ctrl Pts',(61.6438837458237,-7.41477211492232,
60.7948351645046));
#156674=CARTESIAN_POINT('Ctrl Pts',(61.6715250991893,-7.44350522364788,
60.7906751871624));
#156675=CARTESIAN_POINT('Ctrl Pts',(61.6771954599592,-7.4493995476471,60.7898218073726));
#156676=CARTESIAN_POINT('Ctrl Pts',(61.6828630158119,-7.45517337202722,
60.7889354688476));
#156677=CARTESIAN_POINT('Ctrl Pts',(61.6885270782846,-7.46082731767655,
60.7880163558176));
#156678=CARTESIAN_POINT('Ctrl Pts',(61.6955489848948,-7.46783668216003,
60.786876904074));
#156679=CARTESIAN_POINT('Ctrl Pts',(61.702565503283,-7.47466179683456,60.7856870811896));
#156680=CARTESIAN_POINT('Ctrl Pts',(61.7095727627346,-7.48130385739646,
60.7844478028312));
#156681=CARTESIAN_POINT('Origin',(61.4493580047591,-11.67384127833,59.30720639017));
#156682=CARTESIAN_POINT('Origin',(1.07038457110909,25.,122.41156512159));
#156683=CARTESIAN_POINT('Origin',(-10.9843331791359,-92.5,80.581991049076));
#156684=CARTESIAN_POINT('Ctrl Pts',(29.5338632414891,-0.462029067073086,
63.010868215388));
#156685=CARTESIAN_POINT('Ctrl Pts',(29.5346219246491,-0.433752793220286,
63.011230106753));
#156686=CARTESIAN_POINT('Ctrl Pts',(29.5608039722791,0.641998223276014,
63.023714156154));
#156687=CARTESIAN_POINT('Ctrl Pts',(29.4078372281691,2.83176758612401,62.95026782851));
#156688=CARTESIAN_POINT('Ctrl Pts',(28.5737667388991,6.01426195252202,62.55847749973));
#156689=CARTESIAN_POINT('Ctrl Pts',(27.1713456340891,8.95881369369201,61.93185808602));
#156690=CARTESIAN_POINT('Ctrl Pts',(25.3938118350091,11.44424088043,61.19592371053));
#156691=CARTESIAN_POINT('Ctrl Pts',(23.4862351945491,13.39803722808,60.47438298443));
#156692=CARTESIAN_POINT('Ctrl Pts',(21.5959186421791,14.88576337841,59.82526804813));
#156693=CARTESIAN_POINT('Ctrl Pts',(19.7728932383691,16.01167021338,59.25919610008));
#156694=CARTESIAN_POINT('Ctrl Pts',(17.9890179586191,16.88023517151,58.75958030935));
#156695=CARTESIAN_POINT('Ctrl Pts',(16.1694318501091,17.56205741783,58.30367386163));
#156696=CARTESIAN_POINT('Ctrl Pts',(14.2545233152291,18.07545203247,57.8825033362001));
#156697=CARTESIAN_POINT('Ctrl Pts',(12.2750306503891,18.39974030706,57.50985034058));
#156698=CARTESIAN_POINT('Ctrl Pts',(10.2979506383991,18.52298246441,57.20011317475));
#156699=CARTESIAN_POINT('Ctrl Pts',(8.29553577903909,18.45025449476,56.94745644735));
#156700=CARTESIAN_POINT('Ctrl Pts',(6.18046749893909,18.15452185092,56.74590079812));
#156701=CARTESIAN_POINT('Ctrl Pts',(3.8630583959391,17.55006605826,56.60308243839));
#156702=CARTESIAN_POINT('Ctrl Pts',(1.35289501732909,16.52026706539,56.54071687939));
#156703=CARTESIAN_POINT('Ctrl Pts',(-1.22835397511091,14.96025853102,56.57780430316));
#156704=CARTESIAN_POINT('Ctrl Pts',(-2.82698452737391,13.56768331313,56.66360640014));
#156705=CARTESIAN_POINT('Ctrl Pts',(-3.58348738863291,12.77819820572,56.71617340988));
#156706=CARTESIAN_POINT('Ctrl Pts',(30.0860529662091,-0.465286448929386,
62.05420413572));
#156707=CARTESIAN_POINT('Ctrl Pts',(30.0868281149291,-0.436810905979286,
62.05457485453));
#156708=CARTESIAN_POINT('Ctrl Pts',(30.1135782153191,0.646521910559514,
62.06736342767));
#156709=CARTESIAN_POINT('Ctrl Pts',(29.9572832439191,2.85177150159601,61.99211983581));
#156710=CARTESIAN_POINT('Ctrl Pts',(29.1052651413891,6.05572682568202,61.59085102028));
#156711=CARTESIAN_POINT('Ctrl Pts',(27.6732347629591,9.01845477515302,60.9493802108601));
#156712=CARTESIAN_POINT('Ctrl Pts',(25.8588487868591,11.51786388819,60.196375469));
#156713=CARTESIAN_POINT('Ctrl Pts',(23.9121691835891,13.48193550668,59.45836886149));
#156714=CARTESIAN_POINT('Ctrl Pts',(21.9833029704391,14.97718508481,58.7946079262));
#156715=CARTESIAN_POINT('Ctrl Pts',(20.1231372976191,16.10868985698,58.2158677272001));
#156716=CARTESIAN_POINT('Ctrl Pts',(18.3028628908391,16.98156509667,57.70514405855));
#156717=CARTESIAN_POINT('Ctrl Pts',(16.4460310900391,17.66679861647,57.23916702843));
#156718=CARTESIAN_POINT('Ctrl Pts',(14.4917463634591,18.18280526933,56.80876811987));
#156719=CARTESIAN_POINT('Ctrl Pts',(12.4713202820591,18.50878353077,56.42804576509));
#156720=CARTESIAN_POINT('Ctrl Pts',(10.4531101100391,18.6326885709,56.11172577456));
#156721=CARTESIAN_POINT('Ctrl Pts',(8.40879716453909,18.55957000061,55.85386194703));
#156722=CARTESIAN_POINT('Ctrl Pts',(6.24923249066909,18.26219087574,55.6483878136801));
#156723=CARTESIAN_POINT('Ctrl Pts',(3.88282255928909,17.6542832528,55.50319038629));
#156724=CARTESIAN_POINT('Ctrl Pts',(1.31936572697909,16.61847639235,55.44054243506));
#156725=CARTESIAN_POINT('Ctrl Pts',(-1.31681310253091,15.04922855625,55.47988027154));
#156726=CARTESIAN_POINT('Ctrl Pts',(-2.94946644714391,13.64834848308,55.5686612246301));
#156727=CARTESIAN_POINT('Ctrl Pts',(-3.72205763400691,12.85415388889,55.6229400250801));
#156728=CARTESIAN_POINT('Ctrl Pts',(29.6438402590691,-0.440906405366586,
61.0422837596));
#156729=CARTESIAN_POINT('Ctrl Pts',(29.6445863481391,-0.413922302316986,
61.04263099393));
#156730=CARTESIAN_POINT('Ctrl Pts',(29.6703352983091,0.612664138304914,
61.0546093697601));
#156731=CARTESIAN_POINT('Ctrl Pts',(29.5199825989191,2.70205115803401,60.98418855492));
#156732=CARTESIAN_POINT('Ctrl Pts',(28.6983885856991,5.74538083047302,60.60757066705));
#156733=CARTESIAN_POINT('Ctrl Pts',(27.3118968411491,8.57206800556001,60.00247848032));
#156734=CARTESIAN_POINT('Ctrl Pts',(25.5485386075391,10.96682866558,59.28852217894));
#156735=CARTESIAN_POINT('Ctrl Pts',(23.6522177073491,12.85399448613,58.58612492656));
#156736=CARTESIAN_POINT('Ctrl Pts',(21.7712823376891,14.29293457848,57.95274708762));
#156737=CARTESIAN_POINT('Ctrl Pts',(19.9569744205691,15.3825412991,57.399474373));
#156738=CARTESIAN_POINT('Ctrl Pts',(18.1821311163691,16.22315601275,56.9105053048901));
#156739=CARTESIAN_POINT('Ctrl Pts',(16.3728054944391,16.88285767912,56.46373198555));
#156740=CARTESIAN_POINT('Ctrl Pts',(14.4702883739891,17.37931439633,56.0503330424501));
#156741=CARTESIAN_POINT('Ctrl Pts',(12.5056416128591,17.69264386349,55.6837038022));
#156742=CARTESIAN_POINT('Ctrl Pts',(10.5455810396291,17.81158752306,55.37787002278));
#156743=CARTESIAN_POINT('Ctrl Pts',(8.56254414565909,17.74139242357,55.12695247192));
#156744=CARTESIAN_POINT('Ctrl Pts',(6.4700871073191,17.45633647142,54.9246919594001));
#156745=CARTESIAN_POINT('Ctrl Pts',(4.17965284087909,16.87426425135,54.77784196221));
#156746=CARTESIAN_POINT('Ctrl Pts',(1.70063539712909,15.88342358762,54.70699356138));
#156747=CARTESIAN_POINT('Ctrl Pts',(-0.847455673380912,14.38332778486,54.73062029495));
#156748=CARTESIAN_POINT('Ctrl Pts',(-2.42552047959091,13.04460583201,54.80507482908));
#156749=CARTESIAN_POINT('Ctrl Pts',(-3.17239712901691,12.28565963609,54.85169577897));
#156750=CARTESIAN_POINT('Ctrl Pts',(28.5669936237991,-0.408723671234686,
60.79836945316));
#156751=CARTESIAN_POINT('Ctrl Pts',(28.5676887698891,-0.383708334716086,
60.79867999721));
#156752=CARTESIAN_POINT('Ctrl Pts',(28.5916818669991,0.567970383760914,
60.80939260235));
#156753=CARTESIAN_POINT('Ctrl Pts',(28.4517075181491,2.50441369284601,60.74649096621));
#156754=CARTESIAN_POINT('Ctrl Pts',(27.6841573416491,5.33571041184002,60.40859830391));
#156755=CARTESIAN_POINT('Ctrl Pts',(26.3813035283791,7.98281775714401,59.8615184069));
#156756=CARTESIAN_POINT('Ctrl Pts',(24.7153386034591,10.23943783787,59.21096093285));
#156757=CARTESIAN_POINT('Ctrl Pts',(22.9178680255491,12.02508460897,58.5672777695));
#156758=CARTESIAN_POINT('Ctrl Pts',(21.1323491770191,13.38969369344,57.98459351753));
#156759=CARTESIAN_POINT('Ctrl Pts',(19.4095888040891,14.4239931358,57.47420458465));
#156760=CARTESIAN_POINT('Ctrl Pts',(17.7250457055691,15.22202253043,57.02215382759));
#156761=CARTESIAN_POINT('Ctrl Pts',(16.0093287990591,15.84802102278,56.60823505731));
#156762=CARTESIAN_POINT('Ctrl Pts',(14.2076068025491,16.3186709616,56.22423386201));
#156763=CARTESIAN_POINT('Ctrl Pts',(12.3500720308091,16.61530346173,55.88239455409));
#156764=CARTESIAN_POINT('Ctrl Pts',(10.5001323733591,16.72769787988,55.59558481383));
#156765=CARTESIAN_POINT('Ctrl Pts',(8.63169365612909,16.66136189094,55.35811567321));
#156766=CARTESIAN_POINT('Ctrl Pts',(6.66335190121909,16.39257307097,55.16358639907));
#156767=CARTESIAN_POINT('Ctrl Pts',(4.51205869883909,15.8446047236,55.01715480186));
#156768=CARTESIAN_POINT('Ctrl Pts',(2.18651660771909,14.91312142525,54.93685948768));
#156769=CARTESIAN_POINT('Ctrl Pts',(-0.202134170110909,13.50430936028,54.93959559631));
#156770=CARTESIAN_POINT('Ctrl Pts',(-1.68141039720091,12.24763887117,54.99407390047));
#156771=CARTESIAN_POINT('Ctrl Pts',(-2.38169007766091,11.53522211755,55.02989751292));
#156772=CARTESIAN_POINT('Ctrl Pts',(28.8585550967491,1.26413730024185E-6,
60.89678211462));
#156773=CARTESIAN_POINT('Ctrl Pts',(28.858491969845,0.228821303340967,60.8967613163214));
#156774=CARTESIAN_POINT('Ctrl Pts',(28.8510774183777,0.568453705395284,
60.8934108792682));
#156775=CARTESIAN_POINT('Ctrl Pts',(28.8326729224955,0.90268677766527,60.8851040611296));
#156776=CARTESIAN_POINT('Ctrl Pts',(28.8179599071217,1.12430897478207,60.8784672952805));
#156777=CARTESIAN_POINT('Ctrl Pts',(28.8095647672157,1.23247330649146,60.8746818567286));
#156778=CARTESIAN_POINT('Ctrl Pts',(28.7796142842825,1.56744757292938,60.8611868260539));
#156779=CARTESIAN_POINT('Ctrl Pts',(28.7541873146485,1.79256287037361,60.8497408086264));
#156780=CARTESIAN_POINT('Ctrl Pts',(28.6923951978587,2.24639170489994,60.8219907114747));
#156781=CARTESIAN_POINT('Ctrl Pts',(28.6563900151882,2.47312237571838,60.8058475219207));
#156782=CARTESIAN_POINT('Ctrl Pts',(28.5297685422649,3.17060894521255,60.7492526345571));
#156783=CARTESIAN_POINT('Ctrl Pts',(28.4234973497442,3.63253854932098,60.7019477744694));
#156784=CARTESIAN_POINT('Ctrl Pts',(28.1669437708712,4.55027487309582,60.5888659622799));
#156785=CARTESIAN_POINT('Ctrl Pts',(28.0159853327217,5.0078552723136,60.5227968948521));
#156786=CARTESIAN_POINT('Ctrl Pts',(27.7582589840107,5.6843126691546,60.4114351412588));
#156787=CARTESIAN_POINT('Ctrl Pts',(27.6670035462099,5.90831132426182,60.3722155270459));
#156788=CARTESIAN_POINT('Ctrl Pts',(27.4737411368527,6.35333434679668,60.2897187140422));
#156789=CARTESIAN_POINT('Ctrl Pts',(27.3722215625238,6.57354671851138,60.2466453528615));
#156790=CARTESIAN_POINT('Ctrl Pts',(27.2093554140172,6.90572110665497,60.1780719445438));
#156791=CARTESIAN_POINT('Ctrl Pts',(27.1533394348912,7.01669623622962,60.1545704718447));
#156792=CARTESIAN_POINT('Ctrl Pts',(27.0378418193842,7.23914716243249,60.1063078690635));
#156793=CARTESIAN_POINT('Ctrl Pts',(26.97788687327,7.35140606811306,60.0813513934283));
#156794=CARTESIAN_POINT('Ctrl Pts',(26.8578818260713,7.57081252828534,60.0316067674831));
#156795=CARTESIAN_POINT('Ctrl Pts',(26.7675113001991,7.73203134537305,59.9942985092506));
#156796=CARTESIAN_POINT('Ctrl Pts',(26.6765895476588,7.8882461203985,59.9569948841178));
#156797=CARTESIAN_POINT('Ctrl Pts',(26.615852428485,7.99127729440162,59.9321273136503));
#156798=CARTESIAN_POINT('Ctrl Pts',(26.5844046075602,8.04391960438276,59.9192792403542));
#156799=CARTESIAN_POINT('Ctrl Pts',(26.083358749802,8.87217405440387,59.7149904794122));
#156800=CARTESIAN_POINT('Ctrl Pts',(25.5447392608045,9.6186234322292,59.5014887823171));
#156801=CARTESIAN_POINT('Ctrl Pts',(24.9372755532191,10.33198097767,59.2718675406));
#156802=CARTESIAN_POINT('Ctrl Pts',(26.0609344740391,10.60241468947,60.52351356035));
#156803=CARTESIAN_POINT('Ctrl Pts',(25.9123339633033,10.8117020094606,60.5051762448939));
#156804=CARTESIAN_POINT('Ctrl Pts',(25.7589271266988,11.0173666357863,60.4890488905304));
#156805=CARTESIAN_POINT('Ctrl Pts',(25.6004937437591,11.2187557868,60.4750588099));
#156806=CARTESIAN_POINT('Origin',(24.4068932609991,-15.54362135317,60.67496850203));
#156807=CARTESIAN_POINT('',(24.9372684584991,7.5,59.2718640334));
#156808=CARTESIAN_POINT('',(24.9372684584991,7.5,59.2718640334));
#156809=CARTESIAN_POINT('Origin',(24.4068932609991,7.5,60.67496850203));
#156810=CARTESIAN_POINT('Origin',(24.4068932609991,7.5,60.67496850203));
#156811=CARTESIAN_POINT('Ctrl Pts',(24.9372684584991,7.5,59.2718640334));
#156812=CARTESIAN_POINT('Ctrl Pts',(24.7518004578403,7.41080923984522,59.2015326743088));
#156813=CARTESIAN_POINT('Ctrl Pts',(24.3332614377359,7.2243083185516,59.1195420885914));
#156814=CARTESIAN_POINT('Ctrl Pts',(23.7332150533881,6.91634501879556,59.184666298664));
#156815=CARTESIAN_POINT('Ctrl Pts',(23.2249783321078,6.57856080590289,59.3068783133604));
#156816=CARTESIAN_POINT('Ctrl Pts',(22.7661090603145,6.27051635511719,59.351451038476));
#156817=CARTESIAN_POINT('Ctrl Pts',(22.3007795484368,6.06002636053959,59.3141844993433));
#156818=CARTESIAN_POINT('Ctrl Pts',(21.9688150426247,6.00240938788309,59.2562553487836));
#156819=CARTESIAN_POINT('Ctrl Pts',(21.7988764270574,6.00000816827778,59.2227260005147));
#156820=CARTESIAN_POINT('Ctrl Pts',(21.7835206159544,6.00000000027008,59.2196611273475));
#156821=CARTESIAN_POINT('Ctrl Pts',(24.7500115337591,7.66199406857501,59.23234060116));
#156822=CARTESIAN_POINT('Ctrl Pts',(24.7219457315591,7.64878463429501,59.22687875267));
#156823=CARTESIAN_POINT('Ctrl Pts',(24.4990723215691,7.54413806281901,59.1895696092));
#156824=CARTESIAN_POINT('Ctrl Pts',(24.0530888920991,7.33541164648101,59.20365583005));
#156825=CARTESIAN_POINT('Ctrl Pts',(23.5121159558291,7.00326946263901,59.38501229628));
#156826=CARTESIAN_POINT('Ctrl Pts',(23.0769075317691,6.62914306930301,59.5703782362));
#156827=CARTESIAN_POINT('Ctrl Pts',(22.6625868082291,6.28134157023501,59.63701551399));
#156828=CARTESIAN_POINT('Ctrl Pts',(22.2127059182691,6.03754403224301,59.6034463707));
#156829=CARTESIAN_POINT('Ctrl Pts',(21.8319987041491,5.95311734543901,59.53436346757));
#156830=CARTESIAN_POINT('Ctrl Pts',(21.6116966555391,5.95211941027301,59.48764408243));
#156831=CARTESIAN_POINT('Ctrl Pts',(21.5492362715591,5.95568098179701,59.47401549141));
#156832=CARTESIAN_POINT('Ctrl Pts',(25.5892994869691,7.29739447716501,59.3149313448099));
#156833=CARTESIAN_POINT('Ctrl Pts',(25.5641282947991,7.28614135847301,59.2905997259801));
#156834=CARTESIAN_POINT('Ctrl Pts',(25.3587897698691,7.19811075061901,59.10313570938));
#156835=CARTESIAN_POINT('Ctrl Pts',(24.8658955918391,7.03575877646301,58.8143312375401));
#156836=CARTESIAN_POINT('Ctrl Pts',(24.1022737005091,6.80336022964301,58.67731108114));
#156837=CARTESIAN_POINT('Ctrl Pts',(23.4335704902791,6.56741369981001,58.71396001818));
#156838=CARTESIAN_POINT('Ctrl Pts',(22.8987579890791,6.36500644573902,58.74904311935));
#156839=CARTESIAN_POINT('Ctrl Pts',(22.4310250796891,6.23855144037001,58.73175649594));
#156840=CARTESIAN_POINT('Ctrl Pts',(22.0849984951291,6.21512134718301,58.6896704444001));
#156841=CARTESIAN_POINT('Ctrl Pts',(21.8954300117391,6.23523701677601,58.66055462542));
#156842=CARTESIAN_POINT('Ctrl Pts',(21.8424055925791,6.24366294458601,58.65200766024));
#156843=CARTESIAN_POINT('Ctrl Pts',(25.8652585171391,7.04901149428901,60.1553704558201));
#156844=CARTESIAN_POINT('Ctrl Pts',(25.8569176456691,7.03183869736401,60.12394526535));
#156845=CARTESIAN_POINT('Ctrl Pts',(25.7831098699891,6.89796515568501,59.8752379208801));
#156846=CARTESIAN_POINT('Ctrl Pts',(25.5178042067991,6.65664549376101,59.3916362179599));
#156847=CARTESIAN_POINT('Ctrl Pts',(24.8894971195291,6.32304071634601,58.8840204490601));
#156848=CARTESIAN_POINT('Ctrl Pts',(24.1659594138691,5.99743477030701,58.59018788242));
#156849=CARTESIAN_POINT('Ctrl Pts',(23.4809523308491,5.72763799024202,58.40125644434));
#156850=CARTESIAN_POINT('Ctrl Pts',(22.8338129039291,5.56848202078701,58.23167670162));
#156851=CARTESIAN_POINT('Ctrl Pts',(22.3405182440191,5.55291529651302,58.09949298367));
#156852=CARTESIAN_POINT('Ctrl Pts',(22.0685405930591,5.59234130224901,58.02647356417));
#156853=CARTESIAN_POINT('Ctrl Pts',(21.9923847081791,5.60744440708801,58.0059930655201));
#156854=CARTESIAN_POINT('Ctrl Pts',(25.2820011365291,7.18316514851801,60.8525262807));
#156855=CARTESIAN_POINT('Ctrl Pts',(25.2863805694791,7.15854384897201,60.83338955318));
#156856=CARTESIAN_POINT('Ctrl Pts',(25.3170701286091,6.96552196997101,60.6780164578));
#156857=CARTESIAN_POINT('Ctrl Pts',(25.3098283613891,6.60456285147501,60.31657555231));
#156858=CARTESIAN_POINT('Ctrl Pts',(25.0297132372791,6.07731684233201,59.78350345802));
#156859=CARTESIAN_POINT('Ctrl Pts',(24.4887957105791,5.53034639608301,59.33177220365));
#156860=CARTESIAN_POINT('Ctrl Pts',(23.7849321666091,5.05263239825701,58.96655767474));
#156861=CARTESIAN_POINT('Ctrl Pts',(22.9891941327791,4.74579444124201,58.6394001825));
#156862=CARTESIAN_POINT('Ctrl Pts',(22.3245857727091,4.67652663690701,58.3966283744));
#156863=CARTESIAN_POINT('Ctrl Pts',(21.9454165897491,4.71275487277101,58.26527229885));
#156864=CARTESIAN_POINT('Ctrl Pts',(21.8383637195091,4.72918860417001,58.22863842432));
#156865=CARTESIAN_POINT('',(22.0949867135254,5.00000000061885,58.2694348746444));
#156866=CARTESIAN_POINT('Origin',(21.7835175497024,5.00000436630195,59.219661344816));
#156867=CARTESIAN_POINT('Ctrl Pts',(24.9372684584988,7.5,59.2718640334007));
#156868=CARTESIAN_POINT('Ctrl Pts',(24.9253516994804,7.47196095686942,59.2673169679264));
#156869=CARTESIAN_POINT('Ctrl Pts',(24.9136646345482,7.4445580630566,59.2629539372089));
#156870=CARTESIAN_POINT('Ctrl Pts',(24.9021900367248,7.41778866776119,59.2586895691701));
#156871=CARTESIAN_POINT('Ctrl Pts',(24.8898555346574,7.38901317892088,59.2541056301773));
#156872=CARTESIAN_POINT('Ctrl Pts',(24.8777670910077,7.36096968773272,59.2496361489087));
#156873=CARTESIAN_POINT('Ctrl Pts',(24.8659212636497,7.33365634041001,59.2452332101466));
#156874=CARTESIAN_POINT('Ctrl Pts',(24.8521988171317,7.30201600524901,59.2401327566402));
#156875=CARTESIAN_POINT('Ctrl Pts',(24.8388023753174,7.27135540555908,59.2351219906611));
#156876=CARTESIAN_POINT('Ctrl Pts',(24.8257412534641,7.24167417214954,59.2301959155924));
#156877=CARTESIAN_POINT('Ctrl Pts',(24.8101088325862,7.20614969438692,59.2243000607328));
#156878=CARTESIAN_POINT('Ctrl Pts',(24.7949568863169,7.17202795111224,59.2185271755939));
#156879=CARTESIAN_POINT('Ctrl Pts',(24.7803146189784,7.13931403220985,59.2129454519303));
#156880=CARTESIAN_POINT('Ctrl Pts',(24.7723697943765,7.1215636154395,59.2099168352237));
#156881=CARTESIAN_POINT('Ctrl Pts',(24.7645752037018,7.10422779013506,59.2069455313005));
#156882=CARTESIAN_POINT('Ctrl Pts',(24.7569370338574,7.08730817988477,59.2040463791642));
#156883=CARTESIAN_POINT('Ctrl Pts',(24.7518865753216,7.07612071066732,59.2021294215747));
#156884=CARTESIAN_POINT('Ctrl Pts',(24.7468975324174,7.06511492467662,59.2002414188583));
#156885=CARTESIAN_POINT('Ctrl Pts',(24.7419698932784,7.05428965355225,59.198385949465));
#156886=CARTESIAN_POINT('Ctrl Pts',(24.7300658314657,7.0281382465658,59.1939035550105));
#156887=CARTESIAN_POINT('Ctrl Pts',(24.7185160453369,7.00304107430083,59.1896079543967));
#156888=CARTESIAN_POINT('Ctrl Pts',(24.7073185715577,6.97900228018697,59.1854630913426));
#156889=CARTESIAN_POINT('Ctrl Pts',(24.6987957386628,6.96070541883539,59.1823082748297));
#156890=CARTESIAN_POINT('Ctrl Pts',(24.690478341979,6.94302153654002,59.1792416995708));
#156891=CARTESIAN_POINT('Ctrl Pts',(24.6823809140436,6.92594895950459,59.1762593434168));
#156892=CARTESIAN_POINT('Ctrl Pts',(24.6708110196032,6.90155505125387,59.1719980463532));
#156893=CARTESIAN_POINT('Ctrl Pts',(24.6596761393446,6.87841074954737,59.1679030280241));
#156894=CARTESIAN_POINT('Ctrl Pts',(24.6489806389292,6.85651598717019,59.1639625160071));
#156895=CARTESIAN_POINT('Ctrl Pts',(24.6436328887215,6.84556860598159,59.1619922599987));
#156896=CARTESIAN_POINT('Ctrl Pts',(24.6383949110302,6.83493361143069,59.1600608277157));
#156897=CARTESIAN_POINT('Ctrl Pts',(24.6332669050915,6.82461100435038,59.1581676907911));
#156898=CARTESIAN_POINT('Ctrl Pts',(24.6287798998952,6.8155787231551,59.1565111959821));
#156899=CARTESIAN_POINT('Ctrl Pts',(24.6243770872641,6.80678561377664,59.1548840335607));
#156900=CARTESIAN_POINT('Ctrl Pts',(24.6200585030648,6.79823167905871,59.1532861139637));
#156901=CARTESIAN_POINT('Ctrl Pts',(24.6197500327649,6.79762068372172,59.1531719768496));
#156902=CARTESIAN_POINT('Ctrl Pts',(24.6196138894654,6.79735055225575,59.1531215980768));
#156903=CARTESIAN_POINT('Ctrl Pts',(24.6193922250548,6.79691181929018,59.153039569991));
#156904=CARTESIAN_POINT('Ctrl Pts',(24.6191705606442,6.79647308632462,59.1529575419053));
#156905=CARTESIAN_POINT('Ctrl Pts',(24.6188633732126,6.79586575187103,59.1528438697275));
#156906=CARTESIAN_POINT('Ctrl Pts',(24.6182128377217,6.79458035040017,59.1526030827148));
#156907=CARTESIAN_POINT('Ctrl Pts',(24.6006559350706,6.75988943990018,59.1461046299768));
#156908=CARTESIAN_POINT('Ctrl Pts',(24.5829534249965,6.72574806844182,59.1395180821526));
#156909=CARTESIAN_POINT('Ctrl Pts',(24.5650822275888,6.69215856035955,59.1328349464223));
#156910=CARTESIAN_POINT('Ctrl Pts',(24.544839586702,6.65411184562833,59.12526498267));
#156911=CARTESIAN_POINT('Ctrl Pts',(24.5243812689657,6.61677342010873,59.1175714587251));
#156912=CARTESIAN_POINT('Ctrl Pts',(24.5037116120574,6.58014158135225,59.1097967626435));
#156913=CARTESIAN_POINT('Ctrl Pts',(24.4993558779037,6.57242212321638,59.1081583944109));
#156914=CARTESIAN_POINT('Ctrl Pts',(24.4949908548014,6.56473401866839,59.1065165794007));
#156915=CARTESIAN_POINT('Ctrl Pts',(24.4906167188193,6.55707721049565,59.1048719438424));
#156916=CARTESIAN_POINT('Ctrl Pts',(24.488294111182,6.55301154787976,59.1039986643825));
#156917=CARTESIAN_POINT('Ctrl Pts',(24.4859668177808,6.54895257284586,59.1031237990105));
#156918=CARTESIAN_POINT('Ctrl Pts',(24.4836354773033,6.54490078716199,59.1022476768571));
#156919=CARTESIAN_POINT('Ctrl Pts',(24.4642483963475,6.5112067395404,59.0949619752285));
#156920=CARTESIAN_POINT('Ctrl Pts',(24.4445773061652,6.47800912513651,59.0875904676371));
#156921=CARTESIAN_POINT('Ctrl Pts',(24.424864717198,6.44562482280525,59.0802452601898));
#156922=CARTESIAN_POINT('Ctrl Pts',(24.404885950674,6.41280323775635,59.0728008709772));
#156923=CARTESIAN_POINT('Ctrl Pts',(24.3848644759225,6.38081776632692,59.0653826750114));
#156924=CARTESIAN_POINT('Ctrl Pts',(24.3651060732623,6.35000154898329,59.0581016556061));
#156925=CARTESIAN_POINT('Ctrl Pts',(24.3628410088866,6.34646883850564,59.0572669738781));
#156926=CARTESIAN_POINT('Ctrl Pts',(24.3605794578841,6.34295149096412,59.0564340963457));
#156927=CARTESIAN_POINT('Ctrl Pts',(24.3583219236067,6.33945000449852,59.0556031925104));
#156928=CARTESIAN_POINT('Ctrl Pts',(24.336463351073,6.30554686661361,59.0475579672679));
#156929=CARTESIAN_POINT('Ctrl Pts',(24.3148854527657,6.27303962476164,59.0396629899984));
#156930=CARTESIAN_POINT('Ctrl Pts',(24.2935940583983,6.2419284012883,59.0319025816968));
#156931=CARTESIAN_POINT('Ctrl Pts',(24.277926063446,6.21903415190628,59.026191821941));
#156932=CARTESIAN_POINT('Ctrl Pts',(24.2627879209375,6.1973325497693,59.0206898120325));
#156933=CARTESIAN_POINT('Ctrl Pts',(24.2469567428589,6.1753998533279,59.0149448797223));
#156934=CARTESIAN_POINT('Ctrl Pts',(24.2412747753946,6.16752799016243,59.0128829663063));
#156935=CARTESIAN_POINT('Ctrl Pts',(24.2355032201345,6.15962598219805,59.0107897117168));
#156936=CARTESIAN_POINT('Ctrl Pts',(24.2295843206351,6.15162695325244,59.00864394815));
#156937=CARTESIAN_POINT('Ctrl Pts',(24.2071740996707,6.12134091677101,59.0005196277975));
#156938=CARTESIAN_POINT('Ctrl Pts',(24.1828968779168,6.08994168903005,58.9917330499567));
#156939=CARTESIAN_POINT('Ctrl Pts',(24.1567590267025,6.05742911732951,58.9822668028042));
#156940=CARTESIAN_POINT('Ctrl Pts',(24.1436901010953,6.04117283147924,58.9775336792279));
#156941=CARTESIAN_POINT('Ctrl Pts',(24.130156099934,6.02463821158091,58.972630395889));
#156942=CARTESIAN_POINT('Ctrl Pts',(24.1161584234387,6.00782526850175,58.9675530536827));
#156943=CARTESIAN_POINT('Ctrl Pts',(24.1103120661753,6.00080306935884,58.9654324191263));
#156944=CARTESIAN_POINT('Ctrl Pts',(24.104384809627,5.9937323219517,58.9632813984112));
#156945=CARTESIAN_POINT('Ctrl Pts',(24.0983768322138,5.98661301932856,58.9610996566914));
#156946=CARTESIAN_POINT('Ctrl Pts',(24.0971924913651,5.98520960511256,58.960669574209));
#156947=CARTESIAN_POINT('Ctrl Pts',(24.0960050137735,5.98380430425258,58.9602382977778));
#156948=CARTESIAN_POINT('Ctrl Pts',(24.094814393207,5.98239711735019,58.9598058292043));
#156949=CARTESIAN_POINT('Ctrl Pts',(24.0875839391932,5.97385148957186,58.9571795146414));
#156950=CARTESIAN_POINT('Ctrl Pts',(24.0810046985963,5.96612892210129,58.9547881649664));
#156951=CARTESIAN_POINT('Ctrl Pts',(24.0727754155857,5.95655150857973,58.9517959464497));
#156952=CARTESIAN_POINT('Ctrl Pts',(24.0384277390557,5.91657695657942,58.939306917504));
#156953=CARTESIAN_POINT('Ctrl Pts',(24.0034683094554,5.87778350909651,58.9265815786641));
#156954=CARTESIAN_POINT('Ctrl Pts',(23.9678590006497,5.84020063332123,58.9136741411516));
#156955=CARTESIAN_POINT('Ctrl Pts',(23.9294267951761,5.79963840809059,58.8997434778712));
#156956=CARTESIAN_POINT('Ctrl Pts',(23.8902385500751,5.76048641392004,58.8856000807678));
#156957=CARTESIAN_POINT('Ctrl Pts',(23.8502859274976,5.7227525434125,58.8712677102395));
#156958=CARTESIAN_POINT('Ctrl Pts',(23.805405414728,5.68036445101941,58.8551675371591));
#156959=CARTESIAN_POINT('Ctrl Pts',(23.7595617687446,5.63976597255917,58.838828744871));
#156960=CARTESIAN_POINT('Ctrl Pts',(23.7127716509388,5.60093054367276,58.8222377212516));
#156961=CARTESIAN_POINT('Ctrl Pts',(23.6918644204073,5.58357770716384,58.8148243533903));
#156962=CARTESIAN_POINT('Ctrl Pts',(23.6707684261098,5.56657640531636,58.8073600585289));
#156963=CARTESIAN_POINT('Ctrl Pts',(23.6494854904257,5.54992230229696,58.7998410902845));
#156964=CARTESIAN_POINT('Ctrl Pts',(23.6176306075869,5.52499554837809,58.7885871986198));
#156965=CARTESIAN_POINT('Ctrl Pts',(23.5854221965799,5.50089571208605,58.7772340560176));
#156966=CARTESIAN_POINT('Ctrl Pts',(23.5528180096955,5.47760370730453,58.7657468526803));
#156967=CARTESIAN_POINT('Ctrl Pts',(23.5047337231853,5.44325292176636,58.7488056549614));
#156968=CARTESIAN_POINT('Ctrl Pts',(23.4557908853586,5.41065789155379,58.7315749653625));
#156969=CARTESIAN_POINT('Ctrl Pts',(23.4058589113385,5.37973126957867,58.7140549978679));
#156970=CARTESIAN_POINT('Ctrl Pts',(23.3581929283751,5.35020814606693,58.697330113893));
#156971=CARTESIAN_POINT('Ctrl Pts',(23.309625572927,5.32220461048141,58.6803409902794));
#156972=CARTESIAN_POINT('Ctrl Pts',(23.2600149371473,5.29566903861262,58.6630604713512));
#156973=CARTESIAN_POINT('Ctrl Pts',(23.2302353959441,5.27974065665587,58.6526875761576));
#156974=CARTESIAN_POINT('Ctrl Pts',(23.2000793893166,5.26434172998107,58.6422092103898));
#156975=CARTESIAN_POINT('Ctrl Pts',(23.1695109923222,5.24946749702519,58.6316155554101));
#156976=CARTESIAN_POINT('Ctrl Pts',(23.1022132391417,5.21672117871492,58.6082931293689));
#156977=CARTESIAN_POINT('Ctrl Pts',(23.0342782701488,5.18723041932582,58.5848858537487));
#156978=CARTESIAN_POINT('Ctrl Pts',(22.9657107575351,5.16098338851324,58.5613832671255));
#156979=CARTESIAN_POINT('Ctrl Pts',(22.9395452804977,5.15096747783124,58.5524146409181));
#156980=CARTESIAN_POINT('Ctrl Pts',(22.9132873831954,5.14142404593434,58.54343172089));
#156981=CARTESIAN_POINT('Ctrl Pts',(22.8869360879741,5.13235319318208,58.534432507506));
#156982=CARTESIAN_POINT('Ctrl Pts',(22.8235569648741,5.11053632655834,58.512787945139));
#156983=CARTESIAN_POINT('Ctrl Pts',(22.7596400356896,5.09145100616448,58.4910506913766));
#156984=CARTESIAN_POINT('Ctrl Pts',(22.6952160503029,5.07504879209382,58.4692514386328));
#156985=CARTESIAN_POINT('Ctrl Pts',(22.6317741779036,5.05889662196822,58.4477845051194));
#156986=CARTESIAN_POINT('Ctrl Pts',(22.567840169145,5.04534570398895,58.4262570374071));
#156987=CARTESIAN_POINT('Ctrl Pts',(22.5034140292658,5.03438543356313,58.4046801529297));
#156988=CARTESIAN_POINT('Ctrl Pts',(22.4413570922322,5.02382821543768,58.3838967354549));
#156989=CARTESIAN_POINT('Ctrl Pts',(22.3788430671832,5.01567419676257,58.3630671436673));
#156990=CARTESIAN_POINT('Ctrl Pts',(22.3158512579248,5.00995481363774,58.3421896471645));
#156991=CARTESIAN_POINT('Ctrl Pts',(22.2669243643649,5.00551246386765,58.3259737127245));
#156992=CARTESIAN_POINT('Ctrl Pts',(22.2177087606478,5.00253960528567,58.3097286249063));
#156993=CARTESIAN_POINT('Ctrl Pts',(22.1681884154333,5.00107157112627,58.2934501084065));
#156994=CARTESIAN_POINT('Ctrl Pts',(22.1438610190086,5.00035038372731,58.2854531139918));
#156995=CARTESIAN_POINT('Ctrl Pts',(22.119459997522,4.99999267677634,58.277448008364));
#156996=CARTESIAN_POINT('Ctrl Pts',(22.0949867135254,5.00000000061885,58.2694348746444));
#156997=CARTESIAN_POINT('Origin',(1.07038457110909,25.,122.41156512159));
#156998=CARTESIAN_POINT('',(24.9372684584991,-7.5,59.2718640334));
#156999=CARTESIAN_POINT('',(24.9372723528391,-10.33198914208,59.2718657798));
#157000=CARTESIAN_POINT('Origin',(1.07038457110909,5.,122.41156512159));
#157001=CARTESIAN_POINT('Ctrl Pts',(22.0949841886482,-5.00000000380661,
58.2694426477661));
#157002=CARTESIAN_POINT('Ctrl Pts',(22.2805552764597,-4.99991534493558,
58.3302356171032));
#157003=CARTESIAN_POINT('Ctrl Pts',(22.5537696623475,-5.03100736632704,
58.4211274743539));
#157004=CARTESIAN_POINT('Ctrl Pts',(22.863600077902,-5.12191465893277,58.5263497471087));
#157005=CARTESIAN_POINT('Ctrl Pts',(22.9944789641351,-5.17258205687998,
58.5712471933459));
#157006=CARTESIAN_POINT('Ctrl Pts',(23.0813087371768,-5.20896190642875,
58.6011323892443));
#157007=CARTESIAN_POINT('Ctrl Pts',(23.1258275312192,-5.22908872234276,
58.6165074658168));
#157008=CARTESIAN_POINT('Ctrl Pts',(23.3342129069009,-5.32986577239622,
58.6887036403607));
#157009=CARTESIAN_POINT('Ctrl Pts',(23.4918466779593,-5.42782596721495,
58.7440466636716));
#157010=CARTESIAN_POINT('Ctrl Pts',(23.7147825492157,-5.60077409160701,
58.8231427665048));
#157011=CARTESIAN_POINT('Ctrl Pts',(23.822871677724,-5.69375011184404,58.8617117509264));
#157012=CARTESIAN_POINT('Ctrl Pts',(23.9430827095938,-5.81360056202562,
58.9049361286198));
#157013=CARTESIAN_POINT('Ctrl Pts',(24.0059055719926,-5.8808539531689,58.9276096919623));
#157014=CARTESIAN_POINT('Ctrl Pts',(24.0347942568544,-5.91306854597329,
58.9380583730788));
#157015=CARTESIAN_POINT('Ctrl Pts',(24.0511971638391,-5.93168007090743,
58.943996461702));
#157016=CARTESIAN_POINT('Ctrl Pts',(24.0562159179984,-5.93741363096873,
58.9458139752985));
#157017=CARTESIAN_POINT('Ctrl Pts',(24.1603795204009,-6.05697259641673,
58.9835454900929));
#157018=CARTESIAN_POINT('Ctrl Pts',(24.3053416434733,-6.24925311691998,
59.0364640156985));
#157019=CARTESIAN_POINT('Ctrl Pts',(24.4630575940089,-6.50573938967163,
59.0946110881264));
#157020=CARTESIAN_POINT('Ctrl Pts',(24.539070211985,-6.64202227575524,59.1227690617259));
#157021=CARTESIAN_POINT('Ctrl Pts',(24.5803619250404,-6.71968987555994,
59.1381006869307));
#157022=CARTESIAN_POINT('Ctrl Pts',(24.6001039998996,-6.75794394236028,
59.1454414917671));
#157023=CARTESIAN_POINT('Ctrl Pts',(24.610573951587,-6.77851360610602,59.1493371661886));
#157024=CARTESIAN_POINT('Ctrl Pts',(24.6125710338916,-6.78244756197933,
59.1500803383087));
#157025=CARTESIAN_POINT('Ctrl Pts',(24.6921945641985,-6.93949641873107,
59.1797123957439));
#157026=CARTESIAN_POINT('Ctrl Pts',(24.8002777276957,-7.1782747537386,59.2200813703637));
#157027=CARTESIAN_POINT('Ctrl Pts',(24.9372684584991,-7.5,59.2718640334));
#157028=CARTESIAN_POINT('Origin',(-6.80729512863291,91.08441266238,84.10819367738));
#157029=CARTESIAN_POINT('Origin',(-6.80729512863291,5.,84.10819367738));
#157030=CARTESIAN_POINT('Origin',(-6.80729512863291,-5.,84.10819367738));
#157031=CARTESIAN_POINT('Ctrl Pts',(-6.54682286213226,-4.99999999999969,
85.5854053069007));
#157032=CARTESIAN_POINT('Ctrl Pts',(-7.83114436700245,-5.0000000000004,
85.8118658401104));
#157033=CARTESIAN_POINT('Ctrl Pts',(-8.23395173884804,-4.9999999999997,
84.5714980228237));
#157034=CARTESIAN_POINT('Ctrl Pts',(-6.54682286213212,-5.41421633819426,
85.5854053069002));
#157035=CARTESIAN_POINT('Ctrl Pts',(-7.83114436700212,-5.41421633819497,
85.8118658401099));
#157036=CARTESIAN_POINT('Ctrl Pts',(-8.23395173884766,-5.41421633819427,
84.5714980228234));
#157037=CARTESIAN_POINT('Ctrl Pts',(-6.59768381767522,-5.7071101318881,
85.2969584943955));
#157038=CARTESIAN_POINT('Ctrl Pts',(-7.63122308057704,-5.70711013188867,
85.4791993520641));
#157039=CARTESIAN_POINT('Ctrl Pts',(-7.95537652082547,-5.70711013188811,
84.4810311872048));
#157040=CARTESIAN_POINT('Ctrl Pts',(-6.64854477321832,-6.00000392558194,
85.0085116818906));
#157041=CARTESIAN_POINT('Ctrl Pts',(-7.43130179415197,-6.00000392558238,
85.1465328640184));
#157042=CARTESIAN_POINT('Ctrl Pts',(-7.6768013028033,-6.00000392558195,
84.3905643515862));
#157043=CARTESIAN_POINT('Ctrl Pts',(-6.72047268550151,-5.99999999995607,
84.6005882206304));
#157044=CARTESIAN_POINT('Ctrl Pts',(-7.14857173924192,-5.99999999995631,
84.6760736342196));
#157045=CARTESIAN_POINT('Ctrl Pts',(-7.28283831818874,-5.99999999995607,
84.2626255319672));
#157046=CARTESIAN_POINT('Origin',(24.8472308208791,-7.5,80.448558349262));
#157047=CARTESIAN_POINT('Origin',(22.174314171959,-7.5,65.2896947528857));
#157048=CARTESIAN_POINT('Origin',(21.4524700019691,-7.5,61.19591303503));
#157049=CARTESIAN_POINT('Origin',(24.4068932609991,-7.5,60.67496850203));
#157050=CARTESIAN_POINT('Origin',(24.4068932609991,-7.5,60.67496850203));
#157051=CARTESIAN_POINT('Ctrl Pts',(21.7837557160991,-6.00001782727999,
59.21971079975));
#157052=CARTESIAN_POINT('Ctrl Pts',(22.0097728635713,-5.99997040176646,
59.2647219220221));
#157053=CARTESIAN_POINT('Ctrl Pts',(22.2385800253108,-6.04902617145881,
59.3042918067695));
#157054=CARTESIAN_POINT('Ctrl Pts',(22.6838933356787,-6.22980259915816,
59.3443479086447));
#157055=CARTESIAN_POINT('Ctrl Pts',(22.8999827744699,-6.3613180310625,59.3431175932148));
#157056=CARTESIAN_POINT('Ctrl Pts',(23.2438698401328,-6.59046668870961,
59.2922250056415));
#157057=CARTESIAN_POINT('Ctrl Pts',(23.362960063642,-6.67191371077529,59.2687253818218));
#157058=CARTESIAN_POINT('Ctrl Pts',(23.6232995629752,-6.83820229845214,
59.2174361530951));
#157059=CARTESIAN_POINT('Ctrl Pts',(23.7656062250204,-6.92283887189394,
59.1882921399419));
#157060=CARTESIAN_POINT('Ctrl Pts',(24.0739220072904,-7.09103974838947,
59.1494728679439));
#157061=CARTESIAN_POINT('Ctrl Pts',(24.2406714479517,-7.17440448969987,
59.1407005872925));
#157062=CARTESIAN_POINT('Ctrl Pts',(24.5896694075326,-7.33775746185597,
59.1698506720171));
#157063=CARTESIAN_POINT('Ctrl Pts',(24.7695305019998,-7.41833718706608,
59.2065810098722));
#157064=CARTESIAN_POINT('Ctrl Pts',(24.9372684584991,-7.5,59.2718640334));
#157065=CARTESIAN_POINT('Ctrl Pts',(21.5482687433291,-5.95510217575499,
59.47577881262));
#157066=CARTESIAN_POINT('Ctrl Pts',(21.6385071826491,-5.94997535511398,
59.49548084013));
#157067=CARTESIAN_POINT('Ctrl Pts',(21.9131048476991,-5.95866966306399,
59.55304861875));
#157068=CARTESIAN_POINT('Ctrl Pts',(22.3692704752191,-6.096989384513,59.62812563708));
#157069=CARTESIAN_POINT('Ctrl Pts',(22.8683422761291,-6.43730726581498,
59.62980972532));
#157070=CARTESIAN_POINT('Ctrl Pts',(23.3387245707791,-6.87259544505199,
59.46695082988));
#157071=CARTESIAN_POINT('Ctrl Pts',(23.9310250958291,-7.279114747789,59.2220355884));
#157072=CARTESIAN_POINT('Ctrl Pts',(24.4618176914991,-7.52767454181498,
59.18139023564));
#157073=CARTESIAN_POINT('Ctrl Pts',(24.7197883064391,-7.649504286858,59.22728137109));
#157074=CARTESIAN_POINT('Ctrl Pts',(24.7477189671291,-7.66272970212499,
59.23310715875));
#157075=CARTESIAN_POINT('Ctrl Pts',(21.8418959298291,-6.24534546095398,
58.65317069173));
#157076=CARTESIAN_POINT('Ctrl Pts',(21.9183808576391,-6.23320434561899,
58.66549890254));
#157077=CARTESIAN_POINT('Ctrl Pts',(22.1557327029891,-6.21340282184399,
58.70105855136));
#157078=CARTESIAN_POINT('Ctrl Pts',(22.5805331464491,-6.26715359928599,
58.7456295618));
#157079=CARTESIAN_POINT('Ctrl Pts',(23.1393556500491,-6.45444111416999,
58.74233013357));
#157080=CARTESIAN_POINT('Ctrl Pts',(23.8323620899991,-6.71775933814998,
58.67382657826));
#157081=CARTESIAN_POINT('Ctrl Pts',(24.7190342437791,-6.99392094430899,
58.74842003095));
#157082=CARTESIAN_POINT('Ctrl Pts',(25.3277236543091,-7.18300713584699,
59.06935222318));
#157083=CARTESIAN_POINT('Ctrl Pts',(25.5632336614691,-7.28727303124799,
59.28910840377));
#157084=CARTESIAN_POINT('Ctrl Pts',(25.5879717422591,-7.29878131891499,
59.31371561786));
#157085=CARTESIAN_POINT('Ctrl Pts',(21.9922347994691,-5.60881868005499,
58.00554653487));
#157086=CARTESIAN_POINT('Ctrl Pts',(22.1021455439091,-5.58702360762799,
58.03513218664));
#157087=CARTESIAN_POINT('Ctrl Pts',(22.4427011606791,-5.54540958548999,
58.12636252562));
#157088=CARTESIAN_POINT('Ctrl Pts',(23.0461698531791,-5.600768961777,58.28727323461));
#157089=CARTESIAN_POINT('Ctrl Pts',(23.8041883710391,-5.84404758049099,
58.48483376287));
#157090=CARTESIAN_POINT('Ctrl Pts',(24.6291238424591,-6.20144908664698,
58.74340456943));
#157091=CARTESIAN_POINT('Ctrl Pts',(25.4282103275791,-6.59406976343999,
59.26219347932));
#157092=CARTESIAN_POINT('Ctrl Pts',(25.7747832871991,-6.87348915556999,
59.8344135724));
#157093=CARTESIAN_POINT('Ctrl Pts',(25.8574257339091,-7.03298482887899,
60.12294471837));
#157094=CARTESIAN_POINT('Ctrl Pts',(25.8653237391391,-7.05066785691398,
60.1543045333201));
#157095=CARTESIAN_POINT('Ctrl Pts',(21.8377989953191,-4.72924648248199,
58.22855122752));
#157096=CARTESIAN_POINT('Ctrl Pts',(21.9924105746991,-4.70552757959199,
58.2814885137601));
#157097=CARTESIAN_POINT('Ctrl Pts',(22.4657633189691,-4.67221426727299,
58.44626974282));
#157098=CARTESIAN_POINT('Ctrl Pts',(23.2660173601391,-4.81363191030199,
58.74539967786));
#157099=CARTESIAN_POINT('Ctrl Pts',(24.1487109904791,-5.26178031101699,
59.1339101002101));
#157100=CARTESIAN_POINT('Ctrl Pts',(24.8731689331391,-5.87825886677599,
59.60094766893));
#157101=CARTESIAN_POINT('Ctrl Pts',(25.2967925166891,-6.509060979056,60.211486662));
#157102=CARTESIAN_POINT('Ctrl Pts',(25.3227879014891,-6.93158905149599,
60.65478434692));
#157103=CARTESIAN_POINT('Ctrl Pts',(25.2863583828791,-7.15978311571299,
60.83312581344));
#157104=CARTESIAN_POINT('Ctrl Pts',(25.2818575683891,-7.18490016046499,
60.85195610375));
#157105=CARTESIAN_POINT('Origin',(24.4068932609991,-15.54362135317,60.67496850203));
#157106=CARTESIAN_POINT('Ctrl Pts',(-6.72047268773407,5.99999999995523,
84.6005882079846));
#157107=CARTESIAN_POINT('Ctrl Pts',(-7.14857173047982,5.99999999995525,
84.6760736196361));
#157108=CARTESIAN_POINT('Ctrl Pts',(-7.28283830597694,5.99999999995523,
84.2626255280015));
#157109=CARTESIAN_POINT('Ctrl Pts',(-6.64854477479676,6.00000393090208,
85.0085116729493));
#157110=CARTESIAN_POINT('Ctrl Pts',(-7.43130178795857,6.00000393090212,
85.1465328537084));
#157111=CARTESIAN_POINT('Ctrl Pts',(-7.67680129416981,6.00000393090208,
84.390564348781));
#157112=CARTESIAN_POINT('Ctrl Pts',(-6.59768381846433,5.70711013642924,
85.296958489926));
#157113=CARTESIAN_POINT('Ctrl Pts',(-7.63122307748394,5.70711013642929,
85.4791993469125));
#157114=CARTESIAN_POINT('Ctrl Pts',(-7.95537651651139,5.70711013642924,
84.4810311858011));
#157115=CARTESIAN_POINT('Ctrl Pts',(-6.54682286213189,5.4142163419564,85.5854053069028));
#157116=CARTESIAN_POINT('Ctrl Pts',(-7.83114436700931,5.41421634195645,
85.8118658401166));
#157117=CARTESIAN_POINT('Ctrl Pts',(-8.23395173885296,5.4142163419564,84.5714980228211));
#157118=CARTESIAN_POINT('Ctrl Pts',(-6.54682286213193,4.99999999999998,
85.5854053069027));
#157119=CARTESIAN_POINT('Ctrl Pts',(-7.83114436700921,5.00000000000003,
85.8118658401165));
#157120=CARTESIAN_POINT('Ctrl Pts',(-8.23395173885283,4.99999999999998,
84.5714980228211));
#157121=CARTESIAN_POINT('Origin',(-7.28284733203891,5.,84.2626284592));
#157122=CARTESIAN_POINT('Origin',(27.4324635166691,5.,72.98888938658));
#157123=CARTESIAN_POINT('Origin',(1.07038457110909,5.,122.41156512159));
#157124=CARTESIAN_POINT('Origin',(23.9011399714191,10.33198915989,57.80669906563));
#157125=CARTESIAN_POINT('Origin',(24.4127075916591,10.33198621001,60.7079432098));
#157126=CARTESIAN_POINT('Ctrl Pts',(25.7146057871591,10.98822408556,60.32011578917));
#157127=CARTESIAN_POINT('Ctrl Pts',(25.7333595485691,10.98640264379,60.42647365532));
#157128=CARTESIAN_POINT('Ctrl Pts',(25.7902717155191,10.98675745301,60.74923859301));
#157129=CARTESIAN_POINT('Ctrl Pts',(25.8903004917691,11.01610949404,61.31652997325));
#157130=CARTESIAN_POINT('Ctrl Pts',(26.0187410371091,11.09765362491,62.0449525029099));
#157131=CARTESIAN_POINT('Ctrl Pts',(26.1595638381891,11.23024105092,62.84359829445));
#157132=CARTESIAN_POINT('Ctrl Pts',(26.3108478437791,11.41227085738,63.701572524988));
#157133=CARTESIAN_POINT('Ctrl Pts',(26.4698526384791,11.63683182579,64.603333526392));
#157134=CARTESIAN_POINT('Ctrl Pts',(26.6325918522091,11.8932379924,65.526273470543));
#157135=CARTESIAN_POINT('Ctrl Pts',(26.7914529063091,12.16230532054,66.4272192784869));
#157136=CARTESIAN_POINT('Ctrl Pts',(26.9386924978091,12.42231805601,67.26225649691));
#157137=CARTESIAN_POINT('Ctrl Pts',(27.0699044264391,12.65926655649,68.006396322292));
#157138=CARTESIAN_POINT('Ctrl Pts',(27.1862753385091,12.87066869904,68.666368560249));
#157139=CARTESIAN_POINT('Ctrl Pts',(27.2910527846991,13.06027210397,69.260590985898));
#157140=CARTESIAN_POINT('Ctrl Pts',(27.3865217178491,13.23082661369,69.802022210807));
#157141=CARTESIAN_POINT('Ctrl Pts',(27.4739349518891,13.38351975338,70.297767295838));
#157142=CARTESIAN_POINT('Ctrl Pts',(27.5540499498591,13.51934191737,70.7521220272789));
#157143=CARTESIAN_POINT('Ctrl Pts',(27.6273676469791,13.63888432267,71.167927350015));
#157144=CARTESIAN_POINT('Ctrl Pts',(27.6946527386791,13.74332636095,71.549520067312));
#157145=CARTESIAN_POINT('Ctrl Pts',(27.7566735256291,13.8340404781,71.901257428796));
#157146=CARTESIAN_POINT('Ctrl Pts',(27.8139535058191,13.91189665278,72.2261083390753));
#157147=CARTESIAN_POINT('Ctrl Pts',(27.8668525364891,13.97757339522,72.5261136499739));
#157148=CARTESIAN_POINT('Ctrl Pts',(27.9156547649191,14.03175427646,72.8028848408233));
#157149=CARTESIAN_POINT('Ctrl Pts',(27.9606578091391,14.07512867792,73.0581097873241));
#157150=CARTESIAN_POINT('Ctrl Pts',(28.0020959597691,14.10837762916,73.2931172176315));
#157151=CARTESIAN_POINT('Ctrl Pts',(28.0400945627891,14.132263698,73.5086180041178));
#157152=CARTESIAN_POINT('Ctrl Pts',(28.0747458485391,14.14767670304,73.7051352110367));
#157153=CARTESIAN_POINT('Ctrl Pts',(28.1061814400091,14.15583570334,73.8834153093887));
#157154=CARTESIAN_POINT('Ctrl Pts',(28.1346527710791,14.15817719874,74.0448842516899));
#157155=CARTESIAN_POINT('Ctrl Pts',(28.1589709875791,14.15615234085,74.182799710788));
#157156=CARTESIAN_POINT('Ctrl Pts',(28.1738163949191,14.1529441735,74.266992199549));
#157157=CARTESIAN_POINT('Ctrl Pts',(28.1801055443791,14.15123724658,74.302659738554));
#157158=CARTESIAN_POINT('Ctrl Pts',(24.6968047233291,13.13053120709,60.53629255394));
#157159=CARTESIAN_POINT('Ctrl Pts',(24.7110977510391,13.12914347929,60.61735234215));
#157160=CARTESIAN_POINT('Ctrl Pts',(24.7550666420191,13.12935201228,60.86671231419));
#157161=CARTESIAN_POINT('Ctrl Pts',(24.8353614835591,13.15257479162,61.32208698922));
#157162=CARTESIAN_POINT('Ctrl Pts',(24.9432706425091,13.22070256323,61.93407024056));
#157163=CARTESIAN_POINT('Ctrl Pts',(25.0665147321391,13.33640433196,62.63302220545));
#157164=CARTESIAN_POINT('Ctrl Pts',(25.2036262415691,13.50112442483,63.410620216152));
#157165=CARTESIAN_POINT('Ctrl Pts',(25.3518667357391,13.7103233706,64.251333835632));
#157166=CARTESIAN_POINT('Ctrl Pts',(25.5064342999091,13.95375958956,65.127930052254));
#157167=CARTESIAN_POINT('Ctrl Pts',(25.6600936118891,14.21395978547,65.9993753146631));
#157168=CARTESIAN_POINT('Ctrl Pts',(25.8041861213491,14.46839546703,66.816564543937));
#157169=CARTESIAN_POINT('Ctrl Pts',(25.9339809461091,14.7027763825,67.55266757384));
#157170=CARTESIAN_POINT('Ctrl Pts',(26.0503244280891,14.91412817094,68.212484248023));
#157171=CARTESIAN_POINT('Ctrl Pts',(26.1558873440491,15.10515684937,68.811161294153));
#157172=CARTESIAN_POINT('Ctrl Pts',(26.2531435947691,15.27891270155,69.362728900733));
#157173=CARTESIAN_POINT('Ctrl Pts',(26.3431374759891,15.43612444966,69.873109563156));
#157174=CARTESIAN_POINT('Ctrl Pts',(26.4265245286691,15.57750958702,70.3460210390141));
#157175=CARTESIAN_POINT('Ctrl Pts',(26.5039740022191,15.70380916865,70.7852588302931));
#157176=CARTESIAN_POINT('Ctrl Pts',(26.5761186635391,15.81581819599,71.194411536424));
#157177=CARTESIAN_POINT('Ctrl Pts',(26.6437790448791,15.91481279583,71.578132627044));
#157178=CARTESIAN_POINT('Ctrl Pts',(26.7076333815191,16.00164468556,71.940268565508));
#157179=CARTESIAN_POINT('Ctrl Pts',(26.7680135964591,16.07665708509,72.2827017807608));
#157180=CARTESIAN_POINT('Ctrl Pts',(26.8252747392791,16.14028901932,72.607445859035));
#157181=CARTESIAN_POINT('Ctrl Pts',(26.8798137168691,16.19292482343,72.9167517710934));
#157182=CARTESIAN_POINT('Ctrl Pts',(26.9317722155091,16.23468871587,73.2114230597839));
#157183=CARTESIAN_POINT('Ctrl Pts',(26.9811069681591,16.26578384666,73.4912143455473));
#157184=CARTESIAN_POINT('Ctrl Pts',(27.0277124764791,16.28657491746,73.7555273176114));
#157185=CARTESIAN_POINT('Ctrl Pts',(27.0708769258191,16.29781123553,74.000325074377));
#157186=CARTESIAN_POINT('Ctrl Pts',(27.1105081190591,16.3010840103,74.225084740104));
#157187=CARTESIAN_POINT('Ctrl Pts',(27.1444134164591,16.29825389057,74.417371236858));
#157188=CARTESIAN_POINT('Ctrl Pts',(27.1648328335891,16.2938285752,74.5331755059949));
#157189=CARTESIAN_POINT('Ctrl Pts',(27.1733925807291,16.29148605459,74.581720244281));
#157190=CARTESIAN_POINT('Ctrl Pts',(22.4731286993091,12.36649813187,60.9152940194));
#157191=CARTESIAN_POINT('Ctrl Pts',(22.4890126044691,12.36495572419,61.00537612196));
#157192=CARTESIAN_POINT('Ctrl Pts',(22.5375975893991,12.36521642518,61.2809152636801));
#157193=CARTESIAN_POINT('Ctrl Pts',(22.6249303475291,12.39062514631,61.7762039471101));
#157194=CARTESIAN_POINT('Ctrl Pts',(22.7401618264791,12.46353773244,62.42971413873));
#157195=CARTESIAN_POINT('Ctrl Pts',(22.8696751931991,12.58526160721,63.1642209408299));
#157196=CARTESIAN_POINT('Ctrl Pts',(23.0118411860591,12.7561550417,63.970484351462));
#157197=CARTESIAN_POINT('Ctrl Pts',(23.1639206636991,12.97083270398,64.8329699281351));
#157198=CARTESIAN_POINT('Ctrl Pts',(23.3214025674991,13.21889452908,65.726094186094));
#157199=CARTESIAN_POINT('Ctrl Pts',(23.4769170303891,13.48225710178,66.608060532198));
#157200=CARTESIAN_POINT('Ctrl Pts',(23.6221319161691,13.73868178557,67.431615073849));
#157201=CARTESIAN_POINT('Ctrl Pts',(23.7524321372891,13.97397840535,68.17058434898));
#157202=CARTESIAN_POINT('Ctrl Pts',(23.8687854019491,14.1853481521,68.830456503476));
#157203=CARTESIAN_POINT('Ctrl Pts',(23.9740681877291,14.37586852055,69.427544852378));
#157204=CARTESIAN_POINT('Ctrl Pts',(24.0706870089591,14.54848264496,69.9754974166599));
#157205=CARTESIAN_POINT('Ctrl Pts',(24.1597605273691,14.70408287517,70.48065844223));
#157206=CARTESIAN_POINT('Ctrl Pts',(24.2419806334391,14.84348403198,70.946951835013));
#157207=CARTESIAN_POINT('Ctrl Pts',(24.3179565489691,14.96737373215,71.3778326634539));
#157208=CARTESIAN_POINT('Ctrl Pts',(24.3883680918691,15.07668406617,71.7771563666341));
#157209=CARTESIAN_POINT('Ctrl Pts',(24.4540171665291,15.17272551209,72.1494707701902));
#157210=CARTESIAN_POINT('Ctrl Pts',(24.5155268226391,15.25635630003,72.4983093646567));
#157211=CARTESIAN_POINT('Ctrl Pts',(24.5732389457091,15.32803922793,72.825611078962));
#157212=CARTESIAN_POINT('Ctrl Pts',(24.6274832986791,15.38830053569,73.1332460918097));
#157213=CARTESIAN_POINT('Ctrl Pts',(24.6786213780391,15.4376333503,73.4232645515648));
#157214=CARTESIAN_POINT('Ctrl Pts',(24.7268278965091,15.47636047147,73.6966573033259));
#157215=CARTESIAN_POINT('Ctrl Pts',(24.7721197212391,15.50488456017,73.9535200055188));
#157216=CARTESIAN_POINT('Ctrl Pts',(24.8144618719291,15.52375759594,74.193654274908));
#157217=CARTESIAN_POINT('Ctrl Pts',(24.8534433377591,15.53389641844,74.414729153379));
#157218=CARTESIAN_POINT('Ctrl Pts',(24.8890944742991,15.53683706144,74.616916795904));
#157219=CARTESIAN_POINT('Ctrl Pts',(24.9195806321991,15.53429413055,74.7898123889521));
#157220=CARTESIAN_POINT('Ctrl Pts',(24.9380121327491,15.53030289923,74.894342622946));
#157221=CARTESIAN_POINT('Ctrl Pts',(24.9457620932291,15.52818705695,74.938294832893));
#157222=CARTESIAN_POINT('Ctrl Pts',(22.9354926719291,10.03334832269,60.79378548384));
#157223=CARTESIAN_POINT('Ctrl Pts',(22.9562346853791,10.03133356459,60.91141928763));
#157224=CARTESIAN_POINT('Ctrl Pts',(23.0189159693591,10.0317535725,61.26690251386));
#157225=CARTESIAN_POINT('Ctrl Pts',(23.1277406160991,10.06383756704,61.88407775444));
#157226=CARTESIAN_POINT('Ctrl Pts',(23.2653324745291,10.15136167908,62.6643999597399));
#157227=CARTESIAN_POINT('Ctrl Pts',(23.4139905132991,10.29147543254,63.507481592353));
#157228=CARTESIAN_POINT('Ctrl Pts',(23.5715915277691,10.48122057813,64.401281360441));
#157229=CARTESIAN_POINT('Ctrl Pts',(23.7353942198291,10.71262875484,65.330252589921));
#157230=CARTESIAN_POINT('Ctrl Pts',(23.9017757264891,10.97481592666,66.2738490037879));
#157231=CARTESIAN_POINT('Ctrl Pts',(24.0629553171891,11.24783554043,67.187943886222));
#157232=CARTESIAN_POINT('Ctrl Pts',(24.2115976358491,11.51033409764,68.0309363656259));
#157233=CARTESIAN_POINT('Ctrl Pts',(24.3434412004091,11.74842703006,68.778658376371));
#157234=CARTESIAN_POINT('Ctrl Pts',(24.4598243387091,11.9598516166,69.438699952696));
#157235=CARTESIAN_POINT('Ctrl Pts',(24.5642516828691,12.14881974422,70.030936851112));
#157236=CARTESIAN_POINT('Ctrl Pts',(24.6589239672891,12.31794734167,70.5678500566009));
#157237=CARTESIAN_POINT('Ctrl Pts',(24.7451869472891,12.46862643321,71.057071726764));
#157238=CARTESIAN_POINT('Ctrl Pts',(24.8238435148991,12.60196905149,71.5031552886309));
#157239=CARTESIAN_POINT('Ctrl Pts',(24.8953195838391,12.71849962724,71.90851621894));
#157240=CARTESIAN_POINT('Ctrl Pts',(24.9604386531191,12.81956888374,72.2778248126876));
#157241=CARTESIAN_POINT('Ctrl Pts',(25.0199457425991,12.90659219849,72.6153062873973));
#157242=CARTESIAN_POINT('Ctrl Pts',(25.0742953802791,12.98044768968,72.923538399479));
#157243=CARTESIAN_POINT('Ctrl Pts',(25.1238598743391,13.04196331413,73.2046326134905));
#157244=CARTESIAN_POINT('Ctrl Pts',(25.1688917692491,13.09193164278,73.4600211804315));
#157245=CARTESIAN_POINT('Ctrl Pts',(25.2096444277191,13.13117802317,73.6911409915274));
#157246=CARTESIAN_POINT('Ctrl Pts',(25.2463934162691,13.16063166845,73.8995548621547));
#157247=CARTESIAN_POINT('Ctrl Pts',(25.2793392355791,13.18130449189,74.086399888258));
#157248=CARTESIAN_POINT('Ctrl Pts',(25.3086622482391,13.19432036881,74.252698956838));
#157249=CARTESIAN_POINT('Ctrl Pts',(25.3348700168591,13.20110773749,74.4013305985409));
#157250=CARTESIAN_POINT('Ctrl Pts',(25.3583671396191,13.20303414017,74.534589403646));
#157251=CARTESIAN_POINT('Ctrl Pts',(25.3784121727291,13.20136820609,74.6482704355061));
#157252=CARTESIAN_POINT('Ctrl Pts',(25.3907731151691,13.19870254972,74.7183728236471));
#157253=CARTESIAN_POINT('Ctrl Pts',(25.3960502068091,13.19727892159,74.748300697519));
#157254=CARTESIAN_POINT('',(26.0143554277394,12.1868334151086,64.6125968688177));
#157255=CARTESIAN_POINT('Ctrl Pts',(25.5858158203339,11.2436003008624,60.5011154491916));
#157256=CARTESIAN_POINT('Ctrl Pts',(25.5923235730551,11.2475657971982,60.5554809329124));
#157257=CARTESIAN_POINT('Ctrl Pts',(25.5988047894408,11.2520203456228,60.6098721686439));
#157258=CARTESIAN_POINT('Ctrl Pts',(25.605257698237,11.256943112575,60.6642809059383));
#157259=CARTESIAN_POINT('Ctrl Pts',(25.628778699609,11.2748867116392,60.8626020080901));
#157260=CARTESIAN_POINT('Ctrl Pts',(25.6519238690939,11.2990477224041,61.0611576275081));
#157261=CARTESIAN_POINT('Ctrl Pts',(25.6746441124549,11.3284665051122,61.2597526248882));
#157262=CARTESIAN_POINT('Ctrl Pts',(25.6762586313419,11.3305570276282,61.2738649461799));
#157263=CARTESIAN_POINT('Ctrl Pts',(25.6778710031456,11.3326741191816,61.2879774559578));
#157264=CARTESIAN_POINT('Ctrl Pts',(25.6794812096262,11.3348174442319,61.3020900794107));
#157265=CARTESIAN_POINT('Ctrl Pts',(25.7033718798831,11.3666180068602,61.5114793952784));
#157266=CARTESIAN_POINT('Ctrl Pts',(25.7267862729606,11.4041904957477,61.7208967603058));
#157267=CARTESIAN_POINT('Ctrl Pts',(25.7496897387169,11.4465219413156,61.9302341410493));
#157268=CARTESIAN_POINT('Ctrl Pts',(25.7528247338991,11.4523162118999,61.9588879564619));
#157269=CARTESIAN_POINT('Ctrl Pts',(25.755950149292,11.4581997014192,61.9875402170144));
#157270=CARTESIAN_POINT('Ctrl Pts',(25.7590658892414,11.4641698655163,62.0161905917651));
#157271=CARTESIAN_POINT('Ctrl Pts',(25.7787469805256,11.5018814032199,62.1971654644923));
#157272=CARTESIAN_POINT('Ctrl Pts',(25.7980422182077,11.5430503853908,62.3780667868344));
#157273=CARTESIAN_POINT('Ctrl Pts',(25.8169425291683,11.5871162706067,62.5588925163166));
#157274=CARTESIAN_POINT('Ctrl Pts',(25.8253132742067,11.6066325786085,62.6389782927385));
#157275=CARTESIAN_POINT('Ctrl Pts',(25.8336064365499,11.6267173328886,62.7190489153338));
#157276=CARTESIAN_POINT('Ctrl Pts',(25.8418207621813,11.6473228008902,62.7991028537887));
#157277=CARTESIAN_POINT('Ctrl Pts',(25.8651810053786,11.7059214936263,63.0267635961452));
#157278=CARTESIAN_POINT('Ctrl Pts',(25.887904167324,11.7687308903864,63.2542930833719));
#157279=CARTESIAN_POINT('Ctrl Pts',(25.9099789732516,11.8348056312976,63.4817489544971));
#157280=CARTESIAN_POINT('Ctrl Pts',(25.9152209326329,11.8504959666563,63.5357614083949));
#157281=CARTESIAN_POINT('Ctrl Pts',(25.9204263011686,11.8663704736009,63.5897694858818));
#157282=CARTESIAN_POINT('Ctrl Pts',(25.9255948715915,11.8824165709964,63.6437735380379));
#157283=CARTESIAN_POINT('Ctrl Pts',(25.946675266075,11.947861758997,63.8640330353503));
#157284=CARTESIAN_POINT('Ctrl Pts',(25.9671440608878,12.0161618413149,64.0842296705477));
#157285=CARTESIAN_POINT('Ctrl Pts',(25.9869839824368,12.0866833807512,64.3043607663581));
#157286=CARTESIAN_POINT('Ctrl Pts',(25.9939764388603,12.1115382568256,64.3819445960675));
#157287=CARTESIAN_POINT('Ctrl Pts',(26.0008907192042,12.1366690213426,64.4595198159898));
#157288=CARTESIAN_POINT('Ctrl Pts',(26.0077258813949,12.1620477668799,64.5370847939509));
#157289=CARTESIAN_POINT('Ctrl Pts',(26.0099440547828,12.1702837759751,64.5622564819295));
#157290=CARTESIAN_POINT('Ctrl Pts',(26.0121538949578,12.1785459005521,64.5874270845108));
#157291=CARTESIAN_POINT('Ctrl Pts',(26.0143554277394,12.1868334151086,64.6125968688177));
#157292=CARTESIAN_POINT('Ctrl Pts',(26.0143539439513,12.186832623157,64.61259213409));
#157293=CARTESIAN_POINT('Ctrl Pts',(25.8692560444075,12.300907833433,64.6381768086237));
#157294=CARTESIAN_POINT('Ctrl Pts',(25.7047067450537,12.3865457859842,64.6671912897573));
#157295=CARTESIAN_POINT('Ctrl Pts',(25.3555088143332,12.4896377963212,64.7287643065509));
#157296=CARTESIAN_POINT('Ctrl Pts',(25.1748447519745,12.507191289845,64.7606202551849));
#157297=CARTESIAN_POINT('Ctrl Pts',(24.8063198993144,12.4721236628825,64.8256011297705));
#157298=CARTESIAN_POINT('Ctrl Pts',(24.6229546423116,12.4160836022829,64.857933371908));
#157299=CARTESIAN_POINT('Ctrl Pts',(24.2905142312325,12.2372428251354,64.9165515858591));
#157300=CARTESIAN_POINT('Ctrl Pts',(24.144206218523,12.1176245261334,64.9423496360033));
#157301=CARTESIAN_POINT('Ctrl Pts',(23.9019362111796,11.8306644216987,64.9850683749143));
#157302=CARTESIAN_POINT('Ctrl Pts',(23.8078592158878,11.6657964361489,65.0016566874339));
#157303=CARTESIAN_POINT('Ctrl Pts',(23.6829831124488,11.3148237115169,65.0236757137159));
#157304=CARTESIAN_POINT('Ctrl Pts',(23.6515252125594,11.1316314922004,65.0292225902275));
#157305=CARTESIAN_POINT('Ctrl Pts',(23.6515258014821,10.9472980747274,65.0292224863845));
#157306=CARTESIAN_POINT('Ctrl Pts',(25.6728519466291,11.05620868577,60.1753393120401));
#157307=CARTESIAN_POINT('Ctrl Pts',(25.5908811595391,11.17010610055,60.1922130334301));
#157308=CARTESIAN_POINT('Ctrl Pts',(25.0176949940091,11.96220506401,60.3226366877));
#157309=CARTESIAN_POINT('Ctrl Pts',(23.9454509711491,13.3937300709,60.72216890038));
#157310=CARTESIAN_POINT('Ctrl Pts',(22.4585522519091,15.28518638036,61.63777386195));
#157311=CARTESIAN_POINT('Ctrl Pts',(21.0802507927691,16.97737598619,62.82703989993));
#157312=CARTESIAN_POINT('Ctrl Pts',(19.8267910571591,18.48224713566,64.271659173669));
#157313=CARTESIAN_POINT('Ctrl Pts',(18.7098146781291,19.81562337201,66.003616761918));
#157314=CARTESIAN_POINT('Ctrl Pts',(17.7716110472991,20.96488749236,68.078902873165));
#157315=CARTESIAN_POINT('Ctrl Pts',(17.1084342304291,21.8744622819,70.533431788808));
#157316=CARTESIAN_POINT('Ctrl Pts',(16.8638554479991,22.45052823568,73.2803532769174));
#157317=CARTESIAN_POINT('Ctrl Pts',(17.0786448222291,22.59937448267,75.596712572949));
#157318=CARTESIAN_POINT('Ctrl Pts',(17.3662061271091,22.55171003512,76.874515663416));
#157319=CARTESIAN_POINT('Ctrl Pts',(17.4669987734891,22.52571394401,77.2562285499651));
#157320=CARTESIAN_POINT('Ctrl Pts',(27.6093946371291,9.39445532140801,64.447920892227));
#157321=CARTESIAN_POINT('Ctrl Pts',(27.5226174428891,9.46737944809301,64.451034788112));
#157322=CARTESIAN_POINT('Ctrl Pts',(26.9160359092391,9.97752475953103,64.482341733254));
#157323=CARTESIAN_POINT('Ctrl Pts',(25.7838601800091,10.93479181558,64.661006837171));
#157324=CARTESIAN_POINT('Ctrl Pts',(24.2207011124691,12.25908842062,65.194134063823));
#157325=CARTESIAN_POINT('Ctrl Pts',(22.7783053134691,13.48485509378,65.959148542412));
#157326=CARTESIAN_POINT('Ctrl Pts',(21.4726982157391,14.6052048364,66.94431046259));
#157327=CARTESIAN_POINT('Ctrl Pts',(20.3137223160191,15.62131353079,68.176238741846));
#157328=CARTESIAN_POINT('Ctrl Pts',(19.3392518035291,16.51491733119,69.702089136366));
#157329=CARTESIAN_POINT('Ctrl Pts',(18.6353752499191,17.23396255898,71.553480602797));
#157330=CARTESIAN_POINT('Ctrl Pts',(18.3290383767791,17.69470562174,73.6596809561242));
#157331=CARTESIAN_POINT('Ctrl Pts',(18.4647369076291,17.81439079021,75.444726555105));
#157332=CARTESIAN_POINT('Ctrl Pts',(18.6950959018691,17.77610222599,76.424554931989));
#157333=CARTESIAN_POINT('Ctrl Pts',(18.7775986176291,17.7552396856,76.716506355083));
#157334=CARTESIAN_POINT('Ctrl Pts',(31.5629272267991,9.88281068194302,67.430842306303));
#157335=CARTESIAN_POINT('Ctrl Pts',(31.4711681472091,9.92967730101103,67.444807195928));
#157336=CARTESIAN_POINT('Ctrl Pts',(30.8310903628191,10.25631090589,67.5476759313801));
#157337=CARTESIAN_POINT('Ctrl Pts',(29.6521222456891,10.85487243909,67.805767900236));
#157338=CARTESIAN_POINT('Ctrl Pts',(28.0597002587091,11.65964394348,68.317830215232));
#157339=CARTESIAN_POINT('Ctrl Pts',(26.6228516811691,12.38921116325,68.938303098405));
#157340=CARTESIAN_POINT('Ctrl Pts',(25.3542093351291,13.0450930181,69.658831925755));
#157341=CARTESIAN_POINT('Ctrl Pts',(24.2590278301191,13.63170757615,70.4940295766521));
#157342=CARTESIAN_POINT('Ctrl Pts',(23.3629396071591,14.14148255666,71.468571308628));
#157343=CARTESIAN_POINT('Ctrl Pts',(22.7218359561591,14.5476997234,72.5973874861561));
#157344=CARTESIAN_POINT('Ctrl Pts',(22.4115473378591,14.8062209636,73.8396950223705));
#157345=CARTESIAN_POINT('Ctrl Pts',(22.4566140195691,14.87316749049,74.870971069554));
#157346=CARTESIAN_POINT('Ctrl Pts',(22.5996423578891,14.85173828971,75.432105059216));
#157347=CARTESIAN_POINT('Ctrl Pts',(22.6529499976691,14.84005551372,75.5989411619891));
#157348=CARTESIAN_POINT('Ctrl Pts',(35.8805628265291,12.31710390136,67.87700830848));
#157349=CARTESIAN_POINT('Ctrl Pts',(35.7857292024291,12.36372287642,67.921898444141));
#157350=CARTESIAN_POINT('Ctrl Pts',(35.1260583462191,12.68200901524,68.23708902494));
#157351=CARTESIAN_POINT('Ctrl Pts',(33.9330000499891,13.18738451274,68.8416951696051));
#157352=CARTESIAN_POINT('Ctrl Pts',(32.3705467692491,13.73746778379,69.702912182422));
#157353=CARTESIAN_POINT('Ctrl Pts',(31.0065678005891,14.14850934188,70.5189831644171));
#157354=CARTESIAN_POINT('Ctrl Pts',(29.8485481528991,14.4541608558,71.28034056044));
#157355=CARTESIAN_POINT('Ctrl Pts',(28.8962838945291,14.67861693811,71.987970801025));
#157356=CARTESIAN_POINT('Ctrl Pts',(28.1604571839791,14.83686516773,72.6398212113681));
#157357=CARTESIAN_POINT('Ctrl Pts',(27.6593550752991,14.93874245386,73.2287174375679));
#157358=CARTESIAN_POINT('Ctrl Pts',(27.4045731969891,14.99268753181,73.7451354687612));
#157359=CARTESIAN_POINT('Ctrl Pts',(27.3853582494091,15.0053667451,74.11532093663));
#157360=CARTESIAN_POINT('Ctrl Pts',(27.4474386542391,15.00123185086,74.312087977728));
#157361=CARTESIAN_POINT('Ctrl Pts',(27.4728519056491,14.99893719101,74.370762926049));
#157362=CARTESIAN_POINT('',(28.295163666826,10.3190022129161,64.2104232034421));
#157363=CARTESIAN_POINT('Ctrl Pts',(26.0143837217827,12.1868716890914,64.6125868834549));
#157364=CARTESIAN_POINT('Ctrl Pts',(26.3866707717358,11.8943678422565,64.5469426319798));
#157365=CARTESIAN_POINT('Ctrl Pts',(26.7890747474804,11.5770393684394,64.4759879539895));
#157366=CARTESIAN_POINT('Ctrl Pts',(27.546069310181,10.9630297660278,64.3425093883358));
#157367=CARTESIAN_POINT('Ctrl Pts',(27.9293174909002,10.6434402054098,64.2749323936898));
#157368=CARTESIAN_POINT('Ctrl Pts',(28.2951915629989,10.3190345262137,64.2104189232372));
#157369=CARTESIAN_POINT('Origin',(33.823252652802,17.58608062208,59.024939776261));
#157370=CARTESIAN_POINT('Ctrl Pts',(26.0076877261891,10.58495646334,60.26985796972));
#157371=CARTESIAN_POINT('Ctrl Pts',(25.7990037333791,10.89447975427,60.24482455385));
#157372=CARTESIAN_POINT('Ctrl Pts',(25.5896565743691,11.1831771459,60.22557462704));
#157373=CARTESIAN_POINT('Ctrl Pts',(25.3807021623791,11.45236674632,60.21090371374));
#157374=CARTESIAN_POINT('Ctrl Pts',(27.9987970739791,9.17295597816802,64.622590824873));
#157375=CARTESIAN_POINT('Ctrl Pts',(27.7660735618591,9.33426324017502,64.560255312909));
#157376=CARTESIAN_POINT('Ctrl Pts',(27.5333174178191,9.48524635017302,64.499674997551));
#157377=CARTESIAN_POINT('Ctrl Pts',(27.3000253208991,9.63004663000602,64.442635376589));
#157378=CARTESIAN_POINT('Ctrl Pts',(32.0801713998191,9.69904765178202,67.445984142724));
#157379=CARTESIAN_POINT('Ctrl Pts',(31.8033473372391,9.81925633458402,67.454791081483));
#157380=CARTESIAN_POINT('Ctrl Pts',(31.5208971300691,9.93468827936802,67.469340771313));
#157381=CARTESIAN_POINT('Ctrl Pts',(31.2300886277791,10.04875492352,67.490838049821));
#157382=CARTESIAN_POINT('Ctrl Pts',(36.5371673514891,11.94221289613,67.553890268911));
#157383=CARTESIAN_POINT('Ctrl Pts',(36.2147089752091,12.14570654659,67.712396250694));
#157384=CARTESIAN_POINT('Ctrl Pts',(35.8771568089191,12.34268599228,67.886973156649));
#157385=CARTESIAN_POINT('Ctrl Pts',(35.5198166400391,12.53258632276,68.07491847425));
#157386=CARTESIAN_POINT('Ctrl Pts',(28.2951363354843,10.3189703124041,64.210428661338));
#157387=CARTESIAN_POINT('Ctrl Pts',(28.3673395453708,10.2549306784213,64.1976972873413));
#157388=CARTESIAN_POINT('Ctrl Pts',(28.4381421072126,10.1894797611389,64.1852128853848));
#157389=CARTESIAN_POINT('Ctrl Pts',(28.577126093425,10.0553246236656,64.1607062587292));
#157390=CARTESIAN_POINT('Ctrl Pts',(28.6450926511801,9.98682648706178,64.1487219208116));
#157391=CARTESIAN_POINT('Ctrl Pts',(28.7116430428839,9.91672751628407,64.1369872911775));
#157392=CARTESIAN_POINT('Ctrl Pts',(36.2322199092691,1.29987451700601,99.1648548727501));
#157393=CARTESIAN_POINT('Ctrl Pts',(36.2370515565391,1.23373127101501,99.16704017222));
#157394=CARTESIAN_POINT('Ctrl Pts',(36.2583081778491,0.918934546249416,
99.17660179767));
#157395=CARTESIAN_POINT('Ctrl Pts',(36.2789671085291,0.416646817226614,
99.1856530378401));
#157396=CARTESIAN_POINT('Ctrl Pts',(36.2808220405991,-0.0191504896747858,
99.18645022329));
#157397=CARTESIAN_POINT('Ctrl Pts',(36.2786095746291,-0.207586528585886,
99.18548739257));
#157398=CARTESIAN_POINT('Ctrl Pts',(34.9169995834991,0.648872675590514,
92.8720190887701));
#157399=CARTESIAN_POINT('Ctrl Pts',(34.9212091234391,0.615492124139614,
92.87094475832));
#157400=CARTESIAN_POINT('Ctrl Pts',(34.9397227668891,0.457009215198214,
92.86613805011));
#157401=CARTESIAN_POINT('Ctrl Pts',(34.9576892444091,0.206679526451214,
92.86110273846));
#157402=CARTESIAN_POINT('Ctrl Pts',(34.9593035548391,-0.00948024598489779,
92.86063999751));
#157403=CARTESIAN_POINT('Ctrl Pts',(34.9573789807491,-0.103058298997286,
92.86118379398));
#157404=CARTESIAN_POINT('Ctrl Pts',(38.6114884146191,0.506179248681214,
87.57260696818));
#157405=CARTESIAN_POINT('Ctrl Pts',(38.6168724865691,0.480286838357915,
87.57214900918));
#157406=CARTESIAN_POINT('Ctrl Pts',(38.6405854995891,0.357200917525514,
87.57008859617));
#157407=CARTESIAN_POINT('Ctrl Pts',(38.6637464841091,0.161757611975314,
87.56787911336));
#157408=CARTESIAN_POINT('Ctrl Pts',(38.6658219179391,-0.00742765239893279,
87.56767441493));
#157409=CARTESIAN_POINT('Ctrl Pts',(38.6633431586391,-0.0806241679503258,
87.56791373377));
#157410=CARTESIAN_POINT('Ctrl Pts',(44.9848109864291,0.961820384965713,
86.61004976678));
#157411=CARTESIAN_POINT('Ctrl Pts',(44.9924252103591,0.913417248693113,
86.61369530813));
#157412=CARTESIAN_POINT('Ctrl Pts',(45.0259996265791,0.682479313720714,
86.62976316487));
#157413=CARTESIAN_POINT('Ctrl Pts',(45.0589648322991,0.310222582160714,
86.6455090589899));
#157414=CARTESIAN_POINT('Ctrl Pts',(45.0619122089991,-0.0142877026623558,
86.6469175713899));
#157415=CARTESIAN_POINT('Ctrl Pts',(45.0583868262091,-0.154437964819286,
86.64523340457));
#157416=CARTESIAN_POINT('Origin',(36.6704247457035,0.356346398719197,81.8746090081706));
#157417=CARTESIAN_POINT('Ctrl Pts',(39.6130209037191,0.772780366718814,
89.0475659539699));
#157418=CARTESIAN_POINT('Ctrl Pts',(39.6131511234091,0.768070971044614,
89.0483044665601));
#157419=CARTESIAN_POINT('Ctrl Pts',(39.6159992090891,0.664122906098314,
89.0644567630999));
#157420=CARTESIAN_POINT('Ctrl Pts',(39.6205603414591,0.455619638640514,
89.0903242302099));
#157421=CARTESIAN_POINT('Ctrl Pts',(39.6239814776291,0.140849503561414,
89.10972645757));
#157422=CARTESIAN_POINT('Ctrl Pts',(39.6237889996191,-0.142041377329986,
89.10863486051));
#157423=CARTESIAN_POINT('Ctrl Pts',(39.6219727743591,-0.319354852029586,
89.09833453524));
#157424=CARTESIAN_POINT('Ctrl Pts',(39.6210240375191,-0.387361342889386,
89.0929539812099));
#157425=CARTESIAN_POINT('Ctrl Pts',(38.5565416256591,0.971382837408014,
90.50038750645));
#157426=CARTESIAN_POINT('Ctrl Pts',(38.5567042884291,0.965500141328614,
90.50131001286));
#157427=CARTESIAN_POINT('Ctrl Pts',(38.5602625557091,0.835631771075914,
90.5214899494));
#157428=CARTESIAN_POINT('Ctrl Pts',(38.5659866718191,0.574159320760314,
90.55395302502));
#157429=CARTESIAN_POINT('Ctrl Pts',(38.5702990716391,0.177643147708914,
90.57840985973));
#157430=CARTESIAN_POINT('Ctrl Pts',(38.5700563612191,-0.179118474077086,
90.57703338056));
#157431=CARTESIAN_POINT('Ctrl Pts',(38.5677671045191,-0.402543671104486,
90.56405036064));
#157432=CARTESIAN_POINT('Ctrl Pts',(38.5665713020191,-0.488170587549486,
90.55726862766));
#157433=CARTESIAN_POINT('Ctrl Pts',(36.8455425264091,0.835335570085914,
89.93447664681));
#157434=CARTESIAN_POINT('Ctrl Pts',(36.8456829649291,0.830256611811614,
89.93527311321));
#157435=CARTESIAN_POINT('Ctrl Pts',(36.8487547414491,0.718144247780114,
89.95269402358));
#157436=CARTESIAN_POINT('Ctrl Pts',(36.8536821869091,0.492956907891814,
89.98063895543));
#157437=CARTESIAN_POINT('Ctrl Pts',(36.8573840505991,0.152438653909214,
90.00163326767));
#157438=CARTESIAN_POINT('Ctrl Pts',(36.8571757505391,-0.153719808717186,
90.0004519393099));
#157439=CARTESIAN_POINT('Ctrl Pts',(36.8552105312691,-0.345557413745186,
89.9893066270201));
#157440=CARTESIAN_POINT('Ctrl Pts',(36.8541839744391,-0.419113932769686,
89.9834847339001));
#157441=CARTESIAN_POINT('Ctrl Pts',(36.8978805960391,0.556890469747314,
88.14953661764));
#157442=CARTESIAN_POINT('Ctrl Pts',(36.8979755486391,0.553456504850614,
88.15007512059));
#157443=CARTESIAN_POINT('Ctrl Pts',(36.9000516346991,0.477684987873014,
88.16184918971));
#157444=CARTESIAN_POINT('Ctrl Pts',(36.9033485509791,0.326761625590414,
88.18054693109));
#157445=CARTESIAN_POINT('Ctrl Pts',(36.9058008431191,0.100853142908714,
88.19445457091));
#157446=CARTESIAN_POINT('Ctrl Pts',(36.9056629700091,-0.101736890840086,
88.19367265364));
#157447=CARTESIAN_POINT('Ctrl Pts',(36.9043609513991,-0.228924831109186,
88.18628853918));
#157448=CARTESIAN_POINT('Ctrl Pts',(36.9036807861291,-0.277777119853686,
88.18243113024));
#157449=CARTESIAN_POINT('Ctrl Pts',(36.9231015705691,0.454612543733214,
88.46713451361));
#157450=CARTESIAN_POINT('Ctrl Pts',(36.9246228019291,0.381730267779614,
88.47576184538));
#157451=CARTESIAN_POINT('Ctrl Pts',(36.9270069740053,0.233138977846363,
88.4892831592894));
#157452=CARTESIAN_POINT('Ctrl Pts',(36.9278603928332,0.0786786354693159,
88.4941231372269));
#157453=CARTESIAN_POINT('Ctrl Pts',(36.9278603430304,-1.00177093760852E-6,
88.4941228548076));
#157454=CARTESIAN_POINT('Origin',(35.1195182435891,111.0724296188,78.238505182562));
#157455=CARTESIAN_POINT('Origin',(34.1682376097291,0.499074165591614,72.8435246184046));
#157456=CARTESIAN_POINT('Ctrl Pts',(36.9162947564091,-13.53296430165,79.1141410123499));
#157457=CARTESIAN_POINT('Ctrl Pts',(36.8379078596091,-13.54084808517,79.125313649548));
#157458=CARTESIAN_POINT('Ctrl Pts',(36.6331365458791,-13.54075199426,79.161549961231));
#157459=CARTESIAN_POINT('Ctrl Pts',(36.3090821190191,-13.45062514319,79.248712848581));
#157460=CARTESIAN_POINT('Ctrl Pts',(35.9700390021391,-13.22015785476,79.385367769725));
#157461=CARTESIAN_POINT('Ctrl Pts',(35.6829255508391,-12.85709379684,79.5572152706409));
#157462=CARTESIAN_POINT('Ctrl Pts',(35.4759945703691,-12.36078514696,79.76035426938));
#157463=CARTESIAN_POINT('Ctrl Pts',(35.4015806341291,-11.87740516072,79.937203183361));
#157464=CARTESIAN_POINT('Ctrl Pts',(35.4009999658791,-11.56819412752,80.042537145577));
#157465=CARTESIAN_POINT('Ctrl Pts',(35.4046387170491,-11.47622675764,80.073192707259));
#157466=CARTESIAN_POINT('Ctrl Pts',(36.7378435778691,-13.79049802242,77.964715139805));
#157467=CARTESIAN_POINT('Ctrl Pts',(36.6439251111591,-13.80190892298,77.9791527381109));
#157468=CARTESIAN_POINT('Ctrl Pts',(36.3962932068891,-13.80182730288,78.022615822591));
#157469=CARTESIAN_POINT('Ctrl Pts',(36.0104672867091,-13.67100041842,78.115500673479));
#157470=CARTESIAN_POINT('Ctrl Pts',(35.6462725616391,-13.35339373284,78.24515779335));
#157471=CARTESIAN_POINT('Ctrl Pts',(35.4018733334191,-12.89430356954,78.398017084265));
#157472=CARTESIAN_POINT('Ctrl Pts',(35.3103253268891,-12.33293611612,78.577596495555));
#157473=CARTESIAN_POINT('Ctrl Pts',(35.3702242253491,-11.85283482995,78.7438470995349));
#157474=CARTESIAN_POINT('Ctrl Pts',(35.4537140494691,-11.57449314574,78.85189623076));
#157475=CARTESIAN_POINT('Ctrl Pts',(35.4818326284191,-11.49406040224,78.884310074634));
#157476=CARTESIAN_POINT('Ctrl Pts',(36.7652353229291,-14.89891646854,77.528723139282));
#157477=CARTESIAN_POINT('Ctrl Pts',(36.6037070282991,-14.91744611088,77.55712837637));
#157478=CARTESIAN_POINT('Ctrl Pts',(36.1758646851091,-14.91734661094,77.632099353845));
#157479=CARTESIAN_POINT('Ctrl Pts',(35.5036841639991,-14.70473669194,77.752723593715));
#157480=CARTESIAN_POINT('Ctrl Pts',(34.8653075109791,-14.19454494754,77.8734639595339));
#157481=CARTESIAN_POINT('Ctrl Pts',(34.4335323097691,-13.47313071354,77.972684115116));
#157482=CARTESIAN_POINT('Ctrl Pts',(34.2645298594791,-12.62142137233,78.053662285297));
#157483=CARTESIAN_POINT('Ctrl Pts',(34.3553511232591,-11.93074611859,78.113117408706));
#157484=CARTESIAN_POINT('Ctrl Pts',(34.4887982535091,-11.55088371147,78.152250356099));
#157485=CARTESIAN_POINT('Ctrl Pts',(34.5338861201291,-11.44301453344,78.164268167064));
#157486=CARTESIAN_POINT('Ctrl Pts',(36.9738597083291,-15.86235421184,78.197884728009));
#157487=CARTESIAN_POINT('Ctrl Pts',(36.7533877970291,-15.88519834299,78.23841096985));
#157488=CARTESIAN_POINT('Ctrl Pts',(36.1698963531991,-15.88506467682,78.340862498621));
#157489=CARTESIAN_POINT('Ctrl Pts',(35.2440551909491,-15.62306719678,78.486320926825));
#157490=CARTESIAN_POINT('Ctrl Pts',(34.3288067440591,-14.98787397254,78.6042368987989));
#157491=CARTESIAN_POINT('Ctrl Pts',(33.6479144789791,-14.07352439099,78.663359407567));
#157492=CARTESIAN_POINT('Ctrl Pts',(33.2782095926791,-12.96704954774,78.6592835796531));
#157493=CARTESIAN_POINT('Ctrl Pts',(33.2687803614491,-12.0411391461,78.61169711387));
#157494=CARTESIAN_POINT('Ctrl Pts',(33.3731871600291,-11.51857786737,78.5722006974239));
#157495=CARTESIAN_POINT('Ctrl Pts',(33.4124876124591,-11.3689516287,78.559993102657));
#157496=CARTESIAN_POINT('Ctrl Pts',(36.6289738731116,-13.6294450659104,
78.8700122234104));
#157497=CARTESIAN_POINT('Ctrl Pts',(36.6267895588953,-13.6292110353221,
78.8704722093663));
#157498=CARTESIAN_POINT('Ctrl Pts',(36.624607035549,-13.6289708105016,78.8709335732414));
#157499=CARTESIAN_POINT('Ctrl Pts',(36.6224263107416,-13.6287244011036,
78.8713963118592));
#157500=CARTESIAN_POINT('Ctrl Pts',(36.583935576154,-13.6243751688195,78.8795638482938));
#157501=CARTESIAN_POINT('Ctrl Pts',(36.5460052001296,-13.6181035969037,
78.8881584920323));
#157502=CARTESIAN_POINT('Ctrl Pts',(36.5086374234726,-13.6100119136855,
78.89716440318));
#157503=CARTESIAN_POINT('Ctrl Pts',(36.4706975949425,-13.6017963573617,
78.9063081830693));
#157504=CARTESIAN_POINT('Ctrl Pts',(36.4333371557682,-13.5917043217201,
78.9158760369807));
#157505=CARTESIAN_POINT('Ctrl Pts',(36.3965629433869,-13.5797903680907,
78.9258649069554));
#157506=CARTESIAN_POINT('Ctrl Pts',(36.3593905003606,-13.567747397383,78.9359619471362));
#157507=CARTESIAN_POINT('Ctrl Pts',(36.3228164476515,-13.553842624327,78.9464892932658));
#157508=CARTESIAN_POINT('Ctrl Pts',(36.2868612731161,-13.5380825288037,
78.9574556553683));
#157509=CARTESIAN_POINT('Ctrl Pts',(36.2701595863516,-13.5307617416788,
78.9625496855643));
#157510=CARTESIAN_POINT('Ctrl Pts',(36.2535916812617,-13.5230399464007,
78.9677385985922));
#157511=CARTESIAN_POINT('Ctrl Pts',(36.2371611452247,-13.5149143727149,
78.9730240141749));
#157512=CARTESIAN_POINT('Ctrl Pts',(36.2232866202606,-13.5080528512955,
78.9774872057764));
#157513=CARTESIAN_POINT('Ctrl Pts',(36.2095100668752,-13.5009033643706,
78.9820192194605));
#157514=CARTESIAN_POINT('Ctrl Pts',(36.1958317439024,-13.4934659169776,
78.9866212604943));
#157515=CARTESIAN_POINT('Ctrl Pts',(36.1444157381463,-13.4655089928185,
79.0039200601175));
#157516=CARTESIAN_POINT('Ctrl Pts',(36.0943775497546,-13.433536582339,79.0221032244092));
#157517=CARTESIAN_POINT('Ctrl Pts',(36.0460456675535,-13.397702919938,79.0410869201147));
#157518=CARTESIAN_POINT('Ctrl Pts',(36.0159227434528,-13.3753695316321,
79.0529185393036));
#157519=CARTESIAN_POINT('Ctrl Pts',(35.9864634576983,-13.3515359442591,
79.0650610559982));
#157520=CARTESIAN_POINT('Ctrl Pts',(35.9577574687535,-13.3262373968706,
79.0774930494177));
#157521=CARTESIAN_POINT('Ctrl Pts',(35.9352874114504,-13.3064345672032,
79.0872243847522));
#157522=CARTESIAN_POINT('Ctrl Pts',(35.9133671055204,-13.2858181861862,
79.0970883044359));
#157523=CARTESIAN_POINT('Ctrl Pts',(35.8919558472264,-13.2643391294296,
79.1071099047377));
#157524=CARTESIAN_POINT('Ctrl Pts',(35.8670407349144,-13.2393451237483,
79.1187714938716));
#157525=CARTESIAN_POINT('Ctrl Pts',(35.8428139346251,-13.2131835002351,
79.1306465255989));
#157526=CARTESIAN_POINT('Ctrl Pts',(35.8192096787325,-13.1857454858265,
79.1427855534418));
#157527=CARTESIAN_POINT('Ctrl Pts',(35.79560542284,-13.158307471418,79.1549245812846));
#157528=CARTESIAN_POINT('Ctrl Pts',(35.7726233866794,-13.1295926154809,
79.1673277169806));
#157529=CARTESIAN_POINT('Ctrl Pts',(35.7502396011647,-13.0994575617588,
79.1800509756508));
#157530=CARTESIAN_POINT('Ctrl Pts',(35.7151504146276,-13.0522173610044,
79.1999961630518));
#157531=CARTESIAN_POINT('Ctrl Pts',(35.6819319380871,-13.0018483734156,
79.2207485864702));
#157532=CARTESIAN_POINT('Ctrl Pts',(35.6508857720451,-12.9485063268026,
79.2422271853796));
#157533=CARTESIAN_POINT('Ctrl Pts',(35.6380117503611,-12.9263867947534,
79.2511337907147));
#157534=CARTESIAN_POINT('Ctrl Pts',(35.6255115670388,-12.9037565275983,
79.2601651149864));
#157535=CARTESIAN_POINT('Ctrl Pts',(35.6134081179858,-12.8806288083371,
79.2693147004937));
#157536=CARTESIAN_POINT('Ctrl Pts',(35.5831213358917,-12.8227557020407,
79.2922099513679));
#157537=CARTESIAN_POINT('Ctrl Pts',(35.5553181247539,-12.7617645047354,
79.3158466479645));
#157538=CARTESIAN_POINT('Ctrl Pts',(35.5302240670213,-12.6978443630867,
79.3401370271472));
#157539=CARTESIAN_POINT('Ctrl Pts',(35.5062809457656,-12.6368559124151,
79.3633133304901));
#157540=CARTESIAN_POINT('Ctrl Pts',(35.4848039681179,-12.5732008806325,
79.3870847308051));
#157541=CARTESIAN_POINT('Ctrl Pts',(35.4660031304662,-12.5070876508559,
79.4113622174152));
#157542=CARTESIAN_POINT('Ctrl Pts',(35.4620975761915,-12.4933537517631,
79.4164054523691));
#157543=CARTESIAN_POINT('Ctrl Pts',(35.4583075612117,-12.4795139372748,
79.4214704807594));
#157544=CARTESIAN_POINT('Ctrl Pts',(35.4546350596877,-12.4655703406705,
79.4265564316822));
#157545=CARTESIAN_POINT('Ctrl Pts',(35.446244748698,-12.4337143670073,79.4381759530474));
#157546=CARTESIAN_POINT('Ctrl Pts',(35.438466298639,-12.4013151850429,79.4499020521234));
#157547=CARTESIAN_POINT('Ctrl Pts',(35.4313279849064,-12.368402830968,79.4617323991114));
#157548=CARTESIAN_POINT('Ctrl Pts',(35.4166655594567,-12.3007993385919,
79.4860324771486));
#157549=CARTESIAN_POINT('Ctrl Pts',(35.4047053295063,-12.2310279449783,
79.5107727246997));
#157550=CARTESIAN_POINT('Ctrl Pts',(35.3956126986768,-12.159289658879,79.5359445459002));
#157551=CARTESIAN_POINT('Ctrl Pts',(35.3864867829726,-12.0872887645299,
79.56120851215));
#157552=CARTESIAN_POINT('Ctrl Pts',(35.3802497959325,-12.0133066643763,
79.5869072534782));
#157553=CARTESIAN_POINT('Ctrl Pts',(35.3770484236597,-11.9375947461263,
79.6130256997429));
#157554=CARTESIAN_POINT('Ctrl Pts',(35.3744205448052,-11.8754458512009,
79.6344652908936));
#157555=CARTESIAN_POINT('Ctrl Pts',(35.3738377628765,-11.8121323365772,
79.6561875923856));
#157556=CARTESIAN_POINT('Ctrl Pts',(35.3753690601812,-11.7478162345504,
79.6781806669065));
#157557=CARTESIAN_POINT('Ctrl Pts',(35.3762341383981,-11.7114820369465,
79.6906052494042));
#157558=CARTESIAN_POINT('Ctrl Pts',(35.3777737267097,-11.674828239601,79.7031162043097));
#157559=CARTESIAN_POINT('Ctrl Pts',(35.3799958958808,-11.6378856606036,
79.7157076007637));
#157560=CARTESIAN_POINT('Ctrl Pts',(35.5596731802056,-13.409584407367,78.6873025602364));
#157561=CARTESIAN_POINT('Ctrl Pts',(35.5649489821513,-13.410762854301,78.6892006371155));
#157562=CARTESIAN_POINT('Ctrl Pts',(35.572454155639,-13.4127848705518,78.6916420133374));
#157563=CARTESIAN_POINT('Ctrl Pts',(35.5822091762942,-13.4155951123882,
78.6946608021742));
#157564=CARTESIAN_POINT('Ctrl Pts',(35.5888413201348,-13.4175057109143,
78.6967131855056));
#157565=CARTESIAN_POINT('Ctrl Pts',(35.5965133072729,-13.4197796194329,
78.6990327697528));
#157566=CARTESIAN_POINT('Ctrl Pts',(35.6052297520272,-13.4223863862809,
78.7016342587272));
#157567=CARTESIAN_POINT('Ctrl Pts',(35.6159986738011,-13.4256069732357,
78.7048483250181));
#157568=CARTESIAN_POINT('Ctrl Pts',(35.628364387104,-13.4293376813513,78.7084926497722));
#157569=CARTESIAN_POINT('Ctrl Pts',(35.6423428025468,-13.4335034999063,
78.7126042044134));
#157570=CARTESIAN_POINT('Ctrl Pts',(35.6493320102682,-13.4355864091838,
78.7146599817339));
#157571=CARTESIAN_POINT('Ctrl Pts',(35.6567245312736,-13.4377776618008,
78.7168328489925));
#157572=CARTESIAN_POINT('Ctrl Pts',(35.66452171591,-13.440065921592,78.7191278210619));
#157573=CARTESIAN_POINT('Ctrl Pts',(35.6682193836418,-13.4411510856335,
78.7202161682747));
#157574=CARTESIAN_POINT('Ctrl Pts',(35.6720080603159,-13.4422580615983,
78.721331972209));
#157575=CARTESIAN_POINT('Ctrl Pts',(35.6758878046835,-13.4433855189776,
78.7224757778056));
#157576=CARTESIAN_POINT('Ctrl Pts',(35.6760986229854,-13.4434467829754,
78.7225379301359));
#157577=CARTESIAN_POINT('Ctrl Pts',(35.6763097101715,-13.4435081074283,
78.7226001651511));
#157578=CARTESIAN_POINT('Ctrl Pts',(35.6765210662432,-13.4435694921167,
78.7226624829415));
#157579=CARTESIAN_POINT('Ctrl Pts',(35.6797960285612,-13.4445206478591,
78.7236280971005));
#157580=CARTESIAN_POINT('Ctrl Pts',(35.6842564285498,-13.4458099995922,
78.7249439247759));
#157581=CARTESIAN_POINT('Ctrl Pts',(35.6872168365588,-13.4466605313594,
78.7258191404787));
#157582=CARTESIAN_POINT('Ctrl Pts',(35.6879635322211,-13.4468750586744,
78.7260398937556));
#157583=CARTESIAN_POINT('Ctrl Pts',(35.6886148676402,-13.4470619434621,
78.726232514826));
#157584=CARTESIAN_POINT('Ctrl Pts',(35.6891278548595,-13.4472091357767,
78.7263841598653));
#157585=CARTESIAN_POINT('Ctrl Pts',(35.729876918238,-13.4589013353743,78.7384300609778));
#157586=CARTESIAN_POINT('Ctrl Pts',(35.7706602076644,-13.4704088812035,
78.7501898760101));
#157587=CARTESIAN_POINT('Ctrl Pts',(35.8114521558143,-13.4815662061391,
78.7615388724631));
#157588=CARTESIAN_POINT('Ctrl Pts',(35.8318481298892,-13.487144868607,78.7672133706896));
#157589=CARTESIAN_POINT('Ctrl Pts',(35.8520872866738,-13.4925860047892,
78.7727477992517));
#157590=CARTESIAN_POINT('Ctrl Pts',(35.8721725455393,-13.4978862209229,
78.7781234405706));
#157591=CARTESIAN_POINT('Ctrl Pts',(35.8822151749721,-13.5005363289897,
78.7808112612301));
#157592=CARTESIAN_POINT('Ctrl Pts',(35.8922193317316,-13.5031512070723,
78.7834593823422));
#157593=CARTESIAN_POINT('Ctrl Pts',(35.9021856584897,-13.505729861492,78.7860663134503));
#157594=CARTESIAN_POINT('Ctrl Pts',(35.9071688218687,-13.5070191887018,
78.7873697790044));
#157595=CARTESIAN_POINT('Ctrl Pts',(35.9121425274005,-13.5082994605119,
78.7886629476841));
#157596=CARTESIAN_POINT('Ctrl Pts',(35.9171068798581,-13.5095705193357,
78.7899456958789));
#157597=CARTESIAN_POINT('Ctrl Pts',(35.9208245999257,-13.5105223939128,
78.7909063244293));
#157598=CARTESIAN_POINT('Ctrl Pts',(35.9237075813183,-13.511255961388,78.7916505395541));
#157599=CARTESIAN_POINT('Ctrl Pts',(35.9276195592542,-13.5122511243835,
78.792650917631));
#157600=CARTESIAN_POINT('Ctrl Pts',(35.9289313305321,-13.5125848241782,
78.792986366156));
#157601=CARTESIAN_POINT('Ctrl Pts',(35.930358746238,-13.5129475867588,78.7933507170801));
#157602=CARTESIAN_POINT('Ctrl Pts',(35.931971861629,-13.5133561840459,78.793762161952));
#157603=CARTESIAN_POINT('Ctrl Pts',(35.9432221584124,-13.5162058504559,
78.7966316881774));
#157604=CARTESIAN_POINT('Ctrl Pts',(35.9536968873557,-13.5188035375634,
78.7992871885907));
#157605=CARTESIAN_POINT('Ctrl Pts',(35.9640624555409,-13.521342645619,78.8018798382663));
#157606=CARTESIAN_POINT('Ctrl Pts',(35.9744563967455,-13.5238887038157,
78.8044795846393));
#157607=CARTESIAN_POINT('Ctrl Pts',(35.9847405951858,-13.5263757301332,
78.8070161663376));
#157608=CARTESIAN_POINT('Ctrl Pts',(35.9955799080153,-13.5289503325776,
78.8096553848795));
#157609=CARTESIAN_POINT('Ctrl Pts',(35.9986196867187,-13.5296723545179,
78.8103955277689));
#157610=CARTESIAN_POINT('Ctrl Pts',(36.0017030790087,-13.5304009701641,
78.8111438242411));
#157611=CARTESIAN_POINT('Ctrl Pts',(36.0048446387178,-13.5311386965311,
78.8119041305644));
#157612=CARTESIAN_POINT('Ctrl Pts',(36.0157346109575,-13.5336959675688,
78.8145396732634));
#157613=CARTESIAN_POINT('Ctrl Pts',(36.0243877408748,-13.5356865589943,
78.8165955497169));
#157614=CARTESIAN_POINT('Ctrl Pts',(36.0308156514772,-13.5372019178371,
78.8180503777498));
#157615=CARTESIAN_POINT('Ctrl Pts',(36.0372606024798,-13.5387212938984,
78.8195090625338));
#157616=CARTESIAN_POINT('Ctrl Pts',(36.0414686433905,-13.539762858444,78.8203634758004));
#157617=CARTESIAN_POINT('Ctrl Pts',(36.0434419127291,-13.5403694672138,
78.8206064982397));
#157618=CARTESIAN_POINT('Ctrl Pts',(36.0441117127454,-13.5405753724879,
78.8206889889726));
#157619=CARTESIAN_POINT('Ctrl Pts',(36.0445239400253,-13.5407307481149,
78.8207011613338));
#157620=CARTESIAN_POINT('Ctrl Pts',(36.0446784011166,-13.5408359897401,
78.8206431222969));
#157621=CARTESIAN_POINT('Ctrl Pts',(33.8015018549743,-13.7317040852684,
78.231178210434));
#157622=CARTESIAN_POINT('Ctrl Pts',(33.8448367011614,-13.7318398987138,
78.2231897821826));
#157623=CARTESIAN_POINT('Ctrl Pts',(33.9729484993377,-13.7306782863685,
78.2035675708194));
#157624=CARTESIAN_POINT('Ctrl Pts',(34.1794028973399,-13.7215222815351,
78.1905757013909));
#157625=CARTESIAN_POINT('Ctrl Pts',(34.410851781839,-13.7010503656952,78.2017087925164));
#157626=CARTESIAN_POINT('Ctrl Pts',(34.6169343870141,-13.67434261052,78.2323749945655));
#157627=CARTESIAN_POINT('Ctrl Pts',(34.7988676057059,-13.6435683591641,
78.2764569312182));
#157628=CARTESIAN_POINT('Ctrl Pts',(34.9584049522099,-13.6103796896382,
78.3292431282214));
#157629=CARTESIAN_POINT('Ctrl Pts',(35.0975727630671,-13.576019734666,78.3871814162859));
#157630=CARTESIAN_POINT('Ctrl Pts',(35.2184605265174,-13.5414149887607,
78.4476361863756));
#157631=CARTESIAN_POINT('Ctrl Pts',(35.3230564896596,-13.5072433877898,
78.5086867494384));
#157632=CARTESIAN_POINT('Ctrl Pts',(35.4130828699557,-13.4740390254729,
78.5688811234007));
#157633=CARTESIAN_POINT('Ctrl Pts',(35.4899484910174,-13.4422810794632,
78.6270120644502));
#157634=CARTESIAN_POINT('Ctrl Pts',(35.5548824783634,-13.412407270912,78.6820491833158));
#157635=CARTESIAN_POINT('Ctrl Pts',(35.609139363501,-13.3847427053007,78.7332420479501));
#157636=CARTESIAN_POINT('Ctrl Pts',(35.6540406849326,-13.3594694892852,
78.7801592442625));
#157637=CARTESIAN_POINT('Ctrl Pts',(35.6906205410342,-13.3367332240462,
78.8224176266727));
#157638=CARTESIAN_POINT('Ctrl Pts',(35.7198794129803,-13.3166160756286,
78.8598141138234));
#157639=CARTESIAN_POINT('Ctrl Pts',(35.7400793850874,-13.3011802483082,
78.8884757827741));
#157640=CARTESIAN_POINT('Ctrl Pts',(35.7502020927212,-13.2927142033317,
78.9041630984296));
#157641=CARTESIAN_POINT('Ctrl Pts',(35.7536670291067,-13.2897107768893,
78.9097209772309));
#157642=CARTESIAN_POINT('Ctrl Pts',(33.7642812125629,-14.0482563699744,
78.0322674443946));
#157643=CARTESIAN_POINT('Ctrl Pts',(33.8130408089844,-14.0483970404398,
78.0232716765594));
#157644=CARTESIAN_POINT('Ctrl Pts',(33.9571859795452,-14.0471930263636,
78.0012572053819));
#157645=CARTESIAN_POINT('Ctrl Pts',(34.1894920675434,-14.0377087515782,
77.9871247460472));
#157646=CARTESIAN_POINT('Ctrl Pts',(34.4501081986777,-14.0164476769987,
78.0007115608826));
#157647=CARTESIAN_POINT('Ctrl Pts',(34.6825015229247,-13.9885972267012,
78.0366152126997));
#157648=CARTESIAN_POINT('Ctrl Pts',(34.8881313202119,-13.9563387079234,
78.0879027470612));
#157649=CARTESIAN_POINT('Ctrl Pts',(35.0690171621493,-13.9213354830119,
78.1492629281395));
#157650=CARTESIAN_POINT('Ctrl Pts',(35.2274467707762,-13.8848455486338,
78.2167089525784));
#157651=CARTESIAN_POINT('Ctrl Pts',(35.3657608913579,-13.8478127238908,
78.2872967474258));
#157652=CARTESIAN_POINT('Ctrl Pts',(35.4862143351102,-13.8109237809282,
78.3589158860956));
#157653=CARTESIAN_POINT('Ctrl Pts',(35.590733009388,-13.7747236149353,78.4299822582505));
#157654=CARTESIAN_POINT('Ctrl Pts',(35.6808630807593,-13.7397101095713,
78.4991751650237));
#157655=CARTESIAN_POINT('Ctrl Pts',(35.7579171333831,-13.7063530796802,
78.5653476617595));
#157656=CARTESIAN_POINT('Ctrl Pts',(35.8232187425314,-13.6750153646781,
78.6276488136447));
#157657=CARTESIAN_POINT('Ctrl Pts',(35.8781479447624,-13.6459257565499,
78.6855511294384));
#157658=CARTESIAN_POINT('Ctrl Pts',(35.9239726936212,-13.6191899326575,
78.7387922454918));
#157659=CARTESIAN_POINT('Ctrl Pts',(35.9617901538152,-13.5948848845966,
78.7872092453676));
#157660=CARTESIAN_POINT('Ctrl Pts',(35.9890440080014,-13.5755567654701,
78.825728205213));
#157661=CARTESIAN_POINT('Ctrl Pts',(36.0033566791772,-13.5645406906742,
78.847695086863));
#157662=CARTESIAN_POINT('Ctrl Pts',(36.0083664878408,-13.5605601040526,
78.855634972008));
#157663=CARTESIAN_POINT('Ctrl Pts',(33.7098713669441,-14.2651297534302,
77.738616182356));
#157664=CARTESIAN_POINT('Ctrl Pts',(33.7652791838108,-14.2652746724941,
77.7283917307582));
#157665=CARTESIAN_POINT('Ctrl Pts',(33.9290623283902,-14.2640332999716,
77.7033975118487));
#157666=CARTESIAN_POINT('Ctrl Pts',(34.1929785744821,-14.2542616178001,
77.6874861366232));
#157667=CARTESIAN_POINT('Ctrl Pts',(34.4891855565944,-14.2322924438966,
77.7032331310642));
#157668=CARTESIAN_POINT('Ctrl Pts',(34.7536256962505,-14.2033839164636,
77.7444596746802));
#157669=CARTESIAN_POINT('Ctrl Pts',(34.9880716473297,-14.1697073341032,
77.8033262526759));
#157670=CARTESIAN_POINT('Ctrl Pts',(35.1948810444306,-14.1329210158518,
77.8738550465823));
#157671=CARTESIAN_POINT('Ctrl Pts',(35.376670559523,-14.0942867264955,77.9515757927416));
#157672=CARTESIAN_POINT('Ctrl Pts',(35.5360948856724,-14.05475850672,78.0332008651507));
#157673=CARTESIAN_POINT('Ctrl Pts',(35.6757394068685,-14.0150260502892,
78.1164096768387));
#157674=CARTESIAN_POINT('Ctrl Pts',(35.7977824483,-13.9756411113113,78.1994722424931));
#157675=CARTESIAN_POINT('Ctrl Pts',(35.903940888504,-13.9371184259179,78.2809425578672));
#157676=CARTESIAN_POINT('Ctrl Pts',(35.9956318025583,-13.8999610119654,
78.3595434745583));
#157677=CARTESIAN_POINT('Ctrl Pts',(36.0742649614256,-13.8645728621217,
78.4343099401369));
#157678=CARTESIAN_POINT('Ctrl Pts',(36.1412930269105,-13.8312361404342,
78.5046020922704));
#157679=CARTESIAN_POINT('Ctrl Pts',(36.1982698210819,-13.8000075196721,
78.5703016764263));
#157680=CARTESIAN_POINT('Ctrl Pts',(36.2464106531869,-13.7709569337502,
78.6312931394323));
#157681=CARTESIAN_POINT('Ctrl Pts',(36.2821732309277,-13.747181853896,78.6811264949467));
#157682=CARTESIAN_POINT('Ctrl Pts',(36.3015404153484,-13.7332339834193,
78.7103362616371));
#157683=CARTESIAN_POINT('Ctrl Pts',(36.3084139439587,-13.7281272594451,
78.7210288249536));
#157684=CARTESIAN_POINT('Ctrl Pts',(33.646793935444,-14.3652713150121,77.3964138987276));
#157685=CARTESIAN_POINT('Ctrl Pts',(33.709120380352,-14.3654194049986,77.3849150787496));
#157686=CARTESIAN_POINT('Ctrl Pts',(33.8933318204112,-14.3641498743635,
77.3567847235416));
#157687=CARTESIAN_POINT('Ctrl Pts',(34.1900910923022,-14.3541634210384,
77.3387423942183));
#157688=CARTESIAN_POINT('Ctrl Pts',(34.5232230536664,-14.3316474620846,
77.3561158445656));
#157689=CARTESIAN_POINT('Ctrl Pts',(34.8208682377197,-14.3018890672365,
77.4020775669144));
#157690=CARTESIAN_POINT('Ctrl Pts',(35.0851373959727,-14.2670310129054,
77.467912837115));
#157691=CARTESIAN_POINT('Ctrl Pts',(35.3187487836197,-14.228712518735,77.5470003753656));
#157692=CARTESIAN_POINT('Ctrl Pts',(35.5246677233139,-14.1881886671558,
77.6344029014632));
#157693=CARTESIAN_POINT('Ctrl Pts',(35.705880046119,-14.1464160555454,77.7265005683826));
#157694=CARTESIAN_POINT('Ctrl Pts',(35.8653180087285,-14.1040816146407,
77.8207704981658));
#157695=CARTESIAN_POINT('Ctrl Pts',(36.0054246676531,-14.0617395550477,
77.9153426786752));
#157696=CARTESIAN_POINT('Ctrl Pts',(36.1280963134294,-14.0199176941972,
78.0086507860051));
#157697=CARTESIAN_POINT('Ctrl Pts',(36.2348603836339,-13.9791491053273,
78.0992914480622));
#157698=CARTESIAN_POINT('Ctrl Pts',(36.3272175105147,-13.9398768718413,
78.186187496645));
#157699=CARTESIAN_POINT('Ctrl Pts',(36.4066966204188,-13.9024358806681,
78.2685860724393));
#157700=CARTESIAN_POINT('Ctrl Pts',(36.4751484961417,-13.8668317505958,
78.3465160194065));
#157701=CARTESIAN_POINT('Ctrl Pts',(36.5339111440086,-13.8331265451538,
78.4199097088141));
#157702=CARTESIAN_POINT('Ctrl Pts',(36.5784286736335,-13.8049608162598,
78.4809554358667));
#157703=CARTESIAN_POINT('Ctrl Pts',(36.6029969258144,-13.7881038093459,
78.5173702609838));
#157704=CARTESIAN_POINT('Ctrl Pts',(36.61178827325,-13.7818775502543,78.5308052276326));
#157705=CARTESIAN_POINT('Origin',(35.6454492392491,0.499074165591614,72.5830523519042));
#157706=CARTESIAN_POINT('Origin',(82.8534541851791,15.33010667085,62.64107301909));
#157707=CARTESIAN_POINT('Ctrl Pts',(65.6493476995291,-7.55647811801299,
66.484406505602));
#157708=CARTESIAN_POINT('Ctrl Pts',(65.6977795012391,-7.61087860031499,
66.475866672236));
#157709=CARTESIAN_POINT('Ctrl Pts',(65.8511840174591,-7.78393516119298,
66.448817317063));
#157710=CARTESIAN_POINT('Ctrl Pts',(66.1061821657891,-8.07036067158899,
66.403854263482));
#157711=CARTESIAN_POINT('Ctrl Pts',(66.4160097536291,-8.400411439295,66.349223300379));
#157712=CARTESIAN_POINT('Ctrl Pts',(66.7163050559491,-8.69402671421799,
66.296273136399));
#157713=CARTESIAN_POINT('Ctrl Pts',(67.0055863725391,-8.95024991713399,
66.245265035269));
#157714=CARTESIAN_POINT('Ctrl Pts',(67.2020307421891,-9.10615845958399,
66.210626592692));
#157715=CARTESIAN_POINT('Ctrl Pts',(67.2981630439992,-9.17825162599699,
66.193675874165));
#157716=CARTESIAN_POINT('Ctrl Pts',(67.2997288353791,-9.17942477180599,
66.193399782899));
#157717=CARTESIAN_POINT('Ctrl Pts',(65.2976696808791,-7.73950995723499,
65.656652656171));
#157718=CARTESIAN_POINT('Ctrl Pts',(65.3458411451991,-7.79361760798199,
65.648158727311));
#157719=CARTESIAN_POINT('Ctrl Pts',(65.4990058852991,-7.96639406115299,
65.621151651139));
#157720=CARTESIAN_POINT('Ctrl Pts',(65.7563586217791,-8.255493936528,65.575773420139));
#157721=CARTESIAN_POINT('Ctrl Pts',(66.072576141859,-8.592419041958,65.520015739575));
#157722=CARTESIAN_POINT('Ctrl Pts',(66.3821225145791,-8.89513157016199,
65.465434362284));
#157723=CARTESIAN_POINT('Ctrl Pts',(66.6817222931791,-9.16053014774899,
65.412606837902));
#157724=CARTESIAN_POINT('Ctrl Pts',(66.8863394401191,-9.32293981017799,
65.376527314182));
#157725=CARTESIAN_POINT('Ctrl Pts',(66.9862719124592,-9.39788123282599,
65.3589065230591));
#157726=CARTESIAN_POINT('Ctrl Pts',(66.9878995464891,-9.39910068191699,
65.358619527265));
#157727=CARTESIAN_POINT('Ctrl Pts',(65.6592224440491,-7.30445217689799,
64.933904240298));
#157728=CARTESIAN_POINT('Ctrl Pts',(65.7080127176891,-7.35925587400999,
64.9253011986599));
#157729=CARTESIAN_POINT('Ctrl Pts',(65.8617473939792,-7.53269812957599,
64.898193627359));
#157730=CARTESIAN_POINT('Ctrl Pts',(66.1135033889391,-7.81544116946099,
64.853802252892));
#157731=CARTESIAN_POINT('Ctrl Pts',(66.4145323508291,-8.13602630844498,
64.8007227249361));
#157732=CARTESIAN_POINT('Ctrl Pts',(66.7020893791291,-8.41711510803199,
64.750018662355));
#157733=CARTESIAN_POINT('Ctrl Pts',(66.9771626753591,-8.66070426625799,
64.7015158185569));
#157734=CARTESIAN_POINT('Ctrl Pts',(67.1623535281491,-8.80766108266999,
64.66886167463));
#157735=CARTESIAN_POINT('Ctrl Pts',(67.2532531799491,-8.87583233876699,
64.65283361348));
#157736=CARTESIAN_POINT('Ctrl Pts',(67.2547338170091,-8.87694172720999,
64.652572537217));
#157737=CARTESIAN_POINT('Ctrl Pts',(66.3469619223191,-6.71703633739999,
65.089867102845));
#157738=CARTESIAN_POINT('Ctrl Pts',(66.3965877134691,-6.77277983763399,
65.0811167369271));
#157739=CARTESIAN_POINT('Ctrl Pts',(66.5510919186892,-6.94712106085499,
65.0538734769131));
#157740=CARTESIAN_POINT('Ctrl Pts',(66.7952911826491,-7.22128108941499,
65.010814558009));
#157741=CARTESIAN_POINT('Ctrl Pts',(67.0758125244791,-7.51980397473499,
64.961351076778));
#157742=CARTESIAN_POINT('Ctrl Pts',(67.3336794982692,-7.77169637496499,
64.915882171866));
#157743=CARTESIAN_POINT('Ctrl Pts',(67.5756370915191,-7.98583841383899,
64.873218519988));
#157744=CARTESIAN_POINT('Ctrl Pts',(67.7345985251391,-8.11193076827299,
64.845189330349));
#157745=CARTESIAN_POINT('Ctrl Pts',(67.8133020455291,-8.17096093266299,
64.831311776228));
#157746=CARTESIAN_POINT('Ctrl Pts',(67.8145842070092,-8.17192171701199,
64.831085696565));
#157747=CARTESIAN_POINT('Origin',(82.0934733297391,-9.38083151964699,58.3310074104));
#157748=CARTESIAN_POINT('Ctrl Pts',(83.9305070695251,-8.35425122912034,
62.451223254077));
#157749=CARTESIAN_POINT('Ctrl Pts',(83.9721096129046,-8.41502174878494,
62.3585397890282));
#157750=CARTESIAN_POINT('Ctrl Pts',(84.009290601372,-8.48362968832864,62.2534751356656));
#157751=CARTESIAN_POINT('Ctrl Pts',(84.0547015692346,-8.59871915493393,
62.0779605492143));
#157752=CARTESIAN_POINT('Ctrl Pts',(84.0681049073854,-8.63910401461063,
62.0164686566902));
#157753=CARTESIAN_POINT('Ctrl Pts',(84.0850836244519,-8.70266714380778,
61.9198461905371));
#157754=CARTESIAN_POINT('Ctrl Pts',(84.0927908839831,-8.73519400778358,
61.8704388934484));
#157755=CARTESIAN_POINT('Ctrl Pts',(84.1002942620877,-8.77442340519883,
61.8109000502313));
#157756=CARTESIAN_POINT('Ctrl Pts',(84.103658570228,-8.7943545318876,61.7806590728184));
#157757=CARTESIAN_POINT('Ctrl Pts',(84.1050157653578,-8.80296380107318,
61.767597895611));
#157758=CARTESIAN_POINT('Ctrl Pts',(84.1059015676795,-8.80871822946449,
61.7588680856792));
#157759=CARTESIAN_POINT('Ctrl Pts',(84.1064768697166,-8.8125712101865,61.7530231017033));
#157760=CARTESIAN_POINT('Ctrl Pts',(84.1157801312426,-8.87605641934299,
61.6567176345016));
#157761=CARTESIAN_POINT('Ctrl Pts',(84.1223566595417,-8.95342740610009,
61.5385628860497));
#157762=CARTESIAN_POINT('Ctrl Pts',(84.1160489550679,-9.14217474627203,
61.2552874147842));
#157763=CARTESIAN_POINT('Ctrl Pts',(84.103128596185,-9.25373486147343,61.0901730619785));
#157764=CARTESIAN_POINT('Ctrl Pts',(84.0701935481991,-9.38083151964699,
60.90338912307));
#157765=CARTESIAN_POINT('Ctrl Pts',(84.007342440529,-8.34113792735099,62.7303651543501));
#157766=CARTESIAN_POINT('Ctrl Pts',(84.0935574097791,-8.41594609712799,
62.69053588541));
#157767=CARTESIAN_POINT('Ctrl Pts',(84.2989240749091,-8.61704513668698,
62.57230781918));
#157768=CARTESIAN_POINT('Ctrl Pts',(84.5872966976591,-8.99415052088398,
62.31565721301));
#157769=CARTESIAN_POINT('Ctrl Pts',(84.8429254664791,-9.48340020843898,
61.94261309465));
#157770=CARTESIAN_POINT('Ctrl Pts',(84.9636036434391,-9.88804177715397,
61.60883124012));
#157771=CARTESIAN_POINT('Ctrl Pts',(85.000589857989,-10.12788821405,61.40365053913));
#157772=CARTESIAN_POINT('Ctrl Pts',(85.0065710147491,-10.17521122351,61.36296841404));
#157773=CARTESIAN_POINT('Ctrl Pts',(83.6034848088291,-8.23953217489199,
62.25272764276));
#157774=CARTESIAN_POINT('Ctrl Pts',(83.6622877099991,-8.31654637346699,
62.23557356992));
#157775=CARTESIAN_POINT('Ctrl Pts',(83.8066016022891,-8.52254556916299,
62.17796180608));
#157776=CARTESIAN_POINT('Ctrl Pts',(84.0209884017891,-8.90514749704598,
62.03256168289));
#157777=CARTESIAN_POINT('Ctrl Pts',(84.2246311003191,-9.39808266510199,
61.80143661051));
#157778=CARTESIAN_POINT('Ctrl Pts',(84.3331361822591,-9.80365235625799,
61.58278472916));
#157779=CARTESIAN_POINT('Ctrl Pts',(84.3737914439991,-10.04335797538,61.44473164379));
#157780=CARTESIAN_POINT('Ctrl Pts',(84.3809019086191,-10.09062139715,61.41723307588));
#157781=CARTESIAN_POINT('Ctrl Pts',(83.5888040753991,-7.80219022690399,
61.79433169008));
#157782=CARTESIAN_POINT('Ctrl Pts',(83.6280925122191,-7.88869984191799,
61.7686511776601));
#157783=CARTESIAN_POINT('Ctrl Pts',(83.7184869065591,-8.115790794511,61.69745538176));
#157784=CARTESIAN_POINT('Ctrl Pts',(83.8365843313791,-8.52205151202899,
61.55819868633));
#157785=CARTESIAN_POINT('Ctrl Pts',(83.9310436648091,-9.03085010496399,
61.3706688459801));
#157786=CARTESIAN_POINT('Ctrl Pts',(83.9663332001091,-9.44041471634899,
61.21179100688));
#157787=CARTESIAN_POINT('Ctrl Pts',(83.9715830565591,-9.67951421307999,
61.11686765514));
#157788=CARTESIAN_POINT('Ctrl Pts',(83.9720288907591,-9.72652115139598,
61.09814164466));
#157789=CARTESIAN_POINT('Ctrl Pts',(83.9729708222391,-7.31720063036999,
61.65713466525));
#157790=CARTESIAN_POINT('Ctrl Pts',(84.0134970850191,-7.41424017101399,
61.59734266571));
#157791=CARTESIAN_POINT('Ctrl Pts',(84.092623435809,-7.66472079092699,61.44731065951));
#157792=CARTESIAN_POINT('Ctrl Pts',(84.155556256859,-8.09721788227599,61.2050435005));
#157793=CARTESIAN_POINT('Ctrl Pts',(84.1555568604491,-8.62360819278299,
60.93406776197));
#157794=CARTESIAN_POINT('Ctrl Pts',(84.1048173875391,-9.03760296404499,
60.74023331364));
#157795=CARTESIAN_POINT('Ctrl Pts',(84.0589098500391,-9.27603030239999,
60.63603113317));
#157796=CARTESIAN_POINT('Ctrl Pts',(84.049287281419,-9.32275281383199,60.61588796801));
#157797=CARTESIAN_POINT('Origin',(63.4339821949991,0.499074165591614,67.683184237498));
#157798=CARTESIAN_POINT('Origin',(91.5481551204691,-0.0433423696914658,
83.15731994474));
#157799=CARTESIAN_POINT('Ctrl Pts',(87.0625396169313,9.81028965175084,57.7179144389336));
#157800=CARTESIAN_POINT('Ctrl Pts',(86.9560129494815,9.81043336279731,57.7361359393653));
#157801=CARTESIAN_POINT('Ctrl Pts',(86.8423970449262,9.80410270209386,57.7731105945253));
#157802=CARTESIAN_POINT('Ctrl Pts',(86.6235573133266,9.77319335733451,57.8940860262539));
#157803=CARTESIAN_POINT('Ctrl Pts',(86.5188898025592,9.7484075770056,57.9785392281757));
#157804=CARTESIAN_POINT('Ctrl Pts',(86.3506421598397,9.68141743769284,58.1865038597519));
#157805=CARTESIAN_POINT('Ctrl Pts',(86.2879257990702,9.63930718845491,58.3096128797123));
#157806=CARTESIAN_POINT('Ctrl Pts',(86.222153236433,9.54815442195098,58.5637415305018));
#157807=CARTESIAN_POINT('Ctrl Pts',(86.2190078227482,9.49946000046106,58.6938516074194));
#157808=CARTESIAN_POINT('Ctrl Pts',(86.2399778829169,9.45364604184037,58.8119255183517));
#157809=CARTESIAN_POINT('Ctrl Pts',(87.3207027298691,3.13362000020301,55.34789324766));
#157810=CARTESIAN_POINT('Ctrl Pts',(87.325235904929,3.72414610022402,55.47809510729));
#157811=CARTESIAN_POINT('Ctrl Pts',(87.3354008992691,4.83285818851802,55.7901515622));
#157812=CARTESIAN_POINT('Ctrl Pts',(87.3490222678991,6.36326886928801,56.3467657865));
#157813=CARTESIAN_POINT('Ctrl Pts',(87.358579219789,7.71653928886002,56.89258275411));
#157814=CARTESIAN_POINT('Ctrl Pts',(87.3636142925891,8.88581650983902,57.36610360856));
#157815=CARTESIAN_POINT('Ctrl Pts',(87.3634445492491,9.61075958397102,57.64159291478));
#157816=CARTESIAN_POINT('Ctrl Pts',(87.3624396251191,9.93428100300701,57.75825728172));
#157817=CARTESIAN_POINT('Ctrl Pts',(86.2613172939992,3.33310591270701,54.71370312083));
#157818=CARTESIAN_POINT('Ctrl Pts',(86.2511508016791,3.95136525321801,54.87718011019));
#157819=CARTESIAN_POINT('Ctrl Pts',(86.2276527558891,5.09342510158102,55.26541508777));
#157820=CARTESIAN_POINT('Ctrl Pts',(86.1907592952991,6.61840325577501,55.94310458405));
#157821=CARTESIAN_POINT('Ctrl Pts',(86.1610107349092,7.93502804762402,56.59794889373));
#157822=CARTESIAN_POINT('Ctrl Pts',(86.1403419786992,9.05776198640001,57.16244255609));
#157823=CARTESIAN_POINT('Ctrl Pts',(86.1292733867091,9.75138372308601,57.49279715768));
#157824=CARTESIAN_POINT('Ctrl Pts',(86.1244212943492,10.06113013545,57.63371115991));
#157825=CARTESIAN_POINT('Ctrl Pts',(85.3372217806292,3.17169945627801,55.54091804455));
#157826=CARTESIAN_POINT('Ctrl Pts',(85.3463626117991,3.75698441837301,55.7195292026701));
#157827=CARTESIAN_POINT('Ctrl Pts',(85.3702987241291,4.83618885125201,56.14247256533));
#157828=CARTESIAN_POINT('Ctrl Pts',(85.4259847846291,6.28522424215701,56.87789547744));
#157829=CARTESIAN_POINT('Ctrl Pts',(85.4947450446091,7.55724130294601,57.58893555709));
#157830=CARTESIAN_POINT('Ctrl Pts',(85.5664123570691,8.66907253684701,58.20510965777));
#157831=CARTESIAN_POINT('Ctrl Pts',(85.6142557518591,9.37232556154801,58.56812537839));
#157832=CARTESIAN_POINT('Ctrl Pts',(85.6357422321091,9.68980400619803,58.7234820586301));
#157833=CARTESIAN_POINT('Ctrl Pts',(85.897825663029,2.88509423422901,56.62159832173));
#157834=CARTESIAN_POINT('Ctrl Pts',(85.9320873103392,3.42484799939702,56.77510303408));
#157835=CARTESIAN_POINT('Ctrl Pts',(86.0152891009691,4.43677839367301,57.1406017625));
#157836=CARTESIAN_POINT('Ctrl Pts',(86.1714598873992,5.85025612247802,57.78611107631));
#157837=CARTESIAN_POINT('Ctrl Pts',(86.3326959020691,7.13484173987302,58.41845554155));
#157838=CARTESIAN_POINT('Ctrl Pts',(86.4799055365392,8.28733150922102,58.97155140682));
#157839=CARTESIAN_POINT('Ctrl Pts',(86.5704455885891,9.02710436949802,59.29733070642));
#157840=CARTESIAN_POINT('Ctrl Pts',(86.6099955101491,9.36253119362102,59.43623320246));
#157841=CARTESIAN_POINT('Ctrl Pts',(87.0452039026617,3.32467973944959,55.2706236824217));
#157842=CARTESIAN_POINT('Ctrl Pts',(87.0158957985298,3.32776504208187,55.2636439986755));
#157843=CARTESIAN_POINT('Ctrl Pts',(86.9855492369739,3.33060899420873,55.2577943865739));
#157844=CARTESIAN_POINT('Ctrl Pts',(86.954273199712,3.33315210107447,55.2532910470087));
#157845=CARTESIAN_POINT('Ctrl Pts',(86.9240766939803,3.3356074294271,55.248943145839));
#157846=CARTESIAN_POINT('Ctrl Pts',(86.8930137891819,3.33778213321698,55.2458509258659));
#157847=CARTESIAN_POINT('Ctrl Pts',(86.8612303516663,3.33962200565783,55.2442031639726));
#157848=CARTESIAN_POINT('Ctrl Pts',(86.8300187823837,3.34142877391977,55.2425850496806));
#157849=CARTESIAN_POINT('Ctrl Pts',(86.7981124841258,3.34291245168442,55.2423606500344));
#157850=CARTESIAN_POINT('Ctrl Pts',(86.7656957486977,3.34402389978898,55.2436919623959));
#157851=CARTESIAN_POINT('Ctrl Pts',(86.7340599142816,3.3451085737308,55.2449912041878));
#157852=CARTESIAN_POINT('Ctrl Pts',(86.701938312397,3.3458385465234,55.2477727877885));
#157853=CARTESIAN_POINT('Ctrl Pts',(86.6695429664898,3.34617310499231,55.2521605662374));
#157854=CARTESIAN_POINT('Ctrl Pts',(86.6391263937711,3.34648722795391,55.2562803303124));
#157855=CARTESIAN_POINT('Ctrl Pts',(86.6084691690557,3.34645266903372,55.2618163294321));
#157856=CARTESIAN_POINT('Ctrl Pts',(86.5777752292993,3.34604211469778,55.2688409060828));
#157857=CARTESIAN_POINT('Ctrl Pts',(86.5459495982834,3.34561642314723,55.2761244801794));
#157858=CARTESIAN_POINT('Ctrl Pts',(86.5140851157249,3.34478628831945,55.2850091585276));
#157859=CARTESIAN_POINT('Ctrl Pts',(86.4824330539896,3.3435306994631,55.2955334219386));
#157860=CARTESIAN_POINT('Ctrl Pts',(86.4511198312397,3.34228855183082,55.3059450218913));
#157861=CARTESIAN_POINT('Ctrl Pts',(86.4200153076962,3.34062990468923,55.3179615663613));
#157862=CARTESIAN_POINT('Ctrl Pts',(86.3893759355848,3.33854598242068,55.3315724121411));
#157863=CARTESIAN_POINT('Ctrl Pts',(86.3590494891505,3.3364833436427,55.34504424779));
#157864=CARTESIAN_POINT('Ctrl Pts',(86.3291795977555,3.33400402460446,55.3600780218181));
#157865=CARTESIAN_POINT('Ctrl Pts',(86.3000155403359,3.33111205258089,55.3766139078715));
#157866=CARTESIAN_POINT('Ctrl Pts',(86.2709862787503,3.32823344720845,55.3930733653087));
#157867=CARTESIAN_POINT('Ctrl Pts',(86.242657192776,3.32494599924483,55.4110209129365));
#157868=CARTESIAN_POINT('Ctrl Pts',(86.2152619343509,3.32126650475866,55.4303491660492));
#157869=CARTESIAN_POINT('Ctrl Pts',(86.1879315787459,3.31759572745868,55.4496316280941));
#157870=CARTESIAN_POINT('Ctrl Pts',(86.1615314102079,3.31353482388904,55.4702878684087));
#157871=CARTESIAN_POINT('Ctrl Pts',(86.1362689969526,3.30911274928937,55.4921671897273));
#157872=CARTESIAN_POINT('Ctrl Pts',(86.1281989003645,3.30770011428974,55.4991565550956));
#157873=CARTESIAN_POINT('Ctrl Pts',(86.1202446763264,3.30625071155674,55.5062704236528));
#157874=CARTESIAN_POINT('Ctrl Pts',(86.1124123761509,3.30476572772039,55.5135030525225));
#157875=CARTESIAN_POINT('Ctrl Pts',(86.0878456929179,3.30010794817974,55.5361888151211));
#157876=CARTESIAN_POINT('Ctrl Pts',(86.0644816855133,3.29509940836546,55.5600451696905));
#157877=CARTESIAN_POINT('Ctrl Pts',(86.042480546915,3.28978327466456,55.584873701666));
#157878=CARTESIAN_POINT('Ctrl Pts',(86.020389922166,3.28444551843085,55.6098032197674));
#157879=CARTESIAN_POINT('Ctrl Pts',(85.9996736672954,3.27879783898094,55.6357120694331));
#157880=CARTESIAN_POINT('Ctrl Pts',(85.9804477687263,3.27289200124217,55.6623757495974));
#157881=CARTESIAN_POINT('Ctrl Pts',(85.9609988972839,3.26691767039216,55.689348662506));
#157882=CARTESIAN_POINT('Ctrl Pts',(85.9430753564791,3.26067936348671,55.7170931720327));
#157883=CARTESIAN_POINT('Ctrl Pts',(85.9267454044346,3.25423600214559,55.7453649914734));
#157884=CARTESIAN_POINT('Ctrl Pts',(85.9102838611362,3.24774071842311,55.7738646330263));
#157885=CARTESIAN_POINT('Ctrl Pts',(85.8954416007959,3.24103728370016,55.8028992605736));
#157886=CARTESIAN_POINT('Ctrl Pts',(85.8822353778661,3.23418818270307,55.8322196284447));
#157887=CARTESIAN_POINT('Ctrl Pts',(85.8688229092946,3.22723211719102,55.8619979015108));
#157888=CARTESIAN_POINT('Ctrl Pts',(85.857097692062,3.22012601782691,55.8920701018972));
#157889=CARTESIAN_POINT('Ctrl Pts',(85.8470254504323,3.21293416110448,55.9221889194256));
#157890=CARTESIAN_POINT('Ctrl Pts',(85.8443086057684,3.21099425951367,55.9303130442924));
#157891=CARTESIAN_POINT('Ctrl Pts',(85.8417117555785,3.20904810176126,55.9384406745451));
#157892=CARTESIAN_POINT('Ctrl Pts',(85.8392336483774,3.20709690456849,55.9465672349548));
#157893=CARTESIAN_POINT('Ctrl Pts',(85.8298346306164,3.19969636230698,55.9773898263238));
#157894=CARTESIAN_POINT('Ctrl Pts',(85.8221469851188,3.19222381292407,56.0081944884238));
#157895=CARTESIAN_POINT('Ctrl Pts',(85.8160748683465,3.18474201124346,56.0387512009237));
#157896=CARTESIAN_POINT('Ctrl Pts',(85.8098131955518,3.17702664676749,56.0702618161722));
#157897=CARTESIAN_POINT('Ctrl Pts',(85.8052688157992,3.16930161800696,56.1015081902615));
#157898=CARTESIAN_POINT('Ctrl Pts',(85.802298117403,3.16162730259475,56.1322781164847));
#157899=CARTESIAN_POINT('Ctrl Pts',(85.799273347267,3.15381330165044,56.1636081074546));
#157900=CARTESIAN_POINT('Ctrl Pts',(85.7978792042002,3.14605197890152,56.1944438989833));
#157901=CARTESIAN_POINT('Ctrl Pts',(85.7979368396176,3.13839632796352,56.224608603399));
#157902=CARTESIAN_POINT('Ctrl Pts',(85.7979964570438,3.13047740890124,56.2558106337346));
#157903=CARTESIAN_POINT('Ctrl Pts',(85.7996085440693,3.12267162815719,56.2862944915633));
#157904=CARTESIAN_POINT('Ctrl Pts',(85.8025597451988,3.11502482592699,56.3159175912647));
#157905=CARTESIAN_POINT('Ctrl Pts',(85.8049366353535,3.10886611015733,56.3397759631416));
#157906=CARTESIAN_POINT('Ctrl Pts',(85.8081817163382,3.10281025135304,56.3630771210913));
#157907=CARTESIAN_POINT('Ctrl Pts',(85.8121821974198,3.09687523453361,56.385770301083));
#157908=CARTESIAN_POINT('Ctrl Pts',(87.3066738932391,-0.160558520523986,
54.99748094861));
#157909=CARTESIAN_POINT('Ctrl Pts',(87.3057973027491,0.222559046269814,
54.9925095569101));
#157910=CARTESIAN_POINT('Ctrl Pts',(87.3104980049391,1.01336829601901,55.01916856379));
#157911=CARTESIAN_POINT('Ctrl Pts',(87.3376450103591,2.21501333732301,55.17312688208));
#157912=CARTESIAN_POINT('Ctrl Pts',(87.3692248653891,3.02064717406401,55.35222513978));
#157913=CARTESIAN_POINT('Ctrl Pts',(87.3880905029791,3.42517613974502,55.45921748724));
#157914=CARTESIAN_POINT('Ctrl Pts',(86.2302484602191,-0.172977764866286,
54.23064612836));
#157915=CARTESIAN_POINT('Ctrl Pts',(86.2293040482491,0.239788826433014,
54.22529010194));
#157916=CARTESIAN_POINT('Ctrl Pts',(86.234373747229,1.09161263914201,54.25404179361));
#157917=CARTESIAN_POINT('Ctrl Pts',(86.2635437845591,2.38161775413201,54.41947329601));
#157918=CARTESIAN_POINT('Ctrl Pts',(86.2972481600892,3.24065865070901,54.6106203082));
#157919=CARTESIAN_POINT('Ctrl Pts',(86.3172509644792,3.66957413486501,54.72406184906));
#157920=CARTESIAN_POINT('Ctrl Pts',(85.2315241728891,-0.164025917707086,
55.09629689782));
#157921=CARTESIAN_POINT('Ctrl Pts',(85.2306286469491,0.227369523425714,
55.09121811783));
#157922=CARTESIAN_POINT('Ctrl Pts',(85.2354323713891,1.03521376483001,55.1184613929));
#157923=CARTESIAN_POINT('Ctrl Pts',(85.2631441982191,2.26152854143701,55.27562297261));
#157924=CARTESIAN_POINT('Ctrl Pts',(85.2953172098191,3.08207338916501,55.45808518839));
#157925=CARTESIAN_POINT('Ctrl Pts',(85.314500339269,3.49341096116101,55.56687812165));
#157926=CARTESIAN_POINT('Ctrl Pts',(85.837848582719,-0.147393025451686,
56.27059483639));
#157927=CARTESIAN_POINT('Ctrl Pts',(85.8370438889791,0.204293958669714,
56.26603119144));
#157928=CARTESIAN_POINT('Ctrl Pts',(85.8413534220091,0.930422386796514,
56.29047176775));
#157929=CARTESIAN_POINT('Ctrl Pts',(85.8663558350591,2.03839795170801,56.43226749832));
#157930=CARTESIAN_POINT('Ctrl Pts',(85.8956835108491,2.78741559154501,56.59859301288));
#157931=CARTESIAN_POINT('Ctrl Pts',(85.9133436512691,3.16609269539302,56.69874864616));
#157932=CARTESIAN_POINT('Origin',(86.7262508506842,-3.18494591445562E-7,
55.8108970052131));
#157933=CARTESIAN_POINT('Ctrl Pts',(87.3881016241291,-3.42500607027599,
55.45920812828));
#157934=CARTESIAN_POINT('Ctrl Pts',(87.3689745152091,-3.01484055255599,
55.35073290318));
#157935=CARTESIAN_POINT('Ctrl Pts',(87.3372398307191,-2.20322903616999,
55.17075656397));
#157936=CARTESIAN_POINT('Ctrl Pts',(87.3103828227291,-1.00133939355599,
55.01844290285));
#157937=CARTESIAN_POINT('Ctrl Pts',(87.3058297848591,-0.216519809292486,
54.99262134195));
#157938=CARTESIAN_POINT('Ctrl Pts',(87.3066901921091,0.160504427251014,
54.99750095394));
#157939=CARTESIAN_POINT('Ctrl Pts',(86.3172693262291,-3.66938489029899,
54.72402342508));
#157940=CARTESIAN_POINT('Ctrl Pts',(86.2969910364991,-3.23453191356599,
54.60901952918));
#157941=CARTESIAN_POINT('Ctrl Pts',(86.2631186790491,-2.36907727584199,
54.41691984417));
#157942=CARTESIAN_POINT('Ctrl Pts',(86.2342558402292,-1.07862444435799,
54.25323055111));
#157943=CARTESIAN_POINT('Ctrl Pts',(86.2293462065792,-0.233245776100886,
54.22538663505));
#157944=CARTESIAN_POINT('Ctrl Pts',(86.2302729794091,0.172898711608914,
54.23064262496));
#157945=CARTESIAN_POINT('Ctrl Pts',(85.3145018225292,-3.49324296266999,
55.56683463126));
#157946=CARTESIAN_POINT('Ctrl Pts',(85.295053274129,-3.07618406734899,55.45653643227));
#157947=CARTESIAN_POINT('Ctrl Pts',(85.262721696009,-2.24953815773399,55.2731749411));
#157948=CARTESIAN_POINT('Ctrl Pts',(85.2353046081391,-1.02291938029399,
55.11768490907));
#157949=CARTESIAN_POINT('Ctrl Pts',(85.2306519994892,-0.221190132183786,
55.09129865426));
#157950=CARTESIAN_POINT('Ctrl Pts',(85.2315309377292,0.163965232274714,
55.09628336072));
#157951=CARTESIAN_POINT('Ctrl Pts',(85.9133362962291,-3.16595498744899,
56.69872650143));
#157952=CARTESIAN_POINT('Ctrl Pts',(85.895429483869,-2.78195913937999,56.59717192208));
#157953=CARTESIAN_POINT('Ctrl Pts',(85.8659608161091,-2.02742343211599,
56.43004680237));
#157954=CARTESIAN_POINT('Ctrl Pts',(85.841230067059,-0.919414224694086,
56.28979175488));
#157955=CARTESIAN_POINT('Ctrl Pts',(85.837055034629,-0.198789631969386,
56.26611396935));
#157956=CARTESIAN_POINT('Ctrl Pts',(85.8378450917691,0.147366002311014,
56.27059460606));
#157957=CARTESIAN_POINT('Ctrl Pts',(87.0452086535361,-3.32464023403444,
55.2705714208367));
#157958=CARTESIAN_POINT('Ctrl Pts',(87.0161338191475,-3.32769428602402,
55.2636452372544));
#157959=CARTESIAN_POINT('Ctrl Pts',(86.9860064240394,-3.33051660652347,
55.2578243001712));
#157960=CARTESIAN_POINT('Ctrl Pts',(86.9549270148153,-3.33304666480274,
55.2533279251216));
#157961=CARTESIAN_POINT('Ctrl Pts',(86.9249635095899,-3.33548588151774,
55.2489929921014));
#157962=CARTESIAN_POINT('Ctrl Pts',(86.8941151025206,-3.33765326081566,
55.245889948207));
#157963=CARTESIAN_POINT('Ctrl Pts',(86.8625197855615,-3.33949324230545,
55.2442120543826));
#157964=CARTESIAN_POINT('Ctrl Pts',(86.8315197407038,-3.34129855759298,
55.242565772945));
#157965=CARTESIAN_POINT('Ctrl Pts',(86.7998007206826,-3.34278849749598,
55.2422922168608));
#157966=CARTESIAN_POINT('Ctrl Pts',(86.7675399999893,-3.34391209160149,
55.2435596897975));
#157967=CARTESIAN_POINT('Ctrl Pts',(86.736097421926,-3.34500719098597,55.2447950191981));
#157968=CARTESIAN_POINT('Ctrl Pts',(86.7041405970569,-3.34575409864029,
55.2474949039633));
#157969=CARTESIAN_POINT('Ctrl Pts',(86.6718757613232,-3.34610992515415,
55.2517907778763));
#157970=CARTESIAN_POINT('Ctrl Pts',(86.6430925422921,-3.34642735533015,
55.255623094916));
#157971=CARTESIAN_POINT('Ctrl Pts',(86.61406497309,-3.34643350640855,55.2607255884706));
#157972=CARTESIAN_POINT('Ctrl Pts',(86.5849648306966,-3.34610283753138,
55.2671677479827));
#157973=CARTESIAN_POINT('Ctrl Pts',(86.5532472021764,-3.34574242580324,
55.2741893638742));
#157974=CARTESIAN_POINT('Ctrl Pts',(86.5214433295666,-3.34498159188331,
55.2828035872345));
#157975=CARTESIAN_POINT('Ctrl Pts',(86.4898015752697,-3.34379635323437,
55.2930611493146));
#157976=CARTESIAN_POINT('Ctrl Pts',(86.4585364163671,-3.34262522111733,
55.3031966274357));
#157977=CARTESIAN_POINT('Ctrl Pts',(86.4274303116597,-3.34103960634926,
55.3149368972055));
#157978=CARTESIAN_POINT('Ctrl Pts',(86.3967395298491,-3.33902749693949,
55.3282841139911));
#157979=CARTESIAN_POINT('Ctrl Pts',(86.3664165371889,-3.33703950004712,
55.3414713817225));
#157980=CARTESIAN_POINT('Ctrl Pts',(86.3364998186016,-3.33463510590651,
55.3562274133762));
#157981=CARTESIAN_POINT('Ctrl Pts',(86.307240872989,-3.331815016697,55.372505092502));
#157982=CARTESIAN_POINT('Ctrl Pts',(86.2781476065118,-3.32901089627693,
55.3886905990718));
#157983=CARTESIAN_POINT('Ctrl Pts',(86.2497055440448,-3.32579576135565,
55.406380472337));
#157984=CARTESIAN_POINT('Ctrl Pts',(86.222153506037,-3.32218312108875,55.4254793526165));
#157985=CARTESIAN_POINT('Ctrl Pts',(86.1947086340817,-3.31858453250096,
55.4445039461368));
#157986=CARTESIAN_POINT('Ctrl Pts',(86.1681476825843,-3.31459157231305,
55.4649262777229));
#157987=CARTESIAN_POINT('Ctrl Pts',(86.1426857976783,-3.31023010145211,
55.4866064774387));
#157988=CARTESIAN_POINT('Ctrl Pts',(86.1350465971449,-3.30892155141152,
55.4931110780936));
#157989=CARTESIAN_POINT('Ctrl Pts',(86.1275061415236,-3.30757991230072,
55.4997286139691));
#157990=CARTESIAN_POINT('Ctrl Pts',(86.1200697122403,-3.30620608885032,
55.5064545877257));
#157991=CARTESIAN_POINT('Ctrl Pts',(86.0952811849256,-3.30162659796451,
55.5288748888987));
#157992=CARTESIAN_POINT('Ctrl Pts',(86.0716515487885,-3.29668873202253,
55.5525025819528));
#157993=CARTESIAN_POINT('Ctrl Pts',(86.0493521079058,-3.29143289234783,
55.5771483320876));
#157994=CARTESIAN_POINT('Ctrl Pts',(86.0269902517838,-3.286162341789,55.601863064687));
#157995=CARTESIAN_POINT('Ctrl Pts',(86.0059665084832,-3.2805722003403,55.6276008284941));
#157996=CARTESIAN_POINT('Ctrl Pts',(85.9864096839156,-3.27471204681387,
55.6541436075309));
#157997=CARTESIAN_POINT('Ctrl Pts',(85.9666618803187,-3.26879466689938,
55.6809455858133));
#157998=CARTESIAN_POINT('Ctrl Pts',(85.9484100621666,-3.26260217229768,
55.7085675546546));
#157999=CARTESIAN_POINT('Ctrl Pts',(85.931736394215,-3.25619186561974,55.7367692789791));
#158000=CARTESIAN_POINT('Ctrl Pts',(85.914946330045,-3.24973680961259,55.7651678750462));
#158001=CARTESIAN_POINT('Ctrl Pts',(85.8997565149374,-3.24306110901668,
55.794153487594));
#158002=CARTESIAN_POINT('Ctrl Pts',(85.8861979421808,-3.23622641362624,
55.8234777690152));
#158003=CARTESIAN_POINT('Ctrl Pts',(85.8724469419851,-3.22929471813451,
55.8532182296669));
#158004=CARTESIAN_POINT('Ctrl Pts',(85.8603736020248,-3.22219970311276,
55.8833062096247));
#158005=CARTESIAN_POINT('Ctrl Pts',(85.8499576407623,-3.21500553713045,
55.9134924759869));
#158006=CARTESIAN_POINT('Ctrl Pts',(85.8469372655869,-3.21291940414731,
55.9222457583063));
#158007=CARTESIAN_POINT('Ctrl Pts',(85.8440559326875,-3.21082492144357,
55.9310074108718));
#158008=CARTESIAN_POINT('Ctrl Pts',(85.8413123914781,-3.20872361198818,
55.9397716540776));
#158009=CARTESIAN_POINT('Ctrl Pts',(85.8316470423775,-3.2013208110442,55.9706476146413));
#158010=CARTESIAN_POINT('Ctrl Pts',(85.8236951720488,-3.19383373360089,
56.0015534440733));
#158011=CARTESIAN_POINT('Ctrl Pts',(85.8173727327578,-3.18632561112764,
56.0322542653455));
#158012=CARTESIAN_POINT('Ctrl Pts',(85.8108631967492,-3.17859530461987,
56.0638636003451));
#158013=CARTESIAN_POINT('Ctrl Pts',(85.8060803265883,-3.17084287445321,
56.0952549946809));
#158014=CARTESIAN_POINT('Ctrl Pts',(85.8028912389185,-3.16312973200661,
56.1262093260497));
#158015=CARTESIAN_POINT('Ctrl Pts',(85.7996472066774,-3.15528370036114,
56.1576969674572));
#158016=CARTESIAN_POINT('Ctrl Pts',(85.7980515083608,-3.14747844002179,
56.1887320383206));
#158017=CARTESIAN_POINT('Ctrl Pts',(85.7979338246624,-3.13976850575949,
56.2191290300128));
#158018=CARTESIAN_POINT('Ctrl Pts',(85.797812224897,-3.13180201413088,56.2505375182842));
#158019=CARTESIAN_POINT('Ctrl Pts',(85.7992677760407,-3.12393738863357,
56.2812645518244));
#158020=CARTESIAN_POINT('Ctrl Pts',(85.8020935481781,-3.11622246369485,
56.3111575270582));
#158021=CARTESIAN_POINT('Ctrl Pts',(85.804503994011,-3.10964146290445,56.3366568929241));
#158022=CARTESIAN_POINT('Ctrl Pts',(85.8079108851163,-3.10316916366077,
56.3615503605815));
#158023=CARTESIAN_POINT('Ctrl Pts',(85.8121822996917,-3.09682809692899,
56.3857720505554));
#158024=CARTESIAN_POINT('Ctrl Pts',(87.7631107484691,-9.86087935710899,
57.88435148745));
#158025=CARTESIAN_POINT('Ctrl Pts',(87.728897687669,-9.33637382671099,57.69031957761));
#158026=CARTESIAN_POINT('Ctrl Pts',(87.6485159203691,-8.21061242792599,
57.23445192227));
#158027=CARTESIAN_POINT('Ctrl Pts',(87.5191833454691,-6.52081640480999,
56.50097044125));
#158028=CARTESIAN_POINT('Ctrl Pts',(87.399308616539,-4.80924371223799,55.82112707061));
#158029=CARTESIAN_POINT('Ctrl Pts',(87.3381855483191,-3.67011481886699,
55.47448092506));
#158030=CARTESIAN_POINT('Ctrl Pts',(87.3149793525591,-3.12718060160599,
55.34287204894));
#158031=CARTESIAN_POINT('Ctrl Pts',(86.7045062565192,-10.15160363171,57.2850598679101));
#158032=CARTESIAN_POINT('Ctrl Pts',(86.6713315074291,-9.64303537257999,
57.09691651656));
#158033=CARTESIAN_POINT('Ctrl Pts',(86.5926852603991,-8.540837710357,56.65089148561));
#158034=CARTESIAN_POINT('Ctrl Pts',(86.4632718589192,-6.85002147353099,
55.91695161455));
#158035=CARTESIAN_POINT('Ctrl Pts',(86.3401158359792,-5.09357790444299,
55.21849910066));
#158036=CARTESIAN_POINT('Ctrl Pts',(86.275884280909,-3.89841031468999,54.85422385018));
#158037=CARTESIAN_POINT('Ctrl Pts',(86.2513679124891,-3.32479822433799,
54.71518461565));
#158038=CARTESIAN_POINT('Ctrl Pts',(85.7816779657691,-9.91232327874599,
58.0946566077));
#158039=CARTESIAN_POINT('Ctrl Pts',(85.7476486351392,-9.39063786282099,
57.90166668358));
#158040=CARTESIAN_POINT('Ctrl Pts',(85.6675739697391,-8.269046088395,57.44754068947));
#158041=CARTESIAN_POINT('Ctrl Pts',(85.5382270924591,-6.57906953754599,
56.7139780959199));
#158042=CARTESIAN_POINT('Ctrl Pts',(85.4177717356291,-4.85955690305299,
56.03084182066));
#158043=CARTESIAN_POINT('Ctrl Pts',(85.3560986178691,-3.71051191200099,
55.6810761891501));
#158044=CARTESIAN_POINT('Ctrl Pts',(85.3326605858791,-3.16214921752899,
55.54815250443));
#158045=CARTESIAN_POINT('Ctrl Pts',(86.3421937596991,-9.49244947474399,
59.13092116154));
#158046=CARTESIAN_POINT('Ctrl Pts',(86.3066648642291,-8.94774691405598,
58.92942678263));
#158047=CARTESIAN_POINT('Ctrl Pts',(86.2240837019491,-7.79212359644,58.46108573835));
#158048=CARTESIAN_POINT('Ctrl Pts',(86.0948535570791,-6.10362047264499,
57.72818516716));
#158049=CARTESIAN_POINT('Ctrl Pts',(85.9791371557891,-4.44891187158699,
57.0719248443));
#158050=CARTESIAN_POINT('Ctrl Pts',(85.9219534195892,-3.38079985613399,
56.74761976079));
#158051=CARTESIAN_POINT('Ctrl Pts',(85.900407583149,-2.87674318079599,56.62542725032));
#158052=CARTESIAN_POINT('Origin',(28.1938561267191,10.75942675157,83.17555499762));
#158053=CARTESIAN_POINT('Ctrl Pts',(80.8776256911591,11.53578371495,74.526004930479));
#158054=CARTESIAN_POINT('Ctrl Pts',(80.6466807255579,11.4265581751583,74.7033356918515));
#158055=CARTESIAN_POINT('Ctrl Pts',(80.4344623573573,11.2910809302903,74.8372090682622));
#158056=CARTESIAN_POINT('Ctrl Pts',(80.0485761754778,11.0189816647197,75.0242644873895));
#158057=CARTESIAN_POINT('Ctrl Pts',(79.8750390236475,10.8824621328803,75.0781875502727));
#158058=CARTESIAN_POINT('Ctrl Pts',(79.7231088722891,10.75948375202,75.104988805765));
#158059=CARTESIAN_POINT('Ctrl Pts',(80.0846671696191,12.2337111353,74.375202534073));
#158060=CARTESIAN_POINT('Ctrl Pts',(80.0643038624191,12.19866929898,74.425273469824));
#158061=CARTESIAN_POINT('Ctrl Pts',(79.9719432784991,12.03291962305,74.64145218167));
#158062=CARTESIAN_POINT('Ctrl Pts',(79.8139703990991,11.69505677215,74.933862536297));
#158063=CARTESIAN_POINT('Ctrl Pts',(79.6130676484391,11.21422968175,75.144853266097));
#158064=CARTESIAN_POINT('Ctrl Pts',(79.4721307191891,10.90433893298,75.186980135866));
#158065=CARTESIAN_POINT('Ctrl Pts',(79.3982473483891,10.76260680237,75.186691133753));
#158066=CARTESIAN_POINT('Ctrl Pts',(79.3950256211791,10.75646376115,75.186639953909));
#158067=CARTESIAN_POINT('Ctrl Pts',(80.3666475076091,11.86746169039,74.288033087485));
#158068=CARTESIAN_POINT('Ctrl Pts',(80.3506099828591,11.83751354529,74.331758606035));
#158069=CARTESIAN_POINT('Ctrl Pts',(80.2779714098091,11.69543897126,74.5214403561681));
#158070=CARTESIAN_POINT('Ctrl Pts',(80.1528671321391,11.40235418381,74.784376539898));
#158071=CARTESIAN_POINT('Ctrl Pts',(79.9858604313792,10.97672372266,74.981925061155));
#158072=CARTESIAN_POINT('Ctrl Pts',(79.8610606286691,10.69698164451,75.023072286078));
#158073=CARTESIAN_POINT('Ctrl Pts',(79.7931833543991,10.56824068116,75.021923137852));
#158074=CARTESIAN_POINT('Ctrl Pts',(79.7902192472791,10.56265943354,75.021833601096));
#158075=CARTESIAN_POINT('Ctrl Pts',(80.7663533791792,11.62255509433,74.3280108745551));
#158076=CARTESIAN_POINT('Ctrl Pts',(80.7521047661192,11.59565552083,74.369584739658));
#158077=CARTESIAN_POINT('Ctrl Pts',(80.6875878118291,11.46716013595,74.5513747886651));
#158078=CARTESIAN_POINT('Ctrl Pts',(80.5738009008192,11.19460864096,74.81355029025));
#158079=CARTESIAN_POINT('Ctrl Pts',(80.4106645115891,10.77986391846,75.022702472629));
#158080=CARTESIAN_POINT('Ctrl Pts',(80.2825653231991,10.49399265843,75.06900603011));
#158081=CARTESIAN_POINT('Ctrl Pts',(80.2118938500291,10.35949997223,75.066743547213));
#158082=CARTESIAN_POINT('Ctrl Pts',(80.2088062088191,10.35366403843,75.066598511338));
#158083=CARTESIAN_POINT('Ctrl Pts',(81.2029062710791,11.54854698987,74.487046587091));
#158084=CARTESIAN_POINT('Ctrl Pts',(81.1875477215091,11.52203400491,74.531097938973));
#158085=CARTESIAN_POINT('Ctrl Pts',(81.1179086243191,11.39427421441,74.7251983942701));
#158086=CARTESIAN_POINT('Ctrl Pts',(80.9915978315291,11.11385643038,75.015480622744));
#158087=CARTESIAN_POINT('Ctrl Pts',(80.8015228769991,10.66348388033,75.25893439227));
#158088=CARTESIAN_POINT('Ctrl Pts',(80.6513554051391,10.3364457957,75.3154869012339));
#158089=CARTESIAN_POINT('Ctrl Pts',(80.5696548300191,10.17862232931,75.31208317289));
#158090=CARTESIAN_POINT('Ctrl Pts',(80.5660874970391,10.17176676406,75.311876725662));
#158091=CARTESIAN_POINT('Origin',(79.9839384245637,10.7602162427584,76.5820094885442));
#158092=CARTESIAN_POINT('Ctrl Pts',(78.760931083689,11.61208641416,76.341387867119));
#158093=CARTESIAN_POINT('Ctrl Pts',(78.720761931639,11.54538801364,76.34960017132));
#158094=CARTESIAN_POINT('Ctrl Pts',(78.539124905319,11.21497913113,76.384095471138));
#158095=CARTESIAN_POINT('Ctrl Pts',(78.3272248697091,10.53130051923,76.395483468053));
#158096=CARTESIAN_POINT('Ctrl Pts',(78.3210903544191,9.65920748234801,76.30462454924));
#158097=CARTESIAN_POINT('Ctrl Pts',(78.4990584433091,8.88612097175701,76.14832993757));
#158098=CARTESIAN_POINT('Ctrl Pts',(78.7939422207591,8.19874503162601,75.957853167008));
#158099=CARTESIAN_POINT('Ctrl Pts',(79.175049588149,7.56852236834102,75.750228152338));
#158100=CARTESIAN_POINT('Ctrl Pts',(79.6296693412391,6.97116568539302,75.534928347765));
#158101=CARTESIAN_POINT('Ctrl Pts',(80.1516532961491,6.39047926863501,75.318663026047));
#158102=CARTESIAN_POINT('Ctrl Pts',(80.7411739705891,5.81082699109101,75.104561720609));
#158103=CARTESIAN_POINT('Ctrl Pts',(81.396531416289,5.21759815199301,74.898979890115));
#158104=CARTESIAN_POINT('Ctrl Pts',(81.9189771327191,4.76455349315301,74.760481913992));
#158105=CARTESIAN_POINT('Ctrl Pts',(82.2187668424891,4.50327324549201,74.68987766881));
#158106=CARTESIAN_POINT('Ctrl Pts',(82.2811754718592,4.44871069526601,74.675560443258));
#158107=CARTESIAN_POINT('Ctrl Pts',(78.8641595298191,11.42713922143,75.170127744247));
#158108=CARTESIAN_POINT('Ctrl Pts',(78.8278635622092,11.36880057166,75.177351358709));
#158109=CARTESIAN_POINT('Ctrl Pts',(78.6656267334791,11.07828617183,75.207759617271));
#158110=CARTESIAN_POINT('Ctrl Pts',(78.4985841602091,10.4656706454,75.2175449663339));
#158111=CARTESIAN_POINT('Ctrl Pts',(78.5706517692291,9.69219344377001,75.1386809316639));
#158112=CARTESIAN_POINT('Ctrl Pts',(78.8344223404291,9.02554784154501,75.011775205111));
#158113=CARTESIAN_POINT('Ctrl Pts',(79.2155386524891,8.44664301813601,74.869303349441));
#158114=CARTESIAN_POINT('Ctrl Pts',(79.6806598076492,7.92214918321301,74.7285580249969));
#158115=CARTESIAN_POINT('Ctrl Pts',(80.216106658139,7.42405260242701,74.599070810471));
#158116=CARTESIAN_POINT('Ctrl Pts',(80.8150297881292,6.93264887820001,74.487264366057));
#158117=CARTESIAN_POINT('Ctrl Pts',(81.4796940616691,6.42787751324401,74.397564004857));
#158118=CARTESIAN_POINT('Ctrl Pts',(82.2075605569891,5.89010509385001,74.336016015736));
#158119=CARTESIAN_POINT('Ctrl Pts',(82.7812018555291,5.45771440216002,74.316072070765));
#158120=CARTESIAN_POINT('Ctrl Pts',(83.1088424495491,5.19888422833301,74.314523364672));
#158121=CARTESIAN_POINT('Ctrl Pts',(83.1769868269691,5.14441402096701,74.31461935357));
#158122=CARTESIAN_POINT('Ctrl Pts',(79.7706198354091,10.83432890579,74.676686459257));
#158123=CARTESIAN_POINT('Ctrl Pts',(79.7490325589191,10.80132183842,74.680400289062));
#158124=CARTESIAN_POINT('Ctrl Pts',(79.6544599950791,10.63596882446,74.696876463484));
#158125=CARTESIAN_POINT('Ctrl Pts',(79.5763468966291,10.27740128958,74.7116546616779));
#158126=CARTESIAN_POINT('Ctrl Pts',(79.6837480171692,9.79409638780401,74.701642073385));
#158127=CARTESIAN_POINT('Ctrl Pts',(79.941183081199,9.339917463521,74.683093063215));
#158128=CARTESIAN_POINT('Ctrl Pts',(80.3003102645891,8.90682682115901,74.671025266222));
#158129=CARTESIAN_POINT('Ctrl Pts',(80.7366466267892,8.47702391690001,74.67336067523));
#158130=CARTESIAN_POINT('Ctrl Pts',(81.2382284760791,8.03362936517301,74.6944785980151));
#158131=CARTESIAN_POINT('Ctrl Pts',(81.7975241299391,7.56330230079001,74.73697187558));
#158132=CARTESIAN_POINT('Ctrl Pts',(82.416043260439,7.04745267379001,74.804224914257));
#158133=CARTESIAN_POINT('Ctrl Pts',(83.0886572931891,6.46826090235701,74.898479664418));
#158134=CARTESIAN_POINT('Ctrl Pts',(83.6137814815491,5.98357472872301,74.988134994262));
#158135=CARTESIAN_POINT('Ctrl Pts',(83.9113586226891,5.68901254023702,75.044415251821));
#158136=CARTESIAN_POINT('Ctrl Pts',(83.9731390541791,5.62687424178201,75.056330974776));
#158137=CARTESIAN_POINT('Ctrl Pts',(80.6669551324391,10.36557764703,75.303823453054));
#158138=CARTESIAN_POINT('Ctrl Pts',(80.657714106889,10.35214424328,75.304655694476));
#158139=CARTESIAN_POINT('Ctrl Pts',(80.6183554741592,10.28491358268,75.309855847824));
#158140=CARTESIAN_POINT('Ctrl Pts',(80.5934484228191,10.13542447521,75.331742363491));
#158141=CARTESIAN_POINT('Ctrl Pts',(80.6616100705791,9.873479922928,75.385658137821));
#158142=CARTESIAN_POINT('Ctrl Pts',(80.8262564189292,9.54714943156901,75.457206384792));
#158143=CARTESIAN_POINT('Ctrl Pts',(81.0749034137791,9.16637857277802,75.5409316618649));
#158144=CARTESIAN_POINT('Ctrl Pts',(81.3954846805991,8.73526357028401,75.634164078232));
#158145=CARTESIAN_POINT('Ctrl Pts',(81.7788961234291,8.252929445145,75.735543351396));
#158146=CARTESIAN_POINT('Ctrl Pts',(82.2175549486792,7.71656115272501,75.843725751213));
#158147=CARTESIAN_POINT('Ctrl Pts',(82.710045723589,7.11361449180501,75.959652084995));
#158148=CARTESIAN_POINT('Ctrl Pts',(83.249223208889,6.43329272587702,76.081678387038));
#158149=CARTESIAN_POINT('Ctrl Pts',(83.6696514644091,5.87028578229801,76.173636010829));
#158150=CARTESIAN_POINT('Ctrl Pts',(83.906226421349,5.53387143463101,76.224629363201));
#158151=CARTESIAN_POINT('Ctrl Pts',(83.9552535116592,5.46318510498301,76.235165622379));
#158152=CARTESIAN_POINT('Ctrl Pts',(82.3561326848172,4.76438284010715,74.6407108450246));
#158153=CARTESIAN_POINT('Ctrl Pts',(82.3991945347386,4.79680410512389,74.6331152640959));
#158154=CARTESIAN_POINT('Ctrl Pts',(82.4427922163751,4.82923978037722,74.6284382682739));
#158155=CARTESIAN_POINT('Ctrl Pts',(82.486641365581,4.86147824934395,74.62671321235));
#158156=CARTESIAN_POINT('Ctrl Pts',(82.5321824331826,4.89496063888104,74.6249215951837));
#158157=CARTESIAN_POINT('Ctrl Pts',(82.5779942257533,4.928230027107,74.6263133473138));
#158158=CARTESIAN_POINT('Ctrl Pts',(82.6237782932783,4.96107054230688,74.6308753087991));
#158159=CARTESIAN_POINT('Ctrl Pts',(82.673481938154,4.99672253640157,74.6358278201389));
#158160=CARTESIAN_POINT('Ctrl Pts',(82.7231525292242,5.03186890885039,74.6445157813354));
#158161=CARTESIAN_POINT('Ctrl Pts',(82.7724394801782,5.06626223667213,74.6568762190072));
#158162=CARTESIAN_POINT('Ctrl Pts',(82.7917148327503,5.07971292710966,74.6617101920865));
#158163=CARTESIAN_POINT('Ctrl Pts',(82.8109318524455,5.09304874392178,74.6671054613116));
#158164=CARTESIAN_POINT('Ctrl Pts',(82.8300707926036,5.10625594687553,74.6730569730185));
#158165=CARTESIAN_POINT('Ctrl Pts',(82.876573958631,5.13834637333808,74.6875177600179));
#158166=CARTESIAN_POINT('Ctrl Pts',(82.9225997647433,5.1696656549185,74.7052614130784));
#158167=CARTESIAN_POINT('Ctrl Pts',(82.9678250499752,5.19999377004828,74.72616425599));
#158168=CARTESIAN_POINT('Ctrl Pts',(83.0141795455772,5.23107913462234,74.7475890128454));
#158169=CARTESIAN_POINT('Ctrl Pts',(83.059692988644,5.26112322435461,74.7723323244376));
#158170=CARTESIAN_POINT('Ctrl Pts',(83.1040409338527,5.28991207347925,74.8002162089175));
#158171=CARTESIAN_POINT('Ctrl Pts',(83.1495121793079,5.31943012259645,74.8288063713131));
#158172=CARTESIAN_POINT('Ctrl Pts',(83.1937581999166,5.34762859821416,74.860698102205));
#158173=CARTESIAN_POINT('Ctrl Pts',(83.2364535655702,5.3743000951368,74.8956568932294));
#158174=CARTESIAN_POINT('Ctrl Pts',(83.2482659793901,5.38167922760294,74.9053288494219));
#158175=CARTESIAN_POINT('Ctrl Pts',(83.2599598349876,5.38894160859464,74.9152353304516));
#158176=CARTESIAN_POINT('Ctrl Pts',(83.2715285462647,5.39608314048418,74.9253708148277));
#158177=CARTESIAN_POINT('Ctrl Pts',(83.3132133905908,5.42181579453126,74.9618913985181));
#158178=CARTESIAN_POINT('Ctrl Pts',(83.3532611144477,5.44597121910875,75.0013790153269));
#158179=CARTESIAN_POINT('Ctrl Pts',(83.3913802560555,5.46837375986761,75.0435451308988));
#158180=CARTESIAN_POINT('Ctrl Pts',(83.4288356830262,5.49038623690562,75.0849770676063));
#158181=CARTESIAN_POINT('Ctrl Pts',(83.4644290819774,5.51070630669796,75.1289951816093));
#158182=CARTESIAN_POINT('Ctrl Pts',(83.4979051902054,5.5291879854873,75.1752857753653));
#158183=CARTESIAN_POINT('Ctrl Pts',(83.5302094526534,5.5470227050438,75.219955946682));
#158184=CARTESIAN_POINT('Ctrl Pts',(83.5605418940536,5.5631453631716,75.2667422958217));
#158185=CARTESIAN_POINT('Ctrl Pts',(83.5886944258666,5.57744529689563,75.3153243140312));
#158186=CARTESIAN_POINT('Ctrl Pts',(83.5970875853033,5.58170855905898,75.329808148995));
#158187=CARTESIAN_POINT('Ctrl Pts',(83.6052871483651,5.58580996392761,75.3444513188558));
#158188=CARTESIAN_POINT('Ctrl Pts',(83.6132880352556,5.58974698551495,75.3592446366348));
#158189=CARTESIAN_POINT('Ctrl Pts',(83.6414216489043,5.60359078130662,75.4112625557317));
#158190=CARTESIAN_POINT('Ctrl Pts',(83.6670887093203,5.61539658439895,75.4651226559922));
#158191=CARTESIAN_POINT('Ctrl Pts',(83.6901149815983,5.62509354660136,75.5204638505852));
#158192=CARTESIAN_POINT('Ctrl Pts',(83.7117988663748,5.6342251945095,75.572578759697));
#158193=CARTESIAN_POINT('Ctrl Pts',(83.7311402923122,5.64148624770732,75.6260073548933));
#158194=CARTESIAN_POINT('Ctrl Pts',(83.7480075792902,5.64683278713781,75.6804081268761));
#158195=CARTESIAN_POINT('Ctrl Pts',(83.76389816772,5.65186973574279,75.7316588276537));
#158196=CARTESIAN_POINT('Ctrl Pts',(83.7775922677441,5.65520707870626,75.7837721225949));
#158197=CARTESIAN_POINT('Ctrl Pts',(83.7890008849906,5.65682815435045,75.8364262684517));
#158198=CARTESIAN_POINT('Ctrl Pts',(83.7941954682701,5.65756626417167,75.8604008080262));
#158199=CARTESIAN_POINT('Ctrl Pts',(83.7989165831328,5.65794888183426,75.8844869843741));
#158200=CARTESIAN_POINT('Ctrl Pts',(83.803157922374,5.65797626616968,75.908652059077));
#158201=CARTESIAN_POINT('Origin',(76.2877195330491,1.4210854715202E-14,
77.233875802293));
#158202=CARTESIAN_POINT('Origin',(11.833832765324,1.4210854715202E-14,67.1130006183894));
#158203=CARTESIAN_POINT('Origin',(11.833832765324,1.4210854715202E-14,67.1130006183894));
#158204=CARTESIAN_POINT('Origin',(11.833832765324,1.4210854715202E-14,67.1130006183894));
#158205=CARTESIAN_POINT('',(0.,0.,0.));
#158206=CARTESIAN_POINT('Origin',(26.6896610501315,-1.66681552173398E-14,
151.364589485454));
#158207=CARTESIAN_POINT('',(46.6311526176588,-7.22655593335579,147.848368540858));
#158208=CARTESIAN_POINT('',(5.51632265081665,-0.0343503924582198,155.098027723626));
#158209=CARTESIAN_POINT('Origin',(26.6896610501315,-1.66681552173398E-14,
151.364589485454));
#158210=CARTESIAN_POINT('',(46.5922727658143,-6.01049908472091,148.362935266823));
#158211=CARTESIAN_POINT('Ctrl Pts',(46.592272697957,-6.01049893749535,148.362935371323));
#158212=CARTESIAN_POINT('Ctrl Pts',(46.6144830676967,-5.9974822785011,148.359019105243));
#158213=CARTESIAN_POINT('Ctrl Pts',(46.6351119736002,-5.98996913036867,
148.354404235172));
#158214=CARTESIAN_POINT('Ctrl Pts',(46.6541344752789,-5.98752441441695,
148.349041555766));
#158215=CARTESIAN_POINT('Ctrl Pts',(46.6736823414854,-5.98501218016174,
148.343530769577));
#158216=CARTESIAN_POINT('Ctrl Pts',(46.6915328413437,-5.98785213129854,
148.337230105633));
#158217=CARTESIAN_POINT('Ctrl Pts',(46.7076331609104,-5.99555810475863,
148.330134203584));
#158218=CARTESIAN_POINT('Ctrl Pts',(46.7242892474038,-6.00353008071449,
148.322793358093));
#158219=CARTESIAN_POINT('Ctrl Pts',(46.739071016055,-6.0167097143341,148.314601354749));
#158220=CARTESIAN_POINT('Ctrl Pts',(46.7519101453899,-6.03454524601735,
148.305605204033));
#158221=CARTESIAN_POINT('Ctrl Pts',(46.7571747445889,-6.04185858661581,
148.301916392539));
#158222=CARTESIAN_POINT('Ctrl Pts',(46.7621127120552,-6.04995460487111,
148.298092981991));
#158223=CARTESIAN_POINT('Ctrl Pts',(46.7667196262217,-6.058794711895,148.294140644901));
#158224=CARTESIAN_POINT('Ctrl Pts',(46.7802991102161,-6.08485208728866,
148.282490612729));
#158225=CARTESIAN_POINT('Ctrl Pts',(46.7911285461141,-6.11693779180763,
148.269696104708));
#158226=CARTESIAN_POINT('Ctrl Pts',(46.7993490990491,-6.15360029378031,
148.255851527001));
#158227=CARTESIAN_POINT('Ctrl Pts',(46.8071143454513,-6.18823219309309,
148.242773750108));
#158228=CARTESIAN_POINT('Ctrl Pts',(46.8125506373435,-6.22694730095852,
148.228759733826));
#158229=CARTESIAN_POINT('Ctrl Pts',(46.8158102675014,-6.26850580218765,
148.21391438593));
#158230=CARTESIAN_POINT('Ctrl Pts',(46.8185709816293,-6.30370339698346,
148.201341253493));
#158231=CARTESIAN_POINT('Ctrl Pts',(46.8197706507559,-6.34094015738946,
148.188172356552));
#158232=CARTESIAN_POINT('Ctrl Pts',(46.8195289914499,-6.3794577430535,148.174481598226));
#158233=CARTESIAN_POINT('Ctrl Pts',(46.8192248796204,-6.42792950951748,
148.157252708387));
#158234=CARTESIAN_POINT('Ctrl Pts',(46.8166546262969,-6.47841958647206,
148.139178171846));
#158235=CARTESIAN_POINT('Ctrl Pts',(46.8119082091704,-6.53008108437151,
148.120433281528));
#158236=CARTESIAN_POINT('Ctrl Pts',(46.8072393702522,-6.58089819663437,
148.101994768624));
#158237=CARTESIAN_POINT('Ctrl Pts',(46.8004647856395,-6.63284840171413,
148.082907929366));
#158238=CARTESIAN_POINT('Ctrl Pts',(46.7917193796614,-6.68512593250974,
148.06334941683));
#158239=CARTESIAN_POINT('Ctrl Pts',(46.7851181003292,-6.72458648865097,
148.048586099392));
#158240=CARTESIAN_POINT('Ctrl Pts',(46.7773949212129,-6.76423351280253,
148.033554260372));
#158241=CARTESIAN_POINT('Ctrl Pts',(46.768627364254,-6.80372239658839,148.018332209879));
#158242=CARTESIAN_POINT('Ctrl Pts',(46.7573214772964,-6.85464386288281,
147.998703163504));
#158243=CARTESIAN_POINT('Ctrl Pts',(46.7442722310709,-6.90531476842511,
147.97876071212));
#158244=CARTESIAN_POINT('Ctrl Pts',(46.7295296446186,-6.9554691842044,147.958735860062));
#158245=CARTESIAN_POINT('Ctrl Pts',(46.7147691166906,-7.00568463705029,
147.938686638101));
#158246=CARTESIAN_POINT('Ctrl Pts',(46.6983111758215,-7.05538213512469,
147.91855543384));
#158247=CARTESIAN_POINT('Ctrl Pts',(46.6802562768064,-7.10430939864112,
147.898573855963));
#158248=CARTESIAN_POINT('Ctrl Pts',(46.664999047466,-7.1456552117551,147.88168849338));
#158249=CARTESIAN_POINT('Ctrl Pts',(46.64860236062,-7.18645120184107,147.864910163264));
#158250=CARTESIAN_POINT('Ctrl Pts',(46.6311537904856,-7.22655473104065,
147.848373621278));
#158251=CARTESIAN_POINT('',(46.5732575347653,6.074764193991,148.366288161248));
#158252=CARTESIAN_POINT('Origin',(26.7764851389615,-2.04263841746052E-14,
151.856993361954));
#158253=CARTESIAN_POINT('',(46.6083116808377,7.29121844351931,147.852402231042));
#158254=CARTESIAN_POINT('Ctrl Pts',(46.6083123648192,7.29121885610936,147.852402503935));
#158255=CARTESIAN_POINT('Ctrl Pts',(46.629098730082,7.24384081903475,147.871934753254));
#158256=CARTESIAN_POINT('Ctrl Pts',(46.6484155685107,7.19548878528177,147.891804947096));
#158257=CARTESIAN_POINT('Ctrl Pts',(46.6661206992522,7.14640049424429,147.911789154575));
#158258=CARTESIAN_POINT('Ctrl Pts',(46.6838077808551,7.09736224527508,147.931752989557));
#158259=CARTESIAN_POINT('Ctrl Pts',(46.699886262435,7.04758940618498,147.951830001543));
#158260=CARTESIAN_POINT('Ctrl Pts',(46.7142629109001,6.99733606536463,147.971788999166));
#158261=CARTESIAN_POINT('Ctrl Pts',(46.7264430853448,6.95476046374863,147.988698647711));
#158262=CARTESIAN_POINT('Ctrl Pts',(46.7374025380023,6.91184032817418,148.005523251997));
#158263=CARTESIAN_POINT('Ctrl Pts',(46.7471127455659,6.86873826094321,148.022122681677));
#158264=CARTESIAN_POINT('Ctrl Pts',(46.7588660208026,6.81656734120588,148.042214699744));
#158265=CARTESIAN_POINT('Ctrl Pts',(46.7687942102469,6.76411203487173,148.061974411536));
#158266=CARTESIAN_POINT('Ctrl Pts',(46.7767215184415,6.71216953488076,148.081221976832));
#158267=CARTESIAN_POINT('Ctrl Pts',(46.7847711291542,6.65942566595162,148.100766493583));
#158268=CARTESIAN_POINT('Ctrl Pts',(46.7907576638701,6.60721090429097,148.119782660209));
#158269=CARTESIAN_POINT('Ctrl Pts',(46.7945507233129,6.55636449864328,148.138089286346));
#158270=CARTESIAN_POINT('Ctrl Pts',(46.797397365301,6.51820492971532,148.151828172172));
#158271=CARTESIAN_POINT('Ctrl Pts',(46.7990097341067,6.48081618753838,148.165167541349));
#158272=CARTESIAN_POINT('Ctrl Pts',(46.7993515207053,6.44455284067278,148.178034849603));
#158273=CARTESIAN_POINT('Ctrl Pts',(46.7997762982508,6.39948420563544,148.194026534589));
#158274=CARTESIAN_POINT('Ctrl Pts',(46.798221872536,6.35616280553221,148.209304529387));
#158275=CARTESIAN_POINT('Ctrl Pts',(46.7944964971984,6.31580176935984,148.223752333791));
#158276=CARTESIAN_POINT('Ctrl Pts',(46.7905490980168,6.27303530780383,148.239061194272));
#158277=CARTESIAN_POINT('Ctrl Pts',(46.7841648875179,6.23359325766264,148.253437231881));
#158278=CARTESIAN_POINT('Ctrl Pts',(46.7751709819016,6.19890721773494,148.266764157202));
#158279=CARTESIAN_POINT('Ctrl Pts',(46.7677608266292,6.17032909465762,148.277744324233));
#158280=CARTESIAN_POINT('Ctrl Pts',(46.7585806685715,6.14497939587087,148.288012596913));
#158281=CARTESIAN_POINT('Ctrl Pts',(46.7475524713142,6.1236485023314,148.297519676975));
#158282=CARTESIAN_POINT('Ctrl Pts',(46.7364156891186,6.10210758228424,148.307120364876));
#158283=CARTESIAN_POINT('Ctrl Pts',(46.7233062761893,6.08496303983045,148.315957464712));
#158284=CARTESIAN_POINT('Ctrl Pts',(46.7082887242939,6.07276715603841,148.32396398118));
#158285=CARTESIAN_POINT('Ctrl Pts',(46.693623205093,6.0608571610426,148.331782813558));
#158286=CARTESIAN_POINT('Ctrl Pts',(46.6771391359373,6.05366667657209,148.338809443837));
#158287=CARTESIAN_POINT('Ctrl Pts',(46.6588949049778,6.05169860747618,148.345028922708));
#158288=CARTESIAN_POINT('Ctrl Pts',(46.6413878518859,6.0498100603389,148.350997096814));
#158289=CARTESIAN_POINT('Ctrl Pts',(46.6222609319471,6.05273047192043,148.356222244022));
#158290=CARTESIAN_POINT('Ctrl Pts',(46.6015490857105,6.06089226979178,148.360734230142));
#158291=CARTESIAN_POINT('Ctrl Pts',(46.5924259545905,6.06448736949,148.362721664798));
#158292=CARTESIAN_POINT('Ctrl Pts',(46.5829950097966,6.06909924750259,148.364571287597));
#158293=CARTESIAN_POINT('Ctrl Pts',(46.5732574663672,6.07476404354701,148.366288269697));
#158294=CARTESIAN_POINT('Origin',(26.6896610501315,-1.66681552173398E-14,
151.364589485454));
#158295=CARTESIAN_POINT('Origin',(20.7595757828115,-1.33056427483082E-16,
117.733404720054));
#158296=CARTESIAN_POINT('',(46.0417820332401,-4.21831552016986,139.708826847192));
#158297=CARTESIAN_POINT('',(46.3509510310709,0.0343503924439632,139.055898541647));
#158298=CARTESIAN_POINT('Ctrl Pts',(46.0417820332401,-4.21831552016986,
139.708826847192));
#158299=CARTESIAN_POINT('Ctrl Pts',(46.0798964649748,-3.96069965430408,
139.628141305823));
#158300=CARTESIAN_POINT('Ctrl Pts',(46.1145382929002,-3.7023636146849,139.555238670999));
#158301=CARTESIAN_POINT('Ctrl Pts',(46.145633349218,-3.44379565574912,139.489959447747));
#158302=CARTESIAN_POINT('Ctrl Pts',(46.176779243046,-3.18480496237181,139.424573499068));
#158303=CARTESIAN_POINT('Ctrl Pts',(46.204366746486,-2.92558188626453,139.366835911588));
#158304=CARTESIAN_POINT('Ctrl Pts',(46.2283726896026,-2.66662111980495,
139.316577350232));
#158305=CARTESIAN_POINT('Ctrl Pts',(46.2524801304473,-2.40656546074536,
139.266106294421));
#158306=CARTESIAN_POINT('Ctrl Pts',(46.2729756665083,-2.14677463153881,
139.223177640495));
#158307=CARTESIAN_POINT('Ctrl Pts',(46.2898876726048,-1.88774922729219,
139.187610755653));
#158308=CARTESIAN_POINT('Ctrl Pts',(46.3068526632686,-1.62791230790918,
139.151932441334));
#158309=CARTESIAN_POINT('Ctrl Pts',(46.3202116902603,-1.36884591102246,
139.123662086757));
#158310=CARTESIAN_POINT('Ctrl Pts',(46.3300449792115,-1.11105049051174,
139.102608260532));
#158311=CARTESIAN_POINT('Ctrl Pts',(46.3399398726735,-0.851640009074977,
139.081422534321));
#158312=CARTESIAN_POINT('Ctrl Pts',(46.3462647840154,-0.593516770546314,
139.06754402874));
#158313=CARTESIAN_POINT('Ctrl Pts',(46.3491526922906,-0.33718134924774,
139.060768657603));
#158314=CARTESIAN_POINT('Ctrl Pts',(46.3505528770535,-0.212898679269364,
139.057483660115));
#158315=CARTESIAN_POINT('Ctrl Pts',(46.3511458716836,-0.0890361107474958,
139.055868288421));
#158316=CARTESIAN_POINT('Ctrl Pts',(46.3509510310709,0.0343503924439631,
139.055898541647));
#158317=CARTESIAN_POINT('',(46.1497547374386,-7.65783120162291,146.034362956251));
#158318=CARTESIAN_POINT('Ctrl Pts',(46.1497339363911,-7.6578231488931,146.034366627848));
#158319=CARTESIAN_POINT('Ctrl Pts',(46.1042153651043,-7.68998708971556,
145.846479401818));
#158320=CARTESIAN_POINT('Ctrl Pts',(46.0629773097244,-7.71232938446267,
145.66225894746));
#158321=CARTESIAN_POINT('Ctrl Pts',(46.0072879996495,-7.73350808720076,
145.393632086788));
#158322=CARTESIAN_POINT('Ctrl Pts',(45.9897496172286,-7.7385121747197,145.305359799572));
#158323=CARTESIAN_POINT('Ctrl Pts',(45.9566301524631,-7.74481940759447,
145.131590450506));
#158324=CARTESIAN_POINT('Ctrl Pts',(45.941260819711,-7.74613449772924,145.047333435302));
#158325=CARTESIAN_POINT('Ctrl Pts',(45.8965248889764,-7.7453198499371,144.791744275131));
#158326=CARTESIAN_POINT('Ctrl Pts',(45.869145516159,-7.73806024054962,144.620256010497));
#158327=CARTESIAN_POINT('Ctrl Pts',(45.8321120275292,-7.71652195814888,
144.362521087448));
#158328=CARTESIAN_POINT('Ctrl Pts',(45.8204410308522,-7.7075650961645,144.276525090039));
#158329=CARTESIAN_POINT('Ctrl Pts',(45.8039994313618,-7.6913670319232,144.147544670468));
#158330=CARTESIAN_POINT('Ctrl Pts',(45.7960449821503,-7.68257696548179,
144.083057840277));
#158331=CARTESIAN_POINT('Ctrl Pts',(45.7885009205254,-7.67273025071386,
144.0186025713));
#158332=CARTESIAN_POINT('Ctrl Pts',(45.7835622888294,-7.66593221096656,
143.975643011381));
#158333=CARTESIAN_POINT('Ctrl Pts',(45.7813306285701,-7.66270987102601,
143.955903486097));
#158334=CARTESIAN_POINT('Ctrl Pts',(45.7684766770574,-7.64307962434864,
143.839891445313));
#158335=CARTESIAN_POINT('Ctrl Pts',(45.7596408825485,-7.6257233326379,143.7517794149));
#158336=CARTESIAN_POINT('Ctrl Pts',(45.7480663165466,-7.59844081559175,
143.62667668098));
#158337=CARTESIAN_POINT('Ctrl Pts',(45.7444886020521,-7.58913672710442,
143.586151562286));
#158338=CARTESIAN_POINT('Ctrl Pts',(45.737819455117,-7.57029207910011,143.507437894518));
#158339=CARTESIAN_POINT('Ctrl Pts',(45.7345929734825,-7.56030305028397,
143.467514656276));
#158340=CARTESIAN_POINT('Ctrl Pts',(45.7263484282852,-7.53292686773121,
143.361620720427));
#158341=CARTESIAN_POINT('Ctrl Pts',(45.7209182165448,-7.512317140153,143.286466775378));
#158342=CARTESIAN_POINT('Ctrl Pts',(45.7133201123482,-7.47677089169681,
143.167336673486));
#158343=CARTESIAN_POINT('Ctrl Pts',(45.7096587513103,-7.45783790075944,
143.106174761609));
#158344=CARTESIAN_POINT('Ctrl Pts',(45.7062958499248,-7.43694281070744,
143.042730367685));
#158345=CARTESIAN_POINT('Ctrl Pts',(45.7041309931867,-7.42255085999889,
142.999941895134));
#158346=CARTESIAN_POINT('Ctrl Pts',(45.7031826442293,-7.41585694488886,
142.980392066024));
#158347=CARTESIAN_POINT('Ctrl Pts',(45.6977051259425,-7.37383780134823,
142.86054559507));
#158348=CARTESIAN_POINT('Ctrl Pts',(45.6948246180137,-7.34029306004632,
142.773887831552));
#158349=CARTESIAN_POINT('Ctrl Pts',(45.691770042583,-7.29243658114092,142.656955627243));
#158350=CARTESIAN_POINT('Ctrl Pts',(45.690965722722,-7.27688780244582,142.620152809729));
#158351=CARTESIAN_POINT('Ctrl Pts',(45.6899804795069,-7.25440829956244,
142.568108874407));
#158352=CARTESIAN_POINT('Ctrl Pts',(45.6895433986862,-7.2433789219476,142.54287697546));
#158353=CARTESIAN_POINT('Ctrl Pts',(45.6891729752481,-7.23270513479341,
142.518811333593));
#158354=CARTESIAN_POINT('Ctrl Pts',(45.6889391217653,-7.22567243480026,
142.503024679245));
#158355=CARTESIAN_POINT('Ctrl Pts',(45.6888111605613,-7.22162158141484,
142.493977594143));
#158356=CARTESIAN_POINT('Ctrl Pts',(45.6880272138865,-7.19592616713251,
142.436783185656));
#158357=CARTESIAN_POINT('Ctrl Pts',(45.6872649054086,-7.16711518274869,
142.373531033505));
#158358=CARTESIAN_POINT('Ctrl Pts',(45.6869970866555,-7.1124947649413,142.261419388534));
#158359=CARTESIAN_POINT('Ctrl Pts',(45.6870571716022,-7.09237842868069,
142.221184305656));
#158360=CARTESIAN_POINT('Ctrl Pts',(45.6875194253624,-7.05896285169835,
142.156793104236));
#158361=CARTESIAN_POINT('Ctrl Pts',(45.687843822262,-7.04144413250784,142.123588874133));
#158362=CARTESIAN_POINT('Ctrl Pts',(45.6884201262682,-7.01949769659911,
142.08315377698));
#158363=CARTESIAN_POINT('Ctrl Pts',(45.6887133361663,-7.00975907998373,
142.065468995032));
#158364=CARTESIAN_POINT('Ctrl Pts',(45.6889195085684,-7.00319156414997,
142.053601082715));
#158365=CARTESIAN_POINT('Ctrl Pts',(45.6890630123584,-6.99883684277521,
142.045778847938));
#158366=CARTESIAN_POINT('Ctrl Pts',(45.6904048531293,-6.95929473657219,
141.975019900084));
#158367=CARTESIAN_POINT('Ctrl Pts',(45.6921845384018,-6.92005463882973,
141.908007387539));
#158368=CARTESIAN_POINT('Ctrl Pts',(45.6956863675944,-6.85796433617798,
141.807147597128));
#158369=CARTESIAN_POINT('Ctrl Pts',(45.696991894597,-6.83672982750858,141.77346926005));
#158370=CARTESIAN_POINT('Ctrl Pts',(45.6988007920649,-6.80949672370966,
141.731325674698));
#158371=CARTESIAN_POINT('Ctrl Pts',(45.699113663538,-6.80482761333938,141.724122677196));
#158372=CARTESIAN_POINT('Ctrl Pts',(45.7001636123571,-6.78963402102599,
141.70092561296));
#158373=CARTESIAN_POINT('Ctrl Pts',(45.7017539847202,-6.76725055741431,
141.667079480057));
#158374=CARTESIAN_POINT('Ctrl Pts',(45.7033639042665,-6.7461562007986,141.636033786375));
#158375=CARTESIAN_POINT('Ctrl Pts',(45.7065472854106,-6.70584735232583,
141.577556746701));
#158376=CARTESIAN_POINT('Ctrl Pts',(45.7086182735838,-6.6814878045978,141.54338751695));
#158377=CARTESIAN_POINT('Ctrl Pts',(45.7114500524151,-6.64923604612378,
141.498939073594));
#158378=CARTESIAN_POINT('Ctrl Pts',(45.7123488827038,-6.63919837515679,
141.485258043084));
#158379=CARTESIAN_POINT('Ctrl Pts',(45.7134002324388,-6.62758451559962,
141.469539272868));
#158380=CARTESIAN_POINT('Ctrl Pts',(45.7136497257773,-6.62484064018721,
141.465835629711));
#158381=CARTESIAN_POINT('Ctrl Pts',(45.7138335799324,-6.62281422693999,
141.463099121855));
#158382=CARTESIAN_POINT('Ctrl Pts',(45.7141373124748,-6.61945076661083,
141.458550380537));
#158383=CARTESIAN_POINT('Ctrl Pts',(45.7145264540736,-6.61511155314601,
141.452673412528));
#158384=CARTESIAN_POINT('Ctrl Pts',(45.7160229518845,-6.59845306229987,
141.430154955935));
#158385=CARTESIAN_POINT('Ctrl Pts',(45.7178479254177,-6.57813305522803,
141.402739126245));
#158386=CARTESIAN_POINT('Ctrl Pts',(45.7218380877348,-6.53630340439622,
141.348305743493));
#158387=CARTESIAN_POINT('Ctrl Pts',(45.7233789981059,-6.52046270551198,
141.327948884204));
#158388=CARTESIAN_POINT('Ctrl Pts',(45.7260617700661,-6.49369965360933,
141.294250513101));
#158389=CARTESIAN_POINT('Ctrl Pts',(45.7274961568459,-6.47956716151472,
141.276611176011));
#158390=CARTESIAN_POINT('Ctrl Pts',(45.7293458160154,-6.46172641248284,
141.254690011814));
#158391=CARTESIAN_POINT('Ctrl Pts',(45.7303164674517,-6.45246268687009,
141.243399581771));
#158392=CARTESIAN_POINT('Ctrl Pts',(45.7307424708742,-6.44841838679609,
141.238490762029));
#158393=CARTESIAN_POINT('Ctrl Pts',(45.7310287190181,-6.44570565034031,
141.235202715874));
#158394=CARTESIAN_POINT('Ctrl Pts',(45.7312503885032,-6.44360985675879,
141.232667182809));
#158395=CARTESIAN_POINT('Ctrl Pts',(45.7400169956866,-6.36082037669196,
141.132598362081));
#158396=CARTESIAN_POINT('Ctrl Pts',(45.7508279851103,-6.26573217913631,
141.024864807299));
#158397=CARTESIAN_POINT('Ctrl Pts',(45.7712367072148,-6.10013641485336,
140.855713182854));
#158398=CARTESIAN_POINT('Ctrl Pts',(45.7787367562556,-6.0411081552893,140.798076114454));
#158399=CARTESIAN_POINT('Ctrl Pts',(45.7911281773601,-5.94639684561445,
140.710486101705));
#158400=CARTESIAN_POINT('Ctrl Pts',(45.7976087465152,-5.8974994790897,140.666408991859));
#158401=CARTESIAN_POINT('Ctrl Pts',(45.8056828955101,-5.83766901096797,
140.614671644116));
#158402=CARTESIAN_POINT('Ctrl Pts',(45.8098496909852,-5.80704790930028,
140.588748214596));
#158403=CARTESIAN_POINT('Ctrl Pts',(45.8119656691689,-5.79155967192321,
140.575775820276));
#158404=CARTESIAN_POINT('Ctrl Pts',(45.8128795129233,-5.78488365189796,
140.570214260568));
#158405=CARTESIAN_POINT('Ctrl Pts',(45.8134902982546,-5.78042446799032,
140.566506154555));
#158406=CARTESIAN_POINT('Ctrl Pts',(45.8139419819895,-5.77712962556911,
140.563772785789));
#158407=CARTESIAN_POINT('Ctrl Pts',(45.8192693889668,-5.73828518183523,
140.531587282574));
#158408=CARTESIAN_POINT('Ctrl Pts',(45.825943633586,-5.68988489649699,140.492257824353));
#158409=CARTESIAN_POINT('Ctrl Pts',(45.8385455597466,-5.59991727629164,
140.423130510986));
#158410=CARTESIAN_POINT('Ctrl Pts',(45.8431787050888,-5.56702917127515,
140.398408932811));
#158411=CARTESIAN_POINT('Ctrl Pts',(45.8508194009384,-5.51316147609579,
140.35915507419));
#158412=CARTESIAN_POINT('Ctrl Pts',(45.8534813793313,-5.49444964359847,
140.345709308676));
#158413=CARTESIAN_POINT('Ctrl Pts',(45.8590425368407,-5.45548061424916,
140.318160471314));
#158414=CARTESIAN_POINT('Ctrl Pts',(45.8620980256864,-5.43413471853736,
140.303312692143));
#158415=CARTESIAN_POINT('Ctrl Pts',(45.8764235136232,-5.33434004698192,
140.235050331361));
#158416=CARTESIAN_POINT('Ctrl Pts',(45.8869093654876,-5.26225278333579,
140.189348452813));
#158417=CARTESIAN_POINT('Ctrl Pts',(45.9008095038559,-5.16718733759057,
140.131782210991));
#158418=CARTESIAN_POINT('Ctrl Pts',(45.9051402261405,-5.13767045970881,
140.11443064948));
#158419=CARTESIAN_POINT('Ctrl Pts',(45.9111524852506,-5.09678449221605,
140.090917922924));
#158420=CARTESIAN_POINT('Ctrl Pts',(45.9140378013058,-5.07718838456376,
140.079790802148));
#158421=CARTESIAN_POINT('Ctrl Pts',(45.9171874191562,-5.05583253773055,
140.067863841893));
#158422=CARTESIAN_POINT('Ctrl Pts',(45.9184903686662,-5.0470051275582,140.062973711995));
#158423=CARTESIAN_POINT('Ctrl Pts',(45.9193485312138,-5.04119268215965,
140.059762333137));
#158424=CARTESIAN_POINT('Ctrl Pts',(45.9196130476279,-5.03940128342387,
140.058773735075));
#158425=CARTESIAN_POINT('Ctrl Pts',(45.9571775476616,-4.78510952048925,
139.919026012772));
#158426=CARTESIAN_POINT('Ctrl Pts',(45.9983852910152,-4.51174191713301,
139.800717395929));
#158427=CARTESIAN_POINT('Ctrl Pts',(46.04178901647,-4.21831693899752,139.70882561586));
#158428=CARTESIAN_POINT('Ctrl Pts',(46.6311525941371,-7.22655631911563,
147.84836866603));
#158429=CARTESIAN_POINT('Ctrl Pts',(46.5749523425034,-7.28654605238906,
147.652930322284));
#158430=CARTESIAN_POINT('Ctrl Pts',(46.5201920540669,-7.34187891713897,
147.457811989727));
#158431=CARTESIAN_POINT('Ctrl Pts',(46.4669881862245,-7.39272369123276,
147.263294848322));
#158432=CARTESIAN_POINT('Ctrl Pts',(46.4117038947351,-7.44555664164975,
147.061171529451));
#158433=CARTESIAN_POINT('Ctrl Pts',(46.3580998832002,-7.49354395600487,
146.859697404632));
#158434=CARTESIAN_POINT('Ctrl Pts',(46.3062558753462,-7.53690360083462,
146.659141512676));
#158435=CARTESIAN_POINT('Ctrl Pts',(46.2906808817071,-7.54992971938474,
146.598890446625));
#158436=CARTESIAN_POINT('Ctrl Pts',(46.2752645598976,-7.56253823447593,
146.538721942065));
#158437=CARTESIAN_POINT('Ctrl Pts',(46.2600086377472,-7.57473518779224,
146.478642508045));
#158438=CARTESIAN_POINT('Ctrl Pts',(46.2222544574842,-7.60491926775972,
146.32996255545));
#158439=CARTESIAN_POINT('Ctrl Pts',(46.1854830765979,-7.63258269512805,
146.181829353134));
#158440=CARTESIAN_POINT('Ctrl Pts',(46.1497151458197,-7.65781587554136,
146.034369942548));
#158441=CARTESIAN_POINT('',(2.89423390144577,-0.0343503973693096,140.227423469835));
#158442=CARTESIAN_POINT('',(-0.413763883134335,-0.0343503924582198,121.466835774864));
#158443=CARTESIAN_POINT('',(1.71342629329879,-0.0343503924582184,133.530730749341));
#158444=CARTESIAN_POINT('Ctrl Pts',(2.89423390144145,-0.0343503973693145,
140.227423469823));
#158445=CARTESIAN_POINT('Ctrl Pts',(2.89490682052228,-0.462029070005339,
140.227304815406));
#158446=CARTESIAN_POINT('Ctrl Pts',(2.89460237971182,-0.917705420464532,
140.140419107162));
#158447=CARTESIAN_POINT('Ctrl Pts',(2.88567038560036,-1.75510442296394,
139.789430687949));
#158448=CARTESIAN_POINT('Ctrl Pts',(2.87635083480166,-2.13688745377311,
139.525490015263));
#158449=CARTESIAN_POINT('Ctrl Pts',(2.83941701094823,-2.73970894382591,
138.919770610805));
#158450=CARTESIAN_POINT('Ctrl Pts',(2.80921594987279,-3.00119474164409,
138.537367096412));
#158451=CARTESIAN_POINT('Ctrl Pts',(2.71482824727497,-3.34831581410866,
137.70361918511));
#158452=CARTESIAN_POINT('Ctrl Pts',(2.64987594375213,-3.43391381428035,
137.252346126911));
#158453=CARTESIAN_POINT('Ctrl Pts',(2.501341302863,-3.43391381428035,136.409964318453));
#158454=CARTESIAN_POINT('Ctrl Pts',(2.40803202714239,-3.34831581410866,
135.963691359544));
#158455=CARTESIAN_POINT('Ctrl Pts',(2.21156887464543,-3.00119474164409,
135.147942104127));
#158456=CARTESIAN_POINT('Ctrl Pts',(2.10915888407688,-2.73970894382592,
134.778270972251));
#158457=CARTESIAN_POINT('Ctrl Pts',(1.93669708828159,-2.13688745377311,
134.196448805887));
#158458=CARTESIAN_POINT('Ctrl Pts',(1.85518157469485,-1.75510442296394,
133.94523822934));
#158459=CARTESIAN_POINT('Ctrl Pts',(1.74352979420513,-0.917705420464523,
133.612362079917));
#158460=CARTESIAN_POINT('Ctrl Pts',(1.71409921239068,-0.4620290650944,133.530612095549));
#158461=CARTESIAN_POINT('Ctrl Pts',(1.71342629329879,-0.0343503924582188,
133.530730749341));
#158462=CARTESIAN_POINT('',(1.38116159371226,-0.0343503924582198,131.646363999275));
#158463=CARTESIAN_POINT('',(-0.413763883134335,-0.0343503924582198,121.466835774864));
#158464=CARTESIAN_POINT('',(21.0799238088015,-21.4999725592973,119.352372629494));
#158465=CARTESIAN_POINT('Origin',(21.0460952759711,4.44089209850063E-15,
119.358337512575));
#158466=CARTESIAN_POINT('',(21.0122667431774,21.4999725592974,119.364302395616));
#158467=CARTESIAN_POINT('Origin',(21.0460952759615,-9.02974887056722E-15,
119.358337512554));
#158468=CARTESIAN_POINT('Origin',(21.0460952759711,4.44089209850063E-15,
119.358337512575));
#158469=CARTESIAN_POINT('Ctrl Pts',(1.71342629329879,-0.0343503924582162,
133.530730749341));
#158470=CARTESIAN_POINT('Ctrl Pts',(1.7127533742069,0.393328280177966,133.530849403133));
#158471=CARTESIAN_POINT('Ctrl Pts',(1.74074994280215,0.849049561642535,
133.612852242722));
#158472=CARTESIAN_POINT('Ctrl Pts',(1.84976630355433,1.68661093518625,133.94619308775));
#158473=CARTESIAN_POINT('Ctrl Pts',(1.93008022417292,2.06850914312402,134.197615537557));
#158474=CARTESIAN_POINT('Ctrl Pts',(2.10064469350225,2.6715474277491,134.779772253768));
#158475=CARTESIAN_POINT('Ctrl Pts',(2.20223164676253,2.93314903787896,135.149588509328));
#158476=CARTESIAN_POINT('Ctrl Pts',(2.39760220552714,3.28043393904487,135.965530418499));
#158477=CARTESIAN_POINT('Ctrl Pts',(2.49064204597367,3.36607750679975,136.411850886116));
#158478=CARTESIAN_POINT('Ctrl Pts',(2.56490936641823,3.36607750679975,136.833041790345));
#158479=CARTESIAN_POINT('Ctrl Pts',(2.63917668686279,3.36607750679975,137.254232694574));
#158480=CARTESIAN_POINT('Ctrl Pts',(2.70439842565971,3.28043393904489,137.705458244064));
#158481=CARTESIAN_POINT('Ctrl Pts',(2.79987872198988,2.93314903787895,138.539013501613));
#158482=CARTESIAN_POINT('Ctrl Pts',(2.83090282037359,2.6715474277491,138.921271892322));
#158483=CARTESIAN_POINT('Ctrl Pts',(2.86973397069298,2.06850914312402,139.526656746933));
#158484=CARTESIAN_POINT('Ctrl Pts',(2.88025511445985,1.68661093518626,139.790385546358));
#158485=CARTESIAN_POINT('Ctrl Pts',(2.89182252830886,0.849049561642544,
140.140909269967));
#158486=CARTESIAN_POINT('Ctrl Pts',(2.89356098234184,0.393328280177964,
140.227542123616));
#158487=CARTESIAN_POINT('Ctrl Pts',(2.89423390143373,-0.0343503924582163,
140.227423469824));
#158488=CARTESIAN_POINT('',(46.1255152751644,7.72197159682826,146.038637027215));
#158489=CARTESIAN_POINT('Ctrl Pts',(46.1255152751644,7.72197159682826,146.038637027215));
#158490=CARTESIAN_POINT('Ctrl Pts',(46.183994384387,7.68085770665526,146.279171780814));
#158491=CARTESIAN_POINT('Ctrl Pts',(46.2451773117493,7.6332659101491,146.52149373214));
#158492=CARTESIAN_POINT('Ctrl Pts',(46.3089515198577,7.57882968383795,146.765090549348));
#158493=CARTESIAN_POINT('Ctrl Pts',(46.3705589150633,7.52624300017179,147.000410843142));
#158494=CARTESIAN_POINT('Ctrl Pts',(46.4345846392306,7.46726902673398,147.236920819104));
#158495=CARTESIAN_POINT('Ctrl Pts',(46.5008817904809,7.40156269285372,147.4741666267));
#158496=CARTESIAN_POINT('Ctrl Pts',(46.5360620153873,7.36669598199073,147.600059831942));
#158497=CARTESIAN_POINT('Ctrl Pts',(46.571881048459,7.32993330205662,147.726160374427));
#158498=CARTESIAN_POINT('Ctrl Pts',(46.6083112377426,7.29122142518356,147.852401444788));
#158499=CARTESIAN_POINT('',(46.0284016907478,4.28565939879059,139.711186162701));
#158500=CARTESIAN_POINT('Ctrl Pts',(46.0284016907478,4.28565939879059,139.711186162701));
#158501=CARTESIAN_POINT('Ctrl Pts',(46.009451892876,4.41100978518104,139.750554627543));
#158502=CARTESIAN_POINT('Ctrl Pts',(45.9896428349026,4.54135926216652,139.797642870725));
#158503=CARTESIAN_POINT('Ctrl Pts',(45.9692247694648,4.67560735556524,139.854095719192));
#158504=CARTESIAN_POINT('Ctrl Pts',(45.9590157367459,4.7427314022646,139.882322143426));
#158505=CARTESIAN_POINT('Ctrl Pts',(45.9486567169092,4.81082554163191,139.912892067642));
#158506=CARTESIAN_POINT('Ctrl Pts',(45.9381949514543,4.87972100603375,139.946021991183));
#158507=CARTESIAN_POINT('Ctrl Pts',(45.9329640687268,4.91416873823467,139.962586952953));
#158508=CARTESIAN_POINT('Ctrl Pts',(45.9277077024198,4.94881617101466,139.979791741817));
#158509=CARTESIAN_POINT('Ctrl Pts',(45.922433052648,4.98363888587044,139.99766286594));
#158510=CARTESIAN_POINT('Ctrl Pts',(45.9177959001256,5.01425290708772,140.013374075573));
#158511=CARTESIAN_POINT('Ctrl Pts',(45.9129814428359,5.04609222585267,140.030196196397));
#158512=CARTESIAN_POINT('Ctrl Pts',(45.908425332391,5.07626481501438,140.04657579581));
#158513=CARTESIAN_POINT('Ctrl Pts',(45.9077989764833,5.08041282233302,140.048827597864));
#158514=CARTESIAN_POINT('Ctrl Pts',(45.9071775807259,5.08452934809361,140.051071022753));
#158515=CARTESIAN_POINT('Ctrl Pts',(45.9065623496373,5.08860689606862,140.053302021474));
#158516=CARTESIAN_POINT('Ctrl Pts',(45.8862006710659,5.22355736064531,140.127139120553));
#158517=CARTESIAN_POINT('Ctrl Pts',(45.8666105311921,5.35404529556136,140.20707833822));
#158518=CARTESIAN_POINT('Ctrl Pts',(45.8480731697131,5.47967188638401,140.292630687702));
#158519=CARTESIAN_POINT('Ctrl Pts',(45.8388044889737,5.54248518179534,140.335406862442));
#158520=CARTESIAN_POINT('Ctrl Pts',(45.8297989417253,5.60408474185784,140.379586566384));
#158521=CARTESIAN_POINT('Ctrl Pts',(45.821090801588,5.66442993465207,140.425110148166));
#158522=CARTESIAN_POINT('Ctrl Pts',(45.8167367315194,5.69460253104918,140.447871939057));
#158523=CARTESIAN_POINT('Ctrl Pts',(45.8124569345293,5.72446213510723,140.470970159996));
#158524=CARTESIAN_POINT('Ctrl Pts',(45.8082558796439,5.75400203758663,140.494395532349));
#158525=CARTESIAN_POINT('Ctrl Pts',(45.8061553522012,5.76877198882632,140.506108218525));
#158526=CARTESIAN_POINT('Ctrl Pts',(45.8040745109114,5.78346201486672,140.517902692444));
#158527=CARTESIAN_POINT('Ctrl Pts',(45.8020139522343,5.7980709928589,140.529777516931));
#158528=CARTESIAN_POINT('Ctrl Pts',(45.8009836728958,5.805375481855,140.535714929175));
#158529=CARTESIAN_POINT('Ctrl Pts',(45.7999584643093,5.81265970884927,140.541672429043));
#158530=CARTESIAN_POINT('Ctrl Pts',(45.7989383976504,5.81992356232579,140.54764986147));
#158531=CARTESIAN_POINT('Ctrl Pts',(45.798428364321,5.82355548906404,140.550638577684));
#158532=CARTESIAN_POINT('Ctrl Pts',(45.7979196164765,5.82718232242351,140.553632277037));
#158533=CARTESIAN_POINT('Ctrl Pts',(45.7974121631645,5.83080404735202,140.55663093907));
#158534=CARTESIAN_POINT('Ctrl Pts',(45.7969047098525,5.83442577228053,140.559629601103));
#158535=CARTESIAN_POINT('Ctrl Pts',(45.7965205363705,5.83716976420411,140.561906282869));
#158536=CARTESIAN_POINT('Ctrl Pts',(45.7958936958764,5.84165388185056,140.565641792772));
#158537=CARTESIAN_POINT('Ctrl Pts',(45.7806100795712,5.95098557663157,140.656720943858));
#158538=CARTESIAN_POINT('Ctrl Pts',(45.7666915407109,6.05363275282939,140.750035584638));
#158539=CARTESIAN_POINT('Ctrl Pts',(45.7541788910299,6.14992992876353,140.844616000562));
#158540=CARTESIAN_POINT('Ctrl Pts',(45.7412877000483,6.2491403532217,140.942057728403));
#158541=CARTESIAN_POINT('Ctrl Pts',(45.7298886223451,6.3416109033887,141.040842998358));
#158542=CARTESIAN_POINT('Ctrl Pts',(45.7199718226298,6.42769967331016,141.139921000597));
#158543=CARTESIAN_POINT('Ctrl Pts',(45.7142480946429,6.47738795137442,141.197106337661));
#158544=CARTESIAN_POINT('Ctrl Pts',(45.7090171683938,6.52495010581967,141.254389367596));
#158545=CARTESIAN_POINT('Ctrl Pts',(45.7042695604774,6.57045361793451,141.311569384902));
#158546=CARTESIAN_POINT('Ctrl Pts',(45.6959999643079,6.64971367396863,141.411168100804));
#158547=CARTESIAN_POINT('Ctrl Pts',(45.6891813300088,6.72277528512748,141.510435605595));
#158548=CARTESIAN_POINT('Ctrl Pts',(45.6836775820624,6.79018167418363,141.608430686704));
#158549=CARTESIAN_POINT('Ctrl Pts',(45.6822073808803,6.80818775909815,141.634607845522));
#158550=CARTESIAN_POINT('Ctrl Pts',(45.6808307273227,6.82579023568006,141.66069425717));
#158551=CARTESIAN_POINT('Ctrl Pts',(45.6795444407347,6.84299930990636,141.686672084303));
#158552=CARTESIAN_POINT('Ctrl Pts',(45.6764936687251,6.88381522328763,141.748285435967));
#158553=CARTESIAN_POINT('Ctrl Pts',(45.6739516782181,6.92242270120041,141.809296108042));
#158554=CARTESIAN_POINT('Ctrl Pts',(45.67187119573,6.95897798206324,141.869511322291));
#158555=CARTESIAN_POINT('Ctrl Pts',(45.6708309544859,6.97725562249465,141.899618929415));
#158556=CARTESIAN_POINT('Ctrl Pts',(45.6699059875799,6.99502036582419,141.92952811241));
#158557=CARTESIAN_POINT('Ctrl Pts',(45.6690898210906,7.01229252155032,141.959217281051));
#158558=CARTESIAN_POINT('Ctrl Pts',(45.668681737846,7.02092859941338,141.974061865372));
#158559=CARTESIAN_POINT('Ctrl Pts',(45.6683008482816,7.02944152814726,141.988851447237));
#158560=CARTESIAN_POINT('Ctrl Pts',(45.6679463130868,7.03783389502715,142.003583500307));
#158561=CARTESIAN_POINT('Ctrl Pts',(45.6677690454893,7.0420300784671,142.010949526842));
#158562=CARTESIAN_POINT('Ctrl Pts',(45.6675983660977,7.04619612131013,142.018301171247));
#158563=CARTESIAN_POINT('Ctrl Pts',(45.6674341680494,7.05033234744749,142.025638122581));
#158564=CARTESIAN_POINT('Ctrl Pts',(45.6672699700011,7.05446857358485,142.032975073916));
#158565=CARTESIAN_POINT('Ctrl Pts',(45.667138694479,7.05786270423485,142.039020679768));
#158566=CARTESIAN_POINT('Ctrl Pts',(45.6669609097315,7.06265190001152,142.047604589381));
#158567=CARTESIAN_POINT('Ctrl Pts',(45.6643797133639,7.13218460690298,142.17223145763));
#158568=CARTESIAN_POINT('Ctrl Pts',(45.6632752867041,7.19971530774337,142.303556493107));
#158569=CARTESIAN_POINT('Ctrl Pts',(45.6642598432247,7.26386732472425,142.441753873634));
#158570=CARTESIAN_POINT('Ctrl Pts',(45.6643602975754,7.27041275820106,142.455854159229));
#158571=CARTESIAN_POINT('Ctrl Pts',(45.664482539201,7.27692303529989,142.470025979662));
#158572=CARTESIAN_POINT('Ctrl Pts',(45.6646272451483,7.28339670455111,142.484269515212));
#158573=CARTESIAN_POINT('Ctrl Pts',(45.6658824739582,7.33955152264681,142.6078228073));
#158574=CARTESIAN_POINT('Ctrl Pts',(45.6688648672261,7.39326350094975,142.737656382104));
#158575=CARTESIAN_POINT('Ctrl Pts',(45.6739949548805,7.4426081922518,142.871601936082));
#158576=CARTESIAN_POINT('Ctrl Pts',(45.6752527010066,7.45470605461057,142.904441433763));
#158577=CARTESIAN_POINT('Ctrl Pts',(45.6766397732845,7.46654149812806,142.937528055851));
#158578=CARTESIAN_POINT('Ctrl Pts',(45.678162778316,7.47808632877853,142.970829776213));
#158579=CARTESIAN_POINT('Ctrl Pts',(45.6842271030676,7.52405571221501,143.103431076202));
#158580=CARTESIAN_POINT('Ctrl Pts',(45.6921579897756,7.56376098479096,143.234237122771));
#158581=CARTESIAN_POINT('Ctrl Pts',(45.7015834264608,7.59812982795002,143.362462267337));
#158582=CARTESIAN_POINT('Ctrl Pts',(45.7041801077836,7.60759834766917,143.397787934372));
#158583=CARTESIAN_POINT('Ctrl Pts',(45.7068899336171,7.61666173680026,143.432917765412));
#158584=CARTESIAN_POINT('Ctrl Pts',(45.7097045081294,7.62533917254263,143.467835441451));
#158585=CARTESIAN_POINT('Ctrl Pts',(45.716219968196,7.64542657325434,143.548666388674));
#158586=CARTESIAN_POINT('Ctrl Pts',(45.7232940489111,7.66345579613631,143.628364479795));
#158587=CARTESIAN_POINT('Ctrl Pts',(45.730825190822,7.67966776014608,143.706779012972));
#158588=CARTESIAN_POINT('Ctrl Pts',(45.7345907617774,7.68777374215096,143.745986279561));
#158589=CARTESIAN_POINT('Ctrl Pts',(45.7384706822679,7.69542519551929,143.784873283985));
#158590=CARTESIAN_POINT('Ctrl Pts',(45.7424527782053,7.70265099123863,143.82342473189));
#158591=CARTESIAN_POINT('Ctrl Pts',(45.744443826174,7.7062638890983,143.842700455843));
#158592=CARTESIAN_POINT('Ctrl Pts',(45.7464604132963,7.70977037069837,143.861892291497));
#158593=CARTESIAN_POINT('Ctrl Pts',(45.7485010660626,7.713173954904,143.880998580289));
#158594=CARTESIAN_POINT('Ctrl Pts',(45.750541718829,7.71657753910963,143.900104869082));
#158595=CARTESIAN_POINT('Ctrl Pts',(45.7523875871807,7.71954259370185,143.91714049923));
#158596=CARTESIAN_POINT('Ctrl Pts',(45.754693733771,7.72307952403362,143.938059155794));
#158597=CARTESIAN_POINT('Ctrl Pts',(45.7740222053368,7.7527235447722,144.113384375925));
#158598=CARTESIAN_POINT('Ctrl Pts',(45.7967147306483,7.77509870425236,144.29208668924));
#158599=CARTESIAN_POINT('Ctrl Pts',(45.8228388932108,7.78980599766508,144.473167914215));
#158600=CARTESIAN_POINT('Ctrl Pts',(45.8480458992102,7.80399695335224,144.647891812575));
#158601=CARTESIAN_POINT('Ctrl Pts',(45.8764481162649,7.81104914922233,144.824830466553));
#158602=CARTESIAN_POINT('Ctrl Pts',(45.9080636557945,7.81058759439462,145.003094689877));
#158603=CARTESIAN_POINT('Ctrl Pts',(45.9384234946378,7.810144371524,145.174278644735));
#158604=CARTESIAN_POINT('Ctrl Pts',(45.971746665868,7.8027724802356,145.346684928471));
#158605=CARTESIAN_POINT('Ctrl Pts',(46.0080057877663,7.78812270517353,145.519533808147));
#158606=CARTESIAN_POINT('Ctrl Pts',(46.0442649096645,7.77347293011147,145.692382687822));
#158607=CARTESIAN_POINT('Ctrl Pts',(46.0834604821633,7.75154542668907,145.865674075287));
#158608=CARTESIAN_POINT('Ctrl Pts',(46.1255152751644,7.72197159682826,146.038637027215));
#158609=CARTESIAN_POINT('Ctrl Pts',(46.3509510310085,0.0343504322637197,
139.055898541659));
#158610=CARTESIAN_POINT('Ctrl Pts',(46.3505517348952,0.289138438632088,
139.055978266158));
#158611=CARTESIAN_POINT('Ctrl Pts',(46.346783451412,0.54593555688485,139.063076026948));
#158612=CARTESIAN_POINT('Ctrl Pts',(46.3394906583825,0.804246151701623,
139.077400049602));
#158613=CARTESIAN_POINT('Ctrl Pts',(46.3322349286742,1.06124396436419,139.091651274927));
#158614=CARTESIAN_POINT('Ctrl Pts',(46.3214903244831,1.31973962955468,139.113055515702));
#158615=CARTESIAN_POINT('Ctrl Pts',(46.3071533183797,1.57923398323097,139.141809086788));
#158616=CARTESIAN_POINT('Ctrl Pts',(46.2928958374792,1.83728896100349,139.170403166166));
#158617=CARTESIAN_POINT('Ctrl Pts',(46.2750856444827,2.09633129025598,139.206265280019));
#158618=CARTESIAN_POINT('Ctrl Pts',(46.2536712542073,2.35586335520789,139.249579620141));
#158619=CARTESIAN_POINT('Ctrl Pts',(46.2323093671487,2.61475910653701,139.292787763347));
#158620=CARTESIAN_POINT('Ctrl Pts',(46.2073608959045,2.87414190315989,139.343411642094));
#158621=CARTESIAN_POINT('Ctrl Pts',(46.1788256748232,3.13351541783259,139.401625114299));
#158622=CARTESIAN_POINT('Ctrl Pts',(46.1503563543616,3.39228992276671,139.459704145495));
#158623=CARTESIAN_POINT('Ctrl Pts',(46.1183168315074,3.65105489450121,139.525337755125));
#158624=CARTESIAN_POINT('Ctrl Pts',(46.0827580021033,3.90931946967923,139.598689596019));
#158625=CARTESIAN_POINT('Ctrl Pts',(46.0654671907504,4.03490302018918,139.634357610533));
#158626=CARTESIAN_POINT('Ctrl Pts',(46.047345015463,4.16036831109744,139.671850450518));
#158627=CARTESIAN_POINT('Ctrl Pts',(46.0284016907478,4.28565939879059,139.711186162701));
#158628=CARTESIAN_POINT('Origin',(10.4384266411762,-0.0270045052801676,
156.534945497534));
#158629=CARTESIAN_POINT('',(48.9375087269424,-4.00018398478067,142.087510868902));
#158630=CARTESIAN_POINT('',(49.3053711741162,0.0383111611405328,141.534954558003));
#158631=CARTESIAN_POINT('Ctrl Pts',(48.9375087304962,-4.00018624765936,
142.087502763741));
#158632=CARTESIAN_POINT('Ctrl Pts',(48.9949833354212,-3.68955343570011,
142.000798941664));
#158633=CARTESIAN_POINT('Ctrl Pts',(49.0457220209274,-3.37742578915628,
141.924471192877));
#158634=CARTESIAN_POINT('Ctrl Pts',(49.0897258950434,-3.06450751067134,
141.858426739305));
#158635=CARTESIAN_POINT('Ctrl Pts',(49.1341269388833,-2.74876489753937,
141.791786182368));
#158636=CARTESIAN_POINT('Ctrl Pts',(49.1716710490429,-2.43221753600664,
141.735615251058));
#158637=CARTESIAN_POINT('Ctrl Pts',(49.2023593250218,-2.11556420125793,
141.689771614418));
#158638=CARTESIAN_POINT('Ctrl Pts',(49.233208589264,-1.7972497282135,141.643687485694));
#158639=CARTESIAN_POINT('Ctrl Pts',(49.2571299006305,-1.47882835832807,
141.60803910677));
#158640=CARTESIAN_POINT('Ctrl Pts',(49.2741243321198,-1.16098201742068,
141.582637047908));
#158641=CARTESIAN_POINT('Ctrl Pts',(49.2912478117602,-0.840722092827111,
141.557042097114));
#158642=CARTESIAN_POINT('Ctrl Pts',(49.3013388131149,-0.521046152281689,
141.541849489902));
#158643=CARTESIAN_POINT('Ctrl Pts',(49.3043983848133,-0.20262062689389,
141.536822739548));
#158644=CARTESIAN_POINT('Ctrl Pts',(49.3051708417072,-0.122227023957362,
141.535553624669));
#158645=CARTESIAN_POINT('Ctrl Pts',(49.305495099357,-0.0419129635884498,
141.534932300882));
#158646=CARTESIAN_POINT('Ctrl Pts',(49.3053711741162,0.0383111611405328,
141.534954558003));
#158647=CARTESIAN_POINT('',(48.9248217570406,4.07524464379169,142.089728903236));
#158648=CARTESIAN_POINT('Ctrl Pts',(49.3053711741162,0.0383111611405328,
141.534954558003));
#158649=CARTESIAN_POINT('Ctrl Pts',(49.3048343231318,0.372806541263403,
141.535047359322));
#158650=CARTESIAN_POINT('Ctrl Pts',(49.296501913863,0.708834768942396,141.546333420866));
#158651=CARTESIAN_POINT('Ctrl Pts',(49.2803751560891,1.0456269205789,141.569098282739));
#158652=CARTESIAN_POINT('Ctrl Pts',(49.2651845064688,1.36286933483779,141.590541715151));
#158653=CARTESIAN_POINT('Ctrl Pts',(49.2430781218927,1.68078908219588,141.62216982411));
#158654=CARTESIAN_POINT('Ctrl Pts',(49.2140570630999,1.99871197485721,141.664179276538));
#158655=CARTESIAN_POINT('Ctrl Pts',(49.1851901179431,2.31494656753981,141.705965641673));
#158656=CARTESIAN_POINT('Ctrl Pts',(49.1494817433335,2.63118408738318,141.758023563724));
#158657=CARTESIAN_POINT('Ctrl Pts',(49.1069330268926,2.9467332676804,141.820503266713));
#158658=CARTESIAN_POINT('Ctrl Pts',(49.0646947262146,3.25998034705143,141.882527146677));
#158659=CARTESIAN_POINT('Ctrl Pts',(49.0157155278959,3.57254888781943,141.954821446331));
#158660=CARTESIAN_POINT('Ctrl Pts',(48.9599965345,3.88373813372928,142.037487896656));
#158661=CARTESIAN_POINT('Ctrl Pts',(48.9485557565992,3.94763460476313,142.054461794431));
#158662=CARTESIAN_POINT('Ctrl Pts',(48.9368308264528,4.01147284724558,142.071872828551));
#158663=CARTESIAN_POINT('Ctrl Pts',(48.924821753789,4.07524667829838,142.089721632632));
#158664=CARTESIAN_POINT('',(94.5819839425882,4.14714157564843,142.089747519112));
#158665=CARTESIAN_POINT('',(48.924821753789,4.07524667829838,142.089721632632));
#158666=CARTESIAN_POINT('',(93.9162870067071,0.108481919349057,141.534966741905));
#158667=CARTESIAN_POINT('Ctrl Pts',(94.5819839479975,4.14713813598916,142.089759812562));
#158668=CARTESIAN_POINT('Ctrl Pts',(94.3592538320324,3.45222469974125,141.895409168734));
#158669=CARTESIAN_POINT('Ctrl Pts',(94.1924301510237,2.7627644869811,141.756622462181));
#158670=CARTESIAN_POINT('Ctrl Pts',(94.0260343534174,1.74942114702695,141.621535163829));
#158671=CARTESIAN_POINT('Ctrl Pts',(93.9845424294768,1.4150798243908,141.588672491858));
#158672=CARTESIAN_POINT('Ctrl Pts',(93.943262545855,0.920005572230557,141.556241959662));
#158673=CARTESIAN_POINT('Ctrl Pts',(93.9278621095087,0.674074769870453,
141.544241726843));
#158674=CARTESIAN_POINT('Ctrl Pts',(93.9190636792179,0.390213915861264,
141.537307403827));
#158675=CARTESIAN_POINT('Ctrl Pts',(93.9169566054853,0.249076665690299,
141.53556754835));
#158676=CARTESIAN_POINT('Ctrl Pts',(93.9164760984515,0.178709844243637,
141.535124545383));
#158677=CARTESIAN_POINT('Ctrl Pts',(93.9163929583916,0.148596247998712,
141.53502564476));
#158678=CARTESIAN_POINT('Ctrl Pts',(93.9163648186267,0.128530249581641,
141.534979865354));
#158679=CARTESIAN_POINT('Ctrl Pts',(93.916366176505,0.117150856258414,141.534966682013));
#158680=CARTESIAN_POINT('Ctrl Pts',(93.9162870067071,0.108481919349057,
141.534966741905));
#158681=CARTESIAN_POINT('',(94.5946916752436,-3.92833378532365,142.087508698775));
#158682=CARTESIAN_POINT('Ctrl Pts',(93.9162870071781,0.108481918637627,
141.53496917311));
#158683=CARTESIAN_POINT('Ctrl Pts',(93.9164305461748,0.00514822670153565,
141.534938907382));
#158684=CARTESIAN_POINT('Ctrl Pts',(93.9179253256695,-0.0987368552810903,
141.535974789762));
#158685=CARTESIAN_POINT('Ctrl Pts',(93.9208317148094,-0.203146342090515,
141.53811584605));
#158686=CARTESIAN_POINT('Ctrl Pts',(93.925388846452,-0.366857308942038,
141.541472958566));
#158687=CARTESIAN_POINT('Ctrl Pts',(93.933415834867,-0.531859595231141,
141.547546324156));
#158688=CARTESIAN_POINT('Ctrl Pts',(93.9450163344638,-0.698040796407542,
141.556450216679));
#158689=CARTESIAN_POINT('Ctrl Pts',(93.9566168340607,-0.864221997583943,
141.565354109202));
#158690=CARTESIAN_POINT('Ctrl Pts',(93.9717910021007,-1.03158290547825,
141.577088579239));
#158691=CARTESIAN_POINT('Ctrl Pts',(93.9906654644376,-1.19996598454483,
141.591788795191));
#158692=CARTESIAN_POINT('Ctrl Pts',(94.0097354656431,-1.37009350730349,
141.606641304944));
#158693=CARTESIAN_POINT('Ctrl Pts',(94.032584612726,-1.54126418678172,141.624521917453));
#158694=CARTESIAN_POINT('Ctrl Pts',(94.0592177093987,-1.71336391385054,
141.64554051154));
#158695=CARTESIAN_POINT('Ctrl Pts',(94.0858508060713,-1.88546364091937,
141.666559105628));
#158696=CARTESIAN_POINT('Ctrl Pts',(94.1162683856671,-2.05849314321545,
141.690715870679));
#158697=CARTESIAN_POINT('Ctrl Pts',(94.1504711301126,-2.23228203059035,
141.718132816551));
#158698=CARTESIAN_POINT('Ctrl Pts',(94.1837144857192,-2.4011961302375,141.744780715603));
#158699=CARTESIAN_POINT('Ctrl Pts',(94.2205347524744,-2.57082605769036,
141.774508809456));
#158700=CARTESIAN_POINT('Ctrl Pts',(94.2608643460002,-2.74110246525793,
141.807426377993));
#158701=CARTESIAN_POINT('Ctrl Pts',(94.2987854901771,-2.90121010921786,
141.838378137068));
#158702=CARTESIAN_POINT('Ctrl Pts',(94.339809638591,-3.06188925156412,141.872150017002));
#158703=CARTESIAN_POINT('Ctrl Pts',(94.3838582501225,-3.22304667840359,
141.908835852476));
#158704=CARTESIAN_POINT('Ctrl Pts',(94.4299695860226,-3.39175084372076,
141.947239625569));
#158705=CARTESIAN_POINT('Ctrl Pts',(94.4793959638611,-3.56097846054621,
141.988836666638));
#158706=CARTESIAN_POINT('Ctrl Pts',(94.5320209407876,-3.73066988997311,
142.033746929427));
#158707=CARTESIAN_POINT('Ctrl Pts',(94.5524331818669,-3.79649001130812,
142.051166777653));
#158708=CARTESIAN_POINT('Ctrl Pts',(94.5733262516347,-3.86237956533525,
142.069085116504));
#158709=CARTESIAN_POINT('Ctrl Pts',(94.5946916751395,-3.92833371710833,
142.0875089431));
#158710=CARTESIAN_POINT('',(48.9375087304962,-4.00018624765936,142.087502763741));
#158711=CARTESIAN_POINT('Origin',(20.7769406005715,-3.80534757440804E-14,
117.831885495454));
#158712=CARTESIAN_POINT('',(11.4514113671306,-17.0269155958486,125.365772183904));
#158713=CARTESIAN_POINT('',(11.3978832029447,16.9933024121131,125.375210643478));
#158714=CARTESIAN_POINT('Origin',(21.7841119891515,-1.2034114792157E-14,
123.543838280654));
#158715=CARTESIAN_POINT('',(2.75313371105733,-0.0319538534495447,130.789059825797));
#158716=CARTESIAN_POINT('Origin',(21.0460952759475,5.19193629061609E-12,
119.358337512588));
#158717=CARTESIAN_POINT('',(3.19063603741116,-0.0319538534495439,133.270258815289));
#158718=CARTESIAN_POINT('',(1.08081067876142,-0.0319538534495447,121.304844616208));
#158719=CARTESIAN_POINT('',(4.37144364554608,-0.0319538534495668,139.966951535772));
#158720=CARTESIAN_POINT('Ctrl Pts',(3.19063603741116,-0.031953853449541,
133.270258815289));
#158721=CARTESIAN_POINT('Ctrl Pts',(3.19130914580987,-0.4597528414267,133.270140128117));
#158722=CARTESIAN_POINT('Ctrl Pts',(3.22179255511482,-0.915479709149352,
133.351752291131));
#158723=CARTESIAN_POINT('Ctrl Pts',(3.33722344804325,-1.75284033660896,
133.683998128254));
#158724=CARTESIAN_POINT('Ctrl Pts',(3.42141457794632,-2.13454361927574,
133.93471892068));
#158725=CARTESIAN_POINT('Ctrl Pts',(3.59892084762791,-2.73722937084846,
134.515522124483));
#158726=CARTESIAN_POINT('Ctrl Pts',(3.7040443169968,-2.9986912819894,134.884637277465));
#158727=CARTESIAN_POINT('Ctrl Pts',(3.90438475055902,-3.34584029838365,
135.699666792464));
#158728=CARTESIAN_POINT('Ctrl Pts',(3.99879634971067,-3.43148439569077,
136.145797224032));
#158729=CARTESIAN_POINT('Ctrl Pts',(4.14737386872942,-3.43148439569077,
136.988422206447));
#158730=CARTESIAN_POINT('Ctrl Pts',(4.21124157983659,-3.34584029838365,
137.439938349572));
#158731=CARTESIAN_POINT('Ctrl Pts',(4.30173966430781,-2.99869128198941,
138.27433603434));
#158732=CARTESIAN_POINT('Ctrl Pts',(4.32920073339708,-2.73722937084846,
138.657145163879));
#158733=CARTESIAN_POINT('Ctrl Pts',(4.36104579664255,-2.13454361927575,
139.263632368418));
#158734=CARTESIAN_POINT('Ctrl Pts',(4.36768357449715,-1.75284033660896,
139.528027909254));
#158735=CARTESIAN_POINT('Ctrl Pts',(4.372848785034,-0.915479709149344,139.87971656123));
#158736=CARTESIAN_POINT('Ctrl Pts',(4.37211675394481,-0.459752841426703,
139.9668328486));
#158737=CARTESIAN_POINT('Ctrl Pts',(4.3714436455461,-0.0319538534495412,
139.966951535772));
#158738=CARTESIAN_POINT('',(6.47258659531382,-0.0319538534495448,151.883125347209));
#158739=CARTESIAN_POINT('',(1.08081067876142,-0.0319538534495447,121.304844616208));
#158740=CARTESIAN_POINT('',(45.86371189171,0.217029124246953,144.937407156988));
#158741=CARTESIAN_POINT('Origin',(26.1687165171315,-2.57311409771171E-14,
148.410166226454));
#158742=CARTESIAN_POINT('Origin',(26.1687165171315,-2.57311409771171E-14,
148.410166226454));
#158743=CARTESIAN_POINT('Ctrl Pts',(4.3714436455461,-0.0319538534495414,
139.966951535772));
#158744=CARTESIAN_POINT('Ctrl Pts',(4.37077053714739,0.39584513452762,139.967070222943));
#158745=CARTESIAN_POINT('Ctrl Pts',(4.37006839073011,0.851620317635747,
139.880206819763));
#158746=CARTESIAN_POINT('Ctrl Pts',(4.36226786195385,1.68915555832631,139.528982845496));
#158747=CARTESIAN_POINT('Ctrl Pts',(4.35442872841004,2.0709827100228,139.264799136081));
#158748=CARTESIAN_POINT('Ctrl Pts',(4.32068673997907,2.67390169638796,138.658646410632));
#158749=CARTESIAN_POINT('Ctrl Pts',(4.29240269482834,2.93548826733316,138.275982393978));
#158750=CARTESIAN_POINT('Ctrl Pts',(4.20081190886385,3.2828137128186,137.441777381964));
#158751=CARTESIAN_POINT('Ctrl Pts',(4.13667461184008,3.36850692538934,136.99030877411));
#158752=CARTESIAN_POINT('Ctrl Pts',(4.06238585233071,3.36850692538934,136.568996282902));
#158753=CARTESIAN_POINT('Ctrl Pts',(3.98809709282133,3.36850692538933,136.147683791695));
#158754=CARTESIAN_POINT('Ctrl Pts',(3.89395507958628,3.28281371281859,135.701505824857));
#158755=CARTESIAN_POINT('Ctrl Pts',(3.69470734751732,2.93548826733316,134.886283637102));
#158756=CARTESIAN_POINT('Ctrl Pts',(3.5904068542099,2.67390169638796,134.517023371236));
#158757=CARTESIAN_POINT('Ctrl Pts',(3.41479750971382,2.0709827100228,133.935885688343));
#158758=CARTESIAN_POINT('Ctrl Pts',(3.33180773549995,1.68915555832632,133.684953064496));
#158759=CARTESIAN_POINT('Ctrl Pts',(3.21901216081092,0.851620317635762,
133.352242549663));
#158760=CARTESIAN_POINT('Ctrl Pts',(3.18996292901245,0.395845134527619,
133.27037750246));
#158761=CARTESIAN_POINT('Ctrl Pts',(3.19063603741116,-0.0319538534495416,
133.270258815289));
#158762=CARTESIAN_POINT('Origin',(21.0460952759475,5.19193629061609E-12,
119.358337512588));
#158763=CARTESIAN_POINT('Origin',(-3.46221193726519,-0.0437048830555943,
137.895785892187));
#158764=CARTESIAN_POINT('',(-2.87180813319772,-0.0437048830555947,141.244132252429));
#158765=CARTESIAN_POINT('Origin',(21.4151041909515,-3.07084035820744E-14,
121.451091063454));
#158766=CARTESIAN_POINT('',(21.0134477487628,20.7493757828742,119.364094152467));
#158767=CARTESIAN_POINT('Origin',(22.4050280472972,0.00237376213208851,
118.509181234833));
#158768=CARTESIAN_POINT('',(21.078742803216,-20.7493757828747,119.352580872643));
#158769=CARTESIAN_POINT('Origin',(21.0460952759615,-1.96166393586405E-14,
119.358337512554));
#158770=CARTESIAN_POINT('Origin',(22.4050280472236,0.00237376205382667,
118.5091812347));
#158771=CARTESIAN_POINT('Origin',(26.1687165171315,-2.57311409771171E-14,
148.410166226454));
#158772=CARTESIAN_POINT('',(44.6470594068091,0.200751938845159,146.675075734032));
#158773=CARTESIAN_POINT('Origin',(44.3865872386167,0.200751939928429,145.197864087198));
#158774=CARTESIAN_POINT('Origin',(26.4291887836315,-2.1219048984176E-14,
149.887377855954));
#158775=CARTESIAN_POINT('Origin',(19.0737828394622,2.73849310306822,149.661194460162));
#158776=CARTESIAN_POINT('',(16.5110267574855,2.73391286221553,151.636217420201));
#158777=CARTESIAN_POINT('',(17.0138492275693,4.37111689096414,151.547556247505));
#158778=CARTESIAN_POINT('Ctrl Pts',(16.5110267574884,2.73391286260886,151.636217420217));
#158779=CARTESIAN_POINT('Ctrl Pts',(16.5109213014316,2.80093627975376,151.636236014965));
#158780=CARTESIAN_POINT('Ctrl Pts',(16.5131087246683,2.86733052016455,151.635850313274));
#158781=CARTESIAN_POINT('Ctrl Pts',(16.5174994497767,2.93316110936568,151.635076109366));
#158782=CARTESIAN_POINT('Ctrl Pts',(16.5219269490194,2.99954305691286,151.634295421181));
#158783=CARTESIAN_POINT('Ctrl Pts',(16.528594872203,3.06535254744676,151.633119685007));
#158784=CARTESIAN_POINT('Ctrl Pts',(16.5374637983434,3.13066082684022,151.63155585318));
#158785=CARTESIAN_POINT('Ctrl Pts',(16.5463769426455,3.1962947163476,151.629984224493));
#158786=CARTESIAN_POINT('Ctrl Pts',(16.5575132097492,3.26142305811755,151.6280206004));
#158787=CARTESIAN_POINT('Ctrl Pts',(16.5708839249923,3.32611207446319,151.625662984223));
#158788=CARTESIAN_POINT('Ctrl Pts',(16.5786271707001,3.36357476356017,151.624297642055));
#158789=CARTESIAN_POINT('Ctrl Pts',(16.587120749502,3.40088994557632,151.622799996355));
#158790=CARTESIAN_POINT('Ctrl Pts',(16.5963744098056,3.43806820585387,151.621168326374));
#158791=CARTESIAN_POINT('Ctrl Pts',(16.6155372509694,3.5150583992551,151.617789400449));
#158792=CARTESIAN_POINT('Ctrl Pts',(16.6378503686473,3.59147349031497,151.613854992147));
#158793=CARTESIAN_POINT('Ctrl Pts',(16.6632921003587,3.6669574847227,151.609368928814));
#158794=CARTESIAN_POINT('Ctrl Pts',(16.6886237454174,3.742114859057,151.604902276727));
#158795=CARTESIAN_POINT('Ctrl Pts',(16.7170570072394,3.81634864986932,151.599888727443));
#158796=CARTESIAN_POINT('Ctrl Pts',(16.7485197474872,3.88930711941047,151.594340998023));
#158797=CARTESIAN_POINT('Ctrl Pts',(16.7792847645072,3.96064764917713,151.588916296021));
#158798=CARTESIAN_POINT('Ctrl Pts',(16.8129461791987,4.03076832487788,151.58298088017));
#158799=CARTESIAN_POINT('Ctrl Pts',(16.8493895442315,4.09934729821385,151.576554931647));
#158800=CARTESIAN_POINT('Ctrl Pts',(16.8864091997694,4.16901073263477,151.570027367559));
#158801=CARTESIAN_POINT('Ctrl Pts',(16.9263312196188,4.23708316156678,151.562988036505));
#158802=CARTESIAN_POINT('Ctrl Pts',(16.9689085232936,4.30331911518685,151.555480501453));
#158803=CARTESIAN_POINT('Ctrl Pts',(16.9835773374774,4.32613885274841,151.552893991102));
#158804=CARTESIAN_POINT('Ctrl Pts',(16.9985611252097,4.34874102035924,151.550251942044));
#158805=CARTESIAN_POINT('Ctrl Pts',(17.0138492253656,4.37111689096524,151.547556235016));
#158806=CARTESIAN_POINT('',(17.7868045912878,5.1371366674824,151.411263364416));
#158807=CARTESIAN_POINT('Ctrl Pts',(17.013849229773,4.37111689096304,151.547556259993));
#158808=CARTESIAN_POINT('Ctrl Pts',(17.0874139946951,4.47878727439227,151.534584809587));
#158809=CARTESIAN_POINT('Ctrl Pts',(17.3140356434103,4.76667060199688,151.494625297278));
#158810=CARTESIAN_POINT('Ctrl Pts',(17.5873714274621,5.00446152832237,151.446428745532));
#158811=CARTESIAN_POINT('Ctrl Pts',(17.7868045798642,5.13713666751144,151.411263299869));
#158812=CARTESIAN_POINT('',(18.605129224176,4.01827646758674,149.770415815628));
#158813=CARTESIAN_POINT('Ctrl Pts',(17.7868045622877,5.13713666742147,151.411263199672));
#158814=CARTESIAN_POINT('Ctrl Pts',(17.8333695830196,5.10000197274449,151.40308003586));
#158815=CARTESIAN_POINT('Ctrl Pts',(17.8786263509401,5.06215449207173,151.39182828418));
#158816=CARTESIAN_POINT('Ctrl Pts',(17.9223569681114,5.02392012874832,151.377571697894));
#158817=CARTESIAN_POINT('Ctrl Pts',(17.9660416539441,4.98572592391336,151.363330085649));
#158818=CARTESIAN_POINT('Ctrl Pts',(18.0082031654458,4.94714599031353,151.346090043535));
#158819=CARTESIAN_POINT('Ctrl Pts',(18.0486598288029,4.90851753398444,151.325950997884));
#158820=CARTESIAN_POINT('Ctrl Pts',(18.089076324385,4.86992743027787,151.305831947471));
#158821=CARTESIAN_POINT('Ctrl Pts',(18.1277911741071,4.83128925917755,151.282819769792));
#158822=CARTESIAN_POINT('Ctrl Pts',(18.1646617998986,4.79294628030214,151.257047778563));
#158823=CARTESIAN_POINT('Ctrl Pts',(18.1819336501171,4.7749847140457,151.244975025177));
#158824=CARTESIAN_POINT('Ctrl Pts',(18.1988013706392,4.75708799228111,151.232297133882));
#158825=CARTESIAN_POINT('Ctrl Pts',(18.2152533744101,4.73929158706959,151.219030266785));
#158826=CARTESIAN_POINT('Ctrl Pts',(18.2457334285694,4.70632080720359,151.194451204364));
#158827=CARTESIAN_POINT('Ctrl Pts',(18.2748346125101,4.67364117953585,151.167807523998));
#158828=CARTESIAN_POINT('Ctrl Pts',(18.302455989941,4.64152037095539,151.139236557104));
#158829=CARTESIAN_POINT('Ctrl Pts',(18.3298880217829,4.60961975173487,151.110861445272));
#158830=CARTESIAN_POINT('Ctrl Pts',(18.3558604017593,4.578270864997,151.080585687432));
#158831=CARTESIAN_POINT('Ctrl Pts',(18.3803128993181,4.5477287180692,151.048578755568));
#158832=CARTESIAN_POINT('Ctrl Pts',(18.4050185665606,4.51687035208604,151.016240438953));
#158833=CARTESIAN_POINT('Ctrl Pts',(18.4281726447028,4.48683609445531,150.982135203747));
#158834=CARTESIAN_POINT('Ctrl Pts',(18.4497537930202,4.45787304836873,150.946469282319));
#158835=CARTESIAN_POINT('Ctrl Pts',(18.4713349413375,4.42891000228215,150.910803360891));
#158836=CARTESIAN_POINT('Ctrl Pts',(18.4913432679761,4.40101867870896,150.873577155597));
#158837=CARTESIAN_POINT('Ctrl Pts',(18.5097976222555,4.37442217458881,150.835022880457));
#158838=CARTESIAN_POINT('Ctrl Pts',(18.5292444217898,4.34639535359538,150.794395218905));
#158839=CARTESIAN_POINT('Ctrl Pts',(18.5462486579485,4.31943573437702,150.752388020248));
#158840=CARTESIAN_POINT('Ctrl Pts',(18.5609892954202,4.29383785418226,150.709206820558));
#158841=CARTESIAN_POINT('Ctrl Pts',(18.5757609439036,4.26818612176019,150.66593477726));
#158842=CARTESIAN_POINT('Ctrl Pts',(18.5882600126999,4.24390184679293,150.621483899194));
#158843=CARTESIAN_POINT('Ctrl Pts',(18.5986661429026,4.22123002260434,150.576071609115));
#158844=CARTESIAN_POINT('Ctrl Pts',(18.6090913275091,4.19851668460743,150.530576165732));
#158845=CARTESIAN_POINT('Ctrl Pts',(18.617416379132,4.17742164365807,150.484115911147));
#158846=CARTESIAN_POINT('Ctrl Pts',(18.6238137156254,4.1581403294452,150.436918302939));
#158847=CARTESIAN_POINT('Ctrl Pts',(18.6287640278216,4.14322028811149,150.400396401084));
#158848=CARTESIAN_POINT('Ctrl Pts',(18.6325599423428,4.12938523005701,150.36343318447));
#158849=CARTESIAN_POINT('Ctrl Pts',(18.6352754623615,4.11670530563327,150.326136917576));
#158850=CARTESIAN_POINT('Ctrl Pts',(18.6387914804342,4.10028751341469,150.277846222779));
#158851=CARTESIAN_POINT('Ctrl Pts',(18.6404971161023,4.08580781121885,150.228997108719));
#158852=CARTESIAN_POINT('Ctrl Pts',(18.6405359001165,4.07337555758929,150.179829108576));
#158853=CARTESIAN_POINT('Ctrl Pts',(18.6405747401186,4.06092535698763,150.130590130415));
#158854=CARTESIAN_POINT('Ctrl Pts',(18.638942151287,4.05052839958962,150.081031497016));
#158855=CARTESIAN_POINT('Ctrl Pts',(18.6357590644381,4.04224765948019,150.031396813581));
#158856=CARTESIAN_POINT('Ctrl Pts',(18.6325620265088,4.03393062589957,149.981544587398));
#158857=CARTESIAN_POINT('Ctrl Pts',(18.6278010355476,4.02774830027686,149.931615802684));
#158858=CARTESIAN_POINT('Ctrl Pts',(18.6215721414155,4.02371889111107,149.881857991779));
#158859=CARTESIAN_POINT('Ctrl Pts',(18.6169055376704,4.02070011193378,149.844580108773));
#158860=CARTESIAN_POINT('Ctrl Pts',(18.6114144783443,4.01888877449659,149.807398219849));
#158861=CARTESIAN_POINT('Ctrl Pts',(18.6051290423695,4.0182763981666,149.770415847677));
#158862=CARTESIAN_POINT('',(17.7320851166166,2.73630903683038,149.924354425571));
#158863=CARTESIAN_POINT('Origin',(19.0783287073222,2.73849310306824,149.686975357862));
#158864=CARTESIAN_POINT('Origin',(16.2505544908171,2.73391286142859,150.159005790699));
#158865=CARTESIAN_POINT('Origin',(19.0824366510928,-2.76149987721566,149.659668559686));
#158866=CARTESIAN_POINT('',(17.8030144592149,-5.16515196693523,151.408405127377));
#158867=CARTESIAN_POINT('',(17.0246388076071,-4.39725480535896,151.545653753608));
#158868=CARTESIAN_POINT('Ctrl Pts',(17.8030144477807,-5.16515196697007,
151.408405062833));
#158869=CARTESIAN_POINT('Ctrl Pts',(17.6031647754424,-5.03312458159598,
151.443643952118));
#158870=CARTESIAN_POINT('Ctrl Pts',(17.3277548264866,-4.79507474988715,
151.492206235477));
#158871=CARTESIAN_POINT('Ctrl Pts',(17.0993533621461,-4.50629347348466,
151.532479576936));
#158872=CARTESIAN_POINT('Ctrl Pts',(17.0246388097555,-4.3972548053579,151.545653765783));
#158873=CARTESIAN_POINT('',(16.5196805691194,-2.76608011964102,151.634691519724));
#158874=CARTESIAN_POINT('Ctrl Pts',(17.0246388054587,-4.39725480536002,
151.545653741432));
#158875=CARTESIAN_POINT('Ctrl Pts',(16.980179831894,-4.33237122813037,151.553493065376));
#158876=CARTESIAN_POINT('Ctrl Pts',(16.9382853629388,-4.26557476157888,
151.560880198771));
#158877=CARTESIAN_POINT('Ctrl Pts',(16.8992102235566,-4.19709416983573,
151.567770201294));
#158878=CARTESIAN_POINT('Ctrl Pts',(16.8866244911932,-4.17503721972902,
151.56998940586));
#158879=CARTESIAN_POINT('Ctrl Pts',(16.8743310868166,-4.15280592507466,
151.572157064749));
#158880=CARTESIAN_POINT('Ctrl Pts',(16.8623380347648,-4.1304089735751,151.574271763407));
#158881=CARTESIAN_POINT('Ctrl Pts',(16.8248877436378,-4.06047078349699,
151.580875260168));
#158882=CARTESIAN_POINT('Ctrl Pts',(16.7903359033042,-3.98891417475552,
151.586967682095));
#158883=CARTESIAN_POINT('Ctrl Pts',(16.7588050789201,-3.9160820073487,151.592527416549));
#158884=CARTESIAN_POINT('Ctrl Pts',(16.727125626097,-3.84290652727713,151.598113358203));
#158885=CARTESIAN_POINT('Ctrl Pts',(16.6984958086485,-3.76844397059384,
151.603161565509));
#158886=CARTESIAN_POINT('Ctrl Pts',(16.672988491886,-3.69304977473514,151.607659193346));
#158887=CARTESIAN_POINT('Ctrl Pts',(16.6480921897446,-3.61946160796379,
151.612049082827));
#158888=CARTESIAN_POINT('Ctrl Pts',(16.6261703394414,-3.54498638983783,
151.615914500064));
#158889=CARTESIAN_POINT('Ctrl Pts',(16.6072434948582,-3.46995433517785,
151.619251813424));
#158890=CARTESIAN_POINT('Ctrl Pts',(16.5910626489886,-3.40580829612739,
151.622104933121));
#158891=CARTESIAN_POINT('Ctrl Pts',(16.5771441731587,-3.34124760024139,
151.624559132651));
#158892=CARTESIAN_POINT('Ctrl Pts',(16.5654479168803,-3.27621426711835,
151.626621497644));
#158893=CARTESIAN_POINT('Ctrl Pts',(16.5537840579261,-3.21136106906744,
151.628678150116));
#158894=CARTESIAN_POINT('Ctrl Pts',(16.5443299721102,-3.14603718468865,
151.630345161695));
#158895=CARTESIAN_POINT('Ctrl Pts',(16.5370953273655,-3.08017315174642,
151.631620825864));
#158896=CARTESIAN_POINT('Ctrl Pts',(16.5299478482173,-3.01510267231301,
151.632881120374));
#158897=CARTESIAN_POINT('Ctrl Pts',(16.5249666064023,-2.94950433109478,
151.633759448475));
#158898=CARTESIAN_POINT('Ctrl Pts',(16.5222106325192,-2.88330921082613,
151.634245401212));
#158899=CARTESIAN_POINT('Ctrl Pts',(16.5205924674715,-2.84444286648317,
151.634530727476));
#158900=CARTESIAN_POINT('Ctrl Pts',(16.5197423899986,-2.80537079682772,
151.634680619052));
#158901=CARTESIAN_POINT('Ctrl Pts',(16.5196805691229,-2.76608012003402,
151.634691519741));
#158902=CARTESIAN_POINT('',(17.7407389282419,-2.76368394459876,149.922828525116));
#158903=CARTESIAN_POINT('Origin',(16.2592083024477,-2.7660801188553,150.157479890222));
#158904=CARTESIAN_POINT('',(18.6178127187803,-4.0428120877243,149.768179371269));
#158905=CARTESIAN_POINT('Origin',(19.0869825189528,-2.76149987721565,149.685449457386));
#158906=CARTESIAN_POINT('Ctrl Pts',(18.617812536877,-4.04281201894015,149.768179403335));
#158907=CARTESIAN_POINT('Ctrl Pts',(18.6247401961886,-4.0434875741113,149.808927579398));
#158908=CARTESIAN_POINT('Ctrl Pts',(18.6307224387778,-4.04558831789134,
149.850751083093));
#158909=CARTESIAN_POINT('Ctrl Pts',(18.6356396503344,-4.0493168664848,149.893503877485));
#158910=CARTESIAN_POINT('Ctrl Pts',(18.6404443940295,-4.05296013465421,
149.935278817803));
#158911=CARTESIAN_POINT('Ctrl Pts',(18.6442323371476,-4.05815801892354,
149.977941025346));
#158912=CARTESIAN_POINT('Ctrl Pts',(18.646863348556,-4.06507915814563,150.021321280173));
#158913=CARTESIAN_POINT('Ctrl Pts',(18.6495033041142,-4.07202382585026,
150.064849006613));
#158914=CARTESIAN_POINT('Ctrl Pts',(18.6509785664528,-4.08070406885189,
150.109099781635));
#158915=CARTESIAN_POINT('Ctrl Pts',(18.6511169129511,-4.09126184905199,
150.153868015298));
#158916=CARTESIAN_POINT('Ctrl Pts',(18.6512552594495,-4.10181962925208,
150.19863624896));
#158917=CARTESIAN_POINT('Ctrl Pts',(18.6500566898563,-4.11425558887344,
150.243921988825));
#158918=CARTESIAN_POINT('Ctrl Pts',(18.6473174902442,-4.12867414193584,
150.289483893473));
#158919=CARTESIAN_POINT('Ctrl Pts',(18.6447913376859,-4.14197126148257,
150.331502124447));
#158920=CARTESIAN_POINT('Ctrl Pts',(18.6409544671681,-4.15695459366357,
150.373754845816));
#158921=CARTESIAN_POINT('Ctrl Pts',(18.6356240268674,-4.1736703057728,150.416025570632));
#158922=CARTESIAN_POINT('Ctrl Pts',(18.6303765276118,-4.19012592330175,
150.457638567775));
#158923=CARTESIAN_POINT('Ctrl Pts',(18.6236813521633,-4.20826079186167,
150.499268906268));
#158924=CARTESIAN_POINT('Ctrl Pts',(18.6153450232028,-4.2280795345367,150.54068568822));
#158925=CARTESIAN_POINT('Ctrl Pts',(18.6071814355015,-4.24748760309108,
150.581244252233));
#158926=CARTESIAN_POINT('Ctrl Pts',(18.5974436983681,-4.26851076455874,
150.621597865278));
#158927=CARTESIAN_POINT('Ctrl Pts',(18.5859356427768,-4.29111059082044,
150.661508081389));
#158928=CARTESIAN_POINT('Ctrl Pts',(18.582139493849,-4.29856556925292,150.674673218011));
#158929=CARTESIAN_POINT('Ctrl Pts',(18.5781506118915,-4.30619174058161,
150.687789939588));
#158930=CARTESIAN_POINT('Ctrl Pts',(18.5739616953087,-4.3139865953369,150.700849202694));
#158931=CARTESIAN_POINT('Ctrl Pts',(18.5667904471748,-4.32733105720735,
150.723206109146));
#158932=CARTESIAN_POINT('Ctrl Pts',(18.559032968913,-4.34117019340261,150.745394719647));
#158933=CARTESIAN_POINT('Ctrl Pts',(18.5506519942545,-4.355487266246,150.767368082748));
#158934=CARTESIAN_POINT('Ctrl Pts',(18.5464615069252,-4.3626458026677,150.778354764298));
#158935=CARTESIAN_POINT('Ctrl Pts',(18.5421151592065,-4.36992380104806,
150.789287654068));
#158936=CARTESIAN_POINT('Ctrl Pts',(18.5376082142567,-4.3773185881527,150.800160647524));
#158937=CARTESIAN_POINT('Ctrl Pts',(18.5353547417818,-4.38101598170501,
150.805597144252));
#158938=CARTESIAN_POINT('Ctrl Pts',(18.5330611210657,-4.38474257067892,
150.81101866842));
#158939=CARTESIAN_POINT('Ctrl Pts',(18.5307267628424,-4.38849799834734,
150.816424455196));
#158940=CARTESIAN_POINT('Ctrl Pts',(18.5295595837308,-4.39037571218156,
150.819127348584));
#158941=CARTESIAN_POINT('Ctrl Pts',(18.5283822203052,-4.39226063559047,
150.82182630772));
#158942=CARTESIAN_POINT('Ctrl Pts',(18.5271945987749,-4.39415272176831,
150.824521236267));
#158943=CARTESIAN_POINT('Ctrl Pts',(18.526221894561,-4.39570240754895,150.826728478461));
#158944=CARTESIAN_POINT('Ctrl Pts',(18.5248709135798,-4.39784386759893,
150.829763064945));
#158945=CARTESIAN_POINT('Ctrl Pts',(18.5240538436865,-4.39913510367867,
150.831585101082));
#158946=CARTESIAN_POINT('Ctrl Pts',(18.5238733135046,-4.39942040006074,
150.83198767682));
#158947=CARTESIAN_POINT('Ctrl Pts',(18.5237189903995,-4.39966407142166,
150.832331198531));
#158948=CARTESIAN_POINT('Ctrl Pts',(18.5236008861957,-4.39985042090695,
150.832593833795));
#158949=CARTESIAN_POINT('Ctrl Pts',(18.5169837837748,-4.41029114689819,
150.847308673622));
#158950=CARTESIAN_POINT('Ctrl Pts',(18.5094035732404,-4.42195192080497,
150.863333569431));
#158951=CARTESIAN_POINT('Ctrl Pts',(18.5007046991651,-4.43493162585227,
150.880507535861));
#158952=CARTESIAN_POINT('Ctrl Pts',(18.492178102557,-4.44765427341244,150.897341379258));
#158953=CARTESIAN_POINT('Ctrl Pts',(18.4825765824297,-4.46164474473058,
150.915279447519));
#158954=CARTESIAN_POINT('Ctrl Pts',(18.4717247631423,-4.47699417422253,
150.934129532891));
#158955=CARTESIAN_POINT('Ctrl Pts',(18.4612660869295,-4.49178751982269,
150.952296711524));
#158956=CARTESIAN_POINT('Ctrl Pts',(18.4496458069598,-4.50784372002333,
150.971311078383));
#158957=CARTESIAN_POINT('Ctrl Pts',(18.4366827522023,-4.52523385814105,
150.990960683196));
#158958=CARTESIAN_POINT('Ctrl Pts',(18.4240133975992,-4.54222999296668,
151.010165092638));
#158959=CARTESIAN_POINT('Ctrl Pts',(18.4100611626767,-4.56050088978042,
151.029976374868));
#158960=CARTESIAN_POINT('Ctrl Pts',(18.394637062584,-4.58009421356124,151.050156624144));
#158961=CARTESIAN_POINT('Ctrl Pts',(18.3797843883863,-4.59896165171437,
151.069589243611));
#158962=CARTESIAN_POINT('Ctrl Pts',(18.36356653662,-4.61905581378937,151.089363930518));
#158963=CARTESIAN_POINT('Ctrl Pts',(18.3458006418009,-4.64039421716833,
151.109230676935));
#158964=CARTESIAN_POINT('Ctrl Pts',(18.3300948332558,-4.65925827560971,
151.126793727872));
#158965=CARTESIAN_POINT('Ctrl Pts',(18.3131788106762,-4.67909469083498,
151.144428244391));
#158966=CARTESIAN_POINT('Ctrl Pts',(18.2949200820071,-4.69989366150591,
151.161936176571));
#158967=CARTESIAN_POINT('Ctrl Pts',(18.2857552887525,-4.71033350480281,
151.170724114749));
#158968=CARTESIAN_POINT('Ctrl Pts',(18.276252137315,-4.72101549961146,151.179479781068));
#158969=CARTESIAN_POINT('Ctrl Pts',(18.2663936047421,-4.73193600197506,
151.188175816906));
#158970=CARTESIAN_POINT('Ctrl Pts',(18.2611983184977,-4.73769092901845,
151.192758486287));
#158971=CARTESIAN_POINT('Ctrl Pts',(18.25562747465,-4.74381594765354,151.197562783229));
#158972=CARTESIAN_POINT('Ctrl Pts',(18.2501128722837,-4.74983064582462,
151.202203432408));
#158973=CARTESIAN_POINT('Ctrl Pts',(18.2451630104228,-4.75522938957876,
151.206368841055));
#158974=CARTESIAN_POINT('Ctrl Pts',(18.2402590238559,-4.76053903323933,
151.210403073422));
#158975=CARTESIAN_POINT('Ctrl Pts',(18.2357348032586,-4.76540758764143,
151.214056119989));
#158976=CARTESIAN_POINT('Ctrl Pts',(18.2104452633172,-4.79262188861566,
151.234475961391));
#158977=CARTESIAN_POINT('Ctrl Pts',(18.1849808019506,-4.81917655659402,
151.252858774329));
#158978=CARTESIAN_POINT('Ctrl Pts',(18.159568537672,-4.84492883335936,151.269416046978));
#158979=CARTESIAN_POINT('Ctrl Pts',(18.1334500898831,-4.87139674227017,
151.286433431044));
#158980=CARTESIAN_POINT('Ctrl Pts',(18.1073871349694,-4.89701735989194,
151.301522906798));
#158981=CARTESIAN_POINT('Ctrl Pts',(18.0816053781645,-4.92168676407901,
151.314920793821));
#158982=CARTESIAN_POINT('Ctrl Pts',(18.0546865634699,-4.94744416784942,
151.328909570489));
#158983=CARTESIAN_POINT('Ctrl Pts',(18.0280746598158,-4.97216491409709,
151.341054792255));
#158984=CARTESIAN_POINT('Ctrl Pts',(18.0019983724429,-4.99578093615701,
151.351624537475));
#158985=CARTESIAN_POINT('Ctrl Pts',(17.9753055934216,-5.01995528464432,
151.362444171016));
#158986=CARTESIAN_POINT('Ctrl Pts',(17.9491742270689,-5.04297261980922,
151.371613467534));
#158987=CARTESIAN_POINT('Ctrl Pts',(17.9238166183558,-5.06480438672461,
151.379410864763));
#158988=CARTESIAN_POINT('Ctrl Pts',(17.8975602901792,-5.08740991090049,
151.387484615837));
#158989=CARTESIAN_POINT('Ctrl Pts',(17.8721336705373,-5.10874491376694,
151.394088022405));
#158990=CARTESIAN_POINT('Ctrl Pts',(17.8477350782245,-5.12881605336842,
151.399512408282));
#158991=CARTESIAN_POINT('Ctrl Pts',(17.8324094016906,-5.14142349355419,
151.402919669745));
#158992=CARTESIAN_POINT('Ctrl Pts',(17.8174885798052,-5.15353299626255,
151.405861348784));
#158993=CARTESIAN_POINT('Ctrl Pts',(17.8030144302228,-5.16515196687232,
151.408404962689));
#158994=CARTESIAN_POINT('Origin',(-3.46221193726519,-0.0437048830555943,
137.895785892187));
#158995=CARTESIAN_POINT('',(16.1274832823092,-0.0125284566453824,136.624761290332));
#158996=CARTESIAN_POINT('',(15.4719024191847,-0.0123825748629563,132.374023471094));
#158997=CARTESIAN_POINT('Ctrl Pts',(16.1278796078287,-0.012527862009953,
136.624691413793));
#158998=CARTESIAN_POINT('Ctrl Pts',(16.1280756600303,-0.147252630708614,
136.624656901064));
#158999=CARTESIAN_POINT('Ctrl Pts',(16.1260140219066,-0.281703535965217,
136.612160674053));
#159000=CARTESIAN_POINT('Ctrl Pts',(16.1184237857483,-0.550546425183159,
136.561598615638));
#159001=CARTESIAN_POINT('Ctrl Pts',(16.1127815881379,-0.684158670131424,
136.522886157832));
#159002=CARTESIAN_POINT('Ctrl Pts',(16.0999699315943,-0.900695439409687,
136.436931228838));
#159003=CARTESIAN_POINT('Ctrl Pts',(16.0938142045473,-0.985927359311978,
136.396487701947));
#159004=CARTESIAN_POINT('Ctrl Pts',(16.0774730187525,-1.179187317559,136.288758970976));
#159005=CARTESIAN_POINT('Ctrl Pts',(16.0667146508231,-1.28439591328589,
136.217237967408));
#159006=CARTESIAN_POINT('Ctrl Pts',(16.0477442990125,-1.43633696818377,
136.093006015257));
#159007=CARTESIAN_POINT('Ctrl Pts',(16.0406072535459,-1.48790350507802,
136.046492779664));
#159008=CARTESIAN_POINT('Ctrl Pts',(16.0180809062315,-1.63604495799591,
135.899176828029));
#159009=CARTESIAN_POINT('Ctrl Pts',(16.0017341497931,-1.72501087141097,
135.791412214741));
#159010=CARTESIAN_POINT('Ctrl Pts',(15.9484822225129,-1.95897592507266,
135.443568696062));
#159011=CARTESIAN_POINT('Ctrl Pts',(15.9084293170325,-2.06745293008694,
135.183131963649));
#159012=CARTESIAN_POINT('Ctrl Pts',(15.8454622575998,-2.14896862539609,
134.773809102494));
#159013=CARTESIAN_POINT('Ctrl Pts',(15.8242126961341,-2.16253104213606,
134.635901479587));
#159014=CARTESIAN_POINT('Ctrl Pts',(15.7600738513876,-2.16229456842722,
134.220112412375));
#159015=CARTESIAN_POINT('Ctrl Pts',(15.7176216288766,-2.10713461966444,
133.945253864148));
#159016=CARTESIAN_POINT('Ctrl Pts',(15.658003533512,-1.94659995619521,133.560448072899));
#159017=CARTESIAN_POINT('Ctrl Pts',(15.6389302244503,-1.88053411433489,
133.437714497772));
#159018=CARTESIAN_POINT('Ctrl Pts',(15.5849918526666,-1.64667906149591,
133.090062319416));
#159019=CARTESIAN_POINT('Ctrl Pts',(15.5541314319578,-1.44578832059754,
132.890481229408));
#159020=CARTESIAN_POINT('Ctrl Pts',(15.5104027469076,-1.03166236295503,
132.615596514834));
#159021=CARTESIAN_POINT('Ctrl Pts',(15.4963699054271,-0.834355542246234,
132.523574025011));
#159022=CARTESIAN_POINT('Ctrl Pts',(15.4775279834229,-0.427200653112934,
132.403665195811));
#159023=CARTESIAN_POINT('Ctrl Pts',(15.4719964486658,-0.220326112747798,
132.374007009116));
#159024=CARTESIAN_POINT('Ctrl Pts',(15.4715027782058,-0.0123835530891811,
132.374093927259));
#159025=CARTESIAN_POINT('',(18.4340776165402,-0.00878730969903237,136.218046482001));
#159026=CARTESIAN_POINT('',(-3.08886835528135,-0.0437048830555946,140.013122561163));
#159027=CARTESIAN_POINT('Origin',(18.0607340345509,-0.0087873096990321,
134.100709812994));
#159028=CARTESIAN_POINT('Ctrl Pts',(15.4723019669606,-0.0123818775344335,
132.373953008719));
#159029=CARTESIAN_POINT('Ctrl Pts',(15.4720739225224,0.122337644049303,
132.373993159465));
#159030=CARTESIAN_POINT('Ctrl Pts',(15.4734478511091,0.25678132131525,132.386609333691));
#159031=CARTESIAN_POINT('Ctrl Pts',(15.4805945056066,0.525616774422636,
132.437246534484));
#159032=CARTESIAN_POINT('Ctrl Pts',(15.4864564770072,0.659236057971183,
132.475920825168));
#159033=CARTESIAN_POINT('Ctrl Pts',(15.4994543432378,0.875785798846138,
132.561846679565));
#159034=CARTESIAN_POINT('Ctrl Pts',(15.5055005624332,0.961013695629594,
132.602308731372));
#159035=CARTESIAN_POINT('Ctrl Pts',(15.5217640239017,1.15425338252864,132.710038136568));
#159036=CARTESIAN_POINT('Ctrl Pts',(15.5327218200456,1.25946737867874,132.781523829943));
#159037=CARTESIAN_POINT('Ctrl Pts',(15.5515854786746,1.41143029625106,132.905791858573));
#159038=CARTESIAN_POINT('Ctrl Pts',(15.5586329892119,1.46300914551536,132.952333036519));
#159039=CARTESIAN_POINT('Ctrl Pts',(15.5810696143101,1.61114009658696,133.09965967983));
#159040=CARTESIAN_POINT('Ctrl Pts',(15.5976677826201,1.70009826756318,133.207367676168));
#159041=CARTESIAN_POINT('Ctrl Pts',(15.6509515974162,1.9340590641442,133.555197445029));
#159042=CARTESIAN_POINT('Ctrl Pts',(15.6908841576945,2.04253968408142,133.815655476476));
#159043=CARTESIAN_POINT('Ctrl Pts',(15.7539112731536,2.12405772760858,134.224977826637));
#159044=CARTESIAN_POINT('Ctrl Pts',(15.7751563397812,2.13762000308831,134.362886607084));
#159045=CARTESIAN_POINT('Ctrl Pts',(15.8392705263805,2.13738358102934,134.778675904911));
#159046=CARTESIAN_POINT('Ctrl Pts',(15.8817767412965,2.08222503727033,135.05352591926));
#159047=CARTESIAN_POINT('Ctrl Pts',(15.9413746662881,1.92168664483466,135.438343380605));
#159048=CARTESIAN_POINT('Ctrl Pts',(15.960375686495,1.85561760089108,135.561095264048));
#159049=CARTESIAN_POINT('Ctrl Pts',(16.0144310397426,1.62173151582931,135.90876638651));
#159050=CARTESIAN_POINT('Ctrl Pts',(16.0457627258355,1.42084183019191,136.108235901066));
#159051=CARTESIAN_POINT('Ctrl Pts',(16.0882048047342,1.00669224073221,136.383367061237));
#159052=CARTESIAN_POINT('Ctrl Pts',(16.1031585177866,0.809464228630117,
136.475177773857));
#159053=CARTESIAN_POINT('Ctrl Pts',(16.1226011363339,0.402306803369797,
136.594985487103));
#159054=CARTESIAN_POINT('Ctrl Pts',(16.1269248006866,0.195420549416648,
136.624859648122));
#159055=CARTESIAN_POINT('Ctrl Pts',(16.1270868790944,-0.0125287751724091,
136.624831193257));
#159056=CARTESIAN_POINT('Origin',(34.7113261754309,-17.2069969078973,150.45786679959));
#159057=CARTESIAN_POINT('',(34.7286909932009,-17.2069969078973,150.55634757489));
#159058=CARTESIAN_POINT('',(34.1022561745275,-15.848549783591,150.666804935116));
#159059=CARTESIAN_POINT('',(34.7286909932009,-17.2069969078973,150.55634757489));
#159060=CARTESIAN_POINT('',(34.0848913567676,-15.848549783591,150.568324159816));
#159061=CARTESIAN_POINT('',(34.0848913567676,-15.848549783591,150.568324159816));
#159062=CARTESIAN_POINT('',(34.7113261754309,-17.2069969078973,150.45786679959));
#159063=CARTESIAN_POINT('',(34.7113261754309,-17.2069969078973,150.45786679959));
#159064=CARTESIAN_POINT('',(34.7113261754309,-17.2069969078973,150.45786679959));
#159065=CARTESIAN_POINT('Origin',(26.7764851389615,-2.04263841746052E-14,
151.856993361954));
#159066=CARTESIAN_POINT('',(43.7647022487539,-8.00222469971588,148.963054992579));
#159067=CARTESIAN_POINT('Origin',(26.7938499567315,-1.48611011759408E-14,
151.955474137254));
#159068=CARTESIAN_POINT('',(43.7473374309938,-8.00222469971587,148.864574217279));
#159069=CARTESIAN_POINT('Origin',(26.7764851389615,-2.04263841746052E-14,
151.856993361954));
#159070=CARTESIAN_POINT('',(43.7473374309938,-8.00222469971587,148.864574217279));
#159071=CARTESIAN_POINT('Origin',(26.7938499567315,-1.48611011759408E-14,
151.955474137254));
#159072=CARTESIAN_POINT('',(42.4248981204347,-7.37047011815913,149.199298609248));
#159073=CARTESIAN_POINT('Origin',(26.7938499567315,-1.48611011759408E-14,
151.955474137254));
#159074=CARTESIAN_POINT('',(42.4248981204347,-7.37047011815913,149.199298609248));
#159075=CARTESIAN_POINT('Origin',(26.7764851389615,-2.04263841746052E-14,
151.856993361954));
#159076=CARTESIAN_POINT('',(42.4075333026747,-7.37047011815912,149.100817833948));
#159077=CARTESIAN_POINT('Origin',(26.7764851389615,-2.04263841746052E-14,
151.856993361954));
#159078=CARTESIAN_POINT('',(42.4075333026747,-7.37047011815912,149.100817833948));
#159079=CARTESIAN_POINT('Origin',(42.4075333026747,-7.37047011815912,149.100817833948));
#159080=CARTESIAN_POINT('',(42.4075333026747,-7.37047011815912,149.100817833948));
#159081=CARTESIAN_POINT('Origin',(26.7938499567315,-1.48611011759408E-14,
151.955474137254));
#159082=CARTESIAN_POINT('',(43.7394339176877,8.05724874950928,148.967510481072));
#159083=CARTESIAN_POINT('',(34.6745028823554,17.232655043704,150.565902400871));
#159084=CARTESIAN_POINT('Origin',(26.7938499567315,-1.48611011759408E-14,
151.955474137254));
#159085=CARTESIAN_POINT('',(34.052346072443,15.8721822770942,150.675605432751));
#159086=CARTESIAN_POINT('',(34.6745028823554,17.232655043704,150.565902400871));
#159087=CARTESIAN_POINT('',(42.4016246576106,7.42115016402197,149.20340234871));
#159088=CARTESIAN_POINT('Origin',(26.7938499567315,-1.48611011759408E-14,
151.955474137254));
#159089=CARTESIAN_POINT('',(42.4016246576106,7.42115016402197,149.20340234871));
#159090=CARTESIAN_POINT('Origin',(26.7764851389615,-2.04263841746052E-14,
151.856993361954));
#159091=CARTESIAN_POINT('',(34.6571380645954,17.232655043704,150.467421625571));
#159092=CARTESIAN_POINT('',(34.6571380645954,17.232655043704,150.467421625571));
#159093=CARTESIAN_POINT('',(43.7220690999277,8.05724874950929,148.869029705772));
#159094=CARTESIAN_POINT('',(43.7220690999277,8.05724874950929,148.869029705772));
#159095=CARTESIAN_POINT('Origin',(26.7764851389615,-2.04263841746052E-14,
151.856993361954));
#159096=CARTESIAN_POINT('Origin',(34.6571380645954,17.232655043704,150.467421625571));
#159097=CARTESIAN_POINT('',(34.034981254673,15.8721822770942,150.577124657451));
#159098=CARTESIAN_POINT('',(34.034981254673,15.8721822770942,150.577124657451));
#159099=CARTESIAN_POINT('',(34.6571380645954,17.232655043704,150.467421625571));
#159100=CARTESIAN_POINT('Origin',(26.7764851389615,-2.04263841746052E-14,
151.856993361954));
#159101=CARTESIAN_POINT('',(42.3842598398506,7.42115016402198,149.10492157341));
#159102=CARTESIAN_POINT('',(42.3842598398506,7.42115016402198,149.10492157341));
#159103=CARTESIAN_POINT('Origin',(26.7764851389615,-2.04263841746052E-14,
151.856993361954));
#159104=CARTESIAN_POINT('Origin',(42.3842598398506,7.42115016402198,149.10492157341));
#159105=CARTESIAN_POINT('',(42.3842598398506,7.42115016402198,149.10492157341));
#159106=CARTESIAN_POINT('Origin',(16.7219736911164,-6.50941809057164,128.751923016915));
#159107=CARTESIAN_POINT('',(16.7219736911164,-6.50941809057164,128.751923016915));
#159108=CARTESIAN_POINT('',(20.3737087297297,-6.87643093232191,149.458564755529));
#159109=CARTESIAN_POINT('',(16.7219736911164,-6.50941809057164,128.751923016915));
#159110=CARTESIAN_POINT('',(27.5548451481147,-6.49184346932355,126.841795500437));
#159111=CARTESIAN_POINT('',(16.7219736911164,-6.50941809057164,128.751923016915));
#159112=CARTESIAN_POINT('',(31.2065801874991,-6.8588563110934,147.548437240149));
#159113=CARTESIAN_POINT('',(27.5548451481147,-6.49184346932355,126.841795500437));
#159114=CARTESIAN_POINT('',(31.2065802141502,-6.85885631372248,147.548437388466));
#159115=CARTESIAN_POINT('Origin',(29.3788505316782,-5.49184474563557,137.195444817487));
#159116=CARTESIAN_POINT('',(28.5380782239063,-5.49024705279486,126.668424980917));
#159117=CARTESIAN_POINT('Origin',(27.5532717278182,-5.49184474563557,126.842072936887));
#159118=CARTESIAN_POINT('',(32.5506728884128,-5.48966067834193,147.311437431176));
#159119=CARTESIAN_POINT('',(28.5380782239063,-5.49024705279486,126.668424980917));
#159120=CARTESIAN_POINT('Origin',(31.2044292741582,-5.49184474563556,147.548816349987));
#159121=CARTESIAN_POINT('Origin',(28.5380782239063,-5.49024705279486,126.668424980917));
#159122=CARTESIAN_POINT('',(28.5207706006449,5.50973890777291,126.671476781869));
#159123=CARTESIAN_POINT('',(28.5380782239063,-5.49024705279486,126.668424980917));
#159124=CARTESIAN_POINT('',(32.5333652653764,5.51032528280824,147.314489233291));
#159125=CARTESIAN_POINT('',(28.5207706006449,5.50973890777291,126.671476781869));
#159126=CARTESIAN_POINT('',(32.5333652941263,5.51032528330627,147.314489381211));
#159127=CARTESIAN_POINT('Origin',(29.3615429084169,5.5081412149322,137.19849661844));
#159128=CARTESIAN_POINT('',(27.5343906842604,6.50813993862018,126.84540217429));
#159129=CARTESIAN_POINT('Origin',(27.5359641045569,5.5081412149322,126.84512473784));
#159130=CARTESIAN_POINT('',(31.1849707906507,6.87515278037055,147.552247558648));
#159131=CARTESIAN_POINT('',(27.5343906842604,6.50813993862018,126.84540217429));
#159132=CARTESIAN_POINT('Origin',(31.1871216508969,5.5081412149322,147.55186815094));
#159133=CARTESIAN_POINT('Origin',(27.5343906842604,6.50813993862018,126.84540217429));
#159134=CARTESIAN_POINT('',(16.7015192294221,6.4905653173756,128.755529690369));
#159135=CARTESIAN_POINT('',(27.5343906842604,6.50813993862018,126.84540217429));
#159136=CARTESIAN_POINT('',(20.3520993354489,6.85757815914594,149.46237507597));
#159137=CARTESIAN_POINT('',(16.7015192294221,6.4905653173756,128.755529690369));
#159138=CARTESIAN_POINT('',(20.3520993611167,6.85757816177451,149.462375224439));
#159139=CARTESIAN_POINT('Origin',(20.0759123749787,8.35691092392083,149.484491984831));
#159140=CARTESIAN_POINT('',(31.4385374584628,8.37491358353456,149.00409452878));
#159141=CARTESIAN_POINT('Origin',(31.1780651780795,8.3749224115792,147.526882901754));
#159142=CARTESIAN_POINT('',(20.6056660035708,8.3573389629198,150.914222044819));
#159143=CARTESIAN_POINT('Origin',(20.3451937232412,8.35734779033466,149.437010417732));
#159144=CARTESIAN_POINT('',(20.6056659874021,8.35734778978584,150.914222047732));
#159145=CARTESIAN_POINT('Origin',(31.1825758355569,5.50814121493218,147.52608755114));
#159146=CARTESIAN_POINT('',(34.2662677573925,5.51272144253028,148.505489382891));
#159147=CARTESIAN_POINT('Origin',(34.005804184202,5.51272145657184,147.028276220504));
#159148=CARTESIAN_POINT('Origin',(31.4430481020469,5.50814121493219,149.00329918054));
#159149=CARTESIAN_POINT('Origin',(34.0053739547706,5.78615690368945,147.02835208156));
#159150=CARTESIAN_POINT('',(34.2835753800336,-5.48726451810046,148.502437582047));
#159151=CARTESIAN_POINT('Origin',(34.0231118074634,-5.48726450399593,147.025224419551));
#159152=CARTESIAN_POINT('',(34.2662764501683,5.51272145895295,148.505487850204));
#159153=CARTESIAN_POINT('Origin',(31.1998834588183,-5.49184474563559,147.523035750187));
#159154=CARTESIAN_POINT('',(31.4648663689593,-8.35861711486726,148.999452031481));
#159155=CARTESIAN_POINT('Origin',(31.2043941162956,-8.35862594228162,147.522240399573));
#159156=CARTESIAN_POINT('Origin',(31.4603557253082,-5.49184474563557,149.000247379587));
#159157=CARTESIAN_POINT('Origin',(31.4736754645682,-8.35818907586777,147.474758832475));
#159158=CARTESIAN_POINT('',(20.6319949119108,-8.3761917354855,150.909579547881));
#159159=CARTESIAN_POINT('Origin',(20.3715226593074,-8.37620056352966,149.432367915951));
#159160=CARTESIAN_POINT('',(31.4648663851448,-8.35862594173281,148.999452028673));
#159161=CARTESIAN_POINT('Origin',(20.36701200183,-5.50941936688363,149.433163266565));
#159162=CARTESIAN_POINT('',(17.8042733066227,-5.51399958031571,151.408183160806));
#159163=CARTESIAN_POINT('',(19.0253142554132,-5.51160343525972,149.696323083178));
#159164=CARTESIAN_POINT('Origin',(17.5437836531848,-5.51399960852327,149.930974597102));
#159165=CARTESIAN_POINT('Origin',(20.37155781716,-5.50941936688365,149.458943866465));
#159166=CARTESIAN_POINT('Origin',(20.62748426831,-5.50941936688363,150.910374895965));
#159167=CARTESIAN_POINT('Origin',(18.54597907469,-5.50941936688364,139.105572333965));
#159168=CARTESIAN_POINT('',(15.7355937747319,-5.51101705972437,128.925848409336));
#159169=CARTESIAN_POINT('',(15.7355937747319,-5.51101705972437,128.925848409336));
#159170=CARTESIAN_POINT('Origin',(16.72040027082,-5.50941936688366,128.752200453365));
#159171=CARTESIAN_POINT('Origin',(15.7342146708969,-4.63451757771262,128.926091582552));
#159172=CARTESIAN_POINT('',(19.0239390506279,-4.63510509600238,149.696590864325));
#159173=CARTESIAN_POINT('',(19.0253142789822,-5.51160343624773,149.696323231995));
#159174=CARTESIAN_POINT('',(15.7342146642767,-4.63451676584635,128.926091509742));
#159175=CARTESIAN_POINT('',(19.023940582593,-4.63510509608687,149.696600544993));
#159176=CARTESIAN_POINT('',(15.7342146544329,-4.6345167235289,128.926091486888));
#159177=CARTESIAN_POINT('Origin',(17.5670013172358,-20.2701550170947,149.926880696501));
#159178=CARTESIAN_POINT('Ctrl Pts',(17.8042733066227,-5.51399958031571,
151.408183160806));
#159179=CARTESIAN_POINT('Ctrl Pts',(17.8040727766663,-5.39760138028505,
151.408218519755));
#159180=CARTESIAN_POINT('Ctrl Pts',(17.803197591333,-5.28155019758945,151.40837276968));
#159181=CARTESIAN_POINT('Ctrl Pts',(17.8030144477807,-5.16515196697007,
151.408405062833));
#159182=CARTESIAN_POINT('Ctrl Pts',(17.8030145110624,-5.16515196693421,
151.408405421157));
#159183=CARTESIAN_POINT('Ctrl Pts',(17.8032686440368,-5.16506456763226,
151.408360570365));
#159184=CARTESIAN_POINT('Ctrl Pts',(17.8035227301876,-5.16497718304309,
151.40831566124));
#159185=CARTESIAN_POINT('Ctrl Pts',(17.8037767695064,-5.16488981316054,
151.408270693831));
#159186=CARTESIAN_POINT('Ctrl Pts',(17.862944075151,-5.14454083502309,151.397797510206));
#159187=CARTESIAN_POINT('Ctrl Pts',(17.9195683479851,-5.12498821356407,
151.384163610296));
#159188=CARTESIAN_POINT('Ctrl Pts',(17.9735593295081,-5.10616350562641,
151.367997328169));
#159189=CARTESIAN_POINT('Ctrl Pts',(18.0141603152175,-5.09200740628533,
151.355840353596));
#159190=CARTESIAN_POINT('Ctrl Pts',(18.0532723727275,-5.07826346323026,
151.342251170234));
#159191=CARTESIAN_POINT('Ctrl Pts',(18.0908765654888,-5.06490598702596,
151.327492702657));
#159192=CARTESIAN_POINT('Ctrl Pts',(18.1306829185968,-5.05076627612203,
151.311869956134));
#159193=CARTESIAN_POINT('Ctrl Pts',(18.1687985096706,-5.03706161899898,
151.294938929714));
#159194=CARTESIAN_POINT('Ctrl Pts',(18.2051782310708,-5.02382494627252,
151.277032580921));
#159195=CARTESIAN_POINT('Ctrl Pts',(18.2421925228161,-5.01035738667676,
151.258813892245));
#159196=CARTESIAN_POINT('Ctrl Pts',(18.2774097802937,-4.99737420617687,
151.23958542498));
#159197=CARTESIAN_POINT('Ctrl Pts',(18.3108227210156,-4.98488683732149,
151.219669746269));
#159198=CARTESIAN_POINT('Ctrl Pts',(18.3257831989105,-4.97929568007251,
151.210752600257));
#159199=CARTESIAN_POINT('Ctrl Pts',(18.3403824934267,-4.97380362102034,
151.201697325601));
#159200=CARTESIAN_POINT('Ctrl Pts',(18.3546224893735,-4.96841030642996,
151.192531168065));
#159201=CARTESIAN_POINT('Ctrl Pts',(18.3847289059392,-4.95700767848437,
151.173151938035));
#159202=CARTESIAN_POINT('Ctrl Pts',(18.4132283127862,-4.94604727726768,
151.153278696366));
#159203=CARTESIAN_POINT('Ctrl Pts',(18.4401695613823,-4.93552410333679,
151.133157868164));
#159204=CARTESIAN_POINT('Ctrl Pts',(18.4715173128486,-4.923279762105,151.109746083091));
#159205=CARTESIAN_POINT('Ctrl Pts',(18.5007912709236,-4.91161856435262,
151.085973610496));
#159206=CARTESIAN_POINT('Ctrl Pts',(18.5281149683316,-4.90054938866558,
151.062158444953));
#159207=CARTESIAN_POINT('Ctrl Pts',(18.5480297397248,-4.89248166269037,
151.044800853468));
#159208=CARTESIAN_POINT('Ctrl Pts',(18.5669090859487,-4.88472795998422,
151.027419554606));
#159209=CARTESIAN_POINT('Ctrl Pts',(18.5848077147215,-4.87728530986754,
151.01012314597));
#159210=CARTESIAN_POINT('Ctrl Pts',(18.6041734638248,-4.86923259830776,
150.991408979969));
#159211=CARTESIAN_POINT('Ctrl Pts',(18.6223913498396,-4.86154427010307,
150.972794478652));
#159212=CARTESIAN_POINT('Ctrl Pts',(18.6395346836216,-4.85422093190089,
150.95440742827));
#159213=CARTESIAN_POINT('Ctrl Pts',(18.6625785148652,-4.8443770023702,150.92969181044));
#159214=CARTESIAN_POINT('Ctrl Pts',(18.6836843450984,-4.83519218394656,
150.90538522494));
#159215=CARTESIAN_POINT('Ctrl Pts',(18.703043268029,-4.82666826822253,150.881742670367));
#159216=CARTESIAN_POINT('Ctrl Pts',(18.7066722600945,-4.8250703889066,150.877310675712));
#159217=CARTESIAN_POINT('Ctrl Pts',(18.7102398675248,-4.82349567172762,
150.872901881842));
#159218=CARTESIAN_POINT('Ctrl Pts',(18.7137473492472,-4.8219440464152,150.86851778913));
#159219=CARTESIAN_POINT('Ctrl Pts',(18.7248564520267,-4.81702964730051,
150.854632232375));
#159220=CARTESIAN_POINT('Ctrl Pts',(18.7353624974549,-4.81234775577349,
150.840994780032));
#159221=CARTESIAN_POINT('Ctrl Pts',(18.7453055442633,-4.8078983210624,150.827649249466));
#159222=CARTESIAN_POINT('Ctrl Pts',(18.7502770676675,-4.80567360370686,
150.820976484183));
#159223=CARTESIAN_POINT('Ctrl Pts',(18.7551077977608,-4.80350700062168,
150.814376668407));
#159224=CARTESIAN_POINT('Ctrl Pts',(18.7598027413949,-4.80139850535284,
150.807854732614));
#159225=CARTESIAN_POINT('Ctrl Pts',(18.7621502132119,-4.80034425771842,
150.804593764717));
#159226=CARTESIAN_POINT('Ctrl Pts',(18.7644637355996,-4.79930453704117,
150.801352264728));
#159227=CARTESIAN_POINT('Ctrl Pts',(18.7667439227061,-4.79827934252448,
150.798130829766));
#159228=CARTESIAN_POINT('Ctrl Pts',(18.7678840162594,-4.79776674526614,
150.796520112284));
#159229=CARTESIAN_POINT('Ctrl Pts',(18.7690157758177,-4.79725777954814,
150.79491441094));
#159230=CARTESIAN_POINT('Ctrl Pts',(18.7701392779379,-4.79675244527051,
150.793313798456));
#159231=CARTESIAN_POINT('Ctrl Pts',(18.7711622488311,-4.7962923284198,150.791856409145));
#159232=CARTESIAN_POINT('Ctrl Pts',(18.7715594121143,-4.79611369840959,
150.791290836496));
#159233=CARTESIAN_POINT('Ctrl Pts',(18.7730216399206,-4.79545584278048,
150.789192685758));
#159234=CARTESIAN_POINT('Ctrl Pts',(18.7731653385895,-4.7953911928143,150.788986492532));
#159235=CARTESIAN_POINT('Ctrl Pts',(18.7733192946451,-4.79532192767035,
150.788765471694));
#159236=CARTESIAN_POINT('Ctrl Pts',(18.7734850880704,-4.79524733665902,
150.788527299497));
#159237=CARTESIAN_POINT('Ctrl Pts',(18.7735686544069,-4.79520973988732,
150.788407251444));
#159238=CARTESIAN_POINT('Ctrl Pts',(18.7736522009151,-4.79517214962227,
150.788287194308));
#159239=CARTESIAN_POINT('Ctrl Pts',(18.7737357275941,-4.79513456586254,
150.788167128097));
#159240=CARTESIAN_POINT('Ctrl Pts',(18.7994173117021,-4.78357885099189,
150.751250893089));
#159241=CARTESIAN_POINT('Ctrl Pts',(18.8232225180652,-4.77263971823976,
150.713480061588));
#159242=CARTESIAN_POINT('Ctrl Pts',(18.8451390713033,-4.76233225449921,
150.675080910954));
#159243=CARTESIAN_POINT('Ctrl Pts',(18.8660880089645,-4.75247986516592,
150.638377082384));
#159244=CARTESIAN_POINT('Ctrl Pts',(18.8853114789135,-4.74320466491597,
150.601099478334));
#159245=CARTESIAN_POINT('Ctrl Pts',(18.902818577608,-4.7345010424511,150.563405237081));
#159246=CARTESIAN_POINT('Ctrl Pts',(18.9072890851304,-4.73227853771856,
150.553779862139));
#159247=CARTESIAN_POINT('Ctrl Pts',(18.9116477734959,-4.73009320328575,
150.544127096179));
#159248=CARTESIAN_POINT('Ctrl Pts',(18.9158949898502,-4.72794474002493,
150.534449081862));
#159249=CARTESIAN_POINT('Ctrl Pts',(18.9321731474239,-4.71971040002829,
150.497356494878));
#159250=CARTESIAN_POINT('Ctrl Pts',(18.9468132378253,-4.71201873441901,
150.459896796704));
#159251=CARTESIAN_POINT('Ctrl Pts',(18.9598456409741,-4.70487992765189,
150.422248501799));
#159252=CARTESIAN_POINT('Ctrl Pts',(18.9726834715103,-4.69784770263092,
150.385162292567));
#159253=CARTESIAN_POINT('Ctrl Pts',(18.9839615301877,-4.69135194893011,
150.347893225263));
#159254=CARTESIAN_POINT('Ctrl Pts',(18.9937149473093,-4.68538848733506,
150.310563172745));
#159255=CARTESIAN_POINT('Ctrl Pts',(18.9980741755566,-4.68272315579916,
150.293878741291));
#159256=CARTESIAN_POINT('Ctrl Pts',(19.0021289006343,-4.68016396806322,
150.277181459132));
#159257=CARTESIAN_POINT('Ctrl Pts',(19.0058824151226,-4.67770968246238,
150.260478952394));
#159258=CARTESIAN_POINT('Ctrl Pts',(19.0071873230318,-4.67685645099038,
150.254672332169));
#159259=CARTESIAN_POINT('Ctrl Pts',(19.0084558267926,-4.67601589330426,
150.24886506311));
#159260=CARTESIAN_POINT('Ctrl Pts',(19.0096881718686,-4.67518789459185,
150.243057804819));
#159261=CARTESIAN_POINT('Ctrl Pts',(19.0177907306694,-4.66974387701547,
150.204875600259));
#159262=CARTESIAN_POINT('Ctrl Pts',(19.0243258691249,-4.66479586263019,
150.166725395175));
#159263=CARTESIAN_POINT('Ctrl Pts',(19.0293672876622,-4.66039573729584,
150.128732829071));
#159264=CARTESIAN_POINT('Ctrl Pts',(19.0346499413677,-4.65578506309171,
150.088922293875));
#159265=CARTESIAN_POINT('Ctrl Pts',(19.0382926601038,-4.6517758526121,150.049284581529));
#159266=CARTESIAN_POINT('Ctrl Pts',(19.0403583521838,-4.64842129637797,
150.009911502095));
#159267=CARTESIAN_POINT('Ctrl Pts',(19.0409159290519,-4.64751582601433,
149.999283820201));
#159268=CARTESIAN_POINT('Ctrl Pts',(19.0413584816065,-4.64665802362371,
149.988675149452));
#159269=CARTESIAN_POINT('Ctrl Pts',(19.0416869720438,-4.64584887936723,
149.978086731175));
#159270=CARTESIAN_POINT('Ctrl Pts',(19.0428991363296,-4.64286305190253,
149.939014353356));
#159271=CARTESIAN_POINT('Ctrl Pts',(19.0425602936179,-4.64053893606678,
149.900221237493));
#159272=CARTESIAN_POINT('Ctrl Pts',(19.0407796597806,-4.63882574119599,
149.861866673758));
#159273=CARTESIAN_POINT('Ctrl Pts',(19.0389238726557,-4.63704023936122,
149.821893320412));
#159274=CARTESIAN_POINT('Ctrl Pts',(19.0355022508431,-4.63591816343537,
149.782395926731));
#159275=CARTESIAN_POINT('Ctrl Pts',(19.0306062369459,-4.63541455822507,
149.743509320325));
#159276=CARTESIAN_POINT('Ctrl Pts',(19.0286247156489,-4.63521073845036,
149.727771080937));
#159277=CARTESIAN_POINT('Ctrl Pts',(19.0264013147576,-4.63510837488812,
149.712132419708));
#159278=CARTESIAN_POINT('Ctrl Pts',(19.0239405861026,-4.6351050960812,149.696600544437));
#159279=CARTESIAN_POINT('Ctrl Pts',(17.6621982343867,-5.08983843849182,
151.41501950764));
#159280=CARTESIAN_POINT('Ctrl Pts',(17.6847306497354,-5.07160503979059,
151.411230178286));
#159281=CARTESIAN_POINT('Ctrl Pts',(17.7859585568119,-4.98827094266869,
151.390595823914));
#159282=CARTESIAN_POINT('Ctrl Pts',(17.9528371002266,-4.8392053876882,151.327196400169));
#159283=CARTESIAN_POINT('Ctrl Pts',(18.1412192519315,-4.64592260348376,
151.191964020737));
#159284=CARTESIAN_POINT('Ctrl Pts',(18.290663302471,-4.46611281318578,151.013567428543));
#159285=CARTESIAN_POINT('Ctrl Pts',(18.3989836624423,-4.30756139525972,
150.800619385748));
#159286=CARTESIAN_POINT('Ctrl Pts',(18.4664123754855,-4.17761345587552,
150.562907468878));
#159287=CARTESIAN_POINT('Ctrl Pts',(18.4959930732887,-4.08166751220023,
150.310538928411));
#159288=CARTESIAN_POINT('Ctrl Pts',(18.4927145236842,-4.02235496188064,
150.052984722078));
#159289=CARTESIAN_POINT('Ctrl Pts',(18.4685252055117,-4.00488505051922,
149.854449636007));
#159290=CARTESIAN_POINT('Ctrl Pts',(18.4477123504894,-4.00541093234517,
149.744136010205));
#159291=CARTESIAN_POINT('Ctrl Pts',(18.4423888805384,-4.0061290882458,149.718123679723));
#159292=CARTESIAN_POINT('Ctrl Pts',(17.8515417284861,-5.40956555909364,
151.471675872937));
#159293=CARTESIAN_POINT('Ctrl Pts',(17.8765946229952,-5.39089090765192,
151.470972088971));
#159294=CARTESIAN_POINT('Ctrl Pts',(17.9897535980413,-5.3046331251463,151.464325699469));
#159295=CARTESIAN_POINT('Ctrl Pts',(18.1813513235114,-5.14333102257086,
151.424477159));
#159296=CARTESIAN_POINT('Ctrl Pts',(18.4073681596413,-4.92052595862295,
151.31364703635));
#159297=CARTESIAN_POINT('Ctrl Pts',(18.5972951085453,-4.69933599657195,
151.14777762627));
#159298=CARTESIAN_POINT('Ctrl Pts',(18.7454331128204,-4.49100697775858,
150.931283323269));
#159299=CARTESIAN_POINT('Ctrl Pts',(18.8481060957408,-4.30814243871773,
150.670238207001));
#159300=CARTESIAN_POINT('Ctrl Pts',(18.9039096879475,-4.16387944968833,
150.37340949851));
#159301=CARTESIAN_POINT('Ctrl Pts',(18.9136043748492,-4.06987311790436,
150.052640225632));
#159302=CARTESIAN_POINT('Ctrl Pts',(18.8872116191077,-4.04226503063461,
149.797795335174));
#159303=CARTESIAN_POINT('Ctrl Pts',(18.8606390219642,-4.04409959522934,
149.65595859604));
#159304=CARTESIAN_POINT('Ctrl Pts',(18.8537000884272,-4.04552153588302,
149.622549665771));
#159305=CARTESIAN_POINT('Ctrl Pts',(17.9453265591402,-5.68136644548878,
151.229565777176));
#159306=CARTESIAN_POINT('Ctrl Pts',(17.9699637161583,-5.66659577633329,
151.230975467175));
#159307=CARTESIAN_POINT('Ctrl Pts',(18.0816307292424,-5.59777282493662,
151.234694595341));
#159308=CARTESIAN_POINT('Ctrl Pts',(18.274376104946,-5.46432194190647,151.218538751389));
#159309=CARTESIAN_POINT('Ctrl Pts',(18.5118820460989,-5.26934063561602,
151.145798229773));
#159310=CARTESIAN_POINT('Ctrl Pts',(18.7224658531959,-5.06521421683433,
151.01979784497));
#159311=CARTESIAN_POINT('Ctrl Pts',(18.8983183234987,-4.86277986153453,
150.839733266627));
#159312=CARTESIAN_POINT('Ctrl Pts',(19.0316797298042,-4.67617937190132,
150.606963224139));
#159313=CARTESIAN_POINT('Ctrl Pts',(19.1158310094995,-4.52247914657655,
150.326911047139));
#159314=CARTESIAN_POINT('Ctrl Pts',(19.1458603127157,-4.4192415037174,150.011520850732));
#159315=CARTESIAN_POINT('Ctrl Pts',(19.1258473951864,-4.38916359743563,
149.755721082763));
#159316=CARTESIAN_POINT('Ctrl Pts',(19.0992158962855,-4.39200367109623,
149.613897663077));
#159317=CARTESIAN_POINT('Ctrl Pts',(19.0920562581333,-4.39379506526226,
149.580569593459));
#159318=CARTESIAN_POINT('Ctrl Pts',(17.8767193898592,-5.71154921833711,
150.861222724773));
#159319=CARTESIAN_POINT('Ctrl Pts',(17.8983008572918,-5.70224569438056,
150.86226770474));
#159320=CARTESIAN_POINT('Ctrl Pts',(17.9961160866383,-5.65879160865082,
150.865343185256));
#159321=CARTESIAN_POINT('Ctrl Pts',(18.1656197374524,-5.57343226026813,
150.8561378627));
#159322=CARTESIAN_POINT('Ctrl Pts',(18.3802817903841,-5.44379286700894,
150.808030716389));
#159323=CARTESIAN_POINT('Ctrl Pts',(18.5769758391995,-5.30301381326858,
150.720829569143));
#159324=CARTESIAN_POINT('Ctrl Pts',(18.7486895990784,-5.15794570622578,
150.591209998157));
#159325=CARTESIAN_POINT('Ctrl Pts',(18.8863142702363,-5.01945224373198,
150.418173801994));
#159326=CARTESIAN_POINT('Ctrl Pts',(18.9807367833996,-4.90191979379112,
150.204179494235));
#159327=CARTESIAN_POINT('Ctrl Pts',(19.0239711438131,-4.82149176558256,
149.958929257427));
#159328=CARTESIAN_POINT('Ctrl Pts',(19.0143749134135,-4.79837244989064,
149.758210007737));
#159329=CARTESIAN_POINT('Ctrl Pts',(18.9934273279386,-4.80119830885926,
149.647926848569));
#159330=CARTESIAN_POINT('Ctrl Pts',(18.9875990235869,-4.80276154379444,
149.622099476749));
#159331=CARTESIAN_POINT('Origin',(18.4005666698389,-4.63611527055336,149.806488332022));
#159332=CARTESIAN_POINT('Origin',(16.5749874807289,-4.63611527055335,139.453114266522));
#159333=CARTESIAN_POINT('',(15.202263756867,-3.70950744065599,129.683973252045));
#159334=CARTESIAN_POINT('',(18.6178095147825,-4.04281182632481,149.768159429233));
#159335=CARTESIAN_POINT('Origin',(14.9369722812793,-4.63608791228591,130.064673259349));
#159336=CARTESIAN_POINT('Ctrl Pts',(15.6326354081712,0.0908296618712509,
137.316474337295));
#159337=CARTESIAN_POINT('Ctrl Pts',(15.8266313658842,0.0821951493031128,
137.044680273464));
#159338=CARTESIAN_POINT('Ctrl Pts',(16.0206273235873,0.0735606367349667,
136.772886209534));
#159339=CARTESIAN_POINT('Ctrl Pts',(16.2146232813003,0.0649261241668086,
136.501092145703));
#159340=CARTESIAN_POINT('Ctrl Pts',(15.6339880746382,-0.0834675886911582,
137.323205056148));
#159341=CARTESIAN_POINT('Ctrl Pts',(15.8278573503132,-0.0770410283918743,
137.050831116014));
#159342=CARTESIAN_POINT('Ctrl Pts',(16.0217266259883,-0.0706144680925627,
136.778457175779));
#159343=CARTESIAN_POINT('Ctrl Pts',(16.2155959016633,-0.0641879077932888,
136.506083235644));
#159344=CARTESIAN_POINT('Ctrl Pts',(15.6309087180474,-0.490284867328187,
137.299711347775));
#159345=CARTESIAN_POINT('Ctrl Pts',(15.8250778738318,-0.448705023318383,
137.029361549055));
#159346=CARTESIAN_POINT('Ctrl Pts',(16.0192470296262,-0.407125179308591,
136.759011750435));
#159347=CARTESIAN_POINT('Ctrl Pts',(16.2134161854106,-0.365545335298786,
136.488661951715));
#159348=CARTESIAN_POINT('Ctrl Pts',(15.6033825426741,-1.12583594967189,
137.120216729638));
#159349=CARTESIAN_POINT('Ctrl Pts',(15.8001894098461,-1.02933748521726,
136.865331428465));
#159350=CARTESIAN_POINT('Ctrl Pts',(15.9969962770082,-0.932839020763151,
136.610446127291));
#159351=CARTESIAN_POINT('Ctrl Pts',(16.1938031441802,-0.836340556308595,
136.355560826018));
#159352=CARTESIAN_POINT('Ctrl Pts',(15.5449483970485,-1.75570002821504,
136.746489385655));
#159353=CARTESIAN_POINT('Ctrl Pts',(15.7473444668466,-1.60477390395317,
136.523802803418));
#159354=CARTESIAN_POINT('Ctrl Pts',(15.9497405366547,-1.45384777969131,
136.30111622128));
#159355=CARTESIAN_POINT('Ctrl Pts',(16.1521366064528,-1.30292165543043,
136.078429639043));
#159356=CARTESIAN_POINT('Ctrl Pts',(15.4617593776569,-2.26668159677003,
136.218359273874));
#159357=CARTESIAN_POINT('Ctrl Pts',(15.6721069301266,-2.07160013148221,
136.041174053354));
#159358=CARTESIAN_POINT('Ctrl Pts',(15.8824544825962,-1.8765186661934,135.863988832833));
#159359=CARTESIAN_POINT('Ctrl Pts',(16.0928020350659,-1.68143720090556,
135.686803612212));
#159360=CARTESIAN_POINT('Ctrl Pts',(15.3618046767863,-2.6146082031803,135.58649639665));
#159361=CARTESIAN_POINT('Ctrl Pts',(15.5817024284862,-2.38946079206905,
135.46374967683));
#159362=CARTESIAN_POINT('Ctrl Pts',(15.8016001801861,-2.16431338095777,
135.341002956909));
#159363=CARTESIAN_POINT('Ctrl Pts',(16.021497931886,-1.93916596984552,135.218256237088));
#159364=CARTESIAN_POINT('Ctrl Pts',(15.2522266269535,-2.78470879606595,
134.895948354886));
#159365=CARTESIAN_POINT('Ctrl Pts',(15.4825910225606,-2.54486131186758,
134.832696174107));
#159366=CARTESIAN_POINT('Ctrl Pts',(15.7129554181676,-2.30501382766823,
134.769443993427));
#159367=CARTESIAN_POINT('Ctrl Pts',(15.9433198137746,-2.06516634346886,
134.706191812648));
#159368=CARTESIAN_POINT('Ctrl Pts',(15.1396605412371,-2.77118141126198,
134.188484376818));
#159369=CARTESIAN_POINT('Ctrl Pts',(15.3807742998572,-2.53250117447683,
134.186184123501));
#159370=CARTESIAN_POINT('Ctrl Pts',(15.6218880584774,-2.29382093769172,
134.183883870284));
#159371=CARTESIAN_POINT('Ctrl Pts',(15.8630018170975,-2.05514070090757,
134.181583616967));
#159372=CARTESIAN_POINT('Ctrl Pts',(15.0305921321479,-2.57491612832342,
133.504865240957));
#159373=CARTESIAN_POINT('Ctrl Pts',(15.2821186291523,-2.35319364293089,
133.561462537436));
#159374=CARTESIAN_POINT('Ctrl Pts',(15.5336451261467,-2.13147115753737,
133.618059833915));
#159375=CARTESIAN_POINT('Ctrl Pts',(15.7851716231411,-1.90974867214482,
133.674657130294));
#159376=CARTESIAN_POINT('Ctrl Pts',(14.9316301076284,-2.20286413122342,
132.886563257347));
#159377=CARTESIAN_POINT('Ctrl Pts',(15.1926017157584,-2.01328934411237,
132.996430657771));
#159378=CARTESIAN_POINT('Ctrl Pts',(15.4535733238983,-1.82371455700229,
133.106298058095));
#159379=CARTESIAN_POINT('Ctrl Pts',(15.7145449320382,-1.63413976989123,
133.216165458519));
#159380=CARTESIAN_POINT('Ctrl Pts',(14.849904498969,-1.67305154249018,132.378215214644));
#159381=CARTESIAN_POINT('Ctrl Pts',(15.1186729626689,-1.52925686142635,
132.531879568582));
#159382=CARTESIAN_POINT('Ctrl Pts',(15.3874414263788,-1.38546218036253,
132.68554392262));
#159383=CARTESIAN_POINT('Ctrl Pts',(15.6562098900787,-1.2416674992987,132.839208276557));
#159384=CARTESIAN_POINT('Ctrl Pts',(14.793162055357,-1.02580630728256,132.028107883375));
#159385=CARTESIAN_POINT('Ctrl Pts',(15.0673399157224,-0.937939500879029,
132.211935871462));
#159386=CARTESIAN_POINT('Ctrl Pts',(15.3415177760977,-0.85007269447598,
132.395763859549));
#159387=CARTESIAN_POINT('Ctrl Pts',(15.6156956364631,-0.762205888072875,
132.579591847736));
#159388=CARTESIAN_POINT('Ctrl Pts',(14.7690193246188,-0.429827561211837,
131.882404280965));
#159389=CARTESIAN_POINT('Ctrl Pts',(15.0454941881122,-0.393459152817816,
132.078785396901));
#159390=CARTESIAN_POINT('Ctrl Pts',(15.3219690516056,-0.357090744423894,
132.275166512837));
#159391=CARTESIAN_POINT('Ctrl Pts',(15.5984439150991,-0.320722336029973,
132.471547628773));
#159392=CARTESIAN_POINT('Ctrl Pts',(14.7661244244312,-0.0562448076138019,
131.868005288716));
#159393=CARTESIAN_POINT('Ctrl Pts',(15.0428703976198,-0.0521577867173374,
132.065626930907));
#159394=CARTESIAN_POINT('Ctrl Pts',(15.3196163708083,-0.0480707658208829,
132.263248573098));
#159395=CARTESIAN_POINT('Ctrl Pts',(15.5963623440068,-0.0439837449244126,
132.460870215289));
#159396=CARTESIAN_POINT('Ctrl Pts',(14.7667334772298,0.0886098244785636,
131.873306754642));
#159397=CARTESIAN_POINT('Ctrl Pts',(15.0434192179426,0.0801798916379546,
132.070471636069));
#159398=CARTESIAN_POINT('Ctrl Pts',(15.3201049586553,0.0717499587973433,
132.267636517396));
#159399=CARTESIAN_POINT('Ctrl Pts',(15.596790699368,0.0633200259567142,
132.464801398824));
#159400=CARTESIAN_POINT('',(15.7204620888588,-0.013326943698867,137.195385296531));
#159401=CARTESIAN_POINT('Origin',(227.634194189643,0.131638934550563,287.921260411963));
#159402=CARTESIAN_POINT('',(14.8912321715194,-0.0131815370763207,131.959834448354));
#159403=CARTESIAN_POINT('Origin',(168.294554533299,0.439697821287936,-82.4898013238501));
#159404=CARTESIAN_POINT('Ctrl Pts',(15.7205398917825,-0.0133270177734878,
137.195877603114));
#159405=CARTESIAN_POINT('Ctrl Pts',(15.7210832648335,-0.362848575696153,
137.195739139215));
#159406=CARTESIAN_POINT('Ctrl Pts',(15.7105102208732,-0.714886006099241,
137.125388679336));
#159407=CARTESIAN_POINT('Ctrl Pts',(15.6729215390833,-1.30198405806983,
136.882067817117));
#159408=CARTESIAN_POINT('Ctrl Pts',(15.6454643677425,-1.60729537011807,
136.705592307119));
#159409=CARTESIAN_POINT('Ctrl Pts',(15.5631895994256,-2.13639793975214,
136.180726786475));
#159410=CARTESIAN_POINT('Ctrl Pts',(15.5178003232202,-2.33085785365462,
135.892164379888));
#159411=CARTESIAN_POINT('Ctrl Pts',(15.4177062562099,-2.59550999840174,
135.25749269031));
#159412=CARTESIAN_POINT('Ctrl Pts',(15.3641108455972,-2.66344085160448,
134.918410851475));
#159413=CARTESIAN_POINT('Ctrl Pts',(15.2555256364223,-2.66303508426177,
134.232834867303));
#159414=CARTESIAN_POINT('Ctrl Pts',(15.2017550777324,-2.59480606967409,
133.894037601806));
#159415=CARTESIAN_POINT('Ctrl Pts',(15.1011070518146,-2.33030164433699,
133.261271906951));
#159416=CARTESIAN_POINT('Ctrl Pts',(15.055158835653,-2.13624050986265,132.973147927333));
#159417=CARTESIAN_POINT('Ctrl Pts',(14.9700712795838,-1.5999752670426,132.44140230918));
#159418=CARTESIAN_POINT('Ctrl Pts',(14.9422731326707,-1.29173136487026,
132.269039366159));
#159419=CARTESIAN_POINT('Ctrl Pts',(14.9140989162941,-0.874949693559167,
132.095410361788));
#159420=CARTESIAN_POINT('Ctrl Pts',(14.9056757258523,-0.705283371614432,
132.043960993393));
#159421=CARTESIAN_POINT('Ctrl Pts',(14.8944282106145,-0.360086125972263,
131.976471995303));
#159422=CARTESIAN_POINT('Ctrl Pts',(14.8915614467703,-0.187041438110135,
131.960139027468));
#159423=CARTESIAN_POINT('Ctrl Pts',(14.8913098915074,-0.0131819538729922,
131.960326159532));
#159424=CARTESIAN_POINT('Ctrl Pts',(14.766880881743,-0.117682776752729,
131.872322017485));
#159425=CARTESIAN_POINT('Ctrl Pts',(15.0435746463364,-0.108286228136295,
132.06958563023));
#159426=CARTESIAN_POINT('Ctrl Pts',(15.3202684109298,-0.0988896795198714,
132.266849242975));
#159427=CARTESIAN_POINT('Ctrl Pts',(15.5969621755232,-0.0894931309034575,
132.46411285572));
#159428=CARTESIAN_POINT('Ctrl Pts',(14.7655281944518,0.0566164276715459,
131.865591195374));
#159429=CARTESIAN_POINT('Ctrl Pts',(15.0423486518352,0.0509506755153907,
132.063434734082));
#159430=CARTESIAN_POINT('Ctrl Pts',(15.3191691092286,0.0452849233592512,
132.261278272791));
#159431=CARTESIAN_POINT('Ctrl Pts',(15.5959895666119,0.0396191712030961,
132.459121811499));
#159432=CARTESIAN_POINT('Ctrl Pts',(14.7686075831621,0.463438098286559,
131.889085123866));
#159433=CARTESIAN_POINT('Ctrl Pts',(15.0451281366027,0.422616210984097,
132.084904359668));
#159434=CARTESIAN_POINT('Ctrl Pts',(15.3216486900533,0.381794323681724,
132.280723595571));
#159435=CARTESIAN_POINT('Ctrl Pts',(15.5981692434938,0.340972436379235,
132.476542831474));
#159436=CARTESIAN_POINT('Ctrl Pts',(14.7961340834777,1.09899596056801,132.068581651183));
#159437=CARTESIAN_POINT('Ctrl Pts',(15.0700167119187,1.00325100517306,132.248935137205));
#159438=CARTESIAN_POINT('Ctrl Pts',(15.3438993403696,0.907506049779131,
132.429288623227));
#159439=CARTESIAN_POINT('Ctrl Pts',(15.6177819688205,0.811761094384798,
132.60964210925));
#159440=CARTESIAN_POINT('Ctrl Pts',(14.8545689042686,1.72886661379578,132.44231288469));
#159441=CARTESIAN_POINT('Ctrl Pts',(15.1228618787092,1.57868960320719,132.590465051457));
#159442=CARTESIAN_POINT('Ctrl Pts',(15.3911548531599,1.42851259261963,132.738617218224));
#159443=CARTESIAN_POINT('Ctrl Pts',(15.6594478276006,1.27833558203105,132.886769384991));
#159444=CARTESIAN_POINT('Ctrl Pts',(14.9377588841678,2.23985351617292,132.970448492951));
#159445=CARTESIAN_POINT('Ctrl Pts',(15.1980997338175,2.04551759872797,133.073095623512));
#159446=CARTESIAN_POINT('Ctrl Pts',(15.4584405834572,1.851181681283,133.175742754073));
#159447=CARTESIAN_POINT('Ctrl Pts',(15.7187814331068,1.65684576383804,133.278389884633));
#159448=CARTESIAN_POINT('Ctrl Pts',(15.037714738664,2.58778375445155,133.602317946183));
#159449=CARTESIAN_POINT('Ctrl Pts',(15.2885046178437,2.36337946316326,133.65052217977));
#159450=CARTESIAN_POINT('Ctrl Pts',(15.5392944970234,2.13897517187496,133.698726413357));
#159451=CARTESIAN_POINT('Ctrl Pts',(15.7900843762032,1.91457088058667,133.746930646944));
#159452=CARTESIAN_POINT('Ctrl Pts',(15.1472940528428,2.75788612305896,134.292873174639));
#159453=CARTESIAN_POINT('Ctrl Pts',(15.3876164428632,2.51878057155707,134.281578064556));
#159454=CARTESIAN_POINT('Ctrl Pts',(15.6279388328837,2.27967502005419,134.270282954472));
#159455=CARTESIAN_POINT('Ctrl Pts',(15.8682612228942,2.04056946855229,134.258987844389));
#159456=CARTESIAN_POINT('Ctrl Pts',(15.2598614370511,2.74435859725416,135.000344515569));
#159457=CARTESIAN_POINT('Ctrl Pts',(15.4894335959701,2.50642038742937,134.928092555749));
#159458=CARTESIAN_POINT('Ctrl Pts',(15.7190057548991,2.2684821776046,134.855840595929));
#159459=CARTESIAN_POINT('Ctrl Pts',(15.9485779138282,2.03054396777882,134.783588636109));
#159460=CARTESIAN_POINT('Ctrl Pts',(15.3689311039534,2.54809126587522,135.683970765961));
#159461=CARTESIAN_POINT('Ctrl Pts',(15.5880896836034,2.32711217689028,135.552816500125));
#159462=CARTESIAN_POINT('Ctrl Pts',(15.8072482632634,2.10613308790537,135.42166223419));
#159463=CARTESIAN_POINT('Ctrl Pts',(16.0264068429134,1.88515399892043,135.290507968354));
#159464=CARTESIAN_POINT('Ctrl Pts',(15.4678942694229,2.17603538543718,136.302279184494));
#159465=CARTESIAN_POINT('Ctrl Pts',(15.6776069751826,1.98720659087041,136.117850512733));
#159466=CARTESIAN_POINT('Ctrl Pts',(15.8873196809323,1.79837779630263,135.933421840973));
#159467=CARTESIAN_POINT('Ctrl Pts',(16.097032386692,1.60954900173483,135.748993169312));
#159468=CARTESIAN_POINT('Ctrl Pts',(15.5496208199135,1.64621726661601,136.810632517662));
#159469=CARTESIAN_POINT('Ctrl Pts',(15.7515360404562,1.50317227513574,136.582403355514));
#159470=CARTESIAN_POINT('Ctrl Pts',(15.9534512609989,1.36012728365549,136.354174193265));
#159471=CARTESIAN_POINT('Ctrl Pts',(16.1553664815517,1.21708229217522,136.125945031116));
#159472=CARTESIAN_POINT('Ctrl Pts',(15.6063639169654,0.998965275500975,
137.160743492757));
#159473=CARTESIAN_POINT('Ctrl Pts',(15.8028693039962,0.911852675220866,
136.902348260412));
#159474=CARTESIAN_POINT('Ctrl Pts',(15.9993746910371,0.824740074940445,
136.643953028167));
#159475=CARTESIAN_POINT('Ctrl Pts',(16.1958800780679,0.737627474659937,
136.385557795822));
#159476=CARTESIAN_POINT('Ctrl Pts',(15.6305069308838,0.40298016741526,137.306448645902));
#159477=CARTESIAN_POINT('Ctrl Pts',(15.8247151287538,0.367370136173505,
137.035499269165));
#159478=CARTESIAN_POINT('Ctrl Pts',(16.0189233266237,0.331760104931878,
136.764549892329));
#159479=CARTESIAN_POINT('Ctrl Pts',(16.2131315244937,0.29615007369015,136.493600515492));
#159480=CARTESIAN_POINT('Ctrl Pts',(15.6334018603134,0.0293933703536851,
137.320847764629));
#159481=CARTESIAN_POINT('Ctrl Pts',(15.8273389269369,0.026067345982975,
137.048657763365));
#159482=CARTESIAN_POINT('Ctrl Pts',(16.0212759935504,0.0227413216122492,
136.7764677621));
#159483=CARTESIAN_POINT('Ctrl Pts',(16.2152130601639,0.0194152972415234,
136.504277760835));
#159484=CARTESIAN_POINT('Ctrl Pts',(15.6327927962462,-0.11546291508241,
137.315546216845));
#159485=CARTESIAN_POINT('Ctrl Pts',(15.8267901005858,-0.106270962677035,
137.043813015627));
#159486=CARTESIAN_POINT('Ctrl Pts',(16.0207874049254,-0.0970790102716011,
136.77207981431));
#159487=CARTESIAN_POINT('Ctrl Pts',(16.214784709265,-0.0878870578661855,
136.500346613092));
#159488=CARTESIAN_POINT('Ctrl Pts',(14.8911540502061,-0.0131814635361809,
131.959342221145));
#159489=CARTESIAN_POINT('Ctrl Pts',(14.8906106762576,0.336340102835657,
131.959480679464));
#159490=CARTESIAN_POINT('Ctrl Pts',(14.901183720497,0.688377558217891,132.029831141429));
#159491=CARTESIAN_POINT('Ctrl Pts',(14.938772402906,1.275475620005,132.273152007657));
#159492=CARTESIAN_POINT('Ctrl Pts',(14.9662295743078,1.58078693156106,132.44962751801));
#159493=CARTESIAN_POINT('Ctrl Pts',(15.0485043424753,2.10988950019956,132.974493037701));
#159494=CARTESIAN_POINT('Ctrl Pts',(15.0938936187016,2.30434941420721,133.26305544435));
#159495=CARTESIAN_POINT('Ctrl Pts',(15.1939876857224,2.56900155900805,133.897727133996));
#159496=CARTESIAN_POINT('Ctrl Pts',(15.2475830963336,2.63693241219933,134.236808972806));
#159497=CARTESIAN_POINT('Ctrl Pts',(15.3561683054966,2.63652664485352,134.922384956904));
#159498=CARTESIAN_POINT('Ctrl Pts',(15.4099388641883,2.56829763029012,135.261182222416));
#159499=CARTESIAN_POINT('Ctrl Pts',(15.5105868901176,2.30379320491567,135.893947917343));
#159500=CARTESIAN_POINT('Ctrl Pts',(15.5565351062835,2.10973207046068,136.182071896982));
#159501=CARTESIAN_POINT('Ctrl Pts',(15.6416226623923,1.57346682728598,136.713817515381));
#159502=CARTESIAN_POINT('Ctrl Pts',(15.669420809299,1.26522292492855,136.886180458388));
#159503=CARTESIAN_POINT('Ctrl Pts',(15.6975949609052,0.848442211693935,
137.059809063598));
#159504=CARTESIAN_POINT('Ctrl Pts',(15.7060181182242,0.678776904425043,
137.11125823324));
#159505=CARTESIAN_POINT('Ctrl Pts',(15.7172656973454,0.333579735722459,
137.178747635459));
#159506=CARTESIAN_POINT('Ctrl Pts',(15.7201324941116,0.160534015214026,
137.195080800611));
#159507=CARTESIAN_POINT('Ctrl Pts',(15.7203840504836,-0.0133265274405875,
137.194893664742));
#159508=CARTESIAN_POINT('Origin',(17.3095324658322,2.73849310306822,139.655633390962));
#159509=CARTESIAN_POINT('',(14.6493737823773,2.73685851198427,130.460883875229));
#159510=CARTESIAN_POINT('',(14.6493737823824,2.73685851198428,130.460883875214));
#159511=CARTESIAN_POINT('',(15.190628493629,3.68536951497202,129.686024863033));
#159512=CARTESIAN_POINT('',(18.605126018521,4.01827620696241,149.770395858136));
#159513=CARTESIAN_POINT('Origin',(15.465028260172,2.73846506067834,129.296006976405));
#159514=CARTESIAN_POINT('Origin',(14.4423646123641,2.73689541022749,129.153879602933));
#159515=CARTESIAN_POINT('',(14.6580275938616,-2.76313446829959,130.459357973818));
#159516=CARTESIAN_POINT('',(14.6580275938631,-2.76313446829959,130.459357973838));
#159517=CARTESIAN_POINT('',(17.7407389282425,-2.76368394498376,149.922828525115));
#159518=CARTESIAN_POINT('',(14.6493737823824,2.73685851198428,130.460883875214));
#159519=CARTESIAN_POINT('Origin',(17.3181862774528,-2.76149987721566,139.654107490386));
#159520=CARTESIAN_POINT('Origin',(15.4736820716518,-2.76152791963452,129.294481074998));
#159521=CARTESIAN_POINT('Origin',(16.2596385318791,-3.0395155659729,150.157404029166));
#159522=CARTESIAN_POINT('',(16.5196805691196,-2.76608012003402,151.634691519722));
#159523=CARTESIAN_POINT('Ctrl Pts',(17.8587892544387,5.68406649606213,150.864384285181));
#159524=CARTESIAN_POINT('Ctrl Pts',(17.8803999009861,5.67483034719617,150.86542412206));
#159525=CARTESIAN_POINT('Ctrl Pts',(17.9783508188883,5.63168282830363,150.868475560104));
#159526=CARTESIAN_POINT('Ctrl Pts',(18.1481232811645,5.54686197137129,150.859223056995));
#159527=CARTESIAN_POINT('Ctrl Pts',(18.3631933945532,5.41792464037205,150.811043805684));
#159528=CARTESIAN_POINT('Ctrl Pts',(18.5603311747761,5.27781203285765,150.723763167653));
#159529=CARTESIAN_POINT('Ctrl Pts',(18.7325001095741,5.13335675005504,150.594062243622));
#159530=CARTESIAN_POINT('Ctrl Pts',(18.8705588995167,4.9953934251543,150.420948432272));
#159531=CARTESIAN_POINT('Ctrl Pts',(18.9653527121365,4.87827436336384,150.206882039047));
#159532=CARTESIAN_POINT('Ctrl Pts',(19.0088360698327,4.79812181747546,149.961586023878));
#159533=CARTESIAN_POINT('Ctrl Pts',(18.9993099063281,4.77508671018202,149.760856024253));
#159534=CARTESIAN_POINT('Ctrl Pts',(18.9783553383453,4.77790752850252,149.650584360981));
#159535=CARTESIAN_POINT('Ctrl Pts',(18.9725221022922,4.77946670473843,149.624757783732));
#159536=CARTESIAN_POINT('Ctrl Pts',(17.9274913897233,5.65389539357561,151.232710594697));
#159537=CARTESIAN_POINT('Ctrl Pts',(17.9521749134293,5.63920153970202,151.234112111453));
#159538=CARTESIAN_POINT('Ctrl Pts',(18.0640572892245,5.57072866697129,151.237793130604));
#159539=CARTESIAN_POINT('Ctrl Pts',(18.2572228552344,5.43789323666701,151.221563446129));
#159540=CARTESIAN_POINT('Ctrl Pts',(18.4953424478875,5.24369949655056,151.148714398131));
#159541=CARTESIAN_POINT('Ctrl Pts',(18.7065692305997,5.0403044694732,151.02259877758));
#159542=CARTESIAN_POINT('Ctrl Pts',(18.8830571520153,4.83852431651492,150.842420720756));
#159543=CARTESIAN_POINT('Ctrl Pts',(19.0170038617902,4.65247420324261,150.609546302775));
#159544=CARTESIAN_POINT('Ctrl Pts',(19.1016398885586,4.49919095857635,150.329399715761));
#159545=CARTESIAN_POINT('Ctrl Pts',(19.131989851798,4.39622729952393,150.013951395625));
#159546=CARTESIAN_POINT('Ctrl Pts',(19.1120690066584,4.36623211354187,149.75813710317));
#159547=CARTESIAN_POINT('Ctrl Pts',(19.0854310415134,4.36906675560282,149.616328332059));
#159548=CARTESIAN_POINT('Ctrl Pts',(19.078265766194,4.37085406194063,149.583001271904));
#159549=CARTESIAN_POINT('Ctrl Pts',(17.8345625406965,5.38166643196077,151.474669762255));
#159550=CARTESIAN_POINT('Ctrl Pts',(17.859674084597,5.36307109482329,151.473955637923));
#159551=CARTESIAN_POINT('Ctrl Pts',(17.9731032668532,5.27717402724323,151.46726152533));
#159552=CARTESIAN_POINT('Ctrl Pts',(18.1652088286427,5.11649686441713,151.427323582462));
#159553=CARTESIAN_POINT('Ctrl Pts',(18.3919267981537,4.89446435532081,151.316369237397));
#159554=CARTESIAN_POINT('Ctrl Pts',(18.5825501347808,4.67396298072739,151.150374696084));
#159555=CARTESIAN_POINT('Ctrl Pts',(18.7313420940797,4.46622141098541,150.933763687288));
#159556=CARTESIAN_POINT('Ctrl Pts',(18.8345887567204,4.2838265090382,150.672616487709));
#159557=CARTESIAN_POINT('Ctrl Pts',(18.8908467441566,4.13990089484537,150.375698246391));
#159558=CARTESIAN_POINT('Ctrl Pts',(18.900833820193,4.04610736667316,150.054876766821));
#159559=CARTESIAN_POINT('Ctrl Pts',(18.8745260848819,4.01856092057753,149.800018647566));
#159560=CARTESIAN_POINT('Ctrl Pts',(18.847950180088,4.02039035674692,149.658196016061));
#159561=CARTESIAN_POINT('Ctrl Pts',(18.8410067777837,4.02180896773098,149.624787894765));
#159562=CARTESIAN_POINT('Ctrl Pts',(17.6462260514748,5.06137654967593,151.417835836187));
#159563=CARTESIAN_POINT('Ctrl Pts',(17.6688157410725,5.043216242298,151.414036406879));
#159564=CARTESIAN_POINT('Ctrl Pts',(17.7703047866832,4.96021304129056,151.393356019318));
#159565=CARTESIAN_POINT('Ctrl Pts',(17.9376526209387,4.81170767838965,151.329873819149));
#159566=CARTESIAN_POINT('Ctrl Pts',(18.1266429371576,4.61909262015257,151.194533432453));
#159567=CARTESIAN_POINT('Ctrl Pts',(18.2766528928194,4.4398513668303,151.016034714885));
#159568=CARTESIAN_POINT('Ctrl Pts',(18.385470753359,4.28176008337927,150.80299793715));
#159569=CARTESIAN_POINT('Ctrl Pts',(18.4533069975848,4.15215760050746,150.56521364884));
#159570=CARTESIAN_POINT('Ctrl Pts',(18.4831895690037,4.05644295646414,150.312784178972));
#159571=CARTESIAN_POINT('Ctrl Pts',(18.4800953507138,3.99726594629036,150.055197728674));
#159572=CARTESIAN_POINT('Ctrl Pts',(18.4559599690146,3.97983202742149,149.856654856497));
#159573=CARTESIAN_POINT('Ctrl Pts',(18.4351473563841,3.98035356208065,149.746351489287));
#159574=CARTESIAN_POINT('Ctrl Pts',(18.4298216273155,3.98106939347749,149.720339494746));
#159575=CARTESIAN_POINT('',(19.0093911677908,4.61188418703687,149.699165991196));
#159576=CARTESIAN_POINT('Ctrl Pts',(19.0093911677908,4.61188418703687,149.699165991196));
#159577=CARTESIAN_POINT('Ctrl Pts',(19.015500537071,4.61189015756661,149.737727855937));
#159578=CARTESIAN_POINT('Ctrl Pts',(19.0201475819771,4.61250126401147,149.776952028307));
#159579=CARTESIAN_POINT('Ctrl Pts',(19.0232524053809,4.61375762212829,149.816717483555));
#159580=CARTESIAN_POINT('Ctrl Pts',(19.0262253202089,4.61496060380839,149.854793501472));
#159581=CARTESIAN_POINT('Ctrl Pts',(19.0277840966013,4.6167552738848,149.893366191926));
#159582=CARTESIAN_POINT('Ctrl Pts',(19.0278298377205,4.61918822443702,149.932292573303));
#159583=CARTESIAN_POINT('Ctrl Pts',(19.0278487031587,4.62019166902332,149.948347345408));
#159584=CARTESIAN_POINT('Ctrl Pts',(19.0276098584352,4.62130381811468,149.964461804004));
#159585=CARTESIAN_POINT('Ctrl Pts',(19.0271049749971,4.62252845771671,149.980623754727));
#159586=CARTESIAN_POINT('Ctrl Pts',(19.0258742772302,4.62551362441027,150.020019930486));
#159587=CARTESIAN_POINT('Ctrl Pts',(19.0230642858215,4.62916769373579,150.059701359999));
#159588=CARTESIAN_POINT('Ctrl Pts',(19.0186172197646,4.63343797107301,150.099587736542));
#159589=CARTESIAN_POINT('Ctrl Pts',(19.0143834314118,4.63750344935059,150.13756119461));
#159590=CARTESIAN_POINT('Ctrl Pts',(19.0086656935405,4.64212756637824,150.175720699002));
#159591=CARTESIAN_POINT('Ctrl Pts',(19.0013950309014,4.64725969649565,150.213953205714));
#159592=CARTESIAN_POINT('Ctrl Pts',(18.9993908405042,4.64867439092024,150.224492165726));
#159593=CARTESIAN_POINT('Ctrl Pts',(18.9972685407139,4.65012765023049,150.235036393758));
#159594=CARTESIAN_POINT('Ctrl Pts',(18.9950264368246,4.65161832543263,150.24558286292));
#159595=CARTESIAN_POINT('Ctrl Pts',(18.9937878121247,4.65244183193189,150.25140913942));
#159596=CARTESIAN_POINT('Ctrl Pts',(18.9925127279385,4.65327790659982,150.257235578971));
#159597=CARTESIAN_POINT('Ctrl Pts',(18.9912009357774,4.65412666248646,150.263061494053));
#159598=CARTESIAN_POINT('Ctrl Pts',(18.9827757632883,4.65957791837774,150.300479265654));
#159599=CARTESIAN_POINT('Ctrl Pts',(18.9728361281526,4.66555347237378,150.337879447222));
#159600=CARTESIAN_POINT('Ctrl Pts',(18.9613462365199,4.67206205203735,150.375156989378));
#159601=CARTESIAN_POINT('Ctrl Pts',(18.9497081013584,4.67865460593218,150.412915489456));
#159602=CARTESIAN_POINT('Ctrl Pts',(18.9364791401498,4.68579407471151,150.45054810867));
#159603=CARTESIAN_POINT('Ctrl Pts',(18.9216280703525,4.69347387927701,150.487894341172));
#159604=CARTESIAN_POINT('Ctrl Pts',(18.9167497883694,4.69599654281281,150.500161838102));
#159605=CARTESIAN_POINT('Ctrl Pts',(18.9116965481905,4.69857738253454,150.512398033371));
#159606=CARTESIAN_POINT('Ctrl Pts',(18.9064674538662,4.70121580877459,150.524596100463));
#159607=CARTESIAN_POINT('Ctrl Pts',(18.9046851887652,4.70211508018138,150.528753644376));
#159608=CARTESIAN_POINT('Ctrl Pts',(18.9028823913324,4.70302114824624,150.532906997649));
#159609=CARTESIAN_POINT('Ctrl Pts',(18.9010590312277,4.70393398011984,150.537055854138));
#159610=CARTESIAN_POINT('Ctrl Pts',(18.8844178728109,4.71226507159056,150.574920990003));
#159611=CARTESIAN_POINT('Ctrl Pts',(18.8660619770264,4.72116147974709,150.612414949923));
#159612=CARTESIAN_POINT('Ctrl Pts',(18.8459853786395,4.73062400119261,150.649374483313));
#159613=CARTESIAN_POINT('Ctrl Pts',(18.8440014796444,4.73155905435378,150.653026694695));
#159614=CARTESIAN_POINT('Ctrl Pts',(18.8420007978559,4.73249961695326,150.656673655371));
#159615=CARTESIAN_POINT('Ctrl Pts',(18.8399833403143,4.73344567777125,150.66031518714));
#159616=CARTESIAN_POINT('Ctrl Pts',(18.8276480154341,4.73923017003751,150.682580576375));
#159617=CARTESIAN_POINT('Ctrl Pts',(18.8146848936636,4.74522109248284,150.704644275892));
#159618=CARTESIAN_POINT('Ctrl Pts',(18.8010939409842,4.75141845499668,150.726467622821));
#159619=CARTESIAN_POINT('Ctrl Pts',(18.7942984646446,4.7545171362536,150.737379296286));
#159620=CARTESIAN_POINT('Ctrl Pts',(18.7873460194151,4.75766742751596,150.748230877052));
#159621=CARTESIAN_POINT('Ctrl Pts',(18.7802366479733,4.76086933028016,150.759017273877));
#159622=CARTESIAN_POINT('Ctrl Pts',(18.7766819622525,4.76247028166226,150.76441047229));
#159623=CARTESIAN_POINT('Ctrl Pts',(18.7730880441955,4.76408413592108,150.76978737374));
#159624=CARTESIAN_POINT('Ctrl Pts',(18.7694548974234,4.76571089325153,150.77514732952));
#159625=CARTESIAN_POINT('Ctrl Pts',(18.7676383240373,4.76652427191676,150.77782730741));
#159626=CARTESIAN_POINT('Ctrl Pts',(18.765811943414,4.76734087634984,150.780503048798));
#159627=CARTESIAN_POINT('Ctrl Pts',(18.7639757561209,4.7681607065754,150.783174471373));
#159628=CARTESIAN_POINT('Ctrl Pts',(18.7624282261282,4.76885165562388,150.785425933722));
#159629=CARTESIAN_POINT('Ctrl Pts',(18.7603436660376,4.76978089534062,150.78843756471));
#159630=CARTESIAN_POINT('Ctrl Pts',(18.7590620273306,4.77035184413092,150.790279324772));
#159631=CARTESIAN_POINT('Ctrl Pts',(18.7589283971141,4.77041137417634,150.79047135611));
#159632=CARTESIAN_POINT('Ctrl Pts',(18.7588035288813,4.77046699410134,150.79065069989));
#159633=CARTESIAN_POINT('Ctrl Pts',(18.7586889603557,4.77051801916076,150.790815185756));
#159634=CARTESIAN_POINT('Ctrl Pts',(18.758598568586,4.77055827668696,150.790944961089));
#159635=CARTESIAN_POINT('Ctrl Pts',(18.7585145882522,4.77059567396844,150.791065487676));
#159636=CARTESIAN_POINT('Ctrl Pts',(18.7584377747101,4.77062987465357,150.791175699747));
#159637=CARTESIAN_POINT('Ctrl Pts',(18.7427442375651,4.77761731083079,150.813692786982));
#159638=CARTESIAN_POINT('Ctrl Pts',(18.7254013610764,4.78529673082924,150.837260032547));
#159639=CARTESIAN_POINT('Ctrl Pts',(18.7061931998337,4.79370349912867,150.861643479064));
#159640=CARTESIAN_POINT('Ctrl Pts',(18.6872953200397,4.8019744676389,150.885633044512));
#159641=CARTESIAN_POINT('Ctrl Pts',(18.6665914498066,4.81095000020678,150.910413063444));
#159642=CARTESIAN_POINT('Ctrl Pts',(18.643873611093,4.82064367917762,150.935713037193));
#159643=CARTESIAN_POINT('Ctrl Pts',(18.622699857766,4.82967849846426,150.959293423077));
#159644=CARTESIAN_POINT('Ctrl Pts',(18.599776322654,4.83933724842325,150.983325470976));
#159645=CARTESIAN_POINT('Ctrl Pts',(18.5749379084155,4.8496093691693,151.007546322188));
#159646=CARTESIAN_POINT('Ctrl Pts',(18.5731265794623,4.85035845844448,151.009312615666));
#159647=CARTESIAN_POINT('Ctrl Pts',(18.5713050697243,4.8511107992961,151.01107989255));
#159648=CARTESIAN_POINT('Ctrl Pts',(18.5694733164477,4.85186638268389,151.01284804095));
#159649=CARTESIAN_POINT('Ctrl Pts',(18.5449558796609,4.86197962674588,151.036514146632));
#159650=CARTESIAN_POINT('Ctrl Pts',(18.5186020159773,4.87267515880367,151.060339859999));
#159651=CARTESIAN_POINT('Ctrl Pts',(18.4902680732814,4.88394610973416,151.084046519532));
#159652=CARTESIAN_POINT('Ctrl Pts',(18.4695156567062,4.89220120756575,151.101409809898));
#159653=CARTESIAN_POINT('Ctrl Pts',(18.4477012785905,4.90076466329986,151.118708449806));
#159654=CARTESIAN_POINT('Ctrl Pts',(18.4247751170454,4.9096275470227,151.135817514645));
#159655=CARTESIAN_POINT('Ctrl Pts',(18.3977740609141,4.92006571917003,151.15596754365));
#159656=CARTESIAN_POINT('Ctrl Pts',(18.3692092526384,4.93093761255334,151.175870517343));
#159657=CARTESIAN_POINT('Ctrl Pts',(18.3390315397969,4.9422482518405,151.195279017778));
#159658=CARTESIAN_POINT('Ctrl Pts',(18.3071202020531,4.95420865560889,151.215802482089));
#159659=CARTESIAN_POINT('Ctrl Pts',(18.2734038260656,4.9666600997838,151.235772955197));
#159660=CARTESIAN_POINT('Ctrl Pts',(18.2378719169443,4.97960093312966,151.254877447792));
#159661=CARTESIAN_POINT('Ctrl Pts',(18.2029890326836,4.99230538957466,151.273632978257));
#159662=CARTESIAN_POINT('Ctrl Pts',(18.1663563212283,5.00548163002252,151.291553943544));
#159663=CARTESIAN_POINT('Ctrl Pts',(18.1280017693888,5.01910706906789,151.308318507699));
#159664=CARTESIAN_POINT('Ctrl Pts',(18.1106764072625,5.02526189696367,151.315891328419));
#159665=CARTESIAN_POINT('Ctrl Pts',(18.0930002284209,5.03150808482261,151.323227830964));
#159666=CARTESIAN_POINT('Ctrl Pts',(18.0749783669678,5.03784204093478,151.330296483783));
#159667=CARTESIAN_POINT('Ctrl Pts',(18.0274749294532,5.05453757980443,151.348928593923));
#159668=CARTESIAN_POINT('Ctrl Pts',(17.9775661933698,5.07184209113894,151.365699921857));
#159669=CARTESIAN_POINT('Ctrl Pts',(17.9252952106596,5.0898080436658,151.380080876025));
#159670=CARTESIAN_POINT('Ctrl Pts',(17.8810599546647,5.10501205300352,151.392251016247));
#159671=CARTESIAN_POINT('Ctrl Pts',(17.8351346574171,5.12068951564457,151.40270901121));
#159672=CARTESIAN_POINT('Ctrl Pts',(17.7875678303251,5.13687695182573,151.411128767089));
#159673=CARTESIAN_POINT('Ctrl Pts',(17.7873134815034,5.13696350910884,151.411173789116));
#159674=CARTESIAN_POINT('Ctrl Pts',(17.787059085774,5.13705008099148,151.411218752855));
#159675=CARTESIAN_POINT('Ctrl Pts',(17.786804643145,5.13713666747989,151.411263658254));
#159676=CARTESIAN_POINT('Origin',(18.3860172570956,4.6108717272504,149.809053790145));
#159677=CARTESIAN_POINT('Origin',(17.5670013193858,-20.2701550170912,149.926880696201));
#159678=CARTESIAN_POINT('',(17.7869656855113,5.48598638025556,151.411234961359));
#159679=CARTESIAN_POINT('Ctrl Pts',(17.7868045798642,5.13713666751144,151.411263299869));
#159680=CARTESIAN_POINT('Ctrl Pts',(17.7866214367151,5.25353464188215,151.411295592951));
#159681=CARTESIAN_POINT('Ctrl Pts',(17.7871314417319,5.36958837810028,151.411205734173));
#159682=CARTESIAN_POINT('Ctrl Pts',(17.7869656855113,5.48598638025556,151.411234961359));
#159683=CARTESIAN_POINT('',(19.0080066341158,5.48838252639704,149.699374882563));
#159684=CARTESIAN_POINT('Origin',(17.5264760320735,5.48598635204796,149.934026397755));
#159685=CARTESIAN_POINT('',(19.0093911642939,4.61188418703121,149.69916599175));
#159686=CARTESIAN_POINT('Origin',(20.3497043807186,5.49056659368763,149.436215067118));
#159687=CARTESIAN_POINT('Origin',(20.3542501960586,5.49056659368762,149.461995667018));
#159688=CARTESIAN_POINT('Origin',(20.6101766471986,5.4905665936876,150.913426696618));
#159689=CARTESIAN_POINT('Origin',(18.5286714535786,5.49056659368762,139.108624134518));
#159690=CARTESIAN_POINT('',(15.7182861536206,5.48896890084689,128.928900209889));
#159691=CARTESIAN_POINT('Origin',(16.7030926497186,5.49056659368762,128.755252253918));
#159692=CARTESIAN_POINT('',(15.7182861536206,5.48896890084689,128.928900209889));
#159693=CARTESIAN_POINT('Origin',(15.7182861536206,5.48896890084689,128.928900209889));
#159694=CARTESIAN_POINT('',(15.7196652540208,4.61247156689892,128.928657037242));
#159695=CARTESIAN_POINT('',(19.0093911642939,4.61188418703121,149.69916599175));
#159696=CARTESIAN_POINT('',(15.7182861536206,5.48896890084689,128.928900209889));
#159697=CARTESIAN_POINT('Origin',(16.5604381014256,4.61087172725039,139.455679914345));
#159698=CARTESIAN_POINT('Origin',(14.9224228568571,4.6108991365907,130.067238728311));
#159699=CARTESIAN_POINT('Origin',(12.3566858837803,14.4973641791059,133.712013119689));
#159700=CARTESIAN_POINT('',(15.7196652540158,4.61247156689931,128.92865703727));
#159701=CARTESIAN_POINT('Origin',(1.84116836823847,-0.0335515531888081,
131.375810489939));
#159702=CARTESIAN_POINT('',(26.5526523577434,4.55654473273787,127.018509129283));
#159703=CARTESIAN_POINT('',(26.5669704824415,-4.54344365282274,127.015984457585));
#159704=CARTESIAN_POINT('',(26.5526523577434,4.55654473273787,127.018509129283));
#159705=CARTESIAN_POINT('',(17.5909132444034,4.54200572788895,128.598705529056));
#159706=CARTESIAN_POINT('',(17.5909132444034,4.54200572788895,128.598705529056));
#159707=CARTESIAN_POINT('',(17.5929586907863,3.24200738870957,128.598344861672));
#159708=CARTESIAN_POINT('',(17.5929586907863,3.24200738870957,128.598344861672));
#159709=CARTESIAN_POINT('',(17.1005554416673,3.24120854228747,128.685168839857));
#159710=CARTESIAN_POINT('',(17.1005554416673,3.24120854228747,128.685168839857));
#159711=CARTESIAN_POINT('',(17.1107826735945,-3.2587831616844,128.68336550293));
#159712=CARTESIAN_POINT('',(17.1107826735945,-3.2587831616844,128.68336550293));
#159713=CARTESIAN_POINT('',(17.6031859216335,-3.25798431526405,128.596541524945));
#159714=CARTESIAN_POINT('',(17.6031859216335,-3.25798431526405,128.596541524945));
#159715=CARTESIAN_POINT('',(17.6052313680214,-4.55798265767342,128.596180857559));
#159716=CARTESIAN_POINT('',(17.6052313680214,-4.55798265767342,128.596180857559));
#159717=CARTESIAN_POINT('',(26.5669704824415,-4.54344365282274,127.015984457585));
#159718=CARTESIAN_POINT('Origin',(26.5669704824415,-4.54344365282274,127.015984457585));
#159719=CARTESIAN_POINT('',(30.4597363552535,4.55654473273787,149.176683572083));
#159720=CARTESIAN_POINT('',(26.5526523577434,4.55654473273787,127.018509129283));
#159721=CARTESIAN_POINT('',(30.4740544799515,-4.54344365282274,149.174158900385));
#159722=CARTESIAN_POINT('',(26.5669704824415,-4.54344365282274,127.015984457585));
#159723=CARTESIAN_POINT('',(30.4740544799515,-4.54344365282274,149.174158900385));
#159724=CARTESIAN_POINT('Origin',(26.5526523577434,4.55654473273787,127.018509129283));
#159725=CARTESIAN_POINT('',(21.4979972419134,4.54200572788897,150.756879971756));
#159726=CARTESIAN_POINT('',(17.5909132444034,4.54200572788895,128.598705529056));
#159727=CARTESIAN_POINT('',(30.4597363552535,4.55654473273787,149.176683572083));
#159728=CARTESIAN_POINT('Origin',(17.5909132444034,4.54200572788895,128.598705529056));
#159729=CARTESIAN_POINT('',(21.5000426882963,3.2420073887096,150.756519304372));
#159730=CARTESIAN_POINT('',(17.5929586907863,3.24200738870957,128.598344861672));
#159731=CARTESIAN_POINT('',(21.4979972419134,4.54200572788897,150.756879971756));
#159732=CARTESIAN_POINT('Origin',(17.5929586907863,3.24200738870957,128.598344861672));
#159733=CARTESIAN_POINT('',(21.0076394391673,3.24120854228745,150.843343282657));
#159734=CARTESIAN_POINT('',(17.1005554416673,3.24120854228747,128.685168839857));
#159735=CARTESIAN_POINT('',(21.5000426882963,3.2420073887096,150.756519304372));
#159736=CARTESIAN_POINT('Origin',(17.1005554416673,3.24120854228747,128.685168839857));
#159737=CARTESIAN_POINT('',(21.0178666710944,-3.25878316168441,150.84153994573));
#159738=CARTESIAN_POINT('',(17.1107826735945,-3.2587831616844,128.68336550293));
#159739=CARTESIAN_POINT('',(21.0076394391673,3.24120854228745,150.843343282657));
#159740=CARTESIAN_POINT('Origin',(17.1107826735945,-3.2587831616844,128.68336550293));
#159741=CARTESIAN_POINT('',(21.5102699191435,-3.25798431526402,150.754715967645));
#159742=CARTESIAN_POINT('',(17.6031859216335,-3.25798431526405,128.596541524945));
#159743=CARTESIAN_POINT('',(21.0178666710944,-3.25878316168441,150.84153994573));
#159744=CARTESIAN_POINT('Origin',(17.6031859216335,-3.25798431526405,128.596541524945));
#159745=CARTESIAN_POINT('',(21.5123153655314,-4.55798265767339,150.754355300259));
#159746=CARTESIAN_POINT('',(17.6052313680214,-4.55798265767342,128.596180857559));
#159747=CARTESIAN_POINT('',(21.5102699191435,-3.25798431526402,150.754715967645));
#159748=CARTESIAN_POINT('Origin',(17.6052313680214,-4.55798265767342,128.596180857559));
#159749=CARTESIAN_POINT('',(21.5123153655314,-4.55798265767339,150.754355300259));
#159750=CARTESIAN_POINT('Origin',(26.4291887836315,-2.1219048984176E-14,
149.887377855954));
#159751=CARTESIAN_POINT('Origin',(26.4291887836315,-2.1219048984176E-14,
149.887377855954));
#159752=CARTESIAN_POINT('Origin',(-6.15924143489591,24.952514954652,136.340491736592));
#159753=CARTESIAN_POINT('',(21.0787428031861,-20.7493757828675,119.352580872645));
#159754=CARTESIAN_POINT('',(21.012266743147,21.4999725592939,119.364302395635));
#159755=CARTESIAN_POINT('Origin',(21.0460952759615,-9.02974887056722E-15,
119.358337512554));
#159756=CARTESIAN_POINT('Ctrl Pts',(94.4677262089947,4.26458625199329,142.134302812303));
#159757=CARTESIAN_POINT('Ctrl Pts',(94.325324460867,3.88264561414907,142.026683431587));
#159758=CARTESIAN_POINT('Ctrl Pts',(94.0716376882548,3.10957209929612,141.841360490054));
#159759=CARTESIAN_POINT('Ctrl Pts',(93.810153878733,1.9414001629906,141.658481685112));
#159760=CARTESIAN_POINT('Ctrl Pts',(93.6806979553918,0.830568367124271,
141.569555741515));
#159761=CARTESIAN_POINT('Ctrl Pts',(93.6640015230007,-0.217429764701261,
141.556979537194));
#159762=CARTESIAN_POINT('Ctrl Pts',(93.7471059523909,-1.24660990130415,
141.611474474069));
#159763=CARTESIAN_POINT('Ctrl Pts',(93.9298885891748,-2.27247910489614,
141.735159766024));
#159764=CARTESIAN_POINT('Ctrl Pts',(94.1843275940772,-3.21196450833431,
141.913619082162));
#159765=CARTESIAN_POINT('Ctrl Pts',(94.384865518228,-3.79126873095784,142.060241775828));
#159766=CARTESIAN_POINT('Ctrl Pts',(94.4808018463151,-4.04615891951393,
142.131996757721));
#159767=CARTESIAN_POINT('Ctrl Pts',(94.8031311051781,4.17070113450257,142.052929078712));
#159768=CARTESIAN_POINT('Ctrl Pts',(94.6623836287724,3.79574718487004,141.944065691349));
#159769=CARTESIAN_POINT('Ctrl Pts',(94.4120362510534,3.03789023725012,141.756839725743));
#159770=CARTESIAN_POINT('Ctrl Pts',(94.1547643263253,1.89611374480954,141.572553509887));
#159771=CARTESIAN_POINT('Ctrl Pts',(94.0276583019129,0.812719749478585,
141.483112913603));
#159772=CARTESIAN_POINT('Ctrl Pts',(94.0112683209779,-0.208537697884529,
141.470480186353));
#159773=CARTESIAN_POINT('Ctrl Pts',(94.0928124726429,-1.21183598557444,
141.525284855749));
#159774=CARTESIAN_POINT('Ctrl Pts',(94.2724474101964,-2.2134236624816,141.649827072304));
#159775=CARTESIAN_POINT('Ctrl Pts',(94.5230912346179,-3.13277799467634,
141.829876753025));
#159776=CARTESIAN_POINT('Ctrl Pts',(94.7210926373913,-3.70094603761282,
141.978086379388));
#159777=CARTESIAN_POINT('Ctrl Pts',(94.815909527443,-3.95117347469028,142.050675379175));
#159778=CARTESIAN_POINT('Ctrl Pts',(95.1198224210223,4.03339275365646,142.146660496547));
#159779=CARTESIAN_POINT('Ctrl Pts',(94.9835402883144,3.66863510173414,142.037649619029));
#159780=CARTESIAN_POINT('Ctrl Pts',(94.7416652223918,2.93298390507885,141.850476134561));
#159781=CARTESIAN_POINT('Ctrl Pts',(94.4941624531867,1.82972313738508,141.666861333164));
#159782=CARTESIAN_POINT('Ctrl Pts',(94.3722609744833,0.786363145160593,
141.577972687657));
#159783=CARTESIAN_POINT('Ctrl Pts',(94.3565650060748,-0.195879481250129,
141.565437151993));
#159784=CARTESIAN_POINT('Ctrl Pts',(94.4347331412821,-1.16141782934051,
141.619890673295));
#159785=CARTESIAN_POINT('Ctrl Pts',(94.6073024106271,-2.12758230072278,
141.743846418259));
#159786=CARTESIAN_POINT('Ctrl Pts',(94.8488894983716,-3.01757032297491,
141.923521976027));
#159787=CARTESIAN_POINT('Ctrl Pts',(95.0403543380529,-3.56949458930854,
142.071791382735));
#159788=CARTESIAN_POINT('Ctrl Pts',(95.1321672209127,-3.81292095042804,
142.144483189647));
#159789=CARTESIAN_POINT('Ctrl Pts',(95.3363636309633,3.88796967926968,142.391394222942));
#159790=CARTESIAN_POINT('Ctrl Pts',(95.2062096599398,3.53399597741717,142.283370298785));
#159791=CARTESIAN_POINT('Ctrl Pts',(94.9757611852104,2.82182955193183,142.098191305131));
#159792=CARTESIAN_POINT('Ctrl Pts',(94.7410727240179,1.75930054987824,141.917154090713));
#159793=CARTESIAN_POINT('Ctrl Pts',(94.6258920995078,0.758276101163494,
141.829742066319));
#159794=CARTESIAN_POINT('Ctrl Pts',(94.6110992405489,-0.182710149363758,
141.817432444289));
#159795=CARTESIAN_POINT('Ctrl Pts',(94.6849437563614,-1.1083203585478,141.87096423382));
#159796=CARTESIAN_POINT('Ctrl Pts',(94.848346310829,-2.03702895054977,141.993040920939));
#159797=CARTESIAN_POINT('Ctrl Pts',(95.077944026924,-2.89596691080905,142.170474073356));
#159798=CARTESIAN_POINT('Ctrl Pts',(95.2605531255443,-3.43071685761424,
142.317260735522));
#159799=CARTESIAN_POINT('Ctrl Pts',(95.3482499064457,-3.66695270109413,
142.389297701919));
#159800=CARTESIAN_POINT('',(95.2116320414304,3.87890261200112,142.275538234229));
#159801=CARTESIAN_POINT('Origin',(94.5824319951644,3.87766013850041,143.052704236177));
#159802=CARTESIAN_POINT('',(95.223491004657,-3.65821211009624,142.273447286233));
#159803=CARTESIAN_POINT('Ctrl Pts',(95.2116318269622,3.87890261158699,142.275538499172));
#159804=CARTESIAN_POINT('Ctrl Pts',(95.0892916816967,3.54282600750017,142.175974488895));
#159805=CARTESIAN_POINT('Ctrl Pts',(94.8641911706135,2.84386470343991,141.998174645644));
#159806=CARTESIAN_POINT('Ctrl Pts',(94.629784427461,1.78908951785421,141.820372677863));
#159807=CARTESIAN_POINT('Ctrl Pts',(94.5118334959788,0.770149152459641,
141.732389968258));
#159808=CARTESIAN_POINT('Ctrl Pts',(94.496668722276,-0.188296407942078,
141.719992216783));
#159809=CARTESIAN_POINT('Ctrl Pts',(94.5722972036391,-1.1308039059681,141.773880662021));
#159810=CARTESIAN_POINT('Ctrl Pts',(94.7394761249336,-2.07536362700424,
141.896676127896));
#159811=CARTESIAN_POINT('Ctrl Pts',(94.9673857696971,-2.92284253173479,
142.069917541593));
#159812=CARTESIAN_POINT('Ctrl Pts',(95.14392684748,-3.4417481453771,142.20937126949));
#159813=CARTESIAN_POINT('Ctrl Pts',(95.2234908094786,-3.65821211046655,
142.27344752735));
#159814=CARTESIAN_POINT('Origin',(94.5942416492558,-3.65942148632551,143.05082648727));
#159815=CARTESIAN_POINT('Ctrl Pts',(100.709300696936,5.04237442459277,150.282068014958));
#159816=CARTESIAN_POINT('Ctrl Pts',(100.727900795881,-6.7790538657833,150.27878831567));
#159817=CARTESIAN_POINT('Ctrl Pts',(99.5012583427497,5.04146860010937,146.69589528654));
#159818=CARTESIAN_POINT('Ctrl Pts',(99.5198584416948,-6.7799596902667,146.692615587252));
#159819=CARTESIAN_POINT('Ctrl Pts',(97.4016151358028,5.03896189264658,143.82346459845));
#159820=CARTESIAN_POINT('Ctrl Pts',(97.4202152347478,-6.78246639772949,
143.820184899162));
#159821=CARTESIAN_POINT('Ctrl Pts',(94.4103710760951,5.03485430220433,141.664775950885));
#159822=CARTESIAN_POINT('Ctrl Pts',(94.4289711750401,-6.78657398817173,
141.661496251597));
#159823=CARTESIAN_POINT('',(97.16866993185,-4.72410467554793,144.11266556739));
#159824=CARTESIAN_POINT('Ctrl Pts',(95.2234913950221,-3.65821210935081,
142.273446804006));
#159825=CARTESIAN_POINT('Ctrl Pts',(95.2467072678134,-3.72130470321278,
142.292142621898));
#159826=CARTESIAN_POINT('Ctrl Pts',(95.2748644610139,-3.78234564067068,
142.314939154039));
#159827=CARTESIAN_POINT('Ctrl Pts',(95.3069266235745,-3.84060070705387,
142.341129033054));
#159828=CARTESIAN_POINT('Ctrl Pts',(95.3630114364024,-3.94250351813844,
142.386941740159));
#159829=CARTESIAN_POINT('Ctrl Pts',(95.4310450012107,-4.03588190091921,
142.443137694358));
#159830=CARTESIAN_POINT('Ctrl Pts',(95.5063030800419,-4.12035383948242,
142.506553038376));
#159831=CARTESIAN_POINT('Ctrl Pts',(95.5905482312874,-4.21491313930498,
142.577541234342));
#159832=CARTESIAN_POINT('Ctrl Pts',(95.6838463850794,-4.29831182574749,
142.657576009313));
#159833=CARTESIAN_POINT('Ctrl Pts',(95.7819301502628,-4.37102508631497,
142.743838974376));
#159834=CARTESIAN_POINT('Ctrl Pts',(95.8913775114615,-4.45216261685718,
142.840096024437));
#159835=CARTESIAN_POINT('Ctrl Pts',(96.0067836061993,-4.51999534577716,
142.944108012202));
#159836=CARTESIAN_POINT('Ctrl Pts',(96.1245864449981,-4.57509531248624,
143.053498457647));
#159837=CARTESIAN_POINT('Ctrl Pts',(96.252371147288,-4.634864100012,143.172157953862));
#159838=CARTESIAN_POINT('Ctrl Pts',(96.3829759713566,-4.67965091346211,
143.2971459968));
#159839=CARTESIAN_POINT('Ctrl Pts',(96.513330033225,-4.70934161504182,143.42615701659));
#159840=CARTESIAN_POINT('Ctrl Pts',(96.6470643254029,-4.73980223056167,
143.558513440069));
#159841=CARTESIAN_POINT('Ctrl Pts',(96.7805346806551,-4.75437365891532,
143.695104185896));
#159842=CARTESIAN_POINT('Ctrl Pts',(96.9110983918428,-4.75202486117502,
143.833436285795));
#159843=CARTESIAN_POINT('Ctrl Pts',(96.9985940960846,-4.75045084255575,
143.926137882508));
#159844=CARTESIAN_POINT('Ctrl Pts',(97.0847844692051,-4.74127820475585,
144.019621493763));
#159845=CARTESIAN_POINT('Ctrl Pts',(97.168671748338,-4.72410467227896,144.112663929037));
#159846=CARTESIAN_POINT('',(97.153448356702,4.94989036380522,144.115349759976));
#159847=CARTESIAN_POINT('Ctrl Pts',(97.1534510310516,4.94989036871313,144.115347348054));
#159848=CARTESIAN_POINT('Ctrl Pts',(97.0659102985489,4.96757874934412,144.018325642839));
#159849=CARTESIAN_POINT('Ctrl Pts',(96.9758866343682,4.97655737323447,143.920815999854));
#159850=CARTESIAN_POINT('Ctrl Pts',(96.8845082164897,4.9772843793877,143.824195088114));
#159851=CARTESIAN_POINT('Ctrl Pts',(96.753482688462,4.97832681771523,143.685652462043));
#159852=CARTESIAN_POINT('Ctrl Pts',(96.6196717801744,4.96240387464917,143.548937076949));
#159853=CARTESIAN_POINT('Ctrl Pts',(96.4857353063917,4.93053759771028,143.416539758115));
#159854=CARTESIAN_POINT('Ctrl Pts',(96.3555356989818,4.89956039911845,143.287836362785));
#159855=CARTESIAN_POINT('Ctrl Pts',(96.2252174360236,4.85351710908179,143.163213444886));
#159856=CARTESIAN_POINT('Ctrl Pts',(96.09787659053,4.79250224244665,143.044982433951));
#159857=CARTESIAN_POINT('Ctrl Pts',(95.9807258681,4.73636993330757,142.936212555041));
#159858=CARTESIAN_POINT('Ctrl Pts',(95.8660951089851,4.66756630602553,142.83285252219));
#159859=CARTESIAN_POINT('Ctrl Pts',(95.7575771952769,4.58551682113803,142.737294315022));
#159860=CARTESIAN_POINT('Ctrl Pts',(95.6604238270679,4.51205997383748,142.65174344725));
#159861=CARTESIAN_POINT('Ctrl Pts',(95.5681700069202,4.42798635034682,142.572445874935));
#159862=CARTESIAN_POINT('Ctrl Pts',(95.4851091592593,4.33284712380514,142.502236728833));
#159863=CARTESIAN_POINT('Ctrl Pts',(95.4108924557532,4.24783812176753,142.439503304766));
#159864=CARTESIAN_POINT('Ctrl Pts',(95.3440152452747,4.15399454704945,142.384025908196));
#159865=CARTESIAN_POINT('Ctrl Pts',(95.289209369605,4.0517725391194,142.338977034317));
#159866=CARTESIAN_POINT('Ctrl Pts',(95.259519461425,3.99639595782553,142.314572772681));
#159867=CARTESIAN_POINT('Ctrl Pts',(95.2333721263064,3.9385605546291,142.293228968045));
#159868=CARTESIAN_POINT('Ctrl Pts',(95.2116324703669,3.87890261282936,142.275537704344));
#159869=CARTESIAN_POINT('',(100.3971489688,2.11466427441707,149.409381531096));
#159870=CARTESIAN_POINT('Ctrl Pts',(100.397149868591,2.11466427596188,149.409381179598));
#159871=CARTESIAN_POINT('Ctrl Pts',(100.264072070223,2.4743631149336,149.070307282051));
#159872=CARTESIAN_POINT('Ctrl Pts',(99.9316309122332,3.18218183511712,148.28374709774));
#159873=CARTESIAN_POINT('Ctrl Pts',(99.2367363880305,4.03704249542641,146.932753463133));
#159874=CARTESIAN_POINT('Ctrl Pts',(98.3041095906132,4.63847370651756,145.487158534252));
#159875=CARTESIAN_POINT('Ctrl Pts',(97.5462262568398,4.87042480372463,144.550915761011));
#159876=CARTESIAN_POINT('Ctrl Pts',(97.1534470196683,4.94989036130278,144.115350966093));
#159877=CARTESIAN_POINT('',(100.403437304611,-1.88162507939484,149.408270627991));
#159878=CARTESIAN_POINT('Ctrl Pts',(100.403437652402,-1.88162317480153,
149.408272487378));
#159879=CARTESIAN_POINT('Ctrl Pts',(100.451208759698,-1.75118679936034,
149.531126155632));
#159880=CARTESIAN_POINT('Ctrl Pts',(100.545485504079,-1.43297394048954,
149.782281369385));
#159881=CARTESIAN_POINT('Ctrl Pts',(100.644986088431,-0.868477907273701,
150.064530940924));
#159882=CARTESIAN_POINT('Ctrl Pts',(100.69686050395,-0.212788963995321,
150.219404994051));
#159883=CARTESIAN_POINT('Ctrl Pts',(100.695307264391,0.458828142569949,
150.218119833334));
#159884=CARTESIAN_POINT('Ctrl Pts',(100.640359242456,1.11382689997406,150.060732638077));
#159885=CARTESIAN_POINT('Ctrl Pts',(100.538802206203,1.67318407177052,149.778262943369));
#159886=CARTESIAN_POINT('Ctrl Pts',(100.444203553735,1.98735761693585,149.529289759105));
#159887=CARTESIAN_POINT('Ctrl Pts',(100.397149868591,2.11466427596188,149.409381179598));
#159888=CARTESIAN_POINT('Ctrl Pts',(97.168669023838,-4.72410467713493,144.112666386824));
#159889=CARTESIAN_POINT('Ctrl Pts',(97.5655380434849,-4.64275293009404,
144.553083450934));
#159890=CARTESIAN_POINT('Ctrl Pts',(98.3258634243098,-4.40699925250942,
145.494588767759));
#159891=CARTESIAN_POINT('Ctrl Pts',(99.2574692905987,-3.79861237595365,
146.945295844755));
#159892=CARTESIAN_POINT('Ctrl Pts',(99.9451052029796,-2.94278987349825,
148.290837223702));
#159893=CARTESIAN_POINT('Ctrl Pts',(100.272985516958,-2.23746403900694,
149.072839132248));
#159894=CARTESIAN_POINT('Ctrl Pts',(100.403436966518,-1.8816250457219,149.408270723756));
#159895=CARTESIAN_POINT('Ctrl Pts',(93.6948982478023,-3.9130261905305,142.678416629155));
#159896=CARTESIAN_POINT('Ctrl Pts',(93.743554307992,-4.08317118406646,142.715180369127));
#159897=CARTESIAN_POINT('Ctrl Pts',(93.890833594482,-4.43602161921736,142.827213486021));
#159898=CARTESIAN_POINT('Ctrl Pts',(94.197684598825,-4.87048287682669,143.067043278988));
#159899=CARTESIAN_POINT('Ctrl Pts',(94.5858697526221,-5.23220927751511,
143.384411304587));
#159900=CARTESIAN_POINT('Ctrl Pts',(95.0284082738768,-5.50573316404525,
143.76865508919));
#159901=CARTESIAN_POINT('Ctrl Pts',(95.5061222115966,-5.6797337413587,144.215123578903));
#159902=CARTESIAN_POINT('Ctrl Pts',(95.9650706075177,-5.73397405955418,
144.681053992722));
#159903=CARTESIAN_POINT('Ctrl Pts',(96.2562974300626,-5.69489479826764,
145.001037870784));
#159904=CARTESIAN_POINT('Ctrl Pts',(96.3841297881998,-5.66022393088418,
145.146508645044));
#159905=CARTESIAN_POINT('Ctrl Pts',(94.0201637971862,-3.98769337013459,
141.94166108681));
#159906=CARTESIAN_POINT('Ctrl Pts',(94.0755116171319,-4.17658156420627,
141.983279312062));
#159907=CARTESIAN_POINT('Ctrl Pts',(94.2425795356422,-4.56610838669949,
142.109730188625));
#159908=CARTESIAN_POINT('Ctrl Pts',(94.5866480995851,-5.03825401711204,
142.377170408612));
#159909=CARTESIAN_POINT('Ctrl Pts',(95.0169249190105,-5.42560988395097,
142.727049095028));
#159910=CARTESIAN_POINT('Ctrl Pts',(95.5036527056414,-5.71562220389437,
143.147755229396));
#159911=CARTESIAN_POINT('Ctrl Pts',(96.0270857752493,-5.89931148731261,
143.635508492719));
#159912=CARTESIAN_POINT('Ctrl Pts',(96.5298127726263,-5.9566654395584,144.145373780338));
#159913=CARTESIAN_POINT('Ctrl Pts',(96.8495393014006,-5.91530475223614,
144.497000776349));
#159914=CARTESIAN_POINT('Ctrl Pts',(96.990121998386,-5.87841909048293,144.65727863506));
#159915=CARTESIAN_POINT('Ctrl Pts',(94.792363611226,-3.80564312789954,141.784343691287));
#159916=CARTESIAN_POINT('Ctrl Pts',(94.8353416091631,-3.94957461808571,
141.817287026332));
#159917=CARTESIAN_POINT('Ctrl Pts',(94.9665075650647,-4.25112502864957,
141.918519941624));
#159918=CARTESIAN_POINT('Ctrl Pts',(95.2489514150549,-4.6328552561169,142.142626516623));
#159919=CARTESIAN_POINT('Ctrl Pts',(95.6179342728045,-4.9586911421452,142.448605660312));
#159920=CARTESIAN_POINT('Ctrl Pts',(96.0479270829259,-5.20909416509736,
142.826287646371));
#159921=CARTESIAN_POINT('Ctrl Pts',(96.5175822681404,-5.36947399865914,
143.26851859957));
#159922=CARTESIAN_POINT('Ctrl Pts',(96.9700113870813,-5.41929000533494,
143.728991628168));
#159923=CARTESIAN_POINT('Ctrl Pts',(97.2558433417816,-5.38335705658195,
144.042280799348));
#159924=CARTESIAN_POINT('Ctrl Pts',(97.3808064392917,-5.35176423600097,
144.18379587502));
#159925=CARTESIAN_POINT('Ctrl Pts',(95.3016037801828,-3.53423675537427,
142.351088487871));
#159926=CARTESIAN_POINT('Ctrl Pts',(95.3245221219672,-3.61084095345401,
142.369802503292));
#159927=CARTESIAN_POINT('Ctrl Pts',(95.3971006883962,-3.78064007830534,
142.429364954977));
#159928=CARTESIAN_POINT('Ctrl Pts',(95.5757299983015,-4.0269752505514,142.579031028893));
#159929=CARTESIAN_POINT('Ctrl Pts',(95.8363816489282,-4.26069787329206,
142.805057879427));
#159930=CARTESIAN_POINT('Ctrl Pts',(96.1608724850215,-4.45180724034671,
143.099781910541));
#159931=CARTESIAN_POINT('Ctrl Pts',(96.5266915181716,-4.57730816593525,
143.451532755502));
#159932=CARTESIAN_POINT('Ctrl Pts',(96.8809858101989,-4.61586438445729,
143.814693375449));
#159933=CARTESIAN_POINT('Ctrl Pts',(97.1016886587558,-4.58807854415974,
144.054908268628));
#159934=CARTESIAN_POINT('Ctrl Pts',(97.1970215311566,-4.56442041860899,
144.161339578343));
#159935=CARTESIAN_POINT('',(96.4276511501619,-5.70697315835852,144.973748692482));
#159936=CARTESIAN_POINT('Origin',(96.4260783789126,-4.72539616721717,144.782471517403));
#159937=CARTESIAN_POINT('Ctrl Pts',(94.5946916752436,-3.92833378532365,
142.087508698775));
#159938=CARTESIAN_POINT('Ctrl Pts',(94.6072841821975,-3.98846146113012,
142.104301905679));
#159939=CARTESIAN_POINT('Ctrl Pts',(94.6220231953396,-4.04932725666999,
142.123731558378));
#159940=CARTESIAN_POINT('Ctrl Pts',(94.6389082768763,-4.11065296415126,
142.146050941591));
#159941=CARTESIAN_POINT('Ctrl Pts',(94.6555164167165,-4.17097283429421,
142.168004252077));
#159942=CARTESIAN_POINT('Ctrl Pts',(94.674200804506,-4.2317376421803,142.192753727171));
#159943=CARTESIAN_POINT('Ctrl Pts',(94.6949609514218,-4.29263674381567,
142.220522459942));
#159944=CARTESIAN_POINT('Ctrl Pts',(94.715381301438,-4.35253906416544,142.247836681031));
#159945=CARTESIAN_POINT('Ctrl Pts',(94.7378100155495,-4.41257124202651,
142.278072578247));
#159946=CARTESIAN_POINT('Ctrl Pts',(94.7622465591094,-4.47239350470747,
142.311418386374));
#159947=CARTESIAN_POINT('Ctrl Pts',(94.7866831026693,-4.53221576738843,
142.3447641945));
#159948=CARTESIAN_POINT('Ctrl Pts',(94.8131274756349,-4.59182808787051,
142.381220462011));
#159949=CARTESIAN_POINT('Ctrl Pts',(94.8415790742591,-4.65084677191736,
142.420943627582));
#159950=CARTESIAN_POINT('Ctrl Pts',(94.8687546763644,-4.7072185876321,142.458885289707));
#159951=CARTESIAN_POINT('Ctrl Pts',(94.8977615006632,-4.76304838976179,
142.499807595353));
#159952=CARTESIAN_POINT('Ctrl Pts',(94.928598963509,-4.81796525172841,142.54381256834));
#159953=CARTESIAN_POINT('Ctrl Pts',(94.9589917576618,-4.87209022593974,
142.587183000349));
#159954=CARTESIAN_POINT('Ctrl Pts',(94.9911627759117,-4.92532816324288,
142.63354821058));
#159955=CARTESIAN_POINT('Ctrl Pts',(95.0251114089696,-4.97729183372492,
142.68296713936));
#159956=CARTESIAN_POINT('Ctrl Pts',(95.058395671812,-5.02823858211499,142.731418946304));
#159957=CARTESIAN_POINT('Ctrl Pts',(95.0933886544008,-5.07796014305279,
142.78280641666));
#159958=CARTESIAN_POINT('Ctrl Pts',(95.1300897399471,-5.12606451376125,
142.837142732317));
#159959=CARTESIAN_POINT('Ctrl Pts',(95.1387658922046,-5.13743640748879,
142.849987860485));
#159960=CARTESIAN_POINT('Ctrl Pts',(95.1475375018997,-5.14871781501934,
142.862997584704));
#159961=CARTESIAN_POINT('Ctrl Pts',(95.156404560575,-5.15990336111806,142.876171695935));
#159962=CARTESIAN_POINT('Ctrl Pts',(95.1769795765034,-5.18585816728068,
142.906740744631));
#159963=CARTESIAN_POINT('Ctrl Pts',(95.1980685090438,-5.21129696288514,
142.938195204438));
#159964=CARTESIAN_POINT('Ctrl Pts',(95.2196712502921,-5.23615116776965,
142.970529156747));
#159965=CARTESIAN_POINT('Ctrl Pts',(95.2304726209163,-5.24857827021191,
142.986696132901));
#159966=CARTESIAN_POINT('Ctrl Pts',(95.2414024437426,-5.26085924098744,
143.003082970078));
#159967=CARTESIAN_POINT('Ctrl Pts',(95.2524607049315,-5.27298528412071,
143.019688407892));
#159968=CARTESIAN_POINT('Ctrl Pts',(95.257989835526,-5.27904830568736,143.027991126799));
#159969=CARTESIAN_POINT('Ctrl Pts',(95.2635510757132,-5.28507259667165,
143.036348494827));
#159970=CARTESIAN_POINT('Ctrl Pts',(95.2691444237609,-5.29105705605127,
143.044760335691));
#159971=CARTESIAN_POINT('Ctrl Pts',(95.2719410977847,-5.29404928574108,
143.048966256123));
#159972=CARTESIAN_POINT('Ctrl Pts',(95.2747457987738,-5.29703155760949,
143.053185794708));
#159973=CARTESIAN_POINT('Ctrl Pts',(95.2775585265105,-5.30000373341748,
143.057418927516));
#159974=CARTESIAN_POINT('Ctrl Pts',(95.2789648903789,-5.30148982132147,
143.05953549392));
#159975=CARTESIAN_POINT('Ctrl Pts',(95.2803732609343,-5.30297338521556,
143.061655458876));
#159976=CARTESIAN_POINT('Ctrl Pts',(95.2817836381493,-5.30445440777924,
143.063778819269));
#159977=CARTESIAN_POINT('Ctrl Pts',(95.2831940153643,-5.30593543034291,
143.065902179662));
#159978=CARTESIAN_POINT('Ctrl Pts',(95.2852296355216,-5.30806426132359,
143.068967562828));
#159979=CARTESIAN_POINT('Ctrl Pts',(95.2860207897461,-5.30888983415799,
143.070159083596));
#159980=CARTESIAN_POINT('Ctrl Pts',(95.29977098247,-5.32323821937621,143.090867612585));
#159981=CARTESIAN_POINT('Ctrl Pts',(95.3151341469759,-5.33876599641073,
143.113940975202));
#159982=CARTESIAN_POINT('Ctrl Pts',(95.3321099272088,-5.35524689040698,
143.139511997507));
#159983=CARTESIAN_POINT('Ctrl Pts',(95.3489094742827,-5.37155668887929,
143.164817555605));
#159984=CARTESIAN_POINT('Ctrl Pts',(95.3672883285572,-5.38880007239327,
143.192569727119));
#159985=CARTESIAN_POINT('Ctrl Pts',(95.3872460659309,-5.40670751916013,
143.222905563591));
#159986=CARTESIAN_POINT('Ctrl Pts',(95.4067573385441,-5.42421436721271,
143.252562771935));
#159987=CARTESIAN_POINT('Ctrl Pts',(95.4277776435826,-5.44235591927885,
143.284689928006));
#159988=CARTESIAN_POINT('Ctrl Pts',(95.4503065070759,-5.46083095757515,
143.319414767716));
#159989=CARTESIAN_POINT('Ctrl Pts',(95.4724724642041,-5.47900839057976,
143.353580242087));
#159990=CARTESIAN_POINT('Ctrl Pts',(95.4960987700176,-5.49750867406295,
143.390260996447));
#159991=CARTESIAN_POINT('Ctrl Pts',(95.5211848963973,-5.51599617363321,
143.429569587366));
#159992=CARTESIAN_POINT('Ctrl Pts',(95.5455569630813,-5.53395743897682,
143.467759285713));
#159993=CARTESIAN_POINT('Ctrl Pts',(95.5713069272671,-5.55190649923997,
143.508429917924));
#159994=CARTESIAN_POINT('Ctrl Pts',(95.5984342332853,-5.56949020663385,
143.551667475252));
#159995=CARTESIAN_POINT('Ctrl Pts',(95.6186688954836,-5.58260615626295,
143.583919014208));
#159996=CARTESIAN_POINT('Ctrl Pts',(95.6396698941508,-5.59551789842759,
143.617598482181));
#159997=CARTESIAN_POINT('Ctrl Pts',(95.661436972806,-5.60806242852013,143.652732066203));
#159998=CARTESIAN_POINT('Ctrl Pts',(95.6904862361588,-5.62480373607302,
143.699619604533));
#159999=CARTESIAN_POINT('Ctrl Pts',(95.7208999093872,-5.64089259177349,
143.749098762162));
#160000=CARTESIAN_POINT('Ctrl Pts',(95.7526773221263,-5.65590294464707,
143.801200738942));
#160001=CARTESIAN_POINT('Ctrl Pts',(95.7685660284959,-5.66340812108386,
143.827251727332));
#160002=CARTESIAN_POINT('Ctrl Pts',(95.7847956686639,-5.67064298583235,
143.853957809213));
#160003=CARTESIAN_POINT('Ctrl Pts',(95.8013661525195,-5.67755026824592,
143.881318681812));
#160004=CARTESIAN_POINT('Ctrl Pts',(95.8096513944473,-5.6810039094527,143.894999118111));
#160005=CARTESIAN_POINT('Ctrl Pts',(95.8180218472537,-5.68437562754898,
143.908843258848));
#160006=CARTESIAN_POINT('Ctrl Pts',(95.8264774992646,-5.68765800287411,
143.922850681624));
#160007=CARTESIAN_POINT('Ctrl Pts',(95.8320690644977,-5.68982857655982,
143.932113529491));
#160008=CARTESIAN_POINT('Ctrl Pts',(95.8380393093066,-5.69208814865569,
143.942013881579));
#160009=CARTESIAN_POINT('Ctrl Pts',(95.8437108975836,-5.6941782216613,143.951429056206));
#160010=CARTESIAN_POINT('Ctrl Pts',(95.8466159734104,-5.69524878959892,
143.956251655252));
#160011=CARTESIAN_POINT('Ctrl Pts',(95.8494426936656,-5.69627576843121,
143.960946755587));
#160012=CARTESIAN_POINT('Ctrl Pts',(95.8521000410666,-5.69722957306762,
143.965362351826));
#160013=CARTESIAN_POINT('Ctrl Pts',(95.8876723499013,-5.7099975811501,144.024471278662));
#160014=CARTESIAN_POINT('Ctrl Pts',(95.9220548804864,-5.72024626941926,
144.082306677532));
#160015=CARTESIAN_POINT('Ctrl Pts',(95.955248172871,-5.72831884084642,144.138658626608));
#160016=CARTESIAN_POINT('Ctrl Pts',(95.9890946552891,-5.73655026735611,
144.196119490434));
#160017=CARTESIAN_POINT('Ctrl Pts',(96.021704635216,-5.7425195833988,144.252038215401));
#160018=CARTESIAN_POINT('Ctrl Pts',(96.0530786745858,-5.74658390705029,
144.306246926715));
#160019=CARTESIAN_POINT('Ctrl Pts',(96.085399727975,-5.7507709108397,144.362091908355));
#160020=CARTESIAN_POINT('Ctrl Pts',(96.1164091026634,-5.75293667524588,
144.416122349026));
#160021=CARTESIAN_POINT('Ctrl Pts',(96.1461073897856,-5.75345688194664,
144.468208200209));
#160022=CARTESIAN_POINT('Ctrl Pts',(96.1590723910637,-5.75368398193097,
144.490946653925));
#160023=CARTESIAN_POINT('Ctrl Pts',(96.1717875220325,-5.75359723721135,
144.513315153081));
#160024=CARTESIAN_POINT('Ctrl Pts',(96.1842528300077,-5.75322671858692,
144.535305717831));
#160025=CARTESIAN_POINT('Ctrl Pts',(96.2140135587319,-5.75234211113953,
144.58780784881));
#160026=CARTESIAN_POINT('Ctrl Pts',(96.2423502790985,-5.749841982628,144.638152608364));
#160027=CARTESIAN_POINT('Ctrl Pts',(96.2692636041749,-5.74611596217628,
144.686265851186));
#160028=CARTESIAN_POINT('Ctrl Pts',(96.2967084946548,-5.74231634905034,
144.735329379239));
#160029=CARTESIAN_POINT('Ctrl Pts',(96.3226732081329,-5.7372422921589,144.782072904419));
#160030=CARTESIAN_POINT('Ctrl Pts',(96.3471583424773,-5.73127376595626,
144.826461201895));
#160031=CARTESIAN_POINT('Ctrl Pts',(96.3722830473292,-5.72514933726687,
144.872008955781));
#160032=CARTESIAN_POINT('Ctrl Pts',(96.3958498685693,-5.71808342889945,
144.915077380993));
#160033=CARTESIAN_POINT('Ctrl Pts',(96.4178593893165,-5.71044664608885,
144.95566538353));
#160034=CARTESIAN_POINT('Ctrl Pts',(96.4211582959249,-5.70930200356936,
144.961748933978));
#160035=CARTESIAN_POINT('Ctrl Pts',(96.424422216655,-5.70814445968925,144.967776817202));
#160036=CARTESIAN_POINT('Ctrl Pts',(96.4276511533426,-5.70697518124098,
144.973749086811));
#160037=CARTESIAN_POINT('Ctrl Pts',(46.0788495272599,-8.05252143938036,
146.288922141324));
#160038=CARTESIAN_POINT('Ctrl Pts',(45.9880609926109,-8.16322880697465,
145.977772078405));
#160039=CARTESIAN_POINT('Ctrl Pts',(45.7994922443366,-8.35031067032238,
145.232841472766));
#160040=CARTESIAN_POINT('Ctrl Pts',(45.595594892883,-8.37180617735996,144.001345451837));
#160041=CARTESIAN_POINT('Ctrl Pts',(45.5003027990559,-8.05912368336601,
142.714039383314));
#160042=CARTESIAN_POINT('Ctrl Pts',(45.5182680777391,-7.4578196428506,141.583394803538));
#160043=CARTESIAN_POINT('Ctrl Pts',(45.6204150203276,-6.64097899990721,
140.678497336286));
#160044=CARTESIAN_POINT('Ctrl Pts',(45.7705368431435,-5.69964184453771,
140.032177372085));
#160045=CARTESIAN_POINT('Ctrl Pts',(45.9153295749133,-4.84202852027521,
139.689046596473));
#160046=CARTESIAN_POINT('Ctrl Pts',(46.0037739583116,-4.3117657385131,139.572935038824));
#160047=CARTESIAN_POINT('Ctrl Pts',(46.035646729361,-4.11818143590307,139.54229639283));
#160048=CARTESIAN_POINT('Ctrl Pts',(46.3362716867489,-6.53003741894398,
145.884574100139));
#160049=CARTESIAN_POINT('Ctrl Pts',(46.2465821908671,-6.61724703464641,
145.662644640647));
#160050=CARTESIAN_POINT('Ctrl Pts',(46.0606170235145,-6.76824259322373,
145.126576057234));
#160051=CARTESIAN_POINT('Ctrl Pts',(45.8600169789493,-6.80048023565777,
144.229068979079));
#160052=CARTESIAN_POINT('Ctrl Pts',(45.7663729040281,-6.57994028199158,
143.289221553569));
#160053=CARTESIAN_POINT('Ctrl Pts',(45.7842580175622,-6.1429024671548,142.471701432123));
#160054=CARTESIAN_POINT('Ctrl Pts',(45.885543403094,-5.550920127617,141.830975748337));
#160055=CARTESIAN_POINT('Ctrl Pts',(46.034968332973,-4.87786404776204,141.388235045773));
#160056=CARTESIAN_POINT('Ctrl Pts',(46.1797023896077,-4.27548810490898,
141.165229672644));
#160057=CARTESIAN_POINT('Ctrl Pts',(46.2683547176375,-3.90838758777078,
141.095688795383));
#160058=CARTESIAN_POINT('Ctrl Pts',(46.3003354431618,-3.77501126904855,
141.078486179093));
#160059=CARTESIAN_POINT('Ctrl Pts',(47.5411678644865,-5.6196269798719,145.367772703107));
#160060=CARTESIAN_POINT('Ctrl Pts',(47.4567005603587,-5.6735582042356,145.216692900741));
#160061=CARTESIAN_POINT('Ctrl Pts',(47.2829935018905,-5.76476706996246,
144.854924187768));
#160062=CARTESIAN_POINT('Ctrl Pts',(47.0975908720934,-5.77557260627988,
144.256703390162));
#160063=CARTESIAN_POINT('Ctrl Pts',(47.0110339405536,-5.62384586859696,
143.631348870314));
#160064=CARTESIAN_POINT('Ctrl Pts',(47.0275751460305,-5.33175612882522,
143.08220807961));
#160065=CARTESIAN_POINT('Ctrl Pts',(47.1235249583571,-4.93493511480553,
142.642897466375));
#160066=CARTESIAN_POINT('Ctrl Pts',(47.2680941387717,-4.47773164599018,
142.32932716126));
#160067=CARTESIAN_POINT('Ctrl Pts',(47.4109838899983,-4.06133055703064,
142.163019363412));
#160068=CARTESIAN_POINT('Ctrl Pts',(47.4995824081453,-3.80394222364136,
142.106824516817));
#160069=CARTESIAN_POINT('Ctrl Pts',(47.5316865599187,-3.70998577779816,
142.092012095983));
#160070=CARTESIAN_POINT('Ctrl Pts',(49.085823466348,-5.78047467324188,144.999177546568));
#160071=CARTESIAN_POINT('Ctrl Pts',(49.0080675852836,-5.80813151968957,
144.864841948352));
#160072=CARTESIAN_POINT('Ctrl Pts',(48.8500905300059,-5.84600797378507,
144.554899167795));
#160073=CARTESIAN_POINT('Ctrl Pts',(48.6841202887859,-5.81401689355999,
144.070310691762));
#160074=CARTESIAN_POINT('Ctrl Pts',(48.6065150760652,-5.67306666243705,
143.567862263895));
#160075=CARTESIAN_POINT('Ctrl Pts',(48.6211264587277,-5.43349925308774,
143.106992946301));
#160076=CARTESIAN_POINT('Ctrl Pts',(48.7099577896873,-5.10370888932707,
142.7047527862));
#160077=CARTESIAN_POINT('Ctrl Pts',(48.8479614629199,-4.70105978697968,
142.380794222149));
#160078=CARTESIAN_POINT('Ctrl Pts',(48.9881514924996,-4.30757071617114,
142.179159564002));
#160079=CARTESIAN_POINT('Ctrl Pts',(49.0764615863807,-4.0511088505606,142.09635474851));
#160080=CARTESIAN_POINT('Ctrl Pts',(49.1086423835475,-3.95590192902217,
142.071681143907));
#160081=CARTESIAN_POINT('Origin',(48.9387462821982,-4.8069199738566,139.198070090029));
#160082=CARTESIAN_POINT('',(48.9057735093079,-5.78172535422313,144.973729670506));
#160083=CARTESIAN_POINT('Ctrl Pts',(48.9057735093079,-5.78172535422313,
144.973729670506));
#160084=CARTESIAN_POINT('Ctrl Pts',(48.8574830042264,-5.79875125836896,
144.886741723157));
#160085=CARTESIAN_POINT('Ctrl Pts',(48.8130418788545,-5.8111995246564,144.798629889593));
#160086=CARTESIAN_POINT('Ctrl Pts',(48.7726367086002,-5.81891384412796,
144.709933253049));
#160087=CARTESIAN_POINT('Ctrl Pts',(48.7585750597405,-5.8215985513305,144.679065397518));
#160088=CARTESIAN_POINT('Ctrl Pts',(48.7450021368848,-5.82371012549766,
144.648126322326));
#160089=CARTESIAN_POINT('Ctrl Pts',(48.7319255740939,-5.82524255184348,
144.617137367132));
#160090=CARTESIAN_POINT('Ctrl Pts',(48.6962719955212,-5.82942075096211,
144.532645198465));
#160091=CARTESIAN_POINT('Ctrl Pts',(48.6643077444896,-5.82929399145005,
144.447785980287));
#160092=CARTESIAN_POINT('Ctrl Pts',(48.6359541682921,-5.82484331547223,
144.363010384092));
#160093=CARTESIAN_POINT('Ctrl Pts',(48.6080496963055,-5.82046313562193,
144.279577584198));
#160094=CARTESIAN_POINT('Ctrl Pts',(48.5836421004334,-5.8118960502912,144.196225488765));
#160095=CARTESIAN_POINT('Ctrl Pts',(48.5626654288617,-5.79911081975773,
144.113335535882));
#160096=CARTESIAN_POINT('Ctrl Pts',(48.5598696769203,-5.79740681571865,
144.102288037431));
#160097=CARTESIAN_POINT('Ctrl Pts',(48.5571348872439,-5.79562784941034,
144.091248682514));
#160098=CARTESIAN_POINT('Ctrl Pts',(48.5544609211838,-5.79377381185531,
144.08021831539));
#160099=CARTESIAN_POINT('Ctrl Pts',(48.5511232491381,-5.7914595830357,144.066450097253));
#160100=CARTESIAN_POINT('Ctrl Pts',(48.5478803414289,-5.78902839204097,
144.052695883244));
#160101=CARTESIAN_POINT('Ctrl Pts',(48.5447307972159,-5.78648057560322,
144.038957589553));
#160102=CARTESIAN_POINT('Ctrl Pts',(48.5221573243652,-5.76821981744402,
143.94049223118));
#160103=CARTESIAN_POINT('Ctrl Pts',(48.5045343563197,-5.74398192497538,
143.842897887433));
#160104=CARTESIAN_POINT('Ctrl Pts',(48.4918543546712,-5.71388516193183,
143.746894525912));
#160105=CARTESIAN_POINT('Ctrl Pts',(48.4845454288058,-5.69653697728886,
143.691556879149));
#160106=CARTESIAN_POINT('Ctrl Pts',(48.4788793532058,-5.67724131526062,
143.63674821976));
#160107=CARTESIAN_POINT('Ctrl Pts',(48.4748586649403,-5.65601566467528,
143.582610646526));
#160108=CARTESIAN_POINT('Ctrl Pts',(48.4747413674277,-5.65539643835058,
143.581031264524));
#160109=CARTESIAN_POINT('Ctrl Pts',(48.4746254677557,-5.65477557022504,
143.579452456466));
#160110=CARTESIAN_POINT('Ctrl Pts',(48.474510967766,-5.65415306061376,143.577874225666));
#160111=CARTESIAN_POINT('Ctrl Pts',(48.4692585741228,-5.62559702726476,
143.505476931644));
#160112=CARTESIAN_POINT('Ctrl Pts',(48.466950212038,-5.59358706740297,143.43429152169));
#160113=CARTESIAN_POINT('Ctrl Pts',(48.4675859848779,-5.55825509465883,
143.364633654463));
#160114=CARTESIAN_POINT('Ctrl Pts',(48.4679108010891,-5.54020399715544,
143.32904546463));
#160115=CARTESIAN_POINT('Ctrl Pts',(48.4690041002126,-5.52128551225177,
143.293855973406));
#160116=CARTESIAN_POINT('Ctrl Pts',(48.4708659099544,-5.50151600329219,
143.259108081192));
#160117=CARTESIAN_POINT('Ctrl Pts',(48.4717968148254,-5.4916312488124,143.241734135085));
#160118=CARTESIAN_POINT('Ctrl Pts',(48.4729198473072,-5.48153372475322,
143.22447059585));
#160119=CARTESIAN_POINT('Ctrl Pts',(48.4742350105987,-5.47122544851078,
143.207322943274));
#160120=CARTESIAN_POINT('Ctrl Pts',(48.4748925922445,-5.46607131038957,
143.198749116987));
#160121=CARTESIAN_POINT('Ctrl Pts',(48.4755982065885,-5.46086448384824,
143.190204263258));
#160122=CARTESIAN_POINT('Ctrl Pts',(48.476351854012,-5.4556052200133,143.181689073789));
#160123=CARTESIAN_POINT('Ctrl Pts',(48.4767286777238,-5.45297558809582,
143.177431479055));
#160124=CARTESIAN_POINT('Ctrl Pts',(48.4771175097053,-5.4503328468415,143.173181300447));
#160125=CARTESIAN_POINT('Ctrl Pts',(48.4775183500038,-5.44767702770147,
143.168938624996));
#160126=CARTESIAN_POINT('Ctrl Pts',(48.4778243720832,-5.44564943891133,
143.165699548563));
#160127=CARTESIAN_POINT('Ctrl Pts',(48.478231074737,-5.44301375622949,143.161513471526));
#160128=CARTESIAN_POINT('Ctrl Pts',(48.4785244702588,-5.44114456717572,
143.158559835133));
#160129=CARTESIAN_POINT('Ctrl Pts',(48.4786153762513,-5.44056541557508,
143.157644677171));
#160130=CARTESIAN_POINT('Ctrl Pts',(48.4786951456533,-5.44006017141317,
143.156847647423));
#160131=CARTESIAN_POINT('Ctrl Pts',(48.4787568958971,-5.43967036809464,
143.156233195461));
#160132=CARTESIAN_POINT('Ctrl Pts',(48.4802449745291,-5.43027675353651,
143.141425920541));
#160133=CARTESIAN_POINT('Ctrl Pts',(48.4819591686244,-5.4204941631384,143.126350799725));
#160134=CARTESIAN_POINT('Ctrl Pts',(48.4839048570574,-5.41030171981581,
143.111028284083));
#160135=CARTESIAN_POINT('Ctrl Pts',(48.4884010326069,-5.38674860942085,
143.075620395019));
#160136=CARTESIAN_POINT('Ctrl Pts',(48.4941346838576,-5.36100732183593,
143.038888481324));
#160137=CARTESIAN_POINT('Ctrl Pts',(48.5011476052396,-5.33282369208186,
143.001107300327));
#160138=CARTESIAN_POINT('Ctrl Pts',(48.5078840387509,-5.30575121577626,
142.964815660952));
#160139=CARTESIAN_POINT('Ctrl Pts',(48.5158012921635,-5.27642492613411,
142.927555634262));
#160140=CARTESIAN_POINT('Ctrl Pts',(48.5249180660653,-5.24461405749319,
142.889613059426));
#160141=CARTESIAN_POINT('Ctrl Pts',(48.5335054703596,-5.21465030135375,
142.853873637389));
#160142=CARTESIAN_POINT('Ctrl Pts',(48.5431573793493,-5.18248189349009,
142.81752855818));
#160143=CARTESIAN_POINT('Ctrl Pts',(48.5538682402161,-5.14791443396958,
142.780856891134));
#160144=CARTESIAN_POINT('Ctrl Pts',(48.5610547769995,-5.12472112369863,
142.756251746186));
#160145=CARTESIAN_POINT('Ctrl Pts',(48.5687176082766,-5.10044776238925,
142.73150038102));
#160146=CARTESIAN_POINT('Ctrl Pts',(48.5768483642691,-5.07503604108531,
142.706698594798));
#160147=CARTESIAN_POINT('Ctrl Pts',(48.5883349654884,-5.03913602032692,
142.671660250501));
#160148=CARTESIAN_POINT('Ctrl Pts',(48.6007570081408,-5.00096318819923,
142.636519730009));
#160149=CARTESIAN_POINT('Ctrl Pts',(48.6140606015791,-4.96037412893768,
142.601565895071));
#160150=CARTESIAN_POINT('Ctrl Pts',(48.6155444485146,-4.95584693472676,
142.597667238584));
#160151=CARTESIAN_POINT('Ctrl Pts',(48.6170392298211,-4.95128969428845,
142.593770945232));
#160152=CARTESIAN_POINT('Ctrl Pts',(48.6185448454909,-4.94670221900433,
142.589877447084));
#160153=CARTESIAN_POINT('Ctrl Pts',(48.6312990436561,-4.90784132639545,
142.556895293708));
#160154=CARTESIAN_POINT('Ctrl Pts',(48.6447969328006,-4.86682337149193,
142.524122734055));
#160155=CARTESIAN_POINT('Ctrl Pts',(48.659112698478,-4.8235493389134,142.491842849455));
#160156=CARTESIAN_POINT('Ctrl Pts',(48.6730539457726,-4.78140740929511,
142.460407447117));
#160157=CARTESIAN_POINT('Ctrl Pts',(48.6877710045931,-4.73712575480717,
142.429439330805));
#160158=CARTESIAN_POINT('Ctrl Pts',(48.703303248073,-4.69063288592935,142.399235166709));
#160159=CARTESIAN_POINT('Ctrl Pts',(48.7056309371197,-4.68366538366385,
142.394708718098));
#160160=CARTESIAN_POINT('Ctrl Pts',(48.7079768766572,-4.67664826045055,
142.390199491961));
#160161=CARTESIAN_POINT('Ctrl Pts',(48.7103411371858,-4.66958131864314,
142.385708556192));
#160162=CARTESIAN_POINT('Ctrl Pts',(48.7260142670445,-4.62273322584015,
142.355937294251));
#160163=CARTESIAN_POINT('Ctrl Pts',(48.7424950052783,-4.57369357852764,
142.326967368551));
#160164=CARTESIAN_POINT('Ctrl Pts',(48.7598002750494,-4.52243128457966,
142.299109381492));
#160165=CARTESIAN_POINT('Ctrl Pts',(48.7766824729776,-4.47242222929603,
142.2719324546));
#160166=CARTESIAN_POINT('Ctrl Pts',(48.7943494995698,-4.42029781174223,
142.24581383713));
#160167=CARTESIAN_POINT('Ctrl Pts',(48.8127870284115,-4.36605564997263,
142.221070016252));
#160168=CARTESIAN_POINT('Ctrl Pts',(48.8294029814107,-4.31717246078438,
142.198770815082));
#160169=CARTESIAN_POINT('Ctrl Pts',(48.8466444608402,-4.26656957193763,
142.177588497048));
#160170=CARTESIAN_POINT('Ctrl Pts',(48.864477872093,-4.21426504024486,142.157774539181));
#160171=CARTESIAN_POINT('Ctrl Pts',(48.8835392481959,-4.15835894710614,
142.136596240893));
#160172=CARTESIAN_POINT('Ctrl Pts',(48.9032769193088,-4.10050744227999,
142.116981385794));
#160173=CARTESIAN_POINT('Ctrl Pts',(48.9236451106707,-4.04081169564955,
142.099235508675));
#160174=CARTESIAN_POINT('Ctrl Pts',(48.9282346510359,-4.02736052397112,
142.095236851263));
#160175=CARTESIAN_POINT('Ctrl Pts',(48.9328560941336,-4.0138158715974,142.09133316896));
#160176=CARTESIAN_POINT('Ctrl Pts',(48.9375087193678,-4.00017917397872,
142.087528100711));
#160177=CARTESIAN_POINT('Origin',(48.9104317825618,-8.72626638758926,145.547624122242));
#160178=CARTESIAN_POINT('Origin',(10.4437182387877,-3.3884479131999,144.495399400904));
#160179=CARTESIAN_POINT('',(48.9057735357879,-5.78174222830161,144.973732958521));
#160180=CARTESIAN_POINT('Ctrl Pts',(46.0225958916338,4.1854380591026,139.544563094783));
#160181=CARTESIAN_POINT('Ctrl Pts',(45.9812730775996,4.43160751792965,139.583694415389));
#160182=CARTESIAN_POINT('Ctrl Pts',(45.8817256585986,5.01513721022549,139.72158867393));
#160183=CARTESIAN_POINT('Ctrl Pts',(45.7266500710242,5.91846538933026,140.119945925672));
#160184=CARTESIAN_POINT('Ctrl Pts',(45.5790466613153,6.84385432790675,140.806566615535));
#160185=CARTESIAN_POINT('Ctrl Pts',(45.4852947783209,7.63098616909916,141.748557124114));
#160186=CARTESIAN_POINT('Ctrl Pts',(45.4813493332435,8.19023998484079,142.906059572216));
#160187=CARTESIAN_POINT('Ctrl Pts',(45.5942140393653,8.45348830956667,144.205359185367));
#160188=CARTESIAN_POINT('Ctrl Pts',(45.8026477379926,8.38883204657363,145.364075241063));
#160189=CARTESIAN_POINT('Ctrl Pts',(45.9794174121251,8.20606751734297,146.040910018887));
#160190=CARTESIAN_POINT('Ctrl Pts',(46.0534055265581,8.11631521630629,146.293329214793));
#160191=CARTESIAN_POINT('Ctrl Pts',(46.2883692083799,3.84230106733182,141.08057138548));
#160192=CARTESIAN_POINT('Ctrl Pts',(46.2471489482482,4.01187144162188,141.102561270826));
#160193=CARTESIAN_POINT('Ctrl Pts',(46.1479570361563,4.41631048619959,141.186121368824));
#160194=CARTESIAN_POINT('Ctrl Pts',(45.9938835061498,5.05252428928464,141.447777275722));
#160195=CARTESIAN_POINT('Ctrl Pts',(45.8478708762706,5.71572290838207,141.921029285075));
#160196=CARTESIAN_POINT('Ctrl Pts',(45.7556082758894,6.28688824505787,142.590694965869));
#160197=CARTESIAN_POINT('Ctrl Pts',(45.7520119369578,6.69282762784374,143.429483847216));
#160198=CARTESIAN_POINT('Ctrl Pts',(45.8631813379175,6.87599162214231,144.378537428345));
#160199=CARTESIAN_POINT('Ctrl Pts',(46.0683011093412,6.81206541535659,145.221882022372));
#160200=CARTESIAN_POINT('Ctrl Pts',(46.2425858947116,6.66552440867401,145.708123051829));
#160201=CARTESIAN_POINT('Ctrl Pts',(46.3156201733044,6.59488103790824,145.888155999971));
#160202=CARTESIAN_POINT('Ctrl Pts',(47.5199218191278,3.78062210798581,142.094063635992));
#160203=CARTESIAN_POINT('Ctrl Pts',(47.4786970341152,3.90003471796203,142.112982235428));
#160204=CARTESIAN_POINT('Ctrl Pts',(47.3800382801279,4.18312907406931,142.179733051624));
#160205=CARTESIAN_POINT('Ctrl Pts',(47.2289770169779,4.62151410983383,142.372846739715));
#160206=CARTESIAN_POINT('Ctrl Pts',(47.0887712885677,5.07077755475171,142.706010783594));
#160207=CARTESIAN_POINT('Ctrl Pts',(47.0021425885985,5.4530433520793,143.16336790427));
#160208=CARTESIAN_POINT('Ctrl Pts',(46.9992581570219,5.7246874050313,143.725580656898));
#160209=CARTESIAN_POINT('Ctrl Pts',(47.1020581503972,5.85252013288016,144.356769743511));
#160210=CARTESIAN_POINT('Ctrl Pts',(47.291745722439,5.82101797727647,144.919622760124));
#160211=CARTESIAN_POINT('Ctrl Pts',(47.4546670828204,5.73217254703968,145.248311075454));
#160212=CARTESIAN_POINT('Ctrl Pts',(47.5233698054881,5.68855250677466,145.370874265986));
#160213=CARTESIAN_POINT('Ctrl Pts',(49.0960992191677,4.03151001320818,142.073867792845));
#160214=CARTESIAN_POINT('Ctrl Pts',(49.0547651127025,4.15250410057625,142.105334310947));
#160215=CARTESIAN_POINT('Ctrl Pts',(48.9565482606377,4.43320198484628,142.201278771501));
#160216=CARTESIAN_POINT('Ctrl Pts',(48.8089901856194,4.84282216533669,142.428579800424));
#160217=CARTESIAN_POINT('Ctrl Pts',(48.6758786708201,5.23430742494674,142.765592341929));
#160218=CARTESIAN_POINT('Ctrl Pts',(48.5961869355628,5.55001534344916,143.177738603068));
#160219=CARTESIAN_POINT('Ctrl Pts',(48.5940181499387,5.77411730330242,143.645008539377));
#160220=CARTESIAN_POINT('Ctrl Pts',(48.685995886383,5.89927909395418,144.151035032819));
#160221=CARTESIAN_POINT('Ctrl Pts',(48.8559164790919,5.91554136284544,144.609747053932));
#160222=CARTESIAN_POINT('Ctrl Pts',(49.004327214937,5.87676381771975,144.893388080051));
#160223=CARTESIAN_POINT('Ctrl Pts',(49.0675053554823,5.85445183185201,145.002383852898));
#160224=CARTESIAN_POINT('',(48.8874340390554,5.85518035418594,144.976887878439));
#160225=CARTESIAN_POINT('Origin',(48.8828366595184,8.79945069508729,145.552470666265));
#160226=CARTESIAN_POINT('Ctrl Pts',(48.9248217637666,4.07524046612488,142.089743831931));
#160227=CARTESIAN_POINT('Ctrl Pts',(48.9088894384633,4.12146053551437,142.102686008398));
#160228=CARTESIAN_POINT('Ctrl Pts',(48.8936098512241,4.16551766241371,142.116452986942));
#160229=CARTESIAN_POINT('Ctrl Pts',(48.879013781374,4.20742683554834,142.130726436299));
#160230=CARTESIAN_POINT('Ctrl Pts',(48.8637859130388,4.2511500690684,142.145617719345));
#160231=CARTESIAN_POINT('Ctrl Pts',(48.8493018159786,4.29253570059324,142.161060172306));
#160232=CARTESIAN_POINT('Ctrl Pts',(48.8355701607073,4.33163089141771,142.17673234098));
#160233=CARTESIAN_POINT('Ctrl Pts',(48.8318014092585,4.34236084743149,142.181033680274));
#160234=CARTESIAN_POINT('Ctrl Pts',(48.8280892000489,4.3529184239031,142.185352551563));
#160235=CARTESIAN_POINT('Ctrl Pts',(48.8244334187919,4.36330491679753,142.189682819269));
#160236=CARTESIAN_POINT('Ctrl Pts',(48.8104461361547,4.40304438738069,142.206250735686));
#160237=CARTESIAN_POINT('Ctrl Pts',(48.7972868627936,4.44027862099375,142.222981686069));
#160238=CARTESIAN_POINT('Ctrl Pts',(48.7849407050485,4.47510737564834,142.239554542838));
#160239=CARTESIAN_POINT('Ctrl Pts',(48.7757581914447,4.50101142774503,142.251880683965));
#160240=CARTESIAN_POINT('Ctrl Pts',(48.7670248487054,4.52558515411604,142.264120430663));
#160241=CARTESIAN_POINT('Ctrl Pts',(48.7587268923065,4.5488723158606,142.276158338025));
#160242=CARTESIAN_POINT('Ctrl Pts',(48.7468529536423,4.58219501809265,142.293383949585));
#160243=CARTESIAN_POINT('Ctrl Pts',(48.7358978629908,4.61287532880214,142.310189894057));
#160244=CARTESIAN_POINT('Ctrl Pts',(48.7258666794082,4.64103991314218,142.326281092176));
#160245=CARTESIAN_POINT('Ctrl Pts',(48.7176588038369,4.6640851900906,142.339447489827));
#160246=CARTESIAN_POINT('Ctrl Pts',(48.7100689965524,4.68544632172692,142.352136432435));
#160247=CARTESIAN_POINT('Ctrl Pts',(48.7030940396954,4.7051903667889,142.364211306854));
#160248=CARTESIAN_POINT('Ctrl Pts',(48.7013109664932,4.71023772096972,142.367298119494));
#160249=CARTESIAN_POINT('Ctrl Pts',(48.6998394384133,4.71440730500938,142.369867794337));
#160250=CARTESIAN_POINT('Ctrl Pts',(48.6981205105038,4.71929092858846,142.372899133817));
#160251=CARTESIAN_POINT('Ctrl Pts',(48.6966593374644,4.72344224818082,142.375475921067));
#160252=CARTESIAN_POINT('Ctrl Pts',(48.6950192868673,4.72810971549003,142.378386076254));
#160253=CARTESIAN_POINT('Ctrl Pts',(48.6928656811989,4.73425220792585,142.382259196829));
#160254=CARTESIAN_POINT('Ctrl Pts',(48.69204717446,4.73658674461746,142.383731228286));
#160255=CARTESIAN_POINT('Ctrl Pts',(48.6911545979916,4.73913410396654,142.385342717972));
#160256=CARTESIAN_POINT('Ctrl Pts',(48.6901701315476,4.74194575257293,142.387129951436));
#160257=CARTESIAN_POINT('Ctrl Pts',(48.6835481969699,4.76085808141801,142.399151633986));
#160258=CARTESIAN_POINT('Ctrl Pts',(48.6770636059516,4.7794709581225,142.411340421246));
#160259=CARTESIAN_POINT('Ctrl Pts',(48.6707163584928,4.79778440127906,142.423681254348));
#160260=CARTESIAN_POINT('Ctrl Pts',(48.6692228600872,4.80209352871312,142.426585035031));
#160261=CARTESIAN_POINT('Ctrl Pts',(48.6677369620367,4.80638608609014,142.429497239768));
#160262=CARTESIAN_POINT('Ctrl Pts',(48.6662586623385,4.81066208145745,142.432417678715));
#160263=CARTESIAN_POINT('Ctrl Pts',(48.655171653674,4.84273135519406,142.454320498521));
#160264=CARTESIAN_POINT('Ctrl Pts',(48.6445125102291,4.87386872771066,142.476686013722));
#160265=CARTESIAN_POINT('Ctrl Pts',(48.6342809787104,4.90408376147835,142.499430874036));
#160266=CARTESIAN_POINT('Ctrl Pts',(48.6180120989511,4.95212786420115,142.535596857293));
#160267=CARTESIAN_POINT('Ctrl Pts',(48.6028051993584,4.99783953900665,142.572720744986));
#160268=CARTESIAN_POINT('Ctrl Pts',(48.5886903281095,5.04127728535629,142.61049650008));
#160269=CARTESIAN_POINT('Ctrl Pts',(48.5742119799819,5.0858336119734,142.649245031567));
#160270=CARTESIAN_POINT('Ctrl Pts',(48.5608825032169,5.12799749856814,142.6886794128));
#160271=CARTESIAN_POINT('Ctrl Pts',(48.5486991875105,5.16785428489672,142.728505144144));
#160272=CARTESIAN_POINT('Ctrl Pts',(48.5447821694551,5.18066851014064,142.741309385002));
#160273=CARTESIAN_POINT('Ctrl Pts',(48.5409833685402,5.19324441894756,142.754154350228));
#160274=CARTESIAN_POINT('Ctrl Pts',(48.5373019856571,5.20558528587342,142.767031014309));
#160275=CARTESIAN_POINT('Ctrl Pts',(48.5317708300825,5.22412702876113,142.786377774637));
#160276=CARTESIAN_POINT('Ctrl Pts',(48.5265047900417,5.24213816872921,142.80579598422));
#160277=CARTESIAN_POINT('Ctrl Pts',(48.5214984305421,5.25963270414364,142.825254404319));
#160278=CARTESIAN_POINT('Ctrl Pts',(48.5104020313479,5.29840865475055,142.868383228195));
#160279=CARTESIAN_POINT('Ctrl Pts',(48.5006077938204,5.33464508048347,142.911705535247));
#160280=CARTESIAN_POINT('Ctrl Pts',(48.4921198079405,5.36850506162563,142.954916641507));
#160281=CARTESIAN_POINT('Ctrl Pts',(48.4895903889023,5.37859533299852,142.967793547334));
#160282=CARTESIAN_POINT('Ctrl Pts',(48.4871767689155,5.38847462600499,142.980660866471));
#160283=CARTESIAN_POINT('Ctrl Pts',(48.4848785630768,5.39814739688027,142.99351124648));
#160284=CARTESIAN_POINT('Ctrl Pts',(48.4798734089431,5.41921326848959,143.021497483195));
#160285=CARTESIAN_POINT('Ctrl Pts',(48.4754172858013,5.43929967677792,143.049403125118));
#160286=CARTESIAN_POINT('Ctrl Pts',(48.4715101193556,5.45845409577054,143.077158071069));
#160287=CARTESIAN_POINT('Ctrl Pts',(48.4695565361327,5.46803130526684,143.091035544044));
#160288=CARTESIAN_POINT('Ctrl Pts',(48.4677401921302,5.47737547828869,143.104875366129));
#160289=CARTESIAN_POINT('Ctrl Pts',(48.466061077691,5.48649272826543,143.118669513915));
#160290=CARTESIAN_POINT('Ctrl Pts',(48.4652215204714,5.4910513532538,143.125566587808));
#160291=CARTESIAN_POINT('Ctrl Pts',(48.464416270646,5.49555324489794,143.132452244518));
#160292=CARTESIAN_POINT('Ctrl Pts',(48.4636453270126,5.49999916308236,143.139325504608));
#160293=CARTESIAN_POINT('Ctrl Pts',(48.4631422494356,5.5029003372419,143.143810635404));
#160294=CARTESIAN_POINT('Ctrl Pts',(48.4627271566693,5.50534082490976,143.147609135156));
#160295=CARTESIAN_POINT('Ctrl Pts',(48.4622551083268,5.50817764338732,143.152053631565));
#160296=CARTESIAN_POINT('Ctrl Pts',(48.4620037639343,5.50968812092225,143.154420124886));
#160297=CARTESIAN_POINT('Ctrl Pts',(48.461736662224,5.51131047506557,143.15697005603));
#160298=CARTESIAN_POINT('Ctrl Pts',(48.461435413493,5.51316975414571,143.159907129807));
#160299=CARTESIAN_POINT('Ctrl Pts',(48.4606569046263,5.51797463828491,143.167497329341));
#160300=CARTESIAN_POINT('Ctrl Pts',(48.4599162273016,5.52273771424791,143.17511224162));
#160301=CARTESIAN_POINT('Ctrl Pts',(48.459213646533,5.52745867760706,143.182751407617));
#160302=CARTESIAN_POINT('Ctrl Pts',(48.4514706867652,5.57948718591747,143.266940667586));
#160303=CARTESIAN_POINT('Ctrl Pts',(48.448353044463,5.62640005932763,143.354072810273));
#160304=CARTESIAN_POINT('Ctrl Pts',(48.4499804128068,5.66795182294563,143.443443931927));
#160305=CARTESIAN_POINT('Ctrl Pts',(48.4512447100305,5.7002332542409,143.512876068429));
#160306=CARTESIAN_POINT('Ctrl Pts',(48.4553731825803,5.72927947792775,143.58365999408));
#160307=CARTESIAN_POINT('Ctrl Pts',(48.4624330309206,5.75497534443534,143.655484935499));
#160308=CARTESIAN_POINT('Ctrl Pts',(48.4706470433165,5.78487204417221,143.739052022313));
#160309=CARTESIAN_POINT('Ctrl Pts',(48.4828287068606,5.81023470834922,143.824027338883));
#160310=CARTESIAN_POINT('Ctrl Pts',(48.4988171960137,5.83102386157057,143.909935807251));
#160311=CARTESIAN_POINT('Ctrl Pts',(48.5069927734158,5.84165421755082,143.953864368975));
#160312=CARTESIAN_POINT('Ctrl Pts',(48.5161640811989,5.85108838792821,143.998037560987));
#160313=CARTESIAN_POINT('Ctrl Pts',(48.5263120580339,5.85931795799407,144.042395450064));
#160314=CARTESIAN_POINT('Ctrl Pts',(48.5353637138622,5.86665845916609,144.081961203092));
#160315=CARTESIAN_POINT('Ctrl Pts',(48.5451875327568,5.8730383748811,144.121662641184));
#160316=CARTESIAN_POINT('Ctrl Pts',(48.555812740026,5.87845101381005,144.161452853898));
#160317=CARTESIAN_POINT('Ctrl Pts',(48.578289600787,5.88990106165131,144.245626183242));
#160318=CARTESIAN_POINT('Ctrl Pts',(48.6043523108742,5.89702341201655,144.330199990794));
#160319=CARTESIAN_POINT('Ctrl Pts',(48.63403389734,5.89986022843376,144.414775080605));
#160320=CARTESIAN_POINT('Ctrl Pts',(48.6642639406615,5.90274946359261,144.500912950354));
#160321=CARTESIAN_POINT('Ctrl Pts',(48.6982481968732,5.90119208749396,144.587052284651));
#160322=CARTESIAN_POINT('Ctrl Pts',(48.7360268924637,5.89522534133957,144.672718311044));
#160323=CARTESIAN_POINT('Ctrl Pts',(48.7400930294678,5.89458313792431,144.68193858174));
#160324=CARTESIAN_POINT('Ctrl Pts',(48.7442031245072,5.89388985851974,144.691153320021));
#160325=CARTESIAN_POINT('Ctrl Pts',(48.7483572288102,5.89314555373829,144.700361898933));
#160326=CARTESIAN_POINT('Ctrl Pts',(48.7903100036049,5.88562873456459,144.79336039129));
#160327=CARTESIAN_POINT('Ctrl Pts',(48.8367525975183,5.87290511982796,144.885734945757));
#160328=CARTESIAN_POINT('Ctrl Pts',(48.8874340618173,5.85516576140854,144.97688502578));
#160329=CARTESIAN_POINT('Origin',(48.9235486361196,4.8835311182205,139.200683316394));
#160330=CARTESIAN_POINT('Origin',(10.4331297884161,3.34111880277824,144.497266430389));
#160331=CARTESIAN_POINT('',(96.4093348692712,5.9299457611023,144.976966946015));
#160332=CARTESIAN_POINT('',(48.8874340344061,5.85518334895249,144.976888463869));
#160333=CARTESIAN_POINT('Ctrl Pts',(96.4093348654697,5.92994817616452,144.976967418175));
#160334=CARTESIAN_POINT('Ctrl Pts',(96.3879022801485,5.93765465679943,144.937376728462));
#160335=CARTESIAN_POINT('Ctrl Pts',(96.3649282432297,5.94484703642197,144.8953296167));
#160336=CARTESIAN_POINT('Ctrl Pts',(96.3404133194485,5.95116639403942,144.850822032184));
#160337=CARTESIAN_POINT('Ctrl Pts',(96.3163617535213,5.95736630914868,144.807155687847));
#160338=CARTESIAN_POINT('Ctrl Pts',(96.2908269994181,5.96272563710496,144.76112044886));
#160339=CARTESIAN_POINT('Ctrl Pts',(96.2638096495332,5.96686787341956,144.712745233282));
#160340=CARTESIAN_POINT('Ctrl Pts',(96.2375327979243,5.97089657828627,144.665695897699));
#160341=CARTESIAN_POINT('Ctrl Pts',(96.2098535080668,5.97377363439324,144.616432647817));
#160342=CARTESIAN_POINT('Ctrl Pts',(96.1807723742022,5.97512135805271,144.565020584938));
#160343=CARTESIAN_POINT('Ctrl Pts',(96.1757443005913,5.97535437695075,144.5561315355));
#160344=CARTESIAN_POINT('Ctrl Pts',(96.1706743206981,5.97554160861103,144.547178354883));
#160345=CARTESIAN_POINT('Ctrl Pts',(96.165562437728,5.97568101560295,144.53816151594));
#160346=CARTESIAN_POINT('Ctrl Pts',(96.1369556496969,5.97646115597219,144.487702066485));
#160347=CARTESIAN_POINT('Ctrl Pts',(96.107036591701,5.97574528489729,144.435245319868));
#160348=CARTESIAN_POINT('Ctrl Pts',(96.0758058458112,5.97316344779516,144.380900667205));
#160349=CARTESIAN_POINT('Ctrl Pts',(96.0455244413974,5.97066009248959,144.32820796461));
#160350=CARTESIAN_POINT('Ctrl Pts',(96.0140098822271,5.96640205378425,144.273740128256));
#160351=CARTESIAN_POINT('Ctrl Pts',(95.9812627241773,5.96003601986145,144.217642802994));
#160352=CARTESIAN_POINT('Ctrl Pts',(95.962724450751,5.95643218720757,144.185885923432));
#160353=CARTESIAN_POINT('Ctrl Pts',(95.9437911631774,5.9521525367929,144.153607698493));
#160354=CARTESIAN_POINT('Ctrl Pts',(95.9244629647314,5.94713142687235,144.120841865845));
#160355=CARTESIAN_POINT('Ctrl Pts',(95.9096823563841,5.94329169709042,144.095785265723));
#160356=CARTESIAN_POINT('Ctrl Pts',(95.8946708071211,5.93901834229097,144.070443622098));
#160357=CARTESIAN_POINT('Ctrl Pts',(95.8794283635279,5.9342817523375,144.044834308875));
#160358=CARTESIAN_POINT('Ctrl Pts',(95.8718071417313,5.93191345736077,144.032029652263));
#160359=CARTESIAN_POINT('Ctrl Pts',(95.8641281963653,5.92942934523654,144.019158079849));
#160360=CARTESIAN_POINT('Ctrl Pts',(95.8563915332562,5.92682571266049,144.006222002307));
#160361=CARTESIAN_POINT('Ctrl Pts',(95.8511704408754,5.92506864943911,143.997492081548));
#160362=CARTESIAN_POINT('Ctrl Pts',(95.8462652957885,5.92337618064007,143.989303169993));
#160363=CARTESIAN_POINT('Ctrl Pts',(95.8409832275859,5.92150813516453,143.980500826323));
#160364=CARTESIAN_POINT('Ctrl Pts',(95.8384382781412,5.92060809353057,143.976259775512));
#160365=CARTESIAN_POINT('Ctrl Pts',(95.8358058307864,5.91966660169065,143.971876463109));
#160366=CARTESIAN_POINT('Ctrl Pts',(95.8330083965617,5.9186525275665,143.967222690912));
#160367=CARTESIAN_POINT('Ctrl Pts',(95.8003309432189,5.90680690146184,143.912860939527));
#160368=CARTESIAN_POINT('Ctrl Pts',(95.7688813316534,5.89357318545835,143.860839945248));
#160369=CARTESIAN_POINT('Ctrl Pts',(95.7386589333837,5.87935081357124,143.811174028236));
#160370=CARTESIAN_POINT('Ctrl Pts',(95.7077195738219,5.86479104654975,143.760329894337));
#160371=CARTESIAN_POINT('Ctrl Pts',(95.6780663437034,5.84919546427068,143.711953379574));
#160372=CARTESIAN_POINT('Ctrl Pts',(95.6496986267706,5.83295573741233,143.666018673787));
#160373=CARTESIAN_POINT('Ctrl Pts',(95.6199435544842,5.81592178830307,143.617837479144));
#160374=CARTESIAN_POINT('Ctrl Pts',(95.5916028083606,5.79817958420435,143.572342295301));
#160375=CARTESIAN_POINT('Ctrl Pts',(95.5646757498473,5.78013497109662,143.529466183462));
#160376=CARTESIAN_POINT('Ctrl Pts',(95.5375525157259,5.76195889494971,143.486277700062));
#160377=CARTESIAN_POINT('Ctrl Pts',(95.5118636428781,5.74347602511105,143.44574586582));
#160378=CARTESIAN_POINT('Ctrl Pts',(95.48760855564,5.72505224209099,143.407775112115));
#160379=CARTESIAN_POINT('Ctrl Pts',(95.4626908584376,5.70612515095711,143.368767058502));
#160380=CARTESIAN_POINT('Ctrl Pts',(95.4392863541096,5.68726054276461,143.332461268972));
#160381=CARTESIAN_POINT('Ctrl Pts',(95.4173945017372,5.6688022191041,143.298736076541));
#160382=CARTESIAN_POINT('Ctrl Pts',(95.3971293265148,5.65171544376276,143.267516839247));
#160383=CARTESIAN_POINT('Ctrl Pts',(95.3781603603905,5.63497615912823,143.238508358011));
#160384=CARTESIAN_POINT('Ctrl Pts',(95.3604872361498,5.61881776534264,143.211608081182));
#160385=CARTESIAN_POINT('Ctrl Pts',(95.3423922747224,5.60227368924745,143.184065725627));
#160386=CARTESIAN_POINT('Ctrl Pts',(95.3256557539659,5.5863385644449,143.158733001856));
#160387=CARTESIAN_POINT('Ctrl Pts',(95.3102773408986,5.57122403518025,143.135500486791));
#160388=CARTESIAN_POINT('Ctrl Pts',(95.302588134365,5.56366677054793,143.123884229258));
#160389=CARTESIAN_POINT('Ctrl Pts',(95.2952384556976,5.5563140548991,143.112793074231));
#160390=CARTESIAN_POINT('Ctrl Pts',(95.2882282687808,5.54918884354847,143.102213870378));
#160391=CARTESIAN_POINT('Ctrl Pts',(95.2847231753224,5.54562623787317,143.096924268452));
#160392=CARTESIAN_POINT('Ctrl Pts',(95.2813029548454,5.54212048042549,143.09176267315));
#160393=CARTESIAN_POINT('Ctrl Pts',(95.2779676031805,5.53867422137471,143.086727477895));
#160394=CARTESIAN_POINT('Ctrl Pts',(95.276299927348,5.53695109184932,143.084209880267));
#160395=CARTESIAN_POINT('Ctrl Pts',(95.2746534687213,5.53524283515298,143.081723883828));
#160396=CARTESIAN_POINT('Ctrl Pts',(95.2730282267972,5.53354977110422,143.079269293557));
#160397=CARTESIAN_POINT('Ctrl Pts',(95.2722156058352,5.53270323907984,143.078041998422));
#160398=CARTESIAN_POINT('Ctrl Pts',(95.271408289049,5.5318605051085,143.076822554903));
#160399=CARTESIAN_POINT('Ctrl Pts',(95.270606276377,5.53102160834656,143.075610938833));
#160400=CARTESIAN_POINT('Ctrl Pts',(95.269804263705,5.53018271158462,143.074399322764));
#160401=CARTESIAN_POINT('Ctrl Pts',(95.2696238401053,5.52999491397255,143.074126875397));
#160402=CARTESIAN_POINT('Ctrl Pts',(95.2682161506428,5.52851646836343,143.071999549035));
#160403=CARTESIAN_POINT('Ctrl Pts',(95.2279525004652,5.4862290048292,143.011152375909));
#160404=CARTESIAN_POINT('Ctrl Pts',(95.1893336361188,5.44185914784464,142.953075557469));
#160405=CARTESIAN_POINT('Ctrl Pts',(95.1523589348027,5.39580271620714,142.897819507129));
#160406=CARTESIAN_POINT('Ctrl Pts',(95.1145070697088,5.34865367172546,142.841252598171));
#160407=CARTESIAN_POINT('Ctrl Pts',(95.0783783024679,5.2997374734881,142.787641662398));
#160408=CARTESIAN_POINT('Ctrl Pts',(95.0439719984758,5.24945744839374,142.736990312517));
#160409=CARTESIAN_POINT('Ctrl Pts',(95.0090901976324,5.19848255082424,142.685638958434));
#160410=CARTESIAN_POINT('Ctrl Pts',(94.9759787975812,5.14610618341306,142.637329212914));
#160411=CARTESIAN_POINT('Ctrl Pts',(94.9446371796085,5.09272158028245,142.592018014268));
#160412=CARTESIAN_POINT('Ctrl Pts',(94.9126430019111,5.03822546331901,142.545763397087));
#160413=CARTESIAN_POINT('Ctrl Pts',(94.8824930698343,4.98267899110765,142.502633151469));
#160414=CARTESIAN_POINT('Ctrl Pts',(94.8541867767856,4.92646770024733,142.462538193143));
#160415=CARTESIAN_POINT('Ctrl Pts',(94.8447279887801,4.90768422044484,142.449140122607));
#160416=CARTESIAN_POINT('Ctrl Pts',(94.8354750654485,4.88882621996806,142.436080649246));
#160417=CARTESIAN_POINT('Ctrl Pts',(94.8264279855324,4.86990721043875,142.423355507832));
#160418=CARTESIAN_POINT('Ctrl Pts',(94.7978384827799,4.81012161331499,142.383143033877));
#160419=CARTESIAN_POINT('Ctrl Pts',(94.7713045495697,4.74973024913611,142.346272127812));
#160420=CARTESIAN_POINT('Ctrl Pts',(94.7468255618325,4.68912977215539,142.312581600246));
#160421=CARTESIAN_POINT('Ctrl Pts',(94.7224659380738,4.62882479407817,142.279055353796));
#160422=CARTESIAN_POINT('Ctrl Pts',(94.7001412680888,4.56831272953028,142.248677949744));
#160423=CARTESIAN_POINT('Ctrl Pts',(94.6798510077905,4.50793940352672,142.221257865545));
#160424=CARTESIAN_POINT('Ctrl Pts',(94.6590115065883,4.44593182051244,142.193095541886));
#160425=CARTESIAN_POINT('Ctrl Pts',(94.6403180451523,4.38407075363898,142.168052361701));
#160426=CARTESIAN_POINT('Ctrl Pts',(94.6237701114008,4.32268169250134,142.145894009655));
#160427=CARTESIAN_POINT('Ctrl Pts',(94.6078575973277,4.2636498934888,142.124586510237));
#160428=CARTESIAN_POINT('Ctrl Pts',(94.5939290039647,4.20505415878326,142.105945975219));
#160429=CARTESIAN_POINT('Ctrl Pts',(94.5819839425882,4.14714157564843,142.089747519112));
#160430=CARTESIAN_POINT('Ctrl Pts',(96.3661306018733,5.88291686074446,145.149898346109));
#160431=CARTESIAN_POINT('Ctrl Pts',(96.2336307187006,5.91850508830459,144.999258634303));
#160432=CARTESIAN_POINT('Ctrl Pts',(95.9370400132557,5.95617374018587,144.673941950275));
#160433=CARTESIAN_POINT('Ctrl Pts',(95.472942825783,5.89655306604187,144.203772602427));
#160434=CARTESIAN_POINT('Ctrl Pts',(94.9958612560931,5.71763898647953,143.758389400028));
#160435=CARTESIAN_POINT('Ctrl Pts',(94.555371030275,5.43972288207611,143.375854787691));
#160436=CARTESIAN_POINT('Ctrl Pts',(94.1702186344531,5.07392883860579,143.060374039712));
#160437=CARTESIAN_POINT('Ctrl Pts',(93.8704660552985,4.64012915261243,142.825076373237));
#160438=CARTESIAN_POINT('Ctrl Pts',(93.7286434289597,4.29258168026775,142.716188456363));
#160439=CARTESIAN_POINT('Ctrl Pts',(93.6824704065431,4.12946066360959,142.680822116564));
#160440=CARTESIAN_POINT('Ctrl Pts',(96.9714505281978,6.10328824348366,144.660808028422));
#160441=CARTESIAN_POINT('Ctrl Pts',(96.8257383760717,6.14113800679038,144.494833769542));
#160442=CARTESIAN_POINT('Ctrl Pts',(96.5001479545226,6.18096509138251,144.137379834234));
#160443=CARTESIAN_POINT('Ctrl Pts',(95.9917921991142,6.11788775435994,143.622927634238));
#160444=CARTESIAN_POINT('Ctrl Pts',(95.4689973774376,5.92895072694103,143.1363614066));
#160445=CARTESIAN_POINT('Ctrl Pts',(94.9843959772261,5.63416432191659,142.717469726455));
#160446=CARTESIAN_POINT('Ctrl Pts',(94.5572977666698,5.24224883370102,142.369569651044));
#160447=CARTESIAN_POINT('Ctrl Pts',(94.2209968549404,4.7705309705759,142.107074318414));
#160448=CARTESIAN_POINT('Ctrl Pts',(94.0600652555401,4.38673321527885,141.984161786722));
#160449=CARTESIAN_POINT('Ctrl Pts',(94.0075287315537,4.20564485165057,141.944128106535));
#160450=CARTESIAN_POINT('Ctrl Pts',(97.3637713394669,5.57813458096049,144.187008423291));
#160451=CARTESIAN_POINT('Ctrl Pts',(97.2342536699332,5.61054098777057,144.040464696439));
#160452=CARTESIAN_POINT('Ctrl Pts',(96.9431219835961,5.64514693642928,143.721878689172));
#160453=CARTESIAN_POINT('Ctrl Pts',(96.4855868046259,5.59028826864809,143.257126694955));
#160454=CARTESIAN_POINT('Ctrl Pts',(96.0166230847366,5.42531605607883,142.81601143113));
#160455=CARTESIAN_POINT('Ctrl Pts',(95.5888074887858,5.17092447178584,142.440184895844));
#160456=CARTESIAN_POINT('Ctrl Pts',(95.2229838512101,4.84160297747934,142.136297152508));
#160457=CARTESIAN_POINT('Ctrl Pts',(94.9473498528165,4.46078720565056,141.916704379541));
#160458=CARTESIAN_POINT('Ctrl Pts',(94.8210499420246,4.16391263158191,141.818358906195));
#160459=CARTESIAN_POINT('Ctrl Pts',(94.7802440927429,4.02591020899387,141.786670775179));
#160460=CARTESIAN_POINT('Ctrl Pts',(97.1824258872755,4.79023850550465,144.164071510899));
#160461=CARTESIAN_POINT('Ctrl Pts',(97.0836215903891,4.8145008331457,144.053860578577));
#160462=CARTESIAN_POINT('Ctrl Pts',(96.8587285933397,4.84130595567975,143.809415735873));
#160463=CARTESIAN_POINT('Ctrl Pts',(96.500372920897,4.79878572780782,143.442656766612));
#160464=CARTESIAN_POINT('Ctrl Pts',(96.1352968151614,4.66973483371144,143.091842617071));
#160465=CARTESIAN_POINT('Ctrl Pts',(95.812959853118,4.47586755049402,142.798912924401));
#160466=CARTESIAN_POINT('Ctrl Pts',(95.5553004265918,4.24031177287435,142.575007892362));
#160467=CARTESIAN_POINT('Ctrl Pts',(95.3817764691332,3.99565053281577,142.42897685697));
#160468=CARTESIAN_POINT('Ctrl Pts',(95.3120114122748,3.82896265543311,142.371205203281));
#160469=CARTESIAN_POINT('Ctrl Pts',(95.2902462064996,3.75548982853259,142.353203306798));
#160470=CARTESIAN_POINT('Origin',(96.4108977428719,4.94854001386976,144.785115057418));
#160471=CARTESIAN_POINT('Ctrl Pts',(99.337665144168,2.68440392044039,150.587524550829));
#160472=CARTESIAN_POINT('Ctrl Pts',(99.2089333694121,3.10483363460895,150.220822132441));
#160473=CARTESIAN_POINT('Ctrl Pts',(98.8898355193563,3.90863669901366,149.388392501021));
#160474=CARTESIAN_POINT('Ctrl Pts',(98.2113149059165,4.86229080216582,147.979203699892));
#160475=CARTESIAN_POINT('Ctrl Pts',(97.2929264091547,5.52570727006287,146.495303422543));
#160476=CARTESIAN_POINT('Ctrl Pts',(96.5392326064044,5.77525244071227,145.547689944802));
#160477=CARTESIAN_POINT('Ctrl Pts',(96.1403894431067,5.86040135165679,145.102694169841));
#160478=CARTESIAN_POINT('Ctrl Pts',(100.198533022308,2.94032235979275,150.543534132445));
#160479=CARTESIAN_POINT('Ctrl Pts',(100.063340485816,3.37708324184719,150.14543555162));
#160480=CARTESIAN_POINT('Ctrl Pts',(99.7265888703645,4.21189614517861,149.240770382132));
#160481=CARTESIAN_POINT('Ctrl Pts',(99.003229305022,5.20064103458805,147.707164647165));
#160482=CARTESIAN_POINT('Ctrl Pts',(98.0176374078238,5.88575980160995,146.094117975522));
#160483=CARTESIAN_POINT('Ctrl Pts',(97.2078126465949,6.14188910510591,145.06902836783));
#160484=CARTESIAN_POINT('Ctrl Pts',(96.7800495443887,6.22910329868521,144.589455396234));
#160485=CARTESIAN_POINT('Ctrl Pts',(100.725073827536,2.56916981763826,149.916219881134));
#160486=CARTESIAN_POINT('Ctrl Pts',(100.585641409138,2.98204277130932,149.52870008216));
#160487=CARTESIAN_POINT('Ctrl Pts',(100.240256210392,3.77148792109875,148.647183663979));
#160488=CARTESIAN_POINT('Ctrl Pts',(99.5060453138298,4.70885122818818,147.14616146401));
#160489=CARTESIAN_POINT('Ctrl Pts',(98.5111164333379,5.3621183262696,145.55464168182));
#160490=CARTESIAN_POINT('Ctrl Pts',(97.6933636465612,5.60851073757937,144.532109119388));
#160491=CARTESIAN_POINT('Ctrl Pts',(97.2606142673858,5.69264552708383,144.051133856188));
#160492=CARTESIAN_POINT('Ctrl Pts',(100.366821732785,1.95896330808857,149.361400025247));
#160493=CARTESIAN_POINT('Ctrl Pts',(100.229802846635,2.33270258792801,149.015374490835));
#160494=CARTESIAN_POINT('Ctrl Pts',(99.8938301235163,3.04783157046187,148.228190526516));
#160495=CARTESIAN_POINT('Ctrl Pts',(99.1940999116348,3.90105719122696,146.882688260846));
#160496=CARTESIAN_POINT('Ctrl Pts',(98.2574617032448,4.5022176010466,145.4408636212));
#160497=CARTESIAN_POINT('Ctrl Pts',(97.4882720841481,4.73273141335164,144.498248046442));
#160498=CARTESIAN_POINT('Ctrl Pts',(97.0796829339219,4.81186143846457,144.050511405843));
#160499=CARTESIAN_POINT('',(99.4646532247826,2.77892645244027,150.519323369438));
#160500=CARTESIAN_POINT('Origin',(99.4656911297407,2.11308049683359,149.773231206415));
#160501=CARTESIAN_POINT('Ctrl Pts',(99.4646532213738,2.77892893000186,150.519326147371));
#160502=CARTESIAN_POINT('Ctrl Pts',(99.3239171368583,3.22476130620004,150.121270917057));
#160503=CARTESIAN_POINT('Ctrl Pts',(99.1608443399036,3.6176556021037,149.698516751233));
#160504=CARTESIAN_POINT('Ctrl Pts',(98.882723762233,4.13159959597354,149.048756371723));
#160505=CARTESIAN_POINT('Ctrl Pts',(98.7844315917337,4.29039944274377,148.829524813939));
#160506=CARTESIAN_POINT('Ctrl Pts',(98.628613971959,4.51071461205603,148.499009472181));
#160507=CARTESIAN_POINT('Ctrl Pts',(98.54861031565,4.61640448870926,148.333330753123));
#160508=CARTESIAN_POINT('Ctrl Pts',(98.4516063785492,4.73211758154008,148.139762058688));
#160509=CARTESIAN_POINT('Ctrl Pts',(98.4021877775759,4.78810662569635,148.042962783291));
#160510=CARTESIAN_POINT('Ctrl Pts',(98.3808119507347,4.81170504940579,148.001479921152));
#160511=CARTESIAN_POINT('Ctrl Pts',(98.3665177486058,4.8273495077737,147.973825873703));
#160512=CARTESIAN_POINT('Ctrl Pts',(98.3602561392484,4.83415188671379,147.961743928129));
#160513=CARTESIAN_POINT('Ctrl Pts',(97.8338816271381,5.40033632575454,146.949694082833));
#160514=CARTESIAN_POINT('Ctrl Pts',(97.186303247573,5.74404489420849,145.934192155672));
#160515=CARTESIAN_POINT('Ctrl Pts',(96.4093348705373,5.92994495608164,144.976966788632));
#160516=CARTESIAN_POINT('Ctrl Pts',(99.2551003701486,-2.56421655977614,
150.476238993132));
#160517=CARTESIAN_POINT('Ctrl Pts',(99.3174552930352,-2.37766070250849,
150.64908579837));
#160518=CARTESIAN_POINT('Ctrl Pts',(99.430556511845,-1.94379233761575,150.979414891096));
#160519=CARTESIAN_POINT('Ctrl Pts',(99.544239747873,-1.17789014277733,151.34060331677));
#160520=CARTESIAN_POINT('Ctrl Pts',(99.6007567400978,-0.317978856341414,
151.53240043465));
#160521=CARTESIAN_POINT('Ctrl Pts',(99.598827858709,0.563752712360761,151.530820248987));
#160522=CARTESIAN_POINT('Ctrl Pts',(99.5384938659652,1.42275402103272,151.33594849633));
#160523=CARTESIAN_POINT('Ctrl Pts',(99.4220301598475,2.18186997988765,150.974451180374));
#160524=CARTESIAN_POINT('Ctrl Pts',(99.3083038290003,2.61046752158253,150.64687566607));
#160525=CARTESIAN_POINT('Ctrl Pts',(99.2466552601123,2.79308974077101,150.477682111874));
#160526=CARTESIAN_POINT('Ctrl Pts',(100.138640963592,-2.8682884689841,150.454890705336));
#160527=CARTESIAN_POINT('Ctrl Pts',(100.208694670114,-2.66120055593453,
150.654037028246));
#160528=CARTESIAN_POINT('Ctrl Pts',(100.33547556727,-2.17890690967943,151.035071772476));
#160529=CARTESIAN_POINT('Ctrl Pts',(100.462353777589,-1.32568626788162,
151.452270093545));
#160530=CARTESIAN_POINT('Ctrl Pts',(100.52521100835,-0.366620043423776,
151.673941830286));
#160531=CARTESIAN_POINT('Ctrl Pts',(100.523061572049,0.617123998003932,
151.672105262439));
#160532=CARTESIAN_POINT('Ctrl Pts',(100.455947608549,1.57516724292511,151.446862022936));
#160533=CARTESIAN_POINT('Ctrl Pts',(100.325961028424,2.42080884665813,151.029297046142));
#160534=CARTESIAN_POINT('Ctrl Pts',(100.198485119226,2.89723385429586,150.651438085986));
#160535=CARTESIAN_POINT('Ctrl Pts',(100.129232668393,3.09995683942337,150.456496763744));
#160536=CARTESIAN_POINT('Ctrl Pts',(100.704778319826,-2.48166119443758,
149.81962164672));
#160537=CARTESIAN_POINT('Ctrl Pts',(100.770438131139,-2.30048411696688,
149.999089011321));
#160538=CARTESIAN_POINT('Ctrl Pts',(100.889538473198,-1.87930457518617,
150.341464410159));
#160539=CARTESIAN_POINT('Ctrl Pts',(101.009339216701,-1.13628925491381,
150.714884803515));
#160540=CARTESIAN_POINT('Ctrl Pts',(101.068992594997,-0.30237225732779,
150.912880544087));
#160541=CARTESIAN_POINT('Ctrl Pts',(101.067076707445,0.552612099428047,
150.911234705967));
#160542=CARTESIAN_POINT('Ctrl Pts',(101.003629074577,1.38564136001251,150.710031243453));
#160543=CARTESIAN_POINT('Ctrl Pts',(100.881100700713,2.12206307750808,150.336250397738));
#160544=CARTESIAN_POINT('Ctrl Pts',(100.761453366347,2.53811247991719,149.996699652054));
#160545=CARTESIAN_POINT('Ctrl Pts',(100.696584401853,2.71545984408411,149.821018624374));
#160546=CARTESIAN_POINT('Ctrl Pts',(100.334781367952,-1.82687938005125,
149.264716871263));
#160547=CARTESIAN_POINT('Ctrl Pts',(100.388756689852,-1.68973809771872,
149.40003391948));
#160548=CARTESIAN_POINT('Ctrl Pts',(100.487210316049,-1.37242048959108,
149.656635744138));
#160549=CARTESIAN_POINT('Ctrl Pts',(100.587396109514,-0.81669095021094,
149.934335249489));
#160550=CARTESIAN_POINT('Ctrl Pts',(100.637803032097,-0.195451852887956,
150.080979856501));
#160551=CARTESIAN_POINT('Ctrl Pts',(100.636319551743,0.440722019788662,
150.079763411599));
#160552=CARTESIAN_POINT('Ctrl Pts',(100.582977621096,1.06130906049409,149.930737936671));
#160553=CARTESIAN_POINT('Ctrl Pts',(100.480737465914,1.61213168830484,149.652741371662));
#160554=CARTESIAN_POINT('Ctrl Pts',(100.381941016435,1.92558686572514,149.398223483122));
#160555=CARTESIAN_POINT('Ctrl Pts',(100.32865219777,2.05981521819971,149.265761252093));
#160556=CARTESIAN_POINT('',(99.473036986738,-2.54943487890472,150.517848022843));
#160557=CARTESIAN_POINT('Origin',(99.4719804878147,-1.88317108232132,149.772117288637));
#160558=CARTESIAN_POINT('Ctrl Pts',(99.4730370929753,-2.54942168937959,
150.517834241583));
#160559=CARTESIAN_POINT('Ctrl Pts',(99.4967907636544,-2.45800372718185,
150.599438108881));
#160560=CARTESIAN_POINT('Ctrl Pts',(99.5190422531628,-2.36280845187909,
150.676878686175));
#160561=CARTESIAN_POINT('Ctrl Pts',(99.5397843712218,-2.26429015953294,
150.749807891744));
#160562=CARTESIAN_POINT('Ctrl Pts',(99.5588049325091,-2.17394870008527,
150.816684110471));
#160563=CARTESIAN_POINT('Ctrl Pts',(99.5765561600325,-2.08081184155517,
150.879767029523));
#160564=CARTESIAN_POINT('Ctrl Pts',(99.5930244071844,-1.98519308909147,
150.938780862268));
#160565=CARTESIAN_POINT('Ctrl Pts',(99.6116311293227,-1.87715781721955,
151.005457903125));
#160566=CARTESIAN_POINT('Ctrl Pts',(99.6286004374752,-1.76595472631711,
151.06694195465));
#160567=CARTESIAN_POINT('Ctrl Pts',(99.643952288382,-1.65209645148321,151.123024043958));
#160568=CARTESIAN_POINT('Ctrl Pts',(99.6589673571929,-1.54073594898108,
151.177875829266));
#160569=CARTESIAN_POINT('Ctrl Pts',(99.672435055107,-1.42683458110589,151.227560161432));
#160570=CARTESIAN_POINT('Ctrl Pts',(99.6843608369159,-1.31083708730611,
151.271851020231));
#160571=CARTESIAN_POINT('Ctrl Pts',(99.6886764526795,-1.26886075226889,
151.287878676236));
#160572=CARTESIAN_POINT('Ctrl Pts',(99.6927866424733,-1.22661521653128,
151.303197623039));
#160573=CARTESIAN_POINT('Ctrl Pts',(99.6966927939439,-1.18412164531507,
151.317796448963));
#160574=CARTESIAN_POINT('Ctrl Pts',(99.7082673799082,-1.05820602307792,
151.361055233705));
#160575=CARTESIAN_POINT('Ctrl Pts',(99.7180514421784,-0.930114803646029,
151.397994194935));
#160576=CARTESIAN_POINT('Ctrl Pts',(99.7260629675267,-0.800515119850276,
151.42849131307));
#160577=CARTESIAN_POINT('Ctrl Pts',(99.7342791243167,-0.667605183764806,
151.459767392636));
#160578=CARTESIAN_POINT('Ctrl Pts',(99.7406310504297,-0.533107903563072,
151.484268636455));
#160579=CARTESIAN_POINT('Ctrl Pts',(99.7451235870627,-0.397717906999669,
151.501817647624));
#160580=CARTESIAN_POINT('Ctrl Pts',(99.7459852571904,-0.371750057398373,
151.505183554222));
#160581=CARTESIAN_POINT('Ctrl Pts',(99.7467784829984,-0.345749317034777,
151.50829356699));
#160582=CARTESIAN_POINT('Ctrl Pts',(99.7475032390071,-0.319720526119759,
151.511146234637));
#160583=CARTESIAN_POINT('Ctrl Pts',(99.7513019523685,-0.183294039644338,
151.526098117166));
#160584=CARTESIAN_POINT('Ctrl Pts',(99.7532207755369,-0.0460971937661941,
151.533984298809));
#160585=CARTESIAN_POINT('Ctrl Pts',(99.7532263328386,0.0911428227613257,
151.53483434725));
#160586=CARTESIAN_POINT('Ctrl Pts',(99.7532266541401,0.0990775060141712,
151.53488349374));
#160587=CARTESIAN_POINT('Ctrl Pts',(99.7532205761433,0.107012333705595,
151.534909106638));
#160588=CARTESIAN_POINT('Ctrl Pts',(99.7532080909945,0.114947165176344,
151.534911186577));
#160589=CARTESIAN_POINT('Ctrl Pts',(99.7529922360277,0.252131977130439,
151.534947146512));
#160590=CARTESIAN_POINT('Ctrl Pts',(99.750862512385,0.389312840358846,151.527953067603));
#160591=CARTESIAN_POINT('Ctrl Pts',(99.7468548063207,0.525763867825583,
151.513907100217));
#160592=CARTESIAN_POINT('Ctrl Pts',(99.746460230677,0.539198049657002,151.512524215212));
#160593=CARTESIAN_POINT('Ctrl Pts',(99.7460474402716,0.552625155116682,
151.511072934287));
#160594=CARTESIAN_POINT('Ctrl Pts',(99.7456164621056,0.566044489218804,
151.50955320999));
#160595=CARTESIAN_POINT('Ctrl Pts',(99.7412592908233,0.701713397260867,
151.494188860731));
#160596=CARTESIAN_POINT('Ctrl Pts',(99.7350442956388,0.8365891929933,151.471832748309));
#160597=CARTESIAN_POINT('Ctrl Pts',(99.7269706645698,0.969980999090229,
151.44267400733));
#160598=CARTESIAN_POINT('Ctrl Pts',(99.7190966259891,1.10007515605482,151.414236114952));
#160599=CARTESIAN_POINT('Ctrl Pts',(99.7094546995143,1.22875858640403,151.379327502489));
#160600=CARTESIAN_POINT('Ctrl Pts',(99.6980307644927,1.35536927061228,151.338080916739));
#160601=CARTESIAN_POINT('Ctrl Pts',(99.695791476652,1.38018714336065,151.329995876184));
#160602=CARTESIAN_POINT('Ctrl Pts',(99.6934836773458,1.40492528777928,151.321667186016));
#160603=CARTESIAN_POINT('Ctrl Pts',(99.6911071985347,1.4295785787438,151.313095661014));
#160604=CARTESIAN_POINT('Ctrl Pts',(99.6875196942425,1.46679489506052,151.300156188299));
#160605=CARTESIAN_POINT('Ctrl Pts',(99.6837756845175,1.50381785429284,151.286663340033));
#160606=CARTESIAN_POINT('Ctrl Pts',(99.679874274618,1.5406332263635,151.272624883438));
#160607=CARTESIAN_POINT('Ctrl Pts',(99.6671718234397,1.66049898730303,151.226917609886));
#160608=CARTESIAN_POINT('Ctrl Pts',(99.6528294412209,1.77812313234566,151.175445798303));
#160609=CARTESIAN_POINT('Ctrl Pts',(99.6368427551107,1.89301492572233,151.118461815472));
#160610=CARTESIAN_POINT('Ctrl Pts',(99.6208560690006,2.007906719099,151.061477832642));
#160611=CARTESIAN_POINT('Ctrl Pts',(99.6032251344703,2.12006702692561,150.998981439821));
#160612=CARTESIAN_POINT('Ctrl Pts',(99.5839310026564,2.22896582916987,150.931191398442));
#160613=CARTESIAN_POINT('Ctrl Pts',(99.5654544575536,2.33325005665961,150.866273952601));
#160614=CARTESIAN_POINT('Ctrl Pts',(99.5454524324123,2.43454341641421,150.796500723107));
#160615=CARTESIAN_POINT('Ctrl Pts',(99.5239442995816,2.53243417303878,150.722234507839));
#160616=CARTESIAN_POINT('Ctrl Pts',(99.5053093488977,2.61724811000267,150.657889207859));
#160617=CARTESIAN_POINT('Ctrl Pts',(99.4855436277826,2.69950746674519,150.590170673406));
#160618=CARTESIAN_POINT('Ctrl Pts',(99.4646532434582,2.77891385967415,150.519309253246));
#160619=CARTESIAN_POINT('Ctrl Pts',(96.1095365604538,-5.64870947579686,
145.045115075205));
#160620=CARTESIAN_POINT('Ctrl Pts',(96.5308572053903,-5.56138843522124,
145.511012473416));
#160621=CARTESIAN_POINT('Ctrl Pts',(97.3048934612808,-5.30688486101267,
146.482060103913));
#160622=CARTESIAN_POINT('Ctrl Pts',(98.2343781408756,-4.6269474203888,147.991604985967));
#160623=CARTESIAN_POINT('Ctrl Pts',(98.9053783050068,-3.67234523172437,
149.395383695081));
#160624=CARTESIAN_POINT('Ctrl Pts',(99.219715834908,-2.87142907890009,150.223119336563));
#160625=CARTESIAN_POINT('Ctrl Pts',(99.3457480689541,-2.45535167201243,
150.586091782663));
#160626=CARTESIAN_POINT('Ctrl Pts',(96.7468070029816,-6.0153691110066,144.527455594643));
#160627=CARTESIAN_POINT('Ctrl Pts',(97.1986237871683,-5.92590634547683,
145.029389432178));
#160628=CARTESIAN_POINT('Ctrl Pts',(98.030381371963,-5.66464784836167,146.07975379349));
#160629=CARTESIAN_POINT('Ctrl Pts',(99.0279249426309,-4.96236056855711,
147.720706798807));
#160630=CARTESIAN_POINT('Ctrl Pts',(99.7432909122569,-3.97258298620063,
149.248390941142));
#160631=CARTESIAN_POINT('Ctrl Pts',(100.075045233077,-3.14077141997281,
150.1479213953));
#160632=CARTESIAN_POINT('Ctrl Pts',(100.207417619345,-2.7085365723338,150.541960252375));
#160633=CARTESIAN_POINT('Ctrl Pts',(97.2250643942494,-5.47673623309786,
143.989247026138));
#160634=CARTESIAN_POINT('Ctrl Pts',(97.6822311747899,-5.3903411805755,144.492877723975));
#160635=CARTESIAN_POINT('Ctrl Pts',(98.522147759943,-5.13884423720621,145.540803825402));
#160636=CARTESIAN_POINT('Ctrl Pts',(99.5292924902613,-4.46910785789018,
147.159680949567));
#160637=CARTESIAN_POINT('Ctrl Pts',(100.255659340856,-3.5306784397147,148.654798928096));
#160638=CARTESIAN_POINT('Ctrl Pts',(100.596147424224,-2.74400478658357,
149.531291089658));
#160639=CARTESIAN_POINT('Ctrl Pts',(100.73278812393,-2.33538045653838,149.91485216498));
#160640=CARTESIAN_POINT('Ctrl Pts',(97.0443195895004,-4.59591890240999,
143.993153840071));
#160641=CARTESIAN_POINT('Ctrl Pts',(97.4760971262335,-4.51459389265265,
144.462367854611));
#160642=CARTESIAN_POINT('Ctrl Pts',(98.2660806423517,-4.2791698662904,145.428649758681));
#160643=CARTESIAN_POINT('Ctrl Pts',(99.2143313698502,-3.66285513158594,
146.895045994121));
#160644=CARTESIAN_POINT('Ctrl Pts',(99.9068334220222,-2.80861603887669,
148.235172164511));
#160645=CARTESIAN_POINT('Ctrl Pts',(100.238241619548,-2.0959246702422,149.017878068064));
#160646=CARTESIAN_POINT('Ctrl Pts',(100.372616530784,-1.725995449577,149.360371055165));
#160647=CARTESIAN_POINT('Ctrl Pts',(96.427651149101,-5.7069724840649,144.973748561044));
#160648=CARTESIAN_POINT('Ctrl Pts',(96.8158651387083,-5.61306171775944,
145.452438011694));
#160649=CARTESIAN_POINT('Ctrl Pts',(97.171604962232,-5.48012191275615,145.945011203003));
#160650=CARTESIAN_POINT('Ctrl Pts',(97.6564854549691,-5.21073108191675,
146.692342036475));
#160651=CARTESIAN_POINT('Ctrl Pts',(97.8099907649047,-5.10928297209183,
146.942820946374));
#160652=CARTESIAN_POINT('Ctrl Pts',(98.0280644635696,-4.93837235096895,
147.318647637176));
#160653=CARTESIAN_POINT('Ctrl Pts',(98.134055249843,-4.84823465053843,147.506583806796));
#160654=CARTESIAN_POINT('Ctrl Pts',(98.2523801652375,-4.73463088675781,
147.72541212867));
#160655=CARTESIAN_POINT('Ctrl Pts',(98.3102098271935,-4.67568945239159,
147.834656478391));
#160656=CARTESIAN_POINT('Ctrl Pts',(98.3347083642041,-4.64996734854966,
147.881432356425));
#160657=CARTESIAN_POINT('Ctrl Pts',(98.3509772541781,-4.63271639820428,
147.912605932851));
#160658=CARTESIAN_POINT('Ctrl Pts',(98.3599854147836,-4.62306026553232,
147.929934964988));
#160659=CARTESIAN_POINT('Ctrl Pts',(98.8257446738414,-4.11935561886744,
148.828797248321));
#160660=CARTESIAN_POINT('Ctrl Pts',(99.194390231184,-3.44146052063285,149.721292814617));
#160661=CARTESIAN_POINT('Ctrl Pts',(99.473036986738,-2.54943487890472,150.517848022843));
#160662=CARTESIAN_POINT('Origin',(10.4321358521839,3.97302152633873,143.060605499564));
#160663=CARTESIAN_POINT('',(49.4092281495269,-5.40355622549669,146.366089006391));
#160664=CARTESIAN_POINT('Ctrl Pts',(49.4092280986553,-5.40355634587169,
146.366088876705));
#160665=CARTESIAN_POINT('Ctrl Pts',(49.3491597421002,-5.45696437357856,
146.213866663286));
#160666=CARTESIAN_POINT('Ctrl Pts',(49.290306060662,-5.50657128304731,146.06068333748));
#160667=CARTESIAN_POINT('Ctrl Pts',(49.2328669231528,-5.55235928450432,
145.906764540479));
#160668=CARTESIAN_POINT('Ctrl Pts',(49.1754277856436,-5.59814728596133,
145.752845743478));
#160669=CARTESIAN_POINT('Ctrl Pts',(49.1194032009783,-5.64012204557869,
145.598193572679));
#160670=CARTESIAN_POINT('Ctrl Pts',(49.0648470750591,-5.67835385863493,
145.442664128815));
#160671=CARTESIAN_POINT('Ctrl Pts',(49.0102909491892,-5.71658567165666,
145.28713468509));
#160672=CARTESIAN_POINT('Ctrl Pts',(48.9572032709229,-5.75106745791676,
145.130726057922));
#160673=CARTESIAN_POINT('Ctrl Pts',(48.9057735451051,-5.78174806146419,
144.973734095918));
#160674=CARTESIAN_POINT('',(38.9567113513846,-2.64466323934818,150.517847233856));
#160675=CARTESIAN_POINT('',(10.4426172265712,-2.68952697959015,150.5178394068));
#160676=CARTESIAN_POINT('',(47.1095722443351,-3.69329671363621,149.41195583582));
#160677=CARTESIAN_POINT('Origin',(78.0899422202629,1.83103694728723,145.20567672441));
#160678=CARTESIAN_POINT('Ctrl Pts',(47.1095722444578,-3.69329671364967,
149.411955835804));
#160679=CARTESIAN_POINT('Ctrl Pts',(47.2250608567621,-3.70596734775424,
149.396325837562));
#160680=CARTESIAN_POINT('Ctrl Pts',(47.3379399188308,-3.72201473963128,
149.376504407765));
#160681=CARTESIAN_POINT('Ctrl Pts',(47.4482092787277,-3.7413423142383,149.352413744352));
#160682=CARTESIAN_POINT('Ctrl Pts',(47.497914144081,-3.75005438524646,149.341554669969));
#160683=CARTESIAN_POINT('Ctrl Pts',(47.5470887605488,-3.75943237519231,
149.329827732654));
#160684=CARTESIAN_POINT('Ctrl Pts',(47.5957331098251,-3.76946464813312,
149.317223755553));
#160685=CARTESIAN_POINT('Ctrl Pts',(47.6740135964019,-3.78560899416637,
149.296940917465));
#160686=CARTESIAN_POINT('Ctrl Pts',(47.7509208738446,-3.8034483330406,149.274387246225));
#160687=CARTESIAN_POINT('Ctrl Pts',(47.8264548506386,-3.82292449585361,
149.249517889484));
#160688=CARTESIAN_POINT('Ctrl Pts',(47.8642218390356,-3.83266257726011,
149.237083211113));
#160689=CARTESIAN_POINT('Ctrl Pts',(47.9016455019917,-3.84280968744087,
149.224069472177));
#160690=CARTESIAN_POINT('Ctrl Pts',(47.9387258262457,-3.85335739730775,
149.210470352909));
#160691=CARTESIAN_POINT('Ctrl Pts',(47.9572659883727,-3.8586312522412,149.203670793275));
#160692=CARTESIAN_POINT('Ctrl Pts',(47.9757203158068,-3.86400524608101,
149.196724879813));
#160693=CARTESIAN_POINT('Ctrl Pts',(47.9940888067782,-3.86947825385059,
149.189631776819));
#160694=CARTESIAN_POINT('Ctrl Pts',(48.0032730522639,-3.87221475773538,
149.186085225322));
#160695=CARTESIAN_POINT('Ctrl Pts',(48.0124358386328,-3.87497601440758,
149.182501875903));
#160696=CARTESIAN_POINT('Ctrl Pts',(48.0215771656565,-3.87776187865116,
149.178881621419));
#160697=CARTESIAN_POINT('Ctrl Pts',(48.0307184926802,-3.88054774289474,
149.175261366934));
#160698=CARTESIAN_POINT('Ctrl Pts',(48.0384895838107,-3.88293795566613,
149.172151843211));
#160699=CARTESIAN_POINT('Ctrl Pts',(48.0489367684588,-3.88619314595116,
149.167910033663));
#160700=CARTESIAN_POINT('Ctrl Pts',(48.1325142456436,-3.91223466823139,
149.13397555728));
#160701=CARTESIAN_POINT('Ctrl Pts',(48.2105006971708,-3.93849865056287,
149.099313094295));
#160702=CARTESIAN_POINT('Ctrl Pts',(48.2828960847917,-3.96496078184916,
149.063908828405));
#160703=CARTESIAN_POINT('Ctrl Pts',(48.3190937786021,-3.97819184749231,
149.046206695461));
#160704=CARTESIAN_POINT('Ctrl Pts',(48.3538937064191,-3.99147243962569,
149.028319103758));
#160705=CARTESIAN_POINT('Ctrl Pts',(48.3872958632832,-4.00479940600968,
149.010244344515));
#160706=CARTESIAN_POINT('Ctrl Pts',(48.4039969417152,-4.01146288920168,
149.001206964894));
#160707=CARTESIAN_POINT('Ctrl Pts',(48.420348577408,-4.01813796530156,148.992122792891));
#160708=CARTESIAN_POINT('Ctrl Pts',(48.4363507697328,-4.02482423463313,
148.982991614239));
#160709=CARTESIAN_POINT('Ctrl Pts',(48.4523529620575,-4.0315105039647,148.973860435586));
#160710=CARTESIAN_POINT('Ctrl Pts',(48.4665509922826,-4.03757028624714,
148.965559208935));
#160711=CARTESIAN_POINT('Ctrl Pts',(48.4833090159683,-4.04491621910288,
148.955456843318));
#160712=CARTESIAN_POINT('Ctrl Pts',(48.5503411107113,-4.07429995052582,
148.915047380851));
#160713=CARTESIAN_POINT('Ctrl Pts',(48.6170655970785,-4.10661450778534,
148.869993246045));
#160714=CARTESIAN_POINT('Ctrl Pts',(48.6834821181227,-4.14163300915733,
148.820141215516));
#160715=CARTESIAN_POINT('Ctrl Pts',(48.7166903786448,-4.15914225984333,
148.795215200252));
#160716=CARTESIAN_POINT('Ctrl Pts',(48.7498216466353,-4.1773267332877,148.769089329175));
#160717=CARTESIAN_POINT('Ctrl Pts',(48.7828758700986,-4.19615338042924,
148.741742335125));
#160718=CARTESIAN_POINT('Ctrl Pts',(48.7994029818303,-4.20556670400001,
148.7280688381));
#160719=CARTESIAN_POINT('Ctrl Pts',(48.815910832362,-4.21514052762869,148.714090030498));
#160720=CARTESIAN_POINT('Ctrl Pts',(48.8323994147077,-4.22487041093803,
148.699803147087));
#160721=CARTESIAN_POINT('Ctrl Pts',(48.8406437058805,-4.2297353525927,148.692659705382));
#160722=CARTESIAN_POINT('Ctrl Pts',(48.8488831800026,-4.23463930647713,
148.685439242854));
#160723=CARTESIAN_POINT('Ctrl Pts',(48.8571178361721,-4.23958169931045,
148.678141405679));
#160724=CARTESIAN_POINT('Ctrl Pts',(48.8653524923415,-4.24452409214377,
148.670843568505));
#160725=CARTESIAN_POINT('Ctrl Pts',(48.8726808850653,-4.24895488646809,
148.66428518402));
#160726=CARTESIAN_POINT('Ctrl Pts',(48.8818073499018,-4.25452360954717,
148.656015410472));
#160727=CARTESIAN_POINT('Ctrl Pts',(48.954819068594,-4.29907339417987,148.589857222094));
#160728=CARTESIAN_POINT('Ctrl Pts',(49.0211326158252,-4.34298379382797,
148.52295350218));
#160729=CARTESIAN_POINT('Ctrl Pts',(49.080747947528,-4.3862268024775,148.455313496479));
#160730=CARTESIAN_POINT('Ctrl Pts',(49.1105556133794,-4.40784830680226,
148.421493493629));
#160731=CARTESIAN_POINT('Ctrl Pts',(49.1386887253575,-4.42930296893276,
148.387489422859));
#160732=CARTESIAN_POINT('Ctrl Pts',(49.165147277924,-4.45058726912027,148.353302546057));
#160733=CARTESIAN_POINT('Ctrl Pts',(49.1783765542072,-4.46122941921402,
148.336209107656));
#160734=CARTESIAN_POINT('Ctrl Pts',(49.1911871906381,-4.47182897919932,
148.319069967993));
#160735=CARTESIAN_POINT('Ctrl Pts',(49.2035791865256,-4.482385509894,148.301885288595));
#160736=CARTESIAN_POINT('Ctrl Pts',(49.2097751844694,-4.48766377524133,
148.293292948896));
#160737=CARTESIAN_POINT('Ctrl Pts',(49.2158665222773,-4.49293128328941,
148.284689224277));
#160738=CARTESIAN_POINT('Ctrl Pts',(49.221853199863,-4.49818797909476,148.276074135321));
#160739=CARTESIAN_POINT('Ctrl Pts',(49.2278398774487,-4.5034446749001,148.267459046365));
#160740=CARTESIAN_POINT('Ctrl Pts',(49.2329204522465,-4.50796435012504,
148.260030839577));
#160741=CARTESIAN_POINT('Ctrl Pts',(49.239499251867,-4.5139255748782,148.25019479617));
#160742=CARTESIAN_POINT('Ctrl Pts',(49.2921296488308,-4.56161537290345,
148.17150644892));
#160743=CARTESIAN_POINT('Ctrl Pts',(49.3390031528632,-4.61090243896194,
148.087760156192));
#160744=CARTESIAN_POINT('Ctrl Pts',(49.380119120392,-4.66137771917959,147.998763592685));
#160745=CARTESIAN_POINT('Ctrl Pts',(49.4006771041563,-4.68661535928841,
147.954265310931));
#160746=CARTESIAN_POINT('Ctrl Pts',(49.4197957024886,-4.71214922277214,
147.908454436313));
#160747=CARTESIAN_POINT('Ctrl Pts',(49.4374748269396,-4.73792309186303,
147.861307082455));
#160748=CARTESIAN_POINT('Ctrl Pts',(49.4463143891651,-4.75081002640847,
147.837733405526));
#160749=CARTESIAN_POINT('Ctrl Pts',(49.4547940828577,-4.76375692252418,
147.813825587123));
#160750=CARTESIAN_POINT('Ctrl Pts',(49.4629138964232,-4.77675641113063,
147.78958070489));
#160751=CARTESIAN_POINT('Ctrl Pts',(49.4669738032059,-4.78325615543385,
147.777458263774));
#160752=CARTESIAN_POINT('Ctrl Pts',(49.4709437399531,-4.78976904542875,
147.765251555352));
#160753=CARTESIAN_POINT('Ctrl Pts',(49.4748237051864,-4.79629414152205,
147.752960213411));
#160754=CARTESIAN_POINT('Ctrl Pts',(49.4784039650958,-4.80231521092417,
147.741618307971));
#160755=CARTESIAN_POINT('Ctrl Pts',(49.4815970221161,-4.80779628353553,
147.731249998675));
#160756=CARTESIAN_POINT('Ctrl Pts',(49.4852626826503,-4.81426031384824,
147.718960370922));
#160757=CARTESIAN_POINT('Ctrl Pts',(49.4855695369027,-4.81480142101586,
147.717931600118));
#160758=CARTESIAN_POINT('Ctrl Pts',(49.4858797028569,-4.81534938937098,
147.716889351646));
#160759=CARTESIAN_POINT('Ctrl Pts',(49.486193684848,-4.81590509673314,147.715831919202));
#160760=CARTESIAN_POINT('Ctrl Pts',(49.5512303180725,-4.93101149428575,
147.496800739188));
#160761=CARTESIAN_POINT('Ctrl Pts',(49.577334938451,-5.03759764333394,147.274340771407));
#160762=CARTESIAN_POINT('Ctrl Pts',(49.5645073883648,-5.13556346529849,
147.049151818323));
#160763=CARTESIAN_POINT('Ctrl Pts',(49.5516798382786,-5.23352928726304,
146.823962865239));
#160764=CARTESIAN_POINT('Ctrl Pts',(49.4999201179697,-5.32287493596084,
146.59604521302));
#160765=CARTESIAN_POINT('Ctrl Pts',(49.409228157871,-5.40355629319227,146.366089026851));
#160766=CARTESIAN_POINT('Ctrl Pts',(46.6241051349778,-7.32511472728899,
147.989854517212));
#160767=CARTESIAN_POINT('Ctrl Pts',(46.5537157353721,-7.41755726094091,
147.775546153899));
#160768=CARTESIAN_POINT('Ctrl Pts',(46.4047646446039,-7.60394202424138,
147.307357450064));
#160769=CARTESIAN_POINT('Ctrl Pts',(46.2105242916428,-7.8201965195852,146.648322053017));
#160770=CARTESIAN_POINT('Ctrl Pts',(46.0890577707829,-7.939124533019,146.203240389833));
#160771=CARTESIAN_POINT('Ctrl Pts',(46.0413559492253,-7.98304327208021,
146.022524042131));
#160772=CARTESIAN_POINT('Ctrl Pts',(46.9398378390672,-5.94714561945616,
147.399100431922));
#160773=CARTESIAN_POINT('Ctrl Pts',(46.8697497468136,-6.02854475709611,
147.210712584582));
#160774=CARTESIAN_POINT('Ctrl Pts',(46.7215167708399,-6.1926836074711,146.799123352895));
#160775=CARTESIAN_POINT('Ctrl Pts',(46.5284183447193,-6.38318097309383,
146.219681184828));
#160776=CARTESIAN_POINT('Ctrl Pts',(46.4077662646162,-6.48797605067776,
145.828311551126));
#160777=CARTESIAN_POINT('Ctrl Pts',(46.3603984301429,-6.52668138904934,
145.669397775977));
#160778=CARTESIAN_POINT('Ctrl Pts',(48.1092317625503,-5.18444440048026,
146.768005238018));
#160779=CARTESIAN_POINT('Ctrl Pts',(48.0402970656098,-5.25307065169244,
146.597191040467));
#160780=CARTESIAN_POINT('Ctrl Pts',(47.8947955416849,-5.39066904764671,
146.225153440396));
#160781=CARTESIAN_POINT('Ctrl Pts',(47.7059995187861,-5.54827456352389,
145.704630860055));
#160782=CARTESIAN_POINT('Ctrl Pts',(47.5883979384804,-5.63374760400384,
145.354785493422));
#160783=CARTESIAN_POINT('Ctrl Pts',(47.5422785802052,-5.66509900665306,
145.212986568709));
#160784=CARTESIAN_POINT('Ctrl Pts',(49.5798793716172,-5.39730189362096,
146.394690665637));
#160785=CARTESIAN_POINT('Ctrl Pts',(49.5124053079744,-5.45745952492184,
146.224801672306));
#160786=CARTESIAN_POINT('Ctrl Pts',(49.3703582684564,-5.57676031435096,
145.856584151351));
#160787=CARTESIAN_POINT('Ctrl Pts',(49.1869927219503,-5.70987697211657,
145.346474617428));
#160788=CARTESIAN_POINT('Ctrl Pts',(49.0732366813086,-5.7799663706731,145.006350194313));
#160789=CARTESIAN_POINT('Ctrl Pts',(49.0286905233209,-5.80529721278276,
144.868893549847));
#160790=CARTESIAN_POINT('Origin',(49.4136832107095,-8.23492065935952,147.357731263197));
#160791=CARTESIAN_POINT('Ctrl Pts',(45.9818308006136,-4.36386233890014,
139.457590298979));
#160792=CARTESIAN_POINT('Ctrl Pts',(46.0577929151188,-3.88656671250596,
139.336024689025));
#160793=CARTESIAN_POINT('Ctrl Pts',(46.1911667285702,-2.88574456343811,
139.125038002339));
#160794=CARTESIAN_POINT('Ctrl Pts',(46.3079233121362,-1.38770401599913,
138.941983369662));
#160795=CARTESIAN_POINT('Ctrl Pts',(46.3305159825606,-0.371913621033629,
138.9052711071));
#160796=CARTESIAN_POINT('Ctrl Pts',(46.3283370115851,0.114046639445121,
138.907567120453));
#160797=CARTESIAN_POINT('Ctrl Pts',(46.1843239563542,-3.94379274885482,
141.045963619328));
#160798=CARTESIAN_POINT('Ctrl Pts',(46.2608245032563,-3.51190343660015,
140.936336715849));
#160799=CARTESIAN_POINT('Ctrl Pts',(46.3952244407994,-2.60648107776861,
140.746127006659));
#160800=CARTESIAN_POINT('Ctrl Pts',(46.513041603105,-1.25166766168089,140.581163907621));
#160801=CARTESIAN_POINT('Ctrl Pts',(46.5359620147019,-0.333143630120858,
140.548086533492));
#160802=CARTESIAN_POINT('Ctrl Pts',(46.5338464962686,0.106283523993099,
140.550155751043));
#160803=CARTESIAN_POINT('Ctrl Pts',(47.4378078356412,-3.8343211672685,142.121689142346));
#160804=CARTESIAN_POINT('Ctrl Pts',(47.5172130409551,-3.41696992847953,
142.010153939069));
#160805=CARTESIAN_POINT('Ctrl Pts',(47.6570624441036,-2.53923231521643,
141.815778143772));
#160806=CARTESIAN_POINT('Ctrl Pts',(47.7800889888078,-1.21952845390115,
141.646213777249));
#160807=CARTESIAN_POINT('Ctrl Pts',(47.8041216550563,-0.322730017030245,
141.612114186466));
#160808=CARTESIAN_POINT('Ctrl Pts',(47.8019622839384,0.106274688630286,
141.614239265262));
#160809=CARTESIAN_POINT('Ctrl Pts',(49.072697213247,-4.09392505430371,142.110136489086));
#160810=CARTESIAN_POINT('Ctrl Pts',(49.1558216943686,-3.65247770942299,
141.983865354168));
#160811=CARTESIAN_POINT('Ctrl Pts',(49.3026329125726,-2.71992117719697,
141.762605846383));
#160812=CARTESIAN_POINT('Ctrl Pts',(49.432234898711,-1.3084544943288,141.568205313321));
#160813=CARTESIAN_POINT('Ctrl Pts',(49.4575701896293,-0.346235519011063,
141.528972447798));
#160814=CARTESIAN_POINT('Ctrl Pts',(49.4552830858161,0.114024853025236,
141.531406204995));
#160815=CARTESIAN_POINT('Origin',(49.3053670001028,0.0391433951441804,138.53495912845));
#160816=CARTESIAN_POINT('Ctrl Pts',(46.3285875541939,-0.0453398318882474,
138.90752266128));
#160817=CARTESIAN_POINT('Ctrl Pts',(46.3292442208751,0.445985702815633,
138.90547547437));
#160818=CARTESIAN_POINT('Ctrl Pts',(46.3027202641352,1.47862733617782,138.943836932465));
#160819=CARTESIAN_POINT('Ctrl Pts',(46.1794352511173,2.97588016689551,139.130537365369));
#160820=CARTESIAN_POINT('Ctrl Pts',(46.0427961861896,3.9705349119133,139.342385458527));
#160821=CARTESIAN_POINT('Ctrl Pts',(45.9679913898148,4.43115774305712,139.460032410545));
#160822=CARTESIAN_POINT('Ctrl Pts',(46.5340727615371,-0.0378409420050605,
140.550116857512));
#160823=CARTESIAN_POINT('Ctrl Pts',(46.5348132498481,0.406438148398626,
140.548272721693));
#160824=CARTESIAN_POINT('Ctrl Pts',(46.5082651455313,1.34019173849624,140.582837843699));
#160825=CARTESIAN_POINT('Ctrl Pts',(46.3843580200113,2.69426001015636,140.751089543413));
#160826=CARTESIAN_POINT('Ctrl Pts',(46.2469931540946,3.5940664573222,140.942079807452));
#160827=CARTESIAN_POINT('Ctrl Pts',(46.1718065030185,4.01084563788002,141.048173637582));
#160828=CARTESIAN_POINT('Ctrl Pts',(47.8021843455376,-0.0344318706058168,
141.614201840284));
#160829=CARTESIAN_POINT('Ctrl Pts',(47.8030018749016,0.399310045394509,
141.612295274549));
#160830=CARTESIAN_POINT('Ctrl Pts',(47.7753793534869,1.31097231063154,141.647900621391));
#160831=CARTESIAN_POINT('Ctrl Pts',(47.6462983109395,2.62983125453292,141.820797693363));
#160832=CARTESIAN_POINT('Ctrl Pts',(47.5035770892202,3.50199158089965,142.015910523487));
#160833=CARTESIAN_POINT('Ctrl Pts',(47.4256304130497,3.90472204054626,142.123839733063));
#160834=CARTESIAN_POINT('Ctrl Pts',(49.4555224071342,-0.0369336755933763,
141.531364648942));
#160835=CARTESIAN_POINT('Ctrl Pts',(49.4563690431696,0.428409084164662,
141.529163521016));
#160836=CARTESIAN_POINT('Ctrl Pts',(49.4271957672958,1.40657748778552,141.570089986329));
#160837=CARTESIAN_POINT('Ctrl Pts',(49.2911528064204,2.81701045540398,141.768245070864));
#160838=CARTESIAN_POINT('Ctrl Pts',(49.1413059324474,3.74349484399151,141.990258669654));
#160839=CARTESIAN_POINT('Ctrl Pts',(49.0596954111229,4.16947605872563,142.112431337084));
#160840=CARTESIAN_POINT('Ctrl Pts',(46.0161346091238,8.04686257481308,146.026975529383));
#160841=CARTESIAN_POINT('Ctrl Pts',(46.0701379205231,7.99734211175707,146.230946628465));
#160842=CARTESIAN_POINT('Ctrl Pts',(46.1955438597492,7.87416261053135,146.687012632762));
#160843=CARTESIAN_POINT('Ctrl Pts',(46.3910983490287,7.65552025469006,147.34440254582));
#160844=CARTESIAN_POINT('Ctrl Pts',(46.5338233533296,7.47738131305873,147.790445316799));
#160845=CARTESIAN_POINT('Ctrl Pts',(46.6009706655345,7.38965660591495,147.993991853346));
#160846=CARTESIAN_POINT('Ctrl Pts',(46.339758162072,6.59170813014846,145.673040991343));
#160847=CARTESIAN_POINT('Ctrl Pts',(46.3933659254992,6.54808517167697,145.852403893947));
#160848=CARTESIAN_POINT('Ctrl Pts',(46.5178920837304,6.43959031579536,146.253430150673));
#160849=CARTESIAN_POINT('Ctrl Pts',(46.7122329313617,6.24706378925182,146.831420218524));
#160850=CARTESIAN_POINT('Ctrl Pts',(46.8542094315672,6.09023923413186,147.223539299679));
#160851=CARTESIAN_POINT('Ctrl Pts',(46.9210374701065,6.01301872846379,147.402466891096));
#160852=CARTESIAN_POINT('Ctrl Pts',(47.5243433476267,5.73410275588817,145.216152331719));
#160853=CARTESIAN_POINT('Ctrl Pts',(47.5765156814216,5.69878741311937,145.376200040928));
#160854=CARTESIAN_POINT('Ctrl Pts',(47.6978558665834,5.61027001230812,145.73476648539));
#160855=CARTESIAN_POINT('Ctrl Pts',(47.8878268680074,5.450892217511,146.254207184608));
#160856=CARTESIAN_POINT('Ctrl Pts',(48.0271307214227,5.31943503759318,146.608705840733));
#160857=CARTESIAN_POINT('Ctrl Pts',(48.0928248514571,5.25435476791681,146.770945110899));
#160858=CARTESIAN_POINT('Ctrl Pts',(49.0103064657029,5.87916884795805,144.872138221871));
#160859=CARTESIAN_POINT('Ctrl Pts',(49.0606815677909,5.85064681493126,145.027288004096));
#160860=CARTESIAN_POINT('Ctrl Pts',(49.1780346028805,5.77796257100624,145.376032072945));
#160861=CARTESIAN_POINT('Ctrl Pts',(49.3625438159987,5.64310735085286,145.885431893024));
#160862=CARTESIAN_POINT('Ctrl Pts',(49.4985134059075,5.52908729390024,146.236384822334));
#160863=CARTESIAN_POINT('Ctrl Pts',(49.5627946372691,5.47204839422951,146.397749756044));
#160864=CARTESIAN_POINT('',(49.3921071370737,5.47779704596669,146.36910776447));
#160865=CARTESIAN_POINT('Origin',(49.3876377743159,8.30858703474018,147.362326448108));
#160866=CARTESIAN_POINT('Ctrl Pts',(48.887434025587,5.85518895743199,144.97688956023));
#160867=CARTESIAN_POINT('Ctrl Pts',(48.9306897550823,5.82949635711896,145.108669038189));
#160868=CARTESIAN_POINT('Ctrl Pts',(48.9751043926647,5.80114206631471,145.239976811865));
#160869=CARTESIAN_POINT('Ctrl Pts',(49.0205765812721,5.77014957205661,145.370681194462));
#160870=CARTESIAN_POINT('Ctrl Pts',(49.0293081778864,5.76419837493542,145.395779127496));
#160871=CARTESIAN_POINT('Ctrl Pts',(49.0380787584918,5.75814991559219,145.420854810407));
#160872=CARTESIAN_POINT('Ctrl Pts',(49.0468875752625,5.75200433966445,145.445907535824));
#160873=CARTESIAN_POINT('Ctrl Pts',(49.101570725823,5.71385398843274,145.601429212747));
#160874=CARTESIAN_POINT('Ctrl Pts',(49.1577283395669,5.67196688856135,145.75606162316));
#160875=CARTESIAN_POINT('Ctrl Pts',(49.2153072140572,5.62627621912166,145.909943315272));
#160876=CARTESIAN_POINT('Ctrl Pts',(49.219843822728,5.62267627575719,145.922067571345));
#160877=CARTESIAN_POINT('Ctrl Pts',(49.2243892370016,5.61905269833621,145.93418714346));
#160878=CARTESIAN_POINT('Ctrl Pts',(49.2289433747957,5.61540548943111,145.946301935296));
#160879=CARTESIAN_POINT('Ctrl Pts',(49.2821898449036,5.57276273053368,146.087946727469));
#160880=CARTESIAN_POINT('Ctrl Pts',(49.3366294769991,5.52688881483523,146.228938194885));
#160881=CARTESIAN_POINT('Ctrl Pts',(49.3921048021131,5.47779893615921,146.369101802441));
#160882=CARTESIAN_POINT('Origin',(10.4447115478058,-4.01955337529683,143.058388065124));
#160883=CARTESIAN_POINT('',(47.0978472346802,3.75861943712466,149.414023271397));
#160884=CARTESIAN_POINT('Ctrl Pts',(49.3921071370737,5.47779704596669,146.36910776447));
#160885=CARTESIAN_POINT('Ctrl Pts',(49.4361507302258,5.43880070204039,146.48045098635));
#160886=CARTESIAN_POINT('Ctrl Pts',(49.4706982859556,5.39657329383826,146.594657875756));
#160887=CARTESIAN_POINT('Ctrl Pts',(49.4957503680475,5.35075653442217,146.711508385595));
#160888=CARTESIAN_POINT('Ctrl Pts',(49.5082764090935,5.32784815471413,146.769933640515));
#160889=CARTESIAN_POINT('Ctrl Pts',(49.5184285820122,5.30404225791503,146.829019263037));
#160890=CARTESIAN_POINT('Ctrl Pts',(49.5262069586772,5.27929316857397,146.888734263028));
#160891=CARTESIAN_POINT('Ctrl Pts',(49.5300961470098,5.26691862390344,146.918591763023));
#160892=CARTESIAN_POINT('Ctrl Pts',(49.5333918863107,5.25430826082335,146.948606598876));
#160893=CARTESIAN_POINT('Ctrl Pts',(49.5360941856033,5.24145634520237,146.978774621788));
#160894=CARTESIAN_POINT('Ctrl Pts',(49.5379370818315,5.23269168064885,146.999348410852));
#160895=CARTESIAN_POINT('Ctrl Pts',(49.5395474500292,5.22343650687812,147.020869714439));
#160896=CARTESIAN_POINT('Ctrl Pts',(49.5408363523507,5.21446088356659,147.041543643582));
#160897=CARTESIAN_POINT('Ctrl Pts',(49.5414374098535,5.21027525549866,147.051184576037));
#160898=CARTESIAN_POINT('Ctrl Pts',(49.5419685582334,5.20615113024434,147.060641537434));
#160899=CARTESIAN_POINT('Ctrl Pts',(49.5424207725859,5.20217013861614,147.069734049073));
#160900=CARTESIAN_POINT('Ctrl Pts',(49.5481085276126,5.15209896104572,147.184095697475));
#160901=CARTESIAN_POINT('Ctrl Pts',(49.5452460076019,5.10122031784624,147.294445737981));
#160902=CARTESIAN_POINT('Ctrl Pts',(49.5338326352621,5.04990109989827,147.400864052974));
#160903=CARTESIAN_POINT('Ctrl Pts',(49.5281259490923,5.02424149092427,147.454073210471));
#160904=CARTESIAN_POINT('Ctrl Pts',(49.5202815505016,4.99847131783018,147.506299708939));
#160905=CARTESIAN_POINT('Ctrl Pts',(49.5102993713006,4.97263391743248,147.557555018204));
#160906=CARTESIAN_POINT('Ctrl Pts',(49.5053082817001,4.95971521723364,147.583182672837));
#160907=CARTESIAN_POINT('Ctrl Pts',(49.4997827469708,4.9467796950444,147.608567522475));
#160908=CARTESIAN_POINT('Ctrl Pts',(49.4937227588561,4.93383259825042,147.633711106031));
#160909=CARTESIAN_POINT('Ctrl Pts',(49.4906927647988,4.92735904985344,147.646282897809));
#160910=CARTESIAN_POINT('Ctrl Pts',(49.4875291573966,4.9208826068105,147.658794372571));
#160911=CARTESIAN_POINT('Ctrl Pts',(49.4842319356302,4.91440391703237,147.671245723755));
#160912=CARTESIAN_POINT('Ctrl Pts',(49.4811025386957,4.90825498518383,147.683063315347));
#160913=CARTESIAN_POINT('Ctrl Pts',(49.4775545266859,4.90156201404105,147.695858784716));
#160914=CARTESIAN_POINT('Ctrl Pts',(49.4744371246675,4.89586880492085,147.70669375997));
#160915=CARTESIAN_POINT('Ctrl Pts',(49.4742699431049,4.895563486713,147.707274823331));
#160916=CARTESIAN_POINT('Ctrl Pts',(49.474103999966,4.89526105462038,147.707850253944));
#160917=CARTESIAN_POINT('Ctrl Pts',(49.4739394262268,4.89496175022421,147.70841960043));
#160918=CARTESIAN_POINT('Ctrl Pts',(49.448072640778,4.84791874909003,147.797906316196));
#160919=CARTESIAN_POINT('Ctrl Pts',(49.4139503782418,4.79914848496446,147.887360904827));
#160920=CARTESIAN_POINT('Ctrl Pts',(49.3715727001156,4.7486118832405,147.976707891572));
#160921=CARTESIAN_POINT('Ctrl Pts',(49.3503838610525,4.72334358237852,148.021381384944));
#160922=CARTESIAN_POINT('Ctrl Pts',(49.3271311680859,4.69763370090939,148.066027980018));
#160923=CARTESIAN_POINT('Ctrl Pts',(49.3018146284735,4.67147762747258,148.11063783537));
#160924=CARTESIAN_POINT('Ctrl Pts',(49.2891563586674,4.65839959075418,148.132942763046));
#160925=CARTESIAN_POINT('Ctrl Pts',(49.2759821271991,4.64521000649151,148.155238506045));
#160926=CARTESIAN_POINT('Ctrl Pts',(49.2622919349606,4.63190830800298,148.177523823348));
#160927=CARTESIAN_POINT('Ctrl Pts',(49.2554468388413,4.62525745875873,148.188666481999));
#160928=CARTESIAN_POINT('Ctrl Pts',(49.2484727525294,4.61857858098203,148.199806534241));
#160929=CARTESIAN_POINT('Ctrl Pts',(49.2413696761348,4.61187160489373,148.210943823517));
#160930=CARTESIAN_POINT('Ctrl Pts',(49.2346321898464,4.60550983192086,148.221507884724));
#160931=CARTESIAN_POINT('Ctrl Pts',(49.227059866239,4.59846277627678,148.233156671138));
#160932=CARTESIAN_POINT('Ctrl Pts',(49.2206980704094,4.59260844559814,148.242796270887));
#160933=CARTESIAN_POINT('Ctrl Pts',(49.2203528660537,4.59229077736359,148.243319335743));
#160934=CARTESIAN_POINT('Ctrl Pts',(49.2200112259285,4.59197663175015,148.243836491342));
#160935=CARTESIAN_POINT('Ctrl Pts',(49.2196734768118,4.59166631229651,148.244347245497));
#160936=CARTESIAN_POINT('Ctrl Pts',(49.1671762623241,4.54343256092357,148.323735078496));
#160937=CARTESIAN_POINT('Ctrl Pts',(49.1119271759838,4.49707551576149,148.397537522733));
#160938=CARTESIAN_POINT('Ctrl Pts',(49.0539255915381,4.45299316675182,148.465968084059));
#160939=CARTESIAN_POINT('Ctrl Pts',(49.0249247993152,4.43095199224698,148.500183364723));
#160940=CARTESIAN_POINT('Ctrl Pts',(48.9952358841048,4.40947851381734,148.53305551054));
#160941=CARTESIAN_POINT('Ctrl Pts',(48.9648587766526,4.38861674296047,148.564609948554));
#160942=CARTESIAN_POINT('Ctrl Pts',(48.9496702229265,4.37818585753203,148.580387167561));
#160943=CARTESIAN_POINT('Ctrl Pts',(48.9343096212152,4.36790785115326,148.595834927884));
#160944=CARTESIAN_POINT('Ctrl Pts',(48.918776963434,4.35778786171874,148.610956331161));
#160945=CARTESIAN_POINT('Ctrl Pts',(48.9049524615912,4.348780786783,148.62441480494));
#160946=CARTESIAN_POINT('Ctrl Pts',(48.8900288329631,4.3393055695298,148.638492995324));
#160947=CARTESIAN_POINT('Ctrl Pts',(48.8765769164015,4.33094975518149,148.650847922563));
#160948=CARTESIAN_POINT('Ctrl Pts',(48.8749147971136,4.32991731046401,148.652374497812));
#160949=CARTESIAN_POINT('Ctrl Pts',(48.8732751464897,4.32890201005717,148.653874800516));
#160950=CARTESIAN_POINT('Ctrl Pts',(48.8716628140952,4.32790689195046,148.655344440179));
#160951=CARTESIAN_POINT('Ctrl Pts',(48.7928437216884,4.27926040548347,148.727187978661));
#160952=CARTESIAN_POINT('Ctrl Pts',(48.7091012997476,4.23260602872896,148.794063467525));
#160953=CARTESIAN_POINT('Ctrl Pts',(48.6204350301956,4.18827300205104,148.856169581348));
#160954=CARTESIAN_POINT('Ctrl Pts',(48.5312371012076,4.14367414630336,148.918648094975));
#160955=CARTESIAN_POINT('Ctrl Pts',(48.4370560991793,4.10142442556188,148.976300218093));
#160956=CARTESIAN_POINT('Ctrl Pts',(48.3378915759401,4.06180865192953,149.029313001505));
#160957=CARTESIAN_POINT('Ctrl Pts',(48.3155991775574,4.05290294070131,149.041230389383));
#160958=CARTESIAN_POINT('Ctrl Pts',(48.2930549322134,4.04413014298943,149.052913251231));
#160959=CARTESIAN_POINT('Ctrl Pts',(48.2702588353468,4.03549315764655,149.064363580206));
#160960=CARTESIAN_POINT('Ctrl Pts',(48.2327585047276,4.02128503211499,149.08319974873));
#160961=CARTESIAN_POINT('Ctrl Pts',(48.1945766302123,4.00744447862358,149.101406673959));
#160962=CARTESIAN_POINT('Ctrl Pts',(48.1557131926094,3.99398369318984,149.118992912761));
#160963=CARTESIAN_POINT('Ctrl Pts',(48.136281473808,3.98725330047297,149.127786032162));
#160964=CARTESIAN_POINT('Ctrl Pts',(48.1166793642531,3.98061783810165,149.136423971038));
#160965=CARTESIAN_POINT('Ctrl Pts',(48.0969068616784,3.97407874625011,149.144907764067));
#160966=CARTESIAN_POINT('Ctrl Pts',(48.0771343591037,3.96753965439857,149.153391557096));
#160967=CARTESIAN_POINT('Ctrl Pts',(48.0552578353902,3.96048695014219,149.162507265567));
#160968=CARTESIAN_POINT('Ctrl Pts',(48.037078172702,3.95475197591698,149.169897704169));
#160969=CARTESIAN_POINT('Ctrl Pts',(47.9369529244939,3.92316636689794,149.210600852084));
#160970=CARTESIAN_POINT('Ctrl Pts',(47.8341972039513,3.89454764491787,149.246814174914));
#160971=CARTESIAN_POINT('Ctrl Pts',(47.7288107311118,3.86907372372077,149.278671429963));
#160972=CARTESIAN_POINT('Ctrl Pts',(47.6233303443575,3.84357710173865,149.310557074231));
#160973=CARTESIAN_POINT('Ctrl Pts',(47.5152145146778,3.82123076803661,149.33807905775));
#160974=CARTESIAN_POINT('Ctrl Pts',(47.4044630302007,3.80216936475247,149.361342960505));
#160975=CARTESIAN_POINT('Ctrl Pts',(47.3044088952034,3.78494907893479,149.382359831546));
#160976=CARTESIAN_POINT('Ctrl Pts',(47.2022036665947,3.77040919993785,149.399901165777));
#160977=CARTESIAN_POINT('Ctrl Pts',(47.0978472346802,3.75861943712466,149.414023271397));
#160978=CARTESIAN_POINT('',(38.9483300367407,2.68372196522192,150.519324999229));
#160979=CARTESIAN_POINT('Origin',(84.8264838120473,-2.60418696047202,144.299062259712));
#160980=CARTESIAN_POINT('',(10.4342334294899,2.6388562881557,150.519317696389));
#160981=CARTESIAN_POINT('Origin',(10.4384246768163,-0.0245075772277829,
147.534945843904));
#160982=CARTESIAN_POINT('Ctrl Pts',(38.9483300382364,2.68372101404257,150.519323933408));
#160983=CARTESIAN_POINT('Ctrl Pts',(38.6027432695898,2.64416611286694,150.554139247846));
#160984=CARTESIAN_POINT('Ctrl Pts',(38.266183212812,2.604090445613,150.588057906848));
#160985=CARTESIAN_POINT('Ctrl Pts',(37.9386436491546,2.56353408926601,150.621074225556));
#160986=CARTESIAN_POINT('Ctrl Pts',(37.8962911845616,2.55828995439867,150.625343396747));
#160987=CARTESIAN_POINT('Ctrl Pts',(37.8540895096113,2.55303784646761,150.629597485271));
#160988=CARTESIAN_POINT('Ctrl Pts',(37.8120385840336,2.54777790769498,150.633836482566));
#160989=CARTESIAN_POINT('Ctrl Pts',(37.5010385754246,2.50887648088693,150.665187235899));
#160990=CARTESIAN_POINT('Ctrl Pts',(37.1982862600139,2.46954281254957,150.695712266618));
#160991=CARTESIAN_POINT('Ctrl Pts',(36.9037811468005,2.42981074257045,150.725406929677));
#160992=CARTESIAN_POINT('Ctrl Pts',(36.8511029967784,2.42270386445818,150.730718416117));
#160993=CARTESIAN_POINT('Ctrl Pts',(36.7986886496763,2.4155843587941,150.73600334356));
#160994=CARTESIAN_POINT('Ctrl Pts',(36.7465380234107,2.4084525704991,150.741261695967));
#160995=CARTESIAN_POINT('Ctrl Pts',(36.4676886727713,2.37031890505036,150.769378101448));
#160996=CARTESIAN_POINT('Ctrl Pts',(36.1963813298171,2.33183026043562,150.796734448863));
#160997=CARTESIAN_POINT('Ctrl Pts',(35.9326187900983,2.29301640643672,150.823327121199));
#160998=CARTESIAN_POINT('Ctrl Pts',(35.8789578999625,2.28511996307746,150.828737239217));
#160999=CARTESIAN_POINT('Ctrl Pts',(35.8256092008524,2.27721021023271,150.834115759836));
#161000=CARTESIAN_POINT('Ctrl Pts',(35.7725725908774,2.2692876224765,150.839462668646));
#161001=CARTESIAN_POINT('Ctrl Pts',(35.5236784004087,2.23210790705111,150.864555044279));
#161002=CARTESIAN_POINT('Ctrl Pts',(35.2816596094678,2.19464180178193,150.888950959313));
#161003=CARTESIAN_POINT('Ctrl Pts',(35.0465224406967,2.15691561437506,150.912647574482));
#161004=CARTESIAN_POINT('Ctrl Pts',(34.9908865278496,2.14798920395007,150.918254441415));
#161005=CARTESIAN_POINT('Ctrl Pts',(34.9356357602717,2.13904843085661,150.923822172934));
#161006=CARTESIAN_POINT('Ctrl Pts',(34.8807700058312,2.13009399901494,150.929350757835));
#161007=CARTESIAN_POINT('Ctrl Pts',(34.7750750055704,2.11284391860519,150.940001186112));
#161008=CARTESIAN_POINT('Ctrl Pts',(34.6708089477046,2.09554298275572,150.950506323685));
#161009=CARTESIAN_POINT('Ctrl Pts',(34.5679736963875,2.07819246308016,150.960865825684));
#161010=CARTESIAN_POINT('Ctrl Pts',(34.3952114943478,2.04904376215035,150.978269686271));
#161011=CARTESIAN_POINT('Ctrl Pts',(34.2264863600537,2.01975324056144,150.995263064868));
#161012=CARTESIAN_POINT('Ctrl Pts',(34.0617918219847,1.99033795250279,151.011847298683));
#161013=CARTESIAN_POINT('Ctrl Pts',(33.8659875723369,1.95536631061334,151.031564184842));
#161014=CARTESIAN_POINT('Ctrl Pts',(33.6758817556065,1.92021657413703,151.050702627247));
#161015=CARTESIAN_POINT('Ctrl Pts',(33.4914778686697,1.88490334935071,151.069263352936));
#161016=CARTESIAN_POINT('Ctrl Pts',(33.4296932287429,1.87307163086409,151.075482135916));
#161017=CARTESIAN_POINT('Ctrl Pts',(33.3685484270922,1.86122192142731,151.081636090093));
#161018=CARTESIAN_POINT('Ctrl Pts',(33.3080428602635,1.84935581311173,151.087725315099));
#161019=CARTESIAN_POINT('Ctrl Pts',(33.151858337036,1.81872553284213,151.103443582925));
#161020=CARTESIAN_POINT('Ctrl Pts',(32.9999349343395,1.78798371775716,151.118730371713));
#161021=CARTESIAN_POINT('Ctrl Pts',(32.8522803581535,1.75713880684416,151.133585536884));
#161022=CARTESIAN_POINT('Ctrl Pts',(32.7725113616133,1.74047513372642,151.1416109002));
#161023=CARTESIAN_POINT('Ctrl Pts',(32.6939882630894,1.7237810339304,151.149510752151));
#161024=CARTESIAN_POINT('Ctrl Pts',(32.6167083927223,1.70706086971309,151.157285460588));
#161025=CARTESIAN_POINT('Ctrl Pts',(32.4691175929587,1.6751283315594,151.172133770124));
#161026=CARTESIAN_POINT('Ctrl Pts',(32.326063748158,1.64309795647864,151.186525396057));
#161027=CARTESIAN_POINT('Ctrl Pts',(32.1875518770369,1.61097868776279,151.20046042161));
#161028=CARTESIAN_POINT('Ctrl Pts',(32.1625711175385,1.60518594436424,151.202973617909));
#161029=CARTESIAN_POINT('Ctrl Pts',(32.1377380044198,1.59939041388421,151.20547197116));
#161030=CARTESIAN_POINT('Ctrl Pts',(32.1130524542536,1.59359228214992,151.207955492803));
#161031=CARTESIAN_POINT('Ctrl Pts',(32.0701298266207,1.58351063326134,151.212273779167));
#161032=CARTESIAN_POINT('Ctrl Pts',(32.027654141952,1.5734204157536,151.216547519342));
#161033=CARTESIAN_POINT('Ctrl Pts',(31.9856243973538,1.56332289564894,151.220776766451));
#161034=CARTESIAN_POINT('Ctrl Pts',(31.9134652058033,1.54598686626355,151.228037792069));
#161035=CARTESIAN_POINT('Ctrl Pts',(31.8426207416885,1.52862903156681,151.235167641275));
#161036=CARTESIAN_POINT('Ctrl Pts',(31.7730929017198,1.51124959459354,151.242165893124));
#161037=CARTESIAN_POINT('Ctrl Pts',(31.7180804361685,1.49749847449226,151.247703115177));
#161038=CARTESIAN_POINT('Ctrl Pts',(31.6638916996835,1.48373423685283,151.253157836866));
#161039=CARTESIAN_POINT('Ctrl Pts',(31.6105266905512,1.4699579771998,151.258530350681));
#161040=CARTESIAN_POINT('Ctrl Pts',(31.583844185985,1.46306984737328,151.261216607589));
#161041=CARTESIAN_POINT('Ctrl Pts',(31.5573676132506,1.45617871594911,151.263882322376));
#161042=CARTESIAN_POINT('Ctrl Pts',(31.5310969721014,1.4492847387293,151.266527586375));
#161043=CARTESIAN_POINT('Ctrl Pts',(31.5179616515267,1.4458377501194,151.267850218375));
#161044=CARTESIAN_POINT('Ctrl Pts',(31.5048778138481,1.44239005024169,151.269167738205));
#161045=CARTESIAN_POINT('Ctrl Pts',(31.491845459033,1.43894165948415,151.270480160329));
#161046=CARTESIAN_POINT('Ctrl Pts',(31.478813104218,1.43549326872661,151.271792582453));
#161047=CARTESIAN_POINT('Ctrl Pts',(31.4671055638423,1.43238393073357,151.272971657411));
#161048=CARTESIAN_POINT('Ctrl Pts',(31.4529028431458,1.4285944355183,151.274402149949));
#161049=CARTESIAN_POINT('Ctrl Pts',(31.439419072415,1.42499676675048,151.275760230125));
#161050=CARTESIAN_POINT('Ctrl Pts',(31.4259888429677,1.42139781441521,151.277112993081));
#161051=CARTESIAN_POINT('Ctrl Pts',(31.4126120387662,1.41779762190945,151.278460446859));
#161052=CARTESIAN_POINT('Ctrl Pts',(31.3021595831912,1.38807078306107,151.28958639117));
#161053=CARTESIAN_POINT('Ctrl Pts',(31.1953530398958,1.35825622082807,151.300349992595));
#161054=CARTESIAN_POINT('Ctrl Pts',(31.0921689282748,1.32834578422234,151.310751710281));
#161055=CARTESIAN_POINT('Ctrl Pts',(31.0250589479275,1.30889231622949,151.3175168901));
#161056=CARTESIAN_POINT('Ctrl Pts',(30.9594803861762,1.28939911894315,151.324129086344));
#161057=CARTESIAN_POINT('Ctrl Pts',(30.8954181725188,1.26987173470207,151.330589355687));
#161058=CARTESIAN_POINT('Ctrl Pts',(30.8033863044817,1.24181866648935,151.339870187893));
#161059=CARTESIAN_POINT('Ctrl Pts',(30.7144866277601,1.21369299570105,151.348837186809));
#161060=CARTESIAN_POINT('Ctrl Pts',(30.6287161567598,1.18548510478732,151.357489458271));
#161061=CARTESIAN_POINT('Ctrl Pts',(30.5609497064191,1.16319831288184,151.364325537372));
#161062=CARTESIAN_POINT('Ctrl Pts',(30.495135598263,1.14086103694648,151.37096525925));
#161063=CARTESIAN_POINT('Ctrl Pts',(30.4312544687237,1.11848251767363,151.377410080749));
#161064=CARTESIAN_POINT('Ctrl Pts',(30.3562068564538,1.09219221176209,151.384981463229));
#161065=CARTESIAN_POINT('Ctrl Pts',(30.2838295069765,1.06584353282845,151.39228360202));
#161066=CARTESIAN_POINT('Ctrl Pts',(30.2141395724523,1.03942730195697,151.399314111018));
#161067=CARTESIAN_POINT('Ctrl Pts',(30.1460731455833,1.01362646774687,151.406180836174));
#161068=CARTESIAN_POINT('Ctrl Pts',(30.0805696770538,0.987761702529661,
151.412788511418));
#161069=CARTESIAN_POINT('Ctrl Pts',(30.0176051661593,0.961850531843709,
151.419139091241));
#161070=CARTESIAN_POINT('Ctrl Pts',(29.9598133948294,0.938068048189028,
151.424967950255));
#161071=CARTESIAN_POINT('Ctrl Pts',(29.9041620617812,0.914245962732354,
151.43058007034));
#161072=CARTESIAN_POINT('Ctrl Pts',(29.8506854606712,0.890378792179376,
151.435971744736));
#161073=CARTESIAN_POINT('Ctrl Pts',(29.7942287314613,0.865181559054073,
151.441663884757));
#161074=CARTESIAN_POINT('Ctrl Pts',(29.7401956613144,0.839934242751313,
151.447110345417));
#161075=CARTESIAN_POINT('Ctrl Pts',(29.6885754213258,0.814656693484691,
151.452312044106));
#161076=CARTESIAN_POINT('Ctrl Pts',(29.6775138468789,0.809240029534481,
151.453426703342));
#161077=CARTESIAN_POINT('Ctrl Pts',(29.6665628971776,0.803822062990689,
151.454530140923));
#161078=CARTESIAN_POINT('Ctrl Pts',(29.6557221979594,0.798403122736736,
151.45562239356));
#161079=CARTESIAN_POINT('Ctrl Pts',(29.6113559591719,0.776225771216936,
151.460092505708));
#161080=CARTESIAN_POINT('Ctrl Pts',(29.5688406215529,0.754030554791447,
151.464374841223));
#161081=CARTESIAN_POINT('Ctrl Pts',(29.5282257151081,0.731821673711811,
151.46846439376));
#161082=CARTESIAN_POINT('Ctrl Pts',(29.4993439715204,0.716028673927752,
151.471372523265));
#161083=CARTESIAN_POINT('Ctrl Pts',(29.4714220361072,0.700229209359056,
151.474183288859));
#161084=CARTESIAN_POINT('Ctrl Pts',(29.444462864748,0.684430100848601,151.476896405429));
#161085=CARTESIAN_POINT('Ctrl Pts',(29.4120388866724,0.66542840598453,151.480159489113));
#161086=CARTESIAN_POINT('Ctrl Pts',(29.381008471491,0.646424010729459,151.483281922171));
#161087=CARTESIAN_POINT('Ctrl Pts',(29.3513265884524,0.627415074671382,
151.486268046272));
#161088=CARTESIAN_POINT('Ctrl Pts',(29.3173570323049,0.605660217680324,
151.489685528586));
#161089=CARTESIAN_POINT('Ctrl Pts',(29.2851569519863,0.583899258394271,
151.492924153563));
#161090=CARTESIAN_POINT('Ctrl Pts',(29.2547537739581,0.562122696882355,
151.495980991589));
#161091=CARTESIAN_POINT('Ctrl Pts',(29.2208105338232,0.537810532672966,
151.499393759396));
#161092=CARTESIAN_POINT('Ctrl Pts',(29.1891065944066,0.513479201977103,
151.502579983994));
#161093=CARTESIAN_POINT('Ctrl Pts',(29.1596123629576,0.489119825777804,
151.505542526122));
#161094=CARTESIAN_POINT('Ctrl Pts',(29.1424940405993,0.474981750847837,
151.507261972558));
#161095=CARTESIAN_POINT('Ctrl Pts',(29.1261188929719,0.460834281051649,
151.508906190981));
#161096=CARTESIAN_POINT('Ctrl Pts',(29.1104734441162,0.446675643663467,
151.510476529098));
#161097=CARTESIAN_POINT('Ctrl Pts',(29.0866568282643,0.425122358054861,
151.512867009551));
#161098=CARTESIAN_POINT('Ctrl Pts',(29.0645346973072,0.403544304906276,
151.515085931265));
#161099=CARTESIAN_POINT('Ctrl Pts',(29.0441608765425,0.381969017990187,
151.517127919829));
#161100=CARTESIAN_POINT('Ctrl Pts',(29.0215281089998,0.358001571771817,
151.519396313815));
#161101=CARTESIAN_POINT('Ctrl Pts',(29.0010521035118,0.334037774725908,
151.521446442291));
#161102=CARTESIAN_POINT('Ctrl Pts',(28.9827472026584,0.310095949764079,
151.523276883032));
#161103=CARTESIAN_POINT('Ctrl Pts',(28.9815204766048,0.308491458120782,
151.523399552331));
#161104=CARTESIAN_POINT('Ctrl Pts',(28.9803034841381,0.306887057857641,
151.523521236678));
#161105=CARTESIAN_POINT('Ctrl Pts',(28.9790962226575,0.305282751370811,
151.523641936329));
#161106=CARTESIAN_POINT('Ctrl Pts',(28.9672218773354,0.2895031629932,151.524829110244));
#161107=CARTESIAN_POINT('Ctrl Pts',(28.9562872886384,0.273736664172069,
151.525920784737));
#161108=CARTESIAN_POINT('Ctrl Pts',(28.9462822664861,0.257961851789511,
151.526918758088));
#161109=CARTESIAN_POINT('Ctrl Pts',(28.9312208536328,0.234214681782191,
151.52842109246));
#161110=CARTESIAN_POINT('Ctrl Pts',(28.9182635854512,0.210451660595227,
151.52971135097));
#161111=CARTESIAN_POINT('Ctrl Pts',(28.907399609783,0.186702762534852,151.530792636163));
#161112=CARTESIAN_POINT('Ctrl Pts',(28.8972468659891,0.164508633538344,
151.53180313286));
#161113=CARTESIAN_POINT('Ctrl Pts',(28.8889215340135,0.142325550128787,
151.532631170926));
#161114=CARTESIAN_POINT('Ctrl Pts',(28.882455295068,0.120150967013752,151.533274861738));
#161115=CARTESIAN_POINT('Ctrl Pts',(28.8820023145399,0.118597567200818,
151.533319954319));
#161116=CARTESIAN_POINT('Ctrl Pts',(28.8815584774549,0.117044201652551,
151.533364140163));
#161117=CARTESIAN_POINT('Ctrl Pts',(28.8811238041125,0.115490866386377,
151.533407417661));
#161118=CARTESIAN_POINT('Ctrl Pts',(28.8771341750942,0.101233651028576,
151.533804638168));
#161119=CARTESIAN_POINT('Ctrl Pts',(28.8738776244795,0.0869157802293588,
151.53412704013));
#161120=CARTESIAN_POINT('Ctrl Pts',(28.871403161365,0.0725743470340143,
151.534370489789));
#161121=CARTESIAN_POINT('Ctrl Pts',(28.8671330035289,0.0478254700020986,
151.534790608588));
#161122=CARTESIAN_POINT('Ctrl Pts',(28.8651944694018,0.0230063130007055,
151.534975330761));
#161123=CARTESIAN_POINT('Ctrl Pts',(28.8655113019717,-0.00161249851495384,
151.534936134653));
#161124=CARTESIAN_POINT('Ctrl Pts',(28.8658249293817,-0.0259822597976901,
151.534897335062));
#161125=CARTESIAN_POINT('Ctrl Pts',(28.8683484094705,-0.0501548456514469,
151.534639070795));
#161126=CARTESIAN_POINT('Ctrl Pts',(28.8729577422789,-0.0738687071900575,
151.534178059856));
#161127=CARTESIAN_POINT('Ctrl Pts',(28.8749169270865,-0.0839482217723661,
151.533982108367));
#161128=CARTESIAN_POINT('Ctrl Pts',(28.8772876173455,-0.0940506262770279,
151.533747584978));
#161129=CARTESIAN_POINT('Ctrl Pts',(28.8800798808754,-0.104168181396869,
151.533473267271));
#161130=CARTESIAN_POINT('Ctrl Pts',(28.8872124503321,-0.130012505849106,
151.532772548992));
#161131=CARTESIAN_POINT('Ctrl Pts',(28.8970928942548,-0.155956749588127,
151.531812409961));
#161132=CARTESIAN_POINT('Ctrl Pts',(28.9096719124097,-0.181976415511025,
151.53059540908));
#161133=CARTESIAN_POINT('Ctrl Pts',(28.9226734556467,-0.208870073453178,
151.529337529541));
#161134=CARTESIAN_POINT('Ctrl Pts',(28.9385601618265,-0.235846111339722,
151.527805178816));
#161135=CARTESIAN_POINT('Ctrl Pts',(28.9573154776245,-0.262844139658197,
151.525996998897));
#161136=CARTESIAN_POINT('Ctrl Pts',(28.9612710740981,-0.26853816831437,
151.525615644076));
#161137=CARTESIAN_POINT('Ctrl Pts',(28.9653543226671,-0.274233000755657,
151.525222008365));
#161138=CARTESIAN_POINT('Ctrl Pts',(28.9695651013876,-0.279927757494856,
151.524816062986));
#161139=CARTESIAN_POINT('Ctrl Pts',(28.990216475843,-0.307857164776068,
151.52282514145));
#161140=CARTESIAN_POINT('Ctrl Pts',(29.0139372600631,-0.335786096141674,
151.520538260894));
#161141=CARTESIAN_POINT('Ctrl Pts',(29.0407751906054,-0.363792963429348,
151.517943728282));
#161142=CARTESIAN_POINT('Ctrl Pts',(29.0625868467577,-0.386554634945706,
151.515835106192));
#161143=CARTESIAN_POINT('Ctrl Pts',(29.0864588872605,-0.409367699882497,
151.513523097419));
#161144=CARTESIAN_POINT('Ctrl Pts',(29.1123853322711,-0.432261641585833,
151.511002129416));
#161145=CARTESIAN_POINT('Ctrl Pts',(29.1183598179163,-0.437537317676879,
151.510421197971));
#161146=CARTESIAN_POINT('Ctrl Pts',(29.1244431952512,-0.442817229452095,
151.509829179544));
#161147=CARTESIAN_POINT('Ctrl Pts',(29.1306349724997,-0.448101625097921,
151.509226027365));
#161148=CARTESIAN_POINT('Ctrl Pts',(29.1337229685925,-0.45073708701009,
151.508925220102));
#161149=CARTESIAN_POINT('Ctrl Pts',(29.1368377473778,-0.453373191351228,
151.508621698255));
#161150=CARTESIAN_POINT('Ctrl Pts',(29.1399791681834,-0.456009862426074,
151.508315472268));
#161151=CARTESIAN_POINT('Ctrl Pts',(29.1672013400079,-0.478858094956928,
151.505661852472));
#161152=CARTESIAN_POINT('Ctrl Pts',(29.1964280103261,-0.501748584700058,
151.502804832625));
#161153=CARTESIAN_POINT('Ctrl Pts',(29.2277046042288,-0.524673176442512,
151.499737506279));
#161154=CARTESIAN_POINT('Ctrl Pts',(29.2563950096037,-0.545702187216171,
151.496923809986));
#161155=CARTESIAN_POINT('Ctrl Pts',(29.2868105924331,-0.566759770075305,
151.493933117712));
#161156=CARTESIAN_POINT('Ctrl Pts',(29.3189434761364,-0.587843653853886,
151.490763942473));
#161157=CARTESIAN_POINT('Ctrl Pts',(29.3386384193971,-0.600766424762658,
151.488821486044));
#161158=CARTESIAN_POINT('Ctrl Pts',(29.3589776579053,-0.613699159231986,
151.486812054609));
#161159=CARTESIAN_POINT('Ctrl Pts',(29.3799496193799,-0.626642513105162,
151.484736204012));
#161160=CARTESIAN_POINT('Ctrl Pts',(29.3862074017992,-0.630504655061366,
151.484116795026));
#161161=CARTESIAN_POINT('Ctrl Pts',(29.3925214591309,-0.634367750309721,
151.483491477977));
#161162=CARTESIAN_POINT('Ctrl Pts',(29.3988921040743,-0.638231764678178,
151.482860205853));
#161163=CARTESIAN_POINT('Ctrl Pts',(29.4373542694222,-0.661560385385414,
151.479048960207));
#161164=CARTESIAN_POINT('Ctrl Pts',(29.4778950245336,-0.684920994007202,
151.475020427045));
#161165=CARTESIAN_POINT('Ctrl Pts',(29.5205233412297,-0.708305371768688,
151.470767695467));
#161166=CARTESIAN_POINT('Ctrl Pts',(29.5360317789473,-0.716812748887632,
151.469220526169));
#161167=CARTESIAN_POINT('Ctrl Pts',(29.5518160652932,-0.725323430418557,
151.467643717436));
#161168=CARTESIAN_POINT('Ctrl Pts',(29.5678749735161,-0.733837605108871,
151.466037065843));
#161169=CARTESIAN_POINT('Ctrl Pts',(29.5979751299764,-0.749796223637019,
151.463025624238));
#161170=CARTESIAN_POINT('Ctrl Pts',(29.6290434575462,-0.765765969075537,
151.459909415387));
#161171=CARTESIAN_POINT('Ctrl Pts',(29.6610799505251,-0.781745744866384,
151.456689214732));
#161172=CARTESIAN_POINT('Ctrl Pts',(29.6694450062028,-0.785918227612744,
151.455848387436));
#161173=CARTESIAN_POINT('Ctrl Pts',(29.6778762175432,-0.790091360891029,
151.455000490086));
#161174=CARTESIAN_POINT('Ctrl Pts',(29.6863732835912,-0.794265205577799,
151.454145548124));
#161175=CARTESIAN_POINT('Ctrl Pts',(29.6941472507123,-0.798083856766365,
151.453363361582));
#161176=CARTESIAN_POINT('Ctrl Pts',(29.7019763378513,-0.801903104352659,
151.452575278723));
#161177=CARTESIAN_POINT('Ctrl Pts',(29.7098608132034,-0.805722856972097,
151.451781269757));
#161178=CARTESIAN_POINT('Ctrl Pts',(29.7206924334612,-0.810970398248478,
151.450690467489));
#161179=CARTESIAN_POINT('Ctrl Pts',(29.7323703843149,-0.816574297045414,
151.449513602825));
#161180=CARTESIAN_POINT('Ctrl Pts',(29.743435278034,-0.821833182059346,
151.448397796475));
#161181=CARTESIAN_POINT('Ctrl Pts',(29.7492281126836,-0.824586380788653,
151.447813635267));
#161182=CARTESIAN_POINT('Ctrl Pts',(29.7548521918546,-0.827245655506408,
151.447246286198));
#161183=CARTESIAN_POINT('Ctrl Pts',(29.7600939225384,-0.829714105783301,
151.446717305305));
#161184=CARTESIAN_POINT('Ctrl Pts',(29.8143646576473,-0.855271430107522,
151.441240453552));
#161185=CARTESIAN_POINT('Ctrl Pts',(29.8707617826373,-0.880693965368612,
151.435527365135));
#161186=CARTESIAN_POINT('Ctrl Pts',(29.9292810232518,-0.905979619620407,
151.429581190326));
#161187=CARTESIAN_POINT('Ctrl Pts',(29.9694586888553,-0.923340039038501,
151.425498713852));
#161188=CARTESIAN_POINT('Ctrl Pts',(30.0106358156893,-0.940636223409451,
151.421306488752));
#161189=CARTESIAN_POINT('Ctrl Pts',(30.052797859214,-0.957873000490626,
151.417007349118));
#161190=CARTESIAN_POINT('Ctrl Pts',(30.1206046968499,-0.985593937314419,
151.410093285217));
#161191=CARTESIAN_POINT('Ctrl Pts',(30.1909599125678,-1.0131606071397,151.402902463072));
#161192=CARTESIAN_POINT('Ctrl Pts',(30.2638971683645,-1.04055242161206,
151.395439389664));
#161193=CARTESIAN_POINT('Ctrl Pts',(30.3293256421008,-1.06512428950344,
151.388744628569));
#161194=CARTESIAN_POINT('Ctrl Pts',(30.3968316209166,-1.08955541881358,
151.381830849012));
#161195=CARTESIAN_POINT('Ctrl Pts',(30.4664085226188,-1.11384839667623,
151.3747062175));
#161196=CARTESIAN_POINT('Ctrl Pts',(30.5166960397161,-1.13140642972634,
151.369556806988));
#161197=CARTESIAN_POINT('Ctrl Pts',(30.5680643958423,-1.14889286986701,
151.364297384591));
#161198=CARTESIAN_POINT('Ctrl Pts',(30.6205264720779,-1.16630003090646,
151.3589300352));
#161199=CARTESIAN_POINT('Ctrl Pts',(30.702058863791,-1.19335285790684,151.350588527115));
#161200=CARTESIAN_POINT('Ctrl Pts',(30.7863430129809,-1.22025950416132,
151.341971502953));
#161201=CARTESIAN_POINT('Ctrl Pts',(30.8732745922089,-1.24698870044844,
151.333095615084));
#161202=CARTESIAN_POINT('Ctrl Pts',(30.8865931759859,-1.25108381804783,
151.331735761078));
#161203=CARTESIAN_POINT('Ctrl Pts',(30.8999738278721,-1.25517483667929,
151.330369840169));
#161204=CARTESIAN_POINT('Ctrl Pts',(30.9134160915004,-1.25926171694156,
151.328997922409));
#161205=CARTESIAN_POINT('Ctrl Pts',(31.0091841405266,-1.28837828243565,
151.319223832948));
#161206=CARTESIAN_POINT('Ctrl Pts',(31.1080822474525,-1.31728187204803,
151.309144968042));
#161207=CARTESIAN_POINT('Ctrl Pts',(31.2100003455261,-1.34592513978652,
151.29878187842));
#161208=CARTESIAN_POINT('Ctrl Pts',(31.2667389223497,-1.36187106379585,
151.293012667968));
#161209=CARTESIAN_POINT('Ctrl Pts',(31.3244128435392,-1.37773694793607,
151.287155455917));
#161210=CARTESIAN_POINT('Ctrl Pts',(31.3829982596841,-1.39351968941024,
151.281214450372));
#161211=CARTESIAN_POINT('Ctrl Pts',(31.4976982021994,-1.42441952180784,
151.269583006246));
#161212=CARTESIAN_POINT('Ctrl Pts',(31.6158937177216,-1.45499843725536,
151.257630094014));
#161213=CARTESIAN_POINT('Ctrl Pts',(31.7374418502422,-1.4852127666234,151.245384988212));
#161214=CARTESIAN_POINT('Ctrl Pts',(31.7826800930041,-1.49645804977578,
151.240827558513));
#161215=CARTESIAN_POINT('Ctrl Pts',(31.8284876727297,-1.50769531262186,
151.236212699029));
#161216=CARTESIAN_POINT('Ctrl Pts',(31.8748630728464,-1.51892424780116,
151.23154056007));
#161217=CARTESIAN_POINT('Ctrl Pts',(32.0044790319385,-1.55030832641151,
151.218482262553));
#161218=CARTESIAN_POINT('Ctrl Pts',(32.1385327792507,-1.58162478851494,
151.204976297435));
#161219=CARTESIAN_POINT('Ctrl Pts',(32.2770208022029,-1.61284339901664,
151.191022982071));
#161220=CARTESIAN_POINT('Ctrl Pts',(32.3247593551313,-1.62360484436055,
151.186213099817));
#161221=CARTESIAN_POINT('Ctrl Pts',(32.3730245291577,-1.63435499617135,
151.181350089714));
#161222=CARTESIAN_POINT('Ctrl Pts',(32.4218152223614,-1.64509372619346,
151.17643406181));
#161223=CARTESIAN_POINT('Ctrl Pts',(32.5709422999114,-1.67791628557194,
151.161408391414));
#161224=CARTESIAN_POINT('Ctrl Pts',(32.7249809288133,-1.71062936617794,
151.145887210082));
#161225=CARTESIAN_POINT('Ctrl Pts',(32.8839286591928,-1.7432042703979,151.129870758828));
#161226=CARTESIAN_POINT('Ctrl Pts',(32.9304179121803,-1.75273182363638,
151.125186244916));
#161227=CARTESIAN_POINT('Ctrl Pts',(32.9773269097341,-1.76224781831153,
151.12045938391));
#161228=CARTESIAN_POINT('Ctrl Pts',(33.024655057861,-1.77175221467368,151.115690235925));
#161229=CARTESIAN_POINT('Ctrl Pts',(33.1946925415478,-1.80589899001445,
151.098555952104));
#161230=CARTESIAN_POINT('Ctrl Pts',(33.3701424850901,-1.83989303878119,
151.080875617481));
#161231=CARTESIAN_POINT('Ctrl Pts',(33.5510039379001,-1.87370666177705,
151.06264936611));
#161232=CARTESIAN_POINT('Ctrl Pts',(33.5950739705717,-1.8819459380132,151.058208223562));
#161233=CARTESIAN_POINT('Ctrl Pts',(33.6394651643436,-1.89017469593504,
151.053734682196));
#161234=CARTESIAN_POINT('Ctrl Pts',(33.6841772240993,-1.8983929244592,151.049228772592));
#161235=CARTESIAN_POINT('Ctrl Pts',(33.8766766519041,-1.9337749734436,151.029829419818));
#161236=CARTESIAN_POINT('Ctrl Pts',(34.0751257124915,-1.96895863336787,
151.009829878581));
#161237=CARTESIAN_POINT('Ctrl Pts',(34.2795258855267,-2.00391606867805,
150.989230097083));
#161238=CARTESIAN_POINT('Ctrl Pts',(34.3233213711462,-2.01140616926206,
150.984816316895));
#161239=CARTESIAN_POINT('Ctrl Pts',(34.3673899602217,-2.01888604109792,
150.980374991118));
#161240=CARTESIAN_POINT('Ctrl Pts',(34.4117314899297,-2.0263556759316,150.975906137351));
#161241=CARTESIAN_POINT('Ctrl Pts',(34.6286104488291,-2.06289042420837,
150.95404851632));
#161242=CARTESIAN_POINT('Ctrl Pts',(34.8520210191477,-2.0991769182693,150.931532132542));
#161243=CARTESIAN_POINT('Ctrl Pts',(35.081967912608,-2.13518612187403,150.908356685189));
#161244=CARTESIAN_POINT('Ctrl Pts',(35.1270713875043,-2.14224923190949,
150.903810882495));
#161245=CARTESIAN_POINT('Ctrl Pts',(35.1724262550042,-2.14930180934974,
150.899239731789));
#161246=CARTESIAN_POINT('Ctrl Pts',(35.2180324233533,-2.15634384026042,
150.894643243842));
#161247=CARTESIAN_POINT('Ctrl Pts',(35.461479387331,-2.19393439231738,150.870107066476));
#161248=CARTESIAN_POINT('Ctrl Pts',(35.7120890568306,-2.23122096837176,
150.844848709685));
#161249=CARTESIAN_POINT('Ctrl Pts',(35.9698699703844,-2.26817242434974,
150.818867584338));
#161250=CARTESIAN_POINT('Ctrl Pts',(36.0165517626946,-2.27486399887224,
150.814162637487));
#161251=CARTESIAN_POINT('Ctrl Pts',(36.0634686593668,-2.28154470235949,
150.809433995305));
#161252=CARTESIAN_POINT('Ctrl Pts',(36.1106206170988,-2.28821451234414,
150.804681663958));
#161253=CARTESIAN_POINT('Ctrl Pts',(36.3830005854587,-2.32674361526947,
150.777229148215));
#161254=CARTESIAN_POINT('Ctrl Pts',(36.6632263673471,-2.36490566108977,
150.748985935835));
#161255=CARTESIAN_POINT('Ctrl Pts',(36.9513109655905,-2.4026665443615,150.719951108414));
#161256=CARTESIAN_POINT('Ctrl Pts',(36.999531099742,-2.40898703101072,150.715091205171));
#161257=CARTESIAN_POINT('Ctrl Pts',(37.0479713555632,-2.41529638232405,
150.710209129317));
#161258=CARTESIAN_POINT('Ctrl Pts',(37.0966317243219,-2.42159456730874,
150.70530488374));
#161259=CARTESIAN_POINT('Ctrl Pts',(37.4004415492397,-2.4609171315701,150.674685346159));
#161260=CARTESIAN_POINT('Ctrl Pts',(37.7128334435774,-2.49980080752529,
150.643201418644));
#161261=CARTESIAN_POINT('Ctrl Pts',(38.0338250764396,-2.53820730959646,
150.610851858719));
#161262=CARTESIAN_POINT('Ctrl Pts',(38.0870104466146,-2.54457091481435,
150.605491833274));
#161263=CARTESIAN_POINT('Ctrl Pts',(38.1404318565342,-2.55092152317193,
150.600108048707));
#161264=CARTESIAN_POINT('Ctrl Pts',(38.1940893220794,-2.55725908700571,
150.594700506049));
#161265=CARTESIAN_POINT('Ctrl Pts',(38.443204417394,-2.58668244501321,150.569594950076));
#161266=CARTESIAN_POINT('Ctrl Pts',(38.6974080777621,-2.61582361277085,
150.543977247674));
#161267=CARTESIAN_POINT('Ctrl Pts',(38.9567113549366,-2.64466260229147,
150.51784656602));
#161268=CARTESIAN_POINT('Ctrl Pts',(38.6142630337744,4.84795799788072,149.772399489946));
#161269=CARTESIAN_POINT('Ctrl Pts',(38.5518738101667,4.84248449990793,149.78368599245));
#161270=CARTESIAN_POINT('Ctrl Pts',(38.0917828938735,4.80166457174124,149.867090324444));
#161271=CARTESIAN_POINT('Ctrl Pts',(37.2666569365713,4.72231206624815,150.018981574206));
#161272=CARTESIAN_POINT('Ctrl Pts',(36.1675657918577,4.60062603149948,150.227154665666));
#161273=CARTESIAN_POINT('Ctrl Pts',(35.1567210374423,4.47267283862507,150.424283081802));
#161274=CARTESIAN_POINT('Ctrl Pts',(34.2242365051105,4.33830124550419,150.611670270562));
#161275=CARTESIAN_POINT('Ctrl Pts',(33.3605599489944,4.19687721453315,150.790698750079));
#161276=CARTESIAN_POINT('Ctrl Pts',(32.55812194511,4.04747828476444,150.962481754923));
#161277=CARTESIAN_POINT('Ctrl Pts',(31.811522135749,3.88898829657608,151.127760878239));
#161278=CARTESIAN_POINT('Ctrl Pts',(31.1168905319017,3.72004699986921,151.286968739904));
#161279=CARTESIAN_POINT('Ctrl Pts',(30.4700694589394,3.53852193518461,151.440596316724));
#161280=CARTESIAN_POINT('Ctrl Pts',(29.8659802889208,3.34090700461296,151.589333187113));
#161281=CARTESIAN_POINT('Ctrl Pts',(29.2983389023891,3.12136266852428,151.734134145579));
#161282=CARTESIAN_POINT('Ctrl Pts',(28.7606569834451,2.87046298671187,151.875930325475));
#161283=CARTESIAN_POINT('Ctrl Pts',(28.2482144210855,2.5734713359096,152.014964503663));
#161284=CARTESIAN_POINT('Ctrl Pts',(27.7590506808759,2.20617884390867,152.150266879811));
#161285=CARTESIAN_POINT('Ctrl Pts',(27.3022338120033,1.73160085833134,152.277303811874));
#161286=CARTESIAN_POINT('Ctrl Pts',(26.9178210953592,1.10518640460507,152.382971972441));
#161287=CARTESIAN_POINT('Ctrl Pts',(26.7013701547781,0.32781599167213,152.441378793244));
#161288=CARTESIAN_POINT('Ctrl Pts',(26.7294258532341,-0.486044842906302,
152.433991979976));
#161289=CARTESIAN_POINT('Ctrl Pts',(26.9753196545374,-1.20956093171679,
152.367647432518));
#161290=CARTESIAN_POINT('Ctrl Pts',(27.3563514766538,-1.78680816949054,
152.262842017495));
#161291=CARTESIAN_POINT('Ctrl Pts',(27.8053848024584,-2.23610566284,152.138110776586));
#161292=CARTESIAN_POINT('Ctrl Pts',(28.2922563302521,-2.59201839787431,
152.003684594481));
#161293=CARTESIAN_POINT('Ctrl Pts',(28.8060678733685,-2.88269490246962,
151.864609851225));
#161294=CARTESIAN_POINT('Ctrl Pts',(29.3380930897801,-3.12545698987924,
151.724680992667));
#161295=CARTESIAN_POINT('Ctrl Pts',(29.8802119089744,-3.3315629367898,151.586658563829));
#161296=CARTESIAN_POINT('Ctrl Pts',(30.4293702747731,-3.5100274763006,151.451374934494));
#161297=CARTESIAN_POINT('Ctrl Pts',(30.9988560924694,-3.67122058696772,
151.315485074222));
#161298=CARTESIAN_POINT('Ctrl Pts',(31.6039184811202,-3.82174819881736,
151.175566611529));
#161299=CARTESIAN_POINT('Ctrl Pts',(32.2586077383285,-3.96547007121551,
151.028836895302));
#161300=CARTESIAN_POINT('Ctrl Pts',(32.9681837842628,-4.10332519117328,
150.874625504658));
#161301=CARTESIAN_POINT('Ctrl Pts',(33.7411366378276,-4.23634581507805,
150.711639357809));
#161302=CARTESIAN_POINT('Ctrl Pts',(34.5880639009387,-4.3652675586447,150.538296513895));
#161303=CARTESIAN_POINT('Ctrl Pts',(35.5178717828348,-4.49005191045627,
150.353503384014));
#161304=CARTESIAN_POINT('Ctrl Pts',(36.5418485696312,-4.61060570740346,
150.155806013892));
#161305=CARTESIAN_POINT('Ctrl Pts',(37.5891726621944,-4.71793954069787,
149.959318019021));
#161306=CARTESIAN_POINT('Ctrl Pts',(38.2969062223127,-4.78144105096855,
149.829878192235));
#161307=CARTESIAN_POINT('Ctrl Pts',(38.6293920146191,-4.80952011478701,
149.769731800995));
#161308=CARTESIAN_POINT('Ctrl Pts',(38.77048515206,3.99237155033352,149.70739623108));
#161309=CARTESIAN_POINT('Ctrl Pts',(38.7084613789342,3.98711866251867,149.716657743131));
#161310=CARTESIAN_POINT('Ctrl Pts',(38.2511016937558,3.94799145212428,149.785077351974));
#161311=CARTESIAN_POINT('Ctrl Pts',(37.4313682141803,3.87256475402832,149.909402246761));
#161312=CARTESIAN_POINT('Ctrl Pts',(36.3408971723696,3.75847478669996,150.079092112684));
#161313=CARTESIAN_POINT('Ctrl Pts',(35.3395862968383,3.63994278190039,150.239102814392));
#161314=CARTESIAN_POINT('Ctrl Pts',(34.4177106792707,3.51681482324974,150.390547977447));
#161315=CARTESIAN_POINT('Ctrl Pts',(33.5659392784651,3.38854381493149,150.534587184947));
#161316=CARTESIAN_POINT('Ctrl Pts',(32.7769825454908,3.25438053296485,150.672144826256));
#161317=CARTESIAN_POINT('Ctrl Pts',(32.0457800700816,3.11346846660751,150.803833167474));
#161318=CARTESIAN_POINT('Ctrl Pts',(31.3688688032241,2.96481053892936,150.930009129647));
#161319=CARTESIAN_POINT('Ctrl Pts',(30.7426202066326,2.80683155589549,151.051068618564));
#161320=CARTESIAN_POINT('Ctrl Pts',(30.1626748117444,2.63691287705065,151.167554517892));
#161321=CARTESIAN_POINT('Ctrl Pts',(29.6237566708724,2.45067062972154,151.280203104165));
#161322=CARTESIAN_POINT('Ctrl Pts',(29.120750370036,2.24107601553824,151.389712767181));
#161323=CARTESIAN_POINT('Ctrl Pts',(28.6505813012899,1.99729222004304,151.49623650419));
#161324=CARTESIAN_POINT('Ctrl Pts',(28.2128464689627,1.70166153211956,151.599012295857));
#161325=CARTESIAN_POINT('Ctrl Pts',(27.8161807852202,1.32746699158294,151.69465045331));
#161326=CARTESIAN_POINT('Ctrl Pts',(27.4929941553154,0.843037147572355,
151.773521688089));
#161327=CARTESIAN_POINT('Ctrl Pts',(27.3153753829609,0.250080563879788,
151.816850273354));
#161328=CARTESIAN_POINT('Ctrl Pts',(27.3381602911532,-0.368260375098352,
151.811374813555));
#161329=CARTESIAN_POINT('Ctrl Pts',(27.5405501748278,-0.921138298860034,
151.762102665396));
#161330=CARTESIAN_POINT('Ctrl Pts',(27.8621521531751,-1.36846846005605,
151.683779547796));
#161331=CARTESIAN_POINT('Ctrl Pts',(28.2530528820034,-1.72323132189192,
151.589792530011));
#161332=CARTESIAN_POINT('Ctrl Pts',(28.6894815018612,-2.00997774512185,
151.487609628313));
#161333=CARTESIAN_POINT('Ctrl Pts',(29.1615492424393,-2.24874069898568,
151.380983484428));
#161334=CARTESIAN_POINT('Ctrl Pts',(29.6597632906639,-2.45160262431465,
151.272850376333));
#161335=CARTESIAN_POINT('Ctrl Pts',(30.174659009331,-2.62637778219187,151.165434742717));
#161336=CARTESIAN_POINT('Ctrl Pts',(30.7016670012872,-2.77960029340225,
151.059494894605));
#161337=CARTESIAN_POINT('Ctrl Pts',(31.252399319238,-2.91947774127626,150.95249406528));
#161338=CARTESIAN_POINT('Ctrl Pts',(31.8410743687168,-3.05138261896036,
150.841757960612));
#161339=CARTESIAN_POINT('Ctrl Pts',(32.481136182803,-3.17850347235832,150.725064225561));
#161340=CARTESIAN_POINT('Ctrl Pts',(33.1775813527336,-3.30154525563299,
150.601848983836));
#161341=CARTESIAN_POINT('Ctrl Pts',(33.938650360441,-3.42135361558111,150.471039189583));
#161342=CARTESIAN_POINT('Ctrl Pts',(34.7747427552922,-3.53856551809312,
150.331310663964));
#161343=CARTESIAN_POINT('Ctrl Pts',(35.6946436705373,-3.65315819682509,
150.181716199341));
#161344=CARTESIAN_POINT('Ctrl Pts',(36.7095268122545,-3.76509101025319,
150.021004038703));
#161345=CARTESIAN_POINT('Ctrl Pts',(37.7491015370053,-3.86600596623728,
149.860611162443));
#161346=CARTESIAN_POINT('Ctrl Pts',(38.4523857919031,-3.92649415040771,
149.754558862934));
#161347=CARTESIAN_POINT('Ctrl Pts',(38.7829212108065,-3.95341047095119,
149.705201381923));
#161348=CARTESIAN_POINT('Ctrl Pts',(38.9778745397249,3.19731394988081,149.999854791912));
#161349=CARTESIAN_POINT('Ctrl Pts',(38.916338543838,3.19148653742588,150.007208430689));
#161350=CARTESIAN_POINT('Ctrl Pts',(38.4626242424191,3.14816774453271,150.061488346695));
#161351=CARTESIAN_POINT('Ctrl Pts',(37.6500871839756,3.06583842590494,150.159510583659));
#161352=CARTESIAN_POINT('Ctrl Pts',(36.5711171193481,2.94425521394458,150.291751315632));
#161353=CARTESIAN_POINT('Ctrl Pts',(35.5825234494193,2.82065903999647,150.414951700963));
#161354=CARTESIAN_POINT('Ctrl Pts',(34.6747959447111,2.69486489432998,150.530092819935));
#161355=CARTESIAN_POINT('Ctrl Pts',(33.8388980789017,2.56638200743654,150.638150615903));
#161356=CARTESIAN_POINT('Ctrl Pts',(33.0679129044516,2.43463445681279,150.739883001722));
#161357=CARTESIAN_POINT('Ctrl Pts',(32.3572325368435,2.29907405188071,150.83578431523));
#161358=CARTESIAN_POINT('Ctrl Pts',(31.7039355846551,2.15917184513954,150.926142175826));
#161359=CARTESIAN_POINT('Ctrl Pts',(31.1050978364374,2.01406199300395,151.011255576643));
#161360=CARTESIAN_POINT('Ctrl Pts',(30.5573171327811,1.86223441262126,151.091505039686));
#161361=CARTESIAN_POINT('Ctrl Pts',(30.0566596083792,1.70110641993527,151.167371325102));
#161362=CARTESIAN_POINT('Ctrl Pts',(29.5998374677493,1.52665042186927,151.239264487423));
#161363=CARTESIAN_POINT('Ctrl Pts',(29.1859665623272,1.33302382532172,151.307204341295));
#161364=CARTESIAN_POINT('Ctrl Pts',(28.8167173246793,1.11106115618616,151.370660148695));
#161365=CARTESIAN_POINT('Ctrl Pts',(28.5001484425048,0.847535532219305,
151.42766752127));
#161366=CARTESIAN_POINT('Ctrl Pts',(28.2584910330725,0.528043369687139,
151.47305101709));
#161367=CARTESIAN_POINT('Ctrl Pts',(28.1325959852217,0.156106146179826,
151.49733827906));
#161368=CARTESIAN_POINT('Ctrl Pts',(28.1484032568081,-0.225985189187506,
151.494279745528));
#161369=CARTESIAN_POINT('Ctrl Pts',(28.2929267047297,-0.575198524295295,
151.466527011508));
#161370=CARTESIAN_POINT('Ctrl Pts',(28.5354640512508,-0.872474748378928,
151.421227158868));
#161371=CARTESIAN_POINT('Ctrl Pts',(28.8490257151681,-1.12360525762868,
151.365000995308));
#161372=CARTESIAN_POINT('Ctrl Pts',(29.2183489384953,-1.33969537808211,
151.301738585388));
#161373=CARTESIAN_POINT('Ctrl Pts',(29.6348883664465,-1.52990712165847,
151.233565391379));
#161374=CARTESIAN_POINT('Ctrl Pts',(30.0881306936774,-1.69914222580924,
151.162422669829));
#161375=CARTESIAN_POINT('Ctrl Pts',(30.5668214215576,-1.85046911839991,
151.089986846565));
#161376=CARTESIAN_POINT('Ctrl Pts',(31.0643743330293,-1.98717476103146,
151.017025604432));
#161377=CARTESIAN_POINT('Ctrl Pts',(31.5901717625383,-2.11511425971908,
150.941982485002));
#161378=CARTESIAN_POINT('Ctrl Pts',(32.1570609251648,-2.23845076038945,
150.863028933192));
#161379=CARTESIAN_POINT('Ctrl Pts',(32.7776793725769,-2.35976633813407,
150.778534659419));
#161380=CARTESIAN_POINT('Ctrl Pts',(33.4566732442955,-2.47947780796869,
150.688021723612));
#161381=CARTESIAN_POINT('Ctrl Pts',(34.2019510060455,-2.59825578166237,
150.590611811557));
#161382=CARTESIAN_POINT('Ctrl Pts',(35.0236487211914,-2.71668226239647,
150.485196195032));
#161383=CARTESIAN_POINT('Ctrl Pts',(35.9303903808119,-2.83476112433965,
150.370913196746));
#161384=CARTESIAN_POINT('Ctrl Pts',(36.9331972181514,-2.95254208528277,
150.246639883757));
#161385=CARTESIAN_POINT('Ctrl Pts',(37.9624832450496,-3.06120977505067,
150.121139581495));
#161386=CARTESIAN_POINT('Ctrl Pts',(38.6598615437989,-3.12787436936935,
150.037294403468));
#161387=CARTESIAN_POINT('Ctrl Pts',(38.9878083070654,-3.15786586028987,
149.998099350049));
#161388=CARTESIAN_POINT('Ctrl Pts',(39.199880276992,2.60290850229811,150.598231409948));
#161389=CARTESIAN_POINT('Ctrl Pts',(39.1388684177732,2.59581268633088,150.604130541553));
#161390=CARTESIAN_POINT('Ctrl Pts',(38.6890711795356,2.54315674757572,150.647607816424));
#161391=CARTESIAN_POINT('Ctrl Pts',(37.8842661670718,2.44431291877113,150.725226751088));
#161392=CARTESIAN_POINT('Ctrl Pts',(36.8176509876494,2.30146778174905,150.827652586784));
#161393=CARTESIAN_POINT('Ctrl Pts',(35.8427165320655,2.1592146055936,150.920837612846));
#161394=CARTESIAN_POINT('Ctrl Pts',(34.9501828329841,2.01731434812146,151.005711001615));
#161395=CARTESIAN_POINT('Ctrl Pts',(34.1313292830445,1.87529202353466,151.08313671715));
#161396=CARTESIAN_POINT('Ctrl Pts',(33.3796385940567,1.73271453214596,151.15375790474));
#161397=CARTESIAN_POINT('Ctrl Pts',(32.6909882310536,1.5893363355764,151.21798315668));
#161398=CARTESIAN_POINT('Ctrl Pts',(32.0630377144728,1.44511906750028,151.276049401746));
#161399=CARTESIAN_POINT('Ctrl Pts',(31.493618217534,1.29993330176996,151.328173959511));
#161400=CARTESIAN_POINT('Ctrl Pts',(30.9803543207786,1.15340323781994,151.374587937643));
#161401=CARTESIAN_POINT('Ctrl Pts',(30.5207516193253,1.00477545505744,151.415524615468));
#161402=CARTESIAN_POINT('Ctrl Pts',(30.1134825478559,0.853098687842271,
151.451100936464));
#161403=CARTESIAN_POINT('Ctrl Pts',(29.7600123204265,0.697738780618519,
151.48118360327));
#161404=CARTESIAN_POINT('Ctrl Pts',(29.4642352602667,0.538466875207633,
151.505455897129));
#161405=CARTESIAN_POINT('Ctrl Pts',(29.2335922986196,0.37639102177926,151.523408878111));
#161406=CARTESIAN_POINT('Ctrl Pts',(29.0793982921488,0.215720507103053,
151.534515800136));
#161407=CARTESIAN_POINT('Ctrl Pts',(29.009002582731,0.0624550682183219,
151.53915455036));
#161408=CARTESIAN_POINT('Ctrl Pts',(29.0173551306939,-0.0842942852346504,
151.538592549696));
#161409=CARTESIAN_POINT('Ctrl Pts',(29.0998481767366,-0.232711058266448,
151.533013599453));
#161410=CARTESIAN_POINT('Ctrl Pts',(29.257620688208,-0.386242434910132,
151.521457861273));
#161411=CARTESIAN_POINT('Ctrl Pts',(29.4882672850763,-0.542907343188585,
151.503354097979));
#161412=CARTESIAN_POINT('Ctrl Pts',(29.7856494770782,-0.69930384591628,
151.478829928837));
#161413=CARTESIAN_POINT('Ctrl Pts',(30.142662556554,-0.852883528720086,
151.448336973339));
#161414=CARTESIAN_POINT('Ctrl Pts',(30.5476985592488,-1.00069164313119,
151.412859979211));
#161415=CARTESIAN_POINT('Ctrl Pts',(30.9875832809003,-1.14058538588907,
151.373612036067));
#161416=CARTESIAN_POINT('Ctrl Pts',(31.4535676558278,-1.27241030149145,
151.331451977501));
#161417=CARTESIAN_POINT('Ctrl Pts',(31.9526434067819,-1.3998935441149,151.285802925616));
#161418=CARTESIAN_POINT('Ctrl Pts',(32.4961877440683,-1.52622614105896,
151.235630670283));
#161419=CARTESIAN_POINT('Ctrl Pts',(33.0959736577827,-1.65355532546756,
151.179824409168));
#161420=CARTESIAN_POINT('Ctrl Pts',(33.7562714775258,-1.78200644940902,
151.117956385245));
#161421=CARTESIAN_POINT('Ctrl Pts',(34.4846336892086,-1.91211751287444,
151.049283390676));
#161422=CARTESIAN_POINT('Ctrl Pts',(35.2909138741665,-2.04446893024473,
150.972831865546));
#161423=CARTESIAN_POINT('Ctrl Pts',(36.1835632153543,-2.17909741643894,
150.887749737191));
#161424=CARTESIAN_POINT('Ctrl Pts',(37.173439452658,-2.31616496109725,150.792946819857));
#161425=CARTESIAN_POINT('Ctrl Pts',(38.191710762274,-2.44539063098136,150.694986976225));
#161426=CARTESIAN_POINT('Ctrl Pts',(38.8827673371149,-2.52633282288444,
150.628254665011));
#161427=CARTESIAN_POINT('Ctrl Pts',(39.2079433948384,-2.56309542069976,
150.596804500242));
#161428=CARTESIAN_POINT('',(38.4389129826201,-4.64342671970106,149.800591313048));
#161429=CARTESIAN_POINT('Origin',(38.959854943863,-4.6434387520303,152.755016385081));
#161430=CARTESIAN_POINT('',(38.4242418866772,4.68124390104629,149.80317851189));
#161431=CARTESIAN_POINT('Origin',(38.9452145702245,4.68126981419974,152.757635929636));
#161432=CARTESIAN_POINT('Ctrl Pts',(38.4242420684175,4.68124390104622,149.803179542593));
#161433=CARTESIAN_POINT('Ctrl Pts',(38.1355463937705,4.62375019091924,149.854084254797));
#161434=CARTESIAN_POINT('Ctrl Pts',(37.8553097256357,4.56605654774142,149.903496984872));
#161435=CARTESIAN_POINT('Ctrl Pts',(37.5837514565077,4.50834271219169,149.951380422406));
#161436=CARTESIAN_POINT('Ctrl Pts',(37.4840243922502,4.48714788205486,149.968965136976));
#161437=CARTESIAN_POINT('Ctrl Pts',(37.3854678247398,4.46595084000668,149.986343492661));
#161438=CARTESIAN_POINT('Ctrl Pts',(37.2880928440942,4.44476214607814,150.003513312933));
#161439=CARTESIAN_POINT('Ctrl Pts',(37.2830066804605,4.44365540219186,150.004410139971));
#161440=CARTESIAN_POINT('Ctrl Pts',(37.2779237405206,4.44254868126253,150.00530639804));
#161441=CARTESIAN_POINT('Ctrl Pts',(37.2728440257589,4.44144198446882,150.006202086926));
#161442=CARTESIAN_POINT('Ctrl Pts',(36.9479699004643,4.37066298019586,150.063486040292));
#161443=CARTESIAN_POINT('Ctrl Pts',(36.6362872813769,4.29997312554706,150.118443805483));
#161444=CARTESIAN_POINT('Ctrl Pts',(36.3363798818645,4.22930880453252,150.171325919929));
#161445=CARTESIAN_POINT('Ctrl Pts',(36.2983021069356,4.22033690148688,150.178040103223));
#161446=CARTESIAN_POINT('Ctrl Pts',(36.2604141924949,4.211365449165,150.18472079319));
#161447=CARTESIAN_POINT('Ctrl Pts',(36.2227132740173,4.20239434386347,150.191368475827));
#161448=CARTESIAN_POINT('Ctrl Pts',(36.2217748164504,4.20217103361018,150.191533951054));
#161449=CARTESIAN_POINT('Ctrl Pts',(36.2208364747502,4.20194772357203,150.19169940583));
#161450=CARTESIAN_POINT('Ctrl Pts',(36.2198982488716,4.20172441374397,150.191864840162));
#161451=CARTESIAN_POINT('Ctrl Pts',(35.948661370091,4.13716654750797,150.239691160866));
#161452=CARTESIAN_POINT('Ctrl Pts',(35.6871028563909,4.07262604597075,150.285810438586));
#161453=CARTESIAN_POINT('Ctrl Pts',(35.4345007616386,4.00808082045874,150.330351422569));
#161454=CARTESIAN_POINT('Ctrl Pts',(35.3746566780167,3.99278938007412,150.340903648482));
#161455=CARTESIAN_POINT('Ctrl Pts',(35.3153153949423,3.97749786840843,150.351367208456));
#161456=CARTESIAN_POINT('Ctrl Pts',(35.2564674929442,3.96220630375595,150.361743678019));
#161457=CARTESIAN_POINT('Ctrl Pts',(35.2539306927745,3.96154711893392,150.362190984191));
#161458=CARTESIAN_POINT('Ctrl Pts',(35.2513948095389,3.96088793403217,150.362638128502));
#161459=CARTESIAN_POINT('Ctrl Pts',(35.2488598423598,3.96022874902138,150.363085111101));
#161460=CARTESIAN_POINT('Ctrl Pts',(35.0033444450969,3.89638568583368,150.406376050384));
#161461=CARTESIAN_POINT('Ctrl Pts',(34.7664193094501,3.83253763047813,150.448151774801));
#161462=CARTESIAN_POINT('Ctrl Pts',(34.5372789566154,3.76859345616774,150.488555818789));
#161463=CARTESIAN_POINT('Ctrl Pts',(34.4822394955994,3.75323407993558,150.498260861033));
#161464=CARTESIAN_POINT('Ctrl Pts',(34.4276493125477,3.73786934673916,150.50788667875));
#161465=CARTESIAN_POINT('Ctrl Pts',(34.37349746577,3.72249829637841,150.517435116911));
#161466=CARTESIAN_POINT('Ctrl Pts',(34.3680530896807,3.72095290533394,150.518395107964));
#161467=CARTESIAN_POINT('Ctrl Pts',(34.3626131447211,3.71940745057952,150.519354316762));
#161468=CARTESIAN_POINT('Ctrl Pts',(34.3571776208378,3.71786193124537,150.520312744973));
#161469=CARTESIAN_POINT('Ctrl Pts',(34.1432816612982,3.65704344381727,150.558028322412));
#161470=CARTESIAN_POINT('Ctrl Pts',(33.9362294158252,3.59612091795574,150.594536600627));
#161471=CARTESIAN_POINT('Ctrl Pts',(33.7354007572472,3.53497828185585,150.629948516004));
#161472=CARTESIAN_POINT('Ctrl Pts',(33.6770619370553,3.51721692608747,150.640235341493));
#161473=CARTESIAN_POINT('Ctrl Pts',(33.6192484739092,3.49943727844189,150.650429544792));
#161474=CARTESIAN_POINT('Ctrl Pts',(33.5619455742565,3.48163708652143,150.660533610237));
#161475=CARTESIAN_POINT('Ctrl Pts',(33.5540695998418,3.47919054617197,150.661922359522));
#161476=CARTESIAN_POINT('Ctrl Pts',(33.5462032696261,3.47674362287509,150.663309406071));
#161477=CARTESIAN_POINT('Ctrl Pts',(33.5383465770558,3.47429632079451,150.664694750628));
#161478=CARTESIAN_POINT('Ctrl Pts',(33.3659094274534,3.42058341409569,150.695100021608));
#161479=CARTESIAN_POINT('Ctrl Pts',(33.1981132959245,3.36668359002243,150.724686334537));
#161480=CARTESIAN_POINT('Ctrl Pts',(33.0348807818954,3.31259713924036,150.753468932572));
#161481=CARTESIAN_POINT('Ctrl Pts',(32.9604300875545,3.28792819482623,150.766596736316));
#161482=CARTESIAN_POINT('Ctrl Pts',(32.8869289989043,3.26322115034888,150.779557198536));
#161483=CARTESIAN_POINT('Ctrl Pts',(32.8143711806231,3.23847930299279,150.792351142007));
#161484=CARTESIAN_POINT('Ctrl Pts',(32.804489410665,3.23510966964793,150.794093570449));
#161485=CARTESIAN_POINT('Ctrl Pts',(32.7946251368876,3.23173938487948,150.795832909881));
#161486=CARTESIAN_POINT('Ctrl Pts',(32.7847783336901,3.22836845726935,150.797569163755));
#161487=CARTESIAN_POINT('Ctrl Pts',(32.6331987059228,3.17647710307769,150.824296692537));
#161488=CARTESIAN_POINT('Ctrl Pts',(32.4857575529114,3.12442888944696,150.850293861247));
#161489=CARTESIAN_POINT('Ctrl Pts',(32.342353896521,3.07220618801423,150.875580055377));
#161490=CARTESIAN_POINT('Ctrl Pts',(32.2698697907833,3.0458099586025,150.8883610905));
#161491=CARTESIAN_POINT('Ctrl Pts',(32.1984174902979,3.01937001141514,150.900960326406));
#161492=CARTESIAN_POINT('Ctrl Pts',(32.1279853768168,2.99288869106745,150.913379472003));
#161493=CARTESIAN_POINT('Ctrl Pts',(32.1165162491167,2.98857648702126,150.915401799031));
#161494=CARTESIAN_POINT('Ctrl Pts',(32.1050741724831,2.98426317007202,150.917419350178));
#161495=CARTESIAN_POINT('Ctrl Pts',(32.0936590979484,2.97994875777987,150.919432131884));
#161496=CARTESIAN_POINT('Ctrl Pts',(31.9628656099427,2.93051438653068,150.942494507794));
#161497=CARTESIAN_POINT('Ctrl Pts',(31.8356156817233,2.88093160537131,150.964931427134));
#161498=CARTESIAN_POINT('Ctrl Pts',(31.7118292366422,2.83117400237597,150.98675851427));
#161499=CARTESIAN_POINT('Ctrl Pts',(31.6402905927357,2.80241809586303,150.999372821217));
#161500=CARTESIAN_POINT('Ctrl Pts',(31.5699090493162,2.773604857122,151.011783287754));
#161501=CARTESIAN_POINT('Ctrl Pts',(31.5006712021453,2.74473655442193,151.023991877041));
#161502=CARTESIAN_POINT('Ctrl Pts',(31.4880120968377,2.73945841683006,151.026224035084));
#161503=CARTESIAN_POINT('Ctrl Pts',(31.4753912219212,2.73417839586638,151.02844944385));
#161504=CARTESIAN_POINT('Ctrl Pts',(31.4628084881326,2.72889652164137,151.030668115196));
#161505=CARTESIAN_POINT('Ctrl Pts',(31.3508495242083,2.68189932884144,151.050409464683));
#161506=CARTESIAN_POINT('Ctrl Pts',(31.241908972707,2.63475070775182,151.069617979236));
#161507=CARTESIAN_POINT('Ctrl Pts',(31.1359196205206,2.58741358020376,151.088306887775));
#161508=CARTESIAN_POINT('Ctrl Pts',(31.0660982212521,2.5562298394357,151.100618367354));
#161509=CARTESIAN_POINT('Ctrl Pts',(30.9975578850339,2.52496554483507,151.112704200039));
#161510=CARTESIAN_POINT('Ctrl Pts',(30.9302822292632,2.49362176653836,151.124566829132));
#161511=CARTESIAN_POINT('Ctrl Pts',(30.9168051726109,2.48734279577305,151.126943221045));
#161512=CARTESIAN_POINT('Ctrl Pts',(30.9033788717754,2.48106052889335,151.129310653308));
#161513=CARTESIAN_POINT('Ctrl Pts',(30.8900031337578,2.47477498992906,151.131669153867));
#161514=CARTESIAN_POINT('Ctrl Pts',(30.794615455276,2.42995032537447,151.148488554239));
#161515=CARTESIAN_POINT('Ctrl Pts',(30.7017981115883,2.38495443743262,151.164854175054));
#161516=CARTESIAN_POINT('Ctrl Pts',(30.61148076225,2.3397290349788,151.180779615583));
#161517=CARTESIAN_POINT('Ctrl Pts',(30.5444869012194,2.30618260841464,151.192592481632));
#161518=CARTESIAN_POINT('Ctrl Pts',(30.4788689138771,2.27251130679068,151.204163016596));
#161519=CARTESIAN_POINT('Ctrl Pts',(30.4146018444979,2.2387090720738,151.215495176014));
#161520=CARTESIAN_POINT('Ctrl Pts',(30.4006476140079,2.23136963402451,151.217955713984));
#161521=CARTESIAN_POINT('Ctrl Pts',(30.3867571048912,2.22402378188774,151.22040500559));
#161522=CARTESIAN_POINT('Ctrl Pts',(30.3729299231136,2.21667147155003,151.222843111905));
#161523=CARTESIAN_POINT('Ctrl Pts',(30.2923702339112,2.17383556722413,151.237047965077));
#161524=CARTESIAN_POINT('Ctrl Pts',(30.2139592078528,2.13077550160407,151.25087347165));
#161525=CARTESIAN_POINT('Ctrl Pts',(30.1376258859355,2.08740279169798,151.264333079088));
#161526=CARTESIAN_POINT('Ctrl Pts',(30.0739645180164,2.05123030537576,151.275558281918));
#161527=CARTESIAN_POINT('Ctrl Pts',(30.011748589835,2.01484184555696,151.286528882051));
#161528=CARTESIAN_POINT('Ctrl Pts',(29.9509417594417,1.97821297095187,151.297250929889));
#161529=CARTESIAN_POINT('Ctrl Pts',(29.9368185427894,1.96970541467192,151.299741271905));
#161530=CARTESIAN_POINT('Ctrl Pts',(29.9227714224001,1.96118449930074,151.302218188322));
#161531=CARTESIAN_POINT('Ctrl Pts',(29.9088002635435,1.95265029282505,151.304681693433));
#161532=CARTESIAN_POINT('Ctrl Pts',(29.8434571913563,1.9127358322189,151.316203500178));
#161533=CARTESIAN_POINT('Ctrl Pts',(29.7797753830253,1.87252556767506,151.327432057101));
#161534=CARTESIAN_POINT('Ctrl Pts',(29.7177587449049,1.83194049750251,151.338367175733));
#161535=CARTESIAN_POINT('Ctrl Pts',(29.6557421067844,1.79135542732997,151.349302294365));
#161536=CARTESIAN_POINT('Ctrl Pts',(29.5953908442221,1.75039647020468,151.359943927662));
#161537=CARTESIAN_POINT('Ctrl Pts',(29.5367111206233,1.70903815109368,151.370290919576));
#161538=CARTESIAN_POINT('Ctrl Pts',(29.5227530457233,1.69920029773504,151.372752146032));
#161539=CARTESIAN_POINT('Ctrl Pts',(29.5088896292455,1.68933928098665,151.375196684953));
#161540=CARTESIAN_POINT('Ctrl Pts',(29.4951218746314,1.67945619377341,151.377624354707));
#161541=CARTESIAN_POINT('Ctrl Pts',(29.4466018999985,1.64462646631817,151.386179887415));
#161542=CARTESIAN_POINT('Ctrl Pts',(29.3992707072912,1.60951838097622,151.39452574677));
#161543=CARTESIAN_POINT('Ctrl Pts',(29.3531993787577,1.57410391004019,151.402649291676));
#161544=CARTESIAN_POINT('Ctrl Pts',(29.3050768470894,1.53711270415614,151.411134515772));
#161545=CARTESIAN_POINT('Ctrl Pts',(29.2583291609921,1.49978748815046,151.419377141862));
#161546=CARTESIAN_POINT('Ctrl Pts',(29.2130253752663,1.46215189586027,151.42736534959));
#161547=CARTESIAN_POINT('Ctrl Pts',(29.1994676460809,1.45088897026082,151.429755921489));
#161548=CARTESIAN_POINT('Ctrl Pts',(29.1860391345271,1.43959859518491,151.432123727751));
#161549=CARTESIAN_POINT('Ctrl Pts',(29.17274143352,1.42828224908261,151.434468503544));
#161550=CARTESIAN_POINT('Ctrl Pts',(29.1594202525859,1.4169459215579,151.436817419537));
#161551=CARTESIAN_POINT('Ctrl Pts',(29.1462315112643,1.40558085731081,151.439143017953));
#161552=CARTESIAN_POINT('Ctrl Pts',(29.1331743741699,1.39418793964176,151.441445464654));
#161553=CARTESIAN_POINT('Ctrl Pts',(29.094039523704,1.36004108753139,151.448346357758));
#161554=CARTESIAN_POINT('Ctrl Pts',(29.0560887417731,1.32564002108451,151.455038804581));
#161555=CARTESIAN_POINT('Ctrl Pts',(29.0193620706213,1.29091789181491,151.461514806543));
#161556=CARTESIAN_POINT('Ctrl Pts',(28.9794896138272,1.25322167389802,151.468545503862));
#161557=CARTESIAN_POINT('Ctrl Pts',(28.9410601559824,1.21514758132632,151.475321066849));
#161558=CARTESIAN_POINT('Ctrl Pts',(28.9040958965794,1.17666455287375,151.481838344625));
#161559=CARTESIAN_POINT('Ctrl Pts',(28.8906638149357,1.16268058056042,151.484206594621));
#161560=CARTESIAN_POINT('Ctrl Pts',(28.8774249307655,1.14864305292917,151.486540804213));
#161561=CARTESIAN_POINT('Ctrl Pts',(28.8643793941046,1.1345518127135,151.488841034459));
#161562=CARTESIAN_POINT('Ctrl Pts',(28.852338354534,1.12154558802187,151.490964148604));
#161563=CARTESIAN_POINT('Ctrl Pts',(28.8404647618265,1.10849009751035,151.493057834043));
#161564=CARTESIAN_POINT('Ctrl Pts',(28.828758333926,1.09538770375143,151.495122225921));
#161565=CARTESIAN_POINT('Ctrl Pts',(28.8002025600444,1.06342671644882,151.500157947165));
#161566=CARTESIAN_POINT('Ctrl Pts',(28.7726447720803,1.03118399445943,151.50501857134));
#161567=CARTESIAN_POINT('Ctrl Pts',(28.7461821275536,0.998625628472416,
151.509685164022));
#161568=CARTESIAN_POINT('Ctrl Pts',(28.7180835161302,0.964054447442926,
151.514640253614));
#161569=CARTESIAN_POINT('Ctrl Pts',(28.6912197808251,0.929127997819401,
151.519376583851));
#161570=CARTESIAN_POINT('Ctrl Pts',(28.665658116513,0.893838741770888,151.523882827191));
#161571=CARTESIAN_POINT('Ctrl Pts',(28.6489002718861,0.870703633562121,
151.526837052894));
#161572=CARTESIAN_POINT('Ctrl Pts',(28.6327010237128,0.847413257758778,
151.529692623667));
#161573=CARTESIAN_POINT('Ctrl Pts',(28.6170686268516,0.823970377008213,
151.532448697277));
#161574=CARTESIAN_POINT('Ctrl Pts',(28.6071426818823,0.80908508805876,151.534198693469));
#161575=CARTESIAN_POINT('Ctrl Pts',(28.5974488492278,0.794137221794272,
151.535907951886));
#161576=CARTESIAN_POINT('Ctrl Pts',(28.5879885995462,0.779134708010062,
151.537576426224));
#161577=CARTESIAN_POINT('Ctrl Pts',(28.5702786751946,0.751049467858327,
151.540699869613));
#161578=CARTESIAN_POINT('Ctrl Pts',(28.5533911385098,0.722772919265728,
151.543679569537));
#161579=CARTESIAN_POINT('Ctrl Pts',(28.5374369545749,0.694380728259057,
151.54649407696));
#161580=CARTESIAN_POINT('Ctrl Pts',(28.5212919358127,0.665648926095429,
151.549342249913));
#161581=CARTESIAN_POINT('Ctrl Pts',(28.5061026110867,0.636798981699141,
151.552021313744));
#161582=CARTESIAN_POINT('Ctrl Pts',(28.4919314200231,0.607905927755162,
151.55451989888));
#161583=CARTESIAN_POINT('Ctrl Pts',(28.477447964955,0.578376211678344,151.55707354066));
#161584=CARTESIAN_POINT('Ctrl Pts',(28.4640278759436,0.548801765921204,
151.559438724222));
#161585=CARTESIAN_POINT('Ctrl Pts',(28.4516850436384,0.519254673332231,
151.561613683379));
#161586=CARTESIAN_POINT('Ctrl Pts',(28.4487242372839,0.512166898230697,
151.562135413945));
#161587=CARTESIAN_POINT('Ctrl Pts',(28.4458251912471,0.505080650072745,
151.562646241913));
#161588=CARTESIAN_POINT('Ctrl Pts',(28.4429876753242,0.497996828474827,
151.563146222405));
#161589=CARTESIAN_POINT('Ctrl Pts',(28.4363698149362,0.481475426084866,
151.564312313162));
#161590=CARTESIAN_POINT('Ctrl Pts',(28.4301044252218,0.464972804317448,
151.565416263435));
#161591=CARTESIAN_POINT('Ctrl Pts',(28.4241829166714,0.448484248438617,
151.566459789768));
#161592=CARTESIAN_POINT('Ctrl Pts',(28.4141536804503,0.42055764486347,151.568227206299));
#161593=CARTESIAN_POINT('Ctrl Pts',(28.4051119101709,0.39267552392786,151.569821089725));
#161594=CARTESIAN_POINT('Ctrl Pts',(28.3970398727197,0.364937280493078,
151.571244286348));
#161595=CARTESIAN_POINT('Ctrl Pts',(28.3885568109504,0.33578661886001,151.572739951468));
#161596=CARTESIAN_POINT('Ctrl Pts',(28.3811440360992,0.306794434072459,
151.574047256385));
#161597=CARTESIAN_POINT('Ctrl Pts',(28.3747692662043,0.278018244558982,
151.575171690596));
#161598=CARTESIAN_POINT('Ctrl Pts',(28.3679646708835,0.247301790829552,
151.576371940942));
#161599=CARTESIAN_POINT('Ctrl Pts',(28.3623418598648,0.216831067506705,
151.577364018936));
#161600=CARTESIAN_POINT('Ctrl Pts',(28.3578616131784,0.18661797755784,151.578154296732));
#161601=CARTESIAN_POINT('Ctrl Pts',(28.3572889513731,0.182756162830784,
151.578255309453));
#161602=CARTESIAN_POINT('Ctrl Pts',(28.3567349677807,0.178898488924442,
151.578353022512));
#161603=CARTESIAN_POINT('Ctrl Pts',(28.356199592719,0.175044923013026,151.578447446375));
#161604=CARTESIAN_POINT('Ctrl Pts',(28.3538069307026,0.157822826872332,
151.57886943912));
#161605=CARTESIAN_POINT('Ctrl Pts',(28.3517923553221,0.140707906652478,
151.579224611498));
#161606=CARTESIAN_POINT('Ctrl Pts',(28.3501553603895,0.123671004711587,
151.579512843201));
#161607=CARTESIAN_POINT('Ctrl Pts',(28.3477486824018,0.0986236841233151,
151.579936595824));
#161608=CARTESIAN_POINT('Ctrl Pts',(28.3461551320974,0.073745843099456,
151.580216238149));
#161609=CARTESIAN_POINT('Ctrl Pts',(28.3452992114535,0.0489932041348807,
151.580366104403));
#161610=CARTESIAN_POINT('Ctrl Pts',(28.3444242118242,0.0236888139759929,
151.580519311265));
#161611=CARTESIAN_POINT('Ctrl Pts',(28.3443202264207,-0.00148569978635055,
151.580536857902));
#161612=CARTESIAN_POINT('Ctrl Pts',(28.3449599427278,-0.0265873899183545,
151.580423929627));
#161613=CARTESIAN_POINT('Ctrl Pts',(28.3456024747252,-0.0517995643143712,
151.580310504301));
#161614=CARTESIAN_POINT('Ctrl Pts',(28.3469954415848,-0.0769392452442724,
151.580065418563));
#161615=CARTESIAN_POINT('Ctrl Pts',(28.3491618389979,-0.102059265144167,
151.579684384792));
#161616=CARTESIAN_POINT('Ctrl Pts',(28.3500423370033,-0.112268900404609,
151.579529519635));
#161617=CARTESIAN_POINT('Ctrl Pts',(28.3510511638344,-0.122475149165934,
151.57935209078));
#161618=CARTESIAN_POINT('Ctrl Pts',(28.3521921649127,-0.132680756132027,
151.579151376766));
#161619=CARTESIAN_POINT('Ctrl Pts',(28.3541677950609,-0.150351646357203,
151.578803842777));
#161620=CARTESIAN_POINT('Ctrl Pts',(28.3564988941821,-0.168027950876555,
151.578393700082));
#161621=CARTESIAN_POINT('Ctrl Pts',(28.3592130136351,-0.185705005592994,
151.577915738267));
#161622=CARTESIAN_POINT('Ctrl Pts',(28.3636447570318,-0.214568941712832,
151.577135299472));
#161623=CARTESIAN_POINT('Ctrl Pts',(28.3690968123005,-0.243436794795253,
151.576174203392));
#161624=CARTESIAN_POINT('Ctrl Pts',(28.375586296123,-0.272386597642406,
151.575029920963));
#161625=CARTESIAN_POINT('Ctrl Pts',(28.3819105022187,-0.300599091061347,
151.573914781745));
#161626=CARTESIAN_POINT('Ctrl Pts',(28.3892210531441,-0.328889780272276,
151.572625452078));
#161627=CARTESIAN_POINT('Ctrl Pts',(28.3975532793529,-0.357287510894987,
151.571155919633));
#161628=CARTESIAN_POINT('Ctrl Pts',(28.4054830898646,-0.384313736198647,
151.569757360168));
#161629=CARTESIAN_POINT('Ctrl Pts',(28.414339212776,-0.411437132340805,
151.568195394969));
#161630=CARTESIAN_POINT('Ctrl Pts',(28.4241555309917,-0.438638844865651,
151.566464358249));
#161631=CARTESIAN_POINT('Ctrl Pts',(28.4309737242029,-0.457532540811235,
151.56526201919));
#161632=CARTESIAN_POINT('Ctrl Pts',(28.438246110612,-0.476505520160626,
151.563979708771));
#161633=CARTESIAN_POINT('Ctrl Pts',(28.4459628434618,-0.495499582166659,
151.562619400363));
#161634=CARTESIAN_POINT('Ctrl Pts',(28.4579981129699,-0.525123343898964,
151.56049781878));
#161635=CARTESIAN_POINT('Ctrl Pts',(28.4711159948491,-0.554796776916299,
151.558186201867));
#161636=CARTESIAN_POINT('Ctrl Pts',(28.4853086342612,-0.584441168488999,
151.55568470758));
#161637=CARTESIAN_POINT('Ctrl Pts',(28.4992664688762,-0.61359511954932,
151.553224598328));
#161638=CARTESIAN_POINT('Ctrl Pts',(28.5142638513556,-0.642720753405762,
151.550580795653));
#161639=CARTESIAN_POINT('Ctrl Pts',(28.5302441252966,-0.671744059448906,
151.547762810325));
#161640=CARTESIAN_POINT('Ctrl Pts',(28.5444347335186,-0.69751698217131,
151.545260417318));
#161641=CARTESIAN_POINT('Ctrl Pts',(28.5593997749469,-0.723209106787243,
151.542620773781));
#161642=CARTESIAN_POINT('Ctrl Pts',(28.5750658528408,-0.748771480970023,
151.539857312333));
#161643=CARTESIAN_POINT('Ctrl Pts',(28.5873730698822,-0.768853194420763,
151.537686346502));
#161644=CARTESIAN_POINT('Ctrl Pts',(28.6001545842406,-0.788851285535069,
151.535431631614));
#161645=CARTESIAN_POINT('Ctrl Pts',(28.6133751259987,-0.808770178727065,
151.533100099107));
#161646=CARTESIAN_POINT('Ctrl Pts',(28.6404673054132,-0.849588946820708,
151.528322208901));
#161647=CARTESIAN_POINT('Ctrl Pts',(28.6694038328263,-0.890073648743999,
151.523221589708));
#161648=CARTESIAN_POINT('Ctrl Pts',(28.7002046692454,-0.930291659501632,
151.517791423635));
#161649=CARTESIAN_POINT('Ctrl Pts',(28.7267366815885,-0.964935678362477,
151.513113848282));
#161650=CARTESIAN_POINT('Ctrl Pts',(28.7546521213732,-0.999381024742059,
151.508191709033));
#161651=CARTESIAN_POINT('Ctrl Pts',(28.7839279689917,-1.03369193195231,
151.503028897144));
#161652=CARTESIAN_POINT('Ctrl Pts',(28.788638257889,-1.03921232840313,151.502198235096));
#161653=CARTESIAN_POINT('Ctrl Pts',(28.7933836764714,-1.04472930869436,
151.501361363159));
#161654=CARTESIAN_POINT('Ctrl Pts',(28.7981640235505,-1.05024322169471,
151.50051832233));
#161655=CARTESIAN_POINT('Ctrl Pts',(28.8158944374376,-1.07069444793768,
151.497391465103));
#161656=CARTESIAN_POINT('Ctrl Pts',(28.83411887679,-1.0910920270257,151.494177326023));
#161657=CARTESIAN_POINT('Ctrl Pts',(28.8528112558912,-1.11144444760841,
151.490881046906));
#161658=CARTESIAN_POINT('Ctrl Pts',(28.8868664466705,-1.14852402758114,
151.484875636169));
#161659=CARTESIAN_POINT('Ctrl Pts',(28.9224751947787,-1.18545262339267,
151.478597567753));
#161660=CARTESIAN_POINT('Ctrl Pts',(28.9596250610351,-1.22218491422455,
151.472047517969));
#161661=CARTESIAN_POINT('Ctrl Pts',(28.9942912862789,-1.25646148089941,
151.465935369419));
#161662=CARTESIAN_POINT('Ctrl Pts',(29.0302992476044,-1.29056663370428,
151.459586407157));
#161663=CARTESIAN_POINT('Ctrl Pts',(29.0676137132796,-1.32450220720318,
151.453006594243));
#161664=CARTESIAN_POINT('Ctrl Pts',(29.0745937530851,-1.33085019181332,
151.451775775171));
#161665=CARTESIAN_POINT('Ctrl Pts',(29.0816194390092,-1.33719236984751,
151.450536894129));
#161666=CARTESIAN_POINT('Ctrl Pts',(29.0886904426302,-1.34352893841016,
151.449290012448));
#161667=CARTESIAN_POINT('Ctrl Pts',(29.1120739001454,-1.36448365569211,
151.445166636703));
#161668=CARTESIAN_POINT('Ctrl Pts',(29.1359606208211,-1.38536449157222,
151.44095439532));
#161669=CARTESIAN_POINT('Ctrl Pts',(29.1603176844792,-1.40617450552468,
151.436659366932));
#161670=CARTESIAN_POINT('Ctrl Pts',(29.204187252997,-1.4436554739107,151.428923580518));
#161671=CARTESIAN_POINT('Ctrl Pts',(29.2495829757347,-1.48090508051263,
151.420919216224));
#161672=CARTESIAN_POINT('Ctrl Pts',(29.2963865595,-1.51783781305876,151.412666627315));
#161673=CARTESIAN_POINT('Ctrl Pts',(29.3431901432653,-1.55477054560488,
151.404414038406));
#161674=CARTESIAN_POINT('Ctrl Pts',(29.3914012702663,-1.59138588765514,
151.395913272225));
#161675=CARTESIAN_POINT('Ctrl Pts',(29.4408862584704,-1.62765597376399,
151.387187715802));
#161676=CARTESIAN_POINT('Ctrl Pts',(29.4697729320755,-1.64882849854538,
151.382094205435));
#161677=CARTESIAN_POINT('Ctrl Pts',(29.4990964040957,-1.66987327465208,
151.376923623045));
#161678=CARTESIAN_POINT('Ctrl Pts',(29.5288210851771,-1.69079349879652,
151.371682274741));
#161679=CARTESIAN_POINT('Ctrl Pts',(29.583881306592,-1.7295448707721,151.361973514624));
#161680=CARTESIAN_POINT('Ctrl Pts',(29.6403183269796,-1.76786694464797,
151.352021960529));
#161681=CARTESIAN_POINT('Ctrl Pts',(29.6979412888232,-1.80568579260789,
151.341861469206));
#161682=CARTESIAN_POINT('Ctrl Pts',(29.7453791455287,-1.83681999732234,
151.333496888213));
#161683=CARTESIAN_POINT('Ctrl Pts',(29.7936205341707,-1.8676140656969,151.324990737202));
#161684=CARTESIAN_POINT('Ctrl Pts',(29.8425576044251,-1.89805327876354,
151.316361925641));
#161685=CARTESIAN_POINT('Ctrl Pts',(29.8762442931379,-1.91900664376693,
151.310422132198));
#161686=CARTESIAN_POINT('Ctrl Pts',(29.9102614845754,-1.93978414451622,
151.304424061161));
#161687=CARTESIAN_POINT('Ctrl Pts',(29.9445834524753,-1.96039441044776,
151.298372151826));
#161688=CARTESIAN_POINT('Ctrl Pts',(30.0160630182559,-2.00331773185241,
151.2857683334));
#161689=CARTESIAN_POINT('Ctrl Pts',(30.0888641235138,-2.04551315584805,
151.27293115869));
#161690=CARTESIAN_POINT('Ctrl Pts',(30.1627771933051,-2.08695944696762,
151.259898287955));
#161691=CARTESIAN_POINT('Ctrl Pts',(30.2013677697836,-2.10859887111432,
151.253093726917));
#161692=CARTESIAN_POINT('Ctrl Pts',(30.24026157973,-2.13003494085121,151.246235777382));
#161693=CARTESIAN_POINT('Ctrl Pts',(30.2794297577773,-2.1512701895881,151.239329476774));
#161694=CARTESIAN_POINT('Ctrl Pts',(30.3170942296121,-2.17169019551711,
151.232688316075));
#161695=CARTESIAN_POINT('Ctrl Pts',(30.3550119234677,-2.19192082334998,
151.226002530369));
#161696=CARTESIAN_POINT('Ctrl Pts',(30.3931414253752,-2.21196230894521,
151.219279278749));
#161697=CARTESIAN_POINT('Ctrl Pts',(30.4752143388864,-2.25510116551577,
151.204807627633));
#161698=CARTESIAN_POINT('Ctrl Pts',(30.5582681288881,-2.29736068686337,
151.190162591056));
#161699=CARTESIAN_POINT('Ctrl Pts',(30.6418972610801,-2.33867977594509,
151.175416540789));
#161700=CARTESIAN_POINT('Ctrl Pts',(30.6743627499852,-2.35472017231165,
151.169692007738));
#161701=CARTESIAN_POINT('Ctrl Pts',(30.7069150439222,-2.37061940436573,
151.163952214052));
#161702=CARTESIAN_POINT('Ctrl Pts',(30.7395308275734,-2.3863759309605,151.158201245153));
#161703=CARTESIAN_POINT('Ctrl Pts',(30.7807271122191,-2.40627765589118,
151.150937321825));
#161704=CARTESIAN_POINT('Ctrl Pts',(30.8220259218793,-2.42594287864325,
151.143655355438));
#161705=CARTESIAN_POINT('Ctrl Pts',(30.863562833521,-2.44545103297551,151.136331292355));
#161706=CARTESIAN_POINT('Ctrl Pts',(30.945172341805,-2.48377961398125,151.121941363897));
#161707=CARTESIAN_POINT('Ctrl Pts',(31.0276994465686,-2.52150490099597,
151.107389275528));
#161708=CARTESIAN_POINT('Ctrl Pts',(31.112191669517,-2.55913493840193,151.09249101624));
#161709=CARTESIAN_POINT('Ctrl Pts',(31.1471908701709,-2.57472242307004,
151.086319712562));
#161710=CARTESIAN_POINT('Ctrl Pts',(31.1825275816439,-2.59029299310569,
151.080088938532));
#161711=CARTESIAN_POINT('Ctrl Pts',(31.2182775590854,-2.60588061303104,
151.073785315971));
#161712=CARTESIAN_POINT('Ctrl Pts',(31.2634312776054,-2.62556842972012,
151.065823576716));
#161713=CARTESIAN_POINT('Ctrl Pts',(31.3092419322252,-2.64528679282138,
151.057746041459));
#161714=CARTESIAN_POINT('Ctrl Pts',(31.3557214141397,-2.66503620428409,
151.049550455661));
#161715=CARTESIAN_POINT('Ctrl Pts',(31.4731874039566,-2.71494820997369,
151.028838034649));
#161716=CARTESIAN_POINT('Ctrl Pts',(31.5949248965874,-2.76505561399907,
151.007371934376));
#161717=CARTESIAN_POINT('Ctrl Pts',(31.7211181180094,-2.81530679931872,
150.98512086285));
#161718=CARTESIAN_POINT('Ctrl Pts',(31.7285406554425,-2.81826251516373,
150.983812080893));
#161719=CARTESIAN_POINT('Ctrl Pts',(31.7359786106392,-2.82121874361973,
150.982500581475));
#161720=CARTESIAN_POINT('Ctrl Pts',(31.7434320221541,-2.82417548019535,
150.98118635752));
#161721=CARTESIAN_POINT('Ctrl Pts',(31.7957981714862,-2.84494890840955,
150.971952888028));
#161722=CARTESIAN_POINT('Ctrl Pts',(31.8489268182686,-2.8657461266685,150.962585025477));
#161723=CARTESIAN_POINT('Ctrl Pts',(31.9027999515756,-2.88655862667242,
150.953085748909));
#161724=CARTESIAN_POINT('Ctrl Pts',(32.0241632686974,-2.93344422405697,
150.931686144991));
#161725=CARTESIAN_POINT('Ctrl Pts',(32.1493046661099,-2.9804044103554,150.909619836333));
#161726=CARTESIAN_POINT('Ctrl Pts',(32.2780098009442,-3.02731403789428,
150.886925789182));
#161727=CARTESIAN_POINT('Ctrl Pts',(32.2932592768915,-3.03287206973018,
150.884236911798));
#161728=CARTESIAN_POINT('Ctrl Pts',(32.308558787786,-3.0384294518267,150.881539216878));
#161729=CARTESIAN_POINT('Ctrl Pts',(32.3239079825989,-3.04398602555797,
150.878832764762));
#161730=CARTESIAN_POINT('Ctrl Pts',(32.3837616995455,-3.06565371532004,
150.868279037293));
#161731=CARTESIAN_POINT('Ctrl Pts',(32.4443708346114,-3.08730579589398,
150.857592178118));
#161732=CARTESIAN_POINT('Ctrl Pts',(32.5057826768735,-3.10895759434287,
150.846763625539));
#161733=CARTESIAN_POINT('Ctrl Pts',(32.6520415155047,-3.16052365682793,
150.82097427505));
#161734=CARTESIAN_POINT('Ctrl Pts',(32.8028522891403,-3.21208759517891,
150.794381722189));
#161735=CARTESIAN_POINT('Ctrl Pts',(32.9588518239448,-3.26379216756449,
150.766875021505));
#161736=CARTESIAN_POINT('Ctrl Pts',(33.0267189636895,-3.28628609002349,
150.754908312107));
#161737=CARTESIAN_POINT('Ctrl Pts',(33.095567935825,-3.30880544892256,150.742768561037));
#161738=CARTESIAN_POINT('Ctrl Pts',(33.1654559814257,-3.33136269090447,
150.730445423497));
#161739=CARTESIAN_POINT('Ctrl Pts',(33.3236650123146,-3.38242663700293,
150.702548926592));
#161740=CARTESIAN_POINT('Ctrl Pts',(33.4871980878252,-3.43368438659886,
150.673713065512));
#161741=CARTESIAN_POINT('Ctrl Pts',(33.6567152282543,-3.48522689816105,
150.643822845968));
#161742=CARTESIAN_POINT('Ctrl Pts',(33.7342656058241,-3.50880646788727,
150.630148725432));
#161743=CARTESIAN_POINT('Ctrl Pts',(33.8130680689335,-3.5324448583529,150.616253928583));
#161744=CARTESIAN_POINT('Ctrl Pts',(33.8931663711956,-3.55614539415555,
150.602130447634));
#161745=CARTESIAN_POINT('Ctrl Pts',(34.0654983557839,-3.6071372411152,150.571743692455));
#161746=CARTESIAN_POINT('Ctrl Pts',(34.2438282940683,-3.65841587270872,
150.540298707114));
#161747=CARTESIAN_POINT('Ctrl Pts',(34.4285857022663,-3.70997574003565,
150.507721218515));
#161748=CARTESIAN_POINT('Ctrl Pts',(34.5174378428953,-3.73477152293401,
150.492054298164));
#161749=CARTESIAN_POINT('Ctrl Pts',(34.6077762076357,-3.75963167638948,
150.476125439459));
#161750=CARTESIAN_POINT('Ctrl Pts',(34.6996284915187,-3.78455204436383,
150.459929416915));
#161751=CARTESIAN_POINT('Ctrl Pts',(34.8875451472379,-3.83553555844819,
150.42679466769));
#161752=CARTESIAN_POINT('Ctrl Pts',(35.0817980643923,-3.88676991673767,
150.392541997972));
#161753=CARTESIAN_POINT('Ctrl Pts',(35.2826173101892,-3.93819091351075,
150.357132371598));
#161754=CARTESIAN_POINT('Ctrl Pts',(35.3841707649635,-3.96419429704864,
150.33922587127));
#161755=CARTESIAN_POINT('Ctrl Pts',(35.4874032666831,-3.99024409064252,
150.321023457094));
#161756=CARTESIAN_POINT('Ctrl Pts',(35.5923818810437,-4.01634509594526,
150.302512907189));
#161757=CARTESIAN_POINT('Ctrl Pts',(35.7964653212263,-4.06708669685938,
150.266527514095));
#161758=CARTESIAN_POINT('Ctrl Pts',(36.0071475076086,-4.11802152632512,
150.229377874438));
#161759=CARTESIAN_POINT('Ctrl Pts',(36.2249165241759,-4.16915107162306,
150.190979540965));
#161760=CARTESIAN_POINT('Ctrl Pts',(36.3407061067015,-4.19633707263501,
150.170562830303));
#161761=CARTESIAN_POINT('Ctrl Pts',(36.4584992550742,-4.223574957414,150.149793018105));
#161762=CARTESIAN_POINT('Ctrl Pts',(36.5785563414473,-4.25090433708211,
150.128623742154));
#161763=CARTESIAN_POINT('Ctrl Pts',(36.8004411562673,-4.30141342846524,
150.089499513706));
#161764=CARTESIAN_POINT('Ctrl Pts',(37.0300583269974,-4.35223731265307,
150.049011151743));
#161765=CARTESIAN_POINT('Ctrl Pts',(37.2690508250992,-4.40356217142764,
150.006870546684));
#161766=CARTESIAN_POINT('Ctrl Pts',(37.4018946875305,-4.432091068914,149.983446712105));
#161767=CARTESIAN_POINT('Ctrl Pts',(37.5376345268245,-4.46077723240068,
149.959512436394));
#161768=CARTESIAN_POINT('Ctrl Pts',(37.6761845465022,-4.48957184343251,
149.935082274819));
#161769=CARTESIAN_POINT('Ctrl Pts',(37.9217607278213,-4.5406095165863,149.891780470875));
#161770=CARTESIAN_POINT('Ctrl Pts',(38.1761656186326,-4.59198577347407,
149.846920932356));
#161771=CARTESIAN_POINT('Ctrl Pts',(38.4389130596078,-4.64342671970294,
149.800591749672));
#161772=CARTESIAN_POINT('Ctrl Pts',(38.2563686252732,-5.2146737148978,149.893918127215));
#161773=CARTESIAN_POINT('Ctrl Pts',(39.0894774938447,-5.33014235717708,
149.737171640936));
#161774=CARTESIAN_POINT('Ctrl Pts',(41.0081884734667,-5.57912789308956,
149.379459681224));
#161775=CARTESIAN_POINT('Ctrl Pts',(43.8076126339424,-5.89407254053238,
148.867077378471));
#161776=CARTESIAN_POINT('Ctrl Pts',(45.7742555008851,-6.08603592631556,
148.51299562346));
#161777=CARTESIAN_POINT('Ctrl Pts',(46.6545489230723,-6.16674235624256,
148.355562055461));
#161778=CARTESIAN_POINT('Ctrl Pts',(38.4107421964028,-4.21574620337288,
149.656528322788));
#161779=CARTESIAN_POINT('Ctrl Pts',(39.2410978032759,-4.326693041109,149.517014569386));
#161780=CARTESIAN_POINT('Ctrl Pts',(41.1541027316362,-4.56669801382285,
149.198100963248));
#161781=CARTESIAN_POINT('Ctrl Pts',(43.9467860391103,-4.87254124748984,
148.739774565811));
#161782=CARTESIAN_POINT('Ctrl Pts',(45.9095185461389,-5.06048947264209,
148.422110282307));
#161783=CARTESIAN_POINT('Ctrl Pts',(46.7881932180747,-5.13981749100654,
148.280699000599));
#161784=CARTESIAN_POINT('Ctrl Pts',(38.6491896496085,-3.24092093422417,
149.922799308253));
#161785=CARTESIAN_POINT('Ctrl Pts',(39.4753249802897,-3.35550158914587,
149.800373415778));
#161786=CARTESIAN_POINT('Ctrl Pts',(41.3795854643966,-3.60487788190061,
149.519415986963));
#161787=CARTESIAN_POINT('Ctrl Pts',(44.1619431823615,-3.92708203095172,
149.112469591543));
#161788=CARTESIAN_POINT('Ctrl Pts',(46.1186883385217,-4.12806188523935,
148.828465887092));
#161789=CARTESIAN_POINT('Ctrl Pts',(46.9948848783835,-4.21348716646631,
148.701686738985));
#161790=CARTESIAN_POINT('Ctrl Pts',(38.9139099282385,-2.52650125174993,
150.628185440083));
#161791=CARTESIAN_POINT('Ctrl Pts',(39.735380987824,-2.6519904870564,150.51856033928));
#161792=CARTESIAN_POINT('Ctrl Pts',(41.6299783390877,-2.92681832032616,
150.265516112064));
#161793=CARTESIAN_POINT('Ctrl Pts',(44.4009287142964,-3.28687973238183,
149.894819002744));
#161794=CARTESIAN_POINT('Ctrl Pts',(46.3510608975163,-3.51477906248343,
149.633559463568));
#161795=CARTESIAN_POINT('Ctrl Pts',(47.224520637165,-3.61229926883204,149.516475381658));
#161796=CARTESIAN_POINT('Origin',(47.1132772922885,-6.0105076275006,151.317336462008));
#161797=CARTESIAN_POINT('Origin',(80.6089045065798,1.68883371573741,142.364600992296));
#161798=CARTESIAN_POINT('Ctrl Pts',(46.5372798889843,-6.18969355892611,
148.377359242795));
#161799=CARTESIAN_POINT('Ctrl Pts',(46.5530418433047,-6.17420698012464,
148.374439381584));
#161800=CARTESIAN_POINT('Ctrl Pts',(46.5891375270505,-6.14390732156202,
148.366955781747));
#161801=CARTESIAN_POINT('Ctrl Pts',(46.6370786313459,-6.12575715622293,
148.353663770989));
#161802=CARTESIAN_POINT('Ctrl Pts',(46.6799969179442,-6.14247380870429,
148.336241564642));
#161803=CARTESIAN_POINT('Ctrl Pts',(46.7141598403172,-6.19433188653137,
148.314694318236));
#161804=CARTESIAN_POINT('Ctrl Pts',(46.740186434731,-6.28393425976963,148.286265932497));
#161805=CARTESIAN_POINT('Ctrl Pts',(46.7562543404266,-6.41410945175322,
148.247747808364));
#161806=CARTESIAN_POINT('Ctrl Pts',(46.7588839610926,-6.58557960151583,
148.195575967713));
#161807=CARTESIAN_POINT('Ctrl Pts',(46.7429079185317,-6.79517545380282,
148.126545779614));
#161808=CARTESIAN_POINT('Ctrl Pts',(46.7025952223824,-7.02972718747325,
148.040949139118));
#161809=CARTESIAN_POINT('Ctrl Pts',(46.6390661764921,-7.25532850484998,
147.950480251073));
#161810=CARTESIAN_POINT('Ctrl Pts',(46.5838544263694,-7.39557475298945,
147.891484586532));
#161811=CARTESIAN_POINT('Ctrl Pts',(46.5562789209077,-7.45747517935645,
147.865484750416));
#161812=CARTESIAN_POINT('Ctrl Pts',(46.6614159728208,-4.66729930170419,
148.257452201144));
#161813=CARTESIAN_POINT('Ctrl Pts',(46.7082864496826,-4.65394890463263,
148.259742715989));
#161814=CARTESIAN_POINT('Ctrl Pts',(46.8220720189848,-4.63185018237409,
148.258397988294));
#161815=CARTESIAN_POINT('Ctrl Pts',(46.9900857215236,-4.63807663592174,
148.228394581823));
#161816=CARTESIAN_POINT('Ctrl Pts',(47.1476688845866,-4.69207724165032,
148.16235802505));
#161817=CARTESIAN_POINT('Ctrl Pts',(47.268966626375,-4.78579128608015,148.069473219709));
#161818=CARTESIAN_POINT('Ctrl Pts',(47.3488929397349,-4.9165280755285,147.953204928739));
#161819=CARTESIAN_POINT('Ctrl Pts',(47.3795139884807,-5.08012483101266,
147.820397899541));
#161820=CARTESIAN_POINT('Ctrl Pts',(47.3553608942353,-5.27046229206427,
147.680852284493));
#161821=CARTESIAN_POINT('Ctrl Pts',(47.2751162928573,-5.47954989994779,
147.546633237318));
#161822=CARTESIAN_POINT('Ctrl Pts',(47.1459322366506,-5.69408256980547,
147.432441796637));
#161823=CARTESIAN_POINT('Ctrl Pts',(46.9940609684127,-5.8891790323644,147.352132634224));
#161824=CARTESIAN_POINT('Ctrl Pts',(46.8866314685821,-6.00813031043961,
147.315693823849));
#161825=CARTESIAN_POINT('Ctrl Pts',(46.8367952618753,-6.06059112023815,
147.301954032457));
#161826=CARTESIAN_POINT('Ctrl Pts',(46.8710872569602,-3.43668272451928,
149.145776253864));
#161827=CARTESIAN_POINT('Ctrl Pts',(46.9688797033509,-3.43299183240254,
149.149417466047));
#161828=CARTESIAN_POINT('Ctrl Pts',(47.208707877535,-3.436874534301,149.143294412863));
#161829=CARTESIAN_POINT('Ctrl Pts',(47.57336636799,-3.49322218855088,149.073387019189));
#161830=CARTESIAN_POINT('Ctrl Pts',(47.9321847007078,-3.61121601093276,
148.924034453737));
#161831=CARTESIAN_POINT('Ctrl Pts',(48.2304282189886,-3.77344247675182,
148.713447706702));
#161832=CARTESIAN_POINT('Ctrl Pts',(48.4598429050887,-3.97434236430038,
148.445541633467));
#161833=CARTESIAN_POINT('Ctrl Pts',(48.6048887356042,-4.20444485705,148.130362491661));
#161834=CARTESIAN_POINT('Ctrl Pts',(48.6528396833208,-4.45151086311779,
147.783563554233));
#161835=CARTESIAN_POINT('Ctrl Pts',(48.596201214212,-4.7015403993278,147.425907696623));
#161836=CARTESIAN_POINT('Ctrl Pts',(48.4387335772696,-4.93613819975849,
147.087807525499));
#161837=CARTESIAN_POINT('Ctrl Pts',(48.2157364293847,-5.13002728547283,
146.811790570649));
#161838=CARTESIAN_POINT('Ctrl Pts',(48.0410663087532,-5.23832449722567,
146.663304223064));
#161839=CARTESIAN_POINT('Ctrl Pts',(47.9571770914129,-5.28424701090955,
146.602254477145));
#161840=CARTESIAN_POINT('Ctrl Pts',(47.067244768031,-3.07918861709148,150.622686022086));
#161841=CARTESIAN_POINT('Ctrl Pts',(47.211717029689,-3.0881173910915,150.623180181704));
#161842=CARTESIAN_POINT('Ctrl Pts',(47.5663978459836,-3.12348834816712,
150.603618892545));
#161843=CARTESIAN_POINT('Ctrl Pts',(48.1113780735535,-3.23202446786912,
150.489465612828));
#161844=CARTESIAN_POINT('Ctrl Pts',(48.6629381266314,-3.41049029579194,
150.261453965642));
#161845=CARTESIAN_POINT('Ctrl Pts',(49.1443489753141,-3.635520285376,149.942403436868));
#161846=CARTESIAN_POINT('Ctrl Pts',(49.5482221961931,-3.90246681878571,
149.530695579774));
#161847=CARTESIAN_POINT('Ctrl Pts',(49.8535100390613,-4.20074183020728,
149.031213928958));
#161848=CARTESIAN_POINT('Ctrl Pts',(50.0383897472154,-4.51559898034788,
148.455188846487));
#161849=CARTESIAN_POINT('Ctrl Pts',(50.0820805354509,-4.82867960015004,
147.821400051784));
#161850=CARTESIAN_POINT('Ctrl Pts',(49.9702782955123,-5.11394793309396,
147.169851980777));
#161851=CARTESIAN_POINT('Ctrl Pts',(49.7269715640286,-5.33649748624922,
146.584712317804));
#161852=CARTESIAN_POINT('Ctrl Pts',(49.501802503755,-5.44981452949935,146.242505436702));
#161853=CARTESIAN_POINT('Ctrl Pts',(49.3881546506291,-5.49518876667419,
146.096925017937));
#161854=CARTESIAN_POINT('Ctrl Pts',(46.5324438218759,7.52248810062492,147.869391743406));
#161855=CARTESIAN_POINT('Ctrl Pts',(46.5603292779128,7.46045053430261,147.89544515674));
#161856=CARTESIAN_POINT('Ctrl Pts',(46.6159580166382,7.32046069363766,147.95431904588));
#161857=CARTESIAN_POINT('Ctrl Pts',(46.6798388267066,7.09643606942087,148.044098887596));
#161858=CARTESIAN_POINT('Ctrl Pts',(46.7208885772989,6.86371624916407,148.129036809144));
#161859=CARTESIAN_POINT('Ctrl Pts',(46.7379483378916,6.65435052142963,148.198035168892));
#161860=CARTESIAN_POINT('Ctrl Pts',(46.7361607135675,6.48128066160652,148.250639358319));
#161861=CARTESIAN_POINT('Ctrl Pts',(46.7205136063572,6.34960404611417,148.289497564637));
#161862=CARTESIAN_POINT('Ctrl Pts',(46.694714023938,6.2593031987902,148.31804002652));
#161863=CARTESIAN_POINT('Ctrl Pts',(46.6606708856686,6.20711170250637,148.339617470557));
#161864=CARTESIAN_POINT('Ctrl Pts',(46.6177995501911,6.19016220445405,148.357048251876));
#161865=CARTESIAN_POINT('Ctrl Pts',(46.5686258931354,6.20853508983156,148.370685212542));
#161866=CARTESIAN_POINT('Ctrl Pts',(46.5308147637076,6.24060354711479,148.378440266552));
#161867=CARTESIAN_POINT('Ctrl Pts',(46.513318796367,6.25810836185102,148.381614882767));
#161868=CARTESIAN_POINT('Ctrl Pts',(46.817140996116,6.12671552903897,147.305203746767));
#161869=CARTESIAN_POINT('Ctrl Pts',(46.8673279171114,6.07422688234627,147.318945502478));
#161870=CARTESIAN_POINT('Ctrl Pts',(46.9750608726876,5.95569480282076,147.355269739942));
#161871=CARTESIAN_POINT('Ctrl Pts',(47.1266195294122,5.76226877571011,147.434925106998));
#161872=CARTESIAN_POINT('Ctrl Pts',(47.255865560854,5.54983848865781,147.547759376126));
#161873=CARTESIAN_POINT('Ctrl Pts',(47.3376267684437,5.34161667880711,147.680939984286));
#161874=CARTESIAN_POINT('Ctrl Pts',(47.3636311271785,5.14998292950563,147.821022835015));
#161875=CARTESIAN_POINT('Ctrl Pts',(47.3338957106381,4.98465908606635,147.954869946796));
#161876=CARTESIAN_POINT('Ctrl Pts',(47.254316429973,4.85285295357408,148.071673571935));
#161877=CARTESIAN_POINT('Ctrl Pts',(47.1331847450447,4.75839853982045,148.164772631859));
#161878=CARTESIAN_POINT('Ctrl Pts',(46.9757466504496,4.70373740704304,148.230884782075));
#161879=CARTESIAN_POINT('Ctrl Pts',(46.8036079323038,4.69670712590793,148.261696412376));
#161880=CARTESIAN_POINT('Ctrl Pts',(46.6850631980176,4.72028365496785,148.262424896767));
#161881=CARTESIAN_POINT('Ctrl Pts',(46.633692194392,4.73559534664208,148.259359050582));
#161882=CARTESIAN_POINT('Ctrl Pts',(47.9396334410783,5.35422595109969,146.60462115314));
#161883=CARTESIAN_POINT('Ctrl Pts',(48.0239970756342,5.30839102285964,146.665822950002));
#161884=CARTESIAN_POINT('Ctrl Pts',(48.1989133885865,5.20066734658126,146.814095843857));
#161885=CARTESIAN_POINT('Ctrl Pts',(48.4212132744159,5.00858483897843,147.088194437697));
#161886=CARTESIAN_POINT('Ctrl Pts',(48.5791529552626,4.7764715436373,147.422999102021));
#161887=CARTESIAN_POINT('Ctrl Pts',(48.6387109314665,4.52773568939189,147.778764100921));
#161888=CARTESIAN_POINT('Ctrl Pts',(48.5934003704984,4.27903982375646,148.12740068613));
#161889=CARTESIAN_POINT('Ctrl Pts',(48.4490402052191,4.04632339032457,148.44525754295));
#161890=CARTESIAN_POINT('Ctrl Pts',(48.2197557951557,3.84350785940696,148.714483555535));
#161891=CARTESIAN_POINT('Ctrl Pts',(47.9216132493413,3.67976832257381,148.925589113316));
#161892=CARTESIAN_POINT('Ctrl Pts',(47.5630635699461,3.56038028428392,149.075112755935));
#161893=CARTESIAN_POINT('Ctrl Pts',(47.1895622382968,3.50130545071206,149.146868532606));
#161894=CARTESIAN_POINT('Ctrl Pts',(46.9401269640137,3.49770213436046,149.151755253245));
#161895=CARTESIAN_POINT('Ctrl Pts',(46.8332290949316,3.50247108819423,149.146543148058));
#161896=CARTESIAN_POINT('Ctrl Pts',(49.3696542944107,5.56994442846003,146.098600073015));
#161897=CARTESIAN_POINT('Ctrl Pts',(49.4839247680716,5.52472479241387,146.244613426018));
#161898=CARTESIAN_POINT('Ctrl Pts',(49.7093660752448,5.41205425801527,146.586448596255));
#161899=CARTESIAN_POINT('Ctrl Pts',(49.9520523257794,5.19142551199444,147.1677028901));
#161900=CARTESIAN_POINT('Ctrl Pts',(50.0656281080245,4.90895494508271,147.81369289954));
#161901=CARTESIAN_POINT('Ctrl Pts',(50.0265670092713,4.5971859703998,148.445295281496));
#161902=CARTESIAN_POINT('Ctrl Pts',(49.8445238848551,4.27988597809273,149.025039624157));
#161903=CARTESIAN_POINT('Ctrl Pts',(49.5391514088654,3.97786793806996,149.529000627391));
#161904=CARTESIAN_POINT('Ctrl Pts',(49.1349573323231,3.70808382583412,149.94280572139));
#161905=CARTESIAN_POINT('Ctrl Pts',(48.6535017677747,3.48076734080204,150.262656238905));
#161906=CARTESIAN_POINT('Ctrl Pts',(48.102301047001,3.30021419891055,150.490917802173));
#161907=CARTESIAN_POINT('Ctrl Pts',(47.5441635048093,3.18703933991356,150.60804513497));
#161908=CARTESIAN_POINT('Ctrl Pts',(47.1755136133758,3.15040805459456,150.626310541581));
#161909=CARTESIAN_POINT('Ctrl Pts',(47.0176680117271,3.1412650586095,150.624060276346));
#161910=CARTESIAN_POINT('Origin',(47.0941826981424,6.07477576504754,151.320735005098));
#161911=CARTESIAN_POINT('Ctrl Pts',(46.6350328996003,6.23120586969005,148.359003259099));
#161912=CARTESIAN_POINT('Ctrl Pts',(45.724353855216,6.14473278514312,148.521871668148));
#161913=CARTESIAN_POINT('Ctrl Pts',(43.6840233800751,5.93846932051504,148.889307660513));
#161914=CARTESIAN_POINT('Ctrl Pts',(40.885700375115,5.61210790098104,149.401962579257));
#161915=CARTESIAN_POINT('Ctrl Pts',(38.998434282127,5.35951593354733,149.754100140409));
#161916=CARTESIAN_POINT('Ctrl Pts',(38.2399008107496,5.25187133532221,149.896819266026));
#161917=CARTESIAN_POINT('Ctrl Pts',(46.771908326183,5.20474630002223,148.283570245222));
#161918=CARTESIAN_POINT('Ctrl Pts',(45.8628998835332,5.11971407145539,148.429859227114));
#161919=CARTESIAN_POINT('Ctrl Pts',(43.8266248407972,4.91768494165792,148.759481314297));
#161920=CARTESIAN_POINT('Ctrl Pts',(41.0350814900977,4.6006665917656,149.217962899385));
#161921=CARTESIAN_POINT('Ctrl Pts',(39.1534552270697,4.35707271562612,149.531851254533));
#161922=CARTESIAN_POINT('Ctrl Pts',(38.3974166265721,4.25356346129957,149.658875621596));
#161923=CARTESIAN_POINT('Ctrl Pts',(46.9815148757575,4.27883604249698,148.7040456843));
#161924=CARTESIAN_POINT('Ctrl Pts',(46.0750906810986,4.18751069795957,148.835189525106));
#161925=CARTESIAN_POINT('Ctrl Pts',(44.0450879043102,3.97201764509772,149.129836463091));
#161926=CARTESIAN_POINT('Ctrl Pts',(41.2640257099561,3.63882464480218,149.536736352468));
#161927=CARTESIAN_POINT('Ctrl Pts',(39.3911145657453,3.3861418555883,149.813150958076));
#161928=CARTESIAN_POINT('Ctrl Pts',(38.6389304649779,3.27934325045187,149.924608447612));
#161929=CARTESIAN_POINT('Ctrl Pts',(47.2130425126618,3.67792196340846,149.518503505342));
#161930=CARTESIAN_POINT('Ctrl Pts',(46.3094897731806,3.57409502453192,149.639607775137));
#161931=CARTESIAN_POINT('Ctrl Pts',(44.2864556564767,3.33070353610726,149.910596530947));
#161932=CARTESIAN_POINT('Ctrl Pts',(41.5170354178634,2.95973900927576,150.281010112081));
#161933=CARTESIAN_POINT('Ctrl Pts',(39.6538020779683,2.68208351620199,150.529810313275));
#161934=CARTESIAN_POINT('Ctrl Pts',(38.9058977491478,2.56536822628038,150.629602322079));
#161935=CARTESIAN_POINT('Origin',(82.0458803142802,-1.76619892465473,142.111155740591));
#161936=CARTESIAN_POINT('Origin',(26.7764851389615,-2.04263841746052E-14,
151.856993361954));
#161937=CARTESIAN_POINT('',(0.,0.,0.));
#161938=CARTESIAN_POINT('Origin',(69.6316151486327,0.,39.48523201752));
#161939=CARTESIAN_POINT('',(60.7509621221957,-3.44669050145648E-10,42.9650499797481));
#161940=CARTESIAN_POINT('',(60.7214966333422,3.40933537909693E-10,42.7979428885072));
#161941=CARTESIAN_POINT('',(60.4236626579685,-1.14504475720278E-15,41.1088424787055));
#161942=CARTESIAN_POINT('',(60.5714935155857,-0.705868838664094,41.7935745386541));
#161943=CARTESIAN_POINT('Ctrl Pts',(60.7509621221957,-6.89336955246539E-10,
42.9650499797481));
#161944=CARTESIAN_POINT('Ctrl Pts',(60.7509192031534,0.0120680173491838,
42.9648065737692));
#161945=CARTESIAN_POINT('Ctrl Pts',(60.7508994186887,0.0241361063428439,
42.96455982129));
#161946=CARTESIAN_POINT('Ctrl Pts',(60.7509193101621,0.0958428707922907,
42.9630736605288));
#161947=CARTESIAN_POINT('Ctrl Pts',(60.7515007820804,0.155478294986578,
42.9617554993892));
#161948=CARTESIAN_POINT('Ctrl Pts',(60.754942510561,0.334556620519833,42.9575432330028));
#161949=CARTESIAN_POINT('Ctrl Pts',(60.7595036052643,0.453948384734824,
42.9543953553669));
#161950=CARTESIAN_POINT('Ctrl Pts',(60.7761155798191,0.744414997430842,
42.9458647746078));
#161951=CARTESIAN_POINT('Ctrl Pts',(60.7905600076925,0.915297994496103,
42.9401071896087));
#161952=CARTESIAN_POINT('Ctrl Pts',(60.8626996834541,1.55969457761938,42.9154058445961));
#161953=CARTESIAN_POINT('Ctrl Pts',(60.9514830621024,2.02878367975059,42.8912541139455));
#161954=CARTESIAN_POINT('Ctrl Pts',(61.140937930544,2.73404032296258,42.8441574965815));
#161955=CARTESIAN_POINT('Ctrl Pts',(61.2166183987511,2.97638533949813,42.8259430647652));
#161956=CARTESIAN_POINT('Ctrl Pts',(61.3422630634123,3.32828801944589,42.7963719282893));
#161957=CARTESIAN_POINT('Ctrl Pts',(61.3847590529975,3.44050722830918,42.7864610538548));
#161958=CARTESIAN_POINT('Ctrl Pts',(61.4650274392059,3.64085176615261,42.7678894161257));
#161959=CARTESIAN_POINT('Ctrl Pts',(61.5020312261378,3.72928033930315,42.7593781410615));
#161960=CARTESIAN_POINT('Ctrl Pts',(61.5858627862495,3.92133306634782,42.7402000390631));
#161961=CARTESIAN_POINT('Ctrl Pts',(61.633227706131,4.02469541713465,42.7294290408078));
#161962=CARTESIAN_POINT('Ctrl Pts',(61.7850227016679,4.34069982736551,42.6951025985516));
#161963=CARTESIAN_POINT('Ctrl Pts',(61.8955736633756,4.55016508923581,42.6703616834911));
#161964=CARTESIAN_POINT('Ctrl Pts',(62.2085970580832,5.09246338308113,42.6010177453807));
#161965=CARTESIAN_POINT('Ctrl Pts',(62.4239847327386,5.41698247219077,42.55397076249));
#161966=CARTESIAN_POINT('Ctrl Pts',(62.8230995667586,5.94344979920006,42.4683579672737));
#161967=CARTESIAN_POINT('Ctrl Pts',(62.9967249163264,6.15269287100585,42.4315333194129));
#161968=CARTESIAN_POINT('Ctrl Pts',(63.2337305219164,6.41395454682262,42.3820007440121));
#161969=CARTESIAN_POINT('Ctrl Pts',(63.2890445087411,6.47333535521729,42.3704888463692));
#161970=CARTESIAN_POINT('Ctrl Pts',(63.3832206556822,6.57179445517716,42.3509777556499));
#161971=CARTESIAN_POINT('Ctrl Pts',(63.4216679290422,6.61127438489082,42.3430367156097));
#161972=CARTESIAN_POINT('Ctrl Pts',(63.508142132914,6.69848978811027,42.3252314279585));
#161973=CARTESIAN_POINT('Ctrl Pts',(63.5563430576768,6.74604201438635,42.3153431000304));
#161974=CARTESIAN_POINT('Ctrl Pts',(63.717708750903,6.90175862618079,42.2823464393979));
#161975=CARTESIAN_POINT('Ctrl Pts',(63.8330769073322,7.00753318140895,42.2589265241842));
#161976=CARTESIAN_POINT('Ctrl Pts',(64.1504342055915,7.28392522625757,42.1948375781707));
#161977=CARTESIAN_POINT('Ctrl Pts',(64.3570988832823,7.44877621875393,42.1534482115999));
#161978=CARTESIAN_POINT('Ctrl Pts',(64.9248827829799,7.86287678721484,42.0401538531613));
#161979=CARTESIAN_POINT('Ctrl Pts',(65.2970184001635,8.09529916140208,41.9662963731654));
#161980=CARTESIAN_POINT('Ctrl Pts',(65.8052692357616,8.36403058803541,41.8652218846133));
#161981=CARTESIAN_POINT('Ctrl Pts',(65.9280048808312,8.42541753420482,41.8408020108882));
#161982=CARTESIAN_POINT('Ctrl Pts',(66.1394944607363,8.52528278825529,41.7986890799829));
#161983=CARTESIAN_POINT('Ctrl Pts',(66.2275835933159,8.56517237738903,41.7811384899616));
#161984=CARTESIAN_POINT('Ctrl Pts',(66.4106265233465,8.64456456372195,41.7446458447544));
#161985=CARTESIAN_POINT('Ctrl Pts',(66.5056461828842,8.68387380520613,41.7256891366925));
#161986=CARTESIAN_POINT('Ctrl Pts',(66.7617895279916,8.78477571199218,41.6745509061279));
#161987=CARTESIAN_POINT('Ctrl Pts',(66.9239946192751,8.84338317505211,41.642128104044));
#161988=CARTESIAN_POINT('Ctrl Pts',(67.2980024243152,8.96656188810169,41.5672892164927));
#161989=CARTESIAN_POINT('Ctrl Pts',(67.5106660255118,9.0280470415826,41.5246776526347));
#161990=CARTESIAN_POINT('Ctrl Pts',(67.9981555852028,9.14977251804245,41.4269437337242));
#161991=CARTESIAN_POINT('Ctrl Pts',(68.2739360465121,9.20508480570872,41.3716133115562));
#161992=CARTESIAN_POINT('Ctrl Pts',(68.8571890355632,9.29391505157166,41.2547772168552));
#161993=CARTESIAN_POINT('Ctrl Pts',(69.1647254071317,9.32467141193665,41.1932766810052));
#161994=CARTESIAN_POINT('Ctrl Pts',(69.5647089889984,9.3439623287347,41.1137500170015));
#161995=CARTESIAN_POINT('Ctrl Pts',(69.6562243240114,9.34697706212247,41.0955861650997));
#161996=CARTESIAN_POINT('Ctrl Pts',(69.8013386906838,9.34954143049101,41.0668464675245));
#161997=CARTESIAN_POINT('Ctrl Pts',(69.8549111944427,9.3500097683724,41.0562499923985));
#161998=CARTESIAN_POINT('Ctrl Pts',(69.9624342094911,9.34998985422666,41.0350125729487));
#161999=CARTESIAN_POINT('Ctrl Pts',(70.0163826392544,9.34949496796775,41.0243722134257));
#162000=CARTESIAN_POINT('Ctrl Pts',(70.1637306170531,9.34681879104554,40.9953469065423));
#162001=CARTESIAN_POINT('Ctrl Pts',(70.2571117094745,9.34366884165001,40.9769922278763));
#162002=CARTESIAN_POINT('Ctrl Pts',(70.6773069937479,9.3229461074411,40.8945362718053));
#162003=CARTESIAN_POINT('Ctrl Pts',(71.0031659378946,9.28902180796155,40.8309570144352));
#162004=CARTESIAN_POINT('Ctrl Pts',(71.8674102576155,9.15116326016299,40.662325578389));
#162005=CARTESIAN_POINT('Ctrl Pts',(72.3995994001381,9.01576763460601,40.5584222401047));
#162006=CARTESIAN_POINT('Ctrl Pts',(73.0476815844185,8.78648593714721,40.4304890949787));
#162007=CARTESIAN_POINT('Ctrl Pts',(73.1777328614347,8.73707433129832,40.4047472757752));
#162008=CARTESIAN_POINT('Ctrl Pts',(73.3956105142267,8.64849654971577,40.3614910708849));
#162009=CARTESIAN_POINT('Ctrl Pts',(73.484032373736,8.61089910502389,40.343899276431));
#162010=CARTESIAN_POINT('Ctrl Pts',(73.6649595495966,8.53054732173658,40.3078240856901));
#162011=CARTESIAN_POINT('Ctrl Pts',(73.7573777406432,8.4876244032667,40.2893532515719));
#162012=CARTESIAN_POINT('Ctrl Pts',(74.0004265282063,8.36972470535843,40.2406604292785));
#162013=CARTESIAN_POINT('Ctrl Pts',(74.1497584237987,8.29208704341949,40.2106215816142));
#162014=CARTESIAN_POINT('Ctrl Pts',(74.3981966281126,8.15402855962329,40.1604500397329));
#162015=CARTESIAN_POINT('Ctrl Pts',(74.4984336502322,8.0957921161285,40.1401514742407));
#162016=CARTESIAN_POINT('Ctrl Pts',(74.9481911429238,7.82287096350835,40.0488374021029));
#162017=CARTESIAN_POINT('Ctrl Pts',(75.2843906030439,7.58645787724419,39.9798997485762));
#162018=CARTESIAN_POINT('Ctrl Pts',(75.7911853466634,7.17657396715865,39.8754833888091));
#162019=CARTESIAN_POINT('Ctrl Pts',(75.9725038848175,7.01774795338829,39.8380182132098));
#162020=CARTESIAN_POINT('Ctrl Pts',(76.2051496289845,6.79727004618545,39.7899602723674));
#162021=CARTESIAN_POINT('Ctrl Pts',(76.2620722196148,6.74191519448013,39.7782029879682));
#162022=CARTESIAN_POINT('Ctrl Pts',(76.3571718770091,6.64702290325669,39.7585707422223));
#162023=CARTESIAN_POINT('Ctrl Pts',(76.3957140468795,6.60787434334059,39.7506174578851));
#162024=CARTESIAN_POINT('Ctrl Pts',(76.4817438056552,6.5189226116427,39.7328737856309));
#162025=CARTESIAN_POINT('Ctrl Pts',(76.5290332059677,6.46892525082887,39.7231256672476));
#162026=CARTESIAN_POINT('Ctrl Pts',(76.6874077606057,6.29770311810571,39.690484170149));
#162027=CARTESIAN_POINT('Ctrl Pts',(76.795877004395,6.17399840367566,39.668137262632));
#162028=CARTESIAN_POINT('Ctrl Pts',(77.0857415310214,5.82513715987257,39.6083099896063));
#162029=CARTESIAN_POINT('Ctrl Pts',(77.2601226654631,5.59416944127951,39.5721887525485));
#162030=CARTESIAN_POINT('Ctrl Pts',(77.6515396006687,5.02212018218087,39.4902450361049));
#162031=CARTESIAN_POINT('Ctrl Pts',(77.8578449431254,4.67415547923311,39.4462921317525));
#162032=CARTESIAN_POINT('Ctrl Pts',(78.1046014984847,4.18871023810343,39.3920498018891));
#162033=CARTESIAN_POINT('Ctrl Pts',(78.1652837158995,4.06238592074089,39.3785453154062));
#162034=CARTESIAN_POINT('Ctrl Pts',(78.2631915831818,3.84626793852728,39.3564489184212));
#162035=CARTESIAN_POINT('Ctrl Pts',(78.3018888151383,3.75719145402448,39.3476241340115));
#162036=CARTESIAN_POINT('Ctrl Pts',(78.3789448603873,3.57199554854562,39.3298527285725));
#162037=CARTESIAN_POINT('Ctrl Pts',(78.4171123309928,3.47580805464009,39.3209367916894));
#162038=CARTESIAN_POINT('Ctrl Pts',(78.5141091029915,3.21905713401295,39.2979627927361));
#162039=CARTESIAN_POINT('Ctrl Pts',(78.5701699844634,3.05745132674366,39.2843453283008));
#162040=CARTESIAN_POINT('Ctrl Pts',(78.7155991001841,2.59812914572263,39.2479997830359));
#162041=CARTESIAN_POINT('Ctrl Pts',(78.7947105803263,2.29727335994955,39.2269254188885));
#162042=CARTESIAN_POINT('Ctrl Pts',(78.9676427614793,1.47685659793284,39.1769607291523));
#162043=CARTESIAN_POINT('Ctrl Pts',(79.0331076349819,0.952189915331092,
39.1528860741283));
#162044=CARTESIAN_POINT('Ctrl Pts',(79.0584314102317,0.334455309251635,
39.1348128756305));
#162045=CARTESIAN_POINT('Ctrl Pts',(79.0608456650541,0.244315143102979,
39.1324313915528));
#162046=CARTESIAN_POINT('Ctrl Pts',(79.0626614058751,0.100181503155015,
39.129042836859));
#162047=CARTESIAN_POINT('Ctrl Pts',(79.06288328759,0.0462077443700452,39.1278679029619));
#162048=CARTESIAN_POINT('Ctrl Pts',(79.0624040527268,-0.0634553533171274,
39.1256746394488));
#162049=CARTESIAN_POINT('Ctrl Pts',(79.0616733962745,-0.119142365220631,
39.12466236035));
#162050=CARTESIAN_POINT('Ctrl Pts',(79.0582951870379,-0.27354429590103,
39.1221316435911));
#162051=CARTESIAN_POINT('Ctrl Pts',(79.0546026174417,-0.372232464434601,
39.1208270165568));
#162052=CARTESIAN_POINT('Ctrl Pts',(79.0424605751304,-0.601370998227225,
39.1185009079195));
#162053=CARTESIAN_POINT('Ctrl Pts',(79.0328599279125,-0.731741890152604,
39.1177077803513));
#162054=CARTESIAN_POINT('Ctrl Pts',(78.986046386072,-1.22772338659078,39.1166269345832));
#162055=CARTESIAN_POINT('Ctrl Pts',(78.9303567892656,-1.59125959251295,
39.1198472086018));
#162056=CARTESIAN_POINT('Ctrl Pts',(78.7686414432441,-2.34953855474448,
39.1342001747182));
#162057=CARTESIAN_POINT('Ctrl Pts',(78.657917495894,-2.74248264257331,39.1461433744119));
#162058=CARTESIAN_POINT('Ctrl Pts',(78.4781970545509,-3.25155709505892,
39.1672246498674));
#162059=CARTESIAN_POINT('Ctrl Pts',(78.4315853149677,-3.375252006404,39.1728042309735));
#162060=CARTESIAN_POINT('Ctrl Pts',(78.3462069440908,-3.58815734979082,
39.1831984435764));
#162061=CARTESIAN_POINT('Ctrl Pts',(78.3086271336934,-3.67783015233958,
39.1878250506795));
#162062=CARTESIAN_POINT('Ctrl Pts',(78.2268128667642,-3.86488574142884,
39.19799958543));
#162063=CARTESIAN_POINT('Ctrl Pts',(78.1822950065419,-3.96212685525035,
39.2035926000933));
#162064=CARTESIAN_POINT('Ctrl Pts',(78.0535514226896,-4.23114731727244,
39.2199194829015));
#162065=CARTESIAN_POINT('Ctrl Pts',(77.9657471341904,-4.40112023962495,
39.2312221766895));
#162066=CARTESIAN_POINT('Ctrl Pts',(77.7444449990251,-4.79927820762073,
39.2601108414533));
#162067=CARTESIAN_POINT('Ctrl Pts',(77.6064098334748,-5.02469947435709,
39.2784322307871));
#162068=CARTESIAN_POINT('Ctrl Pts',(77.19973334068,-5.63000120720818,39.3333862918379));
#162069=CARTESIAN_POINT('Ctrl Pts',(76.9122235887559,-5.99598527899814,
39.373244174817));
#162070=CARTESIAN_POINT('Ctrl Pts',(76.5419422192553,-6.40142050268571,
39.4265192775781));
#162071=CARTESIAN_POINT('Ctrl Pts',(76.4839137265088,-6.46325055282909,
39.4349196139379));
#162072=CARTESIAN_POINT('Ctrl Pts',(76.3863446747382,-6.56442284904681,
39.4491373703105));
#162073=CARTESIAN_POINT('Ctrl Pts',(76.3472706056982,-6.60422189491118,
39.4548555087303));
#162074=CARTESIAN_POINT('Ctrl Pts',(76.2609901857356,-6.69054611573872,
39.4675367622796));
#162075=CARTESIAN_POINT('Ctrl Pts',(76.2136431890314,-6.73692078537221,
39.4745300494353));
#162076=CARTESIAN_POINT('Ctrl Pts',(76.0608825130346,-6.88339300460807,
39.4971912394676));
#162077=CARTESIAN_POINT('Ctrl Pts',(75.9536540435158,-6.98150601388505,
39.5132440086012));
#162078=CARTESIAN_POINT('Ctrl Pts',(75.6692571413004,-7.22975679850689,
39.5561046507005));
#162079=CARTESIAN_POINT('Ctrl Pts',(75.4887461962047,-7.37579187955797,
39.5835819795774));
#162080=CARTESIAN_POINT('Ctrl Pts',(74.9035266768229,-7.81395952585248,
39.6731189579654));
#162081=CARTESIAN_POINT('Ctrl Pts',(74.4809154638828,-8.0800089184283,39.738385719014));
#162082=CARTESIAN_POINT('Ctrl Pts',(73.9196702373565,-8.37272654588218,
39.824788668525));
#162083=CARTESIAN_POINT('Ctrl Pts',(73.7988255123913,-8.43241287021897,
39.8433809212834));
#162084=CARTESIAN_POINT('Ctrl Pts',(73.5889671351575,-8.53038473369496,
39.8756351846373));
#162085=CARTESIAN_POINT('Ctrl Pts',(73.5005690548199,-8.56996321432973,
39.8892118287083));
#162086=CARTESIAN_POINT('Ctrl Pts',(73.3153955474117,-8.64937968836004,
39.9176281211049));
#162087=CARTESIAN_POINT('Ctrl Pts',(73.2185330405093,-8.68897527875358,
39.932479222441));
#162088=CARTESIAN_POINT('Ctrl Pts',(72.9532887314133,-8.79214497941568,
39.9731089000321));
#162089=CARTESIAN_POINT('Ctrl Pts',(72.7837008382284,-8.85242664272219,
39.9990444158494));
#162090=CARTESIAN_POINT('Ctrl Pts',(72.3887303907514,-8.97986140418576,
40.0593643646413));
#162091=CARTESIAN_POINT('Ctrl Pts',(72.1623350021658,-9.04340297899018,
40.0938768823119));
#162092=CARTESIAN_POINT('Ctrl Pts',(71.617239510483,-9.17399727929768,40.1769217691508));
#162093=CARTESIAN_POINT('Ctrl Pts',(71.2969423699594,-9.23288913498765,
40.2256738259159));
#162094=CARTESIAN_POINT('Ctrl Pts',(70.7033554107673,-9.30959810348645,
40.3163214480786));
#162095=CARTESIAN_POINT('Ctrl Pts',(70.4310517712827,-9.33245101807529,
40.3580215670076));
#162096=CARTESIAN_POINT('Ctrl Pts',(70.0799811772284,-9.34612410411519,
40.4121596413414));
#162097=CARTESIAN_POINT('Ctrl Pts',(70.001735239084,-9.34816517330635,40.4242500444604));
#162098=CARTESIAN_POINT('Ctrl Pts',(69.8725958771397,-9.3498737679233,40.4442521743555));
#162099=CARTESIAN_POINT('Ctrl Pts',(69.8217112419767,-9.35012180670517,
40.4521459348212));
#162100=CARTESIAN_POINT('Ctrl Pts',(69.7125019630862,-9.34974153666798,
40.4691163164953));
#162101=CARTESIAN_POINT('Ctrl Pts',(69.6541811516513,-9.34897972012343,
40.4781960324333));
#162102=CARTESIAN_POINT('Ctrl Pts',(69.4812061468428,-9.34506246656331,
40.5051693708976));
#162103=CARTESIAN_POINT('Ctrl Pts',(69.3666051402666,-9.34030547782814,
40.5230967975248));
#162104=CARTESIAN_POINT('Ctrl Pts',(69.0899791244209,-9.32359642814478,
40.5664658603422));
#162105=CARTESIAN_POINT('Ctrl Pts',(68.9281266169439,-9.30947603019504,
40.5919200340261));
#162106=CARTESIAN_POINT('Ctrl Pts',(68.4535834696805,-9.25528136736339,
40.6666497535579));
#162107=CARTESIAN_POINT('Ctrl Pts',(68.1424690042874,-9.20332329564257,
40.7157652313149));
#162108=CARTESIAN_POINT('Ctrl Pts',(67.4541103344533,-9.05141408180703,
40.8241020605481));
#162109=CARTESIAN_POINT('Ctrl Pts',(67.079248786922,-8.94319346340559,40.88286021374));
#162110=CARTESIAN_POINT('Ctrl Pts',(66.5890744650842,-8.76715364547078,
40.9589555376969));
#162111=CARTESIAN_POINT('Ctrl Pts',(66.4669152086575,-8.72031254626882,
40.977858292704));
#162112=CARTESIAN_POINT('Ctrl Pts',(66.2565687644482,-8.63446293028694,
41.0102901458141));
#162113=CARTESIAN_POINT('Ctrl Pts',(66.1679313543636,-8.59665178470926,
41.0239198038748));
#162114=CARTESIAN_POINT('Ctrl Pts',(65.9829628097528,-8.5142907182108,41.05228233946));
#162115=CARTESIAN_POINT('Ctrl Pts',(65.8867712277192,-8.46945191562868,
41.0669856909708));
#162116=CARTESIAN_POINT('Ctrl Pts',(65.6204485629991,-8.33966229462194,
41.1075638238008));
#162117=CARTESIAN_POINT('Ctrl Pts',(65.4520932642186,-8.25107386304867,
41.133063066968));
#162118=CARTESIAN_POINT('Ctrl Pts',(65.0574591954392,-8.02758609051135,
41.1924926723887));
#162119=CARTESIAN_POINT('Ctrl Pts',(64.8339111359362,-7.88805833575394,
41.22587649101));
#162120=CARTESIAN_POINT('Ctrl Pts',(64.2352897386876,-7.47793010934565,
41.3146801886983));
#162121=CARTESIAN_POINT('Ctrl Pts',(63.8737831585359,-7.18835011748932,
41.3676081483287));
#162122=CARTESIAN_POINT('Ctrl Pts',(63.4732300941808,-6.81510724127859,
41.4262442735139));
#162123=CARTESIAN_POINT('Ctrl Pts',(63.4121166986949,-6.75658119731008,
41.4351912912859));
#162124=CARTESIAN_POINT('Ctrl Pts',(63.3120719743635,-6.65811700365124,
41.4498486271939));
#162125=CARTESIAN_POINT('Ctrl Pts',(63.2726899351033,-6.61865330596437,
41.4556214666843));
#162126=CARTESIAN_POINT('Ctrl Pts',(63.1872159229516,-6.53144649699522,
41.4681597250115));
#162127=CARTESIAN_POINT('Ctrl Pts',(63.1412742178653,-6.4835585285477,41.474904062577));
#162128=CARTESIAN_POINT('Ctrl Pts',(62.9959937969129,-6.32884420324721,
41.4962373956945));
#162129=CARTESIAN_POINT('Ctrl Pts',(62.8986331836758,-6.22015213650578,
41.5105428502645));
#162130=CARTESIAN_POINT('Ctrl Pts',(62.6520250972985,-5.93149374318229,
41.5467136236367));
#162131=CARTESIAN_POINT('Ctrl Pts',(62.5068781974154,-5.74808174746316,
41.5679366968159));
#162132=CARTESIAN_POINT('Ctrl Pts',(62.0738696639912,-5.15670710711674,
41.630652562326));
#162133=CARTESIAN_POINT('Ctrl Pts',(61.8113955772076,-4.73079800418125,
41.6677164516398));
#162134=CARTESIAN_POINT('Ctrl Pts',(61.5217418649459,-4.16471875358986,
41.7062671022462));
#162135=CARTESIAN_POINT('Ctrl Pts',(61.4624250766333,-4.04235722803926,
41.7140076263576));
#162136=CARTESIAN_POINT('Ctrl Pts',(61.3650484619538,-3.82994348226314,
41.7264252181212));
#162137=CARTESIAN_POINT('Ctrl Pts',(61.3257143237137,-3.74051480215264,
41.7313502454636));
#162138=CARTESIAN_POINT('Ctrl Pts',(61.2467825581074,-3.55325405699004,
41.7410341029529));
#162139=CARTESIAN_POINT('Ctrl Pts',(61.2074208088727,-3.45533516128047,
41.7457474788098));
#162140=CARTESIAN_POINT('Ctrl Pts',(61.1048735628266,-3.18739655600134,
41.7576970162287));
#162141=CARTESIAN_POINT('Ctrl Pts',(61.0449066804154,-3.01616693201691,
41.7643101649349));
#162142=CARTESIAN_POINT('Ctrl Pts',(60.76897626378,-2.14942954181391,41.792733402383));
#162143=CARTESIAN_POINT('Ctrl Pts',(60.6284535303241,-1.43210428208144,
41.7999744970083));
#162144=CARTESIAN_POINT('Ctrl Pts',(60.5714935164259,-0.705868838607116,
41.7935745380961));
#162145=CARTESIAN_POINT('',(64.7021225441964,-7.81768501240386,41.0652331929315));
#162146=CARTESIAN_POINT('Origin',(69.7531688729995,0.,40.1745974446286));
#162147=CARTESIAN_POINT('Ctrl Pts',(64.7021225443845,-7.81768501217606,
41.0652331931716));
#162148=CARTESIAN_POINT('Ctrl Pts',(64.9099291419011,-7.95559121670532,
41.0332711740937));
#162149=CARTESIAN_POINT('Ctrl Pts',(65.1231278425908,-8.08495767398618,
41.0004097291694));
#162150=CARTESIAN_POINT('Ctrl Pts',(65.4716214575531,-8.27753191386777,
40.9467318773754));
#162151=CARTESIAN_POINT('Ctrl Pts',(65.603709879995,-8.3463928018554,40.9263939606144));
#162152=CARTESIAN_POINT('Ctrl Pts',(65.8191483003094,-8.45213403987724,
40.8932548174706));
#162153=CARTESIAN_POINT('Ctrl Pts',(65.901493765702,-8.49104321942166,40.8805955987882));
#162154=CARTESIAN_POINT('Ctrl Pts',(66.0710906980177,-8.56811717995667,
40.8545417556752));
#162155=CARTESIAN_POINT('Ctrl Pts',(66.1583839475758,-8.60616165819395,
40.8411415749923));
#162156=CARTESIAN_POINT('Ctrl Pts',(66.3536718854519,-8.6876826377093,40.8111883826705));
#162157=CARTESIAN_POINT('Ctrl Pts',(66.4619292521254,-8.73047428214599,
40.7946006703207));
#162158=CARTESIAN_POINT('Ctrl Pts',(66.8094118826833,-8.86023810010581,
40.7414125136883));
#162159=CARTESIAN_POINT('Ctrl Pts',(67.0514066100683,-8.93930042173176,
40.7044557862505));
#162160=CARTESIAN_POINT('Ctrl Pts',(67.7571047729953,-9.13776017779192,
40.5968433952722));
#162161=CARTESIAN_POINT('Ctrl Pts',(68.2271730990255,-9.23099027745907,
40.5253868666142));
#162162=CARTESIAN_POINT('Ctrl Pts',(68.8701978555925,-9.3068500034002,40.4271135316917));
#162163=CARTESIAN_POINT('Ctrl Pts',(69.0387136091781,-9.32200436187663,
40.4013064915722));
#162164=CARTESIAN_POINT('Ctrl Pts',(69.3252255904355,-9.33977352546646,
40.3572696612854));
#162165=CARTESIAN_POINT('Ctrl Pts',(69.4430414418329,-9.34479432053206,
40.3391156491253));
#162166=CARTESIAN_POINT('Ctrl Pts',(69.6198086283044,-9.3489025349949,40.3117858493284));
#162167=CARTESIAN_POINT('Ctrl Pts',(69.6787161997998,-9.34970163172074,
40.3026628616066));
#162168=CARTESIAN_POINT('Ctrl Pts',(69.7888923395229,-9.35013034127187,
40.2855673639611));
#162169=CARTESIAN_POINT('Ctrl Pts',(69.8401580478434,-9.34989819149722,
40.2775991082422));
#162170=CARTESIAN_POINT('Ctrl Pts',(69.9688753128024,-9.34823141733855,
40.2575613890772));
#162171=CARTESIAN_POINT('Ctrl Pts',(70.0463135826783,-9.34624290081183,
40.2454783741426));
#162172=CARTESIAN_POINT('Ctrl Pts',(70.3993749270469,-9.3326790162918,40.19028576075));
#162173=CARTESIAN_POINT('Ctrl Pts',(70.6743840483041,-9.30960096897578,
40.1470112001541));
#162174=CARTESIAN_POINT('Ctrl Pts',(71.2703390126847,-9.2322717327853,40.0531019595741));
#162175=CARTESIAN_POINT('Ctrl Pts',(71.590305634569,-9.17324724574807,40.0026016387007));
#162176=CARTESIAN_POINT('Ctrl Pts',(72.1342576688283,-9.04258086023592,
39.9170961119826));
#162177=CARTESIAN_POINT('Ctrl Pts',(72.3598283403125,-8.97914977186504,
39.8817416784996));
#162178=CARTESIAN_POINT('Ctrl Pts',(72.7536004321475,-8.85194623240719,
39.8203334737841));
#162179=CARTESIAN_POINT('Ctrl Pts',(72.9227897736543,-8.79175455627838,
39.7940518883034));
#162180=CARTESIAN_POINT('Ctrl Pts',(73.187586112548,-8.68870822660458,39.7531134933955));
#162181=CARTESIAN_POINT('Ctrl Pts',(73.2843758934491,-8.64912815850986,
39.7381913937325));
#162182=CARTESIAN_POINT('Ctrl Pts',(73.4695020748567,-8.56971438833897,
39.7097354223797));
#162183=CARTESIAN_POINT('Ctrl Pts',(73.5579232081475,-8.53012038003188,
39.6961821917585));
#162184=CARTESIAN_POINT('Ctrl Pts',(73.7679775496655,-8.43205304801048,
39.6640779187476));
#162185=CARTESIAN_POINT('Ctrl Pts',(73.8889993798093,-8.37228111383074,
39.64565720777));
#162186=CARTESIAN_POINT('Ctrl Pts',(74.4485702831968,-8.08046556722084,
39.5608356485478));
#162187=CARTESIAN_POINT('Ctrl Pts',(74.8696942638692,-7.81573964254023,
39.4980731132566));
#162188=CARTESIAN_POINT('Ctrl Pts',(75.454875964055,-7.37857536573221,39.4117729182769));
#162189=CARTESIAN_POINT('Ctrl Pts',(75.6365741059568,-7.23184311479738,
39.3851123634291));
#162190=CARTESIAN_POINT('Ctrl Pts',(75.9225061442735,-6.98254187786002,
39.343228249221));
#162191=CARTESIAN_POINT('Ctrl Pts',(76.0301526622264,-6.88413152250635,
39.3274768518852));
#162192=CARTESIAN_POINT('Ctrl Pts',(76.1833606321964,-6.73729819969614,
39.305043322013));
#162193=CARTESIAN_POINT('Ctrl Pts',(76.2307711450976,-6.69087619095716,
39.298098948135));
#162194=CARTESIAN_POINT('Ctrl Pts',(76.317098467256,-6.60451828615961,39.2854448903652));
#162195=CARTESIAN_POINT('Ctrl Pts',(76.3561589204221,-6.56473437913438,
39.2797151301512));
#162196=CARTESIAN_POINT('Ctrl Pts',(76.4536035861444,-6.46368276944742,
39.2654136889022));
#162197=CARTESIAN_POINT('Ctrl Pts',(76.5115183804176,-6.40196036492774,
39.2569075548689));
#162198=CARTESIAN_POINT('Ctrl Pts',(76.8808383246451,-5.99744671559585,
39.2026671252686));
#162199=CARTESIAN_POINT('Ctrl Pts',(77.1673940716131,-5.63236890441859,
39.160622292212));
#162200=CARTESIAN_POINT('Ctrl Pts',(77.5736339895177,-5.02746590723789,
39.1025512176068));
#162201=CARTESIAN_POINT('Ctrl Pts',(77.7119571976737,-4.80142944591827,
39.0831248645218));
#162202=CARTESIAN_POINT('Ctrl Pts',(77.9336393552404,-4.4023387739747,39.0528268008962));
#162203=CARTESIAN_POINT('Ctrl Pts',(78.0215496001567,-4.23207139359831,
39.0410830962408));
#162204=CARTESIAN_POINT('Ctrl Pts',(78.1504193277892,-3.96270033470048,
39.0243574396474));
#162205=CARTESIAN_POINT('Ctrl Pts',(78.194953326286,-3.86540989880228,39.0186813393949));
#162206=CARTESIAN_POINT('Ctrl Pts',(78.2767867924039,-3.67832186678483,
39.0084620556804));
#162207=CARTESIAN_POINT('Ctrl Pts',(78.3143701387671,-3.58866678618905,
39.0038633281515));
#162208=CARTESIAN_POINT('Ctrl Pts',(78.3997376988653,-3.37590375714255,
38.993651629148));
#162209=CARTESIAN_POINT('Ctrl Pts',(78.4463465042021,-3.25233589412948,
38.9882663416327));
#162210=CARTESIAN_POINT('Ctrl Pts',(78.6212760349658,-2.75753448491971,
38.9688513028008));
#162211=CARTESIAN_POINT('Ctrl Pts',(78.7291329471674,-2.37934168111355,
38.9587759037915));
#162212=CARTESIAN_POINT('Ctrl Pts',(78.8803588050422,-1.6894245788458,38.9484853562719));
#162213=CARTESIAN_POINT('Ctrl Pts',(78.9322711270322,-1.38019536582268,
38.9466867740245));
#162214=CARTESIAN_POINT('Ctrl Pts',(78.9883945982626,-0.901753143507995,
38.9478980353824));
#162215=CARTESIAN_POINT('Ctrl Pts',(79.0035527398303,-0.734046478088404,
38.9490662801639));
#162216=CARTESIAN_POINT('Ctrl Pts',(79.021712735615,-0.448293177242299,
38.9522526504847));
#162217=CARTESIAN_POINT('Ctrl Pts',(79.0269932488723,-0.330427808422369,
38.9539114528656));
#162218=CARTESIAN_POINT('Ctrl Pts',(79.031612637129,-0.153153714515487,
38.9569014565597));
#162219=CARTESIAN_POINT('Ctrl Pts',(79.0325998969399,-0.0937954228283715,
38.9579859742503));
#162220=CARTESIAN_POINT('Ctrl Pts',(79.0333974134861,0.0169279385186524,
38.9601606884374));
#162221=CARTESIAN_POINT('Ctrl Pts',(79.0333482878283,0.0682895297017857,
38.9612299826708));
#162222=CARTESIAN_POINT('Ctrl Pts',(79.0321661367575,0.198021635936845,
38.9640866420856));
#162223=CARTESIAN_POINT('Ctrl Pts',(79.0304765796834,0.276381359886681,
38.9659559926883));
#162224=CARTESIAN_POINT('Ctrl Pts',(79.0183263209127,0.633666418580387,
38.9751601075958));
#162225=CARTESIAN_POINT('Ctrl Pts',(78.9964906347116,0.912015756738901,
38.9842273615322));
#162226=CARTESIAN_POINT('Ctrl Pts',(78.9222459742806,1.51522758868374,39.0084924607264));
#162227=CARTESIAN_POINT('Ctrl Pts',(78.8651299927986,1.83910243806911,39.0244819773412));
#162228=CARTESIAN_POINT('Ctrl Pts',(78.738228402067,2.38963678298835,39.0572660187727));
#162229=CARTESIAN_POINT('Ctrl Pts',(78.6765170601622,2.61791813564908,39.0725671268995));
#162230=CARTESIAN_POINT('Ctrl Pts',(78.5526188365452,3.01636894768214,39.10243812103));
#162231=CARTESIAN_POINT('Ctrl Pts',(78.4939490887731,3.18755085990217,39.1163342253296));
#162232=CARTESIAN_POINT('Ctrl Pts',(78.3934522651991,3.4554322822175,39.139806851963));
#162233=CARTESIAN_POINT('Ctrl Pts',(78.3548402839376,3.55334265931871,39.1487597334953));
#162234=CARTESIAN_POINT('Ctrl Pts',(78.2773489730381,3.74059758915825,39.1666103102783));
#162235=CARTESIAN_POINT('Ctrl Pts',(78.2387049339176,3.83002894642994,39.1754620993184));
#162236=CARTESIAN_POINT('Ctrl Pts',(78.1429709962522,4.04246734706523,39.1972765608363));
#162237=CARTESIAN_POINT('Ctrl Pts',(78.084606054502,4.16484966159054,39.2104865870434));
#162238=CARTESIAN_POINT('Ctrl Pts',(77.799593871057,4.73064365405723,39.274587699024));
#162239=CARTESIAN_POINT('Ctrl Pts',(77.5408584132845,5.15626362949474,39.3317025860928));
#162240=CARTESIAN_POINT('Ctrl Pts',(77.1132252810091,5.74753951385887,39.4239889135004));
#162241=CARTESIAN_POINT('Ctrl Pts',(76.9696401386509,5.93110941779543,39.4546846524212));
#162242=CARTESIAN_POINT('Ctrl Pts',(76.7255830412657,6.21997401145938,39.5062520219091));
#162243=CARTESIAN_POINT('Ctrl Pts',(76.6292193151011,6.32872124860053,39.5264731620379));
#162244=CARTESIAN_POINT('Ctrl Pts',(76.4853992540915,6.48349819894039,39.5564137181252));
#162245=CARTESIAN_POINT('Ctrl Pts',(76.4399244267392,6.53139445419446,39.5658475399373));
#162246=CARTESIAN_POINT('Ctrl Pts',(76.3553175251908,6.61860772924905,39.5833338009163));
#162247=CARTESIAN_POINT('Ctrl Pts',(76.3163360324784,6.65806970019674,39.5913649406049));
#162248=CARTESIAN_POINT('Ctrl Pts',(76.2173125465778,6.75651711073263,39.6117061275029));
#162249=CARTESIAN_POINT('Ctrl Pts',(76.1568198200928,6.81502888792346,39.6240784272744));
#162250=CARTESIAN_POINT('Ctrl Pts',(75.7603141335445,7.18815527664897,39.7048736748925));
#162251=CARTESIAN_POINT('Ctrl Pts',(75.4022350063728,7.47765755901793,39.7764953298718));
#162252=CARTESIAN_POINT('Ctrl Pts',(74.8088414438977,7.88781000732387,39.8946865986885));
#162253=CARTESIAN_POINT('Ctrl Pts',(74.5870866063093,8.0274060971477,39.9387517479531));
#162254=CARTESIAN_POINT('Ctrl Pts',(74.1955604120527,8.25098287144491,40.0165789033074));
#162255=CARTESIAN_POINT('Ctrl Pts',(74.0285217136279,8.33959720428372,40.0497895890592));
#162256=CARTESIAN_POINT('Ctrl Pts',(73.764267943593,8.46941388715207,40.1023822276028));
#162257=CARTESIAN_POINT('Ctrl Pts',(73.6688276635238,8.51425702044499,40.1213873714215));
#162258=CARTESIAN_POINT('Ctrl Pts',(73.4853018342307,8.59662186686805,40.1579580924078));
#162259=CARTESIAN_POINT('Ctrl Pts',(73.3973556988506,8.63443279574562,40.1754935984856));
#162260=CARTESIAN_POINT('Ctrl Pts',(73.1886531466785,8.72027658717094,40.2171343876706));
#162261=CARTESIAN_POINT('Ctrl Pts',(73.0674472993297,8.76711237113641,40.2413393450917));
#162262=CARTESIAN_POINT('Ctrl Pts',(72.5821328152752,8.94275033976013,40.338342781684));
#162263=CARTESIAN_POINT('Ctrl Pts',(72.2112304326012,9.05071485767094,40.4126851785677));
#162264=CARTESIAN_POINT('Ctrl Pts',(71.534686762407,9.20141362361004,40.5483505088428));
#162265=CARTESIAN_POINT('Ctrl Pts',(71.2314905750788,9.25284220495611,40.6091652611431));
#162266=CARTESIAN_POINT('Ctrl Pts',(70.7622418829434,9.30791458482255,40.7030133799736));
#162267=CARTESIAN_POINT('Ctrl Pts',(70.5976869651754,9.32264802401544,40.7358711866092));
#162268=CARTESIAN_POINT('Ctrl Pts',(70.3172886761538,9.33998747155943,40.7917033086452));
#162269=CARTESIAN_POINT('Ctrl Pts',(70.2016312674559,9.34490186286306,40.8146873293401));
#162270=CARTESIAN_POINT('Ctrl Pts',(70.0276706962275,9.34893341688283,40.8491664836239));
#162271=CARTESIAN_POINT('Ctrl Pts',(69.9694247596809,9.34971765598558,40.8606955197955));
#162272=CARTESIAN_POINT('Ctrl Pts',(69.8607763742654,9.35012579552253,40.8821685768101));
#162273=CARTESIAN_POINT('Ctrl Pts',(69.8103780187963,9.34989192368821,40.8921157716346));
#162274=CARTESIAN_POINT('Ctrl Pts',(69.6830817400965,9.34823232626495,40.9172095181326));
#162275=CARTESIAN_POINT('Ctrl Pts',(69.6061916781604,9.34624452969243,40.9323385442458));
#162276=CARTESIAN_POINT('Ctrl Pts',(69.255382636236,9.33267699110307,41.0012606129443));
#162277=CARTESIAN_POINT('Ctrl Pts',(68.98198486993,9.30957845371409,41.0546881358325));
#162278=CARTESIAN_POINT('Ctrl Pts',(68.3896824371748,9.23219686380711,41.1703037704086));
#162279=CARTESIAN_POINT('Ctrl Pts',(68.0717424362089,9.17315627498059,41.2322836262543));
#162280=CARTESIAN_POINT('Ctrl Pts',(67.5314335830362,9.04248126521768,41.3379612574257));
#162281=CARTESIAN_POINT('Ctrl Pts',(67.307453715784,8.97906360597333,41.3818733041484));
#162282=CARTESIAN_POINT('Ctrl Pts',(66.9165438949958,8.85188805446307,41.4588234670683));
#162283=CARTESIAN_POINT('Ctrl Pts',(66.7486086226193,8.79170730855993,41.4919852804684));
#162284=CARTESIAN_POINT('Ctrl Pts',(66.4858255752121,8.68867584306493,41.5440724303199));
#162285=CARTESIAN_POINT('Ctrl Pts',(66.3897763281541,8.649097660121,41.5631529198949));
#162286=CARTESIAN_POINT('Ctrl Pts',(66.2060868028911,8.56968420014094,41.599729040958));
#162287=CARTESIAN_POINT('Ctrl Pts',(66.118360409311,8.53008830381383,41.617235444182));
#162288=CARTESIAN_POINT('Ctrl Pts',(65.9099737435583,8.43200938982037,41.6589141325978));
#162289=CARTESIAN_POINT('Ctrl Pts',(65.7899329061692,8.37222704278713,41.6829997361007));
#162290=CARTESIAN_POINT('Ctrl Pts',(65.2353359813671,8.08052596148171,41.794630324685));
#162291=CARTESIAN_POINT('Ctrl Pts',(64.8183762964761,7.81596655159606,41.8796375943263));
#162292=CARTESIAN_POINT('Ctrl Pts',(64.2390400466742,7.37892670577032,41.9986703968613));
#162293=CARTESIAN_POINT('Ctrl Pts',(64.0590538096989,7.23210626661684,42.0357882634628));
#162294=CARTESIAN_POINT('Ctrl Pts',(63.7758740932747,6.98267224975432,42.0942588696114));
#162295=CARTESIAN_POINT('Ctrl Pts',(63.6692877269016,6.88422435624125,42.1162838594886));
#162296=CARTESIAN_POINT('Ctrl Pts',(63.5175972045893,6.73734562877,42.1476136584239));
#162297=CARTESIAN_POINT('Ctrl Pts',(63.4706641079982,6.69091765362099,42.157304812156));
#162298=CARTESIAN_POINT('Ctrl Pts',(63.3852099008563,6.6045555049851,42.1749406313875));
#162299=CARTESIAN_POINT('Ctrl Pts',(63.3465467821001,6.5647734896311,42.1829155949898));
#162300=CARTESIAN_POINT('Ctrl Pts',(63.2501005873297,6.46373696636497,42.2028019537123));
#162301=CARTESIAN_POINT('Ctrl Pts',(63.1927807225319,6.40202806366682,42.2146144594204));
#162302=CARTESIAN_POINT('Ctrl Pts',(62.8272543062874,5.99760384790865,42.2899451208317));
#162303=CARTESIAN_POINT('Ctrl Pts',(62.543649714219,5.63261093300959,42.3484333324682));
#162304=CARTESIAN_POINT('Ctrl Pts',(62.1420331183813,5.02774263907562,42.4328086790844));
#162305=CARTESIAN_POINT('Ctrl Pts',(62.0053609601948,4.80164466135541,42.4618727877515));
#162306=CARTESIAN_POINT('Ctrl Pts',(61.7866246874071,4.40246068513886,42.5092344231956));
#162307=CARTESIAN_POINT('Ctrl Pts',(61.6999817838396,4.23216389745481,42.5282697850598));
#162308=CARTESIAN_POINT('Ctrl Pts',(61.573144348026,3.96275762328901,42.5566329724457));
#162309=CARTESIAN_POINT('Ctrl Pts',(61.5293517709636,3.86546226367517,42.5665313361969));
#162310=CARTESIAN_POINT('Ctrl Pts',(61.4489556442168,3.67837096629996,42.5849175723739));
#162311=CARTESIAN_POINT('Ctrl Pts',(61.4120661141639,3.58871764701531,42.5934503782447));
#162312=CARTESIAN_POINT('Ctrl Pts',(61.3283583596253,3.37596884883982,42.6130508845828));
#162313=CARTESIAN_POINT('Ctrl Pts',(61.2827220644023,3.25241363197094,42.623930598713));
#162314=CARTESIAN_POINT('Ctrl Pts',(61.1119531865601,2.75835602231826,42.6654542945684));
#162315=CARTESIAN_POINT('Ctrl Pts',(61.007311672445,2.38092439142235,42.6928295986166));
#162316=CARTESIAN_POINT('Ctrl Pts',(60.8625199054283,1.69582235897097,42.7346205667345));
#162317=CARTESIAN_POINT('Ctrl Pts',(60.8134966288011,1.39070650910709,42.7505217647879));
#162318=CARTESIAN_POINT('Ctrl Pts',(60.7605733240106,0.913645047299086,
42.7709375909532));
#162319=CARTESIAN_POINT('Ctrl Pts',(60.7463087668312,0.743151767111156,
42.7773610088435));
#162320=CARTESIAN_POINT('Ctrl Pts',(60.7299096178347,0.453262157829723,
42.7867375302493));
#162321=CARTESIAN_POINT('Ctrl Pts',(60.7254110672388,0.334056823156275,
42.7901514675776));
#162322=CARTESIAN_POINT('Ctrl Pts',(60.7220203171114,0.155197480335001,
42.7945890807405));
#162323=CARTESIAN_POINT('Ctrl Pts',(60.7214492321599,0.0955957775431189,
42.7959538955453));
#162324=CARTESIAN_POINT('Ctrl Pts',(60.7214339163937,0.0239934614096055,
42.7974542391796));
#162325=CARTESIAN_POINT('Ctrl Pts',(60.7214539679052,0.0119967102410532,
42.7977009207848));
#162326=CARTESIAN_POINT('Ctrl Pts',(60.7214966333422,6.81868220864142E-10,
42.7979428885072));
#162327=CARTESIAN_POINT('Origin',(69.6316151486327,0.,39.48523201752));
#162328=CARTESIAN_POINT('',(60.959339991465,-1.57574869447161E-5,44.1468196011651));
#162329=CARTESIAN_POINT('',(60.929874446542,4.05628901510058E-10,43.9797121921192));
#162330=CARTESIAN_POINT('',(60.4236626579685,-1.14504475720278E-15,41.1088424787055));
#162331=CARTESIAN_POINT('Ctrl Pts',(60.9593399353935,-7.19695824888743E-14,
44.1468192833488));
#162332=CARTESIAN_POINT('Ctrl Pts',(60.9592011695234,0.039018323097806,
44.1460323029926));
#162333=CARTESIAN_POINT('Ctrl Pts',(60.9593042464182,0.0780364129096037,
44.1452103586968));
#162334=CARTESIAN_POINT('Ctrl Pts',(60.9600768192033,0.165455973684423,
44.1432889493377));
#162335=CARTESIAN_POINT('Ctrl Pts',(60.9608766338813,0.213854746414297,
44.142170326208));
#162336=CARTESIAN_POINT('Ctrl Pts',(60.9649924384163,0.383848718732972,
44.1380441549837));
#162337=CARTESIAN_POINT('Ctrl Pts',(60.9702840870665,0.505376432410811,
44.1347397851575));
#162338=CARTESIAN_POINT('Ctrl Pts',(61.0103947725256,1.14324184570811,44.1154304296644));
#162339=CARTESIAN_POINT('Ctrl Pts',(61.0851820544867,1.65595956485757,44.0930853775808));
#162340=CARTESIAN_POINT('Ctrl Pts',(61.254417884048,2.38999330760417,44.0493671991483));
#162341=CARTESIAN_POINT('Ctrl Pts',(61.3161166739917,2.61819672159879,44.0340696663355));
#162342=CARTESIAN_POINT('Ctrl Pts',(61.4399886201481,3.01653157258925,44.0042054564054));
#162343=CARTESIAN_POINT('Ctrl Pts',(61.4986480887534,3.18767454757481,43.9903119054966));
#162344=CARTESIAN_POINT('Ctrl Pts',(61.5991309158904,3.45551078176694,43.9668426511835));
#162345=CARTESIAN_POINT('Ctrl Pts',(61.6377411246449,3.55341421144728,43.9578902120456));
#162346=CARTESIAN_POINT('Ctrl Pts',(61.7152321514134,3.74066451952898,43.9400397506919));
#162347=CARTESIAN_POINT('Ctrl Pts',(61.7538779760383,3.83009807721125,43.9311875769518));
#162348=CARTESIAN_POINT('Ctrl Pts',(61.849622853789,4.04255604396231,43.909370681766));
#162349=CARTESIAN_POINT('Ctrl Pts',(61.9079976324839,4.1649553813899,43.8961584742693));
#162350=CARTESIAN_POINT('Ctrl Pts',(62.1929017806195,4.73051438383986,43.8320819235754));
#162351=CARTESIAN_POINT('Ctrl Pts',(62.4514798570855,5.15590401043427,43.7750015130925));
#162352=CARTESIAN_POINT('Ctrl Pts',(62.8789950099589,5.747109625867,43.6827388275413));
#162353=CARTESIAN_POINT('Ctrl Pts',(63.0226635000979,5.93080520324176,43.6520248084645));
#162354=CARTESIAN_POINT('Ctrl Pts',(63.2668461916425,6.21983386012601,43.6004304954048));
#162355=CARTESIAN_POINT('Ctrl Pts',(63.3632454332833,6.32862494160068,43.580201788264));
#162356=CARTESIAN_POINT('Ctrl Pts',(63.507108474567,6.48345064180576,43.5502522051747));
#162357=CARTESIAN_POINT('Ctrl Pts',(63.5525889486014,6.53135348063232,43.5408171906781));
#162358=CARTESIAN_POINT('Ctrl Pts',(63.6371998643254,6.61857180536192,43.5233300685671));
#162359=CARTESIAN_POINT('Ctrl Pts',(63.6761795625054,6.65803240109385,43.515299282958));
#162360=CARTESIAN_POINT('Ctrl Pts',(63.7751887497777,6.75646676911935,43.4949609943681));
#162361=CARTESIAN_POINT('Ctrl Pts',(63.8356686779449,6.81496719119529,43.4825912797514));
#162362=CARTESIAN_POINT('Ctrl Pts',(64.2320895852908,7.18802242331507,43.4018130582296));
#162363=CARTESIAN_POINT('Ctrl Pts',(64.5900881648394,7.47747545171792,43.3302071586913));
#162364=CARTESIAN_POINT('Ctrl Pts',(65.1834487745134,7.88764202051685,43.2120221629778));
#162365=CARTESIAN_POINT('Ctrl Pts',(65.4052619474988,8.02728413330826,43.1679454138692));
#162366=CARTESIAN_POINT('Ctrl Pts',(65.7968766236401,8.25092076888774,43.0901006780881));
#162367=CARTESIAN_POINT('Ctrl Pts',(65.963943210823,8.33955259322519,43.0568844591762));
#162368=CARTESIAN_POINT('Ctrl Pts',(66.2282303761327,8.46938804728209,43.0042851860022));
#162369=CARTESIAN_POINT('Ctrl Pts',(66.3236753258305,8.51423411021166,42.9852791167078));
#162370=CARTESIAN_POINT('Ctrl Pts',(66.5072042527139,8.59660154086896,42.948707786122));
#162371=CARTESIAN_POINT('Ctrl Pts',(66.5951487187156,8.63441234394498,42.931172616974));
#162372=CARTESIAN_POINT('Ctrl Pts',(66.8038377792478,8.7202520367896,42.8895345299687));
#162373=CARTESIAN_POINT('Ctrl Pts',(66.9250316375695,8.76708430385657,42.8653319749979));
#162374=CARTESIAN_POINT('Ctrl Pts',(67.4096410303131,8.9424726197836,42.7684695094921));
#162375=CARTESIAN_POINT('Ctrl Pts',(67.7798219999628,9.0502801333161,42.6942721995562));
#162376=CARTESIAN_POINT('Ctrl Pts',(68.4518378808896,9.20014966751034,42.5595149072701));
#162377=CARTESIAN_POINT('Ctrl Pts',(68.7511721451292,9.25119965452689,42.4994748235487));
#162378=CARTESIAN_POINT('Ctrl Pts',(69.2191269334297,9.30685182060255,42.4058770748503));
#162379=CARTESIAN_POINT('Ctrl Pts',(69.3863020010349,9.3220054585555,42.3724928759089));
#162380=CARTESIAN_POINT('Ctrl Pts',(69.6705900515395,9.33977388874443,42.315882417577));
#162381=CARTESIAN_POINT('Ctrl Pts',(69.7875076349303,9.34479450278586,42.292646642121));
#162382=CARTESIAN_POINT('Ctrl Pts',(69.96295926624,9.34890258724526,42.2578708185383));
#162383=CARTESIAN_POINT('Ctrl Pts',(70.0214341345616,9.34970165889319,42.2462961240143));
#162384=CARTESIAN_POINT('Ctrl Pts',(70.130812587057,9.35013033751004,42.2246782297245));
#162385=CARTESIAN_POINT('Ctrl Pts',(70.1817120289497,9.34989817211438,42.2146320107093));
#162386=CARTESIAN_POINT('Ctrl Pts',(70.3095209877298,9.34823134452351,42.1894372159126));
#162387=CARTESIAN_POINT('Ctrl Pts',(70.3864226536441,9.34624277031949,42.1743059193247));
#162388=CARTESIAN_POINT('Ctrl Pts',(70.7370584013524,9.33267907523359,42.1054179630285));
#162389=CARTESIAN_POINT('Ctrl Pts',(71.010272020692,9.30960232183055,42.0520262675107));
#162390=CARTESIAN_POINT('Ctrl Pts',(71.6023944059914,9.23227640381724,41.9364456131107));
#162391=CARTESIAN_POINT('Ctrl Pts',(71.9203369568101,9.17325292138672,41.8744653373229));
#162392=CARTESIAN_POINT('Ctrl Pts',(72.4607344914445,9.04258707399007,41.7687706979663));
#162393=CARTESIAN_POINT('Ctrl Pts',(72.6847984548984,8.9791551477307,41.724842325927));
#162394=CARTESIAN_POINT('Ctrl Pts',(73.0758333745289,8.85194986191113,41.6478677410431));
#162395=CARTESIAN_POINT('Ctrl Pts',(73.2438106486876,8.7917575038101,41.614697707368));
#162396=CARTESIAN_POINT('Ctrl Pts',(73.5066424323439,8.68871024668405,41.5626009701187));
#162397=CARTESIAN_POINT('Ctrl Pts',(73.6026991740363,8.64913006096221,41.5435190163316));
#162398=CARTESIAN_POINT('Ctrl Pts',(73.7863936891685,8.56971627136852,41.5069419436213));
#162399=CARTESIAN_POINT('Ctrl Pts',(73.8741177145433,8.53012238079545,41.4894360347551));
#162400=CARTESIAN_POINT('Ctrl Pts',(74.0824832998574,8.43205577105438,41.4477616179529));
#162401=CARTESIAN_POINT('Ctrl Pts',(74.2025057982643,8.37228448625142,41.4236797390816));
#162402=CARTESIAN_POINT('Ctrl Pts',(74.7573559309023,8.08046183613628,41.3119984478771));
#162403=CARTESIAN_POINT('Ctrl Pts',(75.1745635785788,7.81572557180448,41.2269400662472));
#162404=CARTESIAN_POINT('Ctrl Pts',(75.7539753321687,7.37855356386901,41.1078908311994));
#162405=CARTESIAN_POINT('Ctrl Pts',(75.9338262791899,7.23182678448237,41.0708007567995));
#162406=CARTESIAN_POINT('Ctrl Pts',(76.21682939966,6.98253378605796,41.0123665601668));
#162407=CARTESIAN_POINT('Ctrl Pts',(76.3233685760332,6.88412576028209,40.990351324461));
#162408=CARTESIAN_POINT('Ctrl Pts',(76.4750066279395,6.73729525527626,40.9590323686953));
#162409=CARTESIAN_POINT('Ctrl Pts',(76.5219326386913,6.69087361687547,40.949342680837));
#162410=CARTESIAN_POINT('Ctrl Pts',(76.6073814114384,6.60451597538701,40.9317079882756));
#162411=CARTESIAN_POINT('Ctrl Pts',(76.6460460110928,6.56473195083532,40.9237327221797));
#162412=CARTESIAN_POINT('Ctrl Pts',(76.7425062464142,6.46367940418966,40.9038434734586));
#162413=CARTESIAN_POINT('Ctrl Pts',(76.7998383351589,6.40195616116632,40.8920284514729));
#162414=CARTESIAN_POINT('Ctrl Pts',(77.1654414559112,5.99743685202562,40.8166819796699));
#162415=CARTESIAN_POINT('Ctrl Pts',(77.4490991356294,5.63235364864955,40.7581826986619));
#162416=CARTESIAN_POINT('Ctrl Pts',(77.8507003742193,5.0274484261585,40.6738095502626));
#162417=CARTESIAN_POINT('Ctrl Pts',(77.987322929437,4.80141585042249,40.6447556328777));
#162418=CARTESIAN_POINT('Ctrl Pts',(78.2059947350294,4.40233107207008,40.5974075410352));
#162419=CARTESIAN_POINT('Ctrl Pts',(78.2926188081794,4.23206554937768,40.5783761765879));
#162420=CARTESIAN_POINT('Ctrl Pts',(78.4194360519795,3.96269671506524,40.5500173702641));
#162421=CARTESIAN_POINT('Ctrl Pts',(78.4632254749425,3.86540659021672,40.540119674957));
#162422=CARTESIAN_POINT('Ctrl Pts',(78.5436188144636,3.67831876442622,40.521733999986));
#162423=CARTESIAN_POINT('Ctrl Pts',(78.5805084727915,3.5886635725035,40.5132011246697));
#162424=CARTESIAN_POINT('Ctrl Pts',(78.664220606108,3.37589964412092,40.4935994907015));
#162425=CARTESIAN_POINT('Ctrl Pts',(78.7098606565591,3.25233098193822,40.4827187971432));
#162426=CARTESIAN_POINT('Ctrl Pts',(78.8808972116723,2.75748157894577,40.4411295694266));
#162427=CARTESIAN_POINT('Ctrl Pts',(78.9857056668484,2.37923964034732,40.4137051318709));
#162428=CARTESIAN_POINT('Ctrl Pts',(79.1313804155078,1.68903248615976,40.3716372015968));
#162429=CARTESIAN_POINT('Ctrl Pts',(79.1807987374525,1.37955890879548,40.3555626438913));
#162430=CARTESIAN_POINT('Ctrl Pts',(79.2330867746745,0.901036399115497,
40.3352341776319));
#162431=CARTESIAN_POINT('Ctrl Pts',(79.2469061362153,0.733496976087364,
40.3289604461154));
#162432=CARTESIAN_POINT('Ctrl Pts',(79.2628557554179,0.447992296191848,
40.3197654258101));
#162433=CARTESIAN_POINT('Ctrl Pts',(79.2672442328512,0.330207732233258,
40.3164035776742));
#162434=CARTESIAN_POINT('Ctrl Pts',(79.2705580195277,0.153029291306634,
40.3120168654863));
#162435=CARTESIAN_POINT('Ctrl Pts',(79.2711139470456,0.0936857360576762,
40.310660576402));
#162436=CARTESIAN_POINT('Ctrl Pts',(79.2711184696487,-0.0170278165458702,
40.3083446807105));
#162437=CARTESIAN_POINT('Ctrl Pts',(79.2707059962099,-0.068394340316024,
40.3073566946874));
#162438=CARTESIAN_POINT('Ctrl Pts',(79.2686159971758,-0.198164504203468,
40.3050762702276));
#162439=CARTESIAN_POINT('Ctrl Pts',(79.2663867249648,-0.276557334706842,
40.3038972866039));
#162440=CARTESIAN_POINT('Ctrl Pts',(79.2518252935275,-0.63355012053469,
40.2994091240156));
#162441=CARTESIAN_POINT('Ctrl Pts',(79.2282409446322,-0.911575433521893,
40.2983564799344));
#162442=CARTESIAN_POINT('Ctrl Pts',(79.1502650954314,-1.51447011944969,
40.3009375815794));
#162443=CARTESIAN_POINT('Ctrl Pts',(79.0911512195368,-1.83834904805255,
40.3054425701453));
#162444=CARTESIAN_POINT('Ctrl Pts',(78.9607036614042,-2.38902455281903,
40.318033982787));
#162445=CARTESIAN_POINT('Ctrl Pts',(78.8974583286698,-2.61743978298294,
40.3247637682565));
#162446=CARTESIAN_POINT('Ctrl Pts',(78.7707692099646,-3.01608976400974,
40.3390743896039));
#162447=CARTESIAN_POINT('Ctrl Pts',(78.7108668480139,-3.18733854012721,
40.346084475152));
#162448=CARTESIAN_POINT('Ctrl Pts',(78.608378047351,-3.45529755884479,40.3584021377836));
#162449=CARTESIAN_POINT('Ctrl Pts',(78.5690294674324,-3.55321986489301,
40.3631955836433));
#162450=CARTESIAN_POINT('Ctrl Pts',(78.4901056668316,-3.7404827377327,40.3729250988388));
#162451=CARTESIAN_POINT('Ctrl Pts',(78.4507677608816,-3.82991032402126,
40.3778237504992));
#162452=CARTESIAN_POINT('Ctrl Pts',(78.3533653589933,-4.04231517080979,
40.3900653020223));
#162453=CARTESIAN_POINT('Ctrl Pts',(78.2940192915613,-4.16466829028765,
40.3976116688886));
#162454=CARTESIAN_POINT('Ctrl Pts',(78.0040853101993,-4.7308609468423,40.4348797324491));
#162455=CARTESIAN_POINT('Ctrl Pts',(77.7411480921919,-5.15687198280501,
40.4697383963746));
#162456=CARTESIAN_POINT('Ctrl Pts',(77.3075384551055,-5.74826772979273,
40.5293075740135));
#162457=CARTESIAN_POINT('Ctrl Pts',(77.1622572267894,-5.93162484066259,
40.5495528383983));
#162458=CARTESIAN_POINT('Ctrl Pts',(76.9154969969459,-6.22021157404352,
40.5845379323153));
#162459=CARTESIAN_POINT('Ctrl Pts',(76.8180896171305,-6.32888451799664,
40.5984860770007));
#162460=CARTESIAN_POINT('Ctrl Pts',(76.6727763691276,-6.48357885542733,
40.6195299788531));
#162461=CARTESIAN_POINT('Ctrl Pts',(76.6268271397286,-6.53146394911662,
40.6262170189577));
#162462=CARTESIAN_POINT('Ctrl Pts',(76.5413488926385,-6.6186686696494,40.6387216184551));
#162463=CARTESIAN_POINT('Ctrl Pts',(76.5019683888374,-6.65813297853069,
40.6445077489881));
#162464=CARTESIAN_POINT('Ctrl Pts',(76.401935159927,-6.7566025323501,40.6592649914099));
#162465=CARTESIAN_POINT('Ctrl Pts',(76.3408370992651,-6.81513358485769,
40.668331870445));
#162466=CARTESIAN_POINT('Ctrl Pts',(75.9404576245387,-7.18838755013565,
40.7280452531935));
#162467=CARTESIAN_POINT('Ctrl Pts',(75.579331378679,-7.47797909636203,40.7832361062152));
#162468=CARTESIAN_POINT('Ctrl Pts',(74.9812390012199,-7.88810805242604,
40.8751350827215));
#162469=CARTESIAN_POINT('Ctrl Pts',(74.7578907282277,-8.02762250909813,
40.9095559514904));
#162470=CARTESIAN_POINT('Ctrl Pts',(74.3635161713318,-8.25109308977263,
40.9703078130127));
#162471=CARTESIAN_POINT('Ctrl Pts',(74.1952422766827,-8.33967638575718,
40.9962228767871));
#162472=CARTESIAN_POINT('Ctrl Pts',(73.9289969291622,-8.46945975931981,
41.0371728699192));
#162473=CARTESIAN_POINT('Ctrl Pts',(73.8328206092398,-8.51429769320179,
41.0519550838115));
#162474=CARTESIAN_POINT('Ctrl Pts',(73.6478603502723,-8.59665795442987,
41.0803585146401));
#162475=CARTESIAN_POINT('Ctrl Pts',(73.5592175271624,-8.63446910770138,
41.0939603307918));
#162476=CARTESIAN_POINT('Ctrl Pts',(73.3488351292313,-8.72032017982404,
41.126214951365));
#162477=CARTESIAN_POINT('Ctrl Pts',(73.2266388362571,-8.76716221030664,
41.1449278460924));
#162478=CARTESIAN_POINT('Ctrl Pts',(72.7360783828904,-8.94327028018312,
41.2199661886711));
#162479=CARTESIAN_POINT('Ctrl Pts',(72.360747672531,-9.05153031441586,41.2771711454197));
#162480=CARTESIAN_POINT('Ctrl Pts',(71.6146438540337,-9.21598828431424,
41.3908216282327));
#162481=CARTESIAN_POINT('Ctrl Pts',(71.2450113648896,-9.27401177106631,
41.447099671287));
#162482=CARTESIAN_POINT('Ctrl Pts',(70.7426216104471,-9.32160373129045,
41.5240315512877));
#162483=CARTESIAN_POINT('Ctrl Pts',(70.6120254932216,-9.33115048055859,
41.5440714544694));
#162484=CARTESIAN_POINT('Ctrl Pts',(70.3828688479151,-9.34296033891395,
41.5793431138487));
#162485=CARTESIAN_POINT('Ctrl Pts',(70.2843862065223,-9.34644002596292,
41.594536333219));
#162486=CARTESIAN_POINT('Ctrl Pts',(70.1306539582927,-9.34938334255177,
41.6183219194453));
#162487=CARTESIAN_POINT('Ctrl Pts',(70.0754274562202,-9.3499397919804,41.6268804792593));
#162488=CARTESIAN_POINT('Ctrl Pts',(69.967001283541,-9.35004891768843,41.6437140900858));
#162489=CARTESIAN_POINT('Ctrl Pts',(69.9138038303237,-9.34963765444814,
41.6519878485647));
#162490=CARTESIAN_POINT('Ctrl Pts',(69.7722524177475,-9.34730628279,41.6740374694986));
#162491=CARTESIAN_POINT('Ctrl Pts',(69.6839204605119,-9.34456834027643,
41.6878325046681));
#162492=CARTESIAN_POINT('Ctrl Pts',(69.0699080624955,-9.31660839460732,
41.783915356157));
#162493=CARTESIAN_POINT('Ctrl Pts',(68.5473011312671,-9.2472547137258,41.8666207186992));
#162494=CARTESIAN_POINT('Ctrl Pts',(67.7349761655645,-9.06706731850457,
41.9944599117333));
#162495=CARTESIAN_POINT('Ctrl Pts',(67.4400676372568,-8.98596589100186,
42.0407264249616));
#162496=CARTESIAN_POINT('Ctrl Pts',(66.9887198190538,-8.83719921088504,
42.1110580656074));
#162497=CARTESIAN_POINT('Ctrl Pts',(66.8292750783789,-8.77970378497714,
42.135809458165));
#162498=CARTESIAN_POINT('Ctrl Pts',(66.5758089277539,-8.68029706657569,
42.174979317466));
#162499=CARTESIAN_POINT('Ctrl Pts',(66.4807725337071,-8.64117421924204,
42.1896252236292));
#162500=CARTESIAN_POINT('Ctrl Pts',(66.2977087275427,-8.56220138001157,
42.2177540394568));
#162501=CARTESIAN_POINT('Ctrl Pts',(66.2096157750666,-8.52254263413246,
42.2312520650165));
#162502=CARTESIAN_POINT('Ctrl Pts',(65.9957402744897,-8.42218178350809,
42.2639285618215));
#162503=CARTESIAN_POINT('Ctrl Pts',(65.8706636723969,-8.35998373123995,
42.2829566136051));
#162504=CARTESIAN_POINT('Ctrl Pts',(65.3979336301034,-8.11135839340803,
42.3545672359968));
#162505=CARTESIAN_POINT('Ctrl Pts',(65.0606918978997,-7.90542798625243,
42.404989099112));
#162506=CARTESIAN_POINT('Ctrl Pts',(64.4958575449963,-7.50883378545272,
42.4886322787441));
#162507=CARTESIAN_POINT('Ctrl Pts',(64.2624272784163,-7.32770944102872,
42.5229369039794));
#162508=CARTESIAN_POINT('Ctrl Pts',(63.9111985396855,-7.02726604484864,
42.5744104081198));
#162509=CARTESIAN_POINT('Ctrl Pts',(63.7873850613468,-6.91544450915314,
42.5925266911494));
#162510=CARTESIAN_POINT('Ctrl Pts',(63.6164183557497,-6.75246344023828,
42.6175586793641));
#162511=CARTESIAN_POINT('Ctrl Pts',(63.566750732155,-6.70404297060807,42.6248328376538));
#162512=CARTESIAN_POINT('Ctrl Pts',(63.4785454997894,-6.61610480969267,
42.6377606610672));
#162513=CARTESIAN_POINT('Ctrl Pts',(63.4398115464697,-6.57679402993487,
42.6434416580011));
#162514=CARTESIAN_POINT('Ctrl Pts',(63.3461377269486,-6.48001660749793,
42.6571882414878));
#162515=CARTESIAN_POINT('Ctrl Pts',(63.2915768659843,-6.42218239615651,
42.6652009766809));
#162516=CARTESIAN_POINT('Ctrl Pts',(63.0599241657975,-6.17024356202669,
42.6992227941961));
#162517=CARTESIAN_POINT('Ctrl Pts',(62.8902769064617,-5.96931395311664,
42.724139896814));
#162518=CARTESIAN_POINT('Ctrl Pts',(62.4838819974151,-5.44462052743962,
42.7833655164531));
#162519=CARTESIAN_POINT('Ctrl Pts',(62.2589369410372,-5.11218034067375,
42.815685340908));
#162520=CARTESIAN_POINT('Ctrl Pts',(61.9972718356034,-4.66662169017116,
42.8520069343839));
#162521=CARTESIAN_POINT('Ctrl Pts',(61.9406433965693,-4.56601005140854,
42.8597783710209));
#162522=CARTESIAN_POINT('Ctrl Pts',(61.8058414933842,-4.3158824332008,42.8780324809005));
#162523=CARTESIAN_POINT('Ctrl Pts',(61.72978913071,-4.16524104560711,42.8881105987113));
#162524=CARTESIAN_POINT('Ctrl Pts',(61.6138154578883,-3.91939315977447,
42.9030775538707));
#162525=CARTESIAN_POINT('Ctrl Pts',(61.5713625944114,-3.82545359404603,
42.9084583018507));
#162526=CARTESIAN_POINT('Ctrl Pts',(61.4916526128767,-3.6411126093075,42.9183589384919));
#162527=CARTESIAN_POINT('Ctrl Pts',(61.4542451361088,-3.55079225944025,
42.9229084115732));
#162528=CARTESIAN_POINT('Ctrl Pts',(61.3657429971548,-3.3273940142231,42.933422675009));
#162529=CARTESIAN_POINT('Ctrl Pts',(61.3162337686272,-3.19370041539068,
42.939080352518));
#162530=CARTESIAN_POINT('Ctrl Pts',(61.0655530653476,-2.46690118480169,
42.9664486156816));
#162531=CARTESIAN_POINT('Ctrl Pts',(60.9202954310094,-1.85578835661807,
42.9773142197201));
#162532=CARTESIAN_POINT('Ctrl Pts',(60.7968252928583,-0.94261981963765,
42.9777153545758));
#162533=CARTESIAN_POINT('Ctrl Pts',(60.7709605078862,-0.648742537193085,
42.9755204946933));
#162534=CARTESIAN_POINT('Ctrl Pts',(60.7556501642509,-0.275929395564813,
42.9700738771766));
#162535=CARTESIAN_POINT('Ctrl Pts',(60.7534089544413,-0.197654762270246,
42.968782577162));
#162536=CARTESIAN_POINT('Ctrl Pts',(60.7514966309874,-0.0795781893991349,
42.9666186679888));
#162537=CARTESIAN_POINT('Ctrl Pts',(60.751103630633,-0.0397894807063568,
42.965852513959));
#162538=CARTESIAN_POINT('Ctrl Pts',(60.7509621221957,-6.89336955246539E-10,
42.9650499797481));
#162539=CARTESIAN_POINT('Ctrl Pts',(60.7214966333422,6.81868220864142E-10,
42.7979428885072));
#162540=CARTESIAN_POINT('Ctrl Pts',(60.7216384344148,-0.0398717644279405,
42.7987470823689));
#162541=CARTESIAN_POINT('Ctrl Pts',(60.7220300289147,-0.0797430699037861,
42.7994992074081));
#162542=CARTESIAN_POINT('Ctrl Pts',(60.7239324241189,-0.197976095297675,
42.8015772606206));
#162543=CARTESIAN_POINT('Ctrl Pts',(60.7261587264108,-0.276325270394438,
42.8027559393475));
#162544=CARTESIAN_POINT('Ctrl Pts',(60.7407282582848,-0.633770612581696,
42.8072518609236));
#162545=CARTESIAN_POINT('Ctrl Pts',(60.7643682793433,-0.912290023609129,
42.8083035643672));
#162546=CARTESIAN_POINT('Ctrl Pts',(60.842484874372,-1.51566812981762,42.8057061943277));
#162547=CARTESIAN_POINT('Ctrl Pts',(60.9016403944183,-1.83954063114414,
42.801193935115));
#162548=CARTESIAN_POINT('Ctrl Pts',(61.0321096736188,-2.38999291230631,
42.7885953017863));
#162549=CARTESIAN_POINT('Ctrl Pts',(61.0953196500395,-2.61819641270663,
42.7818680504721));
#162550=CARTESIAN_POINT('Ctrl Pts',(61.2219353950757,-3.01653139225999,
42.7675645244941));
#162551=CARTESIAN_POINT('Ctrl Pts',(61.2818091508149,-3.18767441041751,
42.7605574706621));
#162552=CARTESIAN_POINT('Ctrl Pts',(61.3842590955769,-3.45551069471278,
42.7482442030221));
#162553=CARTESIAN_POINT('Ctrl Pts',(61.423602740362,-3.5534141320965,42.7434512746748));
#162554=CARTESIAN_POINT('Ctrl Pts',(61.5025257040829,-3.74066444530087,
42.7337217294173));
#162555=CARTESIAN_POINT('Ctrl Pts',(61.5418685200311,-3.8300980005415,42.7288224015581));
#162556=CARTESIAN_POINT('Ctrl Pts',(61.6393010804231,-4.04255594558835,
42.7165769017754));
#162557=CARTESIAN_POINT('Ctrl Pts',(61.6986742592231,-4.16495526413319,
42.7090269669468));
#162558=CARTESIAN_POINT('Ctrl Pts',(61.9883121783848,-4.73051452830085,
42.6717962557641));
#162559=CARTESIAN_POINT('Ctrl Pts',(62.2508189167381,-5.15590441137969,
42.6369953616465));
#162560=CARTESIAN_POINT('Ctrl Pts',(62.684107580498,-5.74711010491705,42.5774751123864));
#162561=CARTESIAN_POINT('Ctrl Pts',(62.8296165194742,-5.93080554222332,
42.5571993445042));
#162562=CARTESIAN_POINT('Ctrl Pts',(63.0767193453967,-6.21983401626779,
42.5221667602561));
#162563=CARTESIAN_POINT('Ctrl Pts',(63.1742235866626,-6.32862504888967,
42.5082050502534));
#162564=CARTESIAN_POINT('Ctrl Pts',(63.3196539372216,-6.48345069477836,
42.4871444014065));
#162565=CARTESIAN_POINT('Ctrl Pts',(63.365618561706,-6.53135352627038,42.4804551775611));
#162566=CARTESIAN_POINT('Ctrl Pts',(63.4511077583279,-6.61857184537218,
42.4679490602732));
#162567=CARTESIAN_POINT('Ctrl Pts',(63.4904833855244,-6.65803244263412,
42.462163687978));
#162568=CARTESIAN_POINT('Ctrl Pts',(63.5904777086381,-6.75646682518263,
42.4474122888511));
#162569=CARTESIAN_POINT('Ctrl Pts',(63.6515409567846,-6.81496725990258,
42.4383506625284));
#162570=CARTESIAN_POINT('Ctrl Pts',(64.0516826306627,-7.18802256978761,
42.3786734114279));
#162571=CARTESIAN_POINT('Ctrl Pts',(64.4125820026368,-7.47747565181252,
42.3235182074294));
#162572=CARTESIAN_POINT('Ctrl Pts',(65.0105802740117,-7.88764220478509,
42.2316344892034));
#162573=CARTESIAN_POINT('Ctrl Pts',(65.2340915474207,-8.02728426708803,
42.1971885218025));
#162574=CARTESIAN_POINT('Ctrl Pts',(65.6287133386676,-8.25092083700116,
42.1363985529957));
#162575=CARTESIAN_POINT('Ctrl Pts',(65.7970651629551,-8.33955264215256,
42.1104714554637));
#162576=CARTESIAN_POINT('Ctrl Pts',(66.063403836005,-8.46938807562017,42.0695070758555));
#162577=CARTESIAN_POINT('Ctrl Pts',(66.1595932043114,-8.51423413533653,
42.0547228443441));
#162578=CARTESIAN_POINT('Ctrl Pts',(66.34456211091,-8.59660156315883,42.0263180644849));
#162579=CARTESIAN_POINT('Ctrl Pts',(66.4332002595621,-8.63441236637256,
42.012716954392));
#162580=CARTESIAN_POINT('Ctrl Pts',(66.6435449091828,-8.72025206371114,
41.9804680928254));
#162581=CARTESIAN_POINT('Ctrl Pts',(66.7657076581063,-8.76708433463439,
41.9617603123215));
#162582=CARTESIAN_POINT('Ctrl Pts',(67.2542212081322,-8.9424729192846,41.887034965394));
#162583=CARTESIAN_POINT('Ctrl Pts',(67.6274552913591,-9.05028060184344,
41.8301481628908));
#162584=CARTESIAN_POINT('Ctrl Pts',(68.3050418504365,-9.20015181988067,
41.7269343355587));
#162585=CARTESIAN_POINT('Ctrl Pts',(68.6068668020621,-9.25120264826099,
41.6809740186536));
#162586=CARTESIAN_POINT('Ctrl Pts',(69.0786157844767,-9.30685380816212,
41.6088766939587));
#162587=CARTESIAN_POINT('Ctrl Pts',(69.247122100101,-9.32200665805263,41.5830710879211));
#162588=CARTESIAN_POINT('Ctrl Pts',(69.5336200930502,-9.33977428608612,
41.5390363942365));
#162589=CARTESIAN_POINT('Ctrl Pts',(69.6514314265196,-9.34479470213056,
41.5208830735776));
#162590=CARTESIAN_POINT('Ctrl Pts',(69.8281932716483,-9.34890264439575,
41.4935540956125));
#162591=CARTESIAN_POINT('Ctrl Pts',(69.8871000254112,-9.34970168861369,
41.4844312333286));
#162592=CARTESIAN_POINT('Ctrl Pts',(69.997275621315,-9.35013033339449,41.4673358181496));
#162593=CARTESIAN_POINT('Ctrl Pts',(70.0485416037169,-9.34989815091215,
41.459367518842));
#162594=CARTESIAN_POINT('Ctrl Pts',(70.1772609579311,-9.34823126487482,
41.4393294720256));
#162595=CARTESIAN_POINT('Ctrl Pts',(70.2547010417848,-9.34624262758035,
41.4272461720832));
#162596=CARTESIAN_POINT('Ctrl Pts',(70.6077408026198,-9.33267912822794,
41.3720569225812));
#162597=CARTESIAN_POINT('Ctrl Pts',(70.8827266366174,-9.30960375154021,
41.328786045328));
#162598=CARTESIAN_POINT('Ctrl Pts',(71.4786588249724,-9.23228136575298,
41.2348804135636));
#162599=CARTESIAN_POINT('Ctrl Pts',(71.7986257557919,-9.17325895049772,
41.1843800346556));
#162600=CARTESIAN_POINT('Ctrl Pts',(72.342588590483,-9.04259367473654,41.0988727696695));
#162601=CARTESIAN_POINT('Ctrl Pts',(72.5681695109219,-8.97916085839969,
41.0635167103407));
#162602=CARTESIAN_POINT('Ctrl Pts',(72.9619568538091,-8.85195371743119,
41.0021061027598));
#162603=CARTESIAN_POINT('Ctrl Pts',(73.1311513162953,-8.79176063488057,
40.9758237129305));
#162604=CARTESIAN_POINT('Ctrl Pts',(73.3959535992366,-8.68871239253119,
40.9348843903048));
#162605=CARTESIAN_POINT('Ctrl Pts',(73.4927442937574,-8.64913208185471,
40.9199621468301));
#162606=CARTESIAN_POINT('Ctrl Pts',(73.6778710827111,-8.56971827161967,
40.8915060770526));
#162607=CARTESIAN_POINT('Ctrl Pts',(73.7662919262214,-8.53012450610539,
40.8779528882343));
#162608=CARTESIAN_POINT('Ctrl Pts',(73.9763436929254,-8.43205866358636,
40.8458490021002));
#162609=CARTESIAN_POINT('Ctrl Pts',(74.0973632826702,-8.37228806856663,
40.8274286267294));
#162610=CARTESIAN_POINT('Ctrl Pts',(74.6569649524157,-8.080457877396,40.7426023721919));
#162611=CARTESIAN_POINT('Ctrl Pts',(75.0781191308368,-7.81571063575195,
40.6798354029987));
#162612=CARTESIAN_POINT('Ctrl Pts',(75.6633100798418,-7.3785304193032,40.5935339536315));
#162613=CARTESIAN_POINT('Ctrl Pts',(75.8449917672632,-7.23180944833177,
40.5668758260354));
#162614=CARTESIAN_POINT('Ctrl Pts',(76.1309023198231,-6.98252519568258,
40.5249948655329));
#162615=CARTESIAN_POINT('Ctrl Pts',(76.2385430941341,-6.88411964298136,
40.509244308298));
#162616=CARTESIAN_POINT('Ctrl Pts',(76.3917446776339,-6.73729212935453,
40.4868117128442));
#162617=CARTESIAN_POINT('Ctrl Pts',(76.4391543278598,-6.69087088411331,
40.4798674649997));
#162618=CARTESIAN_POINT('Ctrl Pts',(76.525480988506,-6.60451352214671,40.4672135035835));
#162619=CARTESIAN_POINT('Ctrl Pts',(76.5645416220102,-6.5647293728129,40.4614837165617));
#162620=CARTESIAN_POINT('Ctrl Pts',(76.6619879975111,-6.46367583140274,
40.4471820237762));
#162621=CARTESIAN_POINT('Ctrl Pts',(76.7199042802555,-6.40195169814966,
40.4386756707877));
#162622=CARTESIAN_POINT('Ctrl Pts',(77.0892337656632,-5.99742636585881,
40.3844338402149));
#162623=CARTESIAN_POINT('Ctrl Pts',(77.3757961496233,-5.63233742154819,
40.3423880478601));
#162624=CARTESIAN_POINT('Ctrl Pts',(77.7820342517149,-5.02742982705434,
40.284317357488));
#162625=CARTESIAN_POINT('Ctrl Pts',(77.9203513171859,-4.80140138535834,
40.2648919103462));
#162626=CARTESIAN_POINT('Ctrl Pts',(78.142025478371,-4.40232287747439,40.2345949898328));
#162627=CARTESIAN_POINT('Ctrl Pts',(78.2299333856523,-4.23205933128081,
40.2228516143285));
#162628=CARTESIAN_POINT('Ctrl Pts',(78.3588006025984,-3.96269286383592,
40.2061262997943));
#162629=CARTESIAN_POINT('Ctrl Pts',(78.4033342095557,-3.86540306993304,
40.2004502548094));
#162630=CARTESIAN_POINT('Ctrl Pts',(78.4851673309505,-3.6783154635528,40.1902310233285));
#162631=CARTESIAN_POINT('Ctrl Pts',(78.5227506950441,-3.5886601531748,40.185632298419));
#162632=CARTESIAN_POINT('Ctrl Pts',(78.6081188072846,-3.37589526788816,
40.1754205456761));
#162633=CARTESIAN_POINT('Ctrl Pts',(78.6547280866305,-3.2523257553825,40.1700352135047));
#162634=CARTESIAN_POINT('Ctrl Pts',(78.8296919525895,-2.7574251485224,40.1506164171643));
#162635=CARTESIAN_POINT('Ctrl Pts',(78.9375706290344,-2.37913078600191,
40.1405396493626));
#162636=CARTESIAN_POINT('Ctrl Pts',(79.088903231862,-1.68861472449073,40.1302445082864));
#162637=CARTESIAN_POINT('Ctrl Pts',(79.1408640991085,-1.37888099422469,
40.1284493686468));
#162638=CARTESIAN_POINT('Ctrl Pts',(79.1969131225495,-0.900273005267662,
40.1296765040502));
#162639=CARTESIAN_POINT('Ctrl Pts',(79.2120166812241,-0.732911620517043,
40.1308460556071));
#162640=CARTESIAN_POINT('Ctrl Pts',(79.2301201692722,-0.44767165747966,
40.1340304238583));
#162641=CARTESIAN_POINT('Ctrl Pts',(79.2353864904712,-0.329973162623383,
40.1356878913297));
#162642=CARTESIAN_POINT('Ctrl Pts',(79.2399953393638,-0.152896613307061,
40.1386753662714));
#162643=CARTESIAN_POINT('Ctrl Pts',(79.2409805733825,-0.0935687617643085,
40.1397595508864));
#162644=CARTESIAN_POINT('Ctrl Pts',(79.2417756441276,0.0171343571310466,
40.141934201697));
#162645=CARTESIAN_POINT('Ctrl Pts',(79.2417253579129,0.0685061561100905,
40.1430038747896));
#162646=CARTESIAN_POINT('Ctrl Pts',(79.2405393723288,0.198316966753727,
40.145862727036));
#162647=CARTESIAN_POINT('Ctrl Pts',(79.2388456017844,0.276745149006882,
40.1477341199066));
#162648=CARTESIAN_POINT('Ctrl Pts',(79.2266958131471,0.633535895710569,
40.1569280019748));
#162649=CARTESIAN_POINT('Ctrl Pts',(79.2049162706054,0.911324727069258,
40.1659752389582));
#162650=CARTESIAN_POINT('Ctrl Pts',(79.1308201840326,1.51398763254161,40.1902043929339));
#162651=CARTESIAN_POINT('Ctrl Pts',(79.0737472684379,1.83786918713272,40.2061862422928));
#162652=CARTESIAN_POINT('Ctrl Pts',(78.9468693572766,2.38863464562249,40.238969619491));
#162653=CARTESIAN_POINT('Ctrl Pts',(78.8851227375613,2.61713516379628,40.2542807779887));
#162654=CARTESIAN_POINT('Ctrl Pts',(78.7611506449948,3.01591201382421,40.2841708442066));
#162655=CARTESIAN_POINT('Ctrl Pts',(78.7024520071846,3.18720337326598,40.2980741250929));
#162656=CARTESIAN_POINT('Ctrl Pts',(78.6019158418613,3.45521180937599,40.3215562307497));
#162657=CARTESIAN_POINT('Ctrl Pts',(78.5632988779197,3.55314171169037,40.3305103558352));
#162658=CARTESIAN_POINT('Ctrl Pts',(78.4858067582838,3.74040964736682,40.3483612592754));
#162659=CARTESIAN_POINT('Ctrl Pts',(78.447167727716,3.82983483705147,40.3572119692471));
#162660=CARTESIAN_POINT('Ctrl Pts',(78.3514644851321,4.04221834449071,40.3790196025696));
#162661=CARTESIAN_POINT('Ctrl Pts',(78.2931271441464,4.1645528950215,40.392223508447));
#162662=CARTESIAN_POINT('Ctrl Pts',(78.0078168789051,4.73099632096374,40.4563924015339));
#162663=CARTESIAN_POINT('Ctrl Pts',(77.7486463102321,5.15725351885749,40.5136026126321));
#162664=CARTESIAN_POINT('Ctrl Pts',(77.3206863283474,5.74872508394364,40.6059544544084));
#162665=CARTESIAN_POINT('Ctrl Pts',(77.1773309737015,5.93194861083004,40.6365997975087));
#162666=CARTESIAN_POINT('Ctrl Pts',(76.9336201816306,6.22036087167446,40.6880928754681));
#162667=CARTESIAN_POINT('Ctrl Pts',(76.8373544512968,6.3289871416315,40.7082931366534));
#162668=CARTESIAN_POINT('Ctrl Pts',(76.6936529888984,6.48362957351238,40.7382087838804));
#162669=CARTESIAN_POINT('Ctrl Pts',(76.6481937521214,6.53150765128335,40.7476393126656));
#162670=CARTESIAN_POINT('Ctrl Pts',(76.5635979181965,6.61870699883652,40.765123199216));
#162671=CARTESIAN_POINT('Ctrl Pts',(76.5246114549889,6.6581727814448,40.7731553197284));
#162672=CARTESIAN_POINT('Ctrl Pts',(76.42554841298,6.75665627434309,40.7935045246291));
#162673=CARTESIAN_POINT('Ctrl Pts',(76.365020286901,6.81519945853294,40.8058839748086));
#162674=CARTESIAN_POINT('Ctrl Pts',(75.9682628387157,7.18853890110204,40.8867298339253));
#162675=CARTESIAN_POINT('Ctrl Pts',(75.6099413168321,7.47819094610091,40.9583989267173));
#162676=CARTESIAN_POINT('Ctrl Pts',(75.0164451385431,7.88830547926034,41.0766097788688));
#162677=CARTESIAN_POINT('Ctrl Pts',(74.7948623202521,8.02776587685847,41.1206407226464));
#162678=CARTESIAN_POINT('Ctrl Pts',(74.4035970694484,8.25116612362197,41.1984160313323));
#162679=CARTESIAN_POINT('Ctrl Pts',(74.2366406441687,8.33972885840696,41.2316103939958));
#162680=CARTESIAN_POINT('Ctrl Pts',(73.9724853929517,8.46949016407435,41.2841834598402));
#162681=CARTESIAN_POINT('Ctrl Pts',(73.8770588907614,8.51432465271073,41.3031858730203));
#162682=CARTESIAN_POINT('Ctrl Pts',(73.6935421918448,8.59668187653807,41.3397547972023));
#162683=CARTESIAN_POINT('Ctrl Pts',(73.6055911216708,8.6344931792924,41.3572912992539));
#162684=CARTESIAN_POINT('Ctrl Pts',(73.3968487110747,8.72034908048617,41.3989400714942));
#162685=CARTESIAN_POINT('Ctrl Pts',(73.275607447426,8.76719525347616,41.4231521258974));
#162686=CARTESIAN_POINT('Ctrl Pts',(72.574617214981,9.0208638598537,41.5632644553005));
#162687=CARTESIAN_POINT('Ctrl Pts',(71.9767364706905,9.17050628970856,41.6833724546721));
#162688=CARTESIAN_POINT('Ctrl Pts',(71.0605389639956,9.302462670435,41.8668469884975));
#162689=CARTESIAN_POINT('Ctrl Pts',(70.7503863685099,9.33082130257006,41.9288338080033));
#162690=CARTESIAN_POINT('Ctrl Pts',(70.3616206038549,9.34610747581579,42.0060488675217));
#162691=CARTESIAN_POINT('Ctrl Pts',(70.2838490857534,9.3481559056644,42.0214710740909));
#162692=CARTESIAN_POINT('Ctrl Pts',(70.1550292026933,9.3498779470537,42.0469678176833));
#162693=CARTESIAN_POINT('Ctrl Pts',(70.103995200586,9.35012613747574,42.0570560550074));
#162694=CARTESIAN_POINT('Ctrl Pts',(69.9948658587416,9.34972886556506,42.0785990170841));
#162695=CARTESIAN_POINT('Ctrl Pts',(69.9367731595113,9.34895511508475,42.0900496851414));
#162696=CARTESIAN_POINT('Ctrl Pts',(69.7638200971652,9.34497721317344,42.1240962240466));
#162697=CARTESIAN_POINT('Ctrl Pts',(69.6489993353937,9.34013691494601,42.1466410601758));
#162698=CARTESIAN_POINT('Ctrl Pts',(69.0774723064133,9.30507980673145,42.2586587084679));
#162699=CARTESIAN_POINT('Ctrl Pts',(68.6232402608495,9.24228285780664,42.3470761869048));
#162700=CARTESIAN_POINT('Ctrl Pts',(67.9097657366036,9.08761369718184,42.4864526113399));
#162701=CARTESIAN_POINT('Ctrl Pts',(67.6466408188795,9.01799933247026,42.5379587645335));
#162702=CARTESIAN_POINT('Ctrl Pts',(67.1986103290881,8.87754214742544,42.6260568050637));
#162703=CARTESIAN_POINT('Ctrl Pts',(67.0121825414998,8.81232188638436,42.662836411051));
#162704=CARTESIAN_POINT('Ctrl Pts',(66.728038619582,8.70235398408323,42.7191261300139));
#162705=CARTESIAN_POINT('Ctrl Pts',(66.6287691797809,8.66189476760856,42.7388362275856));
#162706=CARTESIAN_POINT('Ctrl Pts',(66.4426518696476,8.58215867571236,42.7758791117684));
#162707=CARTESIAN_POINT('Ctrl Pts',(66.3556629009143,8.54325654964305,42.7932299775245));
#162708=CARTESIAN_POINT('Ctrl Pts',(66.1567159347037,8.45049602794896,42.8330003126373));
#162709=CARTESIAN_POINT('Ctrl Pts',(66.0452084712299,8.39568989749394,42.8553567766661));
#162710=CARTESIAN_POINT('Ctrl Pts',(65.6229818730283,8.17729419685852,42.9402596343588));
#162711=CARTESIAN_POINT('Ctrl Pts',(65.3205300337658,7.99793250742827,43.0016157665991));
#162712=CARTESIAN_POINT('Ctrl Pts',(64.7884762975327,7.6393216831459,43.1103061647294));
#162713=CARTESIAN_POINT('Ctrl Pts',(64.555693728138,7.46576680244353,43.158148893338));
#162714=CARTESIAN_POINT('Ctrl Pts',(64.2114205164163,7.18271738907033,43.2291182656743));
#162715=CARTESIAN_POINT('Ctrl Pts',(64.0939653786711,7.08105623785201,43.2533706087492));
#162716=CARTESIAN_POINT('Ctrl Pts',(63.8963763295433,6.9011005782983,43.294184314751));
#162717=CARTESIAN_POINT('Ctrl Pts',(63.8150213561381,6.82425344368051,43.310993443668));
#162718=CARTESIAN_POINT('Ctrl Pts',(63.6919449074068,6.70369342141377,43.3364095731042));
#162719=CARTESIAN_POINT('Ctrl Pts',(63.6492442092956,6.66103935392175,43.3452249930653));
#162720=CARTESIAN_POINT('Ctrl Pts',(63.57114551021,6.58148589477237,43.3613393772631));
#162721=CARTESIAN_POINT('Ctrl Pts',(63.5356326743738,6.54470786424593,43.3686632462788));
#162722=CARTESIAN_POINT('Ctrl Pts',(63.4369578602142,6.44081106525514,43.3890072143525));
#162723=CARTESIAN_POINT('Ctrl Pts',(63.3744753284755,6.37302697174889,43.4018825145351));
#162724=CARTESIAN_POINT('Ctrl Pts',(62.9245911232204,5.87013140533381,43.4946014586895));
#162725=CARTESIAN_POINT('Ctrl Pts',(62.5771960843905,5.39953375183719,43.5663550871684));
#162726=CARTESIAN_POINT('Ctrl Pts',(62.1328993282683,4.66149157098412,43.6609930536785));
#162727=CARTESIAN_POINT('Ctrl Pts',(62.0006027829755,4.41783077096674,43.689663020243));
#162728=CARTESIAN_POINT('Ctrl Pts',(61.8273239479175,4.06180653540181,43.7281170695393));
#162729=CARTESIAN_POINT('Ctrl Pts',(61.7774167554764,3.95410969139709,43.7393179233123));
#162730=CARTESIAN_POINT('Ctrl Pts',(61.6909444996785,3.75781204027258,43.7589693305781));
#162731=CARTESIAN_POINT('Ctrl Pts',(61.6536697688438,3.66955354728717,43.767531938949));
#162732=CARTESIAN_POINT('Ctrl Pts',(61.5747152591317,3.47431233467679,43.7858808266835));
#162733=CARTESIAN_POINT('Ctrl Pts',(61.5336302005733,3.3670972434828,43.795572422956));
#162734=CARTESIAN_POINT('Ctrl Pts',(61.4129137765412,3.03391629715225,43.8245141112171));
#162735=CARTESIAN_POINT('Ctrl Pts',(61.3399215869271,2.80555942747109,43.8427060213208));
#162736=CARTESIAN_POINT('Ctrl Pts',(61.1478459981525,2.11476964681497,43.8928282132079));
#162737=CARTESIAN_POINT('Ctrl Pts',(61.0550132523352,1.64554609932949,43.9204740621124));
#162738=CARTESIAN_POINT('Ctrl Pts',(60.9650196414983,0.897656868935989,
43.9537948646728));
#162739=CARTESIAN_POINT('Ctrl Pts',(60.9440265815614,0.622880758051866,
43.9637898398989));
#162740=CARTESIAN_POINT('Ctrl Pts',(60.9324293229476,0.2703185580429,43.9735323750012));
#162741=CARTESIAN_POINT('Ctrl Pts',(60.930828393121,0.193089743113393,43.9754774660033));
#162742=CARTESIAN_POINT('Ctrl Pts',(60.9298340898521,0.0772323930014838,
43.9781056196507));
#162743=CARTESIAN_POINT('Ctrl Pts',(60.9297371095531,0.0386165506464322,
43.9789333153312));
#162744=CARTESIAN_POINT('Ctrl Pts',(60.929874446542,8.11258948064874E-10,
43.9797121921192));
#162745=CARTESIAN_POINT('Origin',(69.6316151486327,0.,39.48523201752));
#162746=CARTESIAN_POINT('',(61.1382522597423,4.12137457381009E-10,45.1614814957336));
#162747=CARTESIAN_POINT('Ctrl Pts',(60.929874446542,8.11258948064874E-10,
43.9797121921192));
#162748=CARTESIAN_POINT('Ctrl Pts',(60.9299209905546,-0.0130872904938113,
43.9799761563382));
#162749=CARTESIAN_POINT('Ctrl Pts',(60.9299944473541,-0.0261746630590688,
43.9802345133084));
#162750=CARTESIAN_POINT('Ctrl Pts',(60.9305559774722,-0.0993897649537978,
43.9816486104862));
#162751=CARTESIAN_POINT('Ctrl Pts',(60.9315852892579,-0.159513992332572,
43.982692009763));
#162752=CARTESIAN_POINT('Ctrl Pts',(60.9364306606604,-0.341809524564983,
43.9855054951462));
#162753=CARTESIAN_POINT('Ctrl Pts',(60.9420263308532,-0.463925828462389,
43.9869132467927));
#162754=CARTESIAN_POINT('Ctrl Pts',(60.9799098776731,-1.04561529117158,
43.9914366266648));
#162755=CARTESIAN_POINT('Ctrl Pts',(61.0431576532714,-1.50257128455147,
43.9885089622415));
#162756=CARTESIAN_POINT('Ctrl Pts',(61.196879571955,-2.22243779266736,43.9748496701503));
#162757=CARTESIAN_POINT('Ctrl Pts',(61.2661133174162,-2.48915851556593,
43.9677287404019));
#162758=CARTESIAN_POINT('Ctrl Pts',(61.4055601963188,-2.9437454262255,43.9522029832889));
#162759=CARTESIAN_POINT('Ctrl Pts',(61.4702990586768,-3.13312396700213,
43.9446837347049));
#162760=CARTESIAN_POINT('Ctrl Pts',(61.579433859146,-3.42203165118672,43.9316138872546));
#162761=CARTESIAN_POINT('Ctrl Pts',(61.6196278176574,-3.5231133364541,43.9267308865454));
#162762=CARTESIAN_POINT('Ctrl Pts',(61.6988604458934,-3.71275113994098,
43.9169840127456));
#162763=CARTESIAN_POINT('Ctrl Pts',(61.7375328853101,-3.80144771614833,
43.9121779867711));
#162764=CARTESIAN_POINT('Ctrl Pts',(61.8297962834592,-4.00446676402548,
43.9006050073493));
#162765=CARTESIAN_POINT('Ctrl Pts',(61.884329831056,-4.11833143294669,43.8936883991611));
#162766=CARTESIAN_POINT('Ctrl Pts',(62.1054104245539,-4.55707892433642,
43.8653597829873));
#162767=CARTESIAN_POINT('Ctrl Pts',(62.2884387343257,-4.87312033652459,
43.8413251412708));
#162768=CARTESIAN_POINT('Ctrl Pts',(62.6778694553592,-5.46351443548356,
43.7888796392884));
#162769=CARTESIAN_POINT('Ctrl Pts',(62.881887916305,-5.73878786888306,43.7608591053587));
#162770=CARTESIAN_POINT('Ctrl Pts',(63.2153108346265,-6.14073293624203,
43.713894031657));
#162771=CARTESIAN_POINT('Ctrl Pts',(63.3342233444991,-6.27595708622766,
43.6969434999822));
#162772=CARTESIAN_POINT('Ctrl Pts',(63.5053464971005,-6.45960618691284,
43.6722085539644));
#162773=CARTESIAN_POINT('Ctrl Pts',(63.5543718618513,-6.51103393484578,
43.6650850600835));
#162774=CARTESIAN_POINT('Ctrl Pts',(63.6423912783223,-6.60128743304134,
43.6522244252394));
#162775=CARTESIAN_POINT('Ctrl Pts',(63.6811540387599,-6.64033917557308,
43.6465364309264));
#162776=CARTESIAN_POINT('Ctrl Pts',(63.7751379313936,-6.7333678802849,43.6326887798273));
#162777=CARTESIAN_POINT('Ctrl Pts',(63.8306816255785,-6.7870013250239,43.6244596838027));
#162778=CARTESIAN_POINT('Ctrl Pts',(64.0574006426934,-7.00055418815421,
43.5907106399741));
#162779=CARTESIAN_POINT('Ctrl Pts',(64.23381449234,-7.15460938819779,43.5640917397328));
#162780=CARTESIAN_POINT('Ctrl Pts',(64.4387743268022,-7.32037836359001,
43.5329262104701));
#162781=CARTESIAN_POINT('Ctrl Pts',(64.4618758988748,-7.33888065488118,
43.5294101374525));
#162782=CARTESIAN_POINT('Ctrl Pts',(64.8000552846765,-7.60708765833748,
43.4778943578133));
#162783=CARTESIAN_POINT('Ctrl Pts',(65.130663091225,-7.83595319738631,43.4269882590408));
#162784=CARTESIAN_POINT('Ctrl Pts',(65.5735765519539,-8.10161883412052,
43.3587624512361));
#162785=CARTESIAN_POINT('Ctrl Pts',(65.6733443395827,-8.1589490318013,43.3433911670074));
#162786=CARTESIAN_POINT('Ctrl Pts',(65.9212273984341,-8.29527941565562,
43.3052113253201));
#162787=CARTESIAN_POINT('Ctrl Pts',(66.0704591653968,-8.37211542221084,
43.2822364845605));
#162788=CARTESIAN_POINT('Ctrl Pts',(66.3138799281448,-8.48913397973545,
43.2448053664669));
#162789=CARTESIAN_POINT('Ctrl Pts',(66.4068054954676,-8.53191079111141,
43.2305260637269));
#162790=CARTESIAN_POINT('Ctrl Pts',(66.5890746599304,-8.61215429028374,
43.2025417815083));
#162791=CARTESIAN_POINT('Ctrl Pts',(66.6783365977451,-8.6497771458296,43.1888480763197));
#162792=CARTESIAN_POINT('Ctrl Pts',(66.8989574384825,-8.73868145263042,
43.1550316990218));
#162793=CARTESIAN_POINT('Ctrl Pts',(67.0309241653182,-8.78835710903653,
43.1348292584908));
#162794=CARTESIAN_POINT('Ctrl Pts',(67.6754425725245,-9.01415018605229,
43.0362797978487));
#162795=CARTESIAN_POINT('Ctrl Pts',(68.2015559974568,-9.14755460333897,
42.9562636022572));
#162796=CARTESIAN_POINT('Ctrl Pts',(69.0683843604958,-9.28715555386641,
42.824099270753));
#162797=CARTESIAN_POINT('Ctrl Pts',(69.4032683390661,-9.32228499097896,
42.7729429953026));
#162798=CARTESIAN_POINT('Ctrl Pts',(69.8339477564941,-9.34355427816323,
42.7066326470644));
#162799=CARTESIAN_POINT('Ctrl Pts',(69.9287245686482,-9.34675724005849,
42.6920073526985));
#162800=CARTESIAN_POINT('Ctrl Pts',(70.0780057445542,-9.34947685933313,
42.6689065932717));
#162801=CARTESIAN_POINT('Ctrl Pts',(70.1324901543966,-9.34998193955134,
42.6604617326749));
#162802=CARTESIAN_POINT('Ctrl Pts',(70.2408015793297,-9.35001689752974,
42.6436436275921));
#162803=CARTESIAN_POINT('Ctrl Pts',(70.2946264739995,-9.34955842850146,
42.6352710140456));
#162804=CARTESIAN_POINT('Ctrl Pts',(70.4399786476469,-9.3470350419613,42.6126257770812));
#162805=CARTESIAN_POINT('Ctrl Pts',(70.5314808258624,-9.34406951025991,
42.5983323429549));
#162806=CARTESIAN_POINT('Ctrl Pts',(71.1304282734307,-9.31563482140017,
42.5045823007641));
#162807=CARTESIAN_POINT('Ctrl Pts',(71.6349727166656,-9.24921818447463,
42.4247596900784));
#162808=CARTESIAN_POINT('Ctrl Pts',(72.4435959916688,-9.0732689185424,42.297474096908));
#162809=CARTESIAN_POINT('Ctrl Pts',(72.7518943480205,-8.98907594780427,
42.2490940805023));
#162810=CARTESIAN_POINT('Ctrl Pts',(73.2154763833307,-8.83603995490335,
42.1768605165121));
#162811=CARTESIAN_POINT('Ctrl Pts',(73.3741840651771,-8.77875008434609,
42.1522248331894));
#162812=CARTESIAN_POINT('Ctrl Pts',(73.6267919481791,-8.67961847217282,
42.1131889577929));
#162813=CARTESIAN_POINT('Ctrl Pts',(73.7216948123277,-8.64052966017992,
42.0985641035961));
#162814=CARTESIAN_POINT('Ctrl Pts',(73.9046859122112,-8.56155209937364,
42.0704472852389));
#162815=CARTESIAN_POINT('Ctrl Pts',(73.9928371042674,-8.52184828206404,
42.0569407723782));
#162816=CARTESIAN_POINT('Ctrl Pts',(74.2071893565151,-8.42121418381412,
42.0241925826026));
#162817=CARTESIAN_POINT('Ctrl Pts',(74.3326759785512,-8.35877049744099,
42.00510312317));
#162818=CARTESIAN_POINT('Ctrl Pts',(74.7859639522824,-8.12017141745381,
41.9364421263923));
#162819=CARTESIAN_POINT('Ctrl Pts',(75.1046785679339,-7.92698624263095,
41.8887545848755));
#162820=CARTESIAN_POINT('Ctrl Pts',(75.6663076405106,-7.53839863897533,
41.8054984011143));
#162821=CARTESIAN_POINT('Ctrl Pts',(75.9126352417361,-7.34900968334908,
41.7692840913695));
#162822=CARTESIAN_POINT('Ctrl Pts',(76.2795040988533,-7.03643446154255,
41.7155123374961));
#162823=CARTESIAN_POINT('Ctrl Pts',(76.4068203834193,-6.92173455258275,
41.6968836145567));
#162824=CARTESIAN_POINT('Ctrl Pts',(76.5815792670809,-6.75530631922667,
41.6712967221839));
#162825=CARTESIAN_POINT('Ctrl Pts',(76.6316925978708,-6.70649115315063,
41.6639574359783));
#162826=CARTESIAN_POINT('Ctrl Pts',(76.7202981554453,-6.61820890004091,
41.650971208612));
#162827=CARTESIAN_POINT('Ctrl Pts',(76.7589965028812,-6.57895958902068,
41.6452955940362));
#162828=CARTESIAN_POINT('Ctrl Pts',(76.852064834678,-6.48287184147069,41.6316381285602));
#162829=CARTESIAN_POINT('Ctrl Pts',(76.9060701671541,-6.42568035877447,
41.6237071242845));
#162830=CARTESIAN_POINT('Ctrl Pts',(77.1285637878929,-6.18399693051358,
41.5910305509958));
#162831=CARTESIAN_POINT('Ctrl Pts',(77.290382709765,-5.99337779251858,41.567261853574));
#162832=CARTESIAN_POINT('Ctrl Pts',(77.6978206354888,-5.47245776213364,
41.5078315652562));
#162833=CARTESIAN_POINT('Ctrl Pts',(77.9297592054409,-5.13190989184838,
41.4744621993957));
#162834=CARTESIAN_POINT('Ctrl Pts',(78.1981728666291,-4.67625446679963,
41.4371742514691));
#162835=CARTESIAN_POINT('Ctrl Pts',(78.2556511865557,-4.57439393170683,
41.4292803215586));
#162836=CARTESIAN_POINT('Ctrl Pts',(78.3920767067075,-4.32177106537669,
41.410794422422));
#162837=CARTESIAN_POINT('Ctrl Pts',(78.4688829512352,-4.16987133210278,
41.4006106551626));
#162838=CARTESIAN_POINT('Ctrl Pts',(78.5856855705646,-3.92251602092376,
41.3855305229244));
#162839=CARTESIAN_POINT('Ctrl Pts',(78.6282759314851,-3.82835982540036,
41.3801301387383));
#162840=CARTESIAN_POINT('Ctrl Pts',(78.7080868822639,-3.64394167841615,
41.3702129906535));
#162841=CARTESIAN_POINT('Ctrl Pts',(78.7454694341236,-3.55376602715356,
41.365664387133));
#162842=CARTESIAN_POINT('Ctrl Pts',(78.8336590320809,-3.33138650378868,
41.3551813586886));
#162843=CARTESIAN_POINT('Ctrl Pts',(78.8829151606207,-3.19857984561665,
41.349547363618));
#162844=CARTESIAN_POINT('Ctrl Pts',(79.1104129561395,-2.5403701156978,41.3246749076488));
#162845=CARTESIAN_POINT('Ctrl Pts',(79.2454394496049,-2.00089460340364,
41.3138032124655));
#162846=CARTESIAN_POINT('Ctrl Pts',(79.3851840669939,-1.12154875001106,
41.3098978866272));
#162847=CARTESIAN_POINT('Ctrl Pts',(79.4202271830719,-0.787861633838131,
41.3114882719926));
#162848=CARTESIAN_POINT('Ctrl Pts',(79.4423995195219,-0.357782861416539,
41.317082592239));
#162849=CARTESIAN_POINT('Ctrl Pts',(79.4458699131387,-0.262444002311809,
41.3185448251693));
#162850=CARTESIAN_POINT('Ctrl Pts',(79.4490650384667,-0.1120659896724,41.3211886110961));
#162851=CARTESIAN_POINT('Ctrl Pts',(79.4497533589494,-0.0570512986255439,
41.3222269714023));
#162852=CARTESIAN_POINT('Ctrl Pts',(79.450141429027,0.0458317549567954,
41.3242988653224));
#162853=CARTESIAN_POINT('Ctrl Pts',(79.4499580066213,0.0936982065092859,
41.3253154275176));
#162854=CARTESIAN_POINT('Ctrl Pts',(79.4484330367104,0.227089348265823,
41.328298384151));
#162855=CARTESIAN_POINT('Ctrl Pts',(79.4462937167672,0.312597542125527,
41.3303825413586));
#162856=CARTESIAN_POINT('Ctrl Pts',(79.4239798614364,0.890640058614525,
41.3456815856209));
#162857=CARTESIAN_POINT('Ctrl Pts',(79.3664794302618,1.38079853340422,41.364634055881));
#162858=CARTESIAN_POINT('Ctrl Pts',(79.1930592154606,2.26037060267193,41.4115758706752));
#162859=CARTESIAN_POINT('Ctrl Pts',(79.0896634774893,2.65113601644154,41.4372784661021));
#162860=CARTESIAN_POINT('Ctrl Pts',(78.9153565721231,3.17255386773523,41.478753547543));
#162861=CARTESIAN_POINT('Ctrl Pts',(78.8657654608926,3.31018336640328,41.4904061176143));
#162862=CARTESIAN_POINT('Ctrl Pts',(78.7772447977201,3.53903831672365,41.5109889941186));
#162863=CARTESIAN_POINT('Ctrl Pts',(78.7400269260037,3.63092667698288,41.5195868869408));
#162864=CARTESIAN_POINT('Ctrl Pts',(78.6615879272084,3.8161385768787,41.537600870881));
#162865=CARTESIAN_POINT('Ctrl Pts',(78.6202865170046,3.90941201579866,41.547032380804));
#162866=CARTESIAN_POINT('Ctrl Pts',(78.5087579794538,4.15061849960385,41.5723669270285));
#162867=CARTESIAN_POINT('Ctrl Pts',(78.4361883237057,4.2973810929582,41.5887241858183));
#162868=CARTESIAN_POINT('Ctrl Pts',(78.2627862883836,4.62614525731714,41.6275227786336));
#162869=CARTESIAN_POINT('Ctrl Pts',(78.1596804943812,4.80679676208777,41.650399441286));
#162870=CARTESIAN_POINT('Ctrl Pts',(77.8775850972401,5.26488466117879,41.7124436014301));
#162871=CARTESIAN_POINT('Ctrl Pts',(77.6898535057495,5.53637245625685,41.7532352551908));
#162872=CARTESIAN_POINT('Ctrl Pts',(77.3361300789358,5.99382616202806,41.8289122953539));
#162873=CARTESIAN_POINT('Ctrl Pts',(77.1762363538057,6.18425650362277,41.8627602558458));
#162874=CARTESIAN_POINT('Ctrl Pts',(76.9562526692443,6.42575330159449,41.9087048707286));
#162875=CARTESIAN_POINT('Ctrl Pts',(76.902820575212,6.48293136439645,41.9198191761165));
#162876=CARTESIAN_POINT('Ctrl Pts',(76.8107200257987,6.57900494192104,41.9388929892983));
#162877=CARTESIAN_POINT('Ctrl Pts',(76.7724158704434,6.6182532544279,41.9468014458163));
#162878=CARTESIAN_POINT('Ctrl Pts',(76.6846955543587,6.70654271995284,41.9648570640654));
#162879=CARTESIAN_POINT('Ctrl Pts',(76.6350725544141,6.75536638226418,41.9750328111978));
#162880=CARTESIAN_POINT('Ctrl Pts',(76.4619578983732,6.92186803363263,42.010414973467));
#162881=CARTESIAN_POINT('Ctrl Pts',(76.3357899255324,7.03663091278496,42.0360009439495));
#162882=CARTESIAN_POINT('Ctrl Pts',(75.9720186263783,7.3494768557231,42.1093733591845));
#162883=CARTESIAN_POINT('Ctrl Pts',(75.7276207193639,7.53905058114165,42.1582185491852));
#162884=CARTESIAN_POINT('Ctrl Pts',(75.1709220369443,7.92747425024709,42.2691305383306));
#162885=CARTESIAN_POINT('Ctrl Pts',(74.8552643274913,8.1203812123864,42.3318060257228));
#162886=CARTESIAN_POINT('Ctrl Pts',(74.406064528023,8.3587553228919,42.4211344157782));
#162887=CARTESIAN_POINT('Ctrl Pts',(74.281573591726,8.4212021924072,42.4459026005887));
#162888=CARTESIAN_POINT('Ctrl Pts',(74.0689080409677,8.52183951921638,42.4882484645318));
#162889=CARTESIAN_POINT('Ctrl Pts',(73.9814469472917,8.56154390675176,42.5056733013665));
#162890=CARTESIAN_POINT('Ctrl Pts',(73.799881376015,8.64052158854995,42.5418698858085));
#162891=CARTESIAN_POINT('Ctrl Pts',(73.7057139769804,8.67960992021873,42.5606556280213));
#162892=CARTESIAN_POINT('Ctrl Pts',(73.4550564346684,8.7787385320311,42.6106958356382));
#162893=CARTESIAN_POINT('Ctrl Pts',(73.2975650648375,8.83602556366342,42.6421735631669));
#162894=CARTESIAN_POINT('Ctrl Pts',(72.8373046401687,8.98912228284667,42.7342617389544));
#162895=CARTESIAN_POINT('Ctrl Pts',(72.531108249263,9.07335714483024,42.7956500358838));
#162896=CARTESIAN_POINT('Ctrl Pts',(71.7284958395458,9.24924260375135,42.9565965913385));
#162897=CARTESIAN_POINT('Ctrl Pts',(71.2278526250868,9.31562014137933,43.057049277711));
#162898=CARTESIAN_POINT('Ctrl Pts',(70.6334199380153,9.34406208962301,43.175232095481));
#162899=CARTESIAN_POINT('Ctrl Pts',(70.5425303840906,9.34703103503685,43.1932710781474));
#162900=CARTESIAN_POINT('Ctrl Pts',(70.3981681784863,9.34955725161712,43.2218611099207));
#162901=CARTESIAN_POINT('Ctrl Pts',(70.3447213966133,9.35001641062416,43.2324324736563));
#162902=CARTESIAN_POINT('Ctrl Pts',(70.2371902283325,9.34998249508892,43.2536710627285));
#162903=CARTESIAN_POINT('Ctrl Pts',(70.1831079350329,9.34947813337265,43.2643375789638));
#162904=CARTESIAN_POINT('Ctrl Pts',(70.0349618363308,9.34676155982657,43.2935193913017));
#162905=CARTESIAN_POINT('Ctrl Pts',(69.9409170113203,9.34356234659907,43.3120038491778));
#162906=CARTESIAN_POINT('Ctrl Pts',(69.513865314358,9.32233191380107,43.3958017314541));
#162907=CARTESIAN_POINT('Ctrl Pts',(69.1818631633314,9.28728878461765,43.4605716254989));
#162908=CARTESIAN_POINT('Ctrl Pts',(68.3210744725876,9.14780960690269,43.6285286192555));
#162909=CARTESIAN_POINT('Ctrl Pts',(67.7981528737183,9.01426858421186,43.7306386355001));
#162910=CARTESIAN_POINT('Ctrl Pts',(67.1579455841596,8.78824228614249,43.8570077433325));
#162911=CARTESIAN_POINT('Ctrl Pts',(67.0270426558559,8.73858274292404,43.8829164751728));
#162912=CARTESIAN_POINT('Ctrl Pts',(66.8081873070179,8.64969885775567,43.9263647410801));
#162913=CARTESIAN_POINT('Ctrl Pts',(66.7196268544439,8.61207756716473,43.9439833051687));
#162914=CARTESIAN_POINT('Ctrl Pts',(66.5387764045311,8.5318275673468,43.9800416334691));
#162915=CARTESIAN_POINT('Ctrl Pts',(66.446568414161,8.48904191379462,43.9984695325005));
#162916=CARTESIAN_POINT('Ctrl Pts',(66.2049827429779,8.37196967333293,44.0468664988398));
#162917=CARTESIAN_POINT('Ctrl Pts',(66.0568718116279,8.29508531521283,44.0766569857511));
#162918=CARTESIAN_POINT('Ctrl Pts',(65.8108567620796,8.15865188963051,44.1263330451793));
#162919=CARTESIAN_POINT('Ctrl Pts',(65.7118336099486,8.10126735062367,44.1463826385841));
#162920=CARTESIAN_POINT('Ctrl Pts',(65.271988490689,7.8351731583931,44.2356677593333));
#162921=CARTESIAN_POINT('Ctrl Pts',(64.9437478937064,7.60586242795574,44.302943578339));
#162922=CARTESIAN_POINT('Ctrl Pts',(64.5178369365655,7.26475498713987,44.3906652689716));
#162923=CARTESIAN_POINT('Ctrl Pts',(64.4066026863542,7.17125310750033,44.4136162063759));
#162924=CARTESIAN_POINT('Ctrl Pts',(64.1897106581652,6.97999193005325,44.4584006015486));
#162925=CARTESIAN_POINT('Ctrl Pts',(64.084035169991,6.88231391618696,44.4802373122885));
#162926=CARTESIAN_POINT('Ctrl Pts',(63.9333581290706,6.73636664256785,44.5113576717171));
#162927=CARTESIAN_POINT('Ctrl Pts',(63.8865623425043,6.6900614563923,44.5210204194965));
#162928=CARTESIAN_POINT('Ctrl Pts',(63.8012128372173,6.60378598122045,44.5386345307307));
#162929=CARTESIAN_POINT('Ctrl Pts',(63.7625204231549,6.56396436231669,44.5466154792701));
#162930=CARTESIAN_POINT('Ctrl Pts',(63.66579922435,6.46261405457758,44.5665584431515));
#162931=CARTESIAN_POINT('Ctrl Pts',(63.6082402284705,6.40062458248858,44.5784201737169));
#162932=CARTESIAN_POINT('Ctrl Pts',(63.4813400024463,6.26015084017721,44.6045728241438));
#162933=CARTESIAN_POINT('Ctrl Pts',(63.4124540040022,6.18125385581165,44.6187702209928));
#162934=CARTESIAN_POINT('Ctrl Pts',(63.1905921492661,5.91829912460944,44.6645398524805));
#162935=CARTESIAN_POINT('Ctrl Pts',(63.0432962000735,5.72938605340831,44.6949995989251));
#162936=CARTESIAN_POINT('Ctrl Pts',(62.6198724885067,5.14079846788911,44.783193732117));
#162937=CARTESIAN_POINT('Ctrl Pts',(62.3672559275494,4.72463370734902,44.8367509308623));
#162938=CARTESIAN_POINT('Ctrl Pts',(62.0865672635927,4.16858268396669,44.8985438975456));
#162939=CARTESIAN_POINT('Ctrl Pts',(62.02781886073,4.04559660439793,44.9116349969973));
#162940=CARTESIAN_POINT('Ctrl Pts',(61.9316656869516,3.83246425641149,44.9333575527785));
#162941=CARTESIAN_POINT('Ctrl Pts',(61.8929534106559,3.74295411952806,44.9421958463912));
#162942=CARTESIAN_POINT('Ctrl Pts',(61.8154785592952,3.55585869649356,44.9600865498486));
#162943=CARTESIAN_POINT('Ctrl Pts',(61.7769423149437,3.458191129328,44.9691027208434));
#162944=CARTESIAN_POINT('Ctrl Pts',(61.676997221994,3.19188556461019,44.992819886734));
#162945=CARTESIAN_POINT('Ctrl Pts',(61.6187555577885,3.02206269472006,45.0070167169159));
#162946=CARTESIAN_POINT('Ctrl Pts',(61.3369077133837,2.11657346626009,45.0778441435093));
#162947=CARTESIAN_POINT('Ctrl Pts',(61.1989673516544,1.35632821540749,45.1208272762866));
#162948=CARTESIAN_POINT('Ctrl Pts',(61.1471447103106,0.464914684249992,
45.1499345847225));
#162949=CARTESIAN_POINT('Ctrl Pts',(61.1423965910819,0.342526707933256,
45.1534657989348));
#162950=CARTESIAN_POINT('Ctrl Pts',(61.1388333915165,0.159909273635988,
45.1580172834175));
#162951=CARTESIAN_POINT('Ctrl Pts',(61.1382289181497,0.099736719295513,
45.1594009230751));
#162952=CARTESIAN_POINT('Ctrl Pts',(61.13818578755,0.0263733213606727,45.1609438644884));
#162953=CARTESIAN_POINT('Ctrl Pts',(61.1382053624156,0.0131866373259202,
45.1612155277709));
#162954=CARTESIAN_POINT('Ctrl Pts',(61.1382522597423,8.24276059806775E-10,
45.1614814957336));
#162955=CARTESIAN_POINT('',(61.1677177485993,-7.6877934180699E-10,45.3285885869945));
#162956=CARTESIAN_POINT('',(60.4236626579685,-1.14504475720278E-15,41.1088424787055));
#162957=CARTESIAN_POINT('Ctrl Pts',(61.1677177485993,-1.53755753856922E-9,
45.3285885869945));
#162958=CARTESIAN_POINT('Ctrl Pts',(61.1676477590131,0.0196797378694619,
45.3281916563455));
#162959=CARTESIAN_POINT('Ctrl Pts',(61.167639291223,0.0393596012676555,
45.3277858276557));
#162960=CARTESIAN_POINT('Ctrl Pts',(61.167863801354,0.122656517391383,45.3260301005657));
#162961=CARTESIAN_POINT('Ctrl Pts',(61.1686780323739,0.186268278702916,
45.3245954280457));
#162962=CARTESIAN_POINT('Ctrl Pts',(61.173410355421,0.392916285528057,45.3196204158403));
#162963=CARTESIAN_POINT('Ctrl Pts',(61.1799347051901,0.535862702174635,
45.3156892391233));
#162964=CARTESIAN_POINT('Ctrl Pts',(61.2050985037226,0.903766273149247,
45.3042277371107));
#162965=CARTESIAN_POINT('Ctrl Pts',(61.2285507049289,1.1282763895979,45.2959329068203));
#162966=CARTESIAN_POINT('Ctrl Pts',(61.3439704193222,1.94846801799224,45.2604403057768));
#162967=CARTESIAN_POINT('Ctrl Pts',(61.4846525612222,2.53542694868968,45.2248135093029));
#162968=CARTESIAN_POINT('Ctrl Pts',(61.7237161276422,3.23224163497682,45.1681809287438));
#162969=CARTESIAN_POINT('Ctrl Pts',(61.7703237391244,3.35914822458267,45.1572613655166));
#162970=CARTESIAN_POINT('Ctrl Pts',(61.8551699609553,3.5756874316554,45.1375692710115));
#162971=CARTESIAN_POINT('Ctrl Pts',(61.8921103361962,3.66582759362413,45.1290489906753));
#162972=CARTESIAN_POINT('Ctrl Pts',(61.9718726162913,3.85217572208756,45.1107562198392));
#162973=CARTESIAN_POINT('Ctrl Pts',(62.0149227113742,3.94826665633113,45.1009395701924));
#162974=CARTESIAN_POINT('Ctrl Pts',(62.1370907716631,4.20913513340219,45.0732303231735));
#162975=CARTESIAN_POINT('Ctrl Pts',(62.2193883904309,4.37230519893804,45.0547214072867));
#162976=CARTESIAN_POINT('Ctrl Pts',(62.423551872379,4.74930801230215,45.0091735457337));
#162977=CARTESIAN_POINT('Ctrl Pts',(62.5491450406586,4.96087934971187,44.9814230874892));
#162978=CARTESIAN_POINT('Ctrl Pts',(62.9454545680935,5.57216908699487,44.8947670463164));
#162979=CARTESIAN_POINT('Ctrl Pts',(63.2387310475505,5.95567651204903,44.8317248904969));
#162980=CARTESIAN_POINT('Ctrl Pts',(63.6201647204983,6.38107464424242,44.7518600097091));
#162981=CARTESIAN_POINT('Ctrl Pts',(63.6811440950029,6.44711479845384,44.7391504286313));
#162982=CARTESIAN_POINT('Ctrl Pts',(63.7814914863825,6.55264943184969,44.7183399509459));
#162983=CARTESIAN_POINT('Ctrl Pts',(63.8202775642236,6.59270555139911,44.7103208491484));
#162984=CARTESIAN_POINT('Ctrl Pts',(63.903858481368,6.67746803081045,44.6930952566027));
#162985=CARTESIAN_POINT('Ctrl Pts',(63.9487536242128,6.72206776685744,44.6838748675467));
#162986=CARTESIAN_POINT('Ctrl Pts',(64.0860348613951,6.85566003434745,44.6557682788216));
#162987=CARTESIAN_POINT('Ctrl Pts',(64.1798054109601,6.94316600886333,44.6366877387674));
#162988=CARTESIAN_POINT('Ctrl Pts',(64.5625954944672,7.28568678347697,44.5591649764643));
#162989=CARTESIAN_POINT('Ctrl Pts',(64.8654605867275,7.52414985056887,44.498629694355));
#162990=CARTESIAN_POINT('Ctrl Pts',(65.5000399179384,7.9620734768268,44.3722405517229));
#162991=CARTESIAN_POINT('Ctrl Pts',(65.8312377835154,8.16092743258981,44.3064878143495));
#162992=CARTESIAN_POINT('Ctrl Pts',(66.2842077868128,8.39521545841935,44.216388367868));
#162993=CARTESIAN_POINT('Ctrl Pts',(66.3958786653038,8.45010302211099,44.1941648789301));
#162994=CARTESIAN_POINT('Ctrl Pts',(66.5950010223712,8.54295361129934,44.154507758706));
#162995=CARTESIAN_POINT('Ctrl Pts',(66.6820057377898,8.58186984597548,44.1371701030178));
#162996=CARTESIAN_POINT('Ctrl Pts',(66.868043911442,8.66159405905865,44.1000737286449));
#162997=CARTESIAN_POINT('Ctrl Pts',(66.967214734366,8.70203041623254,44.0802846228976));
#162998=CARTESIAN_POINT('Ctrl Pts',(67.2507284419084,8.81181845287383,44.0236682754481));
#162999=CARTESIAN_POINT('Ctrl Pts',(67.4365878878049,8.87690857348241,43.9865017852307));
#163000=CARTESIAN_POINT('Ctrl Pts',(67.8827983819796,9.01701280948911,43.8971723781408));
#163001=CARTESIAN_POINT('Ctrl Pts',(68.1446288415709,9.08646694553515,43.8446736501665));
#163002=CARTESIAN_POINT('Ctrl Pts',(68.8518744734904,9.2403893370759,43.7028506978136));
#163003=CARTESIAN_POINT('Ctrl Pts',(69.3010521594204,9.30318695348168,43.6127418206919));
#163004=CARTESIAN_POINT('Ctrl Pts',(69.8717811750552,9.33944131655441,43.4990804655496));
#163005=CARTESIAN_POINT('Ctrl Pts',(69.990654553494,9.34462815263743,43.4754539369393));
#163006=CARTESIAN_POINT('Ctrl Pts',(70.1684171434169,9.34885502096827,43.4402183116053));
#163007=CARTESIAN_POINT('Ctrl Pts',(70.2272440715516,9.34967684163236,43.4285734044959));
#163008=CARTESIAN_POINT('Ctrl Pts',(70.336861325391,9.35013343574715,43.4069074827117));
#163009=CARTESIAN_POINT('Ctrl Pts',(70.3876473481467,9.34991524572804,43.3968832234318));
#163010=CARTESIAN_POINT('Ctrl Pts',(70.5145787140558,9.34829589901693,43.3718603939617));
#163011=CARTESIAN_POINT('Ctrl Pts',(70.5907165381837,9.34635840181797,43.35687855519));
#163012=CARTESIAN_POINT('Ctrl Pts',(70.9430782427855,9.33291794706796,43.2876471116057));
#163013=CARTESIAN_POINT('Ctrl Pts',(71.2187761500021,9.30966600004778,43.2337705059214));
#163014=CARTESIAN_POINT('Ctrl Pts',(71.9615613503377,9.21244669351037,43.0887819980959));
#163015=CARTESIAN_POINT('Ctrl Pts',(72.424764235412,9.11436946647626,42.9985165699943));
#163016=CARTESIAN_POINT('Ctrl Pts',(73.0986166813944,8.91537266134385,42.8662229351626));
#163017=CARTESIAN_POINT('Ctrl Pts',(73.3163506661664,8.84194863882161,42.8233251904865));
#163018=CARTESIAN_POINT('Ctrl Pts',(73.6361121080951,8.72037471691119,42.7600266783593));
#163019=CARTESIAN_POINT('Ctrl Pts',(73.7403678569712,8.678499951483,42.7393404353094));
#163020=CARTESIAN_POINT('Ctrl Pts',(73.9301569633891,8.59813876533699,42.7015883988948));
#163021=CARTESIAN_POINT('Ctrl Pts',(74.0159186706203,8.56024553943473,42.6844929800991));
#163022=CARTESIAN_POINT('Ctrl Pts',(74.2082435135765,8.47167774716821,42.6460721122907));
#163023=CARTESIAN_POINT('Ctrl Pts',(74.3144449665,8.42023672012054,42.6247971368161));
#163024=CARTESIAN_POINT('Ctrl Pts',(74.6696079742394,8.23957366494244,42.5534494681739));
#163025=CARTESIAN_POINT('Ctrl Pts',(74.9136886731471,8.1008393207779,42.5040759136865));
#163026=CARTESIAN_POINT('Ctrl Pts',(75.4306035435402,7.77454279510815,42.3988783192705));
#163027=CARTESIAN_POINT('Ctrl Pts',(75.7005052347357,7.58291884366461,42.3435334817253));
#163028=CARTESIAN_POINT('Ctrl Pts',(76.1678518133562,7.21148272380045,42.247304416424));
#163029=CARTESIAN_POINT('Ctrl Pts',(76.3688854772619,7.03694469905623,42.2057656134607));
#163030=CARTESIAN_POINT('Ctrl Pts',(76.620200299385,6.79891853415568,42.1538510448426));
#163031=CARTESIAN_POINT('Ctrl Pts',(76.6774411557679,6.74328016953733,42.1420279427955));
#163032=CARTESIAN_POINT('Ctrl Pts',(76.7728855253443,6.64807517892203,42.1223243994538));
#163033=CARTESIAN_POINT('Ctrl Pts',(76.8114611868241,6.60890495863334,42.1143641248462));
#163034=CARTESIAN_POINT('Ctrl Pts',(76.8973358540869,6.52014047484161,42.0966523094367));
#163035=CARTESIAN_POINT('Ctrl Pts',(76.9444416088117,6.47035690471482,42.0869419779306));
#163036=CARTESIAN_POINT('Ctrl Pts',(77.1012616674015,6.3008977464525,42.0546207467143));
#163037=CARTESIAN_POINT('Ctrl Pts',(77.2084355543498,6.17881227363132,42.0325407442862));
#163038=CARTESIAN_POINT('Ctrl Pts',(77.493070476014,5.83687859668239,41.9737965593625));
#163039=CARTESIAN_POINT('Ctrl Pts',(77.663907612997,5.61153016549304,41.9384175556734));
#163040=CARTESIAN_POINT('Ctrl Pts',(78.058568218926,5.0384787869797,41.855853885111));
#163041=CARTESIAN_POINT('Ctrl Pts',(78.2701808333373,4.68281150404958,41.8108013660867));
#163042=CARTESIAN_POINT('Ctrl Pts',(78.521208736461,4.18901532643776,41.7556213406319));
#163043=CARTESIAN_POINT('Ctrl Pts',(78.5819209265913,4.06263931737579,41.7421104479428));
#163044=CARTESIAN_POINT('Ctrl Pts',(78.6798621217743,3.84646127984038,41.7200068665661));
#163045=CARTESIAN_POINT('Ctrl Pts',(78.7185648551685,3.75737750943101,41.7111809634627));
#163046=CARTESIAN_POINT('Ctrl Pts',(78.795621425458,3.57219111347478,41.693409710767));
#163047=CARTESIAN_POINT('Ctrl Pts',(78.8337847054525,3.47602074711184,41.6844949207615));
#163048=CARTESIAN_POINT('Ctrl Pts',(78.9307475605304,3.21937993075291,41.6615294758774));
#163049=CARTESIAN_POINT('Ctrl Pts',(78.9867831822521,3.0578687030203,41.6479187067432));
#163050=CARTESIAN_POINT('Ctrl Pts',(79.1313180781754,2.60146159058633,41.6117989491338));
#163051=CARTESIAN_POINT('Ctrl Pts',(79.2098338054738,2.30350981565174,41.590899710545));
#163052=CARTESIAN_POINT('Ctrl Pts',(79.3839277782985,1.48163138476183,41.5406959315158));
#163053=CARTESIAN_POINT('Ctrl Pts',(79.4501062043757,0.952357541808737,
41.5163796898752));
#163054=CARTESIAN_POINT('Ctrl Pts',(79.4752948968429,0.330771953954673,
41.4982523339804));
#163055=CARTESIAN_POINT('Ctrl Pts',(79.4776569956186,0.241428764387,41.4958981718124));
#163056=CARTESIAN_POINT('Ctrl Pts',(79.4794293668053,0.0982487996310115,
41.4925384714185));
#163057=CARTESIAN_POINT('Ctrl Pts',(79.479640148999,0.0444310586602378,
41.4913691028231));
#163058=CARTESIAN_POINT('Ctrl Pts',(79.479142108966,-0.0652733811300169,
41.4891788900632));
#163059=CARTESIAN_POINT('Ctrl Pts',(79.4783976381843,-0.121157702673901,
41.4881653415837));
#163060=CARTESIAN_POINT('Ctrl Pts',(79.4749573213269,-0.276748057348876,
41.4856225142354));
#163061=CARTESIAN_POINT('Ctrl Pts',(79.4711889742514,-0.376426368375324,
41.4843126162585));
#163062=CARTESIAN_POINT('Ctrl Pts',(79.4587711965098,-0.608378627047333,
41.4819828885302));
#163063=CARTESIAN_POINT('Ctrl Pts',(79.4489258043924,-0.740569328250936,
41.4812001631271));
#163064=CARTESIAN_POINT('Ctrl Pts',(79.4003239678058,-1.24939102268216,
41.4801997821917));
#163065=CARTESIAN_POINT('Ctrl Pts',(79.3418693483576,-1.62377876705432,
41.4837172802535));
#163066=CARTESIAN_POINT('Ctrl Pts',(79.1773345948621,-2.3780955630158,41.4986104255801));
#163067=CARTESIAN_POINT('Ctrl Pts',(79.0696242685249,-2.75689576457783,
41.5102727087625));
#163068=CARTESIAN_POINT('Ctrl Pts',(78.8946837323403,-3.25228121011682,
41.5307953126299));
#163069=CARTESIAN_POINT('Ctrl Pts',(78.8481057896132,-3.37585821025091,
41.5363712130807));
#163070=CARTESIAN_POINT('Ctrl Pts',(78.7627668173874,-3.58863083514753,
41.5467610696678));
#163071=CARTESIAN_POINT('Ctrl Pts',(78.7251882646852,-3.67828718114622,
41.551387691164));
#163072=CARTESIAN_POINT('Ctrl Pts',(78.6433493984693,-3.86537301179641,
41.5615656104316));
#163073=CARTESIAN_POINT('Ctrl Pts',(78.5988035946059,-3.96265986515513,
41.5671623259228));
#163074=CARTESIAN_POINT('Ctrl Pts',(78.469881010801,-4.23200731986905,41.5835124971289));
#163075=CARTESIAN_POINT('Ctrl Pts',(78.3819100340444,-4.40225328813357,
41.5948372670927));
#163076=CARTESIAN_POINT('Ctrl Pts',(78.1600381891994,-4.80127674475564,
41.6238024343062));
#163077=CARTESIAN_POINT('Ctrl Pts',(78.0215655062823,-5.02726844703198,
41.6421838866607));
#163078=CARTESIAN_POINT('Ctrl Pts',(77.6147944477545,-5.63219087061544,
41.6971594665461));
#163079=CARTESIAN_POINT('Ctrl Pts',(77.3278003134506,-5.99733621274991,
41.7369505904207));
#163080=CARTESIAN_POINT('Ctrl Pts',(76.9582283939438,-6.40192347428828,
41.7901257607769));
#163081=CARTESIAN_POINT('Ctrl Pts',(76.9002864452452,-6.46365309845526,
41.7985138341587));
#163082=CARTESIAN_POINT('Ctrl Pts',(76.8028168428692,-6.56471313104887,
41.8127174052415));
#163083=CARTESIAN_POINT('Ctrl Pts',(76.7637533245473,-6.60449805577137,
41.8184341197212));
#163084=CARTESIAN_POINT('Ctrl Pts',(76.6774347767246,-6.69085357916132,
41.8311212132567));
#163085=CARTESIAN_POINT('Ctrl Pts',(76.6300379103083,-6.73727242026035,
41.8381220211692));
#163086=CARTESIAN_POINT('Ctrl Pts',(76.4769084909859,-6.88408025898879,
41.8608384702931));
#163087=CARTESIAN_POINT('Ctrl Pts',(76.3693486060981,-6.98247071309434,
41.8769416089686));
#163088=CARTESIAN_POINT('Ctrl Pts',(76.0837139780331,-7.23170111570235,
41.9199911856907));
#163089=CARTESIAN_POINT('Ctrl Pts',(75.9022560713896,-7.37838660281563,
41.9476150334515));
#163090=CARTESIAN_POINT('Ctrl Pts',(75.3175820061411,-7.81562462278688,
42.0370753513736));
#163091=CARTESIAN_POINT('Ctrl Pts',(74.8967233754039,-8.0804368107359,42.1020700007053));
#163092=CARTESIAN_POINT('Ctrl Pts',(74.3372618439705,-8.37230850723725,
42.1881986386075));
#163093=CARTESIAN_POINT('Ctrl Pts',(74.2162826783661,-8.43207525160566,
42.2068116474129));
#163094=CARTESIAN_POINT('Ctrl Pts',(74.0062698268108,-8.53013655614144,
42.2390897516805));
#163095=CARTESIAN_POINT('Ctrl Pts',(73.9178544217449,-8.56972960844439,
42.252669100105));
#163096=CARTESIAN_POINT('Ctrl Pts',(73.7327177194676,-8.64914359718673,
42.2810798338431));
#163097=CARTESIAN_POINT('Ctrl Pts',(73.6359103363512,-8.68872455613769,
42.2959225395044));
#163098=CARTESIAN_POINT('Ctrl Pts',(73.3710246724264,-8.7917789126022,42.3364974534785));
#163099=CARTESIAN_POINT('Ctrl Pts',(73.2017458500141,-8.85197578528895,
42.3623858883258));
#163100=CARTESIAN_POINT('Ctrl Pts',(72.8076965428904,-8.97919331143696,
42.4225656644022));
#163101=CARTESIAN_POINT('Ctrl Pts',(72.5819205404346,-9.04263070916509,
42.4569841644419));
#163102=CARTESIAN_POINT('Ctrl Pts',(72.0374785972847,-9.17329194636696,
42.5399299344996));
#163103=CARTESIAN_POINT('Ctrl Pts',(71.7172007969965,-9.23230866803508,
42.5886787531538));
#163104=CARTESIAN_POINT('Ctrl Pts',(71.1208442236375,-9.30961048539096,
42.6797470511734));
#163105=CARTESIAN_POINT('Ctrl Pts',(70.8457261892187,-9.3326789495219,42.7218775705995));
#163106=CARTESIAN_POINT('Ctrl Pts',(70.4926140787116,-9.34624172756384,
42.7763350439376));
#163107=CARTESIAN_POINT('Ctrl Pts',(70.4151482704105,-9.34823077140995,
42.788305763241));
#163108=CARTESIAN_POINT('Ctrl Pts',(70.2864046800583,-9.34989801630088,
42.8082476338993));
#163109=CARTESIAN_POINT('Ctrl Pts',(70.2351352869908,-9.35013031059697,
42.8162016342404));
#163110=CARTESIAN_POINT('Ctrl Pts',(70.1249660759063,-9.34970187027052,
42.8333225496654));
#163111=CARTESIAN_POINT('Ctrl Pts',(70.0660702936538,-9.34890300397762,
42.8424926294406));
#163112=CARTESIAN_POINT('Ctrl Pts',(69.8893674544513,-9.34479595160383,
42.8700500438711));
#163113=CARTESIAN_POINT('Ctrl Pts',(69.7716182945313,-9.33977680912916,
42.8884730979242));
#163114=CARTESIAN_POINT('Ctrl Pts',(69.4853176391083,-9.32201404737564,
42.9333674531374));
#163115=CARTESIAN_POINT('Ctrl Pts',(69.3169613975907,-9.30686609004303,
42.9598511964446));
#163116=CARTESIAN_POINT('Ctrl Pts',(68.8455710259004,-9.25122078965999,
43.0340980317313));
#163117=CARTESIAN_POINT('Ctrl Pts',(68.5439876103763,-9.20016495741468,
43.0817036702807));
#163118=CARTESIAN_POINT('Ctrl Pts',(67.8669248606584,-9.05028083140165,
43.188258658349));
#163119=CARTESIAN_POINT('Ctrl Pts',(67.4939618036342,-8.94247031749705,
43.2467161332711));
#163120=CARTESIAN_POINT('Ctrl Pts',(67.0056423632166,-8.76708270676925,
43.3225232156578));
#163121=CARTESIAN_POINT('Ctrl Pts',(66.8835136394159,-8.72025049758954,
43.3414211840847));
#163122=CARTESIAN_POINT('Ctrl Pts',(66.6732015555481,-8.63441124246578,
43.3738476573233));
#163123=CARTESIAN_POINT('Ctrl Pts',(66.5845683953219,-8.59660041560209,
43.3874766276869));
#163124=CARTESIAN_POINT('Ctrl Pts',(66.3995919563377,-8.51423282012452,
43.4158403043125));
#163125=CARTESIAN_POINT('Ctrl Pts',(66.3033884763813,-8.46938661504602,
43.4305454313516));
#163126=CARTESIAN_POINT('Ctrl Pts',(66.0369807405777,-8.33954956662249,
43.4711363882876));
#163127=CARTESIAN_POINT('Ctrl Pts',(65.8685543850078,-8.25091694285604,
43.4966462363669));
#163128=CARTESIAN_POINT('Ctrl Pts',(65.4736948571926,-8.02727794998775,
43.5561092902592));
#163129=CARTESIAN_POINT('Ctrl Pts',(65.2499980976918,-7.88763394094255,
43.5895148293524));
#163130=CARTESIAN_POINT('Ctrl Pts',(64.6514617240409,-7.47747101488621,
43.6783044346424));
#163131=CARTESIAN_POINT('Ctrl Pts',(64.2901615842566,-7.18801661849064,
43.7312019642404));
#163132=CARTESIAN_POINT('Ctrl Pts',(63.889825154664,-6.81495433001514,43.7898063872883));
#163133=CARTESIAN_POINT('Ctrl Pts',(63.828743787318,-6.75645643225552,43.7987487232169));
#163134=CARTESIAN_POINT('Ctrl Pts',(63.7287348522407,-6.65802457002916,
43.8134008274902));
#163135=CARTESIAN_POINT('Ctrl Pts',(63.6893573028171,-6.61856428309217,
43.8191730154925));
#163136=CARTESIAN_POINT('Ctrl Pts',(63.6038732356581,-6.53134496740896,
43.8317127601257));
#163137=CARTESIAN_POINT('Ctrl Pts',(63.5579173868938,-6.48344068798444,
43.838459179878));
#163138=CARTESIAN_POINT('Ctrl Pts',(63.412529346836,-6.32860560631025,43.8598083270838));
#163139=CARTESIAN_POINT('Ctrl Pts',(63.3150797588329,-6.2198049361081,43.8741268562085));
#163140=CARTESIAN_POINT('Ctrl Pts',(63.0681569641835,-5.93074023115142,
43.9103436083298));
#163141=CARTESIAN_POINT('Ctrl Pts',(62.9228009974106,-5.74701702744547,
43.9315969026629));
#163142=CARTESIAN_POINT('Ctrl Pts',(62.4900873407863,-5.15581693893105,
43.9942670015785));
#163143=CARTESIAN_POINT('Ctrl Pts',(62.2280082134259,-4.73047887605852,
44.031273141868));
#163144=CARTESIAN_POINT('Ctrl Pts',(61.9386266594116,-4.16498198074783,
44.0697887759788));
#163145=CARTESIAN_POINT('Ctrl Pts',(61.879285033914,-4.04257807511931,44.0775327604615));
#163146=CARTESIAN_POINT('Ctrl Pts',(61.7818807877135,-3.83011562015318,
44.0899541654868));
#163147=CARTESIAN_POINT('Ctrl Pts',(61.7425421561281,-3.74068146336149,
44.0948798755865));
#163148=CARTESIAN_POINT('Ctrl Pts',(61.6636111777775,-3.55343223335918,
44.1045638825173));
#163149=CARTESIAN_POINT('Ctrl Pts',(61.6242539690045,-3.45553064094592,
44.1092768688037));
#163150=CARTESIAN_POINT('Ctrl Pts',(61.5217424197407,-3.18770458761023,
44.1212227418835));
#163151=CARTESIAN_POINT('Ctrl Pts',(61.461801847782,-3.01657194478436,44.1278335525662));
#163152=CARTESIAN_POINT('Ctrl Pts',(61.3349750565256,-2.61826730025979,
44.1408997639938));
#163153=CARTESIAN_POINT('Ctrl Pts',(61.2716028887318,-2.39008461889601,
44.1466854827862));
#163154=CARTESIAN_POINT('Ctrl Pts',(61.0970033232018,-1.6560314643066,44.1600679346971));
#163155=CARTESIAN_POINT('Ctrl Pts',(61.0185350430739,-1.14326162752896,
44.1616014611584));
#163156=CARTESIAN_POINT('Ctrl Pts',(60.9738796242,-0.505365600360473,44.1551322452979));
#163157=CARTESIAN_POINT('Ctrl Pts',(60.9677242252422,-0.383865383910097,
44.1535310365709));
#163158=CARTESIAN_POINT('Ctrl Pts',(60.9623991499425,-0.213903533781448,
44.1507983168674));
#163159=CARTESIAN_POINT('Ctrl Pts',(60.9612549119819,-0.165511012761847,
44.1499644609149));
#163160=CARTESIAN_POINT('Ctrl Pts',(60.9598598539427,-0.0780863857449693,
44.1483592250798));
#163161=CARTESIAN_POINT('Ctrl Pts',(60.9594790287912,-0.0390670884311103,
44.1476072249968));
#163162=CARTESIAN_POINT('Ctrl Pts',(60.9593400679932,-3.72638318321969E-5,
44.1468200349313));
#163163=CARTESIAN_POINT('Origin',(69.6316151486327,0.,39.48523201752));
#163164=CARTESIAN_POINT('',(61.3760955617941,-2.33157398522526E-12,46.5103578905782));
#163165=CARTESIAN_POINT('',(61.3466300729431,3.3917537450853E-10,46.3432507993513));
#163166=CARTESIAN_POINT('',(60.4236626579685,-1.14504475720278E-15,41.1088424787055));
#163167=CARTESIAN_POINT('Ctrl Pts',(61.3760955617941,-4.66200292569332E-12,
46.5103578905782));
#163168=CARTESIAN_POINT('Ctrl Pts',(61.3759092912817,0.0523757248735538,
46.5093014980081));
#163169=CARTESIAN_POINT('Ctrl Pts',(61.3761587903896,0.104750688469651,
46.5081821108365));
#163170=CARTESIAN_POINT('Ctrl Pts',(61.3780382048011,0.24844019208441,46.5049337758213));
#163171=CARTESIAN_POINT('Ctrl Pts',(61.3805567471265,0.339734329378578,
46.5026733604136));
#163172=CARTESIAN_POINT('Ctrl Pts',(61.3969927484521,0.730209909702223,
46.4921281641318));
#163173=CARTESIAN_POINT('Ctrl Pts',(61.4237970986573,1.02861563446639,46.4818594483999));
#163174=CARTESIAN_POINT('Ctrl Pts',(61.5488534409189,1.93587297908879,46.443054388668));
#163175=CARTESIAN_POINT('Ctrl Pts',(61.6923914844532,2.53644451156582,46.4066949979011));
#163176=CARTESIAN_POINT('Ctrl Pts',(61.9363505483461,3.24398340818751,46.3489509174635));
#163177=CARTESIAN_POINT('Ctrl Pts',(61.9824078420049,3.36892239095129,46.3381664069915));
#163178=CARTESIAN_POINT('Ctrl Pts',(62.0666007587671,3.58323118613733,46.3186331981672));
#163179=CARTESIAN_POINT('Ctrl Pts',(62.1035111036226,3.67308080805578,46.3101226004056));
#163180=CARTESIAN_POINT('Ctrl Pts',(62.1836256095551,3.85983654692565,46.291754289559));
#163181=CARTESIAN_POINT('Ctrl Pts',(62.2270901101491,3.9566108614179,46.2818461710201));
#163182=CARTESIAN_POINT('Ctrl Pts',(62.3518621916264,4.22230729476755,46.2535555269216));
#163183=CARTESIAN_POINT('Ctrl Pts',(62.4365708269919,4.38950541783899,46.2345138246346));
#163184=CARTESIAN_POINT('Ctrl Pts',(62.6487579129455,4.7789416004206,46.1872078590987));
#163185=CARTESIAN_POINT('Ctrl Pts',(62.7804148627706,4.99863117742488,46.1581465729979));
#163186=CARTESIAN_POINT('Ctrl Pts',(63.1836407772189,5.6127460169362,46.0701076307508));
#163187=CARTESIAN_POINT('Ctrl Pts',(63.4765194455713,5.99162641785026,46.0072419071673));
#163188=CARTESIAN_POINT('Ctrl Pts',(63.8525971093574,6.4071830179322,45.9286142466717));
#163189=CARTESIAN_POINT('Ctrl Pts',(63.9090279660292,6.46787318500417,45.9168663315544));
#163190=CARTESIAN_POINT('Ctrl Pts',(64.0044648730185,6.56777602463498,45.8970898214856));
#163191=CARTESIAN_POINT('Ctrl Pts',(64.0430255111711,6.607419692317,45.8891236809642));
#163192=CARTESIAN_POINT('Ctrl Pts',(64.1288960647629,6.69412421921133,45.8714393256397));
#163193=CARTESIAN_POINT('Ctrl Pts',(64.1763625683649,6.7410199309346,45.8616994205242));
#163194=CARTESIAN_POINT('Ctrl Pts',(64.3320298421017,6.89150426937819,45.8298597528093));
#163195=CARTESIAN_POINT('Ctrl Pts',(64.4422222633373,6.99293746963674,45.8074787856536));
#163196=CARTESIAN_POINT('Ctrl Pts',(64.7390847999251,7.25309741080842,45.7474910223817));
#163197=CARTESIAN_POINT('Ctrl Pts',(64.9296440427546,7.4070626669649,45.7092883500508));
#163198=CARTESIAN_POINT('Ctrl Pts',(65.5046650375672,7.83480318997433,45.5944528961943));
#163199=CARTESIAN_POINT('Ctrl Pts',(65.9040388206625,8.0864675925758,45.515208836139));
#163200=CARTESIAN_POINT('Ctrl Pts',(66.4402571341688,8.36901326543865,45.4085693128488));
#163201=CARTESIAN_POINT('Ctrl Pts',(66.5613657258613,8.42941865289867,45.3844723012947));
#163202=CARTESIAN_POINT('Ctrl Pts',(66.7709729147365,8.52819061414457,45.3427330328278));
#163203=CARTESIAN_POINT('Ctrl Pts',(66.8588398441722,8.56789991570893,45.3252262025234));
#163204=CARTESIAN_POINT('Ctrl Pts',(67.0422541938191,8.64729907022667,45.2886584668199));
#163205=CARTESIAN_POINT('Ctrl Pts',(67.1378787457414,8.6867678189917,45.2695804336307));
#163206=CARTESIAN_POINT('Ctrl Pts',(67.3979329828805,8.78893599513318,45.2176594235434));
#163207=CARTESIAN_POINT('Ctrl Pts',(67.5635026141149,8.84848016295777,45.1845620049626));
#163208=CARTESIAN_POINT('Ctrl Pts',(68.4850063000921,9.14986299707237,45.0001556968078));
#163209=CARTESIAN_POINT('Ctrl Pts',(69.2673285342023,9.29586948249292,44.8425568081824));
#163210=CARTESIAN_POINT('Ctrl Pts',(70.1575257205164,9.34275452113109,44.6654754883752));
#163211=CARTESIAN_POINT('Ctrl Pts',(70.2565311917286,9.34633087032884,44.6458167574969));
#163212=CARTESIAN_POINT('Ctrl Pts',(70.4106457366081,9.34935112906579,44.6152862706049));
#163213=CARTESIAN_POINT('Ctrl Pts',(70.4657200737278,9.34992484502258,44.60438997345));
#163214=CARTESIAN_POINT('Ctrl Pts',(70.5734268766219,9.35005829707073,44.5831114312398));
#163215=CARTESIAN_POINT('Ctrl Pts',(70.6260567078356,9.34966202131723,44.572728536323));
#163216=CARTESIAN_POINT('Ctrl Pts',(70.7654478362208,9.34739016876703,44.545263405391));
#163217=CARTESIAN_POINT('Ctrl Pts',(70.8521956968284,9.34472181099317,44.5282059248447));
#163218=CARTESIAN_POINT('Ctrl Pts',(71.2873535446512,9.32503833715148,44.4427760506991));
#163219=CARTESIAN_POINT('Ctrl Pts',(71.6347226429596,9.28904679440901,44.3750115881413));
#163220=CARTESIAN_POINT('Ctrl Pts',(72.5082696565916,9.14693220932724,44.2045650957269));
#163221=CARTESIAN_POINT('Ctrl Pts',(73.0288767306544,9.01384622354657,44.1029029096697));
#163222=CARTESIAN_POINT('Ctrl Pts',(73.6670893501812,8.78862670332058,43.9769296012621));
#163223=CARTESIAN_POINT('Ctrl Pts',(73.7981798643658,8.73891257747038,43.9509841054947));
#163224=CARTESIAN_POINT('Ctrl Pts',(74.0172507323125,8.64996113655744,43.9074935005626));
#163225=CARTESIAN_POINT('Ctrl Pts',(74.1058418891245,8.61233445828667,43.8898690034339));
#163226=CARTESIAN_POINT('Ctrl Pts',(74.2866766983746,8.53210614902453,43.853814134279));
#163227=CARTESIAN_POINT('Ctrl Pts',(74.3788394554398,8.4893501038429,43.8353954761207));
#163228=CARTESIAN_POINT('Ctrl Pts',(74.6201102220708,8.37245601451012,43.7870621878547));
#163229=CARTESIAN_POINT('Ctrl Pts',(74.767958316516,8.29573370763082,43.7573251629681));
#163230=CARTESIAN_POINT('Ctrl Pts',(75.013452780197,8.15964903507803,43.7077555450065));
#163231=CARTESIAN_POINT('Ctrl Pts',(75.1122156426323,8.10244687622636,43.687759333083));
#163232=CARTESIAN_POINT('Ctrl Pts',(75.5499763567009,7.83778768918829,43.5989008626704));
#163233=CARTESIAN_POINT('Ctrl Pts',(75.8765450893125,7.60996207728207,43.5319740024443));
#163234=CARTESIAN_POINT('Ctrl Pts',(76.3886521989549,7.20067086027229,43.4265069844938));
#163235=CARTESIAN_POINT('Ctrl Pts',(76.5829946908649,7.03149106693584,43.386350993485));
#163236=CARTESIAN_POINT('Ctrl Pts',(76.8281777448555,6.79930552812252,43.3357030462511));
#163237=CARTESIAN_POINT('Ctrl Pts',(76.8854936490011,6.7436003221825,43.3238644243163));
#163238=CARTESIAN_POINT('Ctrl Pts',(76.9810194883662,6.64832139344032,43.3041440306437));
#163239=CARTESIAN_POINT('Ctrl Pts',(77.0196032349987,6.60914585381322,43.2961820691352));
#163240=CARTESIAN_POINT('Ctrl Pts',(77.1054422415198,6.52042450556793,43.278477578197));
#163241=CARTESIAN_POINT('Ctrl Pts',(77.1525053984017,6.47069052590961,43.2687760115412));
#163242=CARTESIAN_POINT('Ctrl Pts',(77.308967672514,6.30163712528161,43.2365284926531));
#163243=CARTESIAN_POINT('Ctrl Pts',(77.4158435767006,6.17992379094053,43.2145098879679));
#163244=CARTESIAN_POINT('Ctrl Pts',(77.6992878807435,5.83956577684957,43.1560122689862));
#163245=CARTESIAN_POINT('Ctrl Pts',(77.8693191906816,5.61549014546257,43.1208019706101));
#163246=CARTESIAN_POINT('Ctrl Pts',(78.2645139546696,5.04251194527642,43.0381398347686));
#163247=CARTESIAN_POINT('Ctrl Pts',(78.4771699789188,4.6854246407792,42.9928731076335));
#163248=CARTESIAN_POINT('Ctrl Pts',(78.72913729618,4.1899388385151,42.9374903421954));
#163249=CARTESIAN_POINT('Ctrl Pts',(78.7899403351605,4.06340615894743,42.923960032166));
#163250=CARTESIAN_POINT('Ctrl Pts',(78.8879825521177,3.84704605053116,42.9018346729445));
#163251=CARTESIAN_POINT('Ctrl Pts',(78.9267019681156,3.75794014902173,42.8930053765545));
#163252=CARTESIAN_POINT('Ctrl Pts',(79.0037602197051,3.57278227447287,42.8752345638923));
#163253=CARTESIAN_POINT('Ctrl Pts',(79.0419108728264,3.47666356446806,42.8663232308247));
#163254=CARTESIAN_POINT('Ctrl Pts',(79.1387714573907,3.22035477802494,42.8433835799918));
#163255=CARTESIAN_POINT('Ctrl Pts',(79.1947308873815,3.05912875198699,42.8297930039927));
#163256=CARTESIAN_POINT('Ctrl Pts',(79.4942260903285,2.1139608666272,42.754962549496));
#163257=CARTESIAN_POINT('Ctrl Pts',(79.6390112382053,1.30132120338144,42.7093879101799));
#163258=CARTESIAN_POINT('Ctrl Pts',(79.6821495521564,0.379258996189193,
42.6813477226864));
#163259=CARTESIAN_POINT('Ctrl Pts',(79.6852556293486,0.278907727998995,
42.6786115198587));
#163260=CARTESIAN_POINT('Ctrl Pts',(79.6876255680066,0.122509079759497,
42.6748527185915));
#163261=CARTESIAN_POINT('Ctrl Pts',(79.6879809167348,0.0664910649123827,
42.6736074044482));
#163262=CARTESIAN_POINT('Ctrl Pts',(79.6877110157052,-0.0432453595123394,
42.6713690019725));
#163263=CARTESIAN_POINT('Ctrl Pts',(79.6871255268144,-0.0969613195950516,
42.6703678807929));
#163264=CARTESIAN_POINT('Ctrl Pts',(79.6843675992852,-0.239514859363793,
42.6679575682373));
#163265=CARTESIAN_POINT('Ctrl Pts',(79.6814077112249,-0.328334563163165,
42.6667098978525));
#163266=CARTESIAN_POINT('Ctrl Pts',(79.6592055443577,-0.797422543436576,
42.6614231723899));
#163267=CARTESIAN_POINT('Ctrl Pts',(79.6184334884666,-1.1763568640383,42.6616689264385));
#163268=CARTESIAN_POINT('Ctrl Pts',(79.4690907847104,-2.06056441786296,
42.6716831507418));
#163269=CARTESIAN_POINT('Ctrl Pts',(79.3418353239273,-2.56138014471964,
42.6847536373139));
#163270=CARTESIAN_POINT('Ctrl Pts',(79.1276289779917,-3.18542652518842,
42.7096457391364));
#163271=CARTESIAN_POINT('Ctrl Pts',(79.0777278396359,-3.32064257997726,
42.7155828657619));
#163272=CARTESIAN_POINT('Ctrl Pts',(78.9887271607178,-3.5457915028773,42.7263769393121));
#163273=CARTESIAN_POINT('Ctrl Pts',(78.9512821880452,-3.63636332207318,
42.7309715622235));
#163274=CARTESIAN_POINT('Ctrl Pts',(78.871731083482,-3.82059426311495,42.7408352184964));
#163275=CARTESIAN_POINT('Ctrl Pts',(78.8294930825966,-3.91418092044108,
42.7461253227874));
#163276=CARTESIAN_POINT('Ctrl Pts',(78.7148205908441,-4.15757261687448,
42.7606206130241));
#163277=CARTESIAN_POINT('Ctrl Pts',(78.6399408073153,-4.30616148146556,
42.7702142684695));
#163278=CARTESIAN_POINT('Ctrl Pts',(78.4603921507384,-4.64012511377814,
42.7935081386222));
#163279=CARTESIAN_POINT('Ctrl Pts',(78.3533019401944,-4.82406594952968,
42.8075989390933));
#163280=CARTESIAN_POINT('Ctrl Pts',(78.0634210453297,-5.28524572843818,
42.8462958433948));
#163281=CARTESIAN_POINT('Ctrl Pts',(77.8720634162778,-5.55662635508195,
42.8723346140961));
#163282=CARTESIAN_POINT('Ctrl Pts',(77.5163563503823,-6.00826518082021,
42.9219010890529));
#163283=CARTESIAN_POINT('Ctrl Pts',(77.3585241201728,-6.19337025792796,
42.944234256554));
#163284=CARTESIAN_POINT('Ctrl Pts',(77.1410090962564,-6.42924515223729,
42.9755993320967));
#163285=CARTESIAN_POINT('Ctrl Pts',(77.0875455247921,-6.48579069705593,
42.9833525042654));
#163286=CARTESIAN_POINT('Ctrl Pts',(76.9950658439429,-6.58119141694582,
42.9968452903587));
#163287=CARTESIAN_POINT('Ctrl Pts',(76.9563953201769,-6.62038545717565,
43.0025113066169));
#163288=CARTESIAN_POINT('Ctrl Pts',(76.8673651571803,-6.70904220996541,
43.0156110693333));
#163289=CARTESIAN_POINT('Ctrl Pts',(76.8167910862964,-6.75827653459227,
43.0230909207361));
#163290=CARTESIAN_POINT('Ctrl Pts',(76.6379509055128,-6.92847471202823,
43.0496602949232));
#163291=CARTESIAN_POINT('Ctrl Pts',(76.5068683924809,-7.04633011891058,
43.0693444007298));
#163292=CARTESIAN_POINT('Ctrl Pts',(76.1223514603993,-7.37278962727507,
43.1275032680691));
#163293=CARTESIAN_POINT('Ctrl Pts',(75.8612509584303,-7.57167544923386,
43.167483332251));
#163294=CARTESIAN_POINT('Ctrl Pts',(75.2761365725286,-7.97010843562931,
43.2574095030625));
#163295=CARTESIAN_POINT('Ctrl Pts',(74.9492903242468,-8.16431366405078,
43.3078355788));
#163296=CARTESIAN_POINT('Ctrl Pts',(74.5000885771895,-8.39491934386381,
43.3769763652317));
#163297=CARTESIAN_POINT('Ctrl Pts',(74.3874663439199,-8.44985778293434,
43.3942999390171));
#163298=CARTESIAN_POINT('Ctrl Pts',(74.186694130876,-8.54276477195986,43.4251529447234));
#163299=CARTESIAN_POINT('Ctrl Pts',(74.0989983955568,-8.5816898511644,43.438619538588));
#163300=CARTESIAN_POINT('Ctrl Pts',(73.911534104962,-8.66140671936107,43.4673827619334));
#163301=CARTESIAN_POINT('Ctrl Pts',(73.8116268976164,-8.7018289332096,43.4826977093368));
#163302=CARTESIAN_POINT('Ctrl Pts',(73.5261941193496,-8.8115049904056,43.5264101725597));
#163303=CARTESIAN_POINT('Ctrl Pts',(73.3391333662533,-8.87651460606896,
43.5550068319848));
#163304=CARTESIAN_POINT('Ctrl Pts',(72.8902457720778,-9.01640029302703,
43.62353071672));
#163305=CARTESIAN_POINT('Ctrl Pts',(72.626923534052,-9.08575538223764,43.6636471481403));
#163306=CARTESIAN_POINT('Ctrl Pts',(71.9172353002217,-9.23922979413597,
43.7717497780101));
#163307=CARTESIAN_POINT('Ctrl Pts',(71.4671177111447,-9.30202562047584,
43.8402774469245));
#163308=CARTESIAN_POINT('Ctrl Pts',(70.8921769577753,-9.33900976848062,
43.9286193641354));
#163309=CARTESIAN_POINT('Ctrl Pts',(70.7698449820668,-9.34441377493864,
43.947464509943));
#163310=CARTESIAN_POINT('Ctrl Pts',(70.5877488657143,-9.34879410333581,
43.9756142279267));
#163311=CARTESIAN_POINT('Ctrl Pts',(70.528034374026,-9.34964483694112,43.9848610024013));
#163312=CARTESIAN_POINT('Ctrl Pts',(70.4172972151225,-9.35013650285605,
44.0020416961283));
#163313=CARTESIAN_POINT('Ctrl Pts',(70.366277578649,-9.34993553400781,44.0099707579248));
#163314=CARTESIAN_POINT('Ctrl Pts',(70.2395058105395,-9.34837380559993,
44.0297033407116));
#163315=CARTESIAN_POINT('Ctrl Pts',(70.1637658835072,-9.34649781050369,
44.041519525266));
#163316=CARTESIAN_POINT('Ctrl Pts',(69.8253223539133,-9.3338984027968,44.0944177141589));
#163317=CARTESIAN_POINT('Ctrl Pts',(69.5631570128807,-9.31277313229554,
44.1356544586938));
#163318=CARTESIAN_POINT('Ctrl Pts',(68.8376199124167,-9.22263993462805,
44.2499606108062));
#163319=CARTESIAN_POINT('Ctrl Pts',(68.3780312779604,-9.12925636895317,
44.3225503403547));
#163320=CARTESIAN_POINT('Ctrl Pts',(67.6887129841414,-8.93312670244812,
44.4305006617752));
#163321=CARTESIAN_POINT('Ctrl Pts',(67.4528842588676,-8.85555083519632,
44.4672672559396));
#163322=CARTESIAN_POINT('Ctrl Pts',(67.1122192914184,-8.72796457053197,
44.5200427427298));
#163323=CARTESIAN_POINT('Ctrl Pts',(67.0048034773589,-8.68540886517917,
44.5366338064274));
#163324=CARTESIAN_POINT('Ctrl Pts',(66.8103642404619,-8.60410466439594,
44.5665691728336));
#163325=CARTESIAN_POINT('Ctrl Pts',(66.7230932753129,-8.56601080044907,
44.5799688416452));
#163326=CARTESIAN_POINT('Ctrl Pts',(66.5304168652247,-8.47832431403028,
44.6094695718655));
#163327=CARTESIAN_POINT('Ctrl Pts',(66.425321097703,-8.42806878166995,44.6255045429834));
#163328=CARTESIAN_POINT('Ctrl Pts',(66.0870544992686,-8.25836387378462,
44.6769327109813));
#163329=CARTESIAN_POINT('Ctrl Pts',(65.85791147279,-8.13092142876955,44.7114798652892));
#163330=CARTESIAN_POINT('Ctrl Pts',(65.2106574721794,-7.73399611934188,
44.8083280265073));
#163331=CARTESIAN_POINT('Ctrl Pts',(64.8081238675418,-7.44015758791296,
44.8675887806537));
#163332=CARTESIAN_POINT('Ctrl Pts',(64.3140836543493,-7.01464388161671,
44.9399782808404));
#163333=CARTESIAN_POINT('Ctrl Pts',(64.1998672259736,-6.91121300416874,
44.9566912980124));
#163334=CARTESIAN_POINT('Ctrl Pts',(64.0373931684379,-6.75655247588688,
44.9804794082859));
#163335=CARTESIAN_POINT('Ctrl Pts',(63.987082226343,-6.70756232085959,44.9878475705288));
#163336=CARTESIAN_POINT('Ctrl Pts',(63.9022223678176,-6.62303508899495,
45.0002847078665));
#163337=CARTESIAN_POINT('Ctrl Pts',(63.8673969778365,-6.58778690016492,
45.0053918269112));
#163338=CARTESIAN_POINT('Ctrl Pts',(63.7812085642904,-6.4991456541875,45.018038219508));
#163339=CARTESIAN_POINT('Ctrl Pts',(63.7301957853784,-6.44541112584493,
45.0255289107896));
#163340=CARTESIAN_POINT('Ctrl Pts',(63.5386475524898,-6.23875699660736,
45.0536598384338));
#163341=CARTESIAN_POINT('Ctrl Pts',(63.4025573844755,-6.08171362542834,
45.0736538291482));
#163342=CARTESIAN_POINT('Ctrl Pts',(62.9739281766282,-5.55240163661811,
45.1363444327762));
#163343=CARTESIAN_POINT('Ctrl Pts',(62.7041930776312,-5.16220129278606,
45.1752995661453));
#163344=CARTESIAN_POINT('Ctrl Pts',(62.3451261146196,-4.54851625783205,
45.2250930539875));
#163345=CARTESIAN_POINT('Ctrl Pts',(62.2331903127512,-4.33952581898627,
45.2402355760548));
#163346=CARTESIAN_POINT('Ctrl Pts',(62.0792078773349,-4.02408501036952,
45.2603784013492));
#163347=CARTESIAN_POINT('Ctrl Pts',(62.0310743071458,-3.92078947451051,
45.2665599073768));
#163348=CARTESIAN_POINT('Ctrl Pts',(61.9457935966874,-3.72879914958888,
45.2772850380384));
#163349=CARTESIAN_POINT('Ctrl Pts',(61.9081119811342,-3.64036456271324,
45.2819329122069));
#163350=CARTESIAN_POINT('Ctrl Pts',(61.8262837521819,-3.43992300574851,
45.2918109057193));
#163351=CARTESIAN_POINT('Ctrl Pts',(61.782909377705,-3.32761196173122,45.29689148475));
#163352=CARTESIAN_POINT('Ctrl Pts',(61.6458653499301,-2.95162044430915,
45.3124005711507));
#163353=CARTESIAN_POINT('Ctrl Pts',(61.5616940643353,-2.68456528383426,
45.3209931751147));
#163354=CARTESIAN_POINT('Ctrl Pts',(61.3542858775893,-1.90844276427591,
45.3392348352261));
#163355=CARTESIAN_POINT('Ctrl Pts',(61.2611201549604,-1.39230848186249,
45.343229002781));
#163356=CARTESIAN_POINT('Ctrl Pts',(61.1930492975319,-0.683822521086543,
45.3389844111742));
#163357=CARTESIAN_POINT('Ctrl Pts',(61.1806351028151,-0.495995502835025,
45.3369498217409));
#163358=CARTESIAN_POINT('Ctrl Pts',(61.1712554465341,-0.236655462932668,
45.3329687035681));
#163359=CARTESIAN_POINT('Ctrl Pts',(61.1694840595521,-0.165349282080866,
45.3317522351483));
#163360=CARTESIAN_POINT('Ctrl Pts',(61.1680967670258,-0.0626889790138221,
45.3298304263121));
#163361=CARTESIAN_POINT('Ctrl Pts',(61.1678292235918,-0.0313446475437261,
45.3292207930631));
#163362=CARTESIAN_POINT('Ctrl Pts',(61.1677177485993,-1.53755753856922E-9,
45.3285885869945));
#163363=CARTESIAN_POINT('Ctrl Pts',(61.1382522597423,8.24276059806775E-10,
45.1614814957336));
#163364=CARTESIAN_POINT('Ctrl Pts',(61.1383891918146,-0.0385026941639486,
45.1622580761255));
#163365=CARTESIAN_POINT('Ctrl Pts',(61.1387590575512,-0.0770049839012811,
45.1629861025056));
#163366=CARTESIAN_POINT('Ctrl Pts',(61.140569995889,-0.192648155176659,
45.1650288677117));
#163367=CARTESIAN_POINT('Ctrl Pts',(61.1427135671748,-0.269777112292349,
45.1661989697657));
#163368=CARTESIAN_POINT('Ctrl Pts',(61.1567253435757,-0.620565322579443,
45.1706684012576));
#163369=CARTESIAN_POINT('Ctrl Pts',(61.1794464992234,-0.893682308946226,
45.1717893024998));
#163370=CARTESIAN_POINT('Ctrl Pts',(61.2740426684191,-1.63919965951693,
45.1689294731104));
#163371=CARTESIAN_POINT('Ctrl Pts',(61.3697656685128,-2.10770871118466,
45.1605693737304));
#163372=CARTESIAN_POINT('Ctrl Pts',(61.5666335727138,-2.79967176878799,
45.1393888259066));
#163373=CARTESIAN_POINT('Ctrl Pts',(61.6417695656924,-3.02981523768952,
45.1307994313242));
#163374=CARTESIAN_POINT('Ctrl Pts',(61.7656403153891,-3.36499433576385,
45.1160601589259));
#163375=CARTESIAN_POINT('Ctrl Pts',(61.8076135640718,-3.47246663252628,
45.1109854684186));
#163376=CARTESIAN_POINT('Ctrl Pts',(61.8881269110202,-3.66796089670592,
45.1011163549103));
#163377=CARTESIAN_POINT('Ctrl Pts',(61.9260631385096,-3.75621926596353,
45.0964174526486));
#163378=CARTESIAN_POINT('Ctrl Pts',(62.0138970825754,-3.95225062666079,
45.0854344918741));
#163379=CARTESIAN_POINT('Ctrl Pts',(62.0644941531437,-4.05968573230524,
45.0790393923797));
#163380=CARTESIAN_POINT('Ctrl Pts',(62.239146779262,-4.41304384895806,45.0567450957195));
#163381=CARTESIAN_POINT('Ctrl Pts',(62.3719233204807,-4.65440542066785,
45.0394581002291));
#163382=CARTESIAN_POINT('Ctrl Pts',(62.8100961257201,-5.37421576032888,
44.9813042080612));
#163383=CARTESIAN_POINT('Ctrl Pts',(63.1481812897066,-5.83078601011641,
44.9350672797241));
#163384=CARTESIAN_POINT('Ctrl Pts',(63.5948561883113,-6.33206780464021,
44.8711589950957));
#163385=CARTESIAN_POINT('Ctrl Pts',(63.6661304719093,-6.4093938041916,44.8608852320421));
#163386=CARTESIAN_POINT('Ctrl Pts',(63.7795725608885,-6.52838446585308,
44.8443995067381));
#163387=CARTESIAN_POINT('Ctrl Pts',(63.8208729940886,-6.57088939356122,
44.8383708882797));
#163388=CARTESIAN_POINT('Ctrl Pts',(63.9046311568014,-6.65546853676753,
44.8260874874132));
#163389=CARTESIAN_POINT('Ctrl Pts',(63.9470939155611,-6.69753363585606,
44.8198315201332));
#163390=CARTESIAN_POINT('Ctrl Pts',(64.0672577477718,-6.81431041144412,
44.8020552325157));
#163391=CARTESIAN_POINT('Ctrl Pts',(64.1458378504009,-6.88807497182399,
44.7903469753841));
#163392=CARTESIAN_POINT('Ctrl Pts',(64.3344021540265,-7.05903407154023,
44.7620897971016));
#163393=CARTESIAN_POINT('Ctrl Pts',(64.4454210403231,-7.15500852082844,
44.7453283414892));
#163394=CARTESIAN_POINT('Ctrl Pts',(64.9459658873624,-7.56743555634622,
44.6693607796848));
#163395=CARTESIAN_POINT('Ctrl Pts',(65.3580806882549,-7.85431584746642,
44.6058294181406));
#163396=CARTESIAN_POINT('Ctrl Pts',(65.9739878810786,-8.212460373497,44.5109478837378));
#163397=CARTESIAN_POINT('Ctrl Pts',(66.1604226371677,-8.31244403231903,
44.4822282192156));
#163398=CARTESIAN_POINT('Ctrl Pts',(66.4483600754999,-8.45430807339837,
44.4379345689287));
#163399=CARTESIAN_POINT('Ctrl Pts',(66.5474816423781,-8.50096155074436,
44.4226970802018));
#163400=CARTESIAN_POINT('Ctrl Pts',(66.7346528701072,-8.58500281343704,
44.3939497327629));
#163401=CARTESIAN_POINT('Ctrl Pts',(66.8225020233732,-8.62281039569729,
44.3804674276224));
#163402=CARTESIAN_POINT('Ctrl Pts',(67.0257915614878,-8.70656071478264,
44.34929467749));
#163403=CARTESIAN_POINT('Ctrl Pts',(67.14159978068,-8.75154299209778,44.3315557445542));
#163404=CARTESIAN_POINT('Ctrl Pts',(67.5623515620808,-8.90521351337595,
44.2671771107874));
#163405=CARTESIAN_POINT('Ctrl Pts',(67.8720017372156,-9.00006157120899,
44.2199374741881));
#163406=CARTESIAN_POINT('Ctrl Pts',(68.4640910832926,-9.14764165091881,
44.1297196239163));
#163407=CARTESIAN_POINT('Ctrl Pts',(68.7452919938032,-9.20386192961857,
44.0869155835871));
#163408=CARTESIAN_POINT('Ctrl Pts',(69.33776452813,-9.29363307788184,43.9965469013414));
#163409=CARTESIAN_POINT('Ctrl Pts',(69.6490632617353,-9.32459034501279,
43.9489615363812));
#163410=CARTESIAN_POINT('Ctrl Pts',(70.0534515474975,-9.34395539089209,
43.8866856019446));
#163411=CARTESIAN_POINT('Ctrl Pts',(70.1457040579469,-9.34697331193446,
43.8724472339339));
#163412=CARTESIAN_POINT('Ctrl Pts',(70.2919491944493,-9.34954033073362,
43.8498135742253));
#163413=CARTESIAN_POINT('Ctrl Pts',(70.3459239123,-9.35000930398093,43.8414467772714));
#163414=CARTESIAN_POINT('Ctrl Pts',(70.4542257209256,-9.34999035428335,
43.8246284789358));
#163415=CARTESIAN_POINT('Ctrl Pts',(70.5085506593413,-9.34949611816943,
43.816177147714));
#163416=CARTESIAN_POINT('Ctrl Pts',(70.6568847672363,-9.34682270338928,
43.7930646466113));
#163417=CARTESIAN_POINT('Ctrl Pts',(70.7508662883036,-9.34367611460512,
43.7783813699122));
#163418=CARTESIAN_POINT('Ctrl Pts',(71.1734548354196,-9.32298770490505,
43.7122227918697));
#163419=CARTESIAN_POINT('Ctrl Pts',(71.5009892693062,-9.28913858177973,
43.6605838916785));
#163420=CARTESIAN_POINT('Ctrl Pts',(72.3710422288497,-9.15138767381555,
43.5234167040289));
#163421=CARTESIAN_POINT('Ctrl Pts',(72.9073221554565,-9.01586112991982,
43.4389312046817));
#163422=CARTESIAN_POINT('Ctrl Pts',(73.5606217753429,-8.78635140384396,
43.3374077803584));
#163423=CARTESIAN_POINT('Ctrl Pts',(73.69156891526,-8.73695869179434,43.3171272612441));
#163424=CARTESIAN_POINT('Ctrl Pts',(73.911026502517,-8.64840418432932,43.2832679673657));
#163425=CARTESIAN_POINT('Ctrl Pts',(74.0001220585936,-8.61080851366969,
43.2695584759816));
#163426=CARTESIAN_POINT('Ctrl Pts',(74.1824827596076,-8.53044875072412,
43.2415764764608));
#163427=CARTESIAN_POINT('Ctrl Pts',(74.2756613476616,-8.48751518209136,
43.2273220468438));
#163428=CARTESIAN_POINT('Ctrl Pts',(74.5208211787036,-8.36955117402205,
43.1899334610542));
#163429=CARTESIAN_POINT('Ctrl Pts',(74.6715169352929,-8.29185492156071,
43.1670719101866));
#163430=CARTESIAN_POINT('Ctrl Pts',(74.9223226682064,-8.15366977599374,
43.1292185900963));
#163431=CARTESIAN_POINT('Ctrl Pts',(75.0235527925827,-8.09536678830495,
43.1139957886111));
#163432=CARTESIAN_POINT('Ctrl Pts',(75.4782124326391,-7.82190345719705,
43.0458590388681));
#163433=CARTESIAN_POINT('Ctrl Pts',(75.8183541324543,-7.58492369752779,
42.9955600813075));
#163434=CARTESIAN_POINT('Ctrl Pts',(76.3300352707207,-7.17493371267975,
42.9203866492962));
#163435=CARTESIAN_POINT('Ctrl Pts',(76.512452173251,-7.01671503482492,42.8936921021068));
#163436=CARTESIAN_POINT('Ctrl Pts',(76.7467121625727,-6.79695481574242,
42.8593982243701));
#163437=CARTESIAN_POINT('Ctrl Pts',(76.8041618989408,-6.74165395449314,
42.8509867349533));
#163438=CARTESIAN_POINT('Ctrl Pts',(76.9001747992212,-6.64682104063442,
42.8369186825579));
#163439=CARTESIAN_POINT('Ctrl Pts',(76.9391064783845,-6.60767643675937,
42.8312110348119));
#163440=CARTESIAN_POINT('Ctrl Pts',(77.0260472535047,-6.51868824573315,
42.8184562151595));
#163441=CARTESIAN_POINT('Ctrl Pts',(77.0738546905375,-6.46864952745328,
42.8114372410274));
#163442=CARTESIAN_POINT('Ctrl Pts',(77.2341482275809,-6.29708373989492,
42.7878979549438));
#163443=CARTESIAN_POINT('Ctrl Pts',(77.3439742623138,-6.17306294577502,
42.7717610240008));
#163444=CARTESIAN_POINT('Ctrl Pts',(77.6378611362748,-5.82283557549946,
42.7286889049466));
#163445=CARTESIAN_POINT('Ctrl Pts',(77.8147870107264,-5.59075525269269,
42.702888435309));
#163446=CARTESIAN_POINT('Ctrl Pts',(78.2099289152862,-5.01898559763149,
42.6461294373541));
#163447=CARTESIAN_POINT('Ctrl Pts',(78.4177245339355,-4.67263188716936,
42.6170308931888));
#163448=CARTESIAN_POINT('Ctrl Pts',(78.6672884620141,-4.18888980141818,
42.5837208272088));
#163449=CARTESIAN_POINT('Ctrl Pts',(78.7289477644033,-4.06253506423639,
42.5756538627039));
#163450=CARTESIAN_POINT('Ctrl Pts',(78.8285283536836,-3.84638174135585,
42.562928486005));
#163451=CARTESIAN_POINT('Ctrl Pts',(78.8679133782832,-3.75730097016881,
42.5579853493193));
#163452=CARTESIAN_POINT('Ctrl Pts',(78.9464008117894,-3.57211066688893,
42.5483300982718));
#163453=CARTESIAN_POINT('Ctrl Pts',(78.9853133825372,-3.47593325736649,
42.5436545039925));
#163454=CARTESIAN_POINT('Ctrl Pts',(79.0842976154617,-3.21924716498243,
42.5320702487633));
#163455=CARTESIAN_POINT('Ctrl Pts',(79.14161973557,-3.05769704539769,42.525693911188));
#163456=CARTESIAN_POINT('Ctrl Pts',(79.2903895957021,-2.59941208261279,
42.5101399593312));
#163457=CARTESIAN_POINT('Ctrl Pts',(79.3717270832539,-2.29956636865247,
42.5028984416816));
#163458=CARTESIAN_POINT('Ctrl Pts',(79.5517513113485,-1.47858201540354,
42.4906407088634));
#163459=CARTESIAN_POINT('Ctrl Pts',(79.6217739367768,-0.952251686110478,
42.4908670523403));
#163460=CARTESIAN_POINT('Ctrl Pts',(79.6517132336951,-0.333126884221562,
42.4992240432676));
#163461=CARTESIAN_POINT('Ctrl Pts',(79.6547752741753,-0.243274911438908,
42.5006333537901));
#163462=CARTESIAN_POINT('Ctrl Pts',(79.6576221625992,-0.0994862722151973,
42.5031920897253));
#163463=CARTESIAN_POINT('Ctrl Pts',(79.6582280669377,-0.0455690728587685,
42.5042197554209));
#163464=CARTESIAN_POINT('Ctrl Pts',(79.6585211511328,0.0641079833002689,
42.5064459190048));
#163465=CARTESIAN_POINT('Ctrl Pts',(79.6581762866144,0.119865495212415,
42.5076491650542));
#163466=CARTESIAN_POINT('Ctrl Pts',(79.6558480115764,0.274691649171249,
42.5111943210018));
#163467=CARTESIAN_POINT('Ctrl Pts',(79.652799617398,0.373733196296196,42.513694212661));
#163468=CARTESIAN_POINT('Ctrl Pts',(79.6420936919487,0.603874671675038,
42.5200676571738));
#163469=CARTESIAN_POINT('Ctrl Pts',(79.6332603593372,0.734893795255606,
42.524122862127));
#163470=CARTESIAN_POINT('Ctrl Pts',(79.5890380035763,1.23540673627678,42.5413386752479));
#163471=CARTESIAN_POINT('Ctrl Pts',(79.5346595055153,1.60276752291058,42.5575934474194));
#163472=CARTESIAN_POINT('Ctrl Pts',(79.3767974089433,2.35957425469762,42.5995738122192));
#163473=CARTESIAN_POINT('Ctrl Pts',(79.2697139851994,2.74745774704834,42.6259463748392));
#163474=CARTESIAN_POINT('Ctrl Pts',(79.0952985403823,3.25166237822745,42.6672074948404));
#163475=CARTESIAN_POINT('Ctrl Pts',(79.0495943071676,3.37534013457415,42.6779053789683));
#163476=CARTESIAN_POINT('Ctrl Pts',(78.9658154574366,3.58822616531385,42.6973377712738));
#163477=CARTESIAN_POINT('Ctrl Pts',(78.9289197674915,3.67789657022253,42.7058431698303));
#163478=CARTESIAN_POINT('Ctrl Pts',(78.8485560881626,3.86495653900656,42.7242651208208));
#163479=CARTESIAN_POINT('Ctrl Pts',(78.804806064531,3.96220429095443,42.7342362936111));
#163480=CARTESIAN_POINT('Ctrl Pts',(78.6782169860375,4.23127219419301,42.7629326486843));
#163481=CARTESIAN_POINT('Ctrl Pts',(78.5918183775931,4.40128473000045,42.78234768701));
#163482=CARTESIAN_POINT('Ctrl Pts',(78.3739004873866,4.79956818087367,42.8309088357964));
#163483=CARTESIAN_POINT('Ctrl Pts',(78.2378610238797,5.0250721335885,42.8609166741631));
#163484=CARTESIAN_POINT('Ctrl Pts',(77.8369047997137,5.63031275557458,42.9483691811843));
#163485=CARTESIAN_POINT('Ctrl Pts',(77.5531802429082,5.99616976321783,43.0092316426236));
#163486=CARTESIAN_POINT('Ctrl Pts',(77.1871134972828,6.40148009376108,43.0857908745933));
#163487=CARTESIAN_POINT('Ctrl Pts',(77.1297216062,6.46329823634021,43.0977419106633));
#163488=CARTESIAN_POINT('Ctrl Pts',(77.0331855893049,6.56445721735398,43.1177497176243));
#163489=CARTESIAN_POINT('Ctrl Pts',(76.994513494296,6.60425458471733,43.1257402737068));
#163490=CARTESIAN_POINT('Ctrl Pts',(76.9090947140926,6.69058249577736,43.1433343257902));
#163491=CARTESIAN_POINT('Ctrl Pts',(76.8622054028657,6.73696238602991,43.1529575926938));
#163492=CARTESIAN_POINT('Ctrl Pts',(76.7108635985738,6.88347422985578,43.1839190271693));
#163493=CARTESIAN_POINT('Ctrl Pts',(76.6045726332316,6.98161999258863,43.205516447744));
#163494=CARTESIAN_POINT('Ctrl Pts',(76.3225230296137,7.22998628208738,43.2625390633344));
#163495=CARTESIAN_POINT('Ctrl Pts',(76.1433896813764,7.37609803303641,43.2984791375007));
#163496=CARTESIAN_POINT('Ctrl Pts',(75.5629044394448,7.81415511477105,43.4144850285718));
#163497=CARTESIAN_POINT('Ctrl Pts',(75.1436636470306,8.08005791266137,43.4976551122374));
#163498=CARTESIAN_POINT('Ctrl Pts',(74.5869236781629,8.37267567785277,43.6083783553441));
#163499=CARTESIAN_POINT('Ctrl Pts',(74.4669916321185,8.43237178069141,43.6322419022846));
#163500=CARTESIAN_POINT('Ctrl Pts',(74.2587390179006,8.53035451895324,43.6737123006198));
#163501=CARTESIAN_POINT('Ctrl Pts',(74.171026420403,8.56993477055856,43.6911887631566));
#163502=CARTESIAN_POINT('Ctrl Pts',(73.9873057579724,8.6493509348009,43.727818352145));
#163503=CARTESIAN_POINT('Ctrl Pts',(73.8912120669089,8.68894473996208,43.7469904731175));
#163504=CARTESIAN_POINT('Ctrl Pts',(73.6281111760892,8.79210036928979,43.7995212755182));
#163505=CARTESIAN_POINT('Ctrl Pts',(73.4599176114563,8.85237169062116,43.8331448394899));
#163506=CARTESIAN_POINT('Ctrl Pts',(73.0682476616612,8.97977994567656,43.9115281011586));
#163507=CARTESIAN_POINT('Ctrl Pts',(72.8437765954576,9.04330881375593,43.9565136487428));
#163508=CARTESIAN_POINT('Ctrl Pts',(72.3032305367332,9.17391128055197,44.0648946893024));
#163509=CARTESIAN_POINT('Ctrl Pts',(71.9855779059975,9.23281836282717,44.1286303673378));
#163510=CARTESIAN_POINT('Ctrl Pts',(71.396139126813,9.30964010279295,44.2465977655833));
#163511=CARTESIAN_POINT('Ctrl Pts',(71.1253402381074,9.33253167020398,44.300676527649));
#163512=CARTESIAN_POINT('Ctrl Pts',(70.776513484022,9.3461613443158,44.3699569756783));
#163513=CARTESIAN_POINT('Ctrl Pts',(70.6990959858151,9.34818593421559,44.3853085828565));
#163514=CARTESIAN_POINT('Ctrl Pts',(70.5711860171721,9.3498794031418,44.4106247550794));
#163515=CARTESIAN_POINT('Ctrl Pts',(70.5207077770349,9.3501230910819,44.4206030718155));
#163516=CARTESIAN_POINT('Ctrl Pts',(70.4122130108698,9.34973430845383,44.4420209537332));
#163517=CARTESIAN_POINT('Ctrl Pts',(70.3541990466229,9.34896567230278,44.453456220126));
#163518=CARTESIAN_POINT('Ctrl Pts',(70.1817544940958,9.34501381780451,44.4874030365932));
#163519=CARTESIAN_POINT('Ctrl Pts',(70.0673629963074,9.3402093525268,44.5098640163913));
#163520=CARTESIAN_POINT('Ctrl Pts',(69.790844329686,9.32331070217026,44.5640620303458));
#163521=CARTESIAN_POINT('Ctrl Pts',(69.6288787146776,9.30900652781442,44.5957269268059));
#163522=CARTESIAN_POINT('Ctrl Pts',(69.1579534102891,9.25454516109661,44.6876956112489));
#163523=CARTESIAN_POINT('Ctrl Pts',(68.8505087791426,9.20274418269688,44.7476180663682));
#163524=CARTESIAN_POINT('Ctrl Pts',(68.1686521773753,9.05119811535233,44.8808490024888));
#163525=CARTESIAN_POINT('Ctrl Pts',(67.7966616690478,8.94305585212277,44.9537745060253));
#163526=CARTESIAN_POINT('Ctrl Pts',(67.3103740039708,8.76714068293004,45.0498483601642));
#163527=CARTESIAN_POINT('Ctrl Pts',(67.189122272089,8.72030120849037,45.0738654206605));
#163528=CARTESIAN_POINT('Ctrl Pts',(66.9803751612613,8.63445348628344,45.1153309446797));
#163529=CARTESIAN_POINT('Ctrl Pts',(66.892422396613,8.59664239913894,45.1328388876741));
#163530=CARTESIAN_POINT('Ctrl Pts',(66.7089068362032,8.51428014031234,45.1694500875882));
#163531=CARTESIAN_POINT('Ctrl Pts',(66.6134853209868,8.46943998561442,45.1885333538665));
#163532=CARTESIAN_POINT('Ctrl Pts',(66.3493299383934,8.33964170265897,45.2414932109064));
#163533=CARTESIAN_POINT('Ctrl Pts',(66.1823935944975,8.251045200325,45.275115282189));
#163534=CARTESIAN_POINT('Ctrl Pts',(65.7911919742105,8.0275298152719,45.3542508626446));
#163535=CARTESIAN_POINT('Ctrl Pts',(65.5696807032507,7.88798083492555,45.3993438335201));
#163536=CARTESIAN_POINT('Ctrl Pts',(64.976803850965,7.47784657526231,45.5206332480599));
#163537=CARTESIAN_POINT('Ctrl Pts',(64.6190340744635,7.18828988392634,45.5945320135782));
#163538=CARTESIAN_POINT('Ctrl Pts',(64.2226218741965,6.81508024424111,45.6764211767408));
#163539=CARTESIAN_POINT('Ctrl Pts',(64.1621396049242,6.75655917078396,45.6889145848829));
#163540=CARTESIAN_POINT('Ctrl Pts',(64.0631214673264,6.65810068743555,45.7093572118277));
#163541=CARTESIAN_POINT('Ctrl Pts',(64.0241408132752,6.61863759275749,45.7174018046744));
#163542=CARTESIAN_POINT('Ctrl Pts',(63.939531422534,6.53142857852746,45.7348538897822));
#163543=CARTESIAN_POINT('Ctrl Pts',(63.8940511714908,6.48353773236676,45.7442297823508));
#163544=CARTESIAN_POINT('Ctrl Pts',(63.7502170122502,6.32880210927485,45.7738757079306));
#163545=CARTESIAN_POINT('Ctrl Pts',(63.6538196743931,6.22009088945213,45.7937354689004));
#163546=CARTESIAN_POINT('Ctrl Pts',(63.4096578329589,5.93136086736737,45.8441023521848));
#163547=CARTESIAN_POINT('Ctrl Pts',(63.2659691884263,5.7478940184156,45.8738099494438));
#163548=CARTESIAN_POINT('Ctrl Pts',(62.837675918919,5.15655031671898,45.9629637280234));
#163549=CARTESIAN_POINT('Ctrl Pts',(62.5784233733331,4.73074206580403,46.0178922203095));
#163550=CARTESIAN_POINT('Ctrl Pts',(62.2931000338066,4.16476561179506,46.0807232472096));
#163551=CARTESIAN_POINT('Ctrl Pts',(62.2347087060269,4.04239654377244,46.0937380033867));
#163552=CARTESIAN_POINT('Ctrl Pts',(62.1389527001908,3.82997412969038,46.1153750919193));
#163553=CARTESIAN_POINT('Ctrl Pts',(62.1003054492743,3.74054447543286,46.1242003069603));
#163554=CARTESIAN_POINT('Ctrl Pts',(62.0228219007994,3.55328578285513,46.1420966381629));
#163555=CARTESIAN_POINT('Ctrl Pts',(61.9842226698562,3.45536996933814,46.1511298133378));
#163556=CARTESIAN_POINT('Ctrl Pts',(61.8837789958078,3.18745141400362,46.17497258347));
#163557=CARTESIAN_POINT('Ctrl Pts',(61.8251712753624,3.01623906647071,46.1892669265274));
#163558=CARTESIAN_POINT('Ctrl Pts',(61.7014705938649,2.61769704019826,46.2203811378928));
#163559=CARTESIAN_POINT('Ctrl Pts',(61.6399158951708,2.38935480918901,46.2366272675377));
#163560=CARTESIAN_POINT('Ctrl Pts',(61.5134742138492,1.83876015535367,46.271976884671));
#163561=CARTESIAN_POINT('Ctrl Pts',(61.4566789542818,1.514882355785,46.2897162252043));
#163562=CARTESIAN_POINT('Ctrl Pts',(61.3829730502265,0.911817358754139,
46.3167968886324));
#163563=CARTESIAN_POINT('Ctrl Pts',(61.3613509727544,0.633609519968516,
46.3269885572506));
#163564=CARTESIAN_POINT('Ctrl Pts',(61.3493294788365,0.27644775799563,46.3369130930585));
#163565=CARTESIAN_POINT('Ctrl Pts',(61.3476591515173,0.198075737816354,
46.3388963092262));
#163566=CARTESIAN_POINT('Ctrl Pts',(61.3465964072363,0.0797938840208599,
46.3415892699295));
#163567=CARTESIAN_POINT('Ctrl Pts',(61.3464881809499,0.0398973309146011,
46.3424460898535));
#163568=CARTESIAN_POINT('Ctrl Pts',(61.3466300729431,6.78351894061817E-10,
46.3432507993512));
#163569=CARTESIAN_POINT('Origin',(69.6316151486327,0.,39.48523201752));
#163570=CARTESIAN_POINT('',(61.5844733749945,-1.05941772399783E-11,47.6921271941932));
#163571=CARTESIAN_POINT('',(61.5550078861458,-4.86126027327237E-15,47.5250201029796));
#163572=CARTESIAN_POINT('',(60.4236626579685,-1.14504475720278E-15,41.1088424787055));
#163573=CARTESIAN_POINT('Ctrl Pts',(61.5844733749945,-2.11872094351994E-11,
47.6921271941932));
#163574=CARTESIAN_POINT('Ctrl Pts',(61.5842929354516,0.0507361671291354,
47.6911038706948));
#163575=CARTESIAN_POINT('Ctrl Pts',(61.5845214100859,0.101471586690972,
47.6900214356351));
#163576=CARTESIAN_POINT('Ctrl Pts',(61.5862815682886,0.241622984157713,
47.6868639103638));
#163577=CARTESIAN_POINT('Ctrl Pts',(61.5886742245124,0.331019890792252,
47.6846615324012));
#163578=CARTESIAN_POINT('Ctrl Pts',(61.6102159788509,0.85684770224775,47.6705525309141));
#163579=CARTESIAN_POINT('Ctrl Pts',(61.6583199084181,1.29142584940214,47.6541862392567));
#163580=CARTESIAN_POINT('Ctrl Pts',(61.7935917959083,2.03778638130491,47.6165165916725));
#163581=CARTESIAN_POINT('Ctrl Pts',(61.8671215260744,2.35138758969453,47.5976618126942));
#163582=CARTESIAN_POINT('Ctrl Pts',(62.0174597539692,2.87172645419634,47.5608806841529));
#163583=CARTESIAN_POINT('Ctrl Pts',(62.0858229563173,3.08071752135588,47.5445616599601));
#163584=CARTESIAN_POINT('Ctrl Pts',(62.1998241824614,3.39204170854816,47.5178368445746));
#163585=CARTESIAN_POINT('Ctrl Pts',(62.2401288325453,3.49633215786767,47.5084646823107));
#163586=CARTESIAN_POINT('Ctrl Pts',(62.3184627761913,3.68878201727469,47.4903798030388));
#163587=CARTESIAN_POINT('Ctrl Pts',(62.356007213887,3.77713137804031,47.4817614760077));
#163588=CARTESIAN_POINT('Ctrl Pts',(62.444551137137,3.97695331086373,47.4615434050977));
#163589=CARTESIAN_POINT('Ctrl Pts',(62.4963847322258,4.08802022114772,47.449781842913));
#163590=CARTESIAN_POINT('Ctrl Pts',(62.6781413189272,4.45841396233786,47.4087812380242));
#163591=CARTESIAN_POINT('Ctrl Pts',(62.8178094412927,4.7125578435906,47.3776562799437));
#163592=CARTESIAN_POINT('Ctrl Pts',(63.1814521335152,5.30709796324024,47.2976155258387));
#163593=CARTESIAN_POINT('Ctrl Pts',(63.4162224372565,5.63991142013717,47.2466884074534));
#163594=CARTESIAN_POINT('Ctrl Pts',(63.7568268631208,6.06105615200825,47.1742663267379));
#163595=CARTESIAN_POINT('Ctrl Pts',(63.8441382676801,6.16430264500433,47.1558152865586));
#163596=CARTESIAN_POINT('Ctrl Pts',(64.0009468622567,6.34168388079855,47.1229094958199));
#163597=CARTESIAN_POINT('Ctrl Pts',(64.0694756202341,6.41667133055997,47.1086019253659));
#163598=CARTESIAN_POINT('Ctrl Pts',(64.1793136706874,6.5329421853728,47.085798292829));
#163599=CARTESIAN_POINT('Ctrl Pts',(64.2198116851775,6.57500349641795,47.077416987984));
#163600=CARTESIAN_POINT('Ctrl Pts',(64.3028181220067,6.65958816724649,47.0602956712981));
#163601=CARTESIAN_POINT('Ctrl Pts',(64.3453482814871,6.70208543016566,47.0515527011133));
#163602=CARTESIAN_POINT('Ctrl Pts',(64.4673556420151,6.8216316254395,47.0265472894332));
#163603=CARTESIAN_POINT('Ctrl Pts',(64.5477973183034,6.89765283215523,47.010150283614));
#163604=CARTESIAN_POINT('Ctrl Pts',(65.038805601335,7.34518011827836,46.9105005960701));
#163605=CARTESIAN_POINT('Ctrl Pts',(65.480353797727,7.67993856850869,46.8226152984355));
#163606=CARTESIAN_POINT('Ctrl Pts',(66.1782498101072,8.11583051850937,46.6838542653863));
#163607=CARTESIAN_POINT('Ctrl Pts',(66.4139413240052,8.24885968766421,46.637026598617));
#163608=CARTESIAN_POINT('Ctrl Pts',(66.7593094615069,8.42401882617389,46.5683158940448));
#163609=CARTESIAN_POINT('Ctrl Pts',(66.864576240933,8.47488116457744,46.5473621037125));
#163610=CARTESIAN_POINT('Ctrl Pts',(67.0567483309537,8.5632067491331,46.5090814865076));
#163611=CARTESIAN_POINT('Ctrl Pts',(67.1433258714238,8.60137306869108,46.4918252635365));
#163612=CARTESIAN_POINT('Ctrl Pts',(67.335217076235,8.68240881958609,46.453553522453));
#163613=CARTESIAN_POINT('Ctrl Pts',(67.4407632375819,8.72466204937684,46.4324865824092));
#163614=CARTESIAN_POINT('Ctrl Pts',(67.7705233291266,8.84953419786848,46.3666146255636));
#163615=CARTESIAN_POINT('Ctrl Pts',(67.9971346922067,8.92524244646938,46.3212712850732));
#163616=CARTESIAN_POINT('Ctrl Pts',(68.676376836835,9.12264318304177,46.1852021866924));
#163617=CARTESIAN_POINT('Ctrl Pts',(69.1354991681207,9.21811255635417,46.0929954260109));
#163618=CARTESIAN_POINT('Ctrl Pts',(69.8655301277863,9.31138704599842,45.9469092282523));
#163619=CARTESIAN_POINT('Ctrl Pts',(70.132612834611,9.33345516464316,45.8935821136841));
#163620=CARTESIAN_POINT('Ctrl Pts',(70.4758986537097,9.34643310642858,45.82541276935));
#163621=CARTESIAN_POINT('Ctrl Pts',(70.5515222348317,9.34833764530241,45.8104188944733));
#163622=CARTESIAN_POINT('Ctrl Pts',(70.6778712594269,9.34992615942374,45.7854141189114));
#163623=CARTESIAN_POINT('Ctrl Pts',(70.7285837967516,9.35013517765976,45.7753906226654));
#163624=CARTESIAN_POINT('Ctrl Pts',(70.8383720794793,9.34965998121752,45.7537198955298));
#163625=CARTESIAN_POINT('Ctrl Pts',(70.8974450038083,9.34882288301324,45.7420774678941));
#163626=CARTESIAN_POINT('Ctrl Pts',(71.0768185555494,9.34451524391306,45.7067718257637));
#163627=CARTESIAN_POINT('Ctrl Pts',(71.1970727952368,9.33921447984585,45.6831656991541));
#163628=CARTESIAN_POINT('Ctrl Pts',(71.767970359901,9.30257568808484,45.5713006567979));
#163629=CARTESIAN_POINT('Ctrl Pts',(72.2161360986599,9.23978067162353,45.4840601309465));
#163630=CARTESIAN_POINT('Ctrl Pts',(72.9222270747495,9.08609362766255,45.3461211097089));
#163631=CARTESIAN_POINT('Ctrl Pts',(73.1839193302501,9.01669093156669,45.2948927267057));
#163632=CARTESIAN_POINT('Ctrl Pts',(73.6298976479552,8.87670134239577,45.2071950939817));
#163633=CARTESIAN_POINT('Ctrl Pts',(73.8156851763723,8.81165312246985,45.1705406976543));
#163634=CARTESIAN_POINT('Ctrl Pts',(74.099093148297,8.70192459788366,45.1143957831611));
#163635=CARTESIAN_POINT('Ctrl Pts',(74.1982541374931,8.66149560352107,45.0947069027952));
#163636=CARTESIAN_POINT('Ctrl Pts',(74.384281915816,8.58177533992011,45.057681322667));
#163637=CARTESIAN_POINT('Ctrl Pts',(74.4712880488393,8.54285445653339,45.0403267762469));
#163638=CARTESIAN_POINT('Ctrl Pts',(74.670434769791,8.44997414328666,45.0005158898019));
#163639=CARTESIAN_POINT('Ctrl Pts',(74.7821214252236,8.39505992903263,44.9781230320513));
#163640=CARTESIAN_POINT('Ctrl Pts',(75.2318753210742,8.16232396663947,44.8876825574029));
#163641=CARTESIAN_POINT('Ctrl Pts',(75.5599254332986,7.96544299901811,44.8210757649213));
#163642=CARTESIAN_POINT('Ctrl Pts',(76.1928779475659,7.52926816358422,44.6916148293074));
#163643=CARTESIAN_POINT('Ctrl Pts',(76.4969206679319,7.29002776986537,44.6289298468552));
#163644=CARTESIAN_POINT('Ctrl Pts',(76.8817031613893,6.94587147966392,44.5494635255703));
#163645=CARTESIAN_POINT('Ctrl Pts',(76.9762657471438,6.85764477573636,44.5299239699813));
#163646=CARTESIAN_POINT('Ctrl Pts',(77.1144611468848,6.72317323209954,44.5013830758345));
#163647=CARTESIAN_POINT('Ctrl Pts',(77.1594890109749,6.67844761848896,44.4920860919943));
#163648=CARTESIAN_POINT('Ctrl Pts',(77.2431542199366,6.59361772457472,44.4748209491069));
#163649=CARTESIAN_POINT('Ctrl Pts',(77.2818941931828,6.55362401444824,44.466830915629));
#163650=CARTESIAN_POINT('Ctrl Pts',(77.3818783572235,6.44852548867097,44.4462163758196));
#163651=CARTESIAN_POINT('Ctrl Pts',(77.4425576895692,6.38286767609957,44.4337122999456));
#163652=CARTESIAN_POINT('Ctrl Pts',(77.8257500122904,5.95601876208129,44.3547395037467));
#163653=CARTESIAN_POINT('Ctrl Pts',(78.1210224477279,5.57038294798842,44.2938098916412));
#163654=CARTESIAN_POINT('Ctrl Pts',(78.5184935178876,4.95741988162425,44.2100538041697));
#163655=CARTESIAN_POINT('Ctrl Pts',(78.6437057411616,4.74658094648005,44.1833469048989));
#163656=CARTESIAN_POINT('Ctrl Pts',(78.8473550659568,4.37070517350294,44.1391564574824));
#163657=CARTESIAN_POINT('Ctrl Pts',(78.9294991055963,4.20790417673299,44.1210767392552));
#163658=CARTESIAN_POINT('Ctrl Pts',(79.0514882243411,3.94747999309863,44.0937652729814));
#163659=CARTESIAN_POINT('Ctrl Pts',(79.0945127446425,3.85145197166169,44.0840294915981));
#163660=CARTESIAN_POINT('Ctrl Pts',(79.1742485775417,3.66513946355785,44.065775094472));
#163661=CARTESIAN_POINT('Ctrl Pts',(79.2111864757117,3.57497047303852,44.057220953098));
#163662=CARTESIAN_POINT('Ctrl Pts',(79.296062755395,3.35821358200969,44.0373202781904));
#163663=CARTESIAN_POINT('Ctrl Pts',(79.3426874747542,3.23111618883632,44.0261826816205));
#163664=CARTESIAN_POINT('Ctrl Pts',(79.6095671584164,2.45193874627957,43.961108463404));
#163665=CARTESIAN_POINT('Ctrl Pts',(79.7606548515972,1.77750193020893,43.9181130146766));
#163666=CARTESIAN_POINT('Ctrl Pts',(79.8565048939638,0.920491744571245,
43.8812914383959));
#163667=CARTESIAN_POINT('Ctrl Pts',(79.8710149393486,0.74838401433794,43.874785802587));
#163668=CARTESIAN_POINT('Ctrl Pts',(79.887660711033,0.456103357784508,43.8653100264595));
#163669=CARTESIAN_POINT('Ctrl Pts',(79.8922193259913,0.336127208478359,
43.8618677605506));
#163670=CARTESIAN_POINT('Ctrl Pts',(79.8956518364819,0.15635675704603,43.8574025493286));
#163671=CARTESIAN_POINT('Ctrl Pts',(79.896231078801,0.096615854261143,43.8560331407062));
#163672=CARTESIAN_POINT('Ctrl Pts',(79.8962652386196,-0.0149516582472375,
43.8536932349455));
#163673=CARTESIAN_POINT('Ctrl Pts',(79.8958591318493,-0.0667746651457365,
43.8526943805451));
#163674=CARTESIAN_POINT('Ctrl Pts',(79.893783252201,-0.196651454328757,
43.8504088285477));
#163675=CARTESIAN_POINT('Ctrl Pts',(79.8915777443699,-0.274694678543371,
43.8492322904412));
#163676=CARTESIAN_POINT('Ctrl Pts',(79.8774419494162,-0.623239351866993,
43.8448341465956));
#163677=CARTESIAN_POINT('Ctrl Pts',(79.8549509216157,-0.89320715823354,
43.8437310256787));
#163678=CARTESIAN_POINT('Ctrl Pts',(79.761097665114,-1.63513072707011,43.8465248467742));
#163679=CARTESIAN_POINT('Ctrl Pts',(79.6656921721349,-2.10318679714962,
43.8548386650293));
#163680=CARTESIAN_POINT('Ctrl Pts',(79.4698227408968,-2.79306192592099,
43.8758904798355));
#163681=CARTESIAN_POINT('Ctrl Pts',(79.3954270375592,-3.02157658766399,
43.8843862338626));
#163682=CARTESIAN_POINT('Ctrl Pts',(79.272154048444,-3.35627805357526,43.8990393336369));
#163683=CARTESIAN_POINT('Ctrl Pts',(79.2298742603108,-3.46483316014934,
43.9041472701406));
#163684=CARTESIAN_POINT('Ctrl Pts',(79.1490896085262,-3.66140620489206,
43.9140443140295));
#163685=CARTESIAN_POINT('Ctrl Pts',(79.111227501466,-3.74967598103152,43.9187317340391));
#163686=CARTESIAN_POINT('Ctrl Pts',(79.0240451250798,-3.94464965997893,
43.9296282729007));
#163687=CARTESIAN_POINT('Ctrl Pts',(78.9740660983701,-4.0510352142974,43.9359419926541));
#163688=CARTESIAN_POINT('Ctrl Pts',(78.8050064488066,-4.39406661237065,
43.9575099080971));
#163689=CARTESIAN_POINT('Ctrl Pts',(78.6779615505193,-4.62656135263761,
43.9740314033395));
#163690=CARTESIAN_POINT('Ctrl Pts',(78.280674488259,-5.28586991543662,44.0266620854071));
#163691=CARTESIAN_POINT('Ctrl Pts',(77.9857871601714,-5.69639426449568,
44.0668163399807));
#163692=CARTESIAN_POINT('Ctrl Pts',(77.5627833194022,-6.1951079653315,44.1266840464022));
#163693=CARTESIAN_POINT('Ctrl Pts',(77.4631596187382,-6.30700885685074,
44.140927466147));
#163694=CARTESIAN_POINT('Ctrl Pts',(77.3134842806087,-6.46722609250427,
44.1625752464041));
#163695=CARTESIAN_POINT('Ctrl Pts',(77.2654789458563,-6.51747918687255,
44.1695539992147));
#163696=CARTESIAN_POINT('Ctrl Pts',(77.1783702675988,-6.60665771758114,
44.1822864075788));
#163697=CARTESIAN_POINT('Ctrl Pts',(77.1394712133046,-6.64578300526042,
44.1879966853377));
#163698=CARTESIAN_POINT('Ctrl Pts',(77.0438098225237,-6.74031347790275,
44.2020968268391));
#163699=CARTESIAN_POINT('Ctrl Pts',(76.9866903220004,-6.79533882719089,
44.2105635522342));
#163700=CARTESIAN_POINT('Ctrl Pts',(76.7254401133325,-7.04067165445713,
44.2494749222281));
#163701=CARTESIAN_POINT('Ctrl Pts',(76.5136668174149,-7.22237105706044,
44.2815196386154));
#163702=CARTESIAN_POINT('Ctrl Pts',(75.8289899135573,-7.75825424614105,
44.3859355422191));
#163703=CARTESIAN_POINT('Ctrl Pts',(75.3306830973099,-8.07662238378006,
44.4629789001512));
#163704=CARTESIAN_POINT('Ctrl Pts',(74.6960227910028,-8.40105268266193,
44.5606599973577));
#163705=CARTESIAN_POINT('Ctrl Pts',(74.5851387575322,-8.45495128724056,
44.5777151784796));
#163706=CARTESIAN_POINT('Ctrl Pts',(74.3862930427995,-8.54670845206675,
44.6082706204161));
#163707=CARTESIAN_POINT('Ctrl Pts',(74.2987530858974,-8.58545587667913,
44.6217125886091));
#163708=CARTESIAN_POINT('Ctrl Pts',(74.1103622594536,-8.66534407638271,
44.6506164593381));
#163709=CARTESIAN_POINT('Ctrl Pts',(74.0093553248903,-8.7060717758318,44.6660989899191));
#163710=CARTESIAN_POINT('Ctrl Pts',(73.7163971595207,-8.81817812154903,
44.7109606166623));
#163711=CARTESIAN_POINT('Ctrl Pts',(73.5227793895229,-8.88492893541359,
44.7405556616244));
#163712=CARTESIAN_POINT('Ctrl Pts',(73.0526074671429,-9.02959950313031,
44.81231780172));
#163713=CARTESIAN_POINT('Ctrl Pts',(72.7743366292329,-9.10109686795152,
44.854702161811));
#163714=CARTESIAN_POINT('Ctrl Pts',(72.0100883376822,-9.25958522729923,
44.9711176202923));
#163715=CARTESIAN_POINT('Ctrl Pts',(71.5197864970839,-9.32052525431402,
45.0457882796291));
#163716=CARTESIAN_POINT('Ctrl Pts',(70.9431077636185,-9.34522877390416,
45.134663802177));
#163717=CARTESIAN_POINT('Ctrl Pts',(70.8589985663068,-9.34766867069676,
45.1476535652867));
#163718=CARTESIAN_POINT('Ctrl Pts',(70.7276352543985,-9.34966392969701,
45.1679927970317));
#163719=CARTESIAN_POINT('Ctrl Pts',(70.6803939688228,-9.35001496894424,
45.1753176745899));
#163720=CARTESIAN_POINT('Ctrl Pts',(70.5786665679482,-9.34998168171136,
45.1911155105324));
#163721=CARTESIAN_POINT('Ctrl Pts',(70.5241828871197,-9.34947628301745,
45.1995918244727));
#163722=CARTESIAN_POINT('Ctrl Pts',(70.3749020693892,-9.34675527259986,
45.2228526695562));
#163723=CARTESIAN_POINT('Ctrl Pts',(70.2801333916433,-9.34355063555204,
45.2376597266483));
#163724=CARTESIAN_POINT('Ctrl Pts',(69.8494099039252,-9.32226378291602,
45.3050960059052));
#163725=CARTESIAN_POINT('Ctrl Pts',(69.5145911943086,-9.28709552336704,
45.3578927054202));
#163726=CARTESIAN_POINT('Ctrl Pts',(68.6486251493079,-9.14743292108761,
45.4944157637464));
#163727=CARTESIAN_POINT('Ctrl Pts',(68.1233207982288,-9.01408871639936,
45.5771534099938));
#163728=CARTESIAN_POINT('Ctrl Pts',(67.4793680043824,-8.78841095541494,
45.6772353876486));
#163729=CARTESIAN_POINT('Ctrl Pts',(67.3474153734026,-8.73872747713203,
45.6976735660068));
#163730=CARTESIAN_POINT('Ctrl Pts',(67.1268032895602,-8.64981397540812,
45.7317133640528));
#163731=CARTESIAN_POINT('Ctrl Pts',(67.0375442484723,-8.61219032828018,
45.7454489470292));
#163732=CARTESIAN_POINT('Ctrl Pts',(66.8552747594323,-8.5319498712965,45.773418770139));
#163733=CARTESIAN_POINT('Ctrl Pts',(66.7623449495561,-8.4891772279756,45.7876362163649));
#163734=CARTESIAN_POINT('Ctrl Pts',(66.5189155672574,-8.3721832832526,45.8247640727464));
#163735=CARTESIAN_POINT('Ctrl Pts',(66.3696644570503,-8.29537015094108,
45.8474096647137));
#163736=CARTESIAN_POINT('Ctrl Pts',(66.1217267607052,-8.15909004759748,
45.8848372409637));
#163737=CARTESIAN_POINT('Ctrl Pts',(66.0219336368077,-8.10178570775886,
45.8998476125375));
#163738=CARTESIAN_POINT('Ctrl Pts',(65.5790041948646,-7.83632365892998,
45.9662455043399));
#163739=CARTESIAN_POINT('Ctrl Pts',(65.2482939337322,-7.6076674799902,46.015184367765));
#163740=CARTESIAN_POINT('Ctrl Pts',(64.7316571227747,-7.19842344716327,
46.0911276093541));
#163741=CARTESIAN_POINT('Ctrl Pts',(64.5367085343107,-7.03036358650403,
46.1196564078289));
#163742=CARTESIAN_POINT('Ctrl Pts',(64.2902792969943,-6.79939483554443,
46.155731584172));
#163743=CARTESIAN_POINT('Ctrl Pts',(64.2323534000645,-6.74367418913392,
46.1642126727656));
#163744=CARTESIAN_POINT('Ctrl Pts',(64.1358246750655,-6.6483781690436,46.1783561062047));
#163745=CARTESIAN_POINT('Ctrl Pts',(64.0968427633549,-6.60920138930952,
46.1840710023907));
#163746=CARTESIAN_POINT('Ctrl Pts',(64.0101334607199,-6.52048995157325,
46.1967916718428));
#163747=CARTESIAN_POINT('Ctrl Pts',(63.9626003298457,-6.4707673840282,46.2037702714994));
#163748=CARTESIAN_POINT('Ctrl Pts',(63.8046276084255,-6.30180719229914,
46.2269685667879));
#163749=CARTESIAN_POINT('Ctrl Pts',(63.6967354426032,-6.18017931554389,
46.2428214013686));
#163750=CARTESIAN_POINT('Ctrl Pts',(63.4106532575059,-5.84018228267994,
46.2847550609032));
#163751=CARTESIAN_POINT('Ctrl Pts',(63.2390201432225,-5.61639797040577,
46.3097955129248));
#163752=CARTESIAN_POINT('Ctrl Pts',(62.8392886966675,-5.04347252996542,
46.3673001421793));
#163753=CARTESIAN_POINT('Ctrl Pts',(62.623753983855,-4.68609939844356,46.3975289029817));
#163754=CARTESIAN_POINT('Ctrl Pts',(62.3678260815757,-4.19025164771539,
46.4316938538536));
#163755=CARTESIAN_POINT('Ctrl Pts',(62.3060310686472,-4.06366583368732,
46.4397797356504));
#163756=CARTESIAN_POINT('Ctrl Pts',(62.2062994777375,-3.8472439589025,46.4525258896893));
#163757=CARTESIAN_POINT('Ctrl Pts',(62.1668896177593,-3.75813053523251,
46.457472739046));
#163758=CARTESIAN_POINT('Ctrl Pts',(62.0884000553372,-3.57298223156225,
46.4671294501713));
#163759=CARTESIAN_POINT('Ctrl Pts',(62.0495067118821,-3.47688095411806,
46.471803467681));
#163760=CARTESIAN_POINT('Ctrl Pts',(61.9506771143066,-3.22068420441144,
46.4833718946316));
#163761=CARTESIAN_POINT('Ctrl Pts',(61.8934706957066,-3.05955440991123,
46.4897377913923));
#163762=CARTESIAN_POINT('Ctrl Pts',(61.7456597363704,-2.60461511553207,
46.505201460731));
#163763=CARTESIAN_POINT('Ctrl Pts',(61.6649033228772,-2.30777256955171,
46.5124132896182));
#163764=CARTESIAN_POINT('Ctrl Pts',(61.483313556705,-1.48442652282495,46.5248916239801));
#163765=CARTESIAN_POINT('Ctrl Pts',(61.4123666256894,-0.95244722013598,
46.5246862459331));
#163766=CARTESIAN_POINT('Ctrl Pts',(61.3825629698841,-0.328599288406227,
46.5162097791634));
#163767=CARTESIAN_POINT('Ctrl Pts',(61.3795722237579,-0.239723111787004,
46.5148100865087));
#163768=CARTESIAN_POINT('Ctrl Pts',(61.3768903644626,-0.102378217551117,
46.512360485323));
#163769=CARTESIAN_POINT('Ctrl Pts',(61.3763170637519,-0.0539295302680966,
46.5114413258576));
#163770=CARTESIAN_POINT('Ctrl Pts',(61.3761090838066,-0.00365311208907833,
46.5104314954195));
#163771=CARTESIAN_POINT('Ctrl Pts',(61.3761020578081,-0.00182655558397092,
46.5103947313045));
#163772=CARTESIAN_POINT('Ctrl Pts',(61.3760955617941,-4.66200292569332E-12,
46.5103578905782));
#163773=CARTESIAN_POINT('',(61.5550077244638,4.54923683265615E-5,47.5250191853983));
#163774=CARTESIAN_POINT('Ctrl Pts',(61.3466300729431,6.78351894061817E-10,
46.3432507993512));
#163775=CARTESIAN_POINT('Ctrl Pts',(61.3466726607641,-0.0119748847392668,
46.3434923268914));
#163776=CARTESIAN_POINT('Ctrl Pts',(61.3467377807059,-0.0239498401668987,
46.3437291599298));
#163777=CARTESIAN_POINT('Ctrl Pts',(61.3472616663556,-0.0955194346373169,
46.3451166672421));
#163778=CARTESIAN_POINT('Ctrl Pts',(61.348256014986,-0.155110844989952,
46.3461561349238));
#163779=CARTESIAN_POINT('Ctrl Pts',(61.3529156344919,-0.333901531499684,
46.3489343308675));
#163780=CARTESIAN_POINT('Ctrl Pts',(61.3582576403879,-0.453050007964962,
46.3503314868498));
#163781=CARTESIAN_POINT('Ctrl Pts',(61.3767024539108,-0.742763072692121,
46.3526667192506));
#163782=CARTESIAN_POINT('Ctrl Pts',(61.3921642298094,-0.913137614746343,
46.3531419890592));
#163783=CARTESIAN_POINT('Ctrl Pts',(61.4484768670439,-1.3902732856939,46.352084861717));
#163784=CARTESIAN_POINT('Ctrl Pts',(61.4997137632451,-1.69557791631918,
46.3486227128504));
#163785=CARTESIAN_POINT('Ctrl Pts',(61.6495225018596,-2.38089696814083,
46.335037561194));
#163786=CARTESIAN_POINT('Ctrl Pts',(61.7569452993122,-2.75834853336005,
46.3234020627189));
#163787=CARTESIAN_POINT('Ctrl Pts',(61.9314304590403,-3.25241660548061,
46.302932504685));
#163788=CARTESIAN_POINT('Ctrl Pts',(61.9780020879817,-3.37597157857149,
46.2973572918494));
#163789=CARTESIAN_POINT('Ctrl Pts',(62.0633337041784,-3.58871941622418,
46.2869682484681));
#163790=CARTESIAN_POINT('Ctrl Pts',(62.1009120258662,-3.67837269398528,
46.2823416237566));
#163791=CARTESIAN_POINT('Ctrl Pts',(62.1827555074008,-3.86546421015422,
46.2721630696317));
#163792=CARTESIAN_POINT('Ctrl Pts',(62.2273065483308,-3.96275963774058,
46.2665656605729));
#163793=CARTESIAN_POINT('Ctrl Pts',(62.3562627005691,-4.23216841650119,
46.2502111220432));
#163794=CARTESIAN_POINT('Ctrl Pts',(62.4442649437281,-4.4024655934303,46.2388822110638));
#163795=CARTESIAN_POINT('Ctrl Pts',(62.6662437506602,-4.80165151662173,
46.2099026801945));
#163796=CARTESIAN_POINT('Ctrl Pts',(62.8047986237087,-5.0277503326074,46.1915099439424));
#163797=CARTESIAN_POINT('Ctrl Pts',(63.2115943451449,-5.63261191214171,
46.1365293905606));
#163798=CARTESIAN_POINT('Ctrl Pts',(63.4985000435387,-5.99760905925112,
46.0967496198762));
#163799=CARTESIAN_POINT('Ctrl Pts',(63.8679447031853,-6.4020404625602,46.0435922621873));
#163800=CARTESIAN_POINT('Ctrl Pts',(63.9258665430216,-6.46374675374832,
46.0352070381961));
#163801=CARTESIAN_POINT('Ctrl Pts',(64.0233130511043,-6.56478071413928,
46.0210067611629));
#163802=CARTESIAN_POINT('Ctrl Pts',(64.0623741307016,-6.60456236937709,
46.0152903756185));
#163803=CARTESIAN_POINT('Ctrl Pts',(64.1487016008485,-6.69092522428066,
46.0026019156905));
#163804=CARTESIAN_POINT('Ctrl Pts',(64.1961101059915,-6.73735437443061,
45.9955993525748));
#163805=CARTESIAN_POINT('Ctrl Pts',(64.3493257147542,-6.88424065940277,
45.9728699872818));
#163806=CARTESIAN_POINT('Ctrl Pts',(64.4569630883872,-6.98269597000688,
45.9567550712773));
#163807=CARTESIAN_POINT('Ctrl Pts',(64.7428876245874,-7.23215576862245,
45.9136612401674));
#163808=CARTESIAN_POINT('Ctrl Pts',(64.9245675154636,-7.37899361112587,
45.8860030442394));
#163809=CARTESIAN_POINT('Ctrl Pts',(65.5091169965193,-7.81601653809011,
45.7965602056484));
#163810=CARTESIAN_POINT('Ctrl Pts',(65.9295686122815,-8.0805409665039,45.7316287471787));
#163811=CARTESIAN_POINT('Ctrl Pts',(66.4886148872436,-8.37221490034032,
45.6455639737845));
#163812=CARTESIAN_POINT('Ctrl Pts',(66.6096241865374,-8.43199967080375,
45.6269463126964));
#163813=CARTESIAN_POINT('Ctrl Pts',(66.8196716730826,-8.5300810250407,45.5946628630405));
#163814=CARTESIAN_POINT('Ctrl Pts',(66.9080909718603,-8.56967734571778,
45.5810829068597));
#163815=CARTESIAN_POINT('Ctrl Pts',(67.0932194860375,-8.64909079682306,
45.5526734096657));
#163816=CARTESIAN_POINT('Ctrl Pts',(67.1900145651305,-8.68866849190123,
45.5378325779662));
#163817=CARTESIAN_POINT('Ctrl Pts',(67.4548202028363,-8.79169711251207,
45.4972698836512));
#163818=CARTESIAN_POINT('Ctrl Pts',(67.6240300661649,-8.85187506142831,
45.4713919534327));
#163819=CARTESIAN_POINT('Ctrl Pts',(68.0178739928377,-8.97904413005395,
45.411243430795));
#163820=CARTESIAN_POINT('Ctrl Pts',(68.2435119467076,-9.04245827772779,
45.3768458854809));
#163821=CARTESIAN_POINT('Ctrl Pts',(68.7878083763292,-9.17313444876951,
45.2939221829229));
#163822=CARTESIAN_POINT('Ctrl Pts',(69.1080820201528,-9.23217904713312,
45.2451740618639));
#163823=CARTESIAN_POINT('Ctrl Pts',(69.7047365491124,-9.30957189379992,
45.1540607697768));
#163824=CARTESIAN_POINT('Ctrl Pts',(69.9801592643347,-9.33267595224281,
45.1118838544893));
#163825=CARTESIAN_POINT('Ctrl Pts',(70.3335571167051,-9.34624476590553,
45.0573821941967));
#163826=CARTESIAN_POINT('Ctrl Pts',(70.4110027406322,-9.3482324668144,45.0454145715436));
#163827=CARTESIAN_POINT('Ctrl Pts',(70.5397230860263,-9.34989846758445,
45.0254762742257));
#163828=CARTESIAN_POINT('Ctrl Pts',(70.5909894278427,-9.3501303981416,45.0175227362279));
#163829=CARTESIAN_POINT('Ctrl Pts',(70.7011646808674,-9.34970123745941,
45.0004008606364));
#163830=CARTESIAN_POINT('Ctrl Pts',(70.760069552404,-9.34890178716619,44.9912293524378));
#163831=CARTESIAN_POINT('Ctrl Pts',(70.9368317726177,-9.3447917071955,44.963662634205));
#163832=CARTESIAN_POINT('Ctrl Pts',(71.0546311473423,-9.33976834879518,
44.9452316739513));
#163833=CARTESIAN_POINT('Ctrl Pts',(71.3410872683884,-9.32198850567812,
44.9003128067773));
#163834=CARTESIAN_POINT('Ctrl Pts',(71.509548379318,-9.30682376647028,44.8738124606415));
#163835=CARTESIAN_POINT('Ctrl Pts',(71.9808747458421,-9.2511570394844,44.7995754990106));
#163836=CARTESIAN_POINT('Ctrl Pts',(72.2822915445319,-9.20011911921818,
44.7519962490739));
#163837=CARTESIAN_POINT('Ctrl Pts',(72.9591737565349,-9.05027084314983,
44.6454697094686));
#163838=CARTESIAN_POINT('Ctrl Pts',(73.3321201375491,-8.94246393286336,
44.5870148755854));
#163839=CARTESIAN_POINT('Ctrl Pts',(73.8204232690107,-8.76708205076489,
44.5112103276699));
#163840=CARTESIAN_POINT('Ctrl Pts',(73.9425517105278,-8.72024992377672,
44.4923124034965));
#163841=CARTESIAN_POINT('Ctrl Pts',(74.1528634767407,-8.63441076443044,
44.4598859799939));
#163842=CARTESIAN_POINT('Ctrl Pts',(74.2414965976929,-8.59659994050184,
44.4462570159857));
#163843=CARTESIAN_POINT('Ctrl Pts',(74.4264731097673,-8.5142322846033,44.4178933287952));
#163844=CARTESIAN_POINT('Ctrl Pts',(74.522676699809,-8.4693860110368,44.403188185328));
#163845=CARTESIAN_POINT('Ctrl Pts',(74.7890852228057,-8.33954852375368,
44.3625971097258));
#163846=CARTESIAN_POINT('Ctrl Pts',(74.9575122358945,-8.25091549104413,
44.337087163515));
#163847=CARTESIAN_POINT('Ctrl Pts',(75.3523738504045,-8.02727509853063,
44.2776238000474));
#163848=CARTESIAN_POINT('Ctrl Pts',(75.5760719862675,-7.88763001333651,
44.2442180599122));
#163849=CARTESIAN_POINT('Ctrl Pts',(76.1746076003093,-7.47746674754934,
44.1554285809942));
#163850=CARTESIAN_POINT('Ctrl Pts',(76.535905853825,-7.18801349112879,44.1025313295171));
#163851=CARTESIAN_POINT('Ctrl Pts',(76.936240287193,-6.81495285807577,44.0439271985903));
#163852=CARTESIAN_POINT('Ctrl Pts',(76.9973213463289,-6.75645523117442,
44.0349849077155));
#163853=CARTESIAN_POINT('Ctrl Pts',(77.0973299370408,-6.65802368003523,
44.0203328537811));
#163854=CARTESIAN_POINT('Ctrl Pts',(77.1367074432985,-6.61856342587494,
44.0145606720422));
#163855=CARTESIAN_POINT('Ctrl Pts',(77.2221916074237,-6.53134398961019,
44.0020209130758));
#163856=CARTESIAN_POINT('Ctrl Pts',(77.2681475924562,-6.48343955303723,
43.9952744732626));
#163857=CARTESIAN_POINT('Ctrl Pts',(77.4135366697861,-6.32860330746571,
43.9739251736349));
#163858=CARTESIAN_POINT('Ctrl Pts',(77.5109871153879,-6.21980159041315,
43.959606518489));
#163859=CARTESIAN_POINT('Ctrl Pts',(77.7579129448062,-5.93073296709067,
43.923389322992));
#163860=CARTESIAN_POINT('Ctrl Pts',(77.9032709278136,-5.7470067615247,43.9021357372137));
#163861=CARTESIAN_POINT('Ctrl Pts',(78.3359817498253,-5.15580834521874,
43.8394660783437));
#163862=CARTESIAN_POINT('Ctrl Pts',(78.5980570752674,-4.73047577709636,
43.8024604939837));
#163863=CARTESIAN_POINT('Ctrl Pts',(78.8874360059866,-4.16498448900198,
43.7639451975362));
#163864=CARTESIAN_POINT('Ctrl Pts',(78.9467778682253,-4.04258017942232,
43.7562011800701));
#163865=CARTESIAN_POINT('Ctrl Pts',(79.0441823778068,-3.83011726014096,
43.7437797386978));
#163866=CARTESIAN_POINT('Ctrl Pts',(79.0835210522288,-3.74068305111187,
43.7388540220899));
#163867=CARTESIAN_POINT('Ctrl Pts',(79.1624520231416,-3.55343393065613,
43.7291700137279));
#163868=CARTESIAN_POINT('Ctrl Pts',(79.2018091886896,-3.45553250299467,
43.7244570311495));
#163869=CARTESIAN_POINT('Ctrl Pts',(79.3043203981019,-3.18770752122583,
43.7125111929558));
#163870=CARTESIAN_POINT('Ctrl Pts',(79.3642607195549,-3.01657580170413,
43.7059004045354));
#163871=CARTESIAN_POINT('Ctrl Pts',(79.4910868677747,-2.61827390662252,
43.6928342408215));
#163872=CARTESIAN_POINT('Ctrl Pts',(79.5544587247302,-2.39009307307585,
43.6870485320038));
#163873=CARTESIAN_POINT('Ctrl Pts',(79.6853816149668,-1.83966854410041,
43.677013679843));
#163874=CARTESIAN_POINT('Ctrl Pts',(79.7448506469194,-1.51579562147201,
43.6742524479917));
#163875=CARTESIAN_POINT('Ctrl Pts',(79.8234791940555,-0.912379387627375,
43.6744812281231));
#163876=CARTESIAN_POINT('Ctrl Pts',(79.8473251561585,-0.633812339879392,
43.6766641937312));
#163877=CARTESIAN_POINT('Ctrl Pts',(79.8620238830965,-0.276314779159023,
43.681884424806));
#163878=CARTESIAN_POINT('Ctrl Pts',(79.8642700600739,-0.19796777031579,
43.6831764891021));
#163879=CARTESIAN_POINT('Ctrl Pts',(79.8663742280622,-0.0682497633545942,
43.6855532569837));
#163880=CARTESIAN_POINT('Ctrl Pts',(79.8667884538124,-0.0168900632655849,
43.6865557931488));
#163881=CARTESIAN_POINT('Ctrl Pts',(79.8667780725513,0.0938369406020547,
43.6888477114382));
#163882=CARTESIAN_POINT('Ctrl Pts',(79.866212708815,0.153200899447015,43.6901578905364));
#163883=CARTESIAN_POINT('Ctrl Pts',(79.8628528270007,0.330510398218484,
43.6943213851528));
#163884=CARTESIAN_POINT('Ctrl Pts',(79.8584087802861,0.448406855380347,
43.6974207258766));
#163885=CARTESIAN_POINT('Ctrl Pts',(79.8422744922485,0.734255331836819,
43.7057819316328));
#163886=CARTESIAN_POINT('Ctrl Pts',(79.828303006439,0.902026381114984,43.7114007504348));
#163887=CARTESIAN_POINT('Ctrl Pts',(79.7755870792911,1.38043930972032,43.7295972908011));
#163888=CARTESIAN_POINT('Ctrl Pts',(79.7259058096718,1.68957455777478,43.7439975619436));
#163889=CARTESIAN_POINT('Ctrl Pts',(79.5797051199031,2.37939279627776,43.7826895473336));
#163890=CARTESIAN_POINT('Ctrl Pts',(79.4746312691167,2.75756779437402,43.808535770282));
#163891=CARTESIAN_POINT('Ctrl Pts',(79.3034285819782,3.25234275460055,43.8490349265531));
#163892=CARTESIAN_POINT('Ctrl Pts',(79.2577553666244,3.37590974147408,43.8597252007661));
#163893=CARTESIAN_POINT('Ctrl Pts',(79.1740126928187,3.58867109811851,43.8791487803523));
#163894=CARTESIAN_POINT('Ctrl Pts',(79.1371181047329,3.67832604909296,43.8876537629297));
#163895=CARTESIAN_POINT('Ctrl Pts',(79.0567316031642,3.86541446290809,43.9060806342698));
#163896=CARTESIAN_POINT('Ctrl Pts',(79.0129557062284,3.96270521286113,43.9160575220774));
#163897=CARTESIAN_POINT('Ctrl Pts',(78.8862010040632,4.23208053550023,43.9447908598919));
#163898=CARTESIAN_POINT('Ctrl Pts',(78.7996480317851,4.40234977481434,43.9642399944474));
#163899=CARTESIAN_POINT('Ctrl Pts',(78.581202121744,4.80144705626461,44.0129167707692));
#163900=CARTESIAN_POINT('Ctrl Pts',(78.4447566902517,5.02748742971026,44.0430122573211));
#163901=CARTESIAN_POINT('Ctrl Pts',(78.0437031144844,5.63238183204341,44.1304776619868));
#163902=CARTESIAN_POINT('Ctrl Pts',(77.7604473021958,5.99745950068413,44.1912350519678));
#163903=CARTESIAN_POINT('Ctrl Pts',(77.3950336374395,6.40197581988324,44.2676555646764));
#163904=CARTESIAN_POINT('Ctrl Pts',(77.3377260177182,6.46369500267863,44.2795887881123));
#163905=CARTESIAN_POINT('Ctrl Pts',(77.241286860215,6.56474336759332,44.299576214983));
#163906=CARTESIAN_POINT('Ctrl Pts',(77.2026250052317,6.60452682870524,44.3075645356558));
#163907=CARTESIAN_POINT('Ctrl Pts',(77.1171689031824,6.69088563015779,44.3251660399807));
#163908=CARTESIAN_POINT('Ctrl Pts',(77.0702308398464,6.73730908233219,44.3347991582582));
#163909=CARTESIAN_POINT('Ctrl Pts',(76.9185285751454,6.88415200333873,44.3658337798556));
#163910=CARTESIAN_POINT('Ctrl Pts',(76.8119133828088,6.9825714618315,44.3874963293361));
#163911=CARTESIAN_POINT('Ctrl Pts',(76.5286522353668,7.2319044336687,44.4447614961987));
#163912=CARTESIAN_POINT('Ctrl Pts',(76.3485911559729,7.37865804067762,44.4808853429198));
#163913=CARTESIAN_POINT('Ctrl Pts',(75.7686351820489,7.815799767526,44.5967787128622));
#163914=CARTESIAN_POINT('Ctrl Pts',(75.351108782912,8.08048320056685,44.6796101264728));
#163915=CARTESIAN_POINT('Ctrl Pts',(74.7961135331527,8.37226645687446,44.789986101782));
#163916=CARTESIAN_POINT('Ctrl Pts',(74.6760508461963,8.4320412981402,44.8138755720144));
#163917=CARTESIAN_POINT('Ctrl Pts',(74.4676481176996,8.53011160846007,44.8553757657832));
#163918=CARTESIAN_POINT('Ctrl Pts',(74.379918666909,8.56970612874324,44.8728555433475));
#163919=CARTESIAN_POINT('Ctrl Pts',(74.1962336795464,8.64911987511433,44.9094779314105));
#163920=CARTESIAN_POINT('Ctrl Pts',(74.1001934752728,8.68869936729909,44.928639325752));
#163921=CARTESIAN_POINT('Ctrl Pts',(73.8374406052869,8.79174215847888,44.9811004715326));
#163922=CARTESIAN_POINT('Ctrl Pts',(73.669546913669,8.85193052735368,45.0146639044545));
#163923=CARTESIAN_POINT('Ctrl Pts',(73.2787705307102,8.97912627689817,45.0928678432809));
#163924=CARTESIAN_POINT('Ctrl Pts',(73.0549001899189,9.04255322668433,45.1377326031135));
#163925=CARTESIAN_POINT('Ctrl Pts',(72.5149878427279,9.17322117496631,45.245986137296));
#163926=CARTESIAN_POINT('Ctrl Pts',(72.1973539487951,9.23225042323679,45.3097183456386));
#163927=CARTESIAN_POINT('Ctrl Pts',(71.6056777244385,9.30959372118856,45.4281357791377));
#163928=CARTESIAN_POINT('Ctrl Pts',(71.332601583977,9.33267835252477,45.482670079045));
#163929=CARTESIAN_POINT('Ctrl Pts',(70.9820293622766,9.34624341394468,45.5522939643191));
#163930=CARTESIAN_POINT('Ctrl Pts',(70.9051522017376,9.34823171241028,45.567537818062));
#163931=CARTESIAN_POINT('Ctrl Pts',(70.7773650805505,9.34989826679501,45.5928289416275));
#163932=CARTESIAN_POINT('Ctrl Pts',(70.7264688613684,9.35013035922616,45.602889453219));
#163933=CARTESIAN_POINT('Ctrl Pts',(70.6170846369799,9.34970151916232,45.6244817905244));
#163934=CARTESIAN_POINT('Ctrl Pts',(70.5585993426785,9.34890232881752,45.6360092582636));
#163935=CARTESIAN_POINT('Ctrl Pts',(70.3830950720406,9.34479359661985,45.670556107415));
#163936=CARTESIAN_POINT('Ctrl Pts',(70.2661183186129,9.33977211512419,45.6935220909587));
#163937=CARTESIAN_POINT('Ctrl Pts',(69.9816432283738,9.3219998770592,45.7492725090466));
#163938=CARTESIAN_POINT('Ctrl Pts',(69.8143243141681,9.30684261005231,45.7819784001714));
#163939=CARTESIAN_POINT('Ctrl Pts',(69.3460036069198,9.25118542265482,45.8734271983071));
#163940=CARTESIAN_POINT('Ctrl Pts',(69.0464176982463,9.20013952992897,45.931822272195));
#163941=CARTESIAN_POINT('Ctrl Pts',(68.3738424006576,9.05027529716222,46.0632430078357));
#163942=CARTESIAN_POINT('Ctrl Pts',(68.0033873173336,8.94246677995383,46.1358700431178));
#163943=CARTESIAN_POINT('Ctrl Pts',(67.5185985652017,8.76708234335628,46.2316480011527));
#163944=CARTESIAN_POINT('Ctrl Pts',(67.3973717741238,8.72025017970903,46.2556601728448));
#163945=CARTESIAN_POINT('Ctrl Pts',(67.1886527286124,8.63441097764425,46.2971201899961));
#163946=CARTESIAN_POINT('Ctrl Pts',(67.100703441243,8.59660015240663,46.3146274691476));
#163947=CARTESIAN_POINT('Ctrl Pts',(66.917181457716,8.51423252345746,46.351240008046));
#163948=CARTESIAN_POINT('Ctrl Pts',(66.8217502474301,8.46938628043826,46.3703252489888));
#163949=CARTESIAN_POINT('Ctrl Pts',(66.5575255067944,8.33954898889645,46.4232991256447));
#163950=CARTESIAN_POINT('Ctrl Pts',(66.3905312605465,8.25091613858479,46.4569329894159));
#163951=CARTESIAN_POINT('Ctrl Pts',(65.9991459688741,8.02727637034531,46.5361061429746));
#163952=CARTESIAN_POINT('Ctrl Pts',(65.7775136528271,7.88763176513871,46.5812241582663));
#163953=CARTESIAN_POINT('Ctrl Pts',(65.1847060251401,7.47746865092028,46.7025006395234));
#163954=CARTESIAN_POINT('Ctrl Pts',(64.8271039639216,7.18801488609426,46.7763649342709));
#163955=CARTESIAN_POINT('Ctrl Pts',(64.4308679765701,6.81495351472009,46.8582176872529));
#163956=CARTESIAN_POINT('Ctrl Pts',(64.3704119763466,6.75645576698684,46.8707056632443));
#163957=CARTESIAN_POINT('Ctrl Pts',(64.2714231920131,6.65802407706972,46.891142220252));
#163958=CARTESIAN_POINT('Ctrl Pts',(64.232446218481,6.6185638082873,46.8991860479607));
#163959=CARTESIAN_POINT('Ctrl Pts',(64.1478285729352,6.53134442581497,46.9166398262734));
#163960=CARTESIAN_POINT('Ctrl Pts',(64.1023367147926,6.48344005934743,46.9260181067699));
#163961=CARTESIAN_POINT('Ctrl Pts',(63.9584142392529,6.32860433300367,46.9556822261476));
#163962=CARTESIAN_POINT('Ctrl Pts',(63.8619438848834,6.21980308296312,46.9755570289167));
#163963=CARTESIAN_POINT('Ctrl Pts',(63.6175238345535,5.9307362076723,47.0259773279547));
#163964=CARTESIAN_POINT('Ctrl Pts',(63.4736637457863,5.74701134127474,47.0557206629557));
#163965=CARTESIAN_POINT('Ctrl Pts',(63.0456130382846,5.15581217900249,47.1448265123596));
#163966=CARTESIAN_POINT('Ctrl Pts',(62.7866844550062,4.73047715963278,47.1996880252191));
#163967=CARTESIAN_POINT('Ctrl Pts',(62.5015830507618,4.1649833701103,47.2624691674286));
#163968=CARTESIAN_POINT('Ctrl Pts',(62.4431714350186,4.04257924072671,47.2754882612951));
#163969=CARTESIAN_POINT('Ctrl Pts',(62.3473928689251,3.83011652856883,47.2971302038777));
#163970=CARTESIAN_POINT('Ctrl Pts',(62.3087419315082,3.7406823428418,47.3059561595857));
#163971=CARTESIAN_POINT('Ctrl Pts',(62.231258951763,3.55343317352007,47.3238521521074));
#163972=CARTESIAN_POINT('Ctrl Pts',(62.1926633600608,3.45553167236604,47.3328843455987));
#163973=CARTESIAN_POINT('Ctrl Pts',(62.0922484679552,3.18770621258904,47.356719865362));
#163974=CARTESIAN_POINT('Ctrl Pts',(62.0336618589915,3.01657408119746,47.3710085824877));
#163975=CARTESIAN_POINT('Ctrl Pts',(61.9100150953728,2.6182709596395,47.4021075803621));
#163976=CARTESIAN_POINT('Ctrl Pts',(61.848486068248,2.39008930181531,47.4183452873219));
#163977=CARTESIAN_POINT('Ctrl Pts',(61.6798368110033,1.65602837583178,47.4654870472214));
#163978=CARTESIAN_POINT('Ctrl Pts',(61.6055753582875,1.14324940002398,47.4908841185973));
#163979=CARTESIAN_POINT('Ctrl Pts',(61.5658269000459,0.505351179248187,
47.512236036455));
#163980=CARTESIAN_POINT('Ctrl Pts',(61.5605908046069,0.383857980702777,
47.5158457141457));
#163981=CARTESIAN_POINT('Ctrl Pts',(61.5565217323495,0.213904894315144,
47.5202346860237));
#163982=CARTESIAN_POINT('Ctrl Pts',(61.555731712949,0.165514109940709,47.5214095668697));
#163983=CARTESIAN_POINT('Ctrl Pts',(61.5549698199378,0.0780956836856776,
47.523395001381));
#163984=CARTESIAN_POINT('Ctrl Pts',(61.5548691195383,0.0390708528840299,
47.524232024342));
#163985=CARTESIAN_POINT('Ctrl Pts',(61.5550077244638,4.54923683265615E-5,
47.5250191853983));
#163986=CARTESIAN_POINT('Ctrl Pts',(61.5550077244638,4.54923683265615E-5,
47.5250191853983));
#163987=CARTESIAN_POINT('Ctrl Pts',(61.5550077783217,3.03282455134599E-5,
47.5250194912663));
#163988=CARTESIAN_POINT('Ctrl Pts',(61.5550078322157,1.51641227338287E-5,
47.5250197971267));
#163989=CARTESIAN_POINT('Ctrl Pts',(61.5550078861458,-8.57747578934197E-15,
47.5250201029796));
#163990=CARTESIAN_POINT('Origin',(69.6316151486327,0.,39.48523201752));
#163991=CARTESIAN_POINT('',(61.7928511881971,-3.40955384291398E-10,48.8738964978212));
#163992=CARTESIAN_POINT('',(61.763385699346,8.81065254412669E-12,48.7067894065939));
#163993=CARTESIAN_POINT('',(60.4236626579685,-1.14504475720278E-15,41.1088424787055));
#163994=CARTESIAN_POINT('Ctrl Pts',(61.7928511881971,-6.81909623538039E-10,
48.8738964978212));
#163995=CARTESIAN_POINT('Ctrl Pts',(61.7927093875837,0.0398716337037261,
48.8730923065971));
#163996=CARTESIAN_POINT('Ctrl Pts',(61.7928201229409,0.079742808460378,
48.8722516099169));
#163997=CARTESIAN_POINT('Ctrl Pts',(61.7938970464417,0.197975584846006,
48.869648227374));
#163998=CARTESIAN_POINT('Ctrl Pts',(61.7955859471352,0.276324641715018,
48.8677791949698));
#163999=CARTESIAN_POINT('Ctrl Pts',(61.8077391834102,0.633772298995458,
48.858571281954));
#164000=CARTESIAN_POINT('Ctrl Pts',(61.82959410914,0.912294132295975,48.8494975486385));
#164001=CARTESIAN_POINT('Ctrl Pts',(61.90388876499,1.51567460582303,48.8252206613235));
#164002=CARTESIAN_POINT('Ctrl Pts',(61.9610202792514,1.83954707276695,48.8092283784813));
#164003=CARTESIAN_POINT('Ctrl Pts',(62.087930408233,2.38999814777087,48.7764440961858));
#164004=CARTESIAN_POINT('Ctrl Pts',(62.149629027767,2.61820050379103,48.7611466119104));
#164005=CARTESIAN_POINT('Ctrl Pts',(62.2735006171906,3.01653378061279,48.7312824940788));
#164006=CARTESIAN_POINT('Ctrl Pts',(62.3321599462423,3.18767622698851,48.7173889778356));
#164007=CARTESIAN_POINT('Ctrl Pts',(62.4326425833639,3.45551184770372,48.6939197693051));
#164008=CARTESIAN_POINT('Ctrl Pts',(62.4712527680553,3.55341518306191,48.6849673361731));
#164009=CARTESIAN_POINT('Ctrl Pts',(62.5487437909795,3.7406654284178,48.6671168763836));
#164010=CARTESIAN_POINT('Ctrl Pts',(62.5873896398572,3.83009901599484,48.658264697418));
#164011=CARTESIAN_POINT('Ctrl Pts',(62.6831346662027,4.04255724851014,48.6364477691766));
#164012=CARTESIAN_POINT('Ctrl Pts',(62.7415095785075,4.16495681714975,48.6232355320527));
#164013=CARTESIAN_POINT('Ctrl Pts',(63.0264122525956,4.73051261477613,48.5591593164579));
#164014=CARTESIAN_POINT('Ctrl Pts',(63.2849881828916,5.15589910065763,48.5020793761147));
#164015=CARTESIAN_POINT('Ctrl Pts',(63.7125017277984,5.74710375971109,48.4098170127609));
#164016=CARTESIAN_POINT('Ctrl Pts',(63.8561713553807,5.93080105228094,48.3791027442129));
#164017=CARTESIAN_POINT('Ctrl Pts',(64.1003557608425,6.21983194810889,48.3275080634672));
#164018=CARTESIAN_POINT('Ctrl Pts',(64.1967554870541,6.32862362780603,48.3072792530823));
#164019=CARTESIAN_POINT('Ctrl Pts',(64.3406191147498,6.48344999314284,48.2773295468307));
#164020=CARTESIAN_POINT('Ctrl Pts',(64.3860996658139,6.53135292177966,48.2678945160641));
#164021=CARTESIAN_POINT('Ctrl Pts',(64.4707106363186,6.6185713154146,48.2504073822016));
#164022=CARTESIAN_POINT('Ctrl Pts',(64.5096903100394,6.65803189240602,48.2423766014184));
#164023=CARTESIAN_POINT('Ctrl Pts',(64.6086993023588,6.75646608260662,48.2220383523451));
#164024=CARTESIAN_POINT('Ctrl Pts',(64.669179056021,6.8149663498546,48.209668672977));
#164025=CARTESIAN_POINT('Ctrl Pts',(65.0655988267846,7.18802062998159,48.1288906796568));
#164026=CARTESIAN_POINT('Ctrl Pts',(65.4235963300728,7.47747300199336,48.0572849906119));
#164027=CARTESIAN_POINT('Ctrl Pts',(66.0169565033158,7.88763976461308,47.9391000779253));
#164028=CARTESIAN_POINT('Ctrl Pts',(66.2387704597362,8.02728249550912,47.8950231730325));
#164029=CARTESIAN_POINT('Ctrl Pts',(66.6303863241417,8.25091993500563,47.8171782011556));
#164030=CARTESIAN_POINT('Ctrl Pts',(66.7974532858258,8.3395519942289,47.7839619079423));
#164031=CARTESIAN_POINT('Ctrl Pts',(67.0617408995793,8.46938770035125,47.7313625456761));
#164032=CARTESIAN_POINT('Ctrl Pts',(67.1571859119804,8.5142338026188,47.7123564639545));
#164033=CARTESIAN_POINT('Ctrl Pts',(67.3407148804679,8.59660126797913,47.675785125181));
#164034=CARTESIAN_POINT('Ctrl Pts',(67.4286593240644,8.63441206936909,47.6582499605551));
#164035=CARTESIAN_POINT('Ctrl Pts',(67.6373482034933,8.72025170719849,47.6166119098222));
#164036=CARTESIAN_POINT('Ctrl Pts',(67.7585419008783,8.76708392705567,47.5924093871011));
#164037=CARTESIAN_POINT('Ctrl Pts',(68.2431420010052,8.94246895398043,47.4955487795057));
#164038=CARTESIAN_POINT('Ctrl Pts',(68.6133134664131,9.05027439873143,47.4213533810061));
#164039=CARTESIAN_POINT('Ctrl Pts',(69.2852265247751,9.2001233660496,47.2866167086761));
#164040=CARTESIAN_POINT('Ctrl Pts',(69.5844658875582,9.25116307658516,47.2265956650692));
#164041=CARTESIAN_POINT('Ctrl Pts',(70.0523842120146,9.30682753616114,47.1330050204991));
#164042=CARTESIAN_POINT('Ctrl Pts',(70.2196190134392,9.32199080350287,47.0996088203838));
#164043=CARTESIAN_POINT('Ctrl Pts',(70.5039956188471,9.33976903456648,47.0429806418733));
#164044=CARTESIAN_POINT('Ctrl Pts',(70.6209418047642,9.34479206758022,47.0197391521012));
#164045=CARTESIAN_POINT('Ctrl Pts',(70.7964272605224,9.34890188912022,46.9849565986193));
#164046=CARTESIAN_POINT('Ctrl Pts',(70.8549073060047,9.34970129582141,46.9733808715733));
#164047=CARTESIAN_POINT('Ctrl Pts',(70.9642892004743,9.35013038770566,46.9517622846922));
#164048=CARTESIAN_POINT('Ctrl Pts',(71.015186904825,9.34989843097453,46.9417164022726));
#164049=CARTESIAN_POINT('Ctrl Pts',(71.142982625768,9.34823231706115,46.9165242015347));
#164050=CARTESIAN_POINT('Ctrl Pts',(71.219872796493,9.34624451319848,46.9013951541355));
#164051=CARTESIAN_POINT('Ctrl Pts',(71.5706797080047,9.33267703018759,46.8324735046096));
#164052=CARTESIAN_POINT('Ctrl Pts',(71.8440752444452,9.30957876278128,46.7790464154775));
#164053=CARTESIAN_POINT('Ctrl Pts',(72.4363754978243,9.23219786051485,46.6634312042488));
#164054=CARTESIAN_POINT('Ctrl Pts',(72.754315530605,9.17315748604154,46.6014513431682));
#164055=CARTESIAN_POINT('Ctrl Pts',(73.2946254946761,9.04248259108015,46.4957734989395));
#164056=CARTESIAN_POINT('Ctrl Pts',(73.5186064155076,8.97906475306848,46.4518612476887));
#164057=CARTESIAN_POINT('Ctrl Pts',(73.9095178036318,8.85188882900484,46.374910778791));
#164058=CARTESIAN_POINT('Ctrl Pts',(74.0774536022795,8.79170793759926,46.341748862393));
#164059=CARTESIAN_POINT('Ctrl Pts',(74.3402372603444,8.68867627423887,46.2896615924129));
#164060=CARTESIAN_POINT('Ctrl Pts',(74.4362866013123,8.64909806620124,46.270581084491));
#164061=CARTESIAN_POINT('Ctrl Pts',(74.6199761890769,8.56968460210561,46.2340049515081));
#164062=CARTESIAN_POINT('Ctrl Pts',(74.70770255296,8.53008873092478,46.2164985544831));
#164063=CARTESIAN_POINT('Ctrl Pts',(74.9160889544367,8.43200997118076,46.1748199196186));
#164064=CARTESIAN_POINT('Ctrl Pts',(75.0361295619263,8.37222776282541,46.1507343628081));
#164065=CARTESIAN_POINT('Ctrl Pts',(75.5907296749105,8.08052515010787,46.0391031358023));
#164066=CARTESIAN_POINT('Ctrl Pts',(76.0076924810794,7.81596351365729,45.9540952227733));
#164067=CARTESIAN_POINT('Ctrl Pts',(76.5870296794796,7.37892200492217,45.8350622137528));
#164068=CARTESIAN_POINT('Ctrl Pts',(76.7670142116694,7.23210274587378,45.7979446973591));
#164069=CARTESIAN_POINT('Ctrl Pts',(77.0501917030216,6.98267050576356,45.7394745499622));
#164070=CARTESIAN_POINT('Ctrl Pts',(77.1567774749319,6.88422311446124,45.7174496829604));
#164071=CARTESIAN_POINT('Ctrl Pts',(77.3084673362869,6.73734499443617,45.6861200206139));
#164072=CARTESIAN_POINT('Ctrl Pts',(77.3554003436349,6.69091709909592,45.6764288853439));
#164073=CARTESIAN_POINT('Ctrl Pts',(77.440854482312,6.60455500724864,45.6587930803067));
#164074=CARTESIAN_POINT('Ctrl Pts',(77.4795176196987,6.5647729666128,45.6508181128989));
#164075=CARTESIAN_POINT('Ctrl Pts',(77.5759639912022,6.46373624165309,45.6309317177989));
#164076=CARTESIAN_POINT('Ctrl Pts',(77.6332840098771,6.40202715843781,45.6191191804156));
#164077=CARTESIAN_POINT('Ctrl Pts',(77.9988113722254,5.9976017671801,45.5437883239921));
#164078=CARTESIAN_POINT('Ctrl Pts',(78.2824166163544,5.63260774015445,45.485299976364));
#164079=CARTESIAN_POINT('Ctrl Pts',(78.6840330175363,5.02773899565478,45.4009246579117));
#164080=CARTESIAN_POINT('Ctrl Pts',(78.8207045613723,4.80164182792807,45.3718606754667));
#164081=CARTESIAN_POINT('Ctrl Pts',(79.0394400357541,4.40245908022573,45.3244992077555));
#164082=CARTESIAN_POINT('Ctrl Pts',(79.1260827061336,4.23216267970861,45.3054638953936));
#164083=CARTESIAN_POINT('Ctrl Pts',(79.2529198919031,3.96275686917369,45.2771007622597));
#164084=CARTESIAN_POINT('Ctrl Pts',(79.2967124299097,3.86546157438083,45.2672024067856));
#164085=CARTESIAN_POINT('Ctrl Pts',(79.3771085221401,3.67837032000539,45.2488161775587));
#164086=CARTESIAN_POINT('Ctrl Pts',(79.4139980537783,3.58871697754349,45.2402833708288));
#164087=CARTESIAN_POINT('Ctrl Pts',(79.4977058625176,3.3759679920793,45.2206828505326));
#164088=CARTESIAN_POINT('Ctrl Pts',(79.543342204226,3.25241260877376,45.2098031242783));
#164089=CARTESIAN_POINT('Ctrl Pts',(79.7141143293387,2.75834538967054,45.1682786333352));
#164090=CARTESIAN_POINT('Ctrl Pts',(79.8187578690572,2.38090392850897,45.14090273317));
#164091=CARTESIAN_POINT('Ctrl Pts',(79.9635697487114,1.69569555389937,45.0991056934429));
#164092=CARTESIAN_POINT('Ctrl Pts',(80.0126028905576,1.39048155231731,45.0832004164284));
#164093=CARTESIAN_POINT('Ctrl Pts',(80.0655137982829,0.913382414859032,
45.062786091966));
#164094=CARTESIAN_POINT('Ctrl Pts',(80.0797689913388,0.742950917010975,
45.0563658147369));
#164095=CARTESIAN_POINT('Ctrl Pts',(80.0961587154085,0.453152887005338,
45.0469930909051));
#164096=CARTESIAN_POINT('Ctrl Pts',(80.1006549660521,0.333977130123532,
45.0435802396458));
#164097=CARTESIAN_POINT('Ctrl Pts',(80.1040441138188,0.155152760200764,
45.0391436857227));
#164098=CARTESIAN_POINT('Ctrl Pts',(80.1046148848364,0.0955564107881091,
45.0377790476352));
#164099=CARTESIAN_POINT('Ctrl Pts',(80.1046383312521,-0.0159141927496996,
45.0354433926729));
#164100=CARTESIAN_POINT('Ctrl Pts',(80.1042264911596,-0.0677848918374825,
45.0344447366344));
#164101=CARTESIAN_POINT('Ctrl Pts',(80.1021303232615,-0.198027377199186,
45.0321557167181));
#164102=CARTESIAN_POINT('Ctrl Pts',(80.0999032129076,-0.276388431176385,
45.0309769550136));
#164103=CARTESIAN_POINT('Ctrl Pts',(80.0853380512284,-0.63365742266964,
45.0264838144944));
#164104=CARTESIAN_POINT('Ctrl Pts',(80.0617200238406,-0.911989439126223,
45.0254315872871));
#164105=CARTESIAN_POINT('Ctrl Pts',(79.9836587278326,-1.51518432935195,
45.0280224367092));
#164106=CARTESIAN_POINT('Ctrl Pts',(79.9245200285978,-1.83905941027557,
45.032531759564));
#164107=CARTESIAN_POINT('Ctrl Pts',(79.794059522035,-2.3896018148766,45.04512747728));
#164108=CARTESIAN_POINT('Ctrl Pts',(79.7308352654742,-2.61789081272124,
45.0518557524078));
#164109=CARTESIAN_POINT('Ctrl Pts',(79.6041898877887,-3.01635299916493,
45.0661621440667));
#164110=CARTESIAN_POINT('Ctrl Pts',(79.544304578152,-3.18753873037347,45.0731704224207));
#164111=CARTESIAN_POINT('Ctrl Pts',(79.441838940388,-3.4554245847302,45.0854854650915));
#164112=CARTESIAN_POINT('Ctrl Pts',(79.402493302489,-3.5533356432085,45.0902786024331));
#164113=CARTESIAN_POINT('Ctrl Pts',(79.3235700024699,-3.74059102650108,
45.1000081353203));
#164114=CARTESIAN_POINT('Ctrl Pts',(79.2842291712769,-3.83002216813102,
45.1049071898515));
#164115=CARTESIAN_POINT('Ctrl Pts',(79.1868088006053,-4.04245865076035,
45.117151093802));
#164116=CARTESIAN_POINT('Ctrl Pts',(79.127446579768,-4.16483929652454,45.1246995865182));
#164117=CARTESIAN_POINT('Ctrl Pts',(78.8376881397524,-4.73065622344361,
45.1619455053558));
#164118=CARTESIAN_POINT('Ctrl Pts',(78.5750063112216,-5.15629868667662,
45.1967698974858));
#164119=CARTESIAN_POINT('Ctrl Pts',(78.1415872119472,-5.74758144430734,
45.2563100328585));
#164120=CARTESIAN_POINT('Ctrl Pts',(77.9961710005488,-5.93113909249284,
45.2765733795583));
#164121=CARTESIAN_POINT('Ctrl Pts',(77.749207677565,-6.2199876850907,45.3115866262057));
#164122=CARTESIAN_POINT('Ctrl Pts',(77.651742866081,-6.3287306452149,45.3255428141669));
#164123=CARTESIAN_POINT('Ctrl Pts',(77.506360183959,-6.48350283982889,45.3465966458874));
#164124=CARTESIAN_POINT('Ctrl Pts',(77.4604018247016,-6.53139845271807,
45.3532849810303));
#164125=CARTESIAN_POINT('Ctrl Pts',(77.3749170867828,-6.61861123522454,
45.365790480238));
#164126=CARTESIAN_POINT('Ctrl Pts',(77.3355394776719,-6.65807334050427,
45.3715761607064));
#164127=CARTESIAN_POINT('Ctrl Pts',(77.2355293345143,-6.75652202434567,
45.3863299358669));
#164128=CARTESIAN_POINT('Ctrl Pts',(77.1744519297252,-6.81503491003287,
45.3953936982221));
#164129=CARTESIAN_POINT('Ctrl Pts',(76.7742163553425,-7.18816839315752,
45.4550852244507));
#164130=CARTESIAN_POINT('Ctrl Pts',(76.4132278982452,-7.47767560706471,
45.5102544302851));
#164131=CARTESIAN_POINT('Ctrl Pts',(75.8151932141065,-7.88782668734451,
45.6021440598486));
#164132=CARTESIAN_POINT('Ctrl Pts',(75.5917464975128,-8.02741820785937,
45.6365800868764));
#164133=CARTESIAN_POINT('Ctrl Pts',(75.1972226196877,-8.25098903860689,
45.6973549638813));
#164134=CARTESIAN_POINT('Ctrl Pts',(75.0289016541265,-8.33960163458169,
45.7232772962621));
#164135=CARTESIAN_POINT('Ctrl Pts',(74.7625999361083,-8.46941645347655,
45.7642359791166));
#164136=CARTESIAN_POINT('Ctrl Pts',(74.6664157343671,-8.51425929583976,
45.7790194117436));
#164137=CARTESIAN_POINT('Ctrl Pts',(74.481450253293,-8.59662388566012,45.8074236572265));
#164138=CARTESIAN_POINT('Ctrl Pts',(74.3928102552396,-8.63443482705536,
45.8210250466622));
#164139=CARTESIAN_POINT('Ctrl Pts',(74.182450667112,-8.72027902564148,45.8532761872953));
#164140=CARTESIAN_POINT('Ctrl Pts',(74.0602746430061,-8.76711515896276,
45.8719859917722));
#164141=CARTESIAN_POINT('Ctrl Pts',(73.5709789811025,-8.94277846001009,
45.9468309314503));
#164142=CARTESIAN_POINT('Ctrl Pts',(73.1969443301631,-9.05075890642989,
46.0038392179424));
#164143=CARTESIAN_POINT('Ctrl Pts',(72.5143651718206,-9.20153563227824,
46.1078134436371));
#164144=CARTESIAN_POINT('Ctrl Pts',(72.2082869265093,-9.25299899086914,
46.1544213795432));
#164145=CARTESIAN_POINT('Ctrl Pts',(71.7351189661655,-9.30801541318731,
46.2267447213101));
#164146=CARTESIAN_POINT('Ctrl Pts',(71.5695011866917,-9.32270911040497,
46.2521113910088));
#164147=CARTESIAN_POINT('Ctrl Pts',(71.2872907903927,-9.34000785246016,
46.2954911652769));
#164148=CARTESIAN_POINT('Ctrl Pts',(71.1708687670721,-9.34491212923875,
46.3134318333393));
#164149=CARTESIAN_POINT('Ctrl Pts',(70.9957504101543,-9.34893637020397,
46.340507940003));
#164150=CARTESIAN_POINT('Ctrl Pts',(70.9370961065956,-9.34971918461126,
46.3495920779163));
#164151=CARTESIAN_POINT('Ctrl Pts',(70.827670542458,-9.35012556127216,46.3665717061112));
#164152=CARTESIAN_POINT('Ctrl Pts',(70.776902038224,-9.34989080110659,46.3744628303659));
#164153=CARTESIAN_POINT('Ctrl Pts',(70.6486429722421,-9.34822814954453,
46.394429272106));
#164154=CARTESIAN_POINT('Ctrl Pts',(70.5711658249032,-9.34623704442709,
46.4065183953776));
#164155=CARTESIAN_POINT('Ctrl Pts',(70.2184319281362,-9.33267623374973,
46.4616600380233));
#164156=CARTESIAN_POINT('Ctrl Pts',(69.9437874759586,-9.30963798221351,
46.5048769460366));
#164157=CARTESIAN_POINT('Ctrl Pts',(69.3481894664989,-9.23241160402367,
46.5987296503087));
#164158=CARTESIAN_POINT('Ctrl Pts',(69.0282183267463,-9.1734172006384,46.6492308187572));
#164159=CARTESIAN_POINT('Ctrl Pts',(68.4841093852778,-9.04276693141672,
46.7347615984483));
#164160=CARTESIAN_POINT('Ctrl Pts',(68.2583898464631,-8.97931075027964,
46.7701396476123));
#164161=CARTESIAN_POINT('Ctrl Pts',(67.8643962464191,-8.85205490638486,
46.8315827518995));
#164162=CARTESIAN_POINT('Ctrl Pts',(67.6951325365816,-8.79184280688282,
46.8578760183822));
#164163=CARTESIAN_POINT('Ctrl Pts',(67.4302498777407,-8.68876870089034,
46.8988278856758));
#164164=CARTESIAN_POINT('Ctrl Pts',(67.3334468299633,-8.64918510982089,
46.9137520736513));
#164165=CARTESIAN_POINT('Ctrl Pts',(67.1483118208652,-8.56977075447606,
46.942209475053));
#164166=CARTESIAN_POINT('Ctrl Pts',(67.0598948902342,-8.53018026866594,
46.9557620994396));
#164167=CARTESIAN_POINT('Ctrl Pts',(66.8498779073544,-8.43213454901513,
46.9878607591748));
#164168=CARTESIAN_POINT('Ctrl Pts',(66.7288885856046,-8.37238204604089,
47.0062766004639));
#164169=CARTESIAN_POINT('Ctrl Pts',(66.1688744394223,-8.08035568204751,
47.0911658075432));
#164170=CARTESIAN_POINT('Ctrl Pts',(65.7473152088772,-7.81532259479731,
47.153992251449));
#164171=CARTESIAN_POINT('Ctrl Pts',(65.1619997861138,-7.37792841477651,
47.2403105904215));
#164172=CARTESIAN_POINT('Ctrl Pts',(64.9805383962621,-7.23135848563247,
47.2669362214911));
#164173=CARTESIAN_POINT('Ctrl Pts',(64.6949155489118,-6.98230167254136,
47.308774952385));
#164174=CARTESIAN_POINT('Ctrl Pts',(64.5873517124558,-6.88396045552704,
47.3245142562146));
#164175=CARTESIAN_POINT('Ctrl Pts',(64.434235683113,-6.73721076280984,47.3469343340552));
#164176=CARTESIAN_POINT('Ctrl Pts',(64.3868375929826,-6.690799748617,47.3538768930162));
#164177=CARTESIAN_POINT('Ctrl Pts',(64.3005197920082,-6.60444965553853,
47.3665295639714));
#164178=CARTESIAN_POINT('Ctrl Pts',(64.2614567372036,-6.56466225397752,
47.3722597109192));
#164179=CARTESIAN_POINT('Ctrl Pts',(64.1639874271476,-6.46358280133991,
47.3865647777498));
#164180=CARTESIAN_POINT('Ctrl Pts',(64.1060511807115,-6.40183548166547,
47.3950740674123));
#164181=CARTESIAN_POINT('Ctrl Pts',(63.7365884459327,-5.99714766694451,
47.4493354637004));
#164182=CARTESIAN_POINT('Ctrl Pts',(63.449932645172,-5.6319028390746,47.4913947660234));
#164183=CARTESIAN_POINT('Ctrl Pts',(63.0437185164782,-5.02692974599468,
47.5494603011872));
#164184=CARTESIAN_POINT('Ctrl Pts',(62.905486568237,-4.80101243802735,47.5688731951127));
#164185=CARTESIAN_POINT('Ctrl Pts',(62.6839232214926,-4.40210250558855,
47.599154274381));
#164186=CARTESIAN_POINT('Ctrl Pts',(62.5960477146251,-4.23189210386382,
47.6108930877713));
#164187=CARTESIAN_POINT('Ctrl Pts',(62.467215297971,-3.96258927756738,47.6276136610573));
#164188=CARTESIAN_POINT('Ctrl Pts',(62.4226871186887,-3.86530838290369,
47.6332889398925));
#164189=CARTESIAN_POINT('Ctrl Pts',(62.340858775073,-3.67822667365684,47.6435074473755));
#164190=CARTESIAN_POINT('Ctrl Pts',(62.303275164339,-3.58856817504586,47.648106136056));
#164191=CARTESIAN_POINT('Ctrl Pts',(62.2178993929925,-3.3757775421119,47.6583186342856));
#164192=CARTESIAN_POINT('Ctrl Pts',(62.1712835390476,-3.25218515070423,
47.6637045858437));
#164193=CARTESIAN_POINT('Ctrl Pts',(61.995821435896,-2.75584633495742,47.6831779392435));
#164194=CARTESIAN_POINT('Ctrl Pts',(61.8876270265883,-2.37607830650069,
47.6932745526513));
#164195=CARTESIAN_POINT('Ctrl Pts',(61.7226473671648,-1.62151959949796,
47.7044558437569));
#164196=CARTESIAN_POINT('Ctrl Pts',(61.6640252952989,-1.24789122720521,
47.7058983580691));
#164197=CARTESIAN_POINT('Ctrl Pts',(61.6151903277049,-0.739965160821248,
47.7028607836474));
#164198=CARTESIAN_POINT('Ctrl Pts',(61.6052813083504,-0.607899836463236,
47.7016209296473));
#164199=CARTESIAN_POINT('Ctrl Pts',(61.5927768348471,-0.376140884189838,
47.6986919183964));
#164200=CARTESIAN_POINT('Ctrl Pts',(61.5889797094579,-0.276530595462918,
47.6971898566419));
#164201=CARTESIAN_POINT('Ctrl Pts',(61.5855140036737,-0.12102090730317,
47.6944797824192));
#164202=CARTESIAN_POINT('Ctrl Pts',(61.5847645279554,-0.065150117516361,
47.6934326383007));
#164203=CARTESIAN_POINT('Ctrl Pts',(61.5844968904708,-0.0061849436233789,
47.6922517218026));
#164204=CARTESIAN_POINT('Ctrl Pts',(61.5844843731439,-0.00309247043366816,
47.6921895677981));
#164205=CARTESIAN_POINT('Ctrl Pts',(61.5844733749945,-2.11872094351994E-11,
47.6921271941932));
#164206=CARTESIAN_POINT('Ctrl Pts',(61.5550078861458,-8.57747578934197E-15,
47.5250201029796));
#164207=CARTESIAN_POINT('Ctrl Pts',(61.5551466499392,-0.0390177391739191,
47.5258070715583));
#164208=CARTESIAN_POINT('Ctrl Pts',(61.5555246228054,-0.078035244936701,
47.5265441818857));
#164209=CARTESIAN_POINT('Ctrl Pts',(61.5569077936725,-0.165457667185358,
47.5280855343779));
#164210=CARTESIAN_POINT('Ctrl Pts',(61.5580420633262,-0.21385988472972,
47.5288631953164));
#164211=CARTESIAN_POINT('Ctrl Pts',(61.5633215687984,-0.383870843256392,
47.5313330557453));
#164212=CARTESIAN_POINT('Ctrl Pts',(61.5694253014728,-0.505412079323531,
47.5326283672832));
#164213=CARTESIAN_POINT('Ctrl Pts',(61.6137244421188,-1.14327639601798,
47.5370539152006));
#164214=CARTESIAN_POINT('Ctrl Pts',(61.6916432728872,-1.6559795486642,47.532472516678));
#164215=CARTESIAN_POINT('Ctrl Pts',(61.86562232674,-2.38999811288596,47.5156723695157));
#164216=CARTESIAN_POINT('Ctrl Pts',(61.928832113267,-2.61820047653147,47.5089451318185));
#164217=CARTESIAN_POINT('Ctrl Pts',(62.0554474642774,-3.01653376469872,
47.4946416439468));
#164218=CARTESIAN_POINT('Ctrl Pts',(62.115321066375,-3.18767621488445,47.4876346063985));
#164219=CARTESIAN_POINT('Ctrl Pts',(62.2177708024606,-3.45551184002182,
47.4753213623619));
#164220=CARTESIAN_POINT('Ctrl Pts',(62.2571144207432,-3.55341517606029,
47.4705284367934));
#164221=CARTESIAN_POINT('Ctrl Pts',(62.3360373800074,-3.74066542186744,
47.4607988913694));
#164222=CARTESIAN_POINT('Ctrl Pts',(62.3753802223634,-3.83009900922906,
47.4558995598736));
#164223=CARTESIAN_POINT('Ctrl Pts',(62.4728129449329,-4.04255723982814,
47.4436540388593));
#164224=CARTESIAN_POINT('Ctrl Pts',(62.5321862695213,-4.16495680680075,
47.4361040848444));
#164225=CARTESIAN_POINT('Ctrl Pts',(62.8218225772558,-4.73051262752732,
47.398873577017));
#164226=CARTESIAN_POINT('Ctrl Pts',(63.0843269759402,-5.15589913604641,
47.3640729969055));
#164227=CARTESIAN_POINT('Ctrl Pts',(63.5176138977982,-5.74710380199329,
47.304553013241));
#164228=CARTESIAN_POINT('Ctrl Pts',(63.6631240768806,-5.9308010822008,47.2842770792455));
#164229=CARTESIAN_POINT('Ctrl Pts',(63.910228768393,-6.21983196189127,47.2492442363948));
#164230=CARTESIAN_POINT('Ctrl Pts',(64.0077335368504,-6.32862363727644,
47.2352824525607));
#164231=CARTESIAN_POINT('Ctrl Pts',(64.1531645247452,-6.48344999781946,
47.2142217125675));
#164232=CARTESIAN_POINT('Ctrl Pts',(64.1991292329824,-6.53135292580872,
47.207532476842));
#164233=CARTESIAN_POINT('Ctrl Pts',(64.2846184892329,-6.61857131894665,
47.1950263512879));
#164234=CARTESIAN_POINT('Ctrl Pts',(64.3239940899608,-6.65803189607302,
47.1892409831086));
#164235=CARTESIAN_POINT('Ctrl Pts',(64.4239882017162,-6.75646608755569,
47.1744896157259));
#164236=CARTESIAN_POINT('Ctrl Pts',(64.485051260719,-6.81496635591992,47.1654280179423));
#164237=CARTESIAN_POINT('Ctrl Pts',(64.8851917031561,-7.18802064291156,
47.1057509541167));
#164238=CARTESIAN_POINT('Ctrl Pts',(65.246089911098,-7.47747301965684,47.0505959331056));
#164239=CARTESIAN_POINT('Ctrl Pts',(65.8440877113012,-7.88763978087938,
46.9587122914352));
#164240=CARTESIAN_POINT('Ctrl Pts',(66.0675998329727,-8.02728250731837,
46.9242661934201));
#164241=CARTESIAN_POINT('Ctrl Pts',(66.4622229107417,-8.25091994101796,
46.8634760263164));
#164242=CARTESIAN_POINT('Ctrl Pts',(66.6305751404579,-8.33955199854741,
46.8375488661788));
#164243=CARTESIAN_POINT('Ctrl Pts',(66.8969142990296,-8.46938770285203,
46.7965844117256));
#164244=CARTESIAN_POINT('Ctrl Pts',(66.9931037352125,-8.51423380483586,
46.7818001697188));
#164245=CARTESIAN_POINT('Ctrl Pts',(67.1780726868272,-8.59660126994594,
46.7533953828372));
#164246=CARTESIAN_POINT('Ctrl Pts',(67.2667108111955,-8.63441207134806,
46.7397942764122));
#164247=CARTESIAN_POINT('Ctrl Pts',(67.4770552646312,-8.72025170957431,
46.7075454447762));
#164248=CARTESIAN_POINT('Ctrl Pts',(67.5992178392097,-8.76708392977196,
46.6888376908535));
#164249=CARTESIAN_POINT('Ctrl Pts',(68.0877213237592,-8.94246898040873,
46.6141138830279));
#164250=CARTESIAN_POINT('Ctrl Pts',(68.4609451081589,-9.05027444007471,
46.5572286433543));
#164251=CARTESIAN_POINT('Ctrl Pts',(69.1384202529569,-9.20012355536855,
46.454031785933));
#164252=CARTESIAN_POINT('Ctrl Pts',(69.4401423684263,-9.25116333983993,
46.4080871231519));
#164253=CARTESIAN_POINT('Ctrl Pts',(69.9118519146182,-9.30682771093848,
46.335996027152));
#164254=CARTESIAN_POINT('Ctrl Pts',(70.0804229631028,-9.32199090897221,
46.3101805850801));
#164255=CARTESIAN_POINT('Ctrl Pts',(70.3670168959907,-9.33976906949828,
46.2661312373467));
#164256=CARTESIAN_POINT('Ctrl Pts',(70.4848592141131,-9.34479208510376,
46.2479731742685));
#164257=CARTESIAN_POINT('Ctrl Pts',(70.6616576905881,-9.34890189414368,
46.2206385601175));
#164258=CARTESIAN_POINT('Ctrl Pts',(70.7205700520679,-9.34970129843407,
46.2115148376248));
#164259=CARTESIAN_POINT('Ctrl Pts',(70.8307493783468,-9.35013038734498,
46.1944188567541));
#164260=CARTESIAN_POINT('Ctrl Pts',(70.8820134822541,-9.34989842911278,
46.1864508561971));
#164261=CARTESIAN_POINT('Ctrl Pts',(71.0107185141546,-9.34823231006586,
46.1664150555058));
#164262=CARTESIAN_POINT('Ctrl Pts',(71.0881461623868,-9.34624450066235,
46.1543337094176));
#164263=CARTESIAN_POINT('Ctrl Pts',(71.4413678007677,-9.33267705949493,
46.0991160975365));
#164264=CARTESIAN_POINT('Ctrl Pts',(71.7165470145877,-9.30957899594627,
46.0558146266122));
#164265=CARTESIAN_POINT('Ctrl Pts',(72.3126682665991,-9.23219861293737,
45.9618790324743));
#164266=CARTESIAN_POINT('Ctrl Pts',(72.6326325541485,-9.17315840028106,
45.9113791504871));
#164267=CARTESIAN_POINT('Ctrl Pts',(73.1765026348197,-9.0424835919843,45.8258868138484));
#164268=CARTESIAN_POINT('Ctrl Pts',(73.4019955279895,-8.97906561901957,
45.7905447187263));
#164269=CARTESIAN_POINT('Ctrl Pts',(73.795651876037,-8.85188941371181,45.7291547498995));
#164270=CARTESIAN_POINT('Ctrl Pts',(73.9648023501125,-8.79170841246524,
45.7028792692916));
#164271=CARTESIAN_POINT('Ctrl Pts',(74.2295535742093,-8.68867659973452,
45.6619479156828));
#164272=CARTESIAN_POINT('Ctrl Pts',(74.3263364205575,-8.64909837275343,
45.6470269075817));
#164273=CARTESIAN_POINT('Ctrl Pts',(74.5114579923559,-8.56968490555063,
45.618571683026));
#164274=CARTESIAN_POINT('Ctrl Pts',(74.5998813268982,-8.5300890533527,45.6050181348481));
#164275=CARTESIAN_POINT('Ctrl Pts',(74.809955222012,-8.43201041005115,45.5729109238203));
#164276=CARTESIAN_POINT('Ctrl Pts',(74.9309940655172,-8.37222830638353,
45.5544876642797));
#164277=CARTESIAN_POINT('Ctrl Pts',(75.4903302536429,-8.08052453772989,
45.4697019241712));
#164278=CARTESIAN_POINT('Ctrl Pts',(75.9112239243894,-7.81596122060783,
45.4069732045745));
#164279=CARTESIAN_POINT('Ctrl Pts',(76.4963352276659,-7.37891845664684,
45.3206825547105));
#164280=CARTESIAN_POINT('Ctrl Pts',(76.678159003098,-7.23210008835748,45.2940034671813));
#164281=CARTESIAN_POINT('Ctrl Pts',(76.9642550736277,-6.98266918936499,
45.2520952760861));
#164282=CARTESIAN_POINT('Ctrl Pts',(77.0719454317692,-6.88422217714014,
45.2363374664093));
#164283=CARTESIAN_POINT('Ctrl Pts',(77.225202146662,-6.73734451562587,45.2138968045589));
#164284=CARTESIAN_POINT('Ctrl Pts',(77.2726192427457,-6.69091668052719,
45.2069514689035));
#164285=CARTESIAN_POINT('Ctrl Pts',(77.3589516146158,-6.60455463154549,
45.1942966756078));
#164286=CARTESIAN_POINT('Ctrl Pts',(77.3980106932074,-6.56477257182652,
45.188567119731));
#164287=CARTESIAN_POINT('Ctrl Pts',(77.4954423192641,-6.46373569462105,
45.1742675968315));
#164288=CARTESIAN_POINT('Ctrl Pts',(77.5533457608891,-6.40202647514572,
45.1657631327824));
#164289=CARTESIAN_POINT('Ctrl Pts',(77.9225945180331,-5.99760019624139,
45.1115331558459));
#164290=CARTESIAN_POINT('Ctrl Pts',(78.2091009640789,-5.63260532935765,
45.06949544635));
#164291=CARTESIAN_POINT('Ctrl Pts',(78.6153548458468,-5.0277362445293,45.0114214416589));
#164292=CARTESIAN_POINT('Ctrl Pts',(78.7537240859896,-4.8016396884229,44.9919882995805));
#164293=CARTESIAN_POINT('Ctrl Pts',(78.9754661633144,-4.40245786836224,
44.9616816701779));
#164294=CARTESIAN_POINT('Ctrl Pts',(79.063393923333,-4.23216176019283,44.9499354992954));
#164295=CARTESIAN_POINT('Ctrl Pts',(79.1922824622699,-3.96275629974334,
44.9332072798286));
#164296=CARTESIAN_POINT('Ctrl Pts',(79.2368193941881,-3.86546105389666,
44.9275307655133));
#164297=CARTESIAN_POINT('Ctrl Pts',(79.3186554432657,-3.67836983199058,
44.9173110904372));
#164298=CARTESIAN_POINT('Ctrl Pts',(79.3562386570575,-3.58871647202851,
44.912712343258));
#164299=CARTESIAN_POINT('Ctrl Pts',(79.4416020820573,-3.37596734514096,
44.9025010467075));
#164300=CARTESIAN_POINT('Ctrl Pts',(79.4882073372486,-3.25241183615882,
44.8971160936505));
#164301=CARTESIAN_POINT('Ctrl Pts',(79.6628853659389,-2.75833735794606,
44.8777285700723));
#164302=CARTESIAN_POINT('Ctrl Pts',(79.7705828292355,-2.38088847080519,
44.867663202802));
#164303=CARTESIAN_POINT('Ctrl Pts',(79.9209728102791,-1.6955995292544,44.8574101028781));
#164304=CARTESIAN_POINT('Ctrl Pts',(79.9724968997835,-1.390311142986,44.8555861998798));
#164305=CARTESIAN_POINT('Ctrl Pts',(80.0291897862859,-0.913183433070077,
44.8566749372101));
#164306=CARTESIAN_POINT('Ctrl Pts',(80.0447736721481,-0.742798737011347,
44.8578326514166));
#164307=CARTESIAN_POINT('Ctrl Pts',(80.0633729428985,-0.45307008460399,
44.8610342535038));
#164308=CARTESIAN_POINT('Ctrl Pts',(80.068763381637,-0.333916737630476,
44.8627032990736));
#164309=CARTESIAN_POINT('Ctrl Pts',(80.0734641142772,-0.155118865850148,
44.8657128003228));
#164310=CARTESIAN_POINT('Ctrl Pts',(80.0744669279504,-0.0955265730669187,
44.8667998810079));
#164311=CARTESIAN_POINT('Ctrl Pts',(80.0752874772849,0.0159413341490429,
44.8689866509228));
#164312=CARTESIAN_POINT('Ctrl Pts',(80.0752418806346,0.0678133948819915,
44.870065988658));
#164313=CARTESIAN_POINT('Ctrl Pts',(80.0740545116948,0.198066253930946,
44.872934184593));
#164314=CARTESIAN_POINT('Ctrl Pts',(80.0723643185048,0.276436314977128,
44.8748038435572));
#164315=CARTESIAN_POINT('Ctrl Pts',(80.0602153783642,0.633609941853107,
44.8840054660573));
#164316=CARTESIAN_POINT('Ctrl Pts',(80.0383926790477,0.911838032421433,
44.893068252948));
#164317=CARTESIAN_POINT('Ctrl Pts',(79.9641819924431,1.51493124829092,44.9173252648197));
#164318=CARTESIAN_POINT('Ctrl Pts',(79.9070763060138,1.83880768724944,44.9333129482378));
#164319=CARTESIAN_POINT('Ctrl Pts',(79.7801803750855,2.38939724846813,44.9660968304035));
#164320=CARTESIAN_POINT('Ctrl Pts',(79.7184606004295,2.61773097458111,44.9814003407129));
#164321=CARTESIAN_POINT('Ctrl Pts',(79.5945447213174,3.01625970548475,45.0112758931591));
#164322=CARTESIAN_POINT('Ctrl Pts',(79.5358680677186,3.18746777811519,45.025173712915));
#164323=CARTESIAN_POINT('Ctrl Pts',(79.4353618405169,3.45537956016921,45.0486486052679));
#164324=CARTESIAN_POINT('Ctrl Pts',(79.3967486683343,3.55329460465372,45.0576017840323));
#164325=CARTESIAN_POINT('Ctrl Pts',(79.3192571654795,3.74055264121777,45.0754524385989));
#164326=CARTESIAN_POINT('Ctrl Pts',(79.2806143248932,3.82998252195275,45.0843039694124));
#164327=CARTESIAN_POINT('Ctrl Pts',(79.1848877315677,4.04240778784193,45.1061167971568));
#164328=CARTESIAN_POINT('Ctrl Pts',(79.1265293936778,4.16477867426913,45.1193253589925));
#164329=CARTESIAN_POINT('Ctrl Pts',(78.8414452200882,4.73072936788794,45.1834428390304));
#164330=CARTESIAN_POINT('Ctrl Pts',(78.5826047965841,5.15650301509456,45.2405807210477));
#164331=CARTESIAN_POINT('Ctrl Pts',(78.1548929060647,5.74782591547893,45.3328828326126));
#164332=CARTESIAN_POINT('Ctrl Pts',(78.0113632840991,5.93131211553293,45.3635663948128));
#164333=CARTESIAN_POINT('Ctrl Pts',(77.7673898535157,6.22006742031824,45.4151158154594));
#164334=CARTESIAN_POINT('Ctrl Pts',(77.671049793879,6.32878544188141,45.4353319131716));
#164335=CARTESIAN_POINT('Ctrl Pts',(77.5272583743304,6.48352990604932,45.46526645379));
#164336=CARTESIAN_POINT('Ctrl Pts',(77.4817873108411,6.53142177293023,45.4746994806034));
#164337=CARTESIAN_POINT('Ctrl Pts',(77.3971830833238,6.61863168363854,45.4921851679235));
#164338=CARTESIAN_POINT('Ctrl Pts',(77.3582003927593,6.65809457282074,45.5002165439707));
#164339=CARTESIAN_POINT('Ctrl Pts',(77.2591673676685,6.75655068466948,45.5205596644514));
#164340=CARTESIAN_POINT('Ctrl Pts',(77.1986661035534,6.81507003666324,45.5329336887519));
#164341=CARTESIAN_POINT('Ctrl Pts',(76.8021021880893,7.18824546712365,45.613740635306));
#164342=CARTESIAN_POINT('Ctrl Pts',(76.4439674282961,7.47778191758882,45.6853731746204));
#164343=CARTESIAN_POINT('Ctrl Pts',(75.8505507713923,7.88792505719625,45.8035688445681));
#164344=CARTESIAN_POINT('Ctrl Pts',(75.6288358823475,8.0274896321279,45.847626050178));
#164345=CARTESIAN_POINT('Ctrl Pts',(75.2373702839884,8.25102541207991,45.9254411657672));
#164346=CARTESIAN_POINT('Ctrl Pts',(75.0703506874581,8.33962776470298,45.9586480616816));
#164347=CARTESIAN_POINT('Ctrl Pts',(74.8061197910239,8.46943159045896,46.0112361559338));
#164348=CARTESIAN_POINT('Ctrl Pts',(74.7106827095551,8.51427271694368,46.0302406658211));
#164349=CARTESIAN_POINT('Ctrl Pts',(74.5271590011423,8.59663579344307,46.0668109694259));
#164350=CARTESIAN_POINT('Ctrl Pts',(74.4392117213579,8.63444680875874,46.0843467064769));
#164351=CARTESIAN_POINT('Ctrl Pts',(74.2304999226481,8.72029340928881,46.1259893476084));
#164352=CARTESIAN_POINT('Ctrl Pts',(74.1092858588738,8.76713160347592,46.1501959514979));
#164353=CARTESIAN_POINT('Ctrl Pts',(73.623472004764,8.94294650236137,46.2472992278547));
#164354=CARTESIAN_POINT('Ctrl Pts',(73.2520583667685,9.05102226038947,46.321744446618));
#164355=CARTESIAN_POINT('Ctrl Pts',(72.5725213296973,9.20225946910197,46.4580100925124));
#164356=CARTESIAN_POINT('Ctrl Pts',(72.266807608604,9.25392665468341,46.5193298191909));
#164357=CARTESIAN_POINT('Ctrl Pts',(71.7967307155527,9.30861069770923,46.6133379064377));
#164358=CARTESIAN_POINT('Ctrl Pts',(71.6338984807729,9.32307020107794,46.645849649464));
#164359=CARTESIAN_POINT('Ctrl Pts',(71.3560634116172,9.34012859970737,46.7011688961548));
#164360=CARTESIAN_POINT('Ctrl Pts',(71.2412404937854,9.34497303030257,46.7239862122937));
#164361=CARTESIAN_POINT('Ctrl Pts',(71.0682681832646,9.34895390789572,46.7582687371924));
#164362=CARTESIAN_POINT('Ctrl Pts',(71.0101747427237,9.34972824786854,46.7697673586588));
#164363=CARTESIAN_POINT('Ctrl Pts',(70.901627033317,9.3501241138955,46.7912201515143));
#164364=CARTESIAN_POINT('Ctrl Pts',(70.8511767883932,9.34988403705377,46.8011773995548));
#164365=CARTESIAN_POINT('Ctrl Pts',(70.7234825994232,9.34820305143747,46.8263491217628));
#164366=CARTESIAN_POINT('Ctrl Pts',(70.6462466740132,9.34619205452021,46.8415458203407));
#164367=CARTESIAN_POINT('Ctrl Pts',(70.2968982520604,9.33259629184533,46.910178973912));
#164368=CARTESIAN_POINT('Ctrl Pts',(70.0253013412726,9.30966583385118,46.9632555188312));
#164369=CARTESIAN_POINT('Ctrl Pts',(69.4347663982018,9.23273047198067,47.0785272525984));
#164370=CARTESIAN_POINT('Ctrl Pts',(69.1168088671572,9.17380466130383,47.140510010473));
#164371=CARTESIAN_POINT('Ctrl Pts',(68.575903963802,9.04319115422186,47.2463019625653));
#164372=CARTESIAN_POINT('Ctrl Pts',(68.3513592349754,8.97967774756271,47.2903236630419));
#164373=CARTESIAN_POINT('Ctrl Pts',(67.9596093454733,8.85230258111096,47.367437824625));
#164374=CARTESIAN_POINT('Ctrl Pts',(67.7913921456816,8.79204390546941,47.400654814471));
#164375=CARTESIAN_POINT('Ctrl Pts',(67.5282819835793,8.68890644369087,47.4528063144562));
#164376=CARTESIAN_POINT('Ctrl Pts',(67.4321824434198,8.64931481581403,47.4718966298189));
#164377=CARTESIAN_POINT('Ctrl Pts',(67.2484593626417,8.56989909888166,47.5084791513825));
#164378=CARTESIAN_POINT('Ctrl Pts',(67.1607487912074,8.53031662042858,47.5259822513675));
#164379=CARTESIAN_POINT('Ctrl Pts',(66.9525031809757,8.43232004852205,47.5676323568917));
#164380=CARTESIAN_POINT('Ctrl Pts',(66.8325850799753,8.37261173540689,47.591693032778));
#164381=CARTESIAN_POINT('Ctrl Pts',(66.2763344791619,8.08011881748052,47.7036547071207));
#164382=CARTESIAN_POINT('Ctrl Pts',(65.8577528356841,7.81440369621049,47.7889962894379));
#164383=CARTESIAN_POINT('Ctrl Pts',(65.2779173637126,7.37649729721469,47.9081376415754));
#164384=CARTESIAN_POINT('Ctrl Pts',(65.0988108022077,7.23028613382362,47.9450747958339));
#164385=CARTESIAN_POINT('Ctrl Pts',(64.8167799410034,6.98176966596709,48.0033085362981));
#164386=CARTESIAN_POINT('Ctrl Pts',(64.7105009217701,6.88358146425984,48.0252699974668));
#164387=CARTESIAN_POINT('Ctrl Pts',(64.5591522066784,6.73701687399964,48.0565291608474));
#164388=CARTESIAN_POINT('Ctrl Pts',(64.5122653144452,6.69063021813372,48.0662107561013));
#164389=CARTESIAN_POINT('Ctrl Pts',(64.4268464822436,6.60429739213573,48.0838392412265));
#164390=CARTESIAN_POINT('Ctrl Pts',(64.3881736469449,6.56450220826576,48.0918161896623));
#164391=CARTESIAN_POINT('Ctrl Pts',(64.2916356048183,6.46336087245438,48.1117214535804));
#164392=CARTESIAN_POINT('Ctrl Pts',(64.2342358054794,6.40155819219595,48.1235504136862));
#164393=CARTESIAN_POINT('Ctrl Pts',(63.8681269878283,5.99642266751781,48.1990011178357));
#164394=CARTESIAN_POINT('Ctrl Pts',(63.5841079256245,5.63073787295009,48.2575756279011));
#164395=CARTESIAN_POINT('Ctrl Pts',(63.1825862566011,5.02556877408242,48.3419386339542));
#164396=CARTESIAN_POINT('Ctrl Pts',(63.0462802689799,4.79995372401824,48.3709275079765));
#164397=CARTESIAN_POINT('Ctrl Pts',(62.8280200629741,4.40150236508274,48.4181891275067));
#164398=CARTESIAN_POINT('Ctrl Pts',(62.7415162948175,4.23143661175899,48.4371949525007));
#164399=CARTESIAN_POINT('Ctrl Pts',(62.614828075304,3.96230700734142,48.4655257645866));
#164400=CARTESIAN_POINT('Ctrl Pts',(62.5710588156807,3.86505034155375,48.4754191868442));
#164401=CARTESIAN_POINT('Ctrl Pts',(62.4906832805168,3.67798465926539,48.4938012777463));
#164402=CARTESIAN_POINT('Ctrl Pts',(62.4537927894449,3.58831745171678,48.5023346002953));
#164403=CARTESIAN_POINT('Ctrl Pts',(62.3700525881338,3.3754565605272,48.5219434618219));
#164404=CARTESIAN_POINT('Ctrl Pts',(62.3243884767053,3.25180174801528,48.5328304309446));
#164405=CARTESIAN_POINT('Ctrl Pts',(62.1511607465684,2.75050009199837,48.5749553460674));
#164406=CARTESIAN_POINT('Ctrl Pts',(62.0449873355903,2.36562747392848,48.6027816976324));
#164407=CARTESIAN_POINT('Ctrl Pts',(61.8871778716001,1.60968238304879,48.6485502601413));
#164408=CARTESIAN_POINT('Ctrl Pts',(61.832583123548,1.24001638979765,48.6669726065383));
#164409=CARTESIAN_POINT('Ctrl Pts',(61.788351794091,0.736774046757258,48.6863097536381));
#164410=CARTESIAN_POINT('Ctrl Pts',(61.7795485402972,0.605367799175815,
48.6908333914838));
#164411=CARTESIAN_POINT('Ctrl Pts',(61.7688926641797,0.374627363626792,
48.6978226176743));
#164412=CARTESIAN_POINT('Ctrl Pts',(61.7658631597748,0.275375134965116,
48.7005202239672));
#164413=CARTESIAN_POINT('Ctrl Pts',(61.7635527613475,0.120295156280997,
48.7042392363218));
#164414=CARTESIAN_POINT('Ctrl Pts',(61.7632111060365,0.0644956546494876,
48.7054771489709));
#164415=CARTESIAN_POINT('Ctrl Pts',(61.7633664053386,0.00579618557849801,
48.7066722253423));
#164416=CARTESIAN_POINT('Ctrl Pts',(61.763375392491,0.00289809158621373,
48.7067309535146));
#164417=CARTESIAN_POINT('Ctrl Pts',(61.763385699346,1.76224501330106E-11,
48.7067894065939));
#164418=CARTESIAN_POINT('Origin',(69.6316151486327,0.,39.48523201752));
#164419=CARTESIAN_POINT('',(61.9938354925483,-1.14504475720278E-15,50.0137351291169));
#164420=CARTESIAN_POINT('',(61.9717635125435,4.06541970932136E-10,49.8885587101925));
#164421=CARTESIAN_POINT('',(60.4236626579685,-1.14504475720278E-15,41.1088424787055));
#164422=CARTESIAN_POINT('',(62.2702697977904,2.27382383755812,49.9649923028056));
#164423=CARTESIAN_POINT('Origin',(71.2017879831895,0.,48.390124667801));
#164424=CARTESIAN_POINT('Ctrl Pts',(62.2702697981662,2.2738238374481,49.9649923025089));
#164425=CARTESIAN_POINT('Ctrl Pts',(62.338464173385,2.5537129532415,49.9476325953518));
#164426=CARTESIAN_POINT('Ctrl Pts',(62.4193581571629,2.83019087195468,49.9279210944292));
#164427=CARTESIAN_POINT('Ctrl Pts',(62.5465841826798,3.20128874871533,49.8977784992525));
#164428=CARTESIAN_POINT('Ctrl Pts',(62.5821211470682,3.29959436495245,49.8894317833168));
#164429=CARTESIAN_POINT('Ctrl Pts',(62.6511157296328,3.48097710305096,49.8733500262581));
#164430=CARTESIAN_POINT('Ctrl Pts',(62.6841409394582,3.56421300851538,49.8656989389923));
#164431=CARTESIAN_POINT('Ctrl Pts',(62.755504163825,3.73686226755046,49.8492574290012));
#164432=CARTESIAN_POINT('Ctrl Pts',(62.7940500879524,3.82617414250865,49.8404267614445));
#164433=CARTESIAN_POINT('Ctrl Pts',(62.8891808036111,4.03753497415995,49.8187464730798));
#164434=CARTESIAN_POINT('Ctrl Pts',(62.947003098936,4.15897804528599,49.8056567782711));
#164435=CARTESIAN_POINT('Ctrl Pts',(63.2321092720499,4.72609987004622,49.7415198841712));
#164436=CARTESIAN_POINT('Ctrl Pts',(63.4918566382141,5.15381181483561,49.6841744167643));
#164437=CARTESIAN_POINT('Ctrl Pts',(63.9208794975226,5.74710370347294,49.5915863256821));
#164438=CARTESIAN_POINT('Ctrl Pts',(64.0645491360096,5.93080101248646,49.5608720547424));
#164439=CARTESIAN_POINT('Ctrl Pts',(64.3087335579026,6.21983192977895,49.5092773704718));
#164440=CARTESIAN_POINT('Ctrl Pts',(64.4051332887595,6.32862361521098,49.489048559097));
#164441=CARTESIAN_POINT('Ctrl Pts',(64.5489969220775,6.48344998692467,49.4590988516647));
#164442=CARTESIAN_POINT('Ctrl Pts',(64.5944774738798,6.53135291642221,49.4496638207421));
#164443=CARTESIAN_POINT('Ctrl Pts',(64.6790884449091,6.6185713107172,49.4321766867671));
#164444=CARTESIAN_POINT('Ctrl Pts',(64.7180681183952,6.65803188752871,49.4241459060302));
#164445=CARTESIAN_POINT('Ctrl Pts',(64.8170771088458,6.75646607602476,49.4038076573357));
#164446=CARTESIAN_POINT('Ctrl Pts',(64.8775568608351,6.81496634178852,49.3914379783055));
#164447=CARTESIAN_POINT('Ctrl Pts',(65.2739766207081,7.18802061279423,49.3106599871719));
#164448=CARTESIAN_POINT('Ctrl Pts',(65.6319741136846,7.47747297851757,49.2390543001437));
#164449=CARTESIAN_POINT('Ctrl Pts',(66.2253342827472,7.88763974299578,49.1208693882525));
#164450=CARTESIAN_POINT('Ctrl Pts',(66.4471482466748,8.02728247981476,49.0767924818669));
#164451=CARTESIAN_POINT('Ctrl Pts',(66.8387641224665,8.25091992701465,48.9989475077277));
#164452=CARTESIAN_POINT('Ctrl Pts',(67.0058310877387,8.33955198848845,48.9657312138024));
#164453=CARTESIAN_POINT('Ctrl Pts',(67.2701187057887,8.46938769702591,48.9131318506826));
#164454=CARTESIAN_POINT('Ctrl Pts',(67.3655637187904,8.51423379967032,48.894125768842));
#164455=CARTESIAN_POINT('Ctrl Pts',(67.5490926876763,8.59660126536313,48.8575544299901));
#164456=CARTESIAN_POINT('Ctrl Pts',(67.637037131058,8.63441206673688,48.8400192654076));
#164457=CARTESIAN_POINT('Ctrl Pts',(67.8457260087512,8.72025170403908,48.7983812150223));
#164458=CARTESIAN_POINT('Ctrl Pts',(67.9669197045937,8.76708392344383,48.7741786926102));
#164459=CARTESIAN_POINT('Ctrl Pts',(68.4515197156878,8.94246891885684,48.6773181028156));
#164460=CARTESIAN_POINT('Ctrl Pts',(68.8216910900359,9.05027434378702,48.6031227226294));
#164461=CARTESIAN_POINT('Ctrl Pts',(69.4936031650876,9.2001231144595,48.4683862474918));
#164462=CARTESIAN_POINT('Ctrl Pts',(69.7928416204905,9.25116272674127,48.4083653859328));
#164463=CARTESIAN_POINT('Ctrl Pts',(70.260759596456,9.30682730389654,48.3147748092573));
#164464=CARTESIAN_POINT('Ctrl Pts',(70.427994969166,9.32199066334297,48.2813784943645));
#164465=CARTESIAN_POINT('Ctrl Pts',(70.7123724214733,9.33976898814513,48.2247501463861));
#164466=CARTESIAN_POINT('Ctrl Pts',(70.8293188809134,9.34479204429296,48.2015086019685));
#164467=CARTESIAN_POINT('Ctrl Pts',(71.004804660127,9.34890188244447,48.1667259841301));
#164468=CARTESIAN_POINT('Ctrl Pts',(71.063284755114,9.3497012923494,48.155150247211));
#164469=CARTESIAN_POINT('Ctrl Pts',(71.1726666825065,9.35013038818495,48.1335316537052));
#164470=CARTESIAN_POINT('Ctrl Pts',(71.2235643702529,9.34989843344863,48.1234857745022));
#164471=CARTESIAN_POINT('Ctrl Pts',(71.3513599646629,9.34823232635723,48.0982935985594));
#164472=CARTESIAN_POINT('Ctrl Pts',(71.4282500255082,9.34624452985781,48.0831645726596));
#164473=CARTESIAN_POINT('Ctrl Pts',(71.7790590888718,9.33267699070815,48.0142424997428));
#164474=CARTESIAN_POINT('Ctrl Pts',(72.0524568776137,9.30957845060198,47.9608149724904));
#164475=CARTESIAN_POINT('Ctrl Pts',(72.6447593322961,9.23219685377472,47.8451993336549));
#164476=CARTESIAN_POINT('Ctrl Pts',(72.9626993329413,9.17315626279074,47.783219477862));
#164477=CARTESIAN_POINT('Ctrl Pts',(73.5030081749324,9.04248125187234,47.6775418488351));
#164478=CARTESIAN_POINT('Ctrl Pts',(73.7269880315798,8.97906359442736,47.6336298041711));
#164479=CARTESIAN_POINT('Ctrl Pts',(74.1178978365918,8.85188804666713,47.5566796443309));
#164480=CARTESIAN_POINT('Ctrl Pts',(74.2858331036707,8.79170730222868,47.5235178319677));
#164481=CARTESIAN_POINT('Ctrl Pts',(74.5486161449311,8.68867583872546,47.4714306833254));
#164482=CARTESIAN_POINT('Ctrl Pts',(74.6446653910438,8.64909765603412,47.4523501939351));
#164483=CARTESIAN_POINT('Ctrl Pts',(74.8283549156776,8.56968419609555,47.4157740729919));
#164484=CARTESIAN_POINT('Ctrl Pts',(74.9160813095565,8.53008829951544,47.3982676697056));
#164485=CARTESIAN_POINT('Ctrl Pts',(75.1244679779698,8.43200938396914,47.3565889807507));
#164486=CARTESIAN_POINT('Ctrl Pts',(75.244508817673,8.37222703554004,47.3325033767778));
#164487=CARTESIAN_POINT('Ctrl Pts',(75.7991057103828,8.08052596965006,47.2208727946198));
#164488=CARTESIAN_POINT('Ctrl Pts',(76.2160653638557,7.81596658217665,47.1358655314547));
#164489=CARTESIAN_POINT('Ctrl Pts',(76.7954016041098,7.3789267530892,47.016832730998));
#164490=CARTESIAN_POINT('Ctrl Pts',(76.9753878582457,7.23210630205661,46.9797148608713));
#164491=CARTESIAN_POINT('Ctrl Pts',(77.2585675970679,6.98267226730892,46.9212442501048));
#164492=CARTESIAN_POINT('Ctrl Pts',(77.365153969425,6.88422436874041,46.8992192589907));
#164493=CARTESIAN_POINT('Ctrl Pts',(77.5168444983906,6.73734563515452,46.8678894586805));
#164494=CARTESIAN_POINT('Ctrl Pts',(77.56377759588,6.69091765920212,46.8581983047626));
#164495=CARTESIAN_POINT('Ctrl Pts',(77.6492318037112,6.60455550999448,46.8405624853882));
#164496=CARTESIAN_POINT('Ctrl Pts',(77.6878949222799,6.56477349489488,46.8325875218241));
#164497=CARTESIAN_POINT('Ctrl Pts',(77.7843411152716,6.46373697365865,46.8127011634677));
#164498=CARTESIAN_POINT('Ctrl Pts',(77.8416609785207,6.4020280727773,46.8008886580784));
#164499=CARTESIAN_POINT('Ctrl Pts',(78.2071873852409,5.99760386885256,46.7255579986303));
#164500=CARTESIAN_POINT('Ctrl Pts',(78.4907919707448,5.63261096514926,46.6670697883629));
#164501=CARTESIAN_POINT('Ctrl Pts',(78.8924085685413,5.02774267575176,46.5826944414633));
#164502=CARTESIAN_POINT('Ctrl Pts',(79.029080732912,4.80164468987789,46.5536303315256));
#164503=CARTESIAN_POINT('Ctrl Pts',(79.2478170137369,4.40246070129444,46.506268694393));
#164504=CARTESIAN_POINT('Ctrl Pts',(79.3344599196518,4.23216390971288,46.4872333320305));
#164505=CARTESIAN_POINT('Ctrl Pts',(79.4612973579826,3.96275763087981,46.4588701440984));
#164506=CARTESIAN_POINT('Ctrl Pts',(79.5050899354381,3.86546227061342,46.4489717802639));
#164507=CARTESIAN_POINT('Ctrl Pts',(79.5854860625327,3.67837097280466,46.4305855440169));
#164508=CARTESIAN_POINT('Ctrl Pts',(79.6223755925697,3.58871765375311,46.4220527381548));
#164509=CARTESIAN_POINT('Ctrl Pts',(79.7060833465627,3.37596885746274,46.4024522319571));
#164510=CARTESIAN_POINT('Ctrl Pts',(79.7517196413179,3.25241364226893,46.391572517949));
#164511=CARTESIAN_POINT('Ctrl Pts',(79.9224884864789,2.75835612932782,46.3500488300955));
#164512=CARTESIAN_POINT('Ctrl Pts',(80.027129980208,2.38092459736502,46.3226735320467));
#164513=CARTESIAN_POINT('Ctrl Pts',(80.1719215452331,1.69582363312823,46.2808826249113));
#164514=CARTESIAN_POINT('Ctrl Pts',(80.2209447227862,1.39070876900675,46.2649814678225));
#164515=CARTESIAN_POINT('Ctrl Pts',(80.2738681521203,0.913647685411539,
46.2445656265649));
#164516=CARTESIAN_POINT('Ctrl Pts',(80.288132803381,0.743153784572283,46.2381421771222));
#164517=CARTESIAN_POINT('Ctrl Pts',(80.304532047063,0.453263255336513,46.2287656175665));
#164518=CARTESIAN_POINT('Ctrl Pts',(80.3090306207632,0.334057623561011,
46.2253516693286));
#164519=CARTESIAN_POINT('Ctrl Pts',(80.3124213869859,0.155197929449151,
46.2209140455259));
#164520=CARTESIAN_POINT('Ctrl Pts',(80.3129924750905,0.0955961728885822,
46.2195492289462));
#164521=CARTESIAN_POINT('Ctrl Pts',(80.3130163234586,-0.0158780266130571,
46.2172134153308));
#164522=CARTESIAN_POINT('Ctrl Pts',(80.3126046991915,-0.067746912733556,
46.2162147521974));
#164523=CARTESIAN_POINT('Ctrl Pts',(80.3105092968841,-0.19797558035514,
46.213925863527));
#164524=CARTESIAN_POINT('Ctrl Pts',(80.3082830027052,-0.276324636184175,
46.2127471856332));
#164525=CARTESIAN_POINT('Ctrl Pts',(80.2937134039405,-0.633772313972398,
46.2082512290248));
#164526=CARTESIAN_POINT('Ctrl Pts',(80.2700730893575,-0.912294168723618,
46.2071995336871));
#164527=CARTESIAN_POINT('Ctrl Pts',(80.1919557585515,-1.51567466321251,
46.209796991434));
#164528=CARTESIAN_POINT('Ctrl Pts',(80.1328000113206,-1.83954712985001,
46.2143092903021));
#164529=CARTESIAN_POINT('Ctrl Pts',(80.0023306136439,-2.38999819416391,
46.2269079630008));
#164530=CARTESIAN_POINT('Ctrl Pts',(79.9391208300848,-2.61820054004301,
46.2336352004851));
#164531=CARTESIAN_POINT('Ctrl Pts',(79.8125054852325,-3.01653380177633,
46.2479386877612));
#164532=CARTESIAN_POINT('Ctrl Pts',(79.7526318855361,-3.18767624308534,
46.254945725055));
#164533=CARTESIAN_POINT('Ctrl Pts',(79.6501821527119,-3.45551185792078,
46.2672589687228));
#164534=CARTESIAN_POINT('Ctrl Pts',(79.6108385348436,-3.5534151923753,46.2720518942478));
#164535=CARTESIAN_POINT('Ctrl Pts',(79.5319155756486,-3.74066543713012,
46.2817814396745));
#164536=CARTESIAN_POINT('Ctrl Pts',(79.4925727328799,-3.83009902499393,
46.2866807712271));
#164537=CARTESIAN_POINT('Ctrl Pts',(79.3951400077755,-4.04255726005623,
46.2989262925733));
#164538=CARTESIAN_POINT('Ctrl Pts',(79.3357666809084,-4.16495683091177,
46.3064762468881));
#164539=CARTESIAN_POINT('Ctrl Pts',(79.0461303983591,-4.7305125978204,46.3437067515372));
#164540=CARTESIAN_POINT('Ctrl Pts',(78.7836260362418,-5.15589905359773,
46.378507326741));
#164541=CARTESIAN_POINT('Ctrl Pts',(78.3503391416087,-5.7471037034835,46.4380273062544));
#164542=CARTESIAN_POINT('Ctrl Pts',(78.2048289431449,-5.93080101249349,
46.4583032428461));
#164543=CARTESIAN_POINT('Ctrl Pts',(77.9577242224753,-6.21983192978189,
46.4933360897385));
#164544=CARTESIAN_POINT('Ctrl Pts',(77.8602194457785,-6.32862361521281,
46.5072978747265));
#164545=CARTESIAN_POINT('Ctrl Pts',(77.7147884479232,-6.48344998692486,
46.5283586161441));
#164546=CARTESIAN_POINT('Ctrl Pts',(77.6688237383768,-6.53135291642249,
46.5350478520553));
#164547=CARTESIAN_POINT('Ctrl Pts',(77.5833344811941,-6.61857131071789,
46.5475539777387));
#164548=CARTESIAN_POINT('Ctrl Pts',(77.5439588808796,-6.65803188752971,
46.5533393458536));
#164549=CARTESIAN_POINT('Ctrl Pts',(77.4439647724282,-6.75646607602563,
46.5680907127401));
#164550=CARTESIAN_POINT('Ctrl Pts',(77.3829017163821,-6.81496634178941,
46.5771523100776));
#164551=CARTESIAN_POINT('Ctrl Pts',(76.9827612931862,-7.18802061279908,
46.636829370977));
#164552=CARTESIAN_POINT('Ctrl Pts',(76.621863103432,-7.47747297852509,46.691984389129));
#164553=CARTESIAN_POINT('Ctrl Pts',(76.0238653105896,-7.88763974300305,
46.7838680296034));
#164554=CARTESIAN_POINT('Ctrl Pts',(75.8003531756628,-8.02728247982002,
46.8183141296595));
#164555=CARTESIAN_POINT('Ctrl Pts',(75.4057300777903,-8.25091992701731,
46.8791042998619));
#164556=CARTESIAN_POINT('Ctrl Pts',(75.2373778417391,-8.33955198849032,
46.9050314609777));
#164557=CARTESIAN_POINT('Ctrl Pts',(74.971038675581,-8.46938769702689,46.9459959166003));
#164558=CARTESIAN_POINT('Ctrl Pts',(74.8748492383376,-8.51423379967115,
46.9607801587711));
#164559=CARTESIAN_POINT('Ctrl Pts',(74.6898802860195,-8.59660126536383,
46.9891849457625));
#164560=CARTESIAN_POINT('Ctrl Pts',(74.601242162031,-8.63441206673753,47.0027860521301));
#164561=CARTESIAN_POINT('Ctrl Pts',(74.3908977116618,-8.72025170403977,
47.0350348832982));
#164562=CARTESIAN_POINT('Ctrl Pts',(74.2687351398084,-8.76708392344454,
47.0537426368055));
#164563=CARTESIAN_POINT('Ctrl Pts',(73.7802318125389,-8.94246891886013,
47.1284664205816));
#164564=CARTESIAN_POINT('Ctrl Pts',(73.4070081890647,-9.0502743437919,47.185351635835));
#164565=CARTESIAN_POINT('Ctrl Pts',(72.7295347816975,-9.20012311448153,
47.288548228622));
#164566=CARTESIAN_POINT('Ctrl Pts',(72.4278142695469,-9.2511627267719,47.3344926473394));
#164567=CARTESIAN_POINT('Ctrl Pts',(71.9561053379196,-9.3068273039169,47.4065836462716));
#164568=CARTESIAN_POINT('Ctrl Pts',(71.7875332798937,-9.32199066335528,
47.4323992417412));
#164569=CARTESIAN_POINT('Ctrl Pts',(71.5009378508252,-9.33976898814924,
47.4764488180039));
#164570=CARTESIAN_POINT('Ctrl Pts',(71.3830950495335,-9.34479204429503,
47.4946069550345));
#164571=CARTESIAN_POINT('Ctrl Pts',(71.2062960018439,-9.34890188244507,
47.5219416570739));
#164572=CARTESIAN_POINT('Ctrl Pts',(71.1473835529261,-9.34970129234971,
47.5310653929794));
#164573=CARTESIAN_POINT('Ctrl Pts',(71.0372041684618,-9.35013038818491,
47.5481613826737));
#164574=CARTESIAN_POINT('Ctrl Pts',(70.9859400938251,-9.34989843344841,
47.5561293785756));
#164575=CARTESIAN_POINT('Ctrl Pts',(70.8572352851513,-9.34823232635641,
47.5761651442588));
#164576=CARTESIAN_POINT('Ctrl Pts',(70.7798078307469,-9.34624452985634,
47.5882464598933));
#164577=CARTESIAN_POINT('Ctrl Pts',(70.4265824055313,-9.33267699071156,
47.6434646626661));
#164578=CARTESIAN_POINT('Ctrl Pts',(70.1513992305808,-9.30957845062919,
47.6867667604192));
#164579=CARTESIAN_POINT('Ctrl Pts',(69.5552741074706,-9.23219685386255,
47.78070296817));
#164580=CARTESIAN_POINT('Ctrl Pts',(69.2353098758472,-9.17315626289746,
47.8312028396341));
#164581=CARTESIAN_POINT('Ctrl Pts',(68.6914417661586,-9.04248125198924,
47.9166948590491));
#164582=CARTESIAN_POINT('Ctrl Pts',(68.4659507437593,-8.97906359452854,
47.9520366574021));
#164583=CARTESIAN_POINT('Ctrl Pts',(68.0722971797605,-8.85188804673559,
48.0134261875915));
#164584=CARTESIAN_POINT('Ctrl Pts',(67.9031476406525,-8.7917073022843,48.039701521345));
#164585=CARTESIAN_POINT('Ctrl Pts',(67.6383975018137,-8.68867583876348,
48.0806327055719));
#164586=CARTESIAN_POINT('Ctrl Pts',(67.5416148222849,-8.64909765606977,
48.0955536874141));
#164587=CARTESIAN_POINT('Ctrl Pts',(67.3564933613383,-8.56968419613098,
48.1240088940103));
#164588=CARTESIAN_POINT('Ctrl Pts',(67.2680699738037,-8.5300882995531,48.1375624498331));
#164589=CARTESIAN_POINT('Ctrl Pts',(67.057995608079,-8.43200938402033,48.1696697315726));
#164590=CARTESIAN_POINT('Ctrl Pts',(66.9369563551146,-8.3722270356035,48.1880930524492));
#164591=CARTESIAN_POINT('Ctrl Pts',(66.3776258395292,-8.08052596957712,
48.2728779269175));
#164592=CARTESIAN_POINT('Ctrl Pts',(65.9567377333837,-7.81596658190576,
48.335605829491));
#164593=CARTESIAN_POINT('Ctrl Pts',(65.371628127905,-7.37892675267048,48.4218962492074));
#164594=CARTESIAN_POINT('Ctrl Pts',(65.1898013139434,-7.23210630174306,
48.4485757849636));
#164595=CARTESIAN_POINT('Ctrl Pts',(64.9037012765419,-6.98267226715385,
48.4904845583228));
#164596=CARTESIAN_POINT('Ctrl Pts',(64.7960098583973,-6.88422436862999,
48.5062425230424));
#164597=CARTESIAN_POINT('Ctrl Pts',(64.6427519649519,-6.73734563509782,
48.5286833573295));
#164598=CARTESIAN_POINT('Ctrl Pts',(64.5953347097266,-6.69091765915269,
48.5356287162348));
#164599=CARTESIAN_POINT('Ctrl Pts',(64.5090022157491,-6.60455550995061,
48.5482835273164));
#164600=CARTESIAN_POINT('Ctrl Pts',(64.469943170351,-6.5647734948491,48.5540130782587));
#164601=CARTESIAN_POINT('Ctrl Pts',(64.3725118593432,-6.46373697359551,
48.5683125548094));
#164602=CARTESIAN_POINT('Ctrl Pts',(64.3146086920237,-6.40202807269846,
48.5768169785079));
#164603=CARTESIAN_POINT('Ctrl Pts',(63.9453616218992,-5.99760386866832,
48.6310467077339));
#164604=CARTESIAN_POINT('Ctrl Pts',(63.6588563395619,-5.6326109648648,48.6730842491332));
#164605=CARTESIAN_POINT('Ctrl Pts',(63.2526021180041,-5.0277426754259,48.7311583246122));
#164606=CARTESIAN_POINT('Ctrl Pts',(63.114231782687,-4.80164468962441,48.7505916282126));
#164607=CARTESIAN_POINT('Ctrl Pts',(62.8924882798499,-4.40246070115124,
48.7808984613986));
#164608=CARTESIAN_POINT('Ctrl Pts',(62.8045601031759,-4.23216390960435,
48.7926446909488));
#164609=CARTESIAN_POINT('Ctrl Pts',(62.675671116758,-3.96275763081257,48.8093729713809));
#164610=CARTESIAN_POINT('Ctrl Pts',(62.6311341150639,-3.86546227055174,
48.8150494955452));
#164611=CARTESIAN_POINT('Ctrl Pts',(62.5492980045406,-3.67837097274811,
48.8252691799311));
#164612=CARTESIAN_POINT('Ctrl Pts',(62.5117147938965,-3.58871765369472,
48.8298679275782));
#164613=CARTESIAN_POINT('Ctrl Pts',(62.4263514672228,-3.37596885738771,
48.8400792145593));
#164614=CARTESIAN_POINT('Ctrl Pts',(62.3797462964527,-3.2524136421795,48.845464159663));
#164615=CARTESIAN_POINT('Ctrl Pts',(62.2050741348317,-2.75835612839402,
48.8648510415287));
#164616=CARTESIAN_POINT('Ctrl Pts',(62.0973803917991,-2.38092459556769,
48.8749161746551));
#164617=CARTESIAN_POINT('Ctrl Pts',(61.9470274927069,-1.69582362201107,
48.885167199529));
#164618=CARTESIAN_POINT('Ctrl Pts',(61.8955222575518,-1.39070874928956,
48.8869919137234));
#164619=CARTESIAN_POINT('Ctrl Pts',(61.8388078736529,-0.913647662394935,
48.8859081769848));
#164620=CARTESIAN_POINT('Ctrl Pts',(61.8232065378916,-0.743153766970815,
48.8847509069901));
#164621=CARTESIAN_POINT('Ctrl Pts',(61.8045893182642,-0.4532632457609,48.8815486948721));
#164622=CARTESIAN_POINT('Ctrl Pts',(61.7991944029104,-0.334057616577517,
48.8798792357473));
#164623=CARTESIAN_POINT('Ctrl Pts',(61.7944903683467,-0.155197925530483,
48.8768689437948));
#164624=CARTESIAN_POINT('Ctrl Pts',(61.793486926338,-0.0955961694390742,
48.8757817593667));
#164625=CARTESIAN_POINT('Ctrl Pts',(61.7929593826893,-0.0239936871218512,
48.8743771329385));
#164626=CARTESIAN_POINT('Ctrl Pts',(61.7928938540372,-0.0119968230969001,
48.8741384678195));
#164627=CARTESIAN_POINT('Ctrl Pts',(61.7928511881971,-6.81909623538039E-10,
48.8738964978212));
#164628=CARTESIAN_POINT('Ctrl Pts',(61.763385699346,1.76224501330106E-11,
48.7067894065939));
#164629=CARTESIAN_POINT('Ctrl Pts',(61.7635670284536,-0.0509862958350187,
48.7078177750651));
#164630=CARTESIAN_POINT('Ctrl Pts',(61.7641568264916,-0.101971841470106,
48.7087610001154));
#164631=CARTESIAN_POINT('Ctrl Pts',(61.7669122876853,-0.242658808520474,
48.7111328664627));
#164632=CARTESIAN_POINT('Ctrl Pts',(61.7699345808252,-0.332340962945694,
48.7123858331844));
#164633=CARTESIAN_POINT('Ctrl Pts',(61.7950362740921,-0.857011440140505,
48.7182457033326));
#164634=CARTESIAN_POINT('Ctrl Pts',(61.8456440974283,-1.29015662006303,
48.7171819201477));
#164635=CARTESIAN_POINT('Ctrl Pts',(62.0144667619307,-2.19160907988531,
48.7041015590164));
#164636=CARTESIAN_POINT('Ctrl Pts',(62.139015048218,-2.65742979065379,48.6909733641217));
#164637=CARTESIAN_POINT('Ctrl Pts',(62.3429895304684,-3.23839599178517,
48.6670900963039));
#164638=CARTESIAN_POINT('Ctrl Pts',(62.3902242071645,-3.36426539534811,
48.6614426933651));
#164639=CARTESIAN_POINT('Ctrl Pts',(62.4763353451641,-3.57962734167984,
48.6509673174823));
#164640=CARTESIAN_POINT('Ctrl Pts',(62.5139443805906,-3.66961278424621,
48.6463401683691));
#164641=CARTESIAN_POINT('Ctrl Pts',(62.5953356218942,-3.8561660836585,48.6362240593866));
#164642=CARTESIAN_POINT('Ctrl Pts',(62.6393641644619,-3.95260924435909,
48.630695886835));
#164643=CARTESIAN_POINT('Ctrl Pts',(62.7650028927571,-4.21596093714083,
48.614772990969));
#164644=CARTESIAN_POINT('Ctrl Pts',(62.8499254993405,-4.38120253222522,
48.603851809218));
#164645=CARTESIAN_POINT('Ctrl Pts',(63.0615155416433,-4.76456688989362,
48.5762666886725));
#164646=CARTESIAN_POINT('Ctrl Pts',(63.1921565669718,-4.98028422351736,
48.5589593876354));
#164647=CARTESIAN_POINT('Ctrl Pts',(63.5843067069138,-5.57268493641918,
48.5061130236971));
#164648=CARTESIAN_POINT('Ctrl Pts',(63.8648115235453,-5.93563489524881,
48.4673466811831));
#164649=CARTESIAN_POINT('Ctrl Pts',(64.2367528203933,-6.35031862372333,
48.414052315818));
#164650=CARTESIAN_POINT('Ctrl Pts',(64.3042989974593,-6.42325704918564,
48.4043051116645));
#164651=CARTESIAN_POINT('Ctrl Pts',(64.4131880321295,-6.53714812778854,
48.3884704064834));
#164652=CARTESIAN_POINT('Ctrl Pts',(64.4537852915516,-6.57882545251053,
48.3825408498162));
#164653=CARTESIAN_POINT('Ctrl Pts',(64.5377846410195,-6.66346654316011,
48.3702156956732));
#164654=CARTESIAN_POINT('Ctrl Pts',(64.5812233838699,-6.70638843645338,
48.3638122150543));
#164655=CARTESIAN_POINT('Ctrl Pts',(64.707446729401,-6.82868894044251,48.3451278217));
#164656=CARTESIAN_POINT('Ctrl Pts',(64.7912592997073,-6.90695650860338,
48.3326275253081));
#164657=CARTESIAN_POINT('Ctrl Pts',(64.9959118518596,-7.09112224922956,
48.3019229821779));
#164658=CARTESIAN_POINT('Ctrl Pts',(65.1180664558918,-7.1954584903423,48.2834500157771));
#164659=CARTESIAN_POINT('Ctrl Pts',(65.7139136847808,-7.67825396945095,
48.1928635709965));
#164660=CARTESIAN_POINT('Ctrl Pts',(66.2206166288938,-8.0123958941104,48.1145283069838));
#164661=CARTESIAN_POINT('Ctrl Pts',(66.8797595207667,-8.3593594849516,48.0130437236489));
#164662=CARTESIAN_POINT('Ctrl Pts',(67.0050097002923,-8.42168388641225,
47.9937713297349));
#164663=CARTESIAN_POINT('Ctrl Pts',(67.21909549953,-8.52218497524791,47.9608641819839));
#164664=CARTESIAN_POINT('Ctrl Pts',(67.307212638376,-8.56186688076919,47.9473292384465));
#164665=CARTESIAN_POINT('Ctrl Pts',(67.4902443644734,-8.6408420836707,47.91923842343));
#164666=CARTESIAN_POINT('Ctrl Pts',(67.585224166658,-8.67994727941533,47.9046740078978));
#164667=CARTESIAN_POINT('Ctrl Pts',(67.8383058606871,-8.77921231266517,
47.8659014648516));
#164668=CARTESIAN_POINT('Ctrl Pts',(67.9974311542422,-8.83660130820626,
47.8415598974115));
#164669=CARTESIAN_POINT('Ctrl Pts',(68.3617729545538,-8.95672349711548,
47.7859011176601));
#164670=CARTESIAN_POINT('Ctrl Pts',(68.56777483729,-9.01671267829863,47.754484592589));
#164671=CARTESIAN_POINT('Ctrl Pts',(69.1160892795566,-9.15570560998501,
47.6709302037458));
#164672=CARTESIAN_POINT('Ctrl Pts',(69.4611193349979,-9.22233002612046,
47.6184280673959));
#164673=CARTESIAN_POINT('Ctrl Pts',(70.0925386879095,-9.30695659229467,
47.522031437863));
#164674=CARTESIAN_POINT('Ctrl Pts',(70.3776277853248,-9.33163081763205,
47.478389618091));
#164675=CARTESIAN_POINT('Ctrl Pts',(70.7422775623076,-9.34601401622623,
47.4221618743342));
#164676=CARTESIAN_POINT('Ctrl Pts',(70.8212514525622,-9.34810384537796,
47.4099597963782));
#164677=CARTESIAN_POINT('Ctrl Pts',(70.9512328939819,-9.34985700810057,
47.3898282004054));
#164678=CARTESIAN_POINT('Ctrl Pts',(71.0022312937868,-9.3501177631102,47.3819171730687));
#164679=CARTESIAN_POINT('Ctrl Pts',(71.1112515273485,-9.3497621152038,47.3649769000863));
#164680=CARTESIAN_POINT('Ctrl Pts',(71.1692696581125,-9.34901989622982,
47.3559447580405));
#164681=CARTESIAN_POINT('Ctrl Pts',(71.3403040034562,-9.3452012438635,47.3292754815737));
#164682=CARTESIAN_POINT('Ctrl Pts',(71.4532693916326,-9.34057877345878,
47.3116055248515));
#164683=CARTESIAN_POINT('Ctrl Pts',(71.7249238431665,-9.324403991855,47.2690202023061));
#164684=CARTESIAN_POINT('Ctrl Pts',(71.8834513615109,-9.31079879356123,
47.2440923134608));
#164685=CARTESIAN_POINT('Ctrl Pts',(72.6600239590159,-9.22365320535799,
47.1218122500596));
#164686=CARTESIAN_POINT('Ctrl Pts',(73.2699165952279,-9.09117713409731,
47.0253681320263));
#164687=CARTESIAN_POINT('Ctrl Pts',(74.0274098302864,-8.84367639097596,
46.9072902352787));
#164688=CARTESIAN_POINT('Ctrl Pts',(74.1910500952771,-8.78501521042553,
46.8818801140974));
#164689=CARTESIAN_POINT('Ctrl Pts',(74.4493987748614,-8.68404172740784,
46.8419480918929));
#164690=CARTESIAN_POINT('Ctrl Pts',(74.5451932851291,-8.64472338465233,
46.8271827159251));
#164691=CARTESIAN_POINT('Ctrl Pts',(74.7296923696413,-8.56533134070461,
46.7988287875768));
#164692=CARTESIAN_POINT('Ctrl Pts',(74.8184634640849,-8.52545248653272,
46.785224879625));
#164693=CARTESIAN_POINT('Ctrl Pts',(75.0315229739173,-8.4256518730757,46.752668947513));
#164694=CARTESIAN_POINT('Ctrl Pts',(75.1551476013034,-8.36432319250109,
46.733858365037));
#164695=CARTESIAN_POINT('Ctrl Pts',(75.3538259307227,-8.26014287355754,
46.703754929983));
#164696=CARTESIAN_POINT('Ctrl Pts',(75.4297149566855,-8.21898201114749,
46.6922872222443));
#164697=CARTESIAN_POINT('Ctrl Pts',(75.7197956262946,-8.05634289497177,
46.6485674986653));
#164698=CARTESIAN_POINT('Ctrl Pts',(75.9297731803813,-7.92733080760436,
46.6171676408258));
#164699=CARTESIAN_POINT('Ctrl Pts',(76.5331395579719,-7.52257836313178,
46.5275192108297));
#164700=CARTESIAN_POINT('Ctrl Pts',(76.910829075248,-7.22427425532505,46.4721930274057));
#164701=CARTESIAN_POINT('Ctrl Pts',(77.3306039849859,-6.83621273399556,
46.4107438008237));
#164702=CARTESIAN_POINT('Ctrl Pts',(77.3963266071006,-6.77364568569467,
46.401122980671));
#164703=CARTESIAN_POINT('Ctrl Pts',(77.5011914531659,-6.67084555468564,
46.3857610659146));
#164704=CARTESIAN_POINT('Ctrl Pts',(77.5408987154452,-6.63120875084857,
46.3799414558447));
#164705=CARTESIAN_POINT('Ctrl Pts',(77.6247404834355,-6.54598599595001,
46.3676442855158));
#164706=CARTESIAN_POINT('Ctrl Pts',(77.668772809714,-6.50030227635002,46.3611810819779));
#164707=CARTESIAN_POINT('Ctrl Pts',(77.8002191509532,-6.36110420606446,
46.3418807496631));
#164708=CARTESIAN_POINT('Ctrl Pts',(77.8861885412103,-6.26621859480062,
46.3292494346646));
#164709=CARTESIAN_POINT('Ctrl Pts',(78.223761874539,-5.87785118844521,46.2797081354359));
#164710=CARTESIAN_POINT('Ctrl Pts',(78.4591252799246,-5.57045632262373,
46.2453138001229));
#164711=CARTESIAN_POINT('Ctrl Pts',(78.8944465099846,-4.92259419127054,
46.1830797513794));
#164712=CARTESIAN_POINT('Ctrl Pts',(79.0933171348304,-4.58232243093967,
46.1554242711111));
#164713=CARTESIAN_POINT('Ctrl Pts',(79.3271924237105,-4.11775821695195,
46.1244771651663));
#164714=CARTESIAN_POINT('Ctrl Pts',(79.381650120405,-4.00397454892205,46.1174066260347));
#164715=CARTESIAN_POINT('Ctrl Pts',(79.4738352804155,-3.80104638389385,
46.1056971715342));
#164716=CARTESIAN_POINT('Ctrl Pts',(79.5124966460578,-3.7123575962577,46.1008764184885));
#164717=CARTESIAN_POINT('Ctrl Pts',(79.5917481164606,-3.52267927447631,
46.0911956732692));
#164718=CARTESIAN_POINT('Ctrl Pts',(79.6319721350735,-3.42154870577104,
46.0864064186747));
#164719=CARTESIAN_POINT('Ctrl Pts',(79.7412901033082,-3.13230709027199,
46.0737607030887));
#164720=CARTESIAN_POINT('Ctrl Pts',(79.8061896202673,-2.94264012741909,
46.0667158387936));
#164721=CARTESIAN_POINT('Ctrl Pts',(79.9461141263053,-2.48712880831576,
46.0527074105073));
#164722=CARTESIAN_POINT('Ctrl Pts',(80.015654053396,-2.21976353624555,46.0467862408762));
#164723=CARTESIAN_POINT('Ctrl Pts',(80.1704346911762,-1.4966007572829,46.0366590034094));
#164724=CARTESIAN_POINT('Ctrl Pts',(80.2341508866223,-1.03693003125505,
46.0363702166018));
#164725=CARTESIAN_POINT('Ctrl Pts',(80.271659316106,-0.45496640189662,46.0427778767813));
#164726=CARTESIAN_POINT('Ctrl Pts',(80.2770938096886,-0.335299111565848,
46.0444509800905));
#164727=CARTESIAN_POINT('Ctrl Pts',(80.2818270006704,-0.155893663000213,
46.047468251547));
#164728=CARTESIAN_POINT('Ctrl Pts',(80.2828359808091,-0.0962084642501501,
46.048556351027));
#164729=CARTESIAN_POINT('Ctrl Pts',(80.2836639423684,0.0153215143246354,
46.05074332773));
#164730=CARTESIAN_POINT('Ctrl Pts',(80.2836218605704,0.067162709768048,
46.0518215192948));
#164731=CARTESIAN_POINT('Ctrl Pts',(80.2824460247315,0.197179514697998,
46.0546831336917));
#164732=CARTESIAN_POINT('Ctrl Pts',(80.2807684439539,0.275344499674537,
46.0565466762966));
#164733=CARTESIAN_POINT('Ctrl Pts',(80.2682167320729,0.645856198461007,
46.0660841262589));
#164734=CARTESIAN_POINT('Ctrl Pts',(80.2447462441237,0.937560895303463,
46.0756764433261));
#164735=CARTESIAN_POINT('Ctrl Pts',(80.1289917176439,1.8471016411204,46.1129169547145));
#164736=CARTESIAN_POINT('Ctrl Pts',(79.9891427673429,2.4567852965578,46.1487001419168));
#164737=CARTESIAN_POINT('Ctrl Pts',(79.7447561823636,3.1841200718594,46.2067990040271));
#164738=CARTESIAN_POINT('Ctrl Pts',(79.6957665761307,3.31957855970959,46.2183036590978));
#164739=CARTESIAN_POINT('Ctrl Pts',(79.6083575315831,3.54500672234546,46.2386209024404));
#164740=CARTESIAN_POINT('Ctrl Pts',(79.5715921601552,3.63561892100403,46.2471122455683));
#164741=CARTESIAN_POINT('Ctrl Pts',(79.4934890357583,3.81983480190213,46.2650465287439));
#164742=CARTESIAN_POINT('Ctrl Pts',(79.452023179409,3.91336737654442,46.2745141836652));
#164743=CARTESIAN_POINT('Ctrl Pts',(79.3395131363372,4.15638208589489,46.3000677296836));
#164744=CARTESIAN_POINT('Ctrl Pts',(79.2660535538036,4.30465598284,46.3166219564862));
#164745=CARTESIAN_POINT('Ctrl Pts',(79.0899349566932,4.63772012676089,46.3560171971819));
#164746=CARTESIAN_POINT('Ctrl Pts',(78.9848908265478,4.82109118340806,46.3793148004863));
#164747=CARTESIAN_POINT('Ctrl Pts',(78.6998728894683,5.28173156896326,46.4419682649492));
#164748=CARTESIAN_POINT('Ctrl Pts',(78.511324158854,5.55312666615649,46.4829148477562));
#164749=CARTESIAN_POINT('Ctrl Pts',(78.1620088578202,6.0027713619865,46.5576018043202));
#164750=CARTESIAN_POINT('Ctrl Pts',(78.0079285758451,6.18599058892275,46.5902093544676));
#164751=CARTESIAN_POINT('Ctrl Pts',(77.7936558180712,6.42156307501393,46.6349717577744));
#164752=CARTESIAN_POINT('Ctrl Pts',(77.7395648308506,6.47951189241012,46.6462252570751));
#164753=CARTESIAN_POINT('Ctrl Pts',(77.6467453452615,6.57641319025066,46.6654505844092));
#164754=CARTESIAN_POINT('Ctrl Pts',(77.6083987518249,6.61573549341447,46.6733688934481));
#164755=CARTESIAN_POINT('Ctrl Pts',(77.5211511102418,6.70361501719139,46.6913294666023));
#164756=CARTESIAN_POINT('Ctrl Pts',(77.4720552892529,6.75196734058799,46.7013986614867));
#164757=CARTESIAN_POINT('Ctrl Pts',(77.303415959847,6.9143611577255,46.7358721502811));
#164758=CARTESIAN_POINT('Ctrl Pts',(77.1813821199958,7.02569437679335,46.7606292502846));
#164759=CARTESIAN_POINT('Ctrl Pts',(76.8360214369066,7.32412590745934,46.8303198927398));
#164760=CARTESIAN_POINT('Ctrl Pts',(76.606798350837,7.5038831615887,46.8761682380887));
#164761=CARTESIAN_POINT('Ctrl Pts',(76.0463337726893,7.90184595470696,46.9878920041969));
#164762=CARTESIAN_POINT('Ctrl Pts',(75.7088465631406,8.10991443379385,47.0548913170773));
#164763=CARTESIAN_POINT('Ctrl Pts',(75.2367218954305,8.36020400012083,47.1487793658631));
#164764=CARTESIAN_POINT('Ctrl Pts',(75.1127163161697,8.42235767890001,47.1734512387016));
#164765=CARTESIAN_POINT('Ctrl Pts',(74.9006151022461,8.52266886312546,47.2156850673618));
#164766=CARTESIAN_POINT('Ctrl Pts',(74.8132228671696,8.56231946092364,47.2330963292774));
#164767=CARTESIAN_POINT('Ctrl Pts',(74.6315707577106,8.64129160482401,47.2693104563464));
#164768=CARTESIAN_POINT('Ctrl Pts',(74.5372448790734,8.68042064155764,47.2881279924881));
#164769=CARTESIAN_POINT('Ctrl Pts',(74.2855688325895,8.77987820004276,47.3383720629451));
#164770=CARTESIAN_POINT('Ctrl Pts',(74.1272027197919,8.83741098068447,47.3700251659421));
#164771=CARTESIAN_POINT('Ctrl Pts',(73.6842697534294,8.98447133026994,47.4586482778382));
#164772=CARTESIAN_POINT('Ctrl Pts',(73.3968578410585,9.06435450313553,47.5162634325406));
#164773=CARTESIAN_POINT('Ctrl Pts',(72.588628063085,9.24642150572165,47.6783341370818));
#164774=CARTESIAN_POINT('Ctrl Pts',(72.0621839683428,9.31703470328471,47.7839968533797));
#164775=CARTESIAN_POINT('Ctrl Pts',(71.4462111432439,9.34477529788262,47.9064224007076));
#164776=CARTESIAN_POINT('Ctrl Pts',(71.3598304288511,9.34741946180787,47.9235617906978));
#164777=CARTESIAN_POINT('Ctrl Pts',(71.2260315324177,9.34958686887705,47.95005489349));
#164778=CARTESIAN_POINT('Ctrl Pts',(71.1786365410979,9.34998023070964,47.9594287712936));
#164779=CARTESIAN_POINT('Ctrl Pts',(71.077870729738,9.35002071453647,47.9793334044545));
#164780=CARTESIAN_POINT('Ctrl Pts',(71.0245010799648,9.34956760886984,47.9898607001912));
#164781=CARTESIAN_POINT('Ctrl Pts',(70.880606384687,9.34706638420263,48.0182088608707));
#164782=CARTESIAN_POINT('Ctrl Pts',(70.7900975252442,9.34412735863316,48.0360018900547));
#164783=CARTESIAN_POINT('Ctrl Pts',(70.3982657166123,9.32548577265104,48.1129063480163));
#164784=CARTESIAN_POINT('Ctrl Pts',(70.0977095135343,9.29601287225383,48.1715796033842));
#164785=CARTESIAN_POINT('Ctrl Pts',(69.2142188657888,9.16433907346765,48.3439768441029));
#164786=CARTESIAN_POINT('Ctrl Pts',(68.6389457528607,9.01980846731191,48.4562179985451));
#164787=CARTESIAN_POINT('Ctrl Pts',(67.9559191568667,8.77488452073174,48.5911161960689));
#164788=CARTESIAN_POINT('Ctrl Pts',(67.8312720941397,8.72705065872341,48.6157987874264));
#164789=CARTESIAN_POINT('Ctrl Pts',(67.6186834530462,8.64002832520788,48.6580182804227));
#164790=CARTESIAN_POINT('Ctrl Pts',(67.5302361831385,8.60216721727257,48.675620924733));
#164791=CARTESIAN_POINT('Ctrl Pts',(67.3474664984434,8.52046298533827,48.7120758426276));
#164792=CARTESIAN_POINT('Ctrl Pts',(67.2532590537562,8.47638961103273,48.7309117291574));
#164793=CARTESIAN_POINT('Ctrl Pts',(66.9977112251717,8.35143644758021,48.7821316084636));
#164794=CARTESIAN_POINT('Ctrl Pts',(66.8379561619777,8.26733248382455,48.8142914856332));
#164795=CARTESIAN_POINT('Ctrl Pts',(66.4690842617132,8.05887909828604,48.888860198392));
#164796=CARTESIAN_POINT('Ctrl Pts',(66.2621865760908,7.93076334932215,48.9309316614686));
#164797=CARTESIAN_POINT('Ctrl Pts',(65.6619146421346,7.52498492960308,49.0535781095235));
#164798=CARTESIAN_POINT('Ctrl Pts',(65.2847154445787,7.22410189965589,49.1314630440248));
#164799=CARTESIAN_POINT('Ctrl Pts',(64.866939956944,6.83349025458365,49.2177660955589));
#164800=CARTESIAN_POINT('Ctrl Pts',(64.8024995487228,6.7714617167852,49.2310779803241));
#164801=CARTESIAN_POINT('Ctrl Pts',(64.6993994913589,6.66929862117474,49.2523647504695));
#164802=CARTESIAN_POINT('Ctrl Pts',(64.6601965021077,6.62974462839217,49.2604560330086));
#164803=CARTESIAN_POINT('Ctrl Pts',(64.5771015214369,6.5443800044087,49.2775972288615));
#164804=CARTESIAN_POINT('Ctrl Pts',(64.533316503704,6.49846556657053,49.2866243942788));
#164805=CARTESIAN_POINT('Ctrl Pts',(64.4018221984846,6.3577113626466,49.3137283439525));
#164806=CARTESIAN_POINT('Ctrl Pts',(64.3155898362575,6.26145426016034,49.3314942582238));
#164807=CARTESIAN_POINT('Ctrl Pts',(63.9788741076746,5.86942007725401,49.4009272629691));
#164808=CARTESIAN_POINT('Ctrl Pts',(63.7447236835192,5.55957819783879,49.4493659168226));
#164809=CARTESIAN_POINT('Ctrl Pts',(63.3171227674431,4.91342939294318,49.5392371581422));
#164810=CARTESIAN_POINT('Ctrl Pts',(63.1238939789041,4.57790060375784,49.5806184944906));
#164811=CARTESIAN_POINT('Ctrl Pts',(62.8959726140578,4.11833577497276,49.6309876735791));
#164812=CARTESIAN_POINT('Ctrl Pts',(62.842333499432,4.00447026933959,49.6429792921954));
#164813=CARTESIAN_POINT('Ctrl Pts',(62.7516504306612,3.80145085382702,49.6635164143211));
#164814=CARTESIAN_POINT('Ctrl Pts',(62.7136635844201,3.71275418739621,49.672210954206));
#164815=CARTESIAN_POINT('Ctrl Pts',(62.6358873208469,3.52311655419153,49.6902174456147));
#164816=CARTESIAN_POINT('Ctrl Pts',(62.5964641786824,3.42203534210194,49.6994709655434));
#164817=CARTESIAN_POINT('Ctrl Pts',(62.489517734195,3.13312860802896,49.7249506785699));
#164818=CARTESIAN_POINT('Ctrl Pts',(62.426197133163,2.94375289465577,49.7405075524241));
#164819=CARTESIAN_POINT('Ctrl Pts',(62.2901216825293,2.48917447324313,49.7751430550551));
#164820=CARTESIAN_POINT('Ctrl Pts',(62.2228407528162,2.22246015261924,49.7933312560388));
#164821=CARTESIAN_POINT('Ctrl Pts',(62.0743447524768,1.5026287611099,49.8366007825257));
#164822=CARTESIAN_POINT('Ctrl Pts',(62.0143626435984,1.04569009449929,49.8580589365739));
#164823=CARTESIAN_POINT('Ctrl Pts',(61.9806176086439,0.463993601198438,
49.8770388888381));
#164824=CARTESIAN_POINT('Ctrl Pts',(61.9758895286163,0.341859245624509,
49.880560727444));
#164825=CARTESIAN_POINT('Ctrl Pts',(61.9723400736211,0.159540919171869,
49.8851031453375));
#164826=CARTESIAN_POINT('Ctrl Pts',(61.9717382329125,0.0994134776165123,
49.8864852986239));
#164827=CARTESIAN_POINT('Ctrl Pts',(61.971697316922,0.0261879178999035,
49.8880248982242));
#164828=CARTESIAN_POINT('Ctrl Pts',(61.9717169449031,0.013093935805121,
49.8882946119736));
#164829=CARTESIAN_POINT('Ctrl Pts',(61.9717635125435,8.13085086909029E-10,
49.8885587101925));
#164830=CARTESIAN_POINT('Origin',(73.0915550886457,-4.33680868994202E-16,
59.1075264962884));
#164831=CARTESIAN_POINT('',(82.3304102850288,-3.3346522467903E-11,56.7953584157516));
#164832=CARTESIAN_POINT('',(82.3383045685277,3.32536544680013E-11,56.8401291222381));
#164833=CARTESIAN_POINT('',(82.4472287422617,-1.59709532818419E-15,57.4578688084528));
#164834=CARTESIAN_POINT('',(64.0263520775732,-2.56296981511824,60.375952723877));
#164835=CARTESIAN_POINT('Ctrl Pts',(82.3304102850288,-6.66914478404779E-11,
56.7953584157516));
#164836=CARTESIAN_POINT('Ctrl Pts',(82.3304361494038,0.0136416783697664,
56.7955050999108));
#164837=CARTESIAN_POINT('Ctrl Pts',(82.3304329016124,0.0272833261406265,
56.7956558928931));
#164838=CARTESIAN_POINT('Ctrl Pts',(82.3303332321314,0.0693062246595365,
56.7961331583724));
#164839=CARTESIAN_POINT('Ctrl Pts',(82.3301399285843,0.0976868818918377,
56.796473400641));
#164840=CARTESIAN_POINT('Ctrl Pts',(82.3291325800309,0.187235805179669,
56.797604330781));
#164841=CARTESIAN_POINT('Ctrl Pts',(82.3278593968084,0.248396495000157,
56.7984612196501));
#164842=CARTESIAN_POINT('Ctrl Pts',(82.3181493776529,0.56799719273704,56.803394263009));
#164843=CARTESIAN_POINT('Ctrl Pts',(82.2998583057858,0.826005740413701,
56.8089357541939));
#164844=CARTESIAN_POINT('Ctrl Pts',(82.2031651117969,1.69300374792058,56.8334372425269));
#164845=CARTESIAN_POINT('Ctrl Pts',(82.0769427770516,2.29486224576347,56.8604095822293));
#164846=CARTESIAN_POINT('Ctrl Pts',(81.8356818752499,3.06905569972808,56.9105339377435));
#164847=CARTESIAN_POINT('Ctrl Pts',(81.7709902057922,3.25611438548073,56.9238851129339));
#164848=CARTESIAN_POINT('Ctrl Pts',(81.6762616274636,3.50488392340241,56.9433545301387));
#164849=CARTESIAN_POINT('Ctrl Pts',(81.6512449214178,3.56852828973571,56.9484894233616));
#164850=CARTESIAN_POINT('Ctrl Pts',(81.6088238179609,3.67315344280506,56.957186510578));
#164851=CARTESIAN_POINT('Ctrl Pts',(81.5918081416092,3.7142953613545,56.9606724714772));
#164852=CARTESIAN_POINT('Ctrl Pts',(81.5579566751273,3.79455773772598,56.9676027154383));
#164853=CARTESIAN_POINT('Ctrl Pts',(81.5411453064278,3.83368776072029,56.9710422037177));
#164854=CARTESIAN_POINT('Ctrl Pts',(81.5005809897616,3.92639702160487,56.9793361941018));
#164855=CARTESIAN_POINT('Ctrl Pts',(81.4765977448985,3.97986950870148,56.9842358674312));
#164856=CARTESIAN_POINT('Ctrl Pts',(81.3927236818395,4.16237034545123,57.001356961738));
#164857=CARTESIAN_POINT('Ctrl Pts',(81.3304666362066,4.29024605885254,57.0140421095172));
#164858=CARTESIAN_POINT('Ctrl Pts',(81.1698559134361,4.60226073224271,57.0467004299358));
#164859=CARTESIAN_POINT('Ctrl Pts',(81.0683017501658,4.78460127400127,57.0672953529085));
#164860=CARTESIAN_POINT('Ctrl Pts',(80.8119075485792,5.21136267709586,57.1190883190135));
#164861=CARTESIAN_POINT('Ctrl Pts',(80.6517985477197,5.45225106828773,57.1512790088409));
#164862=CARTESIAN_POINT('Ctrl Pts',(80.2803543201951,5.95917071584238,57.2253168712518));
#164863=CARTESIAN_POINT('Ctrl Pts',(80.0652284539025,6.22183124387477,57.2678150177474));
#164864=CARTESIAN_POINT('Ctrl Pts',(79.7910851622844,6.52186675418303,57.32110834585));
#164865=CARTESIAN_POINT('Ctrl Pts',(79.7450868029703,6.57113337166121,57.3300232694491));
#164866=CARTESIAN_POINT('Ctrl Pts',(79.6776116524779,6.64185875188562,57.3430568631205));
#164867=CARTESIAN_POINT('Ctrl Pts',(79.6565501373063,6.66372117959855,57.3471190818423));
#164868=CARTESIAN_POINT('Ctrl Pts',(79.6190475064207,6.70227325175643,57.3543411398114));
#164869=CARTESIAN_POINT('Ctrl Pts',(79.6026488522168,6.71900476719854,57.3574953250551));
#164870=CARTESIAN_POINT('Ctrl Pts',(79.5668198937393,6.75528768582968,57.3643784980096));
#164871=CARTESIAN_POINT('Ctrl Pts',(79.5473661473527,6.77481474216961,57.3681105873054));
#164872=CARTESIAN_POINT('Ctrl Pts',(79.4913568429418,6.8305409954225,57.3788415117707));
#164873=CARTESIAN_POINT('Ctrl Pts',(79.4545915323723,6.86652253971348,57.3858683370367));
#164874=CARTESIAN_POINT('Ctrl Pts',(79.1320123415624,7.17706352077828,57.4473881700254));
#164875=CARTESIAN_POINT('Ctrl Pts',(78.8295625835376,7.4333033625233,57.504180328059));
#164876=CARTESIAN_POINT('Ctrl Pts',(78.0897705792893,7.98344927222312,57.6426411375825));
#164877=CARTESIAN_POINT('Ctrl Pts',(77.6421906136065,8.26086009995398,57.7261220861622));
#164878=CARTESIAN_POINT('Ctrl Pts',(77.0952892025317,8.53880775881918,57.8288291045846));
#164879=CARTESIAN_POINT('Ctrl Pts',(77.0157871421151,8.57779082465693,57.8437738246327));
#164880=CARTESIAN_POINT('Ctrl Pts',(76.8876775618437,8.63834843166178,57.8678814549624));
#164881=CARTESIAN_POINT('Ctrl Pts',(76.8394099992647,8.66065846833518,57.8769701791974));
#164882=CARTESIAN_POINT('Ctrl Pts',(76.753133545694,8.69963913021958,57.8932265835412));
#164883=CARTESIAN_POINT('Ctrl Pts',(76.7151970925453,8.71647313777519,57.9003782859248));
#164884=CARTESIAN_POINT('Ctrl Pts',(76.6354165165366,8.7512351300743,57.9154261194031));
#164885=CARTESIAN_POINT('Ctrl Pts',(76.5935514800197,8.76911030138037,57.9233269469683));
#164886=CARTESIAN_POINT('Ctrl Pts',(76.482689803225,8.81548107329893,57.9442607664512));
#164887=CARTESIAN_POINT('Ctrl Pts',(76.4134848353773,8.84344856394623,57.9573406795673));
#164888=CARTESIAN_POINT('Ctrl Pts',(76.0683221564028,8.97809932576191,58.0226366693852));
#164889=CARTESIAN_POINT('Ctrl Pts',(75.7878639833882,9.07226092402586,58.0758864692123));
#164890=CARTESIAN_POINT('Ctrl Pts',(75.1696910987616,9.24722340595707,58.1935417090461));
#164891=CARTESIAN_POINT('Ctrl Pts',(74.8309858927555,9.32271167789953,58.2581874850533));
#164892=CARTESIAN_POINT('Ctrl Pts',(74.1085416052176,9.44129043426658,58.395918866406));
#164893=CARTESIAN_POINT('Ctrl Pts',(73.72469710605,9.47968808535207,58.4690073968196));
#164894=CARTESIAN_POINT('Ctrl Pts',(73.2721228765592,9.49629949493761,58.5544269878978));
#164895=CARTESIAN_POINT('Ctrl Pts',(73.2047059216205,9.49802993182143,58.5671312946173));
#164896=CARTESIAN_POINT('Ctrl Pts',(73.1109590975419,9.49940219306647,58.5847645326172));
#164897=CARTESIAN_POINT('Ctrl Pts',(73.0846438274134,9.49967417410826,58.5897106939471));
#164898=CARTESIAN_POINT('Ctrl Pts',(73.0366422277101,9.4999637943183,58.5987260355958));
#164899=CARTESIAN_POINT('Ctrl Pts',(73.0149564637516,9.50001777310221,58.6027963254881));
#164900=CARTESIAN_POINT('Ctrl Pts',(72.9698124696333,9.49997013946072,58.6112639834575));
#164901=CARTESIAN_POINT('Ctrl Pts',(72.9463544361966,9.49985545870626,58.6156608886584));
#164902=CARTESIAN_POINT('Ctrl Pts',(72.8843071099303,9.49931425884716,58.6272830451364));
#164903=CARTESIAN_POINT('Ctrl Pts',(72.8457186540859,9.49873431091007,58.634503100477));
#164904=CARTESIAN_POINT('Ctrl Pts',(72.6637228623521,9.49485114654243,58.6685209405539));
#164905=CARTESIAN_POINT('Ctrl Pts',(72.5203824559727,9.48843043595795,58.6952132140827));
#164906=CARTESIAN_POINT('Ctrl Pts',(72.088324422784,9.45892269382461,58.775473376981));
#164907=CARTESIAN_POINT('Ctrl Pts',(71.8004277725095,9.42553847742185,58.8286929365271));
#164908=CARTESIAN_POINT('Ctrl Pts',(70.9294339256922,9.28257215559893,58.9896690517043));
#164909=CARTESIAN_POINT('Ctrl Pts',(70.3546630487159,9.1301344367234,59.0959441166322));
#164910=CARTESIAN_POINT('Ctrl Pts',(69.7026687788365,8.88786067093953,59.2179772337934));
#164911=CARTESIAN_POINT('Ctrl Pts',(69.6077254164951,8.85077925764338,59.2357827832967));
#164912=CARTESIAN_POINT('Ctrl Pts',(69.4654057904454,8.79245932474628,59.2625293803556));
#164913=CARTESIAN_POINT('Ctrl Pts',(69.4175719163595,8.77238542969545,59.2715286399817));
#164914=CARTESIAN_POINT('Ctrl Pts',(69.3320019318184,8.73562417644508,59.2876450707456));
#164915=CARTESIAN_POINT('Ctrl Pts',(69.2942049269219,8.71908556271438,59.2947700795849));
#164916=CARTESIAN_POINT('Ctrl Pts',(69.2138103170834,8.68326417066188,59.3099384454211));
#164917=CARTESIAN_POINT('Ctrl Pts',(69.1712450524896,8.66390982151452,59.3179774919062));
#164918=CARTESIAN_POINT('Ctrl Pts',(69.0558598267407,8.61038392558845,59.3397916328093));
#164919=CARTESIAN_POINT('Ctrl Pts',(68.9833300901668,8.57558076856505,59.3535278008311));
#164920=CARTESIAN_POINT('Ctrl Pts',(68.5016419032388,8.33666294959657,59.4449115638139));
#164921=CARTESIAN_POINT('Ctrl Pts',(68.1073425803984,8.10324525509951,59.5205274318316));
#164922=CARTESIAN_POINT('Ctrl Pts',(67.3394430470525,7.56843792402817,59.668707780197));
#164923=CARTESIAN_POINT('Ctrl Pts',(66.9685695399479,7.26534081608214,59.7407822468252));
#164924=CARTESIAN_POINT('Ctrl Pts',(66.5776529437535,6.89261966482319,59.8162633882389));
#164925=CARTESIAN_POINT('Ctrl Pts',(66.5338127155536,6.84999734922753,59.8247202492948));
#164926=CARTESIAN_POINT('Ctrl Pts',(66.4694231049319,6.78616625869486,59.8371252345835));
#164927=CARTESIAN_POINT('Ctrl Pts',(66.4485602686789,6.7652893266537,59.8411420452457));
#164928=CARTESIAN_POINT('Ctrl Pts',(66.4113734985588,6.72772661838726,59.848296722624));
#164929=CARTESIAN_POINT('Ctrl Pts',(66.3950137437656,6.71107843117556,59.851442508499));
#164930=CARTESIAN_POINT('Ctrl Pts',(66.3587260892882,6.67387605473532,59.858416132229));
#164931=CARTESIAN_POINT('Ctrl Pts',(66.3388291033348,6.65329108414286,59.8622371672081));
#164932=CARTESIAN_POINT('Ctrl Pts',(66.2798530486098,6.59171792780605,59.8735557732884));
#164933=CARTESIAN_POINT('Ctrl Pts',(66.2410432714808,6.55046284603278,59.8809945845597));
#164934=CARTESIAN_POINT('Ctrl Pts',(66.1517045392773,6.45376725075649,59.898101171084));
#164935=CARTESIAN_POINT('Ctrl Pts',(66.1014546419472,6.39806376855125,59.9077098654265));
#164936=CARTESIAN_POINT('Ctrl Pts',(65.9269553932567,6.19993432325553,59.9410474258483));
#164937=CARTESIAN_POINT('Ctrl Pts',(65.8062572280701,6.0543205221251,59.9640525752478));
#164938=CARTESIAN_POINT('Ctrl Pts',(65.2845398860281,5.385053608281,60.0635606843777));
#164939=CARTESIAN_POINT('Ctrl Pts',(64.9338534711927,4.82315064312234,60.1307897232555));
#164940=CARTESIAN_POINT('Ctrl Pts',(64.6062546085833,4.15128264631376,60.1961459212992));
#164941=CARTESIAN_POINT('Ctrl Pts',(64.5695833887254,4.07341224577026,60.2035053404558));
#164942=CARTESIAN_POINT('Ctrl Pts',(64.5118915531841,3.94646975045704,60.2151582713883));
#164943=CARTESIAN_POINT('Ctrl Pts',(64.4902225432207,3.89770722079457,60.2195533944051));
#164944=CARTESIAN_POINT('Ctrl Pts',(64.4523015675538,3.81040424880979,60.2272785808646));
#164945=CARTESIAN_POINT('Ctrl Pts',(64.435892377755,3.77193584703927,60.2306332448688));
#164946=CARTESIAN_POINT('Ctrl Pts',(64.4016743780867,3.69023283095837,60.2376542853273));
#164947=CARTESIAN_POINT('Ctrl Pts',(64.3839290387559,3.6469719951683,60.2413107011729));
#164948=CARTESIAN_POINT('Ctrl Pts',(64.3371378072118,3.53046917569309,60.2509940480175));
#164949=CARTESIAN_POINT('Ctrl Pts',(64.3086771423989,3.45698858947454,60.2569292079204));
#164950=CARTESIAN_POINT('Ctrl Pts',(64.1578442276479,3.05277718437291,60.2886391438428));
#164951=CARTESIAN_POINT('Ctrl Pts',(64.0528856605776,2.71563461648298,60.3116835047421));
#164952=CARTESIAN_POINT('Ctrl Pts',(63.8903311078625,2.06981831953089,60.3493259349052));
#164953=CARTESIAN_POINT('Ctrl Pts',(63.8288103430972,1.76265196805594,60.3645597711951));
#164954=CARTESIAN_POINT('Ctrl Pts',(63.7272171137977,1.08540318133264,60.3919795022382));
#164955=CARTESIAN_POINT('Ctrl Pts',(63.6933763552644,0.71485472970121,60.4030443918243));
#164956=CARTESIAN_POINT('Ctrl Pts',(63.6786693728875,0.276017243088358,
60.4109924405149));
#164957=CARTESIAN_POINT('Ctrl Pts',(63.6771170195282,0.208815160069549,
60.4120669629704));
#164958=CARTESIAN_POINT('Ctrl Pts',(63.6759158954637,0.11423774835206,60.4133741165184));
#164959=CARTESIAN_POINT('Ctrl Pts',(63.6756841947258,0.0868734877545023,
60.4137281666744));
#164960=CARTESIAN_POINT('Ctrl Pts',(63.675474176648,0.0372991303843346,
60.4143254323333));
#164961=CARTESIAN_POINT('Ctrl Pts',(63.6754563435343,0.0150894428150445,
60.4145769581556));
#164962=CARTESIAN_POINT('Ctrl Pts',(63.6755767889806,-0.0307133606495606,
60.4150623408448));
#164963=CARTESIAN_POINT('Ctrl Pts',(63.6757248626156,-0.054306235738305,
60.4152941428821));
#164964=CARTESIAN_POINT('Ctrl Pts',(63.6763363450625,-0.115922537478582,
60.4158523503208));
#164965=CARTESIAN_POINT('Ctrl Pts',(63.676937235388,-0.153944434876264,
60.4161498820628));
#164966=CARTESIAN_POINT('Ctrl Pts',(63.6806354159257,-0.324465369262825,
60.4172766147717));
#164967=CARTESIAN_POINT('Ctrl Pts',(63.6862250977111,-0.456898873532166,
60.4175894071281));
#164968=CARTESIAN_POINT('Ctrl Pts',(63.7102807695795,-0.839965672217378,
60.4169396754294));
#164969=CARTESIAN_POINT('Ctrl Pts',(63.7357871571807,-1.09004065012715,
60.4145855794763));
#164970=CARTESIAN_POINT('Ctrl Pts',(63.8295460682105,-1.7520747728875,60.4036167386114));
#164971=CARTESIAN_POINT('Ctrl Pts',(63.9148127385724,-2.16101571447035,
60.3919202724443));
#164972=CARTESIAN_POINT('Ctrl Pts',(64.0263520775732,-2.56296981511824,
60.3759527238769));
#164973=CARTESIAN_POINT('',(64.0263520775731,2.56296981511791,60.375952723877));
#164974=CARTESIAN_POINT('Origin',(73.035119430904,-4.33680868994202E-16,
58.7874639765594));
#164975=CARTESIAN_POINT('Ctrl Pts',(64.0263520775731,2.56296981511784,60.375952723877));
#164976=CARTESIAN_POINT('Ctrl Pts',(64.1026158838864,2.84095531252864,60.3599465983121));
#164977=CARTESIAN_POINT('Ctrl Pts',(64.1912865984287,3.11523407478812,60.3415890269741));
#164978=CARTESIAN_POINT('Ctrl Pts',(64.3121166968048,3.43859313024599,60.316734836422));
#164979=CARTESIAN_POINT('Ctrl Pts',(64.3326292944016,3.49202629145127,60.3125204147557));
#164980=CARTESIAN_POINT('Ctrl Pts',(64.3691319167927,3.58462893357413,60.3050286346985));
#164981=CARTESIAN_POINT('Ctrl Pts',(64.384906673452,3.62388487384467,60.301793453566));
#164982=CARTESIAN_POINT('Ctrl Pts',(64.4171374354681,3.7025840307606,60.2951880246446));
#164983=CARTESIAN_POINT('Ctrl Pts',(64.4335984321683,3.7420240586799,60.2918168012444));
#164984=CARTESIAN_POINT('Ctrl Pts',(64.465605139931,3.81729204540382,60.2852661135502));
#164985=CARTESIAN_POINT('Ctrl Pts',(64.4811075118149,3.85313821728493,60.2820951550674));
#164986=CARTESIAN_POINT('Ctrl Pts',(64.5180810162231,3.93721827309926,60.2745366457046));
#164987=CARTESIAN_POINT('Ctrl Pts',(64.5397313429847,3.98536875392491,60.2701139508762));
#164988=CARTESIAN_POINT('Ctrl Pts',(64.6170383069826,4.15356906086304,60.2543334243197));
#164989=CARTESIAN_POINT('Ctrl Pts',(64.6747690233333,4.27261015339433,60.2425691636302));
#164990=CARTESIAN_POINT('Ctrl Pts',(64.8752502372591,4.66505394318771,60.2017924666812));
#164991=CARTESIAN_POINT('Ctrl Pts',(65.0286720176914,4.93256295969039,60.170701227291));
#164992=CARTESIAN_POINT('Ctrl Pts',(65.3784084299162,5.47906277106085,60.1002996592275));
#164993=CARTESIAN_POINT('Ctrl Pts',(65.5772991147117,5.75582346692115,60.060516620384));
#164994=CARTESIAN_POINT('Ctrl Pts',(65.8887249983978,6.14316301175874,59.9989998770026));
#164995=CARTESIAN_POINT('Ctrl Pts',(65.9899248847189,6.26279640139174,59.9791166211805));
#164996=CARTESIAN_POINT('Ctrl Pts',(66.1381820222008,6.42943037394125,59.9501891836551));
#164997=CARTESIAN_POINT('Ctrl Pts',(66.1828536172576,6.47857968011895,59.9414977986718));
#164998=CARTESIAN_POINT('Ctrl Pts',(66.2631268857357,6.56503777276278,59.925928732616));
#164999=CARTESIAN_POINT('Ctrl Pts',(66.2985243072835,6.60253766253368,59.9190798382392));
#165000=CARTESIAN_POINT('Ctrl Pts',(66.3533293691965,6.65964668342931,59.9085032102241));
#165001=CARTESIAN_POINT('Ctrl Pts',(66.3725199751832,6.67946812316823,59.9048047474849));
#165002=CARTESIAN_POINT('Ctrl Pts',(66.4081653352504,6.71596130276197,59.8979448358174));
#165003=CARTESIAN_POINT('Ctrl Pts',(66.4245957785227,6.73265679668973,59.894786645205));
#165004=CARTESIAN_POINT('Ctrl Pts',(66.4624375953624,6.77082165504112,59.8875214566757));
#165005=CARTESIAN_POINT('Ctrl Pts',(66.4838903579724,6.79224843342116,59.8834089948238));
#165006=CARTESIAN_POINT('Ctrl Pts',(66.5532233701834,6.86082823973365,59.8701367858147));
#165007=CARTESIAN_POINT('Ctrl Pts',(66.6015020342976,6.90756507122268,59.860923554787));
#165008=CARTESIAN_POINT('Ctrl Pts',(66.8922111241,7.18299217579198,59.8055936149524));
#165009=CARTESIAN_POINT('Ctrl Pts',(67.146045879201,7.3989718977528,59.7578766294237));
#165010=CARTESIAN_POINT('Ctrl Pts',(67.6347841056327,7.771770203166,59.6663354173845));
#165011=CARTESIAN_POINT('Ctrl Pts',(67.8664016884145,7.93239585626526,59.6230783364539));
#165012=CARTESIAN_POINT('Ctrl Pts',(68.2859011575263,8.19602138949855,59.544641764477));
#165013=CARTESIAN_POINT('Ctrl Pts',(68.4708131131366,8.30352124333549,59.5100398493929));
#165014=CARTESIAN_POINT('Ctrl Pts',(68.7861909734666,8.47259935880043,59.4508956317215));
#165015=CARTESIAN_POINT('Ctrl Pts',(68.9147412890686,8.53771126383773,59.4267541741647));
#165016=CARTESIAN_POINT('Ctrl Pts',(69.0974829948091,8.62498525819248,59.3923759285558));
#165017=CARTESIAN_POINT('Ctrl Pts',(69.1504870566599,8.64968583705695,59.3823976762416));
#165018=CARTESIAN_POINT('Ctrl Pts',(69.2421317857423,8.6913423680419,59.3651327296242));
#165019=CARTESIAN_POINT('Ctrl Pts',(69.2806647784383,8.70854058724726,59.3578697627547));
#165020=CARTESIAN_POINT('Ctrl Pts',(69.3594765051011,8.74307225362538,59.3430069905906));
#165021=CARTESIAN_POINT('Ctrl Pts',(69.3997632631269,8.7603839416773,59.3354053660714));
#165022=CARTESIAN_POINT('Ctrl Pts',(69.5017581447034,8.80335633743391,59.3161496575827));
#165023=CARTESIAN_POINT('Ctrl Pts',(69.5636185487956,8.82863364941053,59.3044613196241));
#165024=CARTESIAN_POINT('Ctrl Pts',(69.8016687807245,8.92290780269882,59.2594455518624));
#165025=CARTESIAN_POINT('Ctrl Pts',(69.9796211574574,8.98713361718635,59.2257163919939));
#165026=CARTESIAN_POINT('Ctrl Pts',(70.7411631041489,9.23581158035685,59.0810895768643));
#165027=CARTESIAN_POINT('Ctrl Pts',(71.3397562199109,9.36719190722697,58.9665975655292));
#165028=CARTESIAN_POINT('Ctrl Pts',(72.1991301160983,9.46755469557415,58.8030831991138));
#165029=CARTESIAN_POINT('Ctrl Pts',(72.4526317729423,9.48653004159974,58.7549709429072));
#165030=CARTESIAN_POINT('Ctrl Pts',(72.7667152643384,9.49694909165382,58.6957206744043));
#165031=CARTESIAN_POINT('Ctrl Pts',(72.8268225773865,9.49835171970258,58.6843981288054));
#165032=CARTESIAN_POINT('Ctrl Pts',(72.9148342969626,9.49954013994207,58.6678468103789));
#165033=CARTESIAN_POINT('Ctrl Pts',(72.9427284497063,9.4997895878609,58.6626051527566));
#165034=CARTESIAN_POINT('Ctrl Pts',(72.9920596382648,9.50000580113733,58.6533428463373));
#165035=CARTESIAN_POINT('Ctrl Pts',(73.0134958385132,9.5000246518641,58.6493206074091));
#165036=CARTESIAN_POINT('Ctrl Pts',(73.0601470328791,9.49990223896668,58.640572767602));
#165037=CARTESIAN_POINT('Ctrl Pts',(73.0853617591475,9.49973217395575,58.635848169112));
#165038=CARTESIAN_POINT('Ctrl Pts',(73.1559548792206,9.4989651516351,58.622630221057));
#165039=CARTESIAN_POINT('Ctrl Pts',(73.2013314827324,9.49813557559911,58.6141447288375));
#165040=CARTESIAN_POINT('Ctrl Pts',(73.4756717071102,9.49108498742324,58.5629014524727));
#165041=CARTESIAN_POINT('Ctrl Pts',(73.7043953227572,9.47663371187446,58.520424785588));
#165042=CARTESIAN_POINT('Ctrl Pts',(74.3917813650645,9.40732180445401,58.393091151301));
#165043=CARTESIAN_POINT('Ctrl Pts',(74.8472408255498,9.32642991849195,58.309125448333));
#165044=CARTESIAN_POINT('Ctrl Pts',(75.6180820042786,9.12874438023839,58.166267824476));
#165045=CARTESIAN_POINT('Ctrl Pts',(75.9366495404043,9.02832511309029,58.1070057134264));
#165046=CARTESIAN_POINT('Ctrl Pts',(76.3388574156216,8.87708762555163,58.0316901218072));
#165047=CARTESIAN_POINT('Ctrl Pts',(76.4280039083755,8.84197283064662,58.0149656603079));
#165048=CARTESIAN_POINT('Ctrl Pts',(76.5628067246537,8.78643424963575,57.9896255958651));
#165049=CARTESIAN_POINT('Ctrl Pts',(76.6088623295691,8.76702050247032,57.9809591105854));
#165050=CARTESIAN_POINT('Ctrl Pts',(76.6888663039483,8.73252899666594,57.9658884749638));
#165051=CARTESIAN_POINT('Ctrl Pts',(76.7228841115094,8.71761920191469,57.9594753548488));
#165052=CARTESIAN_POINT('Ctrl Pts',(76.7994668725098,8.68350139355711,57.9450262924261));
#165053=CARTESIAN_POINT('Ctrl Pts',(76.8419790785553,8.66417453909189,57.9369973369525));
#165054=CARTESIAN_POINT('Ctrl Pts',(76.9570610912391,8.61079983659528,57.9152407386684));
#165055=CARTESIAN_POINT('Ctrl Pts',(77.0293433770047,8.57612614010316,57.9015516568086));
#165056=CARTESIAN_POINT('Ctrl Pts',(77.4791503100287,8.35311436444787,57.8162181534779));
#165057=CARTESIAN_POINT('Ctrl Pts',(77.8441297628488,8.13994323877645,57.7462919457192));
#165058=CARTESIAN_POINT('Ctrl Pts',(78.4473444164101,7.73010710357301,57.6300039940216));
#165059=CARTESIAN_POINT('Ctrl Pts',(78.6925258560032,7.54519705412956,57.5825174256679));
#165060=CARTESIAN_POINT('Ctrl Pts',(79.0483369221912,7.24828745903619,57.5136000448928));
#165061=CARTESIAN_POINT('Ctrl Pts',(79.1658306746141,7.1451514156327,57.4908432673551));
#165062=CARTESIAN_POINT('Ctrl Pts',(79.3521655360193,6.97316513836637,57.4548150706156));
#165063=CARTESIAN_POINT('Ctrl Pts',(79.4225748466835,6.90612709784436,57.441216511164));
#165064=CARTESIAN_POINT('Ctrl Pts',(79.5172004461619,6.81319783560062,57.4229754134785));
#165065=CARTESIAN_POINT('Ctrl Pts',(79.5423080858706,6.78826108223574,57.4181387852745));
#165066=CARTESIAN_POINT('Ctrl Pts',(79.5842924771235,6.74609054399936,57.4100576752023));
#165067=CARTESIAN_POINT('Ctrl Pts',(79.6012430289379,6.72893380257166,57.4067968833195));
#165068=CARTESIAN_POINT('Ctrl Pts',(79.6337493060622,6.69577895143755,57.400547446014));
#165069=CARTESIAN_POINT('Ctrl Pts',(79.6493141742717,6.67979056201361,57.3975567301777));
#165070=CARTESIAN_POINT('Ctrl Pts',(79.6916039642043,6.63604086846163,57.3894351774488));
#165071=CARTESIAN_POINT('Ctrl Pts',(79.7182181437304,6.60816861267018,57.384328692972));
#165072=CARTESIAN_POINT('Ctrl Pts',(79.8217969324191,6.49835578827272,57.3644705497745));
#165073=CARTESIAN_POINT('Ctrl Pts',(79.8974917328053,6.41518117655755,57.3499923637494));
#165074=CARTESIAN_POINT('Ctrl Pts',(80.0629949456586,6.22667234011496,57.3183771873583));
#165075=CARTESIAN_POINT('Ctrl Pts',(80.1520256912976,6.12066379376989,57.3013982015584));
#165076=CARTESIAN_POINT('Ctrl Pts',(80.4886843335873,5.7014614296632,57.2371962021518));
#165077=CARTESIAN_POINT('Ctrl Pts',(80.7189754883046,5.37438790626149,57.193265298549));
#165078=CARTESIAN_POINT('Ctrl Pts',(81.0458748967027,4.84150598636741,57.1300555199009));
#165079=CARTESIAN_POINT('Ctrl Pts',(81.1568175176067,4.64534177307042,57.1084179589846));
#165080=CARTESIAN_POINT('Ctrl Pts',(81.3298969470347,4.31220727687835,57.074236822775));
#165081=CARTESIAN_POINT('Ctrl Pts',(81.395923056126,4.17742798080134,57.0610773912451));
#165082=CARTESIAN_POINT('Ctrl Pts',(81.4837841057505,3.98679968239584,57.043376120984));
#165083=CARTESIAN_POINT('Ctrl Pts',(81.5083049184154,3.93225307120993,57.0384133454154));
#165084=CARTESIAN_POINT('Ctrl Pts',(81.5494931035746,3.83827451042939,57.0300370307397));
#165085=CARTESIAN_POINT('Ctrl Pts',(81.5664100024378,3.79895744709865,57.0265844343452));
#165086=CARTESIAN_POINT('Ctrl Pts',(81.5982249145753,3.72362240157526,57.0200673153515));
#165087=CARTESIAN_POINT('Ctrl Pts',(81.6131677746623,3.68762492107599,57.0169957859893));
#165088=CARTESIAN_POINT('Ctrl Pts',(81.6514789843151,3.59371158363027,57.0090928535899));
#165089=CARTESIAN_POINT('Ctrl Pts',(81.6745016502744,3.53565223819036,57.0043156373833));
#165090=CARTESIAN_POINT('Ctrl Pts',(81.7527903732086,3.3324222750149,56.98797038004));
#165091=CARTESIAN_POINT('Ctrl Pts',(81.8050946220889,3.18610056891873,56.9768673450826));
#165092=CARTESIAN_POINT('Ctrl Pts',(82.0631810709142,2.40449066319536,56.9210693824057));
#165093=CARTESIAN_POINT('Ctrl Pts',(82.2057506654363,1.74961261556576,56.8862942838766));
#165094=CARTESIAN_POINT('Ctrl Pts',(82.3079845722295,0.827387173183443,
56.8556309596769));
#165095=CARTESIAN_POINT('Ctrl Pts',(82.3261564031287,0.568832582543673,
56.8490056737307));
#165096=CARTESIAN_POINT('Ctrl Pts',(82.3357834278011,0.248617195333988,
56.8434315861521));
#165097=CARTESIAN_POINT('Ctrl Pts',(82.337043428599,0.187394098147142,56.8424846281103));
#165098=CARTESIAN_POINT('Ctrl Pts',(82.3380389453491,0.0977708298033094,
56.841275725671));
#165099=CARTESIAN_POINT('Ctrl Pts',(82.3382296473736,0.069378543540619,
56.8409187928242));
#165100=CARTESIAN_POINT('Ctrl Pts',(82.3383275266771,0.0273237477979618,
56.8404290385353));
#165101=CARTESIAN_POINT('Ctrl Pts',(82.3383304712431,0.0136619004602319,
56.8402760238369));
#165102=CARTESIAN_POINT('Ctrl Pts',(82.3383045685277,6.65089060313308E-11,
56.8401291222381));
#165103=CARTESIAN_POINT('Origin',(73.0915550886457,-4.33680868994202E-16,
59.1075264962884));
#165104=CARTESIAN_POINT('',(82.2175389695453,-3.85097900598694E-11,56.1552333762936));
#165105=CARTESIAN_POINT('',(82.2254332530441,2.22253630170976E-12,56.2000040827795));
#165106=CARTESIAN_POINT('',(82.4472287422617,-1.59709532818419E-15,57.4578688084528));
#165107=CARTESIAN_POINT('Ctrl Pts',(82.2175389695453,-7.70179830244106E-11,
56.1552333762936));
#165108=CARTESIAN_POINT('Ctrl Pts',(82.2175620745244,0.0121862868716635,
56.1553644111411));
#165109=CARTESIAN_POINT('Ctrl Pts',(82.2175619477936,0.0243725649192966,
56.1554987250275));
#165110=CARTESIAN_POINT('Ctrl Pts',(82.2174857455006,0.0641335245306346,
56.155947728003));
#165111=CARTESIAN_POINT('Ctrl Pts',(82.2173139668202,0.0917076673255851,
56.1562760091775));
#165112=CARTESIAN_POINT('Ctrl Pts',(82.2165566947319,0.163543738420088,
56.1571759083335));
#165113=CARTESIAN_POINT('Ctrl Pts',(82.2157837221288,0.207802678087244,
56.1577745261521));
#165114=CARTESIAN_POINT('Ctrl Pts',(82.2061983382007,0.600873698792638,
56.1634922608861));
#165115=CARTESIAN_POINT('Ctrl Pts',(82.1786784220398,0.948923478496095,
56.1713709101551));
#165116=CARTESIAN_POINT('Ctrl Pts',(82.0538629847073,1.88018669068649,56.2012266847151));
#165117=CARTESIAN_POINT('Ctrl Pts',(81.9216856181147,2.45697178307319,56.229201204761));
#165118=CARTESIAN_POINT('Ctrl Pts',(81.6875862658055,3.17034383592015,56.2776770403699));
#165119=CARTESIAN_POINT('Ctrl Pts',(81.6336012798549,3.3219020002445,56.2888037339773));
#165120=CARTESIAN_POINT('Ctrl Pts',(81.5531229118076,3.53107093947884,56.3053371858243));
#165121=CARTESIAN_POINT('Ctrl Pts',(81.5298083402281,3.58992378570806,56.3101212559712));
#165122=CARTESIAN_POINT('Ctrl Pts',(81.491146103596,3.68476798626927,56.3180461257499));
#165123=CARTESIAN_POINT('Ctrl Pts',(81.4761553594863,3.72090851966491,56.3211169235837));
#165124=CARTESIAN_POINT('Ctrl Pts',(81.4443550207683,3.79626858230797,56.3276271313064));
#165125=CARTESIAN_POINT('Ctrl Pts',(81.4275041822755,3.83546905362349,56.3310746299236));
#165126=CARTESIAN_POINT('Ctrl Pts',(81.3867044148995,3.92866293587459,56.3394165991324));
#165127=CARTESIAN_POINT('Ctrl Pts',(81.3625185207907,3.98254646306949,56.3443575486508));
#165128=CARTESIAN_POINT('Ctrl Pts',(81.2771522854187,4.16812074730835,56.3617826966859));
#165129=CARTESIAN_POINT('Ctrl Pts',(81.2134940697439,4.29860307490458,56.3747524956992));
#165130=CARTESIAN_POINT('Ctrl Pts',(81.0482941283829,4.61852375479393,56.4083401359228));
#165131=CARTESIAN_POINT('Ctrl Pts',(80.9433123773971,4.806022412251,56.4296260573174));
#165132=CARTESIAN_POINT('Ctrl Pts',(80.6865899462031,5.23021834429121,56.4814658488889));
#165133=CARTESIAN_POINT('Ctrl Pts',(80.530558490987,5.46398204266914,56.5128259906746));
#165134=CARTESIAN_POINT('Ctrl Pts',(80.1648041338178,5.96244627766321,56.5857209756538));
#165135=CARTESIAN_POINT('Ctrl Pts',(79.9508678511729,6.22347209507369,56.6279797701092));
#165136=CARTESIAN_POINT('Ctrl Pts',(79.678105468441,6.521983184975,56.6810043200086));
#165137=CARTESIAN_POINT('Ctrl Pts',(79.6321377388087,6.57121556460514,56.6899132678471));
#165138=CARTESIAN_POINT('Ctrl Pts',(79.5646994463674,6.64190129658138,56.7029397132091));
#165139=CARTESIAN_POINT('Ctrl Pts',(79.5436435040226,6.66375768332045,56.7070008495884));
#165140=CARTESIAN_POINT('Ctrl Pts',(79.5061469828496,6.70230312436851,56.7142217205384));
#165141=CARTESIAN_POINT('Ctrl Pts',(79.4897488133509,6.71903399741452,56.7173758080022));
#165142=CARTESIAN_POINT('Ctrl Pts',(79.4539161931046,6.75532031285381,56.7242596750609));
#165143=CARTESIAN_POINT('Ctrl Pts',(79.434458260369,6.77485136752792,56.7279925614772));
#165144=CARTESIAN_POINT('Ctrl Pts',(79.3784249260081,6.83060084423773,56.7387280702822));
#165145=CARTESIAN_POINT('Ctrl Pts',(79.3416394927014,6.86660132105009,56.7457587203696));
#165146=CARTESIAN_POINT('Ctrl Pts',(79.0175287495276,7.1786073355827,56.8075703968907));
#165147=CARTESIAN_POINT('Ctrl Pts',(78.7133905672762,7.43609472433736,56.8646752078561));
#165148=CARTESIAN_POINT('Ctrl Pts',(77.9735201813484,7.98551216630177,57.0031456553133));
#165149=CARTESIAN_POINT('Ctrl Pts',(77.5279529581351,8.26149527837192,57.0862542394029));
#165150=CARTESIAN_POINT('Ctrl Pts',(76.983102419283,8.53846986069015,57.1885754105908));
#165151=CARTESIAN_POINT('Ctrl Pts',(76.9034471491996,8.57753525660988,57.203548851024));
#165152=CARTESIAN_POINT('Ctrl Pts',(76.7751386798869,8.6381939205145,57.2276938284204));
#165153=CARTESIAN_POINT('Ctrl Pts',(76.7268272047935,8.66052641760476,57.2367907960276));
#165154=CARTESIAN_POINT('Ctrl Pts',(76.6405008350899,8.69953263960527,57.2530565700462));
#165155=CARTESIAN_POINT('Ctrl Pts',(76.6025586872288,8.71637043882293,57.2602093307856));
#165156=CARTESIAN_POINT('Ctrl Pts',(76.5227956256994,8.75112733978341,57.2752538299828));
#165157=CARTESIAN_POINT('Ctrl Pts',(76.4809539725674,8.76899405052932,57.2831502259788));
#165158=CARTESIAN_POINT('Ctrl Pts',(76.3702229493109,8.81531470475086,57.3040593187258));
#165159=CARTESIAN_POINT('Ctrl Pts',(76.3011261214664,8.84324279410233,57.3171187399343));
#165160=CARTESIAN_POINT('Ctrl Pts',(75.9576090925401,8.97728014827677,57.3821030649231));
#165161=CARTESIAN_POINT('Ctrl Pts',(75.678739035092,9.07101369527477,57.4350499334955));
#165162=CARTESIAN_POINT('Ctrl Pts',(75.0612281700856,9.2461931608153,57.5525758406731));
#165163=CARTESIAN_POINT('Ctrl Pts',(74.721520829263,9.32205977431937,57.6174126566182));
#165164=CARTESIAN_POINT('Ctrl Pts',(73.9972657324468,9.44113101204135,57.7554901024172));
#165165=CARTESIAN_POINT('Ctrl Pts',(73.6126189152372,9.47965962981043,57.8287326794291));
#165166=CARTESIAN_POINT('Ctrl Pts',(73.1592396026607,9.496299819408,57.9143042024002));
#165167=CARTESIAN_POINT('Ctrl Pts',(73.0918262416238,9.49803008931145,57.9270078295874));
#165168=CARTESIAN_POINT('Ctrl Pts',(72.9980835743534,9.49940224097944,57.9446402841706));
#165169=CARTESIAN_POINT('Ctrl Pts',(72.9717688650273,9.49967420496134,57.9495863397234));
#165170=CARTESIAN_POINT('Ctrl Pts',(72.9237679607012,9.49996380483364,57.9586015502288));
#165171=CARTESIAN_POINT('Ctrl Pts',(72.9020823312584,9.50001777646759,57.9626718146363));
#165172=CARTESIAN_POINT('Ctrl Pts',(72.856938195237,9.49997012948229,57.971139498765));
#165173=CARTESIAN_POINT('Ctrl Pts',(72.8334798853964,9.49985543946105,57.9755364555061));
#165174=CARTESIAN_POINT('Ctrl Pts',(72.771431030582,9.49931420252947,57.9871588975185));
#165175=CARTESIAN_POINT('Ctrl Pts',(72.7328413227241,9.49873421311251,57.9943791863935));
#165176=CARTESIAN_POINT('Ctrl Pts',(72.5508299589987,9.49485057232465,58.0283999328086));
#165177=CARTESIAN_POINT('Ctrl Pts',(72.4074752508745,9.48842877138747,58.0550948567981));
#165178=CARTESIAN_POINT('Ctrl Pts',(71.9753540438651,9.45891434027047,58.1353667090422));
#165179=CARTESIAN_POINT('Ctrl Pts',(71.6874089123619,9.42552056815721,58.1885951733545));
#165180=CARTESIAN_POINT('Ctrl Pts',(70.8161170126059,9.28248609388585,58.3496263522637));
#165181=CARTESIAN_POINT('Ctrl Pts',(70.2411063311084,9.12994596080931,58.4559460771608));
#165182=CARTESIAN_POINT('Ctrl Pts',(69.5890838328112,8.88758409169151,58.5779859853179));
#165183=CARTESIAN_POINT('Ctrl Pts',(69.4943290835659,8.85056846763861,58.5957563229759));
#165184=CARTESIAN_POINT('Ctrl Pts',(69.3522345542083,8.79233419362202,58.6224607516421));
#165185=CARTESIAN_POINT('Ctrl Pts',(69.3044392768821,8.77227464282157,58.6314527881624));
#165186=CARTESIAN_POINT('Ctrl Pts',(69.2189114661975,8.73552884529499,58.647561331022));
#165187=CARTESIAN_POINT('Ctrl Pts',(69.1811182813761,8.71899074709797,58.6546856437987));
#165188=CARTESIAN_POINT('Ctrl Pts',(69.1007034504526,8.68315792932284,58.6698578751031));
#165189=CARTESIAN_POINT('Ctrl Pts',(69.0581143296217,8.66379122099352,58.6779014586559));
#165190=CARTESIAN_POINT('Ctrl Pts',(68.9425927259727,8.61019732111228,58.6997414808514));
#165191=CARTESIAN_POINT('Ctrl Pts',(68.8699516874946,8.57533592037105,58.7134988282191));
#165192=CARTESIAN_POINT('Ctrl Pts',(68.3808720939099,8.33270658786113,58.8062857783619));
#165193=CARTESIAN_POINT('Ctrl Pts',(67.9798541986424,8.09455740946324,58.8832076541506));
#165194=CARTESIAN_POINT('Ctrl Pts',(67.2147222754163,7.55860487548355,59.0308855936294));
#165195=CARTESIAN_POINT('Ctrl Pts',(66.8518098591758,7.26133843998112,59.101405090164));
#165196=CARTESIAN_POINT('Ctrl Pts',(66.4671849021322,6.89494858120251,59.1756746766675));
#165197=CARTESIAN_POINT('Ctrl Pts',(66.4226725371892,6.85169931982702,59.1842615147789));
#165198=CARTESIAN_POINT('Ctrl Pts',(66.3574947827016,6.78710758881896,59.1968186068262));
#165199=CARTESIAN_POINT('Ctrl Pts',(66.3365047582742,6.76610892278493,59.2008599820277));
#165200=CARTESIAN_POINT('Ctrl Pts',(66.2991860104668,6.72842073324678,59.2080401643776));
#165201=CARTESIAN_POINT('Ctrl Pts',(66.2828203404166,6.7117699534582,59.2111871401934));
#165202=CARTESIAN_POINT('Ctrl Pts',(66.2466333623729,6.67467835505118,59.2181415256148));
#165203=CARTESIAN_POINT('Ctrl Pts',(66.22684194196,6.65420778762587,59.2219423594693));
#165204=CARTESIAN_POINT('Ctrl Pts',(66.1684990950266,6.59331417175923,59.233139679782));
#165205=CARTESIAN_POINT('Ctrl Pts',(66.1302081089394,6.55263290968459,59.2404793232206));
#165206=CARTESIAN_POINT('Ctrl Pts',(66.0422595881523,6.45751774152815,59.2573204728252));
#165207=CARTESIAN_POINT('Ctrl Pts',(65.9928682087842,6.4028328036149,59.2667655933367));
#165208=CARTESIAN_POINT('Ctrl Pts',(65.8225424895113,6.20976098797361,59.2993078670539));
#165209=CARTESIAN_POINT('Ctrl Pts',(65.704949852707,6.06836792413911,59.3217230911174));
#165210=CARTESIAN_POINT('Ctrl Pts',(65.215870483904,5.44415901253735,59.4150013797009));
#165211=CARTESIAN_POINT('Ctrl Pts',(64.8867595558317,4.92884250935033,59.478011582582));
#165212=CARTESIAN_POINT('Ctrl Pts',(64.5493840775644,4.26797225134133,59.5448194755039));
#165213=CARTESIAN_POINT('Ctrl Pts',(64.4921291875201,4.14984913494886,59.5562517085704));
#165214=CARTESIAN_POINT('Ctrl Pts',(64.4154356828987,3.98291536388703,59.571712058257));
#165215=CARTESIAN_POINT('Ctrl Pts',(64.3939421956042,3.93509557823367,59.5760622783589));
#165216=CARTESIAN_POINT('Ctrl Pts',(64.3571627202203,3.85142731528745,59.5835377245434));
#165217=CARTESIAN_POINT('Ctrl Pts',(64.3417008356567,3.81566004262481,59.586690486836));
#165218=CARTESIAN_POINT('Ctrl Pts',(64.3097097940619,3.74039323108995,59.5932353433659));
#165219=CARTESIAN_POINT('Ctrl Pts',(64.2932262911236,3.70087462195001,59.5966202714521));
#165220=CARTESIAN_POINT('Ctrl Pts',(64.2543319561201,3.605830728441,59.6046383323961));
#165221=CARTESIAN_POINT('Ctrl Pts',(64.2321754608835,3.55020002443238,59.6092315914428));
#165222=CARTESIAN_POINT('Ctrl Pts',(64.1563921844887,3.35458757211139,59.6250345028206));
#165223=CARTESIAN_POINT('Ctrl Pts',(64.1055283720938,3.21352487109014,59.6358104759258));
#165224=CARTESIAN_POINT('Ctrl Pts',(63.988065760597,2.86205745497629,59.6611334279503));
#165225=CARTESIAN_POINT('Ctrl Pts',(63.9253765203239,2.65039565983729,59.6750591981307));
#165226=CARTESIAN_POINT('Ctrl Pts',(63.7884368219202,2.12161140682363,59.7065306162399));
#165227=CARTESIAN_POINT('Ctrl Pts',(63.7228996629691,1.80243963382905,59.722643823742));
#165228=CARTESIAN_POINT('Ctrl Pts',(63.6160865447336,1.10414900362851,59.7512898850749));
#165229=CARTESIAN_POINT('Ctrl Pts',(63.5808610013559,0.724622868931706,
59.7627366078957));
#165230=CARTESIAN_POINT('Ctrl Pts',(63.565811873296,0.276579473032023,59.7708582425205));
#165231=CARTESIAN_POINT('Ctrl Pts',(63.5642523957128,0.209213552212095,
59.771936077013));
#165232=CARTESIAN_POINT('Ctrl Pts',(63.5630465374347,0.114443810012844,
59.7732463666027));
#165233=CARTESIAN_POINT('Ctrl Pts',(63.5628140543119,0.0870511349330532,
59.7736008980186));
#165234=CARTESIAN_POINT('Ctrl Pts',(63.5626031218862,0.0374410612222554,
59.7741987545936));
#165235=CARTESIAN_POINT('Ctrl Pts',(63.5625849663477,0.0152240743026672,
59.7744504300767));
#165236=CARTESIAN_POINT('Ctrl Pts',(63.5627047979013,-0.0305737816256809,
59.7749358875716));
#165237=CARTESIAN_POINT('Ctrl Pts',(63.5628524406064,-0.0541544114140678,
59.7751676439857));
#165238=CARTESIAN_POINT('Ctrl Pts',(63.5634622090994,-0.115702896466913,
59.77572545554));
#165239=CARTESIAN_POINT('Ctrl Pts',(63.5640612526523,-0.153669231067783,
59.7760227548591));
#165240=CARTESIAN_POINT('Ctrl Pts',(63.5677400631327,-0.323564379696103,
59.777146552675));
#165241=CARTESIAN_POINT('Ctrl Pts',(63.5732895440022,-0.455428398293493,
59.7774613206361));
#165242=CARTESIAN_POINT('Ctrl Pts',(63.5971206372631,-0.836202868321354,
59.7768313736759));
#165243=CARTESIAN_POINT('Ctrl Pts',(63.6223320867661,-1.08456573484011,
59.7745165900299));
#165244=CARTESIAN_POINT('Ctrl Pts',(63.7443233637202,-1.95062406346372,
59.7602871509199));
#165245=CARTESIAN_POINT('Ctrl Pts',(63.8914315948919,-2.55945440010806,
59.7393107377751));
#165246=CARTESIAN_POINT('Ctrl Pts',(64.1385327652096,-3.26990492891155,
59.703122990503));
#165247=CARTESIAN_POINT('Ctrl Pts',(64.1828933734677,-3.38967454326454,
59.6965973917688));
#165248=CARTESIAN_POINT('Ctrl Pts',(64.2487108750063,-3.55701877615604,
59.6868826856176));
#165249=CARTESIAN_POINT('Ctrl Pts',(64.2681873933737,-3.60537513089997,
59.6840042273985));
#165250=CARTESIAN_POINT('Ctrl Pts',(64.3028981612861,-3.68956340370318,
59.6788681789778));
#165251=CARTESIAN_POINT('Ctrl Pts',(64.3179584121365,-3.72546734379838,
59.6766378467166));
#165252=CARTESIAN_POINT('Ctrl Pts',(64.3500969183202,-3.80079360850932,
59.6718744257086));
#165253=CARTESIAN_POINT('Ctrl Pts',(64.367222281152,-3.84019441151532,59.6693339571896));
#165254=CARTESIAN_POINT('Ctrl Pts',(64.4090693029255,-3.93472540099453,
59.663120875671));
#165255=CARTESIAN_POINT('Ctrl Pts',(64.4340481639736,-3.98973699671165,
59.6594079725064));
#165256=CARTESIAN_POINT('Ctrl Pts',(64.5244805229854,-4.18398537948775,
59.6459507146065));
#165257=CARTESIAN_POINT('Ctrl Pts',(64.5927608270677,-4.32184840076192,
59.6357630694951));
#165258=CARTESIAN_POINT('Ctrl Pts',(64.7729616938718,-4.6646132255352,59.6087960152249));
#165259=CARTESIAN_POINT('Ctrl Pts',(64.8891032179446,-4.86712635008318,
59.5913466483073));
#165260=CARTESIAN_POINT('Ctrl Pts',(65.2529335065035,-5.45082121639412,
59.5363472454328));
#165261=CARTESIAN_POINT('Ctrl Pts',(65.5204482048142,-5.81854141906376,
59.4955236191868));
#165262=CARTESIAN_POINT('Ctrl Pts',(65.9247370630333,-6.29813185639718,
59.4323873901518));
#165263=CARTESIAN_POINT('Ctrl Pts',(66.0401874079234,-6.4277107235389,59.4142141817589));
#165264=CARTESIAN_POINT('Ctrl Pts',(66.1897635683192,-6.58661150715075,
59.3904271706775));
#165265=CARTESIAN_POINT('Ctrl Pts',(66.2206889708783,-6.61900258610501,
59.3854966324181));
#165266=CARTESIAN_POINT('Ctrl Pts',(66.2700517067541,-6.66997796876365,
59.3776053745324));
#165267=CARTESIAN_POINT('Ctrl Pts',(66.2883413064505,-6.68870939939189,
59.3746770105363));
#165268=CARTESIAN_POINT('Ctrl Pts',(66.3234458981832,-6.72436576901142,
59.3690473612066));
#165269=CARTESIAN_POINT('Ctrl Pts',(66.3402478009024,-6.74130354862017,
59.3663489302962));
#165270=CARTESIAN_POINT('Ctrl Pts',(66.3809259913035,-6.7820025415984,59.3598067384754));
#165271=CARTESIAN_POINT('Ctrl Pts',(66.4048642247952,-6.80569921666708,
59.3559492727713));
#165272=CARTESIAN_POINT('Ctrl Pts',(66.4897143304273,-6.8888024955165,59.3422515156564));
#165273=CARTESIAN_POINT('Ctrl Pts',(66.5512873626772,-6.94750424524676,
59.3322668481808));
#165274=CARTESIAN_POINT('Ctrl Pts',(66.7084096821243,-7.0933063414243,59.3066948451297));
#165275=CARTESIAN_POINT('Ctrl Pts',(66.8049508350474,-7.17927490182089,
59.290898343425));
#165276=CARTESIAN_POINT('Ctrl Pts',(67.1613982950677,-7.48378914760924,
59.2323604180414));
#165277=CARTESIAN_POINT('Ctrl Pts',(67.4311086149228,-7.69007459519244,
59.1876745378135));
#165278=CARTESIAN_POINT('Ctrl Pts',(68.071693917673,-8.1270845017641,59.0814904797406));
#165279=CARTESIAN_POINT('Ctrl Pts',(68.4486107637276,-8.34730051285811,
59.0189927479848));
#165280=CARTESIAN_POINT('Ctrl Pts',(68.9115515542384,-8.57588875258249,
58.9427127267715));
#165281=CARTESIAN_POINT('Ctrl Pts',(68.9842489482258,-8.61061878555466,
58.9307464776536));
#165282=CARTESIAN_POINT('Ctrl Pts',(69.0999490490133,-8.66405919435124,
58.911722998239));
#165283=CARTESIAN_POINT('Ctrl Pts',(69.1426632811826,-8.68339801746371,
58.9047043961044));
#165284=CARTESIAN_POINT('Ctrl Pts',(69.2195870056219,-8.71752688826053,
58.8920729666375));
#165285=CARTESIAN_POINT('Ctrl Pts',(69.2537436153409,-8.73243619010334,
58.8864671222394));
#165286=CARTESIAN_POINT('Ctrl Pts',(69.3340446243686,-8.76691437695578,
58.8732949155118));
#165287=CARTESIAN_POINT('Ctrl Pts',(69.3802581938401,-8.78631576454893,
58.865719597622));
#165288=CARTESIAN_POINT('Ctrl Pts',(69.5154216480485,-8.84177899321317,
58.8435793224506));
#165289=CARTESIAN_POINT('Ctrl Pts',(69.604768676677,-8.87683519159539,58.8289636824492));
#165290=CARTESIAN_POINT('Ctrl Pts',(70.0072702993052,-9.02760911525914,
58.7632075382063));
#165291=CARTESIAN_POINT('Ctrl Pts',(70.3258850950275,-9.12774502686906,
58.7113985139972));
#165292=CARTESIAN_POINT('Ctrl Pts',(71.0969522993489,-9.32511883330916,
58.5863256146551));
#165293=CARTESIAN_POINT('Ctrl Pts',(71.5525869452587,-9.40608139030943,
58.5126788994558));
#165294=CARTESIAN_POINT('Ctrl Pts',(72.2438926967472,-9.47622088882419,
58.400244879462));
#165295=CARTESIAN_POINT('Ctrl Pts',(72.4763799309137,-9.49097891651943,
58.3623090960784));
#165296=CARTESIAN_POINT('Ctrl Pts',(72.7547908270631,-9.49812560070746,
58.3165745647492));
#165297=CARTESIAN_POINT('Ctrl Pts',(72.8004625647699,-9.49895958987249,
58.3090621959707));
#165298=CARTESIAN_POINT('Ctrl Pts',(72.8714751557372,-9.49973027764158,
58.2973645693163));
#165299=CARTESIAN_POINT('Ctrl Pts',(72.8968140488972,-9.49990115307864,
58.2931872194712));
#165300=CARTESIAN_POINT('Ctrl Pts',(72.9436688625342,-9.50002458677733,
58.2854561870684));
#165301=CARTESIAN_POINT('Ctrl Pts',(72.965184494514,-9.50000619109166,58.2819035101863));
#165302=CARTESIAN_POINT('Ctrl Pts',(73.0146645841112,-9.49979122393638,
58.2737274449891));
#165303=CARTESIAN_POINT('Ctrl Pts',(73.0426282400995,-9.49954289144836,
58.2691024635894));
#165304=CARTESIAN_POINT('Ctrl Pts',(73.1307367887179,-9.49836072409547,
58.2545173298241));
#165305=CARTESIAN_POINT('Ctrl Pts',(73.1908717925495,-9.49696688684111,
58.244544276516));
#165306=CARTESIAN_POINT('Ctrl Pts',(73.5041701253002,-9.48664528586601,
58.1925026773694));
#165307=CARTESIAN_POINT('Ctrl Pts',(73.7568704128003,-9.46790241810498,
58.150247235287));
#165308=CARTESIAN_POINT('Ctrl Pts',(74.6603698854748,-9.36341819237609,
57.9988155375674));
#165309=CARTESIAN_POINT('Ctrl Pts',(75.3025413293082,-9.21882108871517,
57.8906637770959));
#165310=CARTESIAN_POINT('Ctrl Pts',(76.0751313925175,-8.95629786087919,
57.7623404957863));
#165311=CARTESIAN_POINT('Ctrl Pts',(76.224168511168,-8.90135887875654,57.7376640911452));
#165312=CARTESIAN_POINT('Ctrl Pts',(76.4300017368328,-8.81944076371623,
57.7037070194924));
#165313=CARTESIAN_POINT('Ctrl Pts',(76.4880018947259,-8.79567680527895,
57.6941523172009));
#165314=CARTESIAN_POINT('Ctrl Pts',(76.5815080802493,-8.75625874296686,
57.6787713768637));
#165315=CARTESIAN_POINT('Ctrl Pts',(76.6171592983647,-8.74096698003743,
57.6729124962143));
#165316=CARTESIAN_POINT('Ctrl Pts',(76.6915260106254,-8.70851809124034,
57.6607026041018));
#165317=CARTESIAN_POINT('Ctrl Pts',(76.7302227439204,-8.69131863301243,
57.6543557230571));
#165318=CARTESIAN_POINT('Ctrl Pts',(76.8222676616797,-8.64965472452142,
57.6392745429163));
#165319=CARTESIAN_POINT('Ctrl Pts',(76.8755079820579,-8.62494783429335,
57.6305639782182));
#165320=CARTESIAN_POINT('Ctrl Pts',(77.0591192468841,-8.5376265410225,57.6005672169524));
#165321=CARTESIAN_POINT('Ctrl Pts',(77.1883002213919,-8.47247045301536,
57.5795398580098));
#165322=CARTESIAN_POINT('Ctrl Pts',(77.505290310716,-8.30324638365334,57.5281223737234));
#165323=CARTESIAN_POINT('Ctrl Pts',(77.6911784217267,-8.19563718395348,
57.4981331107367));
#165324=CARTESIAN_POINT('Ctrl Pts',(78.1125317238058,-7.93197826357809,
57.4304529739996));
#165325=CARTESIAN_POINT('Ctrl Pts',(78.3450435113787,-7.77145544903179,
57.3933335561804));
#165326=CARTESIAN_POINT('Ctrl Pts',(78.8358689351876,-7.39883103005937,
57.3151697379637));
#165327=CARTESIAN_POINT('Ctrl Pts',(79.0908960030443,-7.18291245339915,
57.2746861830794));
#165328=CARTESIAN_POINT('Ctrl Pts',(79.3830623834846,-6.90755410413531,
57.2280539009541));
#165329=CARTESIAN_POINT('Ctrl Pts',(79.4315945600879,-6.86082045483507,
57.2202984410942));
#165330=CARTESIAN_POINT('Ctrl Pts',(79.5012967023609,-6.79224424901472,
57.209141605724));
#165331=CARTESIAN_POINT('Ctrl Pts',(79.522864787333,-6.77081804980244,57.2056867114393));
#165332=CARTESIAN_POINT('Ctrl Pts',(79.5609114469926,-6.73265380055672,
57.1995869903538));
#165333=CARTESIAN_POINT('Ctrl Pts',(79.5774313805395,-6.71595835660609,
57.1969366955561));
#165334=CARTESIAN_POINT('Ctrl Pts',(79.6132720921959,-6.67946480850964,
57.1911827495876));
#165335=CARTESIAN_POINT('Ctrl Pts',(79.6325685684232,-6.65964293273335,
57.1880823450334));
#165336=CARTESIAN_POINT('Ctrl Pts',(79.6876784168167,-6.60253152853697,
57.1792212366246));
#165337=CARTESIAN_POINT('Ctrl Pts',(79.7232748410593,-6.56502954200024,
57.1734897490192));
#165338=CARTESIAN_POINT('Ctrl Pts',(79.8040039113589,-6.47856586838472,
57.1604767127394));
#165339=CARTESIAN_POINT('Ctrl Pts',(79.8489323281395,-6.42941297542616,
57.1532238516866));
#165340=CARTESIAN_POINT('Ctrl Pts',(79.9980546995396,-6.26276313442566,
57.1291258705521));
#165341=CARTESIAN_POINT('Ctrl Pts',(80.0998629457856,-6.14311628286953,
57.1126323285365));
#165342=CARTESIAN_POINT('Ctrl Pts',(80.3929830460275,-5.78074458578222,
57.0651409734119));
#165343=CARTESIAN_POINT('Ctrl Pts',(80.5755427005811,-5.53102836071804,
57.0355623913189));
#165344=CARTESIAN_POINT('Ctrl Pts',(80.9802669564043,-4.91675757855925,
56.9705976841673));
#165345=CARTESIAN_POINT('Ctrl Pts',(81.1908643999103,-4.54517358206381,
56.9373313267025));
#165346=CARTESIAN_POINT('Ctrl Pts',(81.4113813377762,-4.08738135032824,
56.903668062532));
#165347=CARTESIAN_POINT('Ctrl Pts',(81.4456740060786,-4.01381968472663,
56.8984723920213));
#165348=CARTESIAN_POINT('Ctrl Pts',(81.4984732922601,-3.89670774432487,
56.8905385038862));
#165349=CARTESIAN_POINT('Ctrl Pts',(81.517594267403,-3.85344708955096,56.887679769165));
#165350=CARTESIAN_POINT('Ctrl Pts',(81.5513531681741,-3.77551870635186,
56.8826592486652));
#165351=CARTESIAN_POINT('Ctrl Pts',(81.5661077480066,-3.74090409221866,
56.8804745596192));
#165352=CARTESIAN_POINT('Ctrl Pts',(81.6002440999726,-3.65949864885815,
56.8754429062316));
#165353=CARTESIAN_POINT('Ctrl Pts',(81.6194609877526,-3.61263794251452,
56.8726282660487));
#165354=CARTESIAN_POINT('Ctrl Pts',(81.6744455782646,-3.47548322584599,
56.864628232049));
#165355=CARTESIAN_POINT('Ctrl Pts',(81.7092217585729,-3.38478754154093,
56.8596371019274));
#165356=CARTESIAN_POINT('Ctrl Pts',(81.8590565514482,-2.97561238638222,
56.8384509770979));
#165357=CARTESIAN_POINT('Ctrl Pts',(81.958699239592,-2.6515985568033,56.8252708302773));
#165358=CARTESIAN_POINT('Ctrl Pts',(82.1552523845467,-1.86766016950789,
56.8015427679651));
#165359=CARTESIAN_POINT('Ctrl Pts',(82.2360663723526,-1.40452785883608,
56.7940116455042));
#165360=CARTESIAN_POINT('Ctrl Pts',(82.3059376725285,-0.705470276392925,
56.7911260463762));
#165361=CARTESIAN_POINT('Ctrl Pts',(82.3206849691564,-0.472851123781757,
56.7915423018543));
#165362=CARTESIAN_POINT('Ctrl Pts',(82.3281960917859,-0.193782709245965,
56.7935378153007));
#165363=CARTESIAN_POINT('Ctrl Pts',(82.3291052846221,-0.147622223252684,
56.7939167965575));
#165364=CARTESIAN_POINT('Ctrl Pts',(82.3300012247138,-0.0758064396675572,
56.7945808515836));
#165365=CARTESIAN_POINT('Ctrl Pts',(82.3302183408803,-0.050154416533749,
56.7948328187476));
#165366=CARTESIAN_POINT('Ctrl Pts',(82.3303688796997,-0.0163346475376253,
56.7951842479547));
#165367=CARTESIAN_POINT('Ctrl Pts',(82.3303947999415,-0.00816731830620228,
56.7952705954578));
#165368=CARTESIAN_POINT('Ctrl Pts',(82.3304102850288,-6.66914478404779E-11,
56.7953584157516));
#165369=CARTESIAN_POINT('Ctrl Pts',(82.3383045685277,6.65089060313308E-11,
56.8401291222381));
#165370=CARTESIAN_POINT('Ctrl Pts',(82.3382891198383,-0.00814812083209077,
56.8400415083665));
#165371=CARTESIAN_POINT('Ctrl Pts',(82.3382634099389,-0.0162962606031404,
56.8399560689772));
#165372=CARTESIAN_POINT('Ctrl Pts',(82.3381142235792,-0.0500886157455977,
56.8396107235002));
#165373=CARTESIAN_POINT('Ctrl Pts',(82.3378993598792,-0.0757324820082624,
56.8393701306411));
#165374=CARTESIAN_POINT('Ctrl Pts',(82.3370133961438,-0.147503556506034,
56.8387563346514));
#165375=CARTESIAN_POINT('Ctrl Pts',(82.3361149589866,-0.193627645666198,
56.8384307441625));
#165376=CARTESIAN_POINT('Ctrl Pts',(82.3287105975161,-0.471784942100996,
56.8368758697467));
#165377=CARTESIAN_POINT('Ctrl Pts',(82.3142028398022,-0.703535625737106,
56.8372945169323));
#165378=CARTESIAN_POINT('Ctrl Pts',(82.2451559517499,-1.40204384123383,
56.8433425556184));
#165379=CARTESIAN_POINT('Ctrl Pts',(82.1649285806936,-1.86548886623128,
56.8538309024253));
#165380=CARTESIAN_POINT('Ctrl Pts',(81.9690154662661,-2.65026386832995,
56.8814326097488));
#165381=CARTESIAN_POINT('Ctrl Pts',(81.8694801133853,-2.97478760329092,
56.8958893521575));
#165382=CARTESIAN_POINT('Ctrl Pts',(81.7196022110395,-3.38452010758047,
56.917915740973));
#165383=CARTESIAN_POINT('Ctrl Pts',(81.6848255031272,-3.47528461757496,
56.9230415830219));
#165384=CARTESIAN_POINT('Ctrl Pts',(81.6298318777468,-3.61252089360705,
56.9311668709349));
#165385=CARTESIAN_POINT('Ctrl Pts',(81.6106148190805,-3.6593954274055,56.9340095719962));
#165386=CARTESIAN_POINT('Ctrl Pts',(81.5764771614856,-3.74081598299976,
56.9390650279483));
#165387=CARTESIAN_POINT('Ctrl Pts',(81.5617227328761,-3.77543202779978,
56.9412517604641));
#165388=CARTESIAN_POINT('Ctrl Pts',(81.5279659739346,-3.85335226620104,
56.9462586496192));
#165389=CARTESIAN_POINT('Ctrl Pts',(81.5088463702305,-3.89660337226774,
56.9490971738732));
#165390=CARTESIAN_POINT('Ctrl Pts',(81.4560582893587,-4.01366099589013,
56.9569413162896));
#165391=CARTESIAN_POINT('Ctrl Pts',(81.4217723907162,-4.08717814071998,
56.9620436852196));
#165392=CARTESIAN_POINT('Ctrl Pts',(81.2022765377962,-4.54260135140602,
56.9947577934366));
#165393=CARTESIAN_POINT('Ctrl Pts',(80.9928312549118,-4.9120155174059,57.0261554780359));
#165394=CARTESIAN_POINT('Ctrl Pts',(80.4917720065388,-5.6727623075419,57.1022244479419));
#165395=CARTESIAN_POINT('Ctrl Pts',(80.1933065189435,-6.05801669622355,
57.148060138746));
#165396=CARTESIAN_POINT('Ctrl Pts',(79.8102897917012,-6.48109335088491,
57.2085567934619));
#165397=CARTESIAN_POINT('Ctrl Pts',(79.7526440586559,-6.54308221655692,
57.2177026258355));
#165398=CARTESIAN_POINT('Ctrl Pts',(79.6709682595171,-6.62859098653333,
57.2307261813518));
#165399=CARTESIAN_POINT('Ctrl Pts',(79.6476187347245,-6.65277776772802,
57.2344566311803));
#165400=CARTESIAN_POINT('Ctrl Pts',(79.6074889607966,-6.69390710144073,
57.2408810574269));
#165401=CARTESIAN_POINT('Ctrl Pts',(79.5907713126838,-6.71091248007769,
57.2435612451249));
#165402=CARTESIAN_POINT('Ctrl Pts',(79.5555464442626,-6.74647455622879,
57.2492167994907));
#165403=CARTESIAN_POINT('Ctrl Pts',(79.5370264080459,-6.76501760683904,
57.2521949918781));
#165404=CARTESIAN_POINT('Ctrl Pts',(79.486560666629,-6.8151289741064,57.260322450614));
#165405=CARTESIAN_POINT('Ctrl Pts',(79.4544697775737,-6.84654490320242,
57.265503702611));
#165406=CARTESIAN_POINT('Ctrl Pts',(79.2959633071769,-6.99952600169218,
57.2911537617373));
#165407=CARTESIAN_POINT('Ctrl Pts',(79.1664680583497,-7.11773790032335,
57.312288758826));
#165408=CARTESIAN_POINT('Ctrl Pts',(78.6947239030557,-7.52488294235893,
57.389690861074));
#165409=CARTESIAN_POINT('Ctrl Pts',(78.33560004559,-7.79268367816114,57.4493206218922));
#165410=CARTESIAN_POINT('Ctrl Pts',(77.7626713821278,-8.15921882331197,
57.5442831301041));
#165411=CARTESIAN_POINT('Ctrl Pts',(77.561765893465,-8.27740376737075,57.5775603803411));
#165412=CARTESIAN_POINT('Ctrl Pts',(77.2218963972632,-8.46056403265779,
57.6337081930567));
#165413=CARTESIAN_POINT('Ctrl Pts',(77.0853321787573,-8.52987368028322,
57.6562322506337));
#165414=CARTESIAN_POINT('Ctrl Pts',(76.8930291014963,-8.62158123135433,
57.6878834588329));
#165415=CARTESIAN_POINT('Ctrl Pts',(76.8386639716943,-8.64686570101434,
57.6968242991517));
#165416=CARTESIAN_POINT('Ctrl Pts',(76.7452835752686,-8.6892029638159,57.7121687408336));
#165417=CARTESIAN_POINT('Ctrl Pts',(76.7063864910668,-8.70651743802117,
57.7185566226445));
#165418=CARTESIAN_POINT('Ctrl Pts',(76.632050345331,-8.73899753144086,57.7307571678895));
#165419=CARTESIAN_POINT('Ctrl Pts',(76.5966327910462,-8.75421122066174,
57.7365669923477));
#165420=CARTESIAN_POINT('Ctrl Pts',(76.5136263863602,-8.78925715945195,
57.7501757716148));
#165421=CARTESIAN_POINT('Ctrl Pts',(76.4659664357693,-8.80891415244796,
57.757983880163));
#165422=CARTESIAN_POINT('Ctrl Pts',(76.3012481704526,-8.87525330624797,
57.7849500283185));
#165423=CARTESIAN_POINT('Ctrl Pts',(76.1834195122918,-8.91994521349711,
57.8042057926309));
#165424=CARTESIAN_POINT('Ctrl Pts',(75.4821847703952,-9.16972679342884,
57.9186130025399));
#165425=CARTESIAN_POINT('Ctrl Pts',(74.8806828286827,-9.31841977507539,
58.0158504841562));
#165426=CARTESIAN_POINT('Ctrl Pts',(74.0251887455363,-9.44114770390028,
58.154604647467));
#165427=CARTESIAN_POINT('Ctrl Pts',(73.7799090336407,-9.46639748679715,
58.194456443081));
#165428=CARTESIAN_POINT('Ctrl Pts',(73.4039365392849,-9.48999050918296,
58.2558643071637));
#165429=CARTESIAN_POINT('Ctrl Pts',(73.2737602961642,-9.49540366951665,
58.2771853229029));
#165430=CARTESIAN_POINT('Ctrl Pts',(73.1060636457311,-9.49883267548552,
58.3047588904063));
#165431=CARTESIAN_POINT('Ctrl Pts',(73.0685954717932,-9.49937111005168,
58.3109265067517));
#165432=CARTESIAN_POINT('Ctrl Pts',(73.0078579930843,-9.49987485773845,
58.3209366329845));
#165433=CARTESIAN_POINT('Ctrl Pts',(72.9845894887032,-9.4999800408816,58.3247744019422));
#165434=CARTESIAN_POINT('Ctrl Pts',(72.9394000510039,-9.5000137932809,58.3322335828487));
#165435=CARTESIAN_POINT('Ctrl Pts',(72.9174793054033,-9.4999522333362,58.3358546435921));
#165436=CARTESIAN_POINT('Ctrl Pts',(72.8685329971397,-9.49964075421995,
58.34394581901));
#165437=CARTESIAN_POINT('Ctrl Pts',(72.8415080465706,-9.49935029565232,
58.3484171788094));
#165438=CARTESIAN_POINT('Ctrl Pts',(72.7480191127264,-9.49793557256114,
58.3638979962211));
#165439=CARTESIAN_POINT('Ctrl Pts',(72.681568961811,-9.49621312767748,58.3749238270209));
#165440=CARTESIAN_POINT('Ctrl Pts',(72.2401001081261,-9.48000410984894,
58.4483000399238));
#165441=CARTESIAN_POINT('Ctrl Pts',(71.8663044416641,-9.44341045802422,
58.5110154141277));
#165442=CARTESIAN_POINT('Ctrl Pts',(71.1799472255596,-9.33373857175741,
58.626223208806));
#165443=CARTESIAN_POINT('Ctrl Pts',(70.8669668489122,-9.26693797821629,
58.6787791897272));
#165444=CARTESIAN_POINT('Ctrl Pts',(70.345705704735,-9.12712855994394,58.7659368782599));
#165445=CARTESIAN_POINT('Ctrl Pts',(70.1355039027462,-9.06266400849372,
58.800980257732));
#165446=CARTESIAN_POINT('Ctrl Pts',(69.7867036701401,-8.94199618926502,
58.858875235428));
#165447=CARTESIAN_POINT('Ctrl Pts',(69.6468593818436,-8.8898161252199,58.8820169457841));
#165448=CARTESIAN_POINT('Ctrl Pts',(69.4530881736079,-8.81215633149435,
58.9139731088817));
#165449=CARTESIAN_POINT('Ctrl Pts',(69.3980940694496,-8.7895021137613,58.923030097148));
#165450=CARTESIAN_POINT('Ctrl Pts',(69.304186625981,-8.74976213341657,58.938473884576));
#165451=CARTESIAN_POINT('Ctrl Pts',(69.2651695850224,-8.73293535947142,
58.9448840077675));
#165452=CARTESIAN_POINT('Ctrl Pts',(69.1861929198891,-8.69823313779756,
58.9578457601869));
#165453=CARTESIAN_POINT('Ctrl Pts',(69.1462411574451,-8.68034180201397,
58.9643956967812));
#165454=CARTESIAN_POINT('Ctrl Pts',(69.0463833524403,-8.63477667329076,
58.9807494089848));
#165455=CARTESIAN_POINT('Ctrl Pts',(68.9866374197206,-8.60674526147473,
58.9905180043304));
#165456=CARTESIAN_POINT('Ctrl Pts',(68.7623644378776,-8.49860556379902,
59.0271272788361));
#165457=CARTESIAN_POINT('Ctrl Pts',(68.5998493962872,-8.41427389444658,
59.0535319548189));
#165458=CARTESIAN_POINT('Ctrl Pts',(68.0050549825197,-8.08311244600899,
59.1497548166022));
#165459=CARTESIAN_POINT('Ctrl Pts',(67.589761679224,-7.80647073900792,59.2160517040286));
#165460=CARTESIAN_POINT('Ctrl Pts',(66.9770061171303,-7.32378912219253,
59.3135578327648));
#165461=CARTESIAN_POINT('Ctrl Pts',(66.763799892022,-7.13977014183352,59.3474297706064));
#165462=CARTESIAN_POINT('Ctrl Pts',(66.5118336070239,-6.90175497267654,
59.3876509196392));
#165463=CARTESIAN_POINT('Ctrl Pts',(66.4650570060535,-6.8566430830874,59.3951266518842));
#165464=CARTESIAN_POINT('Ctrl Pts',(66.3971643764735,-6.78979618803113,
59.40599449451));
#165465=CARTESIAN_POINT('Ctrl Pts',(66.3756841422253,-6.76844174794148,
59.4094355249902));
#165466=CARTESIAN_POINT('Ctrl Pts',(66.3393414064274,-6.73196149866272,
59.4152624260524));
#165467=CARTESIAN_POINT('Ctrl Pts',(66.3244268651676,-6.71688905260032,
59.4176551600178));
#165468=CARTESIAN_POINT('Ctrl Pts',(66.2905247219258,-6.68239573820875,
59.423097503339));
#165469=CARTESIAN_POINT('Ctrl Pts',(66.2715697401444,-6.66294263334712,
59.4261427903341));
#165470=CARTESIAN_POINT('Ctrl Pts',(66.2193479518454,-6.60888280405673,
59.4345387651169));
#165471=CARTESIAN_POINT('Ctrl Pts',(66.1862591988292,-6.57410152573327,
59.4398655088593));
#165472=CARTESIAN_POINT('Ctrl Pts',(65.9895407200568,-6.36413328023457,
59.4715677476172));
#165473=CARTESIAN_POINT('Ctrl Pts',(65.8323053909597,-6.18294182417754,
59.4970470434239));
#165474=CARTESIAN_POINT('Ctrl Pts',(65.4139768909903,-5.66217158899336,
59.564824962373));
#165475=CARTESIAN_POINT('Ctrl Pts',(65.1685917171156,-5.31039660839245,
59.6045502507485));
#165476=CARTESIAN_POINT('Ctrl Pts',(64.8421678676457,-4.76800559669767,
59.6564144319839));
#165477=CARTESIAN_POINT('Ctrl Pts',(64.7424525298315,-4.58962278672968,
59.6720952268352));
#165478=CARTESIAN_POINT('Ctrl Pts',(64.5840594199962,-4.28369563725791,
59.6966455880169));
#165479=CARTESIAN_POINT('Ctrl Pts',(64.5223581216261,-4.15784495367329,
59.706103591619));
#165480=CARTESIAN_POINT('Ctrl Pts',(64.4388942640089,-3.97773640434789,
59.7187304472165));
#165481=CARTESIAN_POINT('Ctrl Pts',(64.4148501530161,-3.92458792715902,
59.7223466376905));
#165482=CARTESIAN_POINT('Ctrl Pts',(64.3740895103105,-3.83225968033606,
59.728438731005));
#165483=CARTESIAN_POINT('Ctrl Pts',(64.3571478838635,-3.79318411912509,
59.7309588142063));
#165484=CARTESIAN_POINT('Ctrl Pts',(64.3229580128775,-3.71286833168708,
59.7360194070704));
#165485=CARTESIAN_POINT('Ctrl Pts',(64.3057364256814,-3.671617581086,59.7385547068335));
#165486=CARTESIAN_POINT('Ctrl Pts',(64.2626582208189,-3.56637601683405,
59.7448608344492));
#165487=CARTESIAN_POINT('Ctrl Pts',(64.2371996887342,-3.5022204508791,59.7485536388536));
#165488=CARTESIAN_POINT('Ctrl Pts',(64.1396494799542,-3.24846897680569,
59.7625658668281));
#165489=CARTESIAN_POINT('Ctrl Pts',(64.0728462955235,-3.05684167186129,
59.7718500956756));
#165490=CARTESIAN_POINT('Ctrl Pts',(63.8302999026047,-2.28335826072466,
59.8042539588884));
#165491=CARTESIAN_POINT('Ctrl Pts',(63.7035572942958,-1.6872577654847,59.8178608246046));
#165492=CARTESIAN_POINT('Ctrl Pts',(63.6042199759272,-0.826161271478044,
59.8235794039326));
#165493=CARTESIAN_POINT('Ctrl Pts',(63.584941015755,-0.568092738134471,
59.8235648025054));
#165494=CARTESIAN_POINT('Ctrl Pts',(63.5740151111343,-0.24842110306705,
59.8216215683852));
#165495=CARTESIAN_POINT('Ctrl Pts',(63.5725096607896,-0.187253550499851,
59.8211629249535));
#165496=CARTESIAN_POINT('Ctrl Pts',(63.5711624976983,-0.0976961981605212,
59.8203678857497));
#165497=CARTESIAN_POINT('Ctrl Pts',(63.5708615335676,-0.0693142617862874,
59.8200977716372));
#165498=CARTESIAN_POINT('Ctrl Pts',(63.5705521286986,-0.0191226706383749,
59.8195884233807));
#165499=CARTESIAN_POINT('Ctrl Pts',(63.5704920855359,0.00268643736458375,
59.8193565502891));
#165500=CARTESIAN_POINT('Ctrl Pts',(63.5705233418788,0.0501471080253307,
59.8188290714159));
#165501=CARTESIAN_POINT('Ctrl Pts',(63.5706431601227,0.0757982329107289,
59.8185293918815));
#165502=CARTESIAN_POINT('Ctrl Pts',(63.571266653737,0.147608961795316,59.8176490302096));
#165503=CARTESIAN_POINT('Ctrl Pts',(63.5720006498833,0.193765439259529,
59.8170352762708));
#165504=CARTESIAN_POINT('Ctrl Pts',(63.5784502802361,0.472730219005996,
59.8130294096185));
#165505=CARTESIAN_POINT('Ctrl Pts',(63.5923046411714,0.705253654915414,
59.8084408079444));
#165506=CARTESIAN_POINT('Ctrl Pts',(63.6594860003008,1.40425150710594,59.7904661814547));
#165507=CARTESIAN_POINT('Ctrl Pts',(63.7385182906675,1.86741632043335,59.7728744661237));
#165508=CARTESIAN_POINT('Ctrl Pts',(63.9320210802418,2.65145158777694,59.73181650814));
#165509=CARTESIAN_POINT('Ctrl Pts',(64.0303980899176,2.97552323593261,59.7113795106899));
#165510=CARTESIAN_POINT('Ctrl Pts',(64.1786056606585,3.384757610258,59.6808504330921));
#165511=CARTESIAN_POINT('Ctrl Pts',(64.2130174665081,3.4754611109181,59.6737771000189));
#165512=CARTESIAN_POINT('Ctrl Pts',(64.2674468321649,3.61262476229139,59.6626089507711));
#165513=CARTESIAN_POINT('Ctrl Pts',(64.2864728454777,3.65948703939793,59.6587084964783));
#165514=CARTESIAN_POINT('Ctrl Pts',(64.3202760882699,3.74089414323485,59.6517842797708));
#165515=CARTESIAN_POINT('Ctrl Pts',(64.334888444784,3.77550891937578,59.6487928633556));
#165516=CARTESIAN_POINT('Ctrl Pts',(64.3683257847376,3.85343641493831,59.6419515151001));
#165517=CARTESIAN_POINT('Ctrl Pts',(64.3872673913714,3.8966959826217,59.638078705817));
#165518=CARTESIAN_POINT('Ctrl Pts',(64.4395780297585,4.01380194499636,59.6273904696222));
#165519=CARTESIAN_POINT('Ctrl Pts',(64.4735612223689,4.08735854101666,59.620454614892));
#165520=CARTESIAN_POINT('Ctrl Pts',(64.6920282388881,4.5448871158386,59.5759160712281));
#165521=CARTESIAN_POINT('Ctrl Pts',(64.9008496716447,4.91622406437002,59.5335288811215));
#165522=CARTESIAN_POINT('Ctrl Pts',(65.3021916909747,5.52972072239749,59.4528495573519));
#165523=CARTESIAN_POINT('Ctrl Pts',(65.4831327492413,5.77893126066466,59.4166994414878));
#165524=CARTESIAN_POINT('Ctrl Pts',(65.7743387200406,6.14135779497294,59.3591727318873));
#165525=CARTESIAN_POINT('Ctrl Pts',(65.8759260072531,6.26150186322094,59.3392122245946));
#165526=CARTESIAN_POINT('Ctrl Pts',(66.0247073585395,6.42876363235173,59.3101816008895));
#165527=CARTESIAN_POINT('Ctrl Pts',(66.0694945033245,6.47804861258835,59.3014675179556));
#165528=CARTESIAN_POINT('Ctrl Pts',(66.1499567393336,6.56472028971193,59.2858615364453));
#165529=CARTESIAN_POINT('Ctrl Pts',(66.1854260945617,6.60229945594327,59.2789986377992));
#165530=CARTESIAN_POINT('Ctrl Pts',(66.2403193947665,6.65950313591282,59.2684049029855));
#165531=CARTESIAN_POINT('Ctrl Pts',(66.2595251783984,6.67934105018914,59.2647034915859));
#165532=CARTESIAN_POINT('Ctrl Pts',(66.2951834870417,6.71584869304943,59.2578410516431));
#165533=CARTESIAN_POINT('Ctrl Pts',(66.3116115446323,6.73254233068394,59.2546833021266));
#165534=CARTESIAN_POINT('Ctrl Pts',(66.3494284177101,6.77068336620272,59.2474228628374));
#165535=CARTESIAN_POINT('Ctrl Pts',(66.3708584232646,6.79208837954643,59.2433147354011));
#165536=CARTESIAN_POINT('Ctrl Pts',(66.4400423635843,6.86052450730752,59.2300709566091));
#165537=CARTESIAN_POINT('Ctrl Pts',(66.4881923278073,6.90714194437685,59.2208821445063));
#165538=CARTESIAN_POINT('Ctrl Pts',(66.7752858461878,7.17918920175889,59.1662392248061));
#165539=CARTESIAN_POINT('Ctrl Pts',(67.0253014182388,7.39228551958493,59.1192318487562));
#165540=CARTESIAN_POINT('Ctrl Pts',(67.5034472448691,7.75822600399336,59.0296645377486));
#165541=CARTESIAN_POINT('Ctrl Pts',(67.7281875487765,7.91504007874153,58.9876878795011));
#165542=CARTESIAN_POINT('Ctrl Pts',(68.146618551493,8.18041205986879,58.9094577242688));
#165543=CARTESIAN_POINT('Ctrl Pts',(68.3379754705029,8.29239626911787,58.8736555114032));
#165544=CARTESIAN_POINT('Ctrl Pts',(68.663183631851,8.46742300652365,58.812673695601));
#165545=CARTESIAN_POINT('Ctrl Pts',(68.7949331382456,8.53432572416359,58.7879333130593));
#165546=CARTESIAN_POINT('Ctrl Pts',(68.9814384712572,8.62349745290284,58.7528481575374));
#165547=CARTESIAN_POINT('Ctrl Pts',(69.0349368293633,8.64845105545213,58.7427771152779));
#165548=CARTESIAN_POINT('Ctrl Pts',(69.1271664341179,8.69040220825668,58.7254023231396));
#165549=CARTESIAN_POINT('Ctrl Pts',(69.1657862312919,8.70765039960893,58.7181231292446));
#165550=CARTESIAN_POINT('Ctrl Pts',(69.2398247200556,8.74011063280711,58.7041607633761));
#165551=CARTESIAN_POINT('Ctrl Pts',(69.2752236142209,8.75536749592927,58.6974819722294));
#165552=CARTESIAN_POINT('Ctrl Pts',(69.3676642982094,8.79452643052515,58.6800326065029));
#165553=CARTESIAN_POINT('Ctrl Pts',(69.4248471276524,8.81807638992534,58.6692303525148));
#165554=CARTESIAN_POINT('Ctrl Pts',(69.6255041614652,8.89837022196516,58.6312958932814));
#165555=CARTESIAN_POINT('Ctrl Pts',(69.7701161991164,8.95207794735394,58.6039050835263));
#165556=CARTESIAN_POINT('Ctrl Pts',(70.6011859479906,9.23725048906812,58.4462252347092));
#165557=CARTESIAN_POINT('Ctrl Pts',(71.3106780489233,9.3905309173788,58.3103429840408));
#165558=CARTESIAN_POINT('Ctrl Pts',(72.2449468095197,9.47926456171249,58.1328559682745));
#165559=CARTESIAN_POINT('Ctrl Pts',(72.4599516368399,9.49206922263139,58.0921278131034));
#165560=CARTESIAN_POINT('Ctrl Pts',(72.7186518143162,9.49835056324411,58.0433913083779));
#165561=CARTESIAN_POINT('Ctrl Pts',(72.7620738516078,9.49909645472195,58.0352201700255));
#165562=CARTESIAN_POINT('Ctrl Pts',(72.8300183963571,9.49978114026535,58.0224501711866));
#165563=CARTESIAN_POINT('Ctrl Pts',(72.8545369998379,9.49992994799619,58.0178451772617));
#165564=CARTESIAN_POINT('Ctrl Pts',(72.9006137882423,9.50002493860347,58.0091975680271));
#165565=CARTESIAN_POINT('Ctrl Pts',(72.9221714581237,9.49999342872577,58.00515431673));
#165566=CARTESIAN_POINT('Ctrl Pts',(72.972237131677,9.49974386434254,57.9957702280188));
#165567=CARTESIAN_POINT('Ctrl Pts',(73.0007449635042,9.4994689461167,57.9904313259286));
#165568=CARTESIAN_POINT('Ctrl Pts',(73.0944403425512,9.49812885153303,57.9728979660669));
#165569=CARTESIAN_POINT('Ctrl Pts',(73.1596213860029,9.49650203545229,57.9607224300517));
#165570=CARTESIAN_POINT('Ctrl Pts',(73.6905987997138,9.47758921615189,57.8616886448402));
#165571=CARTESIAN_POINT('Ctrl Pts',(74.1547034234038,9.42554973535961,57.7760402505727));
#165572=CARTESIAN_POINT('Ctrl Pts',(74.976701941755,9.269418330822,57.6241005958556));
#165573=CARTESIAN_POINT('Ctrl Pts',(75.3360069089991,9.17843376406987,57.5576039317642));
#165574=CARTESIAN_POINT('Ctrl Pts',(75.8226786152275,9.02344725629384,57.4669836179226));
#165575=CARTESIAN_POINT('Ctrl Pts',(75.9553995694799,8.97781831081514,57.4422141097941));
#165576=CARTESIAN_POINT('Ctrl Pts',(76.1871659049851,8.89217458746428,57.3988439013957));
#165577=CARTESIAN_POINT('Ctrl Pts',(76.2866456572561,8.85343931488086,57.3801900238829));
#165578=CARTESIAN_POINT('Ctrl Pts',(76.4336824453425,8.79322826421129,57.352557772604));
#165579=CARTESIAN_POINT('Ctrl Pts',(76.4817550428722,8.77306563835036,57.3435138373673));
#165580=CARTESIAN_POINT('Ctrl Pts',(76.5675866365434,8.73620838376513,57.3273484743898));
#165581=CARTESIAN_POINT('Ctrl Pts',(76.6054080296809,8.71966618636268,57.3202190156399));
#165582=CARTESIAN_POINT('Ctrl Pts',(76.6856813345046,8.68391360245852,57.3050738440368));
#165583=CARTESIAN_POINT('Ctrl Pts',(76.7281020312591,8.66463418988177,57.2970622928444));
#165584=CARTESIAN_POINT('Ctrl Pts',(76.8426614179813,8.61152008301531,57.2754048764274));
#165585=CARTESIAN_POINT('Ctrl Pts',(76.9145172207303,8.57706941804644,57.261796945921));
#165586=CARTESIAN_POINT('Ctrl Pts',(77.3325421105607,8.36996425748812,57.1824958930809));
#165587=CARTESIAN_POINT('Ctrl Pts',(77.6682672510631,8.17655306018609,57.1182350869084));
#165588=CARTESIAN_POINT('Ctrl Pts',(78.3312476390071,7.73726114210876,56.9905613950194));
#165589=CARTESIAN_POINT('Ctrl Pts',(78.6564104796808,7.48961277926842,56.92750984377));
#165590=CARTESIAN_POINT('Ctrl Pts',(79.0522314517669,7.14501840411167,56.8508670390811));
#165591=CARTESIAN_POINT('Ctrl Pts',(79.1383460244719,7.0671947692833,56.8342015903395));
#165592=CARTESIAN_POINT('Ctrl Pts',(79.2803633647217,6.9339911678635,56.8067593531978));
#165593=CARTESIAN_POINT('Ctrl Pts',(79.3370361894769,6.87948480197323,56.7958200432123));
#165594=CARTESIAN_POINT('Ctrl Pts',(79.4162520879116,6.80136525864896,56.7805534928331));
#165595=CARTESIAN_POINT('Ctrl Pts',(79.4393531020409,6.77834638070063,56.7761044202744));
#165596=CARTESIAN_POINT('Ctrl Pts',(79.4789944061098,6.73843429083015,56.7684756399244));
#165597=CARTESIAN_POINT('Ctrl Pts',(79.4955902603309,6.72159904241294,56.7652836436591));
#165598=CARTESIAN_POINT('Ctrl Pts',(79.5306951413774,6.68571922095411,56.7585357184119));
#165599=CARTESIAN_POINT('Ctrl Pts',(79.5491876312736,6.66665832687759,56.7549834124743));
#165600=CARTESIAN_POINT('Ctrl Pts',(79.5999882052794,6.61385237897887,56.7452307976009));
#165601=CARTESIAN_POINT('Ctrl Pts',(79.6321300693549,6.57994177901792,56.7390668921501));
#165602=CARTESIAN_POINT('Ctrl Pts',(79.8040858434861,6.39580631426493,56.7061201172949));
#165603=CARTESIAN_POINT('Ctrl Pts',(79.9393158075709,6.24120296649171,56.6803154441407));
#165604=CARTESIAN_POINT('Ctrl Pts',(80.3381543162808,5.75408163218469,56.6042483564325));
#165605=CARTESIAN_POINT('Ctrl Pts',(80.5847868217296,5.40786272369264,56.5572470308202));
#165606=CARTESIAN_POINT('Ctrl Pts',(80.9272043107022,4.85161065398208,56.4910595926873));
#165607=CARTESIAN_POINT('Ctrl Pts',(81.039838065784,4.65295149327204,56.4690996094166));
#165608=CARTESIAN_POINT('Ctrl Pts',(81.2151400404554,4.31602767871536,56.4344871328666));
#165609=CARTESIAN_POINT('Ctrl Pts',(81.2818261734697,4.18003010464455,56.4211983095346));
#165610=CARTESIAN_POINT('Ctrl Pts',(81.3703830547394,3.98797118853472,56.4033581788618));
#165611=CARTESIAN_POINT('Ctrl Pts',(81.3949950949096,3.93323980533567,56.3983772483707));
#165612=CARTESIAN_POINT('Ctrl Pts',(81.4362896825713,3.83904195294486,56.3899796958115));
#165613=CARTESIAN_POINT('Ctrl Pts',(81.4532248170859,3.7996917995099,56.3865235370366));
#165614=CARTESIAN_POINT('Ctrl Pts',(81.485044986955,3.72436107648079,56.3800056294664));
#165615=CARTESIAN_POINT('Ctrl Pts',(81.4999757761343,3.68840140854937,56.3769367318689));
#165616=CARTESIAN_POINT('Ctrl Pts',(81.5344447817902,3.60392884233406,56.3698267634644));
#165617=CARTESIAN_POINT('Ctrl Pts',(81.5538059317664,3.55534275064033,56.3658134551046));
#165618=CARTESIAN_POINT('Ctrl Pts',(81.6199209245155,3.38538030802865,56.3520386517122));
#165619=CARTESIAN_POINT('Ctrl Pts',(81.6646015774089,3.26318715824792,56.3426025471791));
#165620=CARTESIAN_POINT('Ctrl Pts',(81.9081947070157,2.55232658456308,56.2903944682411));
#165621=CARTESIAN_POINT('Ctrl Pts',(82.0519999541262,1.94575083504966,56.2562514419592));
#165622=CARTESIAN_POINT('Ctrl Pts',(82.1700432709274,1.08265002634678,56.2233954359544));
#165623=CARTESIAN_POINT('Ctrl Pts',(82.1942092311057,0.834886255511459,
56.215747290998));
#165624=CARTESIAN_POINT('Ctrl Pts',(82.2165188377026,0.454913275955093,
56.2069402107331));
#165625=CARTESIAN_POINT('Ctrl Pts',(82.221554786607,0.323249158030819,56.2044227986111));
#165626=CARTESIAN_POINT('Ctrl Pts',(82.2245833168324,0.153572390931381,
56.2018960425162));
#165627=CARTESIAN_POINT('Ctrl Pts',(82.2250378102207,0.115625620642261,
56.2013771506365));
#165628=CARTESIAN_POINT('Ctrl Pts',(82.2254136705754,0.0541009240409631,
56.2006116824008));
#165629=CARTESIAN_POINT('Ctrl Pts',(82.2254717611267,0.0305246054823433,
56.2003364058397));
#165630=CARTESIAN_POINT('Ctrl Pts',(82.2254412063335,0.00463207216118171,
56.2000540655189));
#165631=CARTESIAN_POINT('Ctrl Pts',(82.2254376442054,0.00231603550137483,
56.2000289862928));
#165632=CARTESIAN_POINT('Ctrl Pts',(82.2254332530441,4.44666969874771E-12,
56.2000040827795));
#165633=CARTESIAN_POINT('Origin',(73.0915550886457,-4.33680868994202E-16,
59.1075264962884));
#165634=CARTESIAN_POINT('',(82.1046676540618,-3.33476494482013E-11,55.5151083368357));
#165635=CARTESIAN_POINT('',(82.1125619375607,3.32220049501518E-11,55.5598790433222));
#165636=CARTESIAN_POINT('',(82.4472287422617,-1.59709532818419E-15,57.4578688084528));
#165637=CARTESIAN_POINT('Ctrl Pts',(82.1046676540618,-6.66937018010743E-11,
55.5151083368358));
#165638=CARTESIAN_POINT('Ctrl Pts',(82.1046831372505,0.0081663167848822,
55.515196146362));
#165639=CARTESIAN_POINT('Ctrl Pts',(82.1046881878999,0.0163326525156036,
55.5152854286388));
#165640=CARTESIAN_POINT('Ctrl Pts',(82.1046659042388,0.0501509387005742,
55.5156612874468));
#165641=CARTESIAN_POINT('Ctrl Pts',(82.1045460728912,0.0758025391846987,
55.5159609740892));
#165642=CARTESIAN_POINT('Ctrl Pts',(82.1039225209125,0.147615866527537,
55.5168413727629));
#165643=CARTESIAN_POINT('Ctrl Pts',(82.1031884526744,0.193774466373888,
55.5174551604751));
#165644=CARTESIAN_POINT('Ctrl Pts',(82.0967372734946,0.472792206847775,
55.521461835382));
#165645=CARTESIAN_POINT('Ctrl Pts',(82.0828777668914,0.705366327036288,
55.5260517536033));
#165646=CARTESIAN_POINT('Ctrl Pts',(82.0156816707158,1.40439261100474,55.5440290744549));
#165647=CARTESIAN_POINT('Ctrl Pts',(81.9366466032295,1.86753543376037,55.561621141297));
#165648=CARTESIAN_POINT('Ctrl Pts',(81.7431472263391,2.65152174651733,55.6026781636042));
#165649=CARTESIAN_POINT('Ctrl Pts',(81.6447761325593,2.97556669470496,55.6231139082363));
#165650=CARTESIAN_POINT('Ctrl Pts',(81.4965783113512,3.38477164741177,55.6536409687357));
#165651=CARTESIAN_POINT('Ctrl Pts',(81.4621677317308,3.47547154308474,55.6607140485646));
#165652=CARTESIAN_POINT('Ctrl Pts',(81.4077399467971,3.61263090299337,55.6718818724966));
#165653=CARTESIAN_POINT('Ctrl Pts',(81.388714192095,3.6594924557385,55.6757822735029));
#165654=CARTESIAN_POINT('Ctrl Pts',(81.3549112287724,3.74089876470706,55.6827064325909));
#165655=CARTESIAN_POINT('Ctrl Pts',(81.340298882702,3.77551346599158,55.6856978467158));
#165656=CARTESIAN_POINT('Ctrl Pts',(81.3068613116053,3.85344139111431,55.6925392419322));
#165657=CARTESIAN_POINT('Ctrl Pts',(81.2879194550937,3.89670145941487,55.6964121020932));
#165658=CARTESIAN_POINT('Ctrl Pts',(81.2356074432632,4.01381028176885,55.707100618256));
#165659=CARTESIAN_POINT('Ctrl Pts',(81.2016230747816,4.08736921194466,55.7140367123288));
#165660=CARTESIAN_POINT('Ctrl Pts',(80.9830923733534,4.54502939209053,55.7585882335667));
#165661=CARTESIAN_POINT('Ctrl Pts',(80.774191550578,4.91648662986971,55.800991498181));
#165662=CARTESIAN_POINT('Ctrl Pts',(80.3725625843288,5.53035930142778,55.8817279775636));
#165663=CARTESIAN_POINT('Ctrl Pts',(80.1914036554021,5.77981803456371,55.9179211194196));
#165664=CARTESIAN_POINT('Ctrl Pts',(79.9001286772755,6.14221806075194,55.9754595280785));
#165665=CARTESIAN_POINT('Ctrl Pts',(79.7987260380884,6.26211867664327,55.9953832139142));
#165666=CARTESIAN_POINT('Ctrl Pts',(79.6501945337465,6.42908120607563,56.0243646572932));
#165667=CARTESIAN_POINT('Ctrl Pts',(79.6054624396068,6.4783015434828,56.0330679262799));
#165668=CARTESIAN_POINT('Ctrl Pts',(79.5250902268847,6.56487146582401,56.0486563213353));
#165669=CARTESIAN_POINT('Ctrl Pts',(79.4896551364686,6.60241286861436,56.055512549177));
#165670=CARTESIAN_POINT('Ctrl Pts',(79.4348038664856,6.65957145977612,56.0660981355676));
#165671=CARTESIAN_POINT('Ctrl Pts',(79.415605311105,6.67940152823924,56.06979814269));
#165672=CARTESIAN_POINT('Ctrl Pts',(79.3799531745488,6.71590227784108,56.0766593775266));
#165673=CARTESIAN_POINT('Ctrl Pts',(79.3635239862352,6.73259679424968,56.0798173360737));
#165674=CARTESIAN_POINT('Ctrl Pts',(79.3256952573172,6.77074915242421,56.0870800326776));
#165675=CARTESIAN_POINT('Ctrl Pts',(79.3042544320404,6.7921645138499,56.0911902208889));
#165676=CARTESIAN_POINT('Ctrl Pts',(79.2349996431662,6.86066892745571,56.1044475115628));
#165677=CARTESIAN_POINT('Ctrl Pts',(79.1867885175033,6.90734310605114,56.1136479282141));
#165678=CARTESIAN_POINT('Ctrl Pts',(78.8976964697032,7.18126229419028,56.1686706934064));
#165679=CARTESIAN_POINT('Ctrl Pts',(78.645559001247,7.39596465874361,56.2160723888613));
#165680=CARTESIAN_POINT('Ctrl Pts',(78.1619015270093,7.76544087215151,56.3066664954445));
#165681=CARTESIAN_POINT('Ctrl Pts',(77.933738825979,7.9241295867861,56.3492802804894));
#165682=CARTESIAN_POINT('Ctrl Pts',(77.5149074666914,8.18850050147076,56.4275886032426));
#165683=CARTESIAN_POINT('Ctrl Pts',(77.3268952595357,8.29815221108524,56.4627679327325));
#165684=CARTESIAN_POINT('Ctrl Pts',(77.0067828052513,8.47009189980756,56.5227972191076));
#165685=CARTESIAN_POINT('Ctrl Pts',(76.8766863766069,8.53606849880377,56.5472281349927));
#165686=CARTESIAN_POINT('Ctrl Pts',(76.6921247735683,8.62426000440992,56.5819482073274));
#165687=CARTESIAN_POINT('Ctrl Pts',(76.6388805668218,8.64908349941913,56.5919715400614));
#165688=CARTESIAN_POINT('Ctrl Pts',(76.5469519373623,8.69088307927248,56.6092898055402));
#165689=CARTESIAN_POINT('Ctrl Pts',(76.5083770192802,8.70810549192532,56.616560609147));
#165690=CARTESIAN_POINT('Ctrl Pts',(76.4343297779943,8.74055935311842,56.6305247489454));
#165691=CARTESIAN_POINT('Ctrl Pts',(76.3988766978219,8.75583431961461,56.6372138274678));
#165692=CARTESIAN_POINT('Ctrl Pts',(76.3152861227901,8.79123101965565,56.6529927835154));
#165693=CARTESIAN_POINT('Ctrl Pts',(76.2670746326234,8.81116716675332,56.6620992907729));
#165694=CARTESIAN_POINT('Ctrl Pts',(76.0977892732844,8.87949795525368,56.6940956311411));
#165695=CARTESIAN_POINT('Ctrl Pts',(75.9758933647215,8.92572653882055,56.7171718631662));
#165696=CARTESIAN_POINT('Ctrl Pts',(75.2776492345973,9.17375978534379,56.8495538811731));
#165697=CARTESIAN_POINT('Ctrl Pts',(74.6840739425484,9.32031763958669,56.9629710726892));
#165698=CARTESIAN_POINT('Ctrl Pts',(73.8391287839856,9.44160111273542,57.1239553230159));
#165699=CARTESIAN_POINT('Ctrl Pts',(73.5963183040112,9.46662071876087,57.1701471231172));
#165700=CARTESIAN_POINT('Ctrl Pts',(73.2237691952166,9.49003939628665,57.2406995557542));
#165701=CARTESIAN_POINT('Ctrl Pts',(73.0945879536231,9.49542146990205,57.2651043896395));
#165702=CARTESIAN_POINT('Ctrl Pts',(72.928053995339,9.49883599086951,57.2964588184468));
#165703=CARTESIAN_POINT('Ctrl Pts',(72.8907787502528,9.4993730333388,57.3034699553758));
#165704=CARTESIAN_POINT('Ctrl Pts',(72.8303327293459,9.49987551265791,57.3148271185292));
#165705=CARTESIAN_POINT('Ctrl Pts',(72.807164317804,9.49998036921824,57.3191773133001));
#165706=CARTESIAN_POINT('Ctrl Pts',(72.7621527105507,9.50001363679289,57.3276229509993));
#165707=CARTESIAN_POINT('Ctrl Pts',(72.740309809437,9.49995180678593,57.3317186564709));
#165708=CARTESIAN_POINT('Ctrl Pts',(72.6915203269276,9.49963953831488,57.3408612233654));
#165709=CARTESIAN_POINT('Ctrl Pts',(72.6645738958548,9.49934840727279,57.3459067001559));
#165710=CARTESIAN_POINT('Ctrl Pts',(72.5712792404284,9.49792957809917,57.3633624175714));
#165711=CARTESIAN_POINT('Ctrl Pts',(72.5049384604776,9.49620114058441,57.3757524555154));
#165712=CARTESIAN_POINT('Ctrl Pts',(72.0593651423265,9.47975728250069,57.4588421737555));
#165713=CARTESIAN_POINT('Ctrl Pts',(71.6811945947327,9.44226038275326,57.5287569015261));
#165714=CARTESIAN_POINT('Ctrl Pts',(70.9739692781486,9.3275776154078,57.6594673389788));
#165715=CARTESIAN_POINT('Ctrl Pts',(70.6447295853202,9.25546248748561,57.7203015539361));
#165716=CARTESIAN_POINT('Ctrl Pts',(70.1224736982051,9.11064479072532,57.8172237670461));
#165717=CARTESIAN_POINT('Ctrl Pts',(69.9267089411425,9.0492544918558,57.8536510059286));
#165718=CARTESIAN_POINT('Ctrl Pts',(69.5992900501307,8.93444408773968,57.9148035215196));
#165719=CARTESIAN_POINT('Ctrl Pts',(69.4665475187724,8.88443107039321,57.9396606190141));
#165720=CARTESIAN_POINT('Ctrl Pts',(69.2810064387629,8.80959638202293,57.9745055375095));
#165721=CARTESIAN_POINT('Ctrl Pts',(69.2272295146504,8.7873127720697,57.9846170245872));
#165722=CARTESIAN_POINT('Ctrl Pts',(69.1348783782127,8.74801777648703,58.0020027698529));
#165723=CARTESIAN_POINT('Ctrl Pts',(69.0962053286749,8.73124896084119,58.0092897352786));
#165724=CARTESIAN_POINT('Ctrl Pts',(69.0222280031529,8.69856865200554,58.0232414644762));
#165725=CARTESIAN_POINT('Ctrl Pts',(68.9869066647666,8.68269892143716,58.0299084195651));
#165726=CARTESIAN_POINT('Ctrl Pts',(68.903793248601,8.64472670475603,58.0456093004335));
#165727=CARTESIAN_POINT('Ctrl Pts',(68.8560864770542,8.62243607656902,58.0546318394442));
#165728=CARTESIAN_POINT('Ctrl Pts',(68.6880416112906,8.54216209003482,58.0864495549736));
#165729=CARTESIAN_POINT('Ctrl Pts',(68.5687505773935,8.48196965267659,58.1091026585753));
#165730=CARTESIAN_POINT('Ctrl Pts',(67.8620360902405,8.10595933642776,58.2436841110684));
#165731=CARTESIAN_POINT('Ctrl Pts',(67.3081640330838,7.72964916123593,58.3509193445901));
#165732=CARTESIAN_POINT('Ctrl Pts',(66.6919868223647,7.20644801995258,58.4702599631192));
#165733=CARTESIAN_POINT('Ctrl Pts',(66.5877223417527,7.11383692795435,58.4904483094891));
#165734=CARTESIAN_POINT('Ctrl Pts',(66.4197861244975,6.95784719479171,58.5229115247445));
#165735=CARTESIAN_POINT('Ctrl Pts',(66.3549175998932,6.89584140615282,58.5354372139019));
#165736=CARTESIAN_POINT('Ctrl Pts',(66.2664560913634,6.80883177659919,58.5524884106032));
#165737=CARTESIAN_POINT('Ctrl Pts',(66.2421150705354,6.78462733301814,58.5571769721059));
#165738=CARTESIAN_POINT('Ctrl Pts',(66.2010356331124,6.74333005224545,58.5650833981811));
#165739=CARTESIAN_POINT('Ctrl Pts',(66.1842304851331,6.72630683448447,58.5683160154738));
#165740=CARTESIAN_POINT('Ctrl Pts',(66.1494220374238,6.6907776199164,58.5750076626894));
#165741=CARTESIAN_POINT('Ctrl Pts',(66.1314294404848,6.67226116211173,58.5784643550833));
#165742=CARTESIAN_POINT('Ctrl Pts',(66.0834453141416,6.62247302469418,58.587677477598));
#165743=CARTESIAN_POINT('Ctrl Pts',(66.0535898977672,6.5910655260915,58.5934040525778));
#165744=CARTESIAN_POINT('Ctrl Pts',(65.9159484399966,6.44425865080944,58.6197826292321));
#165745=CARTESIAN_POINT('Ctrl Pts',(65.8107995817224,6.32632082078509,58.6398697160837));
#165746=CARTESIAN_POINT('Ctrl Pts',(65.447187312382,5.89730224878749,58.7092560063207));
#165747=CARTESIAN_POINT('Ctrl Pts',(65.2055034651842,5.5720571763071,58.7552481396823));
#165748=CARTESIAN_POINT('Ctrl Pts',(64.7808138047891,4.91669049455642,58.8369564969829));
#165749=CARTESIAN_POINT('Ctrl Pts',(64.5952023813503,4.58922749354895,58.8731033986191));
#165750=CARTESIAN_POINT('Ctrl Pts',(64.3849917464723,4.16100425652833,58.9149934297197));
#165751=CARTESIAN_POINT('Ctrl Pts',(64.3420553102035,4.06991394828237,58.9236086251639));
#165752=CARTESIAN_POINT('Ctrl Pts',(64.2794368460239,3.93141580287353,58.9362687519412));
#165753=CARTESIAN_POINT('Ctrl Pts',(64.258685942999,3.8845146726464,58.9404811439993));
#165754=CARTESIAN_POINT('Ctrl Pts',(64.2217726030343,3.79922974446169,58.9480062209492));
#165755=CARTESIAN_POINT('Ctrl Pts',(64.2054818540183,3.76090469970925,58.951338978688));
#165756=CARTESIAN_POINT('Ctrl Pts',(64.1709011699647,3.67804817051531,58.9584393886893));
#165757=CARTESIAN_POINT('Ctrl Pts',(64.1526958543573,3.63348150617339,58.9621937671403));
#165758=CARTESIAN_POINT('Ctrl Pts',(64.1040270418712,3.51171581159866,58.9722758391137));
#165759=CARTESIAN_POINT('Ctrl Pts',(64.0742290339685,3.43424684793218,58.9784991616309));
#165760=CARTESIAN_POINT('Ctrl Pts',(63.8821866410214,2.91486465460458,59.0189543440854));
#165761=CARTESIAN_POINT('Ctrl Pts',(63.7516782296472,2.46153848179776,59.0482232182268));
#165762=CARTESIAN_POINT('Ctrl Pts',(63.5850256595648,1.66677409635791,59.0888193295504));
#165763=CARTESIAN_POINT('Ctrl Pts',(63.5328667405273,1.32975184675359,59.1028295217104));
#165764=CARTESIAN_POINT('Ctrl Pts',(63.4732790652233,0.739351186250466,
59.1213514861095));
#165765=CARTESIAN_POINT('Ctrl Pts',(63.4577808905696,0.487180544235924,
59.1273738831734));
#165766=CARTESIAN_POINT('Ctrl Pts',(63.451130350729,0.188969836213798,59.1320893438065));
#165767=CARTESIAN_POINT('Ctrl Pts',(63.4504344815118,0.143273027569161,
59.1327452370923));
#165768=CARTESIAN_POINT('Ctrl Pts',(63.44985533765,0.0723001197369106,59.1336587975064));
#165769=CARTESIAN_POINT('Ctrl Pts',(63.4497478738907,0.0470271383427463,
59.1339634119294));
#165770=CARTESIAN_POINT('Ctrl Pts',(63.4497315844953,-0.000111857181628876,
59.1344926467005));
#165771=CARTESIAN_POINT('Ctrl Pts',(63.4497979227852,-0.0219774458935335,
59.1347224763209));
#165772=CARTESIAN_POINT('Ctrl Pts',(63.4501207371716,-0.0723079847418672,
59.1352156021532));
#165773=CARTESIAN_POINT('Ctrl Pts',(63.4504285637723,-0.100772441046243,
59.1354680870719));
#165774=CARTESIAN_POINT('Ctrl Pts',(63.4518247001461,-0.192520906325654,
59.1361976654566));
#165775=CARTESIAN_POINT('Ctrl Pts',(63.4534070938291,-0.255796486702477,
59.1365716201473));
#165776=CARTESIAN_POINT('Ctrl Pts',(63.4734969926213,-0.832898076404157,
59.1388295792473));
#165777=CARTESIAN_POINT('Ctrl Pts',(63.532248671359,-1.34450388879123,59.1325340977909));
#165778=CARTESIAN_POINT('Ctrl Pts',(63.6993547987218,-2.19348172572141,
59.1102140452665));
#165779=CARTESIAN_POINT('Ctrl Pts',(63.7859840566445,-2.53407443213869,
59.0979090671673));
#165780=CARTESIAN_POINT('Ctrl Pts',(63.9523549740527,-3.06450153426549,
59.0737571105813));
#165781=CARTESIAN_POINT('Ctrl Pts',(64.0198954654271,-3.25790799180822,
59.0638571323772));
#165782=CARTESIAN_POINT('Ctrl Pts',(64.1177203463775,-3.5115913955153,59.0494341331305));
#165783=CARTESIAN_POINT('Ctrl Pts',(64.1425305199046,-3.57396758640219,
59.0457698072429));
#165784=CARTESIAN_POINT('Ctrl Pts',(64.1847994231312,-3.67706542313569,
59.0395171815474));
#165785=CARTESIAN_POINT('Ctrl Pts',(64.2018896681755,-3.71793896794379,
59.0369866118446));
#165786=CARTESIAN_POINT('Ctrl Pts',(64.2358664409931,-3.79763866887981,
59.0319509276408));
#165787=CARTESIAN_POINT('Ctrl Pts',(64.2527281633351,-3.83647451939185,
59.0294496941545));
#165788=CARTESIAN_POINT('Ctrl Pts',(64.2938328790742,-3.92945162299446,
59.0233471949904));
#165789=CARTESIAN_POINT('Ctrl Pts',(64.318321969458,-3.98347956943434,59.0197073794883));
#165790=CARTESIAN_POINT('Ctrl Pts',(64.4005075619662,-4.16039963263101,
59.0074785224434));
#165791=CARTESIAN_POINT('Ctrl Pts',(64.4603109116928,-4.28227123182679,
58.9985590624346));
#165792=CARTESIAN_POINT('Ctrl Pts',(64.8302564832783,-4.99722774000309,
58.9432396329212));
#165793=CARTESIAN_POINT('Ctrl Pts',(65.1991912428121,-5.55704924364375,
58.8876724094771));
#165794=CARTESIAN_POINT('Ctrl Pts',(65.713789053458,-6.18341508401888,58.8076088935999));
#165795=CARTESIAN_POINT('Ctrl Pts',(65.807055753738,-6.29185438975616,58.7930065567522));
#165796=CARTESIAN_POINT('Ctrl Pts',(65.9638401994224,-6.46603793241588,
58.7682668419714));
#165797=CARTESIAN_POINT('Ctrl Pts',(66.0259450869616,-6.53306410259867,
58.7584201202982));
#165798=CARTESIAN_POINT('Ctrl Pts',(66.1128893669043,-6.62422429119724,
58.7445602906985));
#165799=CARTESIAN_POINT('Ctrl Pts',(66.136921722301,-6.64914757106302,58.7407215974516));
#165800=CARTESIAN_POINT('Ctrl Pts',(66.1778565703575,-6.69113787880428,
58.7341693510924));
#165801=CARTESIAN_POINT('Ctrl Pts',(66.1946897427538,-6.70827445305186,
58.7314710617903));
#165802=CARTESIAN_POINT('Ctrl Pts',(66.2297466646922,-6.7436933071832,58.7258432743214));
#165803=CARTESIAN_POINT('Ctrl Pts',(66.2479800694958,-6.76196523509998,
58.7229116486028));
#165804=CARTESIAN_POINT('Ctrl Pts',(66.2968630664495,-6.81055323044644,
58.7150404917573));
#165805=CARTESIAN_POINT('Ctrl Pts',(66.3276428317794,-6.84073279924547,
58.7100722633174));
#165806=CARTESIAN_POINT('Ctrl Pts',(66.4697229047843,-6.97815348490206,
58.6870882135298));
#165807=CARTESIAN_POINT('Ctrl Pts',(66.5833881581997,-7.08282897644763,
58.6685600972062));
#165808=CARTESIAN_POINT('Ctrl Pts',(67.0598541869205,-7.50048208756614,
58.5904995629257));
#165809=CARTESIAN_POINT('Ctrl Pts',(67.443275480518,-7.78804695485937,58.5268146046099));
#165810=CARTESIAN_POINT('Ctrl Pts',(68.0396253335662,-8.16769251134123,
58.4279738930985));
#165811=CARTESIAN_POINT('Ctrl Pts',(68.2369862389141,-8.28338278802693,
58.3952868361985));
#165812=CARTESIAN_POINT('Ctrl Pts',(68.5714886110786,-8.46328341855298,
58.3400288204572));
#165813=CARTESIAN_POINT('Ctrl Pts',(68.706342788626,-8.53163420263656,58.3177878010472));
#165814=CARTESIAN_POINT('Ctrl Pts',(68.8966402770467,-8.6223335520558,58.2864672673073));
#165815=CARTESIAN_POINT('Ctrl Pts',(68.95074948605,-8.64748745445042,58.2775686487063));
#165816=CARTESIAN_POINT('Ctrl Pts',(69.0438255446409,-8.68967224322549,
58.262274386077));
#165817=CARTESIAN_POINT('Ctrl Pts',(69.0826762131982,-8.70696044170122,
58.2558941936876));
#165818=CARTESIAN_POINT('Ctrl Pts',(69.1570157440917,-8.73943209192528,
58.2436932119723));
#165819=CARTESIAN_POINT('Ctrl Pts',(69.1924836493893,-8.75466234255305,
58.2378751893835));
#165820=CARTESIAN_POINT('Ctrl Pts',(69.2757473516295,-8.78980424494869,
58.2242243807533));
#165821=CARTESIAN_POINT('Ctrl Pts',(69.3236153746011,-8.80953781953575,
58.2163822968633));
#165822=CARTESIAN_POINT('Ctrl Pts',(69.4897749866052,-8.87641871399374,
58.1891806589193));
#165823=CARTESIAN_POINT('Ctrl Pts',(69.6088545500402,-8.92152877525408,
58.1697211654617));
#165824=CARTESIAN_POINT('Ctrl Pts',(70.3101291570692,-9.17082972819739,
58.0553132013703));
#165825=CARTESIAN_POINT('Ctrl Pts',(70.9102826091913,-9.31893795512639,
57.9582944622942));
#165826=CARTESIAN_POINT('Ctrl Pts',(71.764016064951,-9.44127115823504,57.819824825256));
#165827=CARTESIAN_POINT('Ctrl Pts',(72.0089382817627,-9.46645823239192,
57.7800306574467));
#165828=CARTESIAN_POINT('Ctrl Pts',(72.3844319472909,-9.49000379832992,
57.71870062551));
#165829=CARTESIAN_POINT('Ctrl Pts',(72.5144890092581,-9.49540850518504,
57.6973990288106));
#165830=CARTESIAN_POINT('Ctrl Pts',(72.6820546923221,-9.49883357520942,
57.6698469575177));
#165831=CARTESIAN_POINT('Ctrl Pts',(72.7195112113965,-9.49937163194484,
57.6636812529279));
#165832=CARTESIAN_POINT('Ctrl Pts',(72.7802344656364,-9.49987503546522,
57.6536734635712));
#165833=CARTESIAN_POINT('Ctrl Pts',(72.8035004016127,-9.49998013002439,
57.6498361156224));
#165834=CARTESIAN_POINT('Ctrl Pts',(72.8486888084411,-9.50001375096868,
57.6423771003517));
#165835=CARTESIAN_POINT('Ctrl Pts',(72.8706110917601,-9.49995211783509,
57.6387557832221));
#165836=CARTESIAN_POINT('Ctrl Pts',(72.9195649160004,-9.49964042486989,
57.6306633598357));
#165837=CARTESIAN_POINT('Ctrl Pts',(72.9465958440896,-9.4993497841532,57.6261910072101));
#165838=CARTESIAN_POINT('Ctrl Pts',(73.0401252756043,-9.49793394946541,
57.6107034682325));
#165839=CARTESIAN_POINT('Ctrl Pts',(73.1066099269781,-9.49620988285458,
57.5996718911103));
#165840=CARTESIAN_POINT('Ctrl Pts',(73.5497324598121,-9.47993281031314,
57.5260206290239));
#165841=CARTESIAN_POINT('Ctrl Pts',(73.9251347111281,-9.44307601256934,
57.4630331891849));
#165842=CARTESIAN_POINT('Ctrl Pts',(74.6182284293805,-9.33194263293071,
57.3466939766465));
#165843=CARTESIAN_POINT('Ctrl Pts',(74.9362728467005,-9.26359772317145,
57.29328888963));
#165844=CARTESIAN_POINT('Ctrl Pts',(75.5643524840488,-9.09362735020921,
57.1882896720197));
#165845=CARTESIAN_POINT('Ctrl Pts',(75.8739539255729,-8.99209655483669,
57.1367692950126));
#165846=CARTESIAN_POINT('Ctrl Pts',(76.2493713887129,-8.84674209398468,
57.0747537356981));
#165847=CARTESIAN_POINT('Ctrl Pts',(76.3206236207922,-8.81813636116631,
57.0630038745012));
#165848=CARTESIAN_POINT('Ctrl Pts',(76.434073051199,-8.77095282666222,57.0443292166408));
#165849=CARTESIAN_POINT('Ctrl Pts',(76.4764930731016,-8.75294016323587,
57.0373541744268));
#165850=CARTESIAN_POINT('Ctrl Pts',(76.5569017188852,-8.71809049907456,
57.0241473977026));
#165851=CARTESIAN_POINT('Ctrl Pts',(76.5949140495991,-8.70131304058684,
57.0179103189341));
#165852=CARTESIAN_POINT('Ctrl Pts',(76.681585926515,-8.66236474551072,57.0037035963794));
#165853=CARTESIAN_POINT('Ctrl Pts',(76.7301717221771,-8.64002748184918,
56.9957501951603));
#165854=CARTESIAN_POINT('Ctrl Pts',(76.8575062155302,-8.58015464658321,
56.9749333050698));
#165855=CARTESIAN_POINT('Ctrl Pts',(76.9359347137147,-8.54192645023717,
56.9621396337513));
#165856=CARTESIAN_POINT('Ctrl Pts',(77.5027763721314,-8.25573693285314,
56.8698722743975));
#165857=CARTESIAN_POINT('Ctrl Pts',(77.9696845222031,-7.96606661635586,
56.7950366509687));
#165858=CARTESIAN_POINT('Ctrl Pts',(78.7086770974681,-7.412474549301,56.6773091172826));
#165859=CARTESIAN_POINT('Ctrl Pts',(78.9948260910236,-7.17017542567809,
56.631910123448));
#165860=CARTESIAN_POINT('Ctrl Pts',(79.3051312050996,-6.87385812327918,
56.5823445978682));
#165861=CARTESIAN_POINT('Ctrl Pts',(79.3440108968386,-6.83608389584711,
56.5761275783788));
#165862=CARTESIAN_POINT('Ctrl Pts',(79.4026074612306,-6.77816131282105,
56.5667448560018));
#165863=CARTESIAN_POINT('Ctrl Pts',(79.4225611359854,-6.75825927064249,
56.5635474787788));
#165864=CARTESIAN_POINT('Ctrl Pts',(79.4589415917199,-6.72164567551471,
56.5577131659297));
#165865=CARTESIAN_POINT('Ctrl Pts',(79.4753954821686,-6.70496226249003,
56.5550726376095));
#165866=CARTESIAN_POINT('Ctrl Pts',(79.5129227598308,-6.66662639344478,
56.5490461415989));
#165867=CARTESIAN_POINT('Ctrl Pts',(79.5339549054514,-6.64493327170735,
56.5456656563551));
#165868=CARTESIAN_POINT('Ctrl Pts',(79.5996144994989,-6.57655524275546,
56.5351039944811));
#165869=CARTESIAN_POINT('Ctrl Pts',(79.6438705318666,-6.52950854742274,
56.5279731602701));
#165870=CARTESIAN_POINT('Ctrl Pts',(79.9855428791404,-6.15873494632548,
56.4728501572721));
#165871=CARTESIAN_POINT('Ctrl Pts',(80.260728051821,-5.81478797497322,56.4280549634609));
#165872=CARTESIAN_POINT('Ctrl Pts',(80.7938629293535,-5.04443120862511,
56.3421351942791));
#165873=CARTESIAN_POINT('Ctrl Pts',(81.0443246187931,-4.61429916332988,
56.3023587383068));
#165874=CARTESIAN_POINT('Ctrl Pts',(81.2962839137847,-4.09212441356338,
56.263880837066));
#165875=CARTESIAN_POINT('Ctrl Pts',(81.3311071477423,-4.01751901645962,
56.2586031812913));
#165876=CARTESIAN_POINT('Ctrl Pts',(81.3845258927951,-3.89912838455132,
56.2505745858118));
#165877=CARTESIAN_POINT('Ctrl Pts',(81.4037593434249,-3.85564413146906,
56.2476985052862));
#165878=CARTESIAN_POINT('Ctrl Pts',(81.439283128616,-3.77369193169898,56.2424146519987));
#165879=CARTESIAN_POINT('Ctrl Pts',(81.4556465687234,-3.73525785157648,
56.2399925163393));
#165880=CARTESIAN_POINT('Ctrl Pts',(81.4919254014947,-3.64848326151286,
56.2346495645819));
#165881=CARTESIAN_POINT('Ctrl Pts',(81.5116987919796,-3.6000831566221,56.2317565795328));
#165882=CARTESIAN_POINT('Ctrl Pts',(81.5701357584086,-3.45364820506756,
56.223265848742));
#165883=CARTESIAN_POINT('Ctrl Pts',(81.6075896679452,-3.35512585625018,
56.2179050820122));
#165884=CARTESIAN_POINT('Ctrl Pts',(81.8441821977068,-2.70062994864765,
56.1845966892776));
#165885=CARTESIAN_POINT('Ctrl Pts',(81.9936263514858,-2.12757611206901,
56.1664208804195));
#165886=CARTESIAN_POINT('Ctrl Pts',(82.1596767102879,-1.11909655564106,
56.151342744878));
#165887=CARTESIAN_POINT('Ctrl Pts',(82.2011112941517,-0.689618758341124,
56.1499948221716));
#165888=CARTESIAN_POINT('Ctrl Pts',(82.215011841021,-0.208411550980801,
56.1532962934307));
#165889=CARTESIAN_POINT('Ctrl Pts',(82.2160710233358,-0.157971248743679,
56.1537009227633));
#165890=CARTESIAN_POINT('Ctrl Pts',(82.217076659079,-0.081253318392736,
56.1544033351846));
#165891=CARTESIAN_POINT('Ctrl Pts',(82.2173131050438,-0.0549800076835477,
56.1546593992613));
#165892=CARTESIAN_POINT('Ctrl Pts',(82.2174883617966,-0.0191374724957702,
56.1550296195407));
#165893=CARTESIAN_POINT('Ctrl Pts',(82.2175208274001,-0.00956873354244861,
56.1551304870759));
#165894=CARTESIAN_POINT('Ctrl Pts',(82.2175389695453,-7.70179830244106E-11,
56.1552333762936));
#165895=CARTESIAN_POINT('Ctrl Pts',(82.2254332530441,4.44666969874771E-12,
56.2000040827795));
#165896=CARTESIAN_POINT('Ctrl Pts',(82.2253955162052,-0.0199035864588712,
56.1997900665309));
#165897=CARTESIAN_POINT('Ctrl Pts',(82.2252965522329,-0.0398070870381526,
56.1995890272647));
#165898=CARTESIAN_POINT('Ctrl Pts',(82.2249157684035,-0.0871137839519527,
56.1991418195417));
#165899=CARTESIAN_POINT('Ctrl Pts',(82.2245790953923,-0.114516504828974,
56.1989071958335));
#165900=CARTESIAN_POINT('Ctrl Pts',(82.2230119138865,-0.209353958669355,
56.1981789048622));
#165901=CARTESIAN_POINT('Ctrl Pts',(82.2211941976636,-0.276777880483236,
56.1978076317294));
#165902=CARTESIAN_POINT('Ctrl Pts',(82.204333910507,-0.727478752833875,
56.196282364896));
#165903=CARTESIAN_POINT('Ctrl Pts',(82.1672510969061,-1.10959181644738,
56.1996048160965));
#165904=CARTESIAN_POINT('Ctrl Pts',(82.0557041387056,-1.81713780611838,
56.2133622885313));
#165905=CARTESIAN_POINT('Ctrl Pts',(81.9869103648884,-2.14289188473711,
56.2227894455887));
#165906=CARTESIAN_POINT('Ctrl Pts',(81.8178229056863,-2.77840528625268,
56.2468536484031));
#165907=CARTESIAN_POINT('Ctrl Pts',(81.7183993652482,-3.08793791222269,
56.2613499728732));
#165908=CARTESIAN_POINT('Ctrl Pts',(81.5761387521535,-3.46400593713413,
56.2823008088395));
#165909=CARTESIAN_POINT('Ctrl Pts',(81.5479180886168,-3.5359623843275,56.2864656992188));
#165910=CARTESIAN_POINT('Ctrl Pts',(81.5013383007465,-3.65062476754098,
56.2933527663705));
#165911=CARTESIAN_POINT('Ctrl Pts',(81.4835323305294,-3.69355676183597,
56.2959882599742));
#165912=CARTESIAN_POINT('Ctrl Pts',(81.4490588683304,-3.77499364385461,
56.3010958269628));
#165913=CARTESIAN_POINT('Ctrl Pts',(81.432449278758,-3.8135224077732,56.3035588362739));
#165914=CARTESIAN_POINT('Ctrl Pts',(81.3938545960449,-3.90145308925757,
56.3092867861315));
#165915=CARTESIAN_POINT('Ctrl Pts',(81.3717035388202,-3.9507788578324,56.3125777225235));
#165916=CARTESIAN_POINT('Ctrl Pts',(81.3122469461368,-4.08022628791294,
56.3214201090177));
#165917=CARTESIAN_POINT('Ctrl Pts',(81.2742493685627,-4.16001674333413,
56.3270800786198));
#165918=CARTESIAN_POINT('Ctrl Pts',(80.9929389801881,-4.73022065043414,
56.3690516585816));
#165919=CARTESIAN_POINT('Ctrl Pts',(80.7091515037419,-5.1990457639627,56.411670866996));
#165920=CARTESIAN_POINT('Ctrl Pts',(80.1632985133085,-5.94727017028107,
56.4953519264619));
#165921=CARTESIAN_POINT('Ctrl Pts',(79.9215006325915,-6.24016071407357,
56.5328718526995));
#165922=CARTESIAN_POINT('Ctrl Pts',(79.6260668652627,-6.55733592235234,
56.5797659783561));
#165923=CARTESIAN_POINT('Ctrl Pts',(79.5886785386282,-6.59679099859632,
56.5857185875736));
#165924=CARTESIAN_POINT('Ctrl Pts',(79.5313772010698,-6.6562294461383,56.5948712450172));
#165925=CARTESIAN_POINT('Ctrl Pts',(79.5117063169185,-6.6764527770008,56.5980184681503));
#165926=CARTESIAN_POINT('Ctrl Pts',(79.4755347925571,-6.71331003224424,
56.6038156651583));
#165927=CARTESIAN_POINT('Ctrl Pts',(79.4590618219615,-6.72997143915911,
56.606459565508));
#165928=CARTESIAN_POINT('Ctrl Pts',(79.4212306585479,-6.76795298820711,
56.6125399695534));
#165929=CARTESIAN_POINT('Ctrl Pts',(79.3998329159405,-6.78923176041793,
56.6159852278508));
#165930=CARTESIAN_POINT('Ctrl Pts',(79.3324587409256,-6.85559469885949,
56.6268512048442));
#165931=CARTESIAN_POINT('Ctrl Pts',(79.2861306689006,-6.90030655555888,
56.6343489896785));
#165932=CARTESIAN_POINT('Ctrl Pts',(78.9146862544009,-7.2515465451748,56.694644277855));
#165933=CARTESIAN_POINT('Ctrl Pts',(78.5690707915128,-7.53481074161679,
56.7518050996022));
#165934=CARTESIAN_POINT('Ctrl Pts',(77.8076719151865,-8.07302690735746,
56.8779693187153));
#165935=CARTESIAN_POINT('Ctrl Pts',(77.3895128398198,-8.32222894540669,
56.9473698915649));
#165936=CARTESIAN_POINT('Ctrl Pts',(76.8809355490933,-8.57375966340547,
57.0311738505378));
#165937=CARTESIAN_POINT('Ctrl Pts',(76.8072632540691,-8.60899784913653,
57.0433010510237));
#165938=CARTESIAN_POINT('Ctrl Pts',(76.6903687544093,-8.66303131409896,
57.0625213902721));
#165939=CARTESIAN_POINT('Ctrl Pts',(76.6474457059946,-8.68247781399196,
57.06957445866));
#165940=CARTESIAN_POINT('Ctrl Pts',(76.566561211271,-8.71838489330554,57.0828565240553));
#165941=CARTESIAN_POINT('Ctrl Pts',(76.5286334552846,-8.73492015715773,
57.0890810567793));
#165942=CARTESIAN_POINT('Ctrl Pts',(76.4430160384094,-8.77156866829192,
57.1031239821759));
#165943=CARTESIAN_POINT('Ctrl Pts',(76.395267320709,-8.79153750841962,57.1109500011659));
#165944=CARTESIAN_POINT('Ctrl Pts',(76.2508549171489,-8.85052004741923,
57.1346019131531));
#165945=CARTESIAN_POINT('Ctrl Pts',(76.1537081368881,-8.88830405527304,
57.1504893590829));
#165946=CARTESIAN_POINT('Ctrl Pts',(75.5067039672198,-9.12749706667559,
57.2561516370138));
#165947=CARTESIAN_POINT('Ctrl Pts',(74.9397802215985,-9.27805352121886,
57.3479215953453));
#165948=CARTESIAN_POINT('Ctrl Pts',(73.9439667610207,-9.44389509369572,
57.5093074319521));
#165949=CARTESIAN_POINT('Ctrl Pts',(73.5210000827707,-9.48476412561141,
57.5779457722092));
#165950=CARTESIAN_POINT('Ctrl Pts',(73.047144466932,-9.4978486805272,57.6557592949775));
#165951=CARTESIAN_POINT('Ctrl Pts',(72.9973819656997,-9.49882102592703,
57.6639425322809));
#165952=CARTESIAN_POINT('Ctrl Pts',(72.9216943573471,-9.49968903325272,
57.6764087503415));
#165953=CARTESIAN_POINT('Ctrl Pts',(72.8957718895608,-9.49987734448565,
57.680681856886));
#165954=CARTESIAN_POINT('Ctrl Pts',(72.8483832736218,-9.50002237968127,
57.6885002767504));
#165955=CARTESIAN_POINT('Ctrl Pts',(72.8269174283608,-9.50001334844315,
57.692044405234));
#165956=CARTESIAN_POINT('Ctrl Pts',(72.7782415360183,-9.49982340758179,
57.7000868573998));
#165957=CARTESIAN_POINT('Ctrl Pts',(72.7510322551577,-9.49959714264678,
57.704586564061));
#165958=CARTESIAN_POINT('Ctrl Pts',(72.680143022119,-9.49869473362846,57.7163197378305));
#165959=CARTESIAN_POINT('Ctrl Pts',(72.636467052151,-9.49782915050843,57.7235585642748));
#165960=CARTESIAN_POINT('Ctrl Pts',(72.2488883797173,-9.48739972769602,
57.7878738130109));
#165961=CARTESIAN_POINT('Ctrl Pts',(71.9058274434864,-9.4589580807626,57.845340194433));
#165962=CARTESIAN_POINT('Ctrl Pts',(70.9881031441345,-9.33101752781764,
57.9993182455476));
#165963=CARTESIAN_POINT('Ctrl Pts',(70.4197804593559,-9.19619900314946,
58.0948653460216));
#165964=CARTESIAN_POINT('Ctrl Pts',(69.7159478974758,-8.95740017155845,
58.2117748411039));
#165965=CARTESIAN_POINT('Ctrl Pts',(69.5658995930875,-8.90213758300391,
58.2366196633658));
#165966=CARTESIAN_POINT('Ctrl Pts',(69.3589219203545,-8.81979211963938,
58.270766107965));
#165967=CARTESIAN_POINT('Ctrl Pts',(69.3007710173797,-8.79597260492069,
58.2803457710644));
#165968=CARTESIAN_POINT('Ctrl Pts',(69.2070877663521,-8.75648712924794,
58.2957559864126));
#165969=CARTESIAN_POINT('Ctrl Pts',(69.1714091763204,-8.74118619755758,
58.3016194186712));
#165970=CARTESIAN_POINT('Ctrl Pts',(69.0970364615773,-8.70873966856432,
58.3138303997084));
#165971=CARTESIAN_POINT('Ctrl Pts',(69.0583608280893,-8.69155237292025,
58.3201738779777));
#165972=CARTESIAN_POINT('Ctrl Pts',(68.9664597646636,-8.64996066596164,
58.3352316354396));
#165973=CARTESIAN_POINT('Ctrl Pts',(68.9133412761308,-8.62531586063123,
58.3439223826436));
#165974=CARTESIAN_POINT('Ctrl Pts',(68.730647609949,-8.53845511514459,58.3737697325573));
#165975=CARTESIAN_POINT('Ctrl Pts',(68.6022456828645,-8.47373231820895,
58.3946711154594));
#165976=CARTESIAN_POINT('Ctrl Pts',(68.2876309439214,-8.30593524448026,
58.4457063579273));
#165977=CARTESIAN_POINT('Ctrl Pts',(68.1032959641086,-8.19939567851772,
58.4754482386249));
#165978=CARTESIAN_POINT('Ctrl Pts',(67.683390104038,-7.93722237801352,58.5429044841003));
#165979=CARTESIAN_POINT('Ctrl Pts',(67.4508270479315,-7.77701183523437,
58.580036018487));
#165980=CARTESIAN_POINT('Ctrl Pts',(66.9572753802927,-7.40312119395153,
58.6586383908438));
#165981=CARTESIAN_POINT('Ctrl Pts',(66.6997767536239,-7.18535010465191,
58.699512471634));
#165982=CARTESIAN_POINT('Ctrl Pts',(66.405273990402,-6.90781887102201,58.7465173880349));
#165983=CARTESIAN_POINT('Ctrl Pts',(66.3566607637489,-6.86101043103078,
58.7542857612975));
#165984=CARTESIAN_POINT('Ctrl Pts',(66.2868647553706,-6.79234423523244,
58.7654575914626));
#165985=CARTESIAN_POINT('Ctrl Pts',(66.2652823576705,-6.77090441929182,
58.768914770285));
#165986=CARTESIAN_POINT('Ctrl Pts',(66.2272199959874,-6.73272525092269,
58.775016997003));
#165987=CARTESIAN_POINT('Ctrl Pts',(66.2106985487345,-6.7160286307236,58.7776675293043));
#165988=CARTESIAN_POINT('Ctrl Pts',(66.1748659220609,-6.67954406521607,
58.7834201664776));
#165989=CARTESIAN_POINT('Ctrl Pts',(66.1555789469824,-6.65973244490992,
58.7865190376159));
#165990=CARTESIAN_POINT('Ctrl Pts',(66.1005243044022,-6.60267993284934,
58.7953712476851));
#165991=CARTESIAN_POINT('Ctrl Pts',(66.0649728854007,-6.56522726138834,
58.8010954656928));
#165992=CARTESIAN_POINT('Ctrl Pts',(65.7565366276555,-6.23490498020041,
58.8508132727081));
#165993=CARTESIAN_POINT('Ctrl Pts',(65.5020490795595,-5.92502819383749,
58.8922054022425));
#165994=CARTESIAN_POINT('Ctrl Pts',(64.9597925342817,-5.1723311809188,58.979809576188));
#165995=CARTESIAN_POINT('Ctrl Pts',(64.6875876356503,-4.71962774960106,
59.0232680778935));
#165996=CARTESIAN_POINT('Ctrl Pts',(64.4140003988791,-4.16582397143773,
59.0652657993448));
#165997=CARTESIAN_POINT('Ctrl Pts',(64.3753492468967,-4.08473939659121,
59.071152542755));
#165998=CARTESIAN_POINT('Ctrl Pts',(64.3153268503904,-3.95413642661544,
59.0802148035751));
#165999=CARTESIAN_POINT('Ctrl Pts',(64.2932291289846,-3.90496796953349,
59.0835327507685));
#166000=CARTESIAN_POINT('Ctrl Pts',(64.2546305702355,-3.81711575259759,
59.0892944688107));
#166001=CARTESIAN_POINT('Ctrl Pts',(64.2379685302801,-3.7785065003449,59.0917698858875));
#166002=CARTESIAN_POINT('Ctrl Pts',(64.2035733188108,-3.69734723674761,
59.0968546319753));
#166003=CARTESIAN_POINT('Ctrl Pts',(64.1858914669361,-3.6547760371065,59.0994539134053));
#166004=CARTESIAN_POINT('Ctrl Pts',(64.140050284931,-3.54212984967439,59.1061531492582));
#166005=CARTESIAN_POINT('Ctrl Pts',(64.1124065295386,-3.47184266590105,
59.1101520607643));
#166006=CARTESIAN_POINT('Ctrl Pts',(63.9798027934927,-3.12267875624334,
59.1291260463045));
#166007=CARTESIAN_POINT('Ctrl Pts',(63.8869542553808,-2.83925523774258,
59.1417289170361));
#166008=CARTESIAN_POINT('Ctrl Pts',(63.7129069177458,-2.21089146099731,
59.1637793026284));
#166009=CARTESIAN_POINT('Ctrl Pts',(63.6372555378738,-1.86483676705409,
59.1721779357039));
#166010=CARTESIAN_POINT('Ctrl Pts',(63.5180956564049,-1.12714682735523,
59.1828106063956));
#166011=CARTESIAN_POINT('Ctrl Pts',(63.4791919297343,-0.735415082438569,
59.1842481822503));
#166012=CARTESIAN_POINT('Ctrl Pts',(63.4618343046548,-0.273853639113625,
59.1816777182735));
#166013=CARTESIAN_POINT('Ctrl Pts',(63.4599906839625,-0.205259520316795,
59.1811859786441));
#166014=CARTESIAN_POINT('Ctrl Pts',(63.4584507715836,-0.109880378036844,
59.180354428042));
#166015=CARTESIAN_POINT('Ctrl Pts',(63.4581306047383,-0.0831067375661545,
59.1801048217527));
#166016=CARTESIAN_POINT('Ctrl Pts',(63.4577511232452,-0.0342698018506897,
59.1796203810379));
#166017=CARTESIAN_POINT('Ctrl Pts',(63.4576558191881,-0.0122068709101067,
59.1793906833755));
#166018=CARTESIAN_POINT('Ctrl Pts',(63.4576159489983,0.0337218633400005,
59.1788901583135));
#166019=CARTESIAN_POINT('Ctrl Pts',(63.457684329794,0.057587392495471,59.1786174763401));
#166020=CARTESIAN_POINT('Ctrl Pts',(63.4581008010244,0.120712245365185,
59.1778624818704));
#166021=CARTESIAN_POINT('Ctrl Pts',(63.4586008700874,0.159969842269242,
59.1773584203561));
#166022=CARTESIAN_POINT('Ctrl Pts',(63.4620960595867,0.345128205376628,
59.1748148461257));
#166023=CARTESIAN_POINT('Ctrl Pts',(63.468178171613,0.490944708985161,59.1723247478192));
#166024=CARTESIAN_POINT('Ctrl Pts',(63.4965488189744,0.93045841966588,59.163244855723));
#166025=CARTESIAN_POINT('Ctrl Pts',(63.5290179378633,1.22328611112202,59.1550636036953));
#166026=CARTESIAN_POINT('Ctrl Pts',(63.6686181643724,2.10929532762212,59.1230494862041));
#166027=CARTESIAN_POINT('Ctrl Pts',(63.8179937930836,2.69401063654907,59.0917808437044));
#166028=CARTESIAN_POINT('Ctrl Pts',(64.0554570573112,3.35730063841636,59.0428391276018));
#166029=CARTESIAN_POINT('Ctrl Pts',(64.0917292030743,3.45370334411235,59.0353808334483));
#166030=CARTESIAN_POINT('Ctrl Pts',(64.1487974626554,3.59827835157036,59.023668808162));
#166031=CARTESIAN_POINT('Ctrl Pts',(64.1684558640806,3.64690931156324,59.0196380582994));
#166032=CARTESIAN_POINT('Ctrl Pts',(64.2044678011045,3.73393536353802,59.0122604959219));
#166033=CARTESIAN_POINT('Ctrl Pts',(64.2206759275625,3.77239154330483,59.0089422111169));
#166034=CARTESIAN_POINT('Ctrl Pts',(64.2557944637189,3.8542191385288,59.0017569413866));
#166035=CARTESIAN_POINT('Ctrl Pts',(64.274775525406,3.89755777175095,58.9978760985742));
#166036=CARTESIAN_POINT('Ctrl Pts',(64.3273031571468,4.01511558334929,58.9871436296259));
#166037=CARTESIAN_POINT('Ctrl Pts',(64.3614721754089,4.0890409679415,58.9801699512999));
#166038=CARTESIAN_POINT('Ctrl Pts',(64.5992607382395,4.58673075596616,58.9316933437187));
#166039=CARTESIAN_POINT('Ctrl Pts',(64.8326852170686,4.99494823534751,58.8843238715129));
#166040=CARTESIAN_POINT('Ctrl Pts',(65.358300816401,5.77412544274659,58.7788790045957));
#166041=CARTESIAN_POINT('Ctrl Pts',(65.649988220925,6.14384609553888,58.7209169826352));
#166042=CARTESIAN_POINT('Ctrl Pts',(66.0097675065149,6.53558542780356,58.6510273826178));
#166043=CARTESIAN_POINT('Ctrl Pts',(66.05222831445,6.58090687953461,58.6428023858132));
#166044=CARTESIAN_POINT('Ctrl Pts',(66.1156504345957,6.64726820658499,58.6305549699009));
#166045=CARTESIAN_POINT('Ctrl Pts',(66.1362708934304,6.66864003795814,58.62657877699));
#166046=CARTESIAN_POINT('Ctrl Pts',(66.1732828920289,6.70663752490071,58.6194527015869));
#166047=CARTESIAN_POINT('Ctrl Pts',(66.1896360034283,6.7233009746769,58.616307941506));
#166048=CARTESIAN_POINT('Ctrl Pts',(66.2260668866879,6.76014664358343,58.6093105369019));
#166049=CARTESIAN_POINT('Ctrl Pts',(66.2461741871432,6.78029827867692,58.6054539918353));
#166050=CARTESIAN_POINT('Ctrl Pts',(66.3059925588714,6.83970444268061,58.593996417753));
#166051=CARTESIAN_POINT('Ctrl Pts',(66.3459598583983,6.87869254361963,58.5863611320225));
#166052=CARTESIAN_POINT('Ctrl Pts',(66.4394146701516,6.96824093468274,58.5685489086856));
#166053=CARTESIAN_POINT('Ctrl Pts',(66.4931511128061,7.01852921551875,58.5583375366121));
#166054=CARTESIAN_POINT('Ctrl Pts',(66.6829009485287,7.19195270944137,58.5223697847538));
#166055=CARTESIAN_POINT('Ctrl Pts',(66.8218921440944,7.31167686861458,58.4961810736965));
#166056=CARTESIAN_POINT('Ctrl Pts',(67.4356645422906,7.80970632140385,58.380913421749));
#166057=CARTESIAN_POINT('Ctrl Pts',(67.9425461031012,8.14487508335537,58.2865552367253));
#166058=CARTESIAN_POINT('Ctrl Pts',(68.5921948127466,8.48867485512041,58.1646835488871));
#166059=CARTESIAN_POINT('Ctrl Pts',(68.7080953465377,8.54693471289744,58.142912691477));
#166060=CARTESIAN_POINT('Ctrl Pts',(68.8719258426988,8.62502866111454,58.1120904502235));
#166061=CARTESIAN_POINT('Ctrl Pts',(68.9188907261812,8.64693427662143,58.1032493063875));
#166062=CARTESIAN_POINT('Ctrl Pts',(69.0010780212418,8.68443250504215,58.0877676998032));
#166063=CARTESIAN_POINT('Ctrl Pts',(69.0362212648362,8.70020266442263,58.0811446666722));
#166064=CARTESIAN_POINT('Ctrl Pts',(69.1101901815239,8.73284265346263,58.0671979567376));
#166065=CARTESIAN_POINT('Ctrl Pts',(69.1490345705707,8.74966607146115,58.0598700918789));
#166066=CARTESIAN_POINT('Ctrl Pts',(69.2424866468514,8.78938097557269,58.0422313740177));
#166067=CARTESIAN_POINT('Ctrl Pts',(69.2971975807493,8.81201435652634,58.0318973295296));
#166068=CARTESIAN_POINT('Ctrl Pts',(69.4897458104812,8.88951323494433,57.9955013836361));
#166069=CARTESIAN_POINT('Ctrl Pts',(69.6286431754133,8.94156962665868,57.9691988128118));
#166070=CARTESIAN_POINT('Ctrl Pts',(69.9748682489228,9.06190106629557,57.9035264465876));
#166071=CARTESIAN_POINT('Ctrl Pts',(70.1834304044669,9.12618978726953,57.863870368685));
#166072=CARTESIAN_POINT('Ctrl Pts',(70.7028002024069,9.26629221478336,57.7649666553917));
#166073=CARTESIAN_POINT('Ctrl Pts',(71.0155745061857,9.33339916284094,57.705270111172));
#166074=CARTESIAN_POINT('Ctrl Pts',(71.7005761738355,9.44334972702121,57.5746884034147));
#166075=CARTESIAN_POINT('Ctrl Pts',(72.0732182454311,9.47999121557342,57.5037495315944));
#166076=CARTESIAN_POINT('Ctrl Pts',(72.513290420408,9.49621256482875,57.4206877415447));
#166077=CARTESIAN_POINT('Ctrl Pts',(72.5794908998034,9.49793529243034,57.4082120144596));
#166078=CARTESIAN_POINT('Ctrl Pts',(72.6726276418172,9.49935020822693,57.3906918969534));
#166079=CARTESIAN_POINT('Ctrl Pts',(72.6995497270857,9.49964069820312,57.3856312785984));
#166080=CARTESIAN_POINT('Ctrl Pts',(72.7483092080848,9.49995221351492,57.3764730155845));
#166081=CARTESIAN_POINT('Ctrl Pts',(72.7701459677609,9.50001378619696,57.3723741342232));
#166082=CARTESIAN_POINT('Ctrl Pts',(72.8151615606201,9.4999800559609,57.3639300826564));
#166083=CARTESIAN_POINT('Ctrl Pts',(72.8383402134398,9.49987488822714,57.3595852674416));
#166084=CARTESIAN_POINT('Ctrl Pts',(72.8988418013406,9.49937119930833,57.3482518546046));
#166085=CARTESIAN_POINT('Ctrl Pts',(72.9361640276583,9.49883283030553,57.3412679960177));
#166086=CARTESIAN_POINT('Ctrl Pts',(73.10319284995,9.49540451543168,57.3100436522301));
#166087=CARTESIAN_POINT('Ctrl Pts',(73.2328486573126,9.48999284421492,57.2858883954586));
#166088=CARTESIAN_POINT('Ctrl Pts',(73.6072928003073,9.46640790572726,57.216291097849));
#166089=CARTESIAN_POINT('Ctrl Pts',(73.8515669108966,9.441168921131,57.1710879382823));
#166090=CARTESIAN_POINT('Ctrl Pts',(74.7034632924967,9.31850590757357,57.0135927396289));
#166091=CARTESIAN_POINT('Ctrl Pts',(75.3023796762721,9.16990982265294,56.9030231328975));
#166092=CARTESIAN_POINT('Ctrl Pts',(76.0007690120131,8.92021274348208,56.7724941712806));
#166093=CARTESIAN_POINT('Ctrl Pts',(76.1183267105528,8.87545021938119,56.7504709276739));
#166094=CARTESIAN_POINT('Ctrl Pts',(76.2826085955656,8.80901992753693,56.7196150568381));
#166095=CARTESIAN_POINT('Ctrl Pts',(76.330106822762,8.78934997369507,56.7106843669005));
#166096=CARTESIAN_POINT('Ctrl Pts',(76.4128125868205,8.75428783924872,56.69511709506));
#166097=CARTESIAN_POINT('Ctrl Pts',(76.4480914823061,8.73907136046434,56.6884713459493));
#166098=CARTESIAN_POINT('Ctrl Pts',(76.522118476229,8.70659275695773,56.6745149012532));
#166099=CARTESIAN_POINT('Ctrl Pts',(76.5608451456952,8.68928278384494,56.6672070542079));
#166100=CARTESIAN_POINT('Ctrl Pts',(76.6537825333726,8.6469715533625,56.6496534405775));
#166101=CARTESIAN_POINT('Ctrl Pts',(76.7078753199147,8.62170940100036,56.6394233953001));
#166102=CARTESIAN_POINT('Ctrl Pts',(76.8990236621945,8.53017444644027,56.6032266241227));
#166103=CARTESIAN_POINT('Ctrl Pts',(77.0347113767622,8.46102951430872,56.5774457164988));
#166104=CARTESIAN_POINT('Ctrl Pts',(77.372188359274,8.2784308202126,56.513120628478));
#166105=CARTESIAN_POINT('Ctrl Pts',(77.5715967846075,8.16067677074287,56.4749214948603));
#166106=CARTESIAN_POINT('Ctrl Pts',(78.1435115207567,7.79343686371792,56.3649417854438));
#166107=CARTESIAN_POINT('Ctrl Pts',(78.5029051506694,7.52414998124982,56.2952553351274));
#166108=CARTESIAN_POINT('Ctrl Pts',(78.9731276143691,7.11592841205867,56.2042026624885));
#166109=CARTESIAN_POINT('Ctrl Pts',(79.1011037590377,6.99844373604352,56.1794400529462));
#166110=CARTESIAN_POINT('Ctrl Pts',(79.2579034729459,6.84628899232401,56.1491920621841));
#166111=CARTESIAN_POINT('Ctrl Pts',(79.289764636081,6.81492843323477,56.1430507643067));
#166112=CARTESIAN_POINT('Ctrl Pts',(79.3398887488457,6.76488519594189,56.1333987718262));
#166113=CARTESIAN_POINT('Ctrl Pts',(79.3582961158376,6.74635426586193,56.1298562806674));
#166114=CARTESIAN_POINT('Ctrl Pts',(79.3933220572914,6.71079923891036,56.1231198966335));
#166115=CARTESIAN_POINT('Ctrl Pts',(79.4099533049714,6.69378865455075,56.1199232173048));
#166116=CARTESIAN_POINT('Ctrl Pts',(79.4498969180057,6.65262389789042,56.1122500527163));
#166117=CARTESIAN_POINT('Ctrl Pts',(79.4731464459963,6.62840658658628,56.1077874188129));
#166118=CARTESIAN_POINT('Ctrl Pts',(79.5545828876644,6.54266990921175,56.0921672264141));
#166119=CARTESIAN_POINT('Ctrl Pts',(79.6120847655959,6.48047858045167,56.0811580853381));
#166120=CARTESIAN_POINT('Ctrl Pts',(79.9932580253986,6.0569350518507,56.0082697235066));
#166121=CARTESIAN_POINT('Ctrl Pts',(80.2899998620266,5.67139016463378,55.9519340984355));
#166122=CARTESIAN_POINT('Ctrl Pts',(80.7872610621668,4.91081443741658,55.8563313444425));
#166123=CARTESIAN_POINT('Ctrl Pts',(80.9947410748632,4.54194499828788,55.8159041640985));
#166124=CARTESIAN_POINT('Ctrl Pts',(81.2120322527243,4.08712522786176,55.7724037211774));
#166125=CARTESIAN_POINT('Ctrl Pts',(81.2460056044337,4.01361957094386,55.7655628714518));
#166126=CARTESIAN_POINT('Ctrl Pts',(81.2983012757139,3.89657625643701,55.7549664623227));
#166127=CARTESIAN_POINT('Ctrl Pts',(81.3172408583193,3.85332761465832,55.7511142273554));
#166128=CARTESIAN_POINT('Ctrl Pts',(81.3506754159879,3.77540953365872,55.7442868377559));
#166129=CARTESIAN_POINT('Ctrl Pts',(81.3652876431223,3.74079311765809,55.74129333845));
#166130=CARTESIAN_POINT('Ctrl Pts',(81.3990929565398,3.65936857304152,55.7343447963729));
#166131=CARTESIAN_POINT('Ctrl Pts',(81.4181197947196,3.61249046291403,55.7304158120876));
#166132=CARTESIAN_POINT('Ctrl Pts',(81.4725625338198,3.47523262042645,55.7191195440899));
#166133=CARTESIAN_POINT('Ctrl Pts',(81.506977945323,3.38445030414383,55.7119091971599));
#166134=CARTESIAN_POINT('Ctrl Pts',(81.6552567033774,2.97456775411852,55.6805205439986));
#166135=CARTESIAN_POINT('Ctrl Pts',(81.753539505228,2.64991192052269,55.6587916894816));
#166136=CARTESIAN_POINT('Ctrl Pts',(81.9463990317789,1.8649415804742,55.6138400937547));
#166137=CARTESIAN_POINT('Ctrl Pts',(82.0248331947055,1.40143044588836,55.5932858276554));
#166138=CARTESIAN_POINT('Ctrl Pts',(82.0911569428425,0.703069833957399,
55.5721697258594));
#166139=CARTESIAN_POINT('Ctrl Pts',(82.1047641805439,0.471530348682286,
55.5667690652911));
#166140=CARTESIAN_POINT('Ctrl Pts',(82.1111072228302,0.193590158400646,
55.5623443144614));
#166141=CARTESIAN_POINT('Ctrl Pts',(82.1118304466039,0.147474929573563,
55.5616780488397));
#166142=CARTESIAN_POINT('Ctrl Pts',(82.1124440055481,0.0757145567867833,
55.5607484876857));
#166143=CARTESIAN_POINT('Ctrl Pts',(82.1125615741381,0.0500726765295319,
55.5604376291905));
#166144=CARTESIAN_POINT('Ctrl Pts',(82.1125825678391,0.0162869168660211,
55.5600563429909));
#166145=CARTESIAN_POINT('Ctrl Pts',(82.1125773773997,0.00814345295206416,
55.5599666070003));
#166146=CARTESIAN_POINT('Ctrl Pts',(82.1125619375607,6.64456069956318E-11,
55.5598790433222));
#166147=CARTESIAN_POINT('Origin',(73.0915550886457,-4.33680868994202E-16,
59.1075264962884));
#166148=CARTESIAN_POINT('',(81.9917963385783,-3.33461157104299E-11,54.8749832973778));
#166149=CARTESIAN_POINT('',(81.9996906220771,-1.55047049271929E-14,54.9197540038636));
#166150=CARTESIAN_POINT('',(82.4472287422617,-1.59709532818419E-15,57.4578688084528));
#166151=CARTESIAN_POINT('',(63.3368846312614,3.0524913646464E-5,58.4943608645448));
#166152=CARTESIAN_POINT('Ctrl Pts',(81.9917963385783,-6.66906343255317E-11,
54.8749832973778));
#166153=CARTESIAN_POINT('Ctrl Pts',(81.991822202953,0.0136416781824146,
54.8751299815349));
#166154=CARTESIAN_POINT('Ctrl Pts',(81.991818955162,0.0272833257654345,
54.8752807745152));
#166155=CARTESIAN_POINT('Ctrl Pts',(81.9917192856842,0.0693062239870782,
54.8757580399907));
#166156=CARTESIAN_POINT('Ctrl Pts',(81.99152598214,0.0976868811112656,54.8760982822577));
#166157=CARTESIAN_POINT('Ctrl Pts',(81.9905186336026,0.187235803710298,
54.8772292123879));
#166158=CARTESIAN_POINT('Ctrl Pts',(81.9892454504036,0.248396492949711,
54.8780861012472));
#166159=CARTESIAN_POINT('Ctrl Pts',(81.9795354315075,0.567997185026232,
54.8830191445056));
#166160=CARTESIAN_POINT('Ctrl Pts',(81.9612443602764,0.826005727639437,
54.8885606355397));
#166161=CARTESIAN_POINT('Ctrl Pts',(81.8645511642046,1.69300376845709,54.913062124542));
#166162=CARTESIAN_POINT('Ctrl Pts',(81.7383288190462,2.29486230360472,54.9400344663477));
#166163=CARTESIAN_POINT('Ctrl Pts',(81.497067905793,3.06905576684948,54.9901588241199));
#166164=CARTESIAN_POINT('Ctrl Pts',(81.432376243716,3.25611442761254,55.0035099977753));
#166165=CARTESIAN_POINT('Ctrl Pts',(81.3376476752165,3.50488393824609,55.022979412955));
#166166=CARTESIAN_POINT('Ctrl Pts',(81.3126309701757,3.56852830174184,55.0281143059707));
#166167=CARTESIAN_POINT('Ctrl Pts',(81.2702098679784,3.67315345139376,55.0368113929279));
#166168=CARTESIAN_POINT('Ctrl Pts',(81.253194191831,3.71429536934038,55.040297353785));
#166169=CARTESIAN_POINT('Ctrl Pts',(81.2193427253909,3.7945577454254,55.0472275977369));
#166170=CARTESIAN_POINT('Ctrl Pts',(81.2025313565162,3.83368776873125,55.0506670860519));
#166171=CARTESIAN_POINT('Ctrl Pts',(81.1619670388033,3.92639703176895,55.0589610766492));
#166172=CARTESIAN_POINT('Ctrl Pts',(81.1379837930375,3.97986952069685,55.0638607501625));
#166173=CARTESIAN_POINT('Ctrl Pts',(81.0541097233846,4.16237037103102,55.0809818458129));
#166174=CARTESIAN_POINT('Ctrl Pts',(80.9918526715719,4.29024609594483,55.0936669948476));
#166175=CARTESIAN_POINT('Ctrl Pts',(80.8312419286745,4.60226080407488,55.1263253193423));
#166176=CARTESIAN_POINT('Ctrl Pts',(80.7296877504282,4.78460136845639,55.1469202453345));
#166177=CARTESIAN_POINT('Ctrl Pts',(80.4732935602959,5.21136273873443,55.1987132090407));
#166178=CARTESIAN_POINT('Ctrl Pts',(80.3131845921018,5.45225107835511,55.2309038922635));
#166179=CARTESIAN_POINT('Ctrl Pts',(79.9417403939865,5.9591706910903,55.3049417488796));
#166180=CARTESIAN_POINT('Ctrl Pts',(79.7266145186263,6.22183123157583,55.3474398971995));
#166181=CARTESIAN_POINT('Ctrl Pts',(79.4524712165179,6.52186675344831,55.4007332273436));
#166182=CARTESIAN_POINT('Ctrl Pts',(79.4064728570105,6.57113337114255,55.4096481509804));
#166183=CARTESIAN_POINT('Ctrl Pts',(79.338997706285,6.64185875161774,55.422681744697));
#166184=CARTESIAN_POINT('Ctrl Pts',(79.3179361910792,6.66372117936767,55.4267439634255));
#166185=CARTESIAN_POINT('Ctrl Pts',(79.2804335601575,6.70227325156488,55.4339660214015));
#166186=CARTESIAN_POINT('Ctrl Pts',(79.2640349059499,6.71900476701175,55.437120206646));
#166187=CARTESIAN_POINT('Ctrl Pts',(79.2282059474958,6.75528768562118,55.4440033795961));
#166188=CARTESIAN_POINT('Ctrl Pts',(79.2087522011366,6.77481474193493,55.4477354688866));
#166189=CARTESIAN_POINT('Ctrl Pts',(79.1527428968766,6.83054099504196,55.4584663933232));
#166190=CARTESIAN_POINT('Ctrl Pts',(79.1159775864347,6.86652253921298,55.4654932185649));
#166191=CARTESIAN_POINT('Ctrl Pts',(78.7933984052931,7.17706351102956,55.5270130497113));
#166192=CARTESIAN_POINT('Ctrl Pts',(78.4909486579221,7.43330334489731,55.5838052057719));
#166193=CARTESIAN_POINT('Ctrl Pts',(77.7511566541425,7.98344925921708,55.7222660152397));
#166194=CARTESIAN_POINT('Ctrl Pts',(77.3035766757266,8.26086009597974,55.805746966175));
#166195=CARTESIAN_POINT('Ctrl Pts',(76.7566752516894,8.53880776098687,55.9084539870362));
#166196=CARTESIAN_POINT('Ctrl Pts',(76.6771731922565,8.57779082629611,55.9233987068999));
#166197=CARTESIAN_POINT('Ctrl Pts',(76.5490636132609,8.63834843265285,55.9475063369901));
#166198=CARTESIAN_POINT('Ctrl Pts',(76.500796050963,8.66065846918242,55.9565950611723));
#166199=CARTESIAN_POINT('Ctrl Pts',(76.4145195977121,8.69963913090307,55.9728514654561));
#166200=CARTESIAN_POINT('Ctrl Pts',(76.3765831446,8.71647313843432,55.9800031678328));
#166201=CARTESIAN_POINT('Ctrl Pts',(76.2968025684778,8.75123513076655,55.9950510013327));
#166202=CARTESIAN_POINT('Ctrl Pts',(76.2549375318103,8.76911030212713,56.0029518289265));
#166203=CARTESIAN_POINT('Ctrl Pts',(76.1440758541751,8.81548107436813,56.0238856485684));
#166204=CARTESIAN_POINT('Ctrl Pts',(76.0748708856314,8.84344856526899,56.0369655618164));
#166205=CARTESIAN_POINT('Ctrl Pts',(75.7297081960262,8.97809933104723,56.1022615536476));
#166206=CARTESIAN_POINT('Ctrl Pts',(75.4492500127483,9.07226093207452,56.1555113554325));
#166207=CARTESIAN_POINT('Ctrl Pts',(74.8310771239294,9.24722341257852,56.2731665960856));
#166208=CARTESIAN_POINT('Ctrl Pts',(74.4923719244879,9.32271168206536,56.3378123708414));
#166209=CARTESIAN_POINT('Ctrl Pts',(74.0129518046217,9.40140154366368,56.4292120766649));
#166210=CARTESIAN_POINT('Ctrl Pts',(73.8751021455843,9.4208187929465,56.45547904903));
#166211=CARTESIAN_POINT('Ctrl Pts',(73.7175404796332,9.43936722476629,56.4854602625635));
#166212=CARTESIAN_POINT('Ctrl Pts',(73.6982026510341,9.44158133535963,56.4891391895567));
#166213=CARTESIAN_POINT('Ctrl Pts',(73.4220823440751,9.47230612172538,56.5416584423132));
#166214=CARTESIAN_POINT('Ctrl Pts',(73.1642259668995,9.49001679707639,56.5905675372639));
#166215=CARTESIAN_POINT('Ctrl Pts',(72.8594630057541,9.49804316407024,56.6480002327844));
#166216=CARTESIAN_POINT('Ctrl Pts',(72.8129906181892,9.49891377063772,56.6567476616759));
#166217=CARTESIAN_POINT('Ctrl Pts',(72.7410540043522,9.49971469902503,56.6702704363055));
#166218=CARTESIAN_POINT('Ctrl Pts',(72.7155946351273,9.49989219977281,56.675052894336));
#166219=CARTESIAN_POINT('Ctrl Pts',(72.6687248088224,9.50002392434837,56.6838505462437));
#166220=CARTESIAN_POINT('Ctrl Pts',(72.6473149955808,9.50000918001051,56.6878666488272));
#166221=CARTESIAN_POINT('Ctrl Pts',(72.5983459483423,9.49980411519282,56.6970465111595));
#166222=CARTESIAN_POINT('Ctrl Pts',(72.5707869368163,9.49956458812455,56.7022085834119));
#166223=CARTESIAN_POINT('Ctrl Pts',(72.4848976354765,9.49843124767219,56.7182841912745));
#166224=CARTESIAN_POINT('Ctrl Pts',(72.4265717902344,9.49710551926816,56.7291831664741));
#166225=CARTESIAN_POINT('Ctrl Pts',(72.1296332775477,9.48752409589665,56.7845926839847));
#166226=CARTESIAN_POINT('Ctrl Pts',(71.8913397750163,9.47051927253352,56.8288058687247));
#166227=CARTESIAN_POINT('Ctrl Pts',(71.1171880893997,9.38484804840058,56.9721234769666));
#166228=CARTESIAN_POINT('Ctrl Pts',(70.5864432169096,9.27824049392138,57.0699384308583));
#166229=CARTESIAN_POINT('Ctrl Pts',(69.8156442116516,9.0513864358103,57.213171090579));
#166230=CARTESIAN_POINT('Ctrl Pts',(69.5666531002123,8.96637507420435,57.2596181024116));
#166231=CARTESIAN_POINT('Ctrl Pts',(69.2519054533381,8.84364950773871,57.3186429608563));
#166232=CARTESIAN_POINT('Ctrl Pts',(69.1825805723832,8.8156434547148,57.3316630610408));
#166233=CARTESIAN_POINT('Ctrl Pts',(69.0715775351641,8.76922371636642,57.3525433929398));
#166234=CARTESIAN_POINT('Ctrl Pts',(69.029686498261,8.7513402610294,57.360430878969));
#166235=CARTESIAN_POINT('Ctrl Pts',(68.9498867236237,8.71657325746769,57.3754705973699));
#166236=CARTESIAN_POINT('Ctrl Pts',(68.9119565312135,8.69974292344304,57.3826255719642));
#166237=CARTESIAN_POINT('Ctrl Pts',(68.8249146434011,8.66041682892671,57.399059404075));
#166238=CARTESIAN_POINT('Ctrl Pts',(68.775882588084,8.63774409131317,57.4083276623536));
#166239=CARTESIAN_POINT('Ctrl Pts',(68.6211333199697,8.56453366338655,57.4376132721707));
#166240=CARTESIAN_POINT('Ctrl Pts',(68.5161612741623,8.51240814632917,57.457529901406));
#166241=CARTESIAN_POINT('Ctrl Pts',(68.0223239866527,8.25537752182242,57.5514608053063));
#166242=CARTESIAN_POINT('Ctrl Pts',(67.647104262967,8.02479308931199,57.6235614884343));
#166243=CARTESIAN_POINT('Ctrl Pts',(66.9399448512522,7.51785093283388,57.7601611502722));
#166244=CARTESIAN_POINT('Ctrl Pts',(66.6080119512906,7.24331659887673,57.8246334087274));
#166245=CARTESIAN_POINT('Ctrl Pts',(66.2486458041058,6.90192052883975,57.8940346930678));
#166246=CARTESIAN_POINT('Ctrl Pts',(66.2020840203413,6.85676277896533,57.9030178785215));
#166247=CARTESIAN_POINT('Ctrl Pts',(66.1345113211875,6.78986044647605,57.9160371865043));
#166248=CARTESIAN_POINT('Ctrl Pts',(66.1131405661603,6.76849735758833,57.9201520934272));
#166249=CARTESIAN_POINT('Ctrl Pts',(66.0754199704642,6.73042629166389,57.9274099213748));
#166250=CARTESIAN_POINT('Ctrl Pts',(66.0590298253972,6.71376050645764,57.9305617550486));
#166251=CARTESIAN_POINT('Ctrl Pts',(66.0231142448563,6.67696861203359,57.9374642952437));
#166252=CARTESIAN_POINT('Ctrl Pts',(66.0036158180696,6.65681565072191,57.9412090632313));
#166253=CARTESIAN_POINT('Ctrl Pts',(65.9470124781257,6.59778835740629,57.9520731916278));
#166254=CARTESIAN_POINT('Ctrl Pts',(65.910144454658,6.55867893066332,57.9591408116212));
#166255=CARTESIAN_POINT('Ctrl Pts',(65.6269926458696,6.2531302195564,58.013368062779));
#166256=CARTESIAN_POINT('Ctrl Pts',(65.3956304170986,5.97272513253239,58.0573724679904));
#166257=CARTESIAN_POINT('Ctrl Pts',(64.8474171024937,5.22442921639762,58.1620855123274));
#166258=CARTESIAN_POINT('Ctrl Pts',(64.5548844302348,4.73991907109159,58.2184731058303));
#166259=CARTESIAN_POINT('Ctrl Pts',(64.2688475762087,4.15382796894945,58.2755288795974));
#166260=CARTESIAN_POINT('Ctrl Pts',(64.2318891786658,4.07540125109142,58.2829450348384));
#166261=CARTESIAN_POINT('Ctrl Pts',(64.1738420288055,3.9477326263978,58.2946687941808));
#166262=CARTESIAN_POINT('Ctrl Pts',(64.1520923378673,3.89880641086579,58.2990799771926));
#166263=CARTESIAN_POINT('Ctrl Pts',(64.1140813270938,3.81132173476508,58.3068230679135));
#166264=CARTESIAN_POINT('Ctrl Pts',(64.0976602374692,3.77283648832602,58.310179974861));
#166265=CARTESIAN_POINT('Ctrl Pts',(64.0634664255108,3.69121423632517,58.3171956561457));
#166266=CARTESIAN_POINT('Ctrl Pts',(64.045755523884,3.64805171104448,58.3208447283219));
#166267=CARTESIAN_POINT('Ctrl Pts',(63.9991674693799,3.53209939745555,58.3304852567978));
#166268=CARTESIAN_POINT('Ctrl Pts',(63.9708658961972,3.4590748500883,58.3363864556028));
#166269=CARTESIAN_POINT('Ctrl Pts',(63.8232071111125,3.06371322672641,58.3674231579553));
#166270=CARTESIAN_POINT('Ctrl Pts',(63.7203555870873,2.73528691767668,58.389970233282));
#166271=CARTESIAN_POINT('Ctrl Pts',(63.5567199579687,2.09351567700281,58.4277325472171));
#166272=CARTESIAN_POINT('Ctrl Pts',(63.4934588896194,1.7812977680813,58.4433452294117));
#166273=CARTESIAN_POINT('Ctrl Pts',(63.3872349261475,1.0799454195237,58.4719251273082));
#166274=CARTESIAN_POINT('Ctrl Pts',(63.3522544858942,0.690120749571852,
58.4834602951632));
#166275=CARTESIAN_POINT('Ctrl Pts',(63.3392591469475,0.241427481035377,
58.4911696626021));
#166276=CARTESIAN_POINT('Ctrl Pts',(63.3381031341895,0.183678751037265,
58.4920560999298));
#166277=CARTESIAN_POINT('Ctrl Pts',(63.3372051441276,0.102655098814244,
58.4931485860234));
#166278=CARTESIAN_POINT('Ctrl Pts',(63.3370309983082,0.0793874405663537,
58.493444825801));
#166279=CARTESIAN_POINT('Ctrl Pts',(63.3368678653725,0.0374198454953173,
58.493947359837));
#166280=CARTESIAN_POINT('Ctrl Pts',(63.3368492358014,0.0187302153537607,
58.494159780901));
#166281=CARTESIAN_POINT('Ctrl Pts',(63.3368846312614,3.05249101211109E-5,
58.4943608645448));
#166282=CARTESIAN_POINT('Ctrl Pts',(63.3368846312614,3.05249136617253E-5,
58.4943608645448));
#166283=CARTESIAN_POINT('Ctrl Pts',(63.3369208637748,-0.0191113871700155,
58.4945667035367));
#166284=CARTESIAN_POINT('Ctrl Pts',(63.3370136687594,-0.0382432773275274,
58.4947604411253));
#166285=CARTESIAN_POINT('Ctrl Pts',(63.3373508002251,-0.081412204403057,
58.4951707098884));
#166286=CARTESIAN_POINT('Ctrl Pts',(63.3376276930398,-0.105438922169356,
58.4953802730565));
#166287=CARTESIAN_POINT('Ctrl Pts',(63.3389067619386,-0.189363842556669,
58.4960472253987));
#166288=CARTESIAN_POINT('Ctrl Pts',(63.3403745355787,-0.249254289988703,
58.4964074262296));
#166289=CARTESIAN_POINT('Ctrl Pts',(63.3600723622294,-0.83227138533733,
58.4988104441391));
#166290=CARTESIAN_POINT('Ctrl Pts',(63.4201008376448,-1.35312302820521,
58.4923494029091));
#166291=CARTESIAN_POINT('Ctrl Pts',(63.5897881989267,-2.20684882306762,
58.469621999276));
#166292=CARTESIAN_POINT('Ctrl Pts',(63.6758097808222,-2.54333582905673,
58.4573954212617));
#166293=CARTESIAN_POINT('Ctrl Pts',(63.8408072476067,-3.06832455602437,
58.4334381770832));
#166294=CARTESIAN_POINT('Ctrl Pts',(63.9079247690089,-3.26030711162486,
58.4235995160826));
#166295=CARTESIAN_POINT('Ctrl Pts',(64.0051843994766,-3.51243991047723,
58.4092595788151));
#166296=CARTESIAN_POINT('Ctrl Pts',(64.0299377876326,-3.57465765612895,
58.4056035909721));
#166297=CARTESIAN_POINT('Ctrl Pts',(64.0721357637391,-3.67756484516007,
58.3993614027841));
#166298=CARTESIAN_POINT('Ctrl Pts',(64.0892146914298,-3.71840504596493,
58.3968324897989));
#166299=CARTESIAN_POINT('Ctrl Pts',(64.1231901244958,-3.79809073582831,
58.3917969713027));
#166300=CARTESIAN_POINT('Ctrl Pts',(64.1400625365877,-3.83694561066209,
58.3892941352866));
#166301=CARTESIAN_POINT('Ctrl Pts',(64.1812311848857,-3.93005322047514,
58.383182101967));
#166302=CARTESIAN_POINT('Ctrl Pts',(64.2057753422229,-3.9841917966498,58.3795340690249));
#166303=CARTESIAN_POINT('Ctrl Pts',(64.2883248672261,-4.16185120570181,
58.3672509236198));
#166304=CARTESIAN_POINT('Ctrl Pts',(64.3484618297949,-4.28433922271799,
58.3582815095215));
#166305=CARTESIAN_POINT('Ctrl Pts',(64.6905627408281,-4.94497349033314,
58.3071238990448));
#166306=CARTESIAN_POINT('Ctrl Pts',(65.0205461204864,-5.45606972650783,
58.2574253140063));
#166307=CARTESIAN_POINT('Ctrl Pts',(65.5092364819749,-6.07456577013193,
58.1817935662063));
#166308=CARTESIAN_POINT('Ctrl Pts',(65.6261553977769,-6.21410952578817,
58.1635654708648));
#166309=CARTESIAN_POINT('Ctrl Pts',(65.7956166646602,-6.4049591856445,58.1368857455231));
#166310=CARTESIAN_POINT('Ctrl Pts',(65.8449059334505,-6.45919241571806,
58.1290964935448));
#166311=CARTESIAN_POINT('Ctrl Pts',(65.9327277908391,-6.55360555782429,
58.115159915273));
#166312=CARTESIAN_POINT('Ctrl Pts',(65.9709997234127,-6.59403121683617,
58.1090676965539));
#166313=CARTESIAN_POINT('Ctrl Pts',(66.0293810769665,-6.65462197163174,
58.0997434517078));
#166314=CARTESIAN_POINT('Ctrl Pts',(66.0492338026511,-6.67504131205081,
58.0965674034375));
#166315=CARTESIAN_POINT('Ctrl Pts',(66.0855740390587,-6.71208378603744,
58.0907435687896));
#166316=CARTESIAN_POINT('Ctrl Pts',(66.1020321035148,-6.72873618763518,
58.0881022489186));
#166317=CARTESIAN_POINT('Ctrl Pts',(66.1396151271271,-6.76648257787124,
58.0820621457074));
#166318=CARTESIAN_POINT('Ctrl Pts',(66.160777570398,-6.78753731511597,58.0786550651021));
#166319=CARTESIAN_POINT('Ctrl Pts',(66.2266729591109,-6.852481059745,58.0680286443838));
#166320=CARTESIAN_POINT('Ctrl Pts',(66.2717359575052,-6.89602084411713,
58.0607369423431));
#166321=CARTESIAN_POINT('Ctrl Pts',(66.6586584089125,-7.26250928516937,
57.9979444446001));
#166322=CARTESIAN_POINT('Ctrl Pts',(67.0232922894948,-7.55960861704001,
57.937592563155));
#166323=CARTESIAN_POINT('Ctrl Pts',(67.7915681430084,-8.09507772881114,
57.8102654879827));
#166324=CARTESIAN_POINT('Ctrl Pts',(68.1939658545534,-8.33294420832425,
57.743505870903));
#166325=CARTESIAN_POINT('Ctrl Pts',(68.6846877278869,-8.57534972289602,
57.6626472369883));
#166326=CARTESIAN_POINT('Ctrl Pts',(68.7576310234073,-8.61020786993134,
57.6506403913566));
#166327=CARTESIAN_POINT('Ctrl Pts',(68.8736324174974,-8.66379787626326,
57.6315672530401));
#166328=CARTESIAN_POINT('Ctrl Pts',(68.9163993634356,-8.68316389436018,
57.624539950053));
#166329=CARTESIAN_POINT('Ctrl Pts',(68.9971501917322,-8.71899606356189,
57.611280019271));
#166330=CARTESIAN_POINT('Ctrl Pts',(69.0351015825265,-8.73553418863046,
57.6050516972604));
#166331=CARTESIAN_POINT('Ctrl Pts',(69.1209883407484,-8.77228086811203,
57.5909648021187));
#166332=CARTESIAN_POINT('Ctrl Pts',(69.1689843142457,-8.79234121316166,
57.5830984031688));
#166333=CARTESIAN_POINT('Ctrl Pts',(69.311680099136,-8.85058041724986,57.559728156058));
#166334=CARTESIAN_POINT('Ctrl Pts',(69.4068350908284,-8.88759967514904,
57.5441663208849));
#166335=CARTESIAN_POINT('Ctrl Pts',(70.0614171591809,-9.12991788946181,
57.4372626359304));
#166336=CARTESIAN_POINT('Ctrl Pts',(70.6385650868135,-9.28243004052871,
57.3438531483033));
#166337=CARTESIAN_POINT('Ctrl Pts',(71.513186721696,-9.42548798437507,57.2020976284825));
#166338=CARTESIAN_POINT('Ctrl Pts',(71.8023342095742,-9.45889916442988,
57.1551797555897));
#166339=CARTESIAN_POINT('Ctrl Pts',(72.2362399202519,-9.48842566885487,
57.0843579497743));
#166340=CARTESIAN_POINT('Ctrl Pts',(72.3801735704896,-9.4948495061206,57.0607963021624));
#166341=CARTESIAN_POINT('Ctrl Pts',(72.5629167595653,-9.49873403448535,
57.0307531726488));
#166342=CARTESIAN_POINT('Ctrl Pts',(72.6016575913313,-9.49931410024482,
57.0243768121353));
#166343=CARTESIAN_POINT('Ctrl Pts',(72.6639486647109,-9.49985540442961,
57.0141114504137));
#166344=CARTESIAN_POINT('Ctrl Pts',(72.6874979688409,-9.49997011154059,
57.0102276474667));
#166345=CARTESIAN_POINT('Ctrl Pts',(72.7328165285815,-9.50001778243422,
57.0027476311316));
#166346=CARTESIAN_POINT('Ctrl Pts',(72.754585577935,-9.49996382400027,56.9991518766479));
#166347=CARTESIAN_POINT('Ctrl Pts',(72.8027704012823,-9.49967426068319,
56.9911871488104));
#166348=CARTESIAN_POINT('Ctrl Pts',(72.829185631001,-9.49940232792237,56.9868170583928));
#166349=CARTESIAN_POINT('Ctrl Pts',(72.9232821546964,-9.4980303780061,56.971237255248));
#166350=CARTESIAN_POINT('Ctrl Pts',(72.9909492174259,-9.49630041718572,
56.9600101630647));
#166351=CARTESIAN_POINT('Ctrl Pts',(73.4346395656196,-9.48007980871439,
56.8862665531732));
#166352=CARTESIAN_POINT('Ctrl Pts',(73.8094364466946,-9.44338615530301,
56.8233824204234));
#166353=CARTESIAN_POINT('Ctrl Pts',(74.4985605949375,-9.33315350902319,
56.7077099752523));
#166354=CARTESIAN_POINT('Ctrl Pts',(74.813291182377,-9.26582733056012,56.6548604715169));
#166355=CARTESIAN_POINT('Ctrl Pts',(75.3348497331866,-9.12551582848721,
56.5676583618627));
#166356=CARTESIAN_POINT('Ctrl Pts',(75.5436750060612,-9.061352846041,56.5328465768688));
#166357=CARTESIAN_POINT('Ctrl Pts',(75.8904674353115,-8.94126287332556,
56.4752869999921));
#166358=CARTESIAN_POINT('Ctrl Pts',(76.0296620639175,-8.88929502592799,
56.4522534085077));
#166359=CARTESIAN_POINT('Ctrl Pts',(76.2226974185921,-8.81191216675489,
56.4204189653304));
#166360=CARTESIAN_POINT('Ctrl Pts',(76.2775947265289,-8.78929373745793,
56.4113780026013));
#166361=CARTESIAN_POINT('Ctrl Pts',(76.3713879423166,-8.74959689799275,
56.3959531082265));
#166362=CARTESIAN_POINT('Ctrl Pts',(76.4103869223857,-8.73277587998832,
56.3895459944723));
#166363=CARTESIAN_POINT('Ctrl Pts',(76.4893705324138,-8.69806675157806,
56.3765831823614));
#166364=CARTESIAN_POINT('Ctrl Pts',(76.5293470450378,-8.68016215303519,
56.3700292334103));
#166365=CARTESIAN_POINT('Ctrl Pts',(76.6293506996679,-8.6345244447365,56.3536517606071));
#166366=CARTESIAN_POINT('Ctrl Pts',(76.689216708219,-8.60643147073267,56.34386364101));
#166367=CARTESIAN_POINT('Ctrl Pts',(76.9145193677493,-8.49776941214144,
56.3070868172415));
#166368=CARTESIAN_POINT('Ctrl Pts',(77.0779188610577,-8.41292555410641,
56.2805395390404));
#166369=CARTESIAN_POINT('Ctrl Pts',(77.6726651150445,-8.08146368281936,
56.1843304610601));
#166370=CARTESIAN_POINT('Ctrl Pts',(78.0871146175184,-7.80522107436626,
56.1181699073794));
#166371=CARTESIAN_POINT('Ctrl Pts',(78.6988207004769,-7.32324201516067,
56.0208311704537));
#166372=CARTESIAN_POINT('Ctrl Pts',(78.9117571459242,-7.13942939984271,
55.9870018997138));
#166373=CARTESIAN_POINT('Ctrl Pts',(79.1634469617107,-6.90166717403784,
55.9468248047271));
#166374=CARTESIAN_POINT('Ctrl Pts',(79.210197274325,-6.85657959476065,55.939353261449));
#166375=CARTESIAN_POINT('Ctrl Pts',(79.2780592614554,-6.78976208851189,
55.9284903139532));
#166376=CARTESIAN_POINT('Ctrl Pts',(79.2995346761457,-6.76841223526,55.9250500527615));
#166377=CARTESIAN_POINT('Ctrl Pts',(79.3358720275714,-6.73193711867265,
55.9192240111268));
#166378=CARTESIAN_POINT('Ctrl Pts',(79.3507859627285,-6.7168651764674,55.9168313727608));
#166379=CARTESIAN_POINT('Ctrl Pts',(79.3846905380177,-6.68236914756725,
55.911388635546));
#166380=CARTESIAN_POINT('Ctrl Pts',(79.4036485269671,-6.66291279369679,
55.9083428631627));
#166381=CARTESIAN_POINT('Ctrl Pts',(79.4558868017254,-6.60883536891432,
55.8999442308619));
#166382=CARTESIAN_POINT('Ctrl Pts',(79.4889888457069,-6.57403956121119,
55.8946153406252));
#166383=CARTESIAN_POINT('Ctrl Pts',(79.6860798861485,-6.363668962265,55.8628530117063));
#166384=CARTESIAN_POINT('Ctrl Pts',(79.84364510948,-6.18206247020525,55.8373199245345));
#166385=CARTESIAN_POINT('Ctrl Pts',(80.2619401450234,-5.66114345369423,
55.7695474550765));
#166386=CARTESIAN_POINT('Ctrl Pts',(80.5070370553553,-5.30969996049169,
55.7298698045886));
#166387=CARTESIAN_POINT('Ctrl Pts',(80.8331744871437,-4.76773514606693,
55.6780517617711));
#166388=CARTESIAN_POINT('Ctrl Pts',(80.93284726701,-4.58941656460383,55.6623778404422));
#166389=CARTESIAN_POINT('Ctrl Pts',(81.0911828028448,-4.28358834369425,
55.6378365961909));
#166390=CARTESIAN_POINT('Ctrl Pts',(81.1528662611215,-4.15777070352312,
55.6283813833674));
#166391=CARTESIAN_POINT('Ctrl Pts',(81.2363110073525,-3.97770120371416,
55.6157574560281));
#166392=CARTESIAN_POINT('Ctrl Pts',(81.2603524732508,-3.92455804778409,
55.6121416723445));
#166393=CARTESIAN_POINT('Ctrl Pts',(81.3011100503674,-3.83223604861605,
55.6060500491535));
#166394=CARTESIAN_POINT('Ctrl Pts',(81.3180511706121,-3.79316137361405,
55.603530046097));
#166395=CARTESIAN_POINT('Ctrl Pts',(81.3522411992092,-3.71284466570169,
55.5984694394092));
#166396=CARTESIAN_POINT('Ctrl Pts',(81.3694634132779,-3.67159209235742,
55.5959340529241));
#166397=CARTESIAN_POINT('Ctrl Pts',(81.412545460645,-3.56634021987553,55.589627378788));
#166398=CARTESIAN_POINT('Ctrl Pts',(81.4380070523745,-3.50217610519317,
55.5859341451506));
#166399=CARTESIAN_POINT('Ctrl Pts',(81.53558783923,-3.24834062503304,55.571917602389));
#166400=CARTESIAN_POINT('Ctrl Pts',(81.6024139697956,-3.05663616059278,
55.5626303829469));
#166401=CARTESIAN_POINT('Ctrl Pts',(81.8449420280424,-2.28312757208262,
55.5302303672368));
#166402=CARTESIAN_POINT('Ctrl Pts',(81.9716589841839,-1.68708541232549,
55.5166271718393));
#166403=CARTESIAN_POINT('Ctrl Pts',(82.0709754922155,-0.826081109782583,
55.5109108782228));
#166404=CARTESIAN_POINT('Ctrl Pts',(82.0902503395178,-0.56804435403418,
55.5109257407692));
#166405=CARTESIAN_POINT('Ctrl Pts',(82.1011744800333,-0.248408270794094,
55.5128688402182));
#166406=CARTESIAN_POINT('Ctrl Pts',(82.1026797706731,-0.187244352105316,
55.5133274666071));
#166407=CARTESIAN_POINT('Ctrl Pts',(82.104026816949,-0.0976913123765372,
55.5141224750122));
#166408=CARTESIAN_POINT('Ctrl Pts',(82.104327760441,-0.0693100533167987,
55.5143925846016));
#166409=CARTESIAN_POINT('Ctrl Pts',(82.1045868046991,-0.0272854394580932,
55.5148190559226));
#166410=CARTESIAN_POINT('Ctrl Pts',(82.1046417876626,-0.0136427461076473,
55.514961641197));
#166411=CARTESIAN_POINT('Ctrl Pts',(82.1046676540618,-6.66937018010743E-11,
55.5151083368358));
#166412=CARTESIAN_POINT('',(81.9996908076899,9.81597696801075E-5,54.9197550594462));
#166413=CARTESIAN_POINT('Ctrl Pts',(82.1125619375607,6.64456069956318E-11,
55.5598790433222));
#166414=CARTESIAN_POINT('Ctrl Pts',(82.1125360255529,-0.0136668014906386,
55.5597320890229));
#166415=CARTESIAN_POINT('Ctrl Pts',(82.1124812457219,-0.0273335719858172,
55.5595912531169));
#166416=CARTESIAN_POINT('Ctrl Pts',(82.1122237839164,-0.0693960590722018,
55.5591765377402));
#166417=CARTESIAN_POINT('Ctrl Pts',(82.1119253322823,-0.0977911812342799,
55.5589228587031));
#166418=CARTESIAN_POINT('Ctrl Pts',(82.1105894637986,-0.187432230743492,
55.55820415569));
#166419=CARTESIAN_POINT('Ctrl Pts',(82.1090966125081,-0.248670552593953,
55.5578342368826));
#166420=CARTESIAN_POINT('Ctrl Pts',(82.0982476273081,-0.569031278259053,
55.5565189630936));
#166421=CARTESIAN_POINT('Ctrl Pts',(82.0790771428474,-0.827719230267891,
55.557577764286));
#166422=CARTESIAN_POINT('Ctrl Pts',(81.9800912821575,-1.69058319990238,
55.5676174054073));
#166423=CARTESIAN_POINT('Ctrl Pts',(81.8535609968872,-2.28776150893319,
55.5852456228765));
#166424=CARTESIAN_POINT('Ctrl Pts',(81.6111483540582,-3.06075393816077,
55.6204359434127));
#166425=CARTESIAN_POINT('Ctrl Pts',(81.5448674797552,-3.25091457336205,
55.6301497961054));
#166426=CARTESIAN_POINT('Ctrl Pts',(81.4479620218375,-3.50306690856643,
55.6444344463764));
#166427=CARTESIAN_POINT('Ctrl Pts',(81.4225731932735,-3.56705957764205,
55.6481837324348));
#166428=CARTESIAN_POINT('Ctrl Pts',(81.3795794719202,-3.67210458368161,
55.6545430240807));
#166429=CARTESIAN_POINT('Ctrl Pts',(81.3623722929424,-3.71332061847222,
55.6570907175287));
#166430=CARTESIAN_POINT('Ctrl Pts',(81.3281864041571,-3.79361902625666,
55.6621570676167));
#166431=CARTESIAN_POINT('Ctrl Pts',(81.3112338122779,-3.83271162603291,
55.6646716377605));
#166432=CARTESIAN_POINT('Ctrl Pts',(81.2704072612829,-3.92515976751463,
55.6707325374166));
#166433=CARTESIAN_POINT('Ctrl Pts',(81.2463050545487,-3.97841024212875,
55.6743146204079));
#166434=CARTESIAN_POINT('Ctrl Pts',(81.1624376258653,-4.15926951853397,
55.6867927392426));
#166435=CARTESIAN_POINT('Ctrl Pts',(81.1003491686526,-4.28575489135513,
55.6960530732046));
#166436=CARTESIAN_POINT('Ctrl Pts',(80.940697981556,-4.59358539212979,55.7199290102874));
#166437=CARTESIAN_POINT('Ctrl Pts',(80.8400382007869,-4.77320404669988,
55.7350353862728));
#166438=CARTESIAN_POINT('Ctrl Pts',(80.5138828051378,-5.31344372736145,
55.7842304526298));
#166439=CARTESIAN_POINT('Ctrl Pts',(80.2701319312162,-5.66213831350987,
55.8213027277249));
#166440=CARTESIAN_POINT('Ctrl Pts',(79.8531072124986,-6.1810730799033,55.885987986311));
#166441=CARTESIAN_POINT('Ctrl Pts',(79.6950258598222,-6.36314554350392,
55.9107520212205));
#166442=CARTESIAN_POINT('Ctrl Pts',(79.4974382461152,-6.57397003278031,
55.9421495739343));
#166443=CARTESIAN_POINT('Ctrl Pts',(79.4643119514582,-6.60878211357146,
55.9474277305992));
#166444=CARTESIAN_POINT('Ctrl Pts',(79.412046315553,-6.66287934452541,55.9557794450618));
#166445=CARTESIAN_POINT('Ctrl Pts',(79.3930829798991,-6.68233933675426,
55.9588145315035));
#166446=CARTESIAN_POINT('Ctrl Pts',(79.3591744100656,-6.71683842750533,
55.9642506286868));
#166447=CARTESIAN_POINT('Ctrl Pts',(79.3442613938861,-6.73190980792745,
55.9666445346258));
#166448=CARTESIAN_POINT('Ctrl Pts',(79.3079325587747,-6.76837915527102,
55.9724835941919));
#166449=CARTESIAN_POINT('Ctrl Pts',(79.286465547779,-6.7897238808116,55.9759400913013));
#166450=CARTESIAN_POINT('Ctrl Pts',(79.2186520693956,-6.85650833587099,
55.986877235347));
#166451=CARTESIAN_POINT('Ctrl Pts',(79.1719474145352,-6.90156874971383,
55.9944363750182));
#166452=CARTESIAN_POINT('Ctrl Pts',(78.9206856817879,-7.13904600760519,
56.0352257413341));
#166453=CARTESIAN_POINT('Ctrl Pts',(78.7082496555849,-7.32262844922743,
56.0701359412207));
#166454=CARTESIAN_POINT('Ctrl Pts',(78.0983332284704,-7.80382989095364,
56.1708456612503));
#166455=CARTESIAN_POINT('Ctrl Pts',(77.6852946023917,-8.0796274366257,56.2395330219509));
#166456=CARTESIAN_POINT('Ctrl Pts',(77.0909677876752,-8.41142496431611,
56.3378098325893));
#166457=CARTESIAN_POINT('Ctrl Pts',(76.9266534935861,-8.49684137376437,
56.3649325470597));
#166458=CARTESIAN_POINT('Ctrl Pts',(76.7002583345621,-8.60608562749063,
56.4022090418431));
#166459=CARTESIAN_POINT('Ctrl Pts',(76.6402700312127,-8.63424663202308,
56.4120776684254));
#166460=CARTESIAN_POINT('Ctrl Pts',(76.5401154361674,-8.67996449625796,
56.4285388695781));
#166461=CARTESIAN_POINT('Ctrl Pts',(76.5001136913954,-8.69788376026319,
56.435109507075));
#166462=CARTESIAN_POINT('Ctrl Pts',(76.4211226249072,-8.73260063254941,
56.4480764806771));
#166463=CARTESIAN_POINT('Ctrl Pts',(76.3821418118313,-8.74941538885511,
56.454471670396));
#166464=CARTESIAN_POINT('Ctrl Pts',(76.2884654744931,-8.78906510808121,
56.4698309722384));
#166465=CARTESIAN_POINT('Ctrl Pts',(76.2336659638703,-8.81164437711394,
56.478808480221));
#166466=CARTESIAN_POINT('Ctrl Pts',(76.0413915199108,-8.8887256656826,56.5102815162446));
#166467=CARTESIAN_POINT('Ctrl Pts',(75.9028543189174,-8.94046200180463,
56.5329114272489));
#166468=CARTESIAN_POINT('Ctrl Pts',(75.5580704757652,-9.05992314015649,
56.5891247484948));
#166469=CARTESIAN_POINT('Ctrl Pts',(75.3505939047013,-9.12375718500429,
56.6228579811986));
#166470=CARTESIAN_POINT('Ctrl Pts',(74.8283151887886,-9.26460489578375,
56.7076239639697));
#166471=CARTESIAN_POINT('Ctrl Pts',(74.5113952427779,-9.33249773916729,
56.7589218462161));
#166472=CARTESIAN_POINT('Ctrl Pts',(73.8196223814295,-9.44318442541645,
56.8710530418786));
#166473=CARTESIAN_POINT('Ctrl Pts',(73.4443952264645,-9.47995599251494,
56.9319713033499));
#166474=CARTESIAN_POINT('Ctrl Pts',(73.0016358359056,-9.49621096932413,
57.0045663251759));
#166475=CARTESIAN_POINT('Ctrl Pts',(72.9351438112067,-9.49793449432923,
57.0154876508926));
#166476=CARTESIAN_POINT('Ctrl Pts',(72.8416117494996,-9.49934995670988,
57.0308820384208));
#166477=CARTESIAN_POINT('Ctrl Pts',(72.8145794909049,-9.49964053625336,
57.0353349906176));
#166478=CARTESIAN_POINT('Ctrl Pts',(72.7656245590012,-9.49995215672126,
57.0434063699352));
#166479=CARTESIAN_POINT('Ctrl Pts',(72.7437020605574,-9.50001376539328,
57.0470234166934));
#166480=CARTESIAN_POINT('Ctrl Pts',(72.6985137107118,-9.49998009980099,
57.0544847574435));
#166481=CARTESIAN_POINT('Ctrl Pts',(72.6752481499632,-9.49987497562994,
57.0583293228877));
#166482=CARTESIAN_POINT('Ctrl Pts',(72.614525992139,-9.49937145596472,57.0683710000932));
#166483=CARTESIAN_POINT('Ctrl Pts',(72.5770716807192,-9.49883327277347,
57.0745723209678));
#166484=CARTESIAN_POINT('Ctrl Pts',(72.4095009643444,-9.49540689366203,
57.1023475659263));
#166485=CARTESIAN_POINT('Ctrl Pts',(72.2794613473683,-9.48999938018888,
57.1239841525583));
#166486=CARTESIAN_POINT('Ctrl Pts',(71.904030582383,-9.46643778442168,57.1866120961271));
#166487=CARTESIAN_POINT('Ctrl Pts',(71.6592032220148,-9.44122964631399,
57.227652043293));
#166488=CARTESIAN_POINT('Ctrl Pts',(70.8056812299706,-9.31876084621198,
57.3708751745608));
#166489=CARTESIAN_POINT('Ctrl Pts',(70.2057298384782,-9.17045251366239,
57.4717045855736));
#166490=CARTESIAN_POINT('Ctrl Pts',(69.504796880521,-8.92099197253348,57.5879182777093));
#166491=CARTESIAN_POINT('Ctrl Pts',(69.3861815633877,-8.87602377153626,
57.6075325211451));
#166492=CARTESIAN_POINT('Ctrl Pts',(69.220545102184,-8.80932702504476,57.6348424277852));
#166493=CARTESIAN_POINT('Ctrl Pts',(69.1727545382097,-8.78961938390927,
57.6427126237254));
#166494=CARTESIAN_POINT('Ctrl Pts',(69.0895856639037,-8.75451003261279,
57.6563921548573));
#166495=CARTESIAN_POINT('Ctrl Pts',(69.0541366177832,-8.73928541170523,
57.6622174047591));
#166496=CARTESIAN_POINT('Ctrl Pts',(68.9797990557655,-8.70681100364406,
57.6744217166096));
#166497=CARTESIAN_POINT('Ctrl Pts',(68.9409313836164,-8.68951399426703,
57.680796185491));
#166498=CARTESIAN_POINT('Ctrl Pts',(68.8477452670836,-8.64727796026977,
57.6960631916992));
#166499=CARTESIAN_POINT('Ctrl Pts',(68.7935420454523,-8.62208019548396,
57.7049303807334));
#166500=CARTESIAN_POINT('Ctrl Pts',(68.6025315004657,-8.53104282966057,
57.7361319102404));
#166501=CARTESIAN_POINT('Ctrl Pts',(68.4670537498172,-8.46237123217672,
57.7581772140976));
#166502=CARTESIAN_POINT('Ctrl Pts',(68.1305815346606,-8.28138267081173,
57.8127287105792));
#166503=CARTESIAN_POINT('Ctrl Pts',(67.9318871771172,-8.16486140122882,
57.8447561602995));
#166504=CARTESIAN_POINT('Ctrl Pts',(67.3358376680028,-7.7851260434429,57.9403992392503));
#166505=CARTESIAN_POINT('Ctrl Pts',(66.9537402845773,-7.49867085352006,
58.0010619802806));
#166506=CARTESIAN_POINT('Ctrl Pts',(66.4786535375545,-7.08249886625802,
58.0766784000258));
#166507=CARTESIAN_POINT('Ctrl Pts',(66.3650651565212,-6.97795131916147,
58.094777363123));
#166508=CARTESIAN_POINT('Ctrl Pts',(66.2230921323951,-6.84067619280946,
58.1174733905887));
#166509=CARTESIAN_POINT('Ctrl Pts',(66.1923175456572,-6.81050848079737,
58.1223977178687));
#166510=CARTESIAN_POINT('Ctrl Pts',(66.1434427289572,-6.76193501459169,
58.1302271998457));
#166511=CARTESIAN_POINT('Ctrl Pts',(66.1252105831228,-6.74366568990208,
58.1331498983603));
#166512=CARTESIAN_POINT('Ctrl Pts',(66.0901544777273,-6.70824804413174,
58.1387738157274));
#166513=CARTESIAN_POINT('Ctrl Pts',(66.0733207557135,-6.69111004895203,
58.1414763395027));
#166514=CARTESIAN_POINT('Ctrl Pts',(66.0323816262767,-6.649110770648,58.1480532305458));
#166515=CARTESIAN_POINT('Ctrl Pts',(66.008346610756,-6.62417983030463,58.1519182391814));
#166516=CARTESIAN_POINT('Ctrl Pts',(65.9213693332408,-6.5329596392893,58.1659168384311));
#166517=CARTESIAN_POINT('Ctrl Pts',(65.8592461385075,-6.46587934785723,
58.1759383743014));
#166518=CARTESIAN_POINT('Ctrl Pts',(65.7024131566258,-6.29151872738471,
58.2012757541372));
#166519=CARTESIAN_POINT('Ctrl Pts',(65.6091341018514,-6.18295275927967,
58.2163818292685));
#166520=CARTESIAN_POINT('Ctrl Pts',(65.117094794154,-5.58328562049482,58.2960957636188));
#166521=CARTESIAN_POINT('Ctrl Pts',(64.7653396514642,-5.05472175361954,
58.3530731883585));
#166522=CARTESIAN_POINT('Ctrl Pts',(64.392566943181,-4.35233090368823,58.4111254271624));
#166523=CARTESIAN_POINT('Ctrl Pts',(64.3206750710312,-4.2082197362665,58.4221876428815));
#166524=CARTESIAN_POINT('Ctrl Pts',(64.2256324991032,-4.00506479649708,
58.4365988594911));
#166525=CARTESIAN_POINT('Ctrl Pts',(64.1994064674166,-3.94753370053154,
58.440550718768));
#166526=CARTESIAN_POINT('Ctrl Pts',(64.1578585200484,-3.8539562227327,58.4467696347737));
#166527=CARTESIAN_POINT('Ctrl Pts',(64.1421875837915,-3.81807153525195,
58.4491051738658));
#166528=CARTESIAN_POINT('Ctrl Pts',(64.109862687214,-3.7428011143,58.4539011915989));
#166529=CARTESIAN_POINT('Ctrl Pts',(64.0932511274301,-3.7033976001956,58.4563533685969));
#166530=CARTESIAN_POINT('Ctrl Pts',(64.0542313617415,-3.60908922144042,
58.4620830489079));
#166531=CARTESIAN_POINT('Ctrl Pts',(64.0320658676684,-3.55408301751158,
58.4653129782517));
#166532=CARTESIAN_POINT('Ctrl Pts',(63.9571741375909,-3.36316065001344,
58.4761380288964));
#166533=CARTESIAN_POINT('Ctrl Pts',(63.9070175956668,-3.22623048014024,
58.4832299329698));
#166534=CARTESIAN_POINT('Ctrl Pts',(63.7915698364866,-2.88743425540025,
58.4991497296821));
#166535=CARTESIAN_POINT('Ctrl Pts',(63.729787306591,-2.6844248219704,58.5072971236605));
#166536=CARTESIAN_POINT('Ctrl Pts',(63.5875153708102,-2.15479781856576,
58.5250663127387));
#166537=CARTESIAN_POINT('Ctrl Pts',(63.5172992143608,-1.8256623217694,58.532747625524));
#166538=CARTESIAN_POINT('Ctrl Pts',(63.4038724050146,-1.11306713989593,
58.5427300164016));
#166539=CARTESIAN_POINT('Ctrl Pts',(63.3661688939888,-0.729313567826545,
58.5440775717329));
#166540=CARTESIAN_POINT('Ctrl Pts',(63.3490646836895,-0.2769138713198,58.5415717179955));
#166541=CARTESIAN_POINT('Ctrl Pts',(63.3472259471866,-0.209450397333085,
58.5410918560795));
#166542=CARTESIAN_POINT('Ctrl Pts',(63.3456413777209,-0.114566163059452,
58.5402722242381));
#166543=CARTESIAN_POINT('Ctrl Pts',(63.3453011231222,-0.0871565957880548,
58.5400184778408));
#166544=CARTESIAN_POINT('Ctrl Pts',(63.3448978017111,-0.0375252792831324,
58.5395286752416));
#166545=CARTESIAN_POINT('Ctrl Pts',(63.3447944526855,-0.0153039432741772,
58.5392983690199));
#166546=CARTESIAN_POINT('Ctrl Pts',(63.3447406639745,0.0304910167184051,
58.5388012857994));
#166547=CARTESIAN_POINT('Ctrl Pts',(63.3447999067499,0.0540644024239192,
58.5385331218232));
#166548=CARTESIAN_POINT('Ctrl Pts',(63.3451812460527,0.115572764262319,
58.5378009642449));
#166549=CARTESIAN_POINT('Ctrl Pts',(63.3456415014136,0.153506224787392,
58.5373172121439));
#166550=CARTESIAN_POINT('Ctrl Pts',(63.3487039550173,0.323032355641628,
58.5350084924542));
#166551=CARTESIAN_POINT('Ctrl Pts',(63.353788490623,0.454560662918221,58.532821676005));
#166552=CARTESIAN_POINT('Ctrl Pts',(63.3762701073733,0.833987689020082,
58.5252970938101));
#166553=CARTESIAN_POINT('Ctrl Pts',(63.4005828058213,1.08134506544725,58.5188868951615));
#166554=CARTESIAN_POINT('Ctrl Pts',(63.5190153250352,1.94246850127986,58.4907628123768));
#166555=CARTESIAN_POINT('Ctrl Pts',(63.6628423739426,2.54752174277458,58.4604747325846));
#166556=CARTESIAN_POINT('Ctrl Pts',(63.9061204508566,3.258103172746,58.4102197181101));
#166557=CARTESIAN_POINT('Ctrl Pts',(63.9511751225037,3.38139949019407,58.4009440319482));
#166558=CARTESIAN_POINT('Ctrl Pts',(64.0178203776762,3.55280161797357,58.387258329664));
#166559=CARTESIAN_POINT('Ctrl Pts',(64.0373136565667,3.60173922230622,58.3832592048031));
#166560=CARTESIAN_POINT('Ctrl Pts',(64.0719475837959,3.68664740079326,58.3761602129072));
#166561=CARTESIAN_POINT('Ctrl Pts',(64.086907741873,3.72269313639632,58.3730957448931));
#166562=CARTESIAN_POINT('Ctrl Pts',(64.1187174420369,3.79803514866314,58.3665837432107));
#166563=CARTESIAN_POINT('Ctrl Pts',(64.1356103907788,3.83731140773162,58.3631276964778));
#166564=CARTESIAN_POINT('Ctrl Pts',(64.176658854597,3.93101765144412,58.3547350478729));
#166565=CARTESIAN_POINT('Ctrl Pts',(64.2010584059769,3.98533442751659,58.3497505804098));
#166566=CARTESIAN_POINT('Ctrl Pts',(64.2880222327021,4.17419769256586,58.3319999033415));
#166567=CARTESIAN_POINT('Ctrl Pts',(64.3531869243333,4.30747443543313,58.3187240848827));
#166568=CARTESIAN_POINT('Ctrl Pts',(64.5233796491981,4.63596255462977,58.2841255659868));
#166569=CARTESIAN_POINT('Ctrl Pts',(64.6321198533269,4.82907307667321,58.2620821698103));
#166570=CARTESIAN_POINT('Ctrl Pts',(64.8918203435309,5.25482656633036,58.2096626561683));
#166571=CARTESIAN_POINT('Ctrl Pts',(65.046385783662,5.48494807235221,58.1786110215429));
#166572=CARTESIAN_POINT('Ctrl Pts',(65.4069336383958,5.9739581172662,58.1067839061018));
#166573=CARTESIAN_POINT('Ctrl Pts',(65.6168242144495,6.22941413096834,58.0653392555951));
#166574=CARTESIAN_POINT('Ctrl Pts',(65.8848283569779,6.52264476239926,58.0132415429448));
#166575=CARTESIAN_POINT('Ctrl Pts',(65.9306222360787,6.57168283794933,58.0043665121508));
#166576=CARTESIAN_POINT('Ctrl Pts',(65.9978512917886,6.64214349978431,57.9913806463445));
#166577=CARTESIAN_POINT('Ctrl Pts',(66.0188755589456,6.66396555056729,57.9873256618525));
#166578=CARTESIAN_POINT('Ctrl Pts',(66.056337391677,6.7024733384773,57.980111530446));
#166579=CARTESIAN_POINT('Ctrl Pts',(66.0727328444927,6.71920059729626,57.9769579914442));
#166580=CARTESIAN_POINT('Ctrl Pts',(66.1085864471861,6.7555063847317,57.9700701468326));
#166581=CARTESIAN_POINT('Ctrl Pts',(66.1280683066891,6.77506029231369,57.9663327045083));
#166582=CARTESIAN_POINT('Ctrl Pts',(66.1842390678595,6.83094258158476,57.9555709779972));
#166583=CARTESIAN_POINT('Ctrl Pts',(66.2211396009993,6.86705134104539,57.9485184505943));
#166584=CARTESIAN_POINT('Ctrl Pts',(66.3062464979302,6.94896565995924,57.9322879421562));
#166585=CARTESIAN_POINT('Ctrl Pts',(66.3546434840923,6.9945639287013,57.923083711614));
#166586=CARTESIAN_POINT('Ctrl Pts',(66.5188730674604,7.14602711647788,57.891923372572));
#166587=CARTESIAN_POINT('Ctrl Pts',(66.6368492177105,7.2494645539054,57.8696587999886));
#166588=CARTESIAN_POINT('Ctrl Pts',(66.9930432406784,7.5462632952188,57.8026602317816));
#166589=CARTESIAN_POINT('Ctrl Pts',(67.2381163367901,7.73081873352753,57.7568401022762));
#166590=CARTESIAN_POINT('Ctrl Pts',(67.8413484825217,8.14019029590115,57.6440814531632));
#166591=CARTESIAN_POINT('Ctrl Pts',(68.2064285287763,8.35322982114183,57.575842169));
#166592=CARTESIAN_POINT('Ctrl Pts',(68.6561574217945,8.57613378851909,57.4913254979524));
#166593=CARTESIAN_POINT('Ctrl Pts',(68.728452176626,8.61080570323646,57.4777269728817));
#166594=CARTESIAN_POINT('Ctrl Pts',(68.8435449427241,8.66417823082398,57.4560570162182));
#166595=CARTESIAN_POINT('Ctrl Pts',(68.8860598592975,8.6835047066625,57.4480476894804));
#166596=CARTESIAN_POINT('Ctrl Pts',(68.9626442390345,8.71762214702849,57.4336117200641));
#166597=CARTESIAN_POINT('Ctrl Pts',(68.9966618001168,8.73253195661687,57.4271965628337));
#166598=CARTESIAN_POINT('Ctrl Pts',(69.0766629336065,8.76702391116082,57.4121026809964));
#166599=CARTESIAN_POINT('Ctrl Pts',(69.1227147726885,8.78643804609169,57.4034086681932));
#166600=CARTESIAN_POINT('Ctrl Pts',(69.2575028925935,8.84197916381548,57.3779465626433));
#166601=CARTESIAN_POINT('Ctrl Pts',(69.3466314833654,8.87709579207641,57.3610898604267));
#166602=CARTESIAN_POINT('Ctrl Pts',(69.7487432582385,9.02834969343535,57.2849522709281));
#166603=CARTESIAN_POINT('Ctrl Pts',(70.0671274266133,9.12877731614799,57.2244223562583));
#166604=CARTESIAN_POINT('Ctrl Pts',(70.8373676477867,9.32647079816782,57.0776774276926));
#166605=CARTESIAN_POINT('Ctrl Pts',(71.2923517948619,9.40736026884724,56.9907323209208));
#166606=CARTESIAN_POINT('Ctrl Pts',(71.979129529797,9.47664608914504,56.8602012104029));
#166607=CARTESIAN_POINT('Ctrl Pts',(72.2076153269439,9.49108817887239,56.8168975996582));
#166608=CARTESIAN_POINT('Ctrl Pts',(72.4817890629712,9.49813588071572,56.7652345179813));
#166609=CARTESIAN_POINT('Ctrl Pts',(72.5271525457802,9.49896532260876,56.7566964591517));
#166610=CARTESIAN_POINT('Ctrl Pts',(72.5977324290803,9.49973223228133,56.7434293398238));
#166611=CARTESIAN_POINT('Ctrl Pts',(72.6229443210239,9.49990227262387,56.7386935620761));
#166612=CARTESIAN_POINT('Ctrl Pts',(72.6695933548331,9.50002465368916,56.7299376531561));
#166613=CARTESIAN_POINT('Ctrl Pts',(72.6910298853012,9.50000578912789,56.7259166835128));
#166614=CARTESIAN_POINT('Ctrl Pts',(72.7403648739039,9.49978953698635,56.7166685481759));
#166615=CARTESIAN_POINT('Ctrl Pts',(72.7682631253118,9.49954005495001,56.7114431646031));
#166616=CARTESIAN_POINT('Ctrl Pts',(72.8562956805742,9.49835144245543,56.6949672683449));
#166617=CARTESIAN_POINT('Ctrl Pts',(72.9164250452732,9.49694854588446,56.6837323873429));
#166618=CARTESIAN_POINT('Ctrl Pts',(73.2306780699394,9.48652655700116,56.6250996199903));
#166619=CARTESIAN_POINT('Ctrl Pts',(73.4844231668491,9.4675442330946,56.5780408243862));
#166620=CARTESIAN_POINT('Ctrl Pts',(74.3311218594117,9.36873109314952,56.4213444578738));
#166621=CARTESIAN_POINT('Ctrl Pts',(74.9172950855356,9.24157334392083,56.3133137460433));
#166622=CARTESIAN_POINT('Ctrl Pts',(75.6777403911334,8.99710230269761,56.1716771819452));
#166623=CARTESIAN_POINT('Ctrl Pts',(75.8661696468452,8.9296855204103,56.1364645986918));
#166624=CARTESIAN_POINT('Ctrl Pts',(76.1156397729411,8.83116327839062,56.089656179576));
#166625=CARTESIAN_POINT('Ctrl Pts',(76.1787018474511,8.80544810603254,56.0778074029109));
#166626=CARTESIAN_POINT('Ctrl Pts',(76.2821422055465,8.76192666057605,56.0583442041768));
#166627=CARTESIAN_POINT('Ctrl Pts',(76.3226842767657,8.74452601422051,56.0507087780499));
#166628=CARTESIAN_POINT('Ctrl Pts',(76.4016160559352,8.70997669597214,56.0358293137047));
#166629=CARTESIAN_POINT('Ctrl Pts',(76.4400162399858,8.69285519987277,56.0285839615913));
#166630=CARTESIAN_POINT('Ctrl Pts',(76.53074328329,8.65165805148271,56.0114500705618));
#166631=CARTESIAN_POINT('Ctrl Pts',(76.5829666966652,8.62735314649564,56.0015753129146));
#166632=CARTESIAN_POINT('Ctrl Pts',(76.7599196486291,8.54297779475444,55.9680741110235));
#166633=CARTESIAN_POINT('Ctrl Pts',(76.8835486393362,8.48058409024693,55.944596909408));
#166634=CARTESIAN_POINT('Ctrl Pts',(77.1840346612582,8.32037460543431,55.8873681083627));
#166635=CARTESIAN_POINT('Ctrl Pts',(77.3592148871461,8.21948126215258,55.8538578264081));
#166636=CARTESIAN_POINT('Ctrl Pts',(77.8916498018825,7.88921152618273,55.751640958093));
#166637=CARTESIAN_POINT('Ctrl Pts',(78.236837012401,7.64085749729854,55.6848186048476));
#166638=CARTESIAN_POINT('Ctrl Pts',(78.748450442419,7.21699554661016,55.5857238012496));
#166639=CARTESIAN_POINT('Ctrl Pts',(78.926805324731,7.05733574788239,55.5511727688975));
#166640=CARTESIAN_POINT('Ctrl Pts',(79.1333303485869,6.85775331938775,55.5113231900014));
#166641=CARTESIAN_POINT('Ctrl Pts',(79.1674042680018,6.82432039398413,55.5047540500755));
#166642=CARTESIAN_POINT('Ctrl Pts',(79.2203949721892,6.77153081844813,55.4945485127131));
#166643=CARTESIAN_POINT('Ctrl Pts',(79.2394812566104,6.75235267674756,55.4908748507105));
#166644=CARTESIAN_POINT('Ctrl Pts',(79.2750009730927,6.71635371881951,55.4840426575004));
#166645=CARTESIAN_POINT('Ctrl Pts',(79.2914539975338,6.69955363143591,55.4808798082087));
#166646=CARTESIAN_POINT('Ctrl Pts',(79.3299256628392,6.65997575177617,55.4734884202254));
#166647=CARTESIAN_POINT('Ctrl Pts',(79.351893796531,6.63714725129234,55.4692710175102));
#166648=CARTESIAN_POINT('Ctrl Pts',(79.4241345916666,6.56131716603358,55.4554118423714));
#166649=CARTESIAN_POINT('Ctrl Pts',(79.4739170211828,6.50783286035037,55.4458765512534));
#166650=CARTESIAN_POINT('Ctrl Pts',(79.5937847596349,6.37601841968089,55.422943767704));
#166651=CARTESIAN_POINT('Ctrl Pts',(79.6632059424909,6.29707372856666,55.4096850881321));
#166652=CARTESIAN_POINT('Ctrl Pts',(79.948226373592,5.96184219810876,55.3552920956997));
#166653=CARTESIAN_POINT('Ctrl Pts',(80.1516476416783,5.69513761824494,55.3165688469124));
#166654=CARTESIAN_POINT('Ctrl Pts',(80.5914765342703,5.05018728247726,55.2322601975524));
#166655=CARTESIAN_POINT('Ctrl Pts',(80.8163592090348,4.66479907830197,55.1886603967258));
#166656=CARTESIAN_POINT('Ctrl Pts',(81.0588454266084,4.17276775217562,55.1403700966464));
#166657=CARTESIAN_POINT('Ctrl Pts',(81.1026736434647,4.0800915849361,55.1315810831492));
#166658=CARTESIAN_POINT('Ctrl Pts',(81.1666034884089,3.93906378649308,55.1186620917445));
#166659=CARTESIAN_POINT('Ctrl Pts',(81.1878107359992,3.89123780940432,55.1143588799458));
#166660=CARTESIAN_POINT('Ctrl Pts',(81.2252206886373,3.80496221223433,55.106735246783));
#166661=CARTESIAN_POINT('Ctrl Pts',(81.2415660739167,3.76657793901731,55.1033925025104));
#166662=CARTESIAN_POINT('Ctrl Pts',(81.2759447923359,3.68435290878306,55.0963361039098));
#166663=CARTESIAN_POINT('Ctrl Pts',(81.2939046120829,3.64048166784317,55.0926339834636));
#166664=CARTESIAN_POINT('Ctrl Pts',(81.3419608038894,3.52055122724325,55.0826840494763));
#166665=CARTESIAN_POINT('Ctrl Pts',(81.3714103483635,3.44422892696746,55.076537671794));
#166666=CARTESIAN_POINT('Ctrl Pts',(81.5466344001559,2.97213799971209,55.0396565448256));
#166667=CARTESIAN_POINT('Ctrl Pts',(81.667136108596,2.5671907497471,55.012878823399));
#166668=CARTESIAN_POINT('Ctrl Pts',(81.8688883039445,1.67847989412539,54.9648233998089));
#166669=CARTESIAN_POINT('Ctrl Pts',(81.9406202039826,1.19370601529443,54.945150242408));
#166670=CARTESIAN_POINT('Ctrl Pts',(81.986895659199,0.542753960261524,54.9284747858057));
#166671=CARTESIAN_POINT('Ctrl Pts',(81.9943441450247,0.379830580717261,
54.9251101533736));
#166672=CARTESIAN_POINT('Ctrl Pts',(81.9984871251316,0.177303085997581,
54.9219848611074));
#166673=CARTESIAN_POINT('Ctrl Pts',(81.9990535529322,0.13781745766436,54.9214254268815));
#166674=CARTESIAN_POINT('Ctrl Pts',(81.99952399041,0.0807122232168575,54.9206894370387));
#166675=CARTESIAN_POINT('Ctrl Pts',(81.999621128999,0.0630951403504671,
54.920472439619));
#166676=CARTESIAN_POINT('Ctrl Pts',(81.9997125061064,0.0303480227767184,
54.9200878819032));
#166677=CARTESIAN_POINT('Ctrl Pts',(81.9997193407733,0.0152281085298869,
54.9199177788824));
#166678=CARTESIAN_POINT('Ctrl Pts',(81.9996908076899,9.81597684577923E-5,
54.9197550594462));
#166679=CARTESIAN_POINT('Ctrl Pts',(81.9996908076899,9.81597696801076E-5,
54.9197550594462));
#166680=CARTESIAN_POINT('Ctrl Pts',(81.9996907396986,6.21067117015059E-5,
54.9197546717031));
#166681=CARTESIAN_POINT('Ctrl Pts',(81.9996906904331,3.60530577702464E-5,
54.9197543915294));
#166682=CARTESIAN_POINT('Ctrl Pts',(81.9996906220771,-2.94123145262016E-14,
54.9197540038636));
#166683=CARTESIAN_POINT('Origin',(73.0915550886457,-4.33680868994202E-16,
59.1075264962884));
#166684=CARTESIAN_POINT('',(81.8789250230948,-3.34120657753585E-11,54.2348582579198));
#166685=CARTESIAN_POINT('',(81.8868193065938,3.36461090144049E-11,54.2796289644064));
#166686=CARTESIAN_POINT('',(82.4472287422617,-1.59709532818419E-15,57.4578688084528));
#166687=CARTESIAN_POINT('Ctrl Pts',(81.8789250230948,-6.6822534455389E-11,
54.2348582579198));
#166688=CARTESIAN_POINT('Ctrl Pts',(81.8789508660046,0.0136303569671984,
54.2350048203439));
#166689=CARTESIAN_POINT('Ctrl Pts',(81.8789476450494,0.0272606835137892,
54.2351554847755));
#166690=CARTESIAN_POINT('Ctrl Pts',(81.8788481666303,0.0692657480702391,
54.2356325265563));
#166691=CARTESIAN_POINT('Ctrl Pts',(81.8786550368243,0.0976398929770492,
54.2359726722447));
#166692=CARTESIAN_POINT('Ctrl Pts',(81.8776486538947,0.187147359440565,
54.237103006747));
#166693=CARTESIAN_POINT('Ctrl Pts',(81.8763768729974,0.248273117906502,
54.2379593079502));
#166694=CARTESIAN_POINT('Ctrl Pts',(81.8666825031072,0.567532233263183,
54.242886293918));
#166695=CARTESIAN_POINT('Ctrl Pts',(81.8484297613539,0.825235470181819,
54.2484186926386));
#166696=CARTESIAN_POINT('Ctrl Pts',(81.7510447555305,1.6993262079535,54.2731040882037));
#166697=CARTESIAN_POINT('Ctrl Pts',(81.6226518984717,2.30836761060028,54.3005120704126));
#166698=CARTESIAN_POINT('Ctrl Pts',(81.3791622878337,3.08371269393863,54.3510731391634));
#166699=CARTESIAN_POINT('Ctrl Pts',(81.3160752599985,3.26535601010979,54.3640906268238));
#166700=CARTESIAN_POINT('Ctrl Pts',(81.2234824320398,3.5081956727569,54.3831200279833));
#166701=CARTESIAN_POINT('Ctrl Pts',(81.1986887950296,3.57121042141983,54.3882089393183));
#166702=CARTESIAN_POINT('Ctrl Pts',(81.1565472718624,3.67507700839285,54.3968484931838));
#166703=CARTESIAN_POINT('Ctrl Pts',(81.139576772074,3.71608537315862,54.4003251244743));
#166704=CARTESIAN_POINT('Ctrl Pts',(81.1057333739227,3.79628661606075,54.4072535887144));
#166705=CARTESIAN_POINT('Ctrl Pts',(81.0888821125161,3.83548784540568,54.410701173171));
#166706=CARTESIAN_POINT('Ctrl Pts',(81.048079835128,3.928686896371,54.4190436538633));
#166707=CARTESIAN_POINT('Ctrl Pts',(81.0238917826987,3.98257480078041,54.4239850429927));
#166708=CARTESIAN_POINT('Ctrl Pts',(80.9385095351167,4.16818205768405,54.441413453742));
#166709=CARTESIAN_POINT('Ctrl Pts',(80.8748362528023,4.29869237429813,54.4543863134589));
#166710=CARTESIAN_POINT('Ctrl Pts',(80.7095866810805,4.61869838952139,54.4879840030721));
#166711=CARTESIAN_POINT('Ctrl Pts',(80.6045677206145,4.80625282979567,54.5092774247772));
#166712=CARTESIAN_POINT('Ctrl Pts',(80.3478371335481,5.23042888140658,54.5611186516719));
#166713=CARTESIAN_POINT('Ctrl Pts',(80.1918445821812,5.46412296194305,54.5924708543749));
#166714=CARTESIAN_POINT('Ctrl Pts',(79.826149960122,5.9624954624937,54.6653538029573));
#166715=CARTESIAN_POINT('Ctrl Pts',(79.612231374794,6.22349694401463,54.7076090363644));
#166716=CARTESIAN_POINT('Ctrl Pts',(79.3394896120106,6.52198523683414,54.7606295719624));
#166717=CARTESIAN_POINT('Ctrl Pts',(79.2935224220743,6.57121701320449,54.7695384145081));
#166718=CARTESIAN_POINT('Ctrl Pts',(79.2260847790901,6.64190204656182,54.7825647339134));
#166719=CARTESIAN_POINT('Ctrl Pts',(79.205028934959,6.66375832683685,54.7866258512179));
#166720=CARTESIAN_POINT('Ctrl Pts',(79.1675325214451,6.70230365103613,54.7938467012514));
#166721=CARTESIAN_POINT('Ctrl Pts',(79.1511343604701,6.71903451277881,54.7970007869954));
#166722=CARTESIAN_POINT('Ctrl Pts',(79.1153016756083,6.75532088816186,54.8038846663024));
#166723=CARTESIAN_POINT('Ctrl Pts',(79.0958436690304,6.77485201336231,54.807617566779));
#166724=CARTESIAN_POINT('Ctrl Pts',(79.0398099107747,6.83060189973919,54.818353156453));
#166725=CARTESIAN_POINT('Ctrl Pts',(79.0030241224877,6.86660271053121,54.825383874013));
#166726=CARTESIAN_POINT('Ctrl Pts',(78.6788861540233,7.17863476839374,54.8872007384371));
#166727=CARTESIAN_POINT('Ctrl Pts',(78.3747179465517,7.43614432683576,54.9443111089608));
#166728=CARTESIAN_POINT('Ctrl Pts',(77.6348460892549,7.98554888392823,55.0827817430526));
#166729=CARTESIAN_POINT('Ctrl Pts',(77.1893145608434,8.26150667456777,55.1658837232267));
#166730=CARTESIAN_POINT('Ctrl Pts',(76.644500425792,8.53846395991299,55.2681980457221));
#166731=CARTESIAN_POINT('Ctrl Pts',(76.5648424787215,8.57753079452375,55.2831719879763));
#166732=CARTESIAN_POINT('Ctrl Pts',(76.4365305345214,8.63819122410475,55.307317617881));
#166733=CARTESIAN_POINT('Ctrl Pts',(76.3882182924372,8.66052411349516,55.3164147294697));
#166734=CARTESIAN_POINT('Ctrl Pts',(76.3018910505516,8.69953078205289,55.3326806672048));
#166735=CARTESIAN_POINT('Ctrl Pts',(76.2639488028959,8.71636864761554,55.3398334464921));
#166736=CARTESIAN_POINT('Ctrl Pts',(76.1841860456536,8.75112546027824,55.3548778877595));
#166737=CARTESIAN_POINT('Ctrl Pts',(76.1423447996391,8.76899202374362,55.3627742065991));
#166738=CARTESIAN_POINT('Ctrl Pts',(76.0316160511195,8.81531180539807,55.3836828688425));
#166739=CARTESIAN_POINT('Ctrl Pts',(75.9625211060265,8.84323920870426,55.3967419332811));
#166740=CARTESIAN_POINT('Ctrl Pts',(75.6190326135437,8.97726592596113,55.4617208538378));
#166741=CARTESIAN_POINT('Ctrl Pts',(75.3401900846677,9.07099204479333,55.5146624714897));
#166742=CARTESIAN_POINT('Ctrl Pts',(74.7226909777175,9.24617518968099,55.6321860828827));
#166743=CARTESIAN_POINT('Ctrl Pts',(74.3829665550192,9.32204832449705,55.6970261548631));
#166744=CARTESIAN_POINT('Ctrl Pts',(73.6586800511553,9.44112818631614,55.8351096031619));
#166745=CARTESIAN_POINT('Ctrl Pts',(73.2740190077182,9.47965912719769,55.908354911667));
#166746=CARTESIAN_POINT('Ctrl Pts',(72.8206254254149,9.49629982567009,55.9939291275275));
#166747=CARTESIAN_POINT('Ctrl Pts',(72.7532121337388,9.49803009235094,56.0066327416));
#166748=CARTESIAN_POINT('Ctrl Pts',(72.6594695466927,9.49940224190416,56.0242651810636));
#166749=CARTESIAN_POINT('Ctrl Pts',(72.6331548481899,9.49967420555681,56.029211234575));
#166750=CARTESIAN_POINT('Ctrl Pts',(72.5851539572848,9.49996380503658,56.0382264425493));
#166751=CARTESIAN_POINT('Ctrl Pts',(72.563468330438,9.50001777653254,56.0422967064649));
#166752=CARTESIAN_POINT('Ctrl Pts',(72.5183241916775,9.49997012928969,56.0507643910986));
#166753=CARTESIAN_POINT('Ctrl Pts',(72.494865876502,9.4998554390896,56.0551613488345));
#166754=CARTESIAN_POINT('Ctrl Pts',(72.4328169921833,9.49931420144246,56.0667837963582));
#166755=CARTESIAN_POINT('Ctrl Pts',(72.3942272601592,9.49873421122485,56.074004089741));
#166756=CARTESIAN_POINT('Ctrl Pts',(72.212215595854,9.49485056124079,56.1080248922559));
#166757=CARTESIAN_POINT('Ctrl Pts',(72.0688606116671,9.48842873925612,56.1347198674065));
#166758=CARTESIAN_POINT('Ctrl Pts',(71.6367381851645,9.45891417901261,56.214991945299));
#166759=CARTESIAN_POINT('Ctrl Pts',(71.3487921177771,9.42552022242463,56.2682205815093));
#166760=CARTESIAN_POINT('Ctrl Pts',(70.477500788138,9.28248547054327,56.4292516546246));
#166761=CARTESIAN_POINT('Ctrl Pts',(69.9024915634766,9.12994561566432,56.5355711132637));
#166762=CARTESIAN_POINT('Ctrl Pts',(69.2504703161442,8.88758425827938,56.6576107863682));
#166763=CARTESIAN_POINT('Ctrl Pts',(69.1557154533756,8.85056859462303,56.6753811452198));
#166764=CARTESIAN_POINT('Ctrl Pts',(69.0136207885224,8.79233426904305,56.7020855992691));
#166765=CARTESIAN_POINT('Ctrl Pts',(68.9658254879533,8.77227470960467,56.7110776401391));
#166766=CARTESIAN_POINT('Ctrl Pts',(68.8802976518815,8.73552890277593,56.7271861877469));
#166767=CARTESIAN_POINT('Ctrl Pts',(68.8425044647696,8.71899080427367,56.7343105009408));
#166768=CARTESIAN_POINT('Ctrl Pts',(68.7620896460758,8.68315799340499,56.7494827299075));
#166769=CARTESIAN_POINT('Ctrl Pts',(68.7195005396518,8.66379129253889,56.7575263107204));
#166770=CARTESIAN_POINT('Ctrl Pts',(68.6039790183743,8.61019743373174,56.7793663172837));
#166771=CARTESIAN_POINT('Ctrl Pts',(68.5313380471226,8.57533606817214,56.7931236518591));
#166772=CARTESIAN_POINT('Ctrl Pts',(68.0422632332377,8.33270913423026,56.8859096946526));
#166773=CARTESIAN_POINT('Ctrl Pts',(67.6412496836092,8.09456302332125,56.9628307255044));
#166774=CARTESIAN_POINT('Ctrl Pts',(66.8761160733876,7.55861129633076,57.1105089703873));
#166775=CARTESIAN_POINT('Ctrl Pts',(66.5131986017449,7.26134116772372,57.181029454186));
#166776=CARTESIAN_POINT('Ctrl Pts',(66.1285695959665,6.89494726396894,57.2552998206332));
#166777=CARTESIAN_POINT('Ctrl Pts',(66.0840576129619,6.85169835870725,57.2638865848842));
#166778=CARTESIAN_POINT('Ctrl Pts',(66.018880305953,6.78710705952695,57.2764435905706));
#166779=CARTESIAN_POINT('Ctrl Pts',(65.9978903534727,6.76610846235605,57.2804849518767));
#166780=CARTESIAN_POINT('Ctrl Pts',(65.9605716806631,6.72842034416463,57.2876651197337));
#166781=CARTESIAN_POINT('Ctrl Pts',(65.9442060142965,6.71176956620389,57.2908120948118));
#166782=CARTESIAN_POINT('Ctrl Pts',(65.9080189807995,6.67467790672599,57.2977664908289));
#166783=CARTESIAN_POINT('Ctrl Pts',(65.8882275018205,6.65420727582768,57.3015673358906));
#166784=CARTESIAN_POINT('Ctrl Pts',(65.8298843045737,6.59331328404003,57.3127647233032));
#166785=CARTESIAN_POINT('Ctrl Pts',(65.7915930315932,6.55263170475197,57.3201044215832));
#166786=CARTESIAN_POINT('Ctrl Pts',(65.7036437432867,6.45751566453136,57.3369457177357));
#166787=CARTESIAN_POINT('Ctrl Pts',(65.6542518903138,6.40283016526812,57.3463909284866));
#166788=CARTESIAN_POINT('Ctrl Pts',(65.4839238826797,6.20975557944587,57.3789336382707));
#166789=CARTESIAN_POINT('Ctrl Pts',(65.3663295438945,6.06836020886151,57.4013491856481));
#166790=CARTESIAN_POINT('Ctrl Pts',(64.8772381868979,5.44413425101124,57.4946297629701));
#166791=CARTESIAN_POINT('Ctrl Pts',(64.5481196569545,4.92880109143663,57.5576414547113));
#166792=CARTESIAN_POINT('Ctrl Pts',(64.2107475951982,4.26792608278854,57.6244488516881));
#166793=CARTESIAN_POINT('Ctrl Pts',(64.1534999542628,4.14981654154612,57.635879660366));
#166794=CARTESIAN_POINT('Ctrl Pts',(64.0768142638135,3.98289882691513,57.6513384508323));
#166795=CARTESIAN_POINT('Ctrl Pts',(64.0553218750463,3.93508125841348,57.6556884524486));
#166796=CARTESIAN_POINT('Ctrl Pts',(64.018543749879,3.85141575252323,57.663163629565));
#166797=CARTESIAN_POINT('Ctrl Pts',(64.0030821473655,3.81564900553301,57.6663163365184));
#166798=CARTESIAN_POINT('Ctrl Pts',(63.9710912080004,3.74038218419297,57.6728611764342));
#166799=CARTESIAN_POINT('Ctrl Pts',(63.9546075388912,3.70086303365946,57.6762461411081));
#166800=CARTESIAN_POINT('Ctrl Pts',(63.9157119534642,3.60581571198785,57.6842644662583));
#166801=CARTESIAN_POINT('Ctrl Pts',(63.8935544206719,3.55018210214804,57.6888579456023));
#166802=CARTESIAN_POINT('Ctrl Pts',(63.8177631276299,3.35454759700674,57.7046625521922));
#166803=CARTESIAN_POINT('Ctrl Pts',(63.7668931790818,3.21346542895748,57.7154398678302));
#166804=CARTESIAN_POINT('Ctrl Pts',(63.6494138935544,2.86193791026962,57.7407665878182));
#166805=CARTESIAN_POINT('Ctrl Pts',(63.5867159741442,2.65023492558059,57.7546944865716));
#166806=CARTESIAN_POINT('Ctrl Pts',(63.4497907887842,2.12145917454508,57.7861633185172));
#166807=CARTESIAN_POINT('Ctrl Pts',(63.3842687511748,1.802339396006,57.802273113305));
#166808=CARTESIAN_POINT('Ctrl Pts',(63.2774695783862,1.10411678499286,57.8309157425616));
#166809=CARTESIAN_POINT('Ctrl Pts',(63.242246431142,0.724605983936422,57.8423618071329));
#166810=CARTESIAN_POINT('Ctrl Pts',(63.2271978994398,0.276578358908958,
57.8504831423012));
#166811=CARTESIAN_POINT('Ctrl Pts',(63.2256384359945,0.20921276297513,57.8515609702238));
#166812=CARTESIAN_POINT('Ctrl Pts',(63.2244325871052,0.114443402103744,
57.8528712535952));
#166813=CARTESIAN_POINT('Ctrl Pts',(63.2242001055327,0.0870507833191807,
57.8532257840577));
#166814=CARTESIAN_POINT('Ctrl Pts',(63.2239891749179,0.0374407803890094,
57.8538236394618));
#166815=CARTESIAN_POINT('Ctrl Pts',(63.2239710200176,0.0152238079495488,
57.8540753146484));
#166816=CARTESIAN_POINT('Ctrl Pts',(63.2240908527852,-0.0305740576833721,
57.8545607719944));
#166817=CARTESIAN_POINT('Ctrl Pts',(63.2242384963419,-0.0541547116533171,
57.8547925284985));
#166818=CARTESIAN_POINT('Ctrl Pts',(63.2248482682202,-0.115703330649285,
57.8553503408347));
#166819=CARTESIAN_POINT('Ctrl Pts',(63.2254473154192,-0.153669774989378,
57.8556476406131));
#166820=CARTESIAN_POINT('Ctrl Pts',(63.2291261640653,-0.323566157002608,
57.8567714442158));
#166821=CARTESIAN_POINT('Ctrl Pts',(63.2346757240404,-0.45543129779514,
57.8570862083068));
#166822=CARTESIAN_POINT('Ctrl Pts',(63.2585072584479,-0.836210276788409,
57.8564562225438));
#166823=CARTESIAN_POINT('Ctrl Pts',(63.2837192864116,-1.08457650910745,
57.854141361867));
#166824=CARTESIAN_POINT('Ctrl Pts',(63.4057142023206,-1.95065142595822,
57.8399114145395));
#166825=CARTESIAN_POINT('Ctrl Pts',(63.5528278126081,-2.5594944699328,57.8189341717185));
#166826=CARTESIAN_POINT('Ctrl Pts',(63.799933403572,-3.26994464349393,57.7827457278398));
#166827=CARTESIAN_POINT('Ctrl Pts',(63.8442901636461,-3.38970248143127,
57.7762206907059));
#166828=CARTESIAN_POINT('Ctrl Pts',(63.910102680954,-3.55703314062706,57.7665067173512));
#166829=CARTESIAN_POINT('Ctrl Pts',(63.9295784938296,-3.60538753336158,
57.7636283627451));
#166830=CARTESIAN_POINT('Ctrl Pts',(63.9642883780948,-3.68957338063784,
57.7584924442084));
#166831=CARTESIAN_POINT('Ctrl Pts',(63.9793484767071,-3.72547684665783,
57.7562621341555));
#166832=CARTESIAN_POINT('Ctrl Pts',(64.0114870623206,-3.80080308331473,
57.7514987007274));
#166833=CARTESIAN_POINT('Ctrl Pts',(64.0286126685412,-3.84020432716331,
57.7489581957445));
#166834=CARTESIAN_POINT('Ctrl Pts',(64.0704611014992,-3.9347382020334,57.7427449037923));
#166835=CARTESIAN_POINT('Ctrl Pts',(64.095441170743,-3.98975222340022,57.7390318203278));
#166836=CARTESIAN_POINT('Ctrl Pts',(64.1858828772381,-4.18401965148234,
57.7255731682155));
#166837=CARTESIAN_POINT('Ctrl Pts',(64.2541720748244,-4.32189891649985,
57.7153841908847));
#166838=CARTESIAN_POINT('Ctrl Pts',(64.4344032182216,-4.66471479959257,
57.6884125803448));
#166839=CARTESIAN_POINT('Ctrl Pts',(64.5505679328568,-4.86726166506303,
57.67095970094));
#166840=CARTESIAN_POINT('Ctrl Pts',(64.9143587859409,-5.45086637805468,
57.6159660764193));
#166841=CARTESIAN_POINT('Ctrl Pts',(65.1817916778534,-5.81847493084467,
57.5751548378277));
#166842=CARTESIAN_POINT('Ctrl Pts',(65.5860218602254,-6.2980178523416,57.512028204186));
#166843=CARTESIAN_POINT('Ctrl Pts',(65.7015127419095,-6.42764553183768,
57.4938487010207));
#166844=CARTESIAN_POINT('Ctrl Pts',(65.851135055557,-6.58659621003425,57.4700543735663));
#166845=CARTESIAN_POINT('Ctrl Pts',(65.8820636022155,-6.61899071049763,
57.4651233376893));
#166846=CARTESIAN_POINT('Ctrl Pts',(65.9314302114396,-6.66997022017942,
57.4572314643077));
#166847=CARTESIAN_POINT('Ctrl Pts',(65.9497204995777,-6.68870239658131,
57.4543029913016));
#166848=CARTESIAN_POINT('Ctrl Pts',(65.98482548799,-6.72435923515315,57.4486732803684));
#166849=CARTESIAN_POINT('Ctrl Pts',(66.0016270908808,-6.74129674603194,
57.4459748986392));
#166850=CARTESIAN_POINT('Ctrl Pts',(66.0423032481958,-6.7819937906323,57.4394330363391));
#166851=CARTESIAN_POINT('Ctrl Pts',(66.0662397327312,-6.80568880243069,
57.4355758544385));
#166852=CARTESIAN_POINT('Ctrl Pts',(66.1510767222687,-6.88877953741214,
57.4218802231341));
#166853=CARTESIAN_POINT('Ctrl Pts',(66.2126381165621,-6.94747069852206,
57.4118974564689));
#166854=CARTESIAN_POINT('Ctrl Pts',(66.3697235215974,-7.09324053084566,
57.3863315077649));
#166855=CARTESIAN_POINT('Ctrl Pts',(66.4662387860024,-7.17918813222846,
57.3705392866961));
#166856=CARTESIAN_POINT('Ctrl Pts',(66.8226848109313,-7.48371188821404,
57.3120017759671));
#166857=CARTESIAN_POINT('Ctrl Pts',(67.0924232362203,-7.69002369457173,
57.2673112570304));
#166858=CARTESIAN_POINT('Ctrl Pts',(67.7330514449455,-8.12706783224505,
57.1611200938878));
#166859=CARTESIAN_POINT('Ctrl Pts',(68.1099820083774,-8.3472931988225,57.0986200697327));
#166860=CARTESIAN_POINT('Ctrl Pts',(68.572937582603,-8.57588874047639,57.022337612544));
#166861=CARTESIAN_POINT('Ctrl Pts',(68.6456349821064,-8.61061877632187,
57.0103713625155));
#166862=CARTESIAN_POINT('Ctrl Pts',(68.761335089652,-8.66405918847396,56.991347881987));
#166863=CARTESIAN_POINT('Ctrl Pts',(68.8040493230036,-8.68339801219653,
56.9843292796573));
#166864=CARTESIAN_POINT('Ctrl Pts',(68.8809730484611,-8.71752688355916,
56.9716978500219));
#166865=CARTESIAN_POINT('Ctrl Pts',(68.9151296580056,-8.73243618537735,
56.9660920056517));
#166866=CARTESIAN_POINT('Ctrl Pts',(68.9954306651665,-8.76691437155132,
56.9529197992289));
#166867=CARTESIAN_POINT('Ctrl Pts',(69.0416442329359,-8.78631575851614,
56.945344481617));
#166868=CARTESIAN_POINT('Ctrl Pts',(69.1768076770679,-8.84177898334242,
56.9232042080925));
#166869=CARTESIAN_POINT('Ctrl Pts',(69.2661546972328,-8.8768351787469,56.9085885694714));
#166870=CARTESIAN_POINT('Ctrl Pts',(69.668656250943,-9.02760907878606,56.8428324364613));
#166871=CARTESIAN_POINT('Ctrl Pts',(69.9872709841347,-9.12774497602621,
56.7910234223515));
#166872=CARTESIAN_POINT('Ctrl Pts',(70.7583380200208,-9.3251187602244,56.6659505502013));
#166873=CARTESIAN_POINT('Ctrl Pts',(71.2139725588415,-9.40608131811315,
56.5923038522454));
#166874=CARTESIAN_POINT('Ctrl Pts',(71.905278372099,-9.47622086434692,56.4798698227964));
#166875=CARTESIAN_POINT('Ctrl Pts',(72.137765776598,-9.49097891025053,56.4419340118233));
#166876=CARTESIAN_POINT('Ctrl Pts',(72.4161768506161,-9.49812560012054,
56.3961994513083));
#166877=CARTESIAN_POINT('Ctrl Pts',(72.4618485953898,-9.49895958954531,
56.3886870813714));
#166878=CARTESIAN_POINT('Ctrl Pts',(72.5328611950074,-9.49973027753006,
56.3769894532961));
#166879=CARTESIAN_POINT('Ctrl Pts',(72.5582000897494,-9.49990115301473,
56.3728121031914));
#166880=CARTESIAN_POINT('Ctrl Pts',(72.6050549047792,-9.50002458677341,
56.3650810705607));
#166881=CARTESIAN_POINT('Ctrl Pts',(72.6265705365697,-9.50000619111442,
56.3615283937108));
#166882=CARTESIAN_POINT('Ctrl Pts',(72.6760506237442,-9.49979122403217,
56.353352328916));
#166883=CARTESIAN_POINT('Ctrl Pts',(72.7040142774998,-9.49954289160944,
56.3487273478871));
#166884=CARTESIAN_POINT('Ctrl Pts',(72.7921228119273,-9.49836072462214,
56.3341422164764));
#166885=CARTESIAN_POINT('Ctrl Pts',(72.8522578038061,-9.49696688788121,
56.3241691651579));
#166886=CARTESIAN_POINT('Ctrl Pts',(73.1655560201388,-9.48664529258244,
56.2721275853992));
#166887=CARTESIAN_POINT('Ctrl Pts',(73.418256203661,-9.46790243833621,56.2298721608435));
#166888=CARTESIAN_POINT('Ctrl Pts',(74.3217552675573,-9.36341829631492,
56.0784405319889));
#166889=CARTESIAN_POINT('Ctrl Pts',(74.9639264179844,-9.21882131945944,
55.9702888207293));
#166890=CARTESIAN_POINT('Ctrl Pts',(75.7365165269794,-8.95629819664322,
55.8419655296463));
#166891=CARTESIAN_POINT('Ctrl Pts',(75.885553953018,-8.90135911607756,55.8172890738096));
#166892=CARTESIAN_POINT('Ctrl Pts',(76.0913875267459,-8.81944087105524,
55.7833319445627));
#166893=CARTESIAN_POINT('Ctrl Pts',(76.149387730611,-8.79567689567379,55.7737772346591));
#166894=CARTESIAN_POINT('Ctrl Pts',(76.2428939701221,-8.75625881280899,
55.7583962853958));
#166895=CARTESIAN_POINT('Ctrl Pts',(76.2785451965742,-8.74096704708965,
55.7525374033601));
#166896=CARTESIAN_POINT('Ctrl Pts',(76.3529119105924,-8.70851815904882,
55.7403275109274));
#166897=CARTESIAN_POINT('Ctrl Pts',(76.3916086373921,-8.69131870456047,
55.7339806309303));
#166898=CARTESIAN_POINT('Ctrl Pts',(76.4836535109801,-8.64965481823642,
55.7188994579816));
#166899=CARTESIAN_POINT('Ctrl Pts',(76.5368937939655,-8.62494794706429,
55.7101888993659));
#166900=CARTESIAN_POINT('Ctrl Pts',(76.7205047765371,-8.5376267954686,55.6801921840591));
#166901=CARTESIAN_POINT('Ctrl Pts',(76.8496855113463,-8.47247084083345,
55.6591648638758));
#166902=CARTESIAN_POINT('Ctrl Pts',(77.1666748686668,-8.30324721147573,
55.6077474973792));
#166903=CARTESIAN_POINT('Ctrl Pts',(77.3525625007767,-8.19563834196867,
55.5777583106651));
#166904=CARTESIAN_POINT('Ctrl Pts',(77.773915924229,-7.93197952498977,55.5100781517785));
#166905=CARTESIAN_POINT('Ctrl Pts',(78.0064282629588,-7.77145640037084,
55.4729586453456));
#166906=CARTESIAN_POINT('Ctrl Pts',(78.4972544724062,-7.3988314658469,55.3947947015783));
#166907=CARTESIAN_POINT('Ctrl Pts',(78.7522817881167,-7.18291270359349,
55.3543111075302));
#166908=CARTESIAN_POINT('Ctrl Pts',(79.0444484044455,-6.90755413542126,
55.3076787877871));
#166909=CARTESIAN_POINT('Ctrl Pts',(79.0929805906219,-6.86082047728686,
55.2999233264019));
#166910=CARTESIAN_POINT('Ctrl Pts',(79.1626827439834,-6.79224426083568,
55.2887664892603));
#166911=CARTESIAN_POINT('Ctrl Pts',(79.1842508306468,-6.77081806001443,
55.2853115947057));
#166912=CARTESIAN_POINT('Ctrl Pts',(79.2222974921599,-6.73265380900773,
55.2792118733245));
#166913=CARTESIAN_POINT('Ctrl Pts',(79.2388174258855,-6.71595836491827,
55.2765615784987));
#166914=CARTESIAN_POINT('Ctrl Pts',(79.2746581365841,-6.67946481788585,
55.2708076326853));
#166915=CARTESIAN_POINT('Ctrl Pts',(79.2939546116864,-6.65964294332387,
55.2677072283126));
#166916=CARTESIAN_POINT('Ctrl Pts',(79.349064453543,-6.60253154610103,55.2588461209575));
#166917=CARTESIAN_POINT('Ctrl Pts',(79.3846608724563,-6.56502956540398,
55.2531146342129));
#166918=CARTESIAN_POINT('Ctrl Pts',(79.465389928753,-6.47856590752355,55.2401016001979));
#166919=CARTESIAN_POINT('Ctrl Pts',(79.5103183369713,-6.42941302455843,
55.2328487405332));
#166920=CARTESIAN_POINT('Ctrl Pts',(79.6594406695574,-6.2627632297597,55.2087507656911));
#166921=CARTESIAN_POINT('Ctrl Pts',(79.7612488871114,-6.14311641577636,
55.1922572283434));
#166922=CARTESIAN_POINT('Ctrl Pts',(80.0543689978334,-5.78074472302806,
55.144765871526));
#166923=CARTESIAN_POINT('Ctrl Pts',(80.2369286860602,-5.53102845992008,
55.1151872839117));
#166924=CARTESIAN_POINT('Ctrl Pts',(80.6416529865645,-4.91675761972446,
55.0502225694924));
#166925=CARTESIAN_POINT('Ctrl Pts',(80.8522504426097,-4.54517360435976,
55.0169562099889));
#166926=CARTESIAN_POINT('Ctrl Pts',(81.0727673905489,-4.08738135198437,
54.9832929442761));
#166927=CARTESIAN_POINT('Ctrl Pts',(81.1070600590357,-4.0138196860199,54.9780972737369));
#166928=CARTESIAN_POINT('Ctrl Pts',(81.1598593454323,-3.89670774517398,
54.9701633855689));
#166929=CARTESIAN_POINT('Ctrl Pts',(81.1789803206142,-3.85344709032269,
54.9673046508416));
#166930=CARTESIAN_POINT('Ctrl Pts',(81.212739221421,-3.77551870705794,54.9622841303363));
#166931=CARTESIAN_POINT('Ctrl Pts',(81.2274938012511,-3.74090409293813,
54.9600994412905));
#166932=CARTESIAN_POINT('Ctrl Pts',(81.2616301531713,-3.65949864970567,
54.9550677879093));
#166933=CARTESIAN_POINT('Ctrl Pts',(81.2808470409104,-3.61263794347518,
54.9522531477322));
#166934=CARTESIAN_POINT('Ctrl Pts',(81.3358316311714,-3.4754832274807,54.9442531137681));
#166935=CARTESIAN_POINT('Ctrl Pts',(81.370607811285,-3.38478754374128,54.9392619836735));
#166936=CARTESIAN_POINT('Ctrl Pts',(81.5204426026143,-2.97561239319266,
54.9180758590559));
#166937=CARTESIAN_POINT('Ctrl Pts',(81.620085289815,-2.65159856779745,54.9048957123404));
#166938=CARTESIAN_POINT('Ctrl Pts',(81.8166384341606,-1.86766018835391,
54.8811676500175));
#166939=CARTESIAN_POINT('Ctrl Pts',(81.89745242237,-1.40452788131614,54.873636527431));
#166940=CARTESIAN_POINT('Ctrl Pts',(81.9673237249124,-0.705470294435794,
54.8707509279738));
#166941=CARTESIAN_POINT('Ctrl Pts',(81.9820710223955,-0.472851133707171,
54.8711671834158));
#166942=CARTESIAN_POINT('Ctrl Pts',(81.9895821453053,-0.193782710685954,
54.8731626969154));
#166943=CARTESIAN_POINT('Ctrl Pts',(81.9904913381543,-0.14762222435378,
54.8735416781741));
#166944=CARTESIAN_POINT('Ctrl Pts',(81.9913872782568,-0.0758064403519598,
54.8742057332032));
#166945=CARTESIAN_POINT('Ctrl Pts',(81.9916043944257,-0.0501544171433835,
54.8744577003677));
#166946=CARTESIAN_POINT('Ctrl Pts',(81.9917549332481,-0.0163346478941346,
54.8748091295772));
#166947=CARTESIAN_POINT('Ctrl Pts',(81.9917808534907,-0.00816731848436852,
54.8748954770821));
#166948=CARTESIAN_POINT('Ctrl Pts',(81.9917963385783,-6.66906343255317E-11,
54.8749832973778));
#166949=CARTESIAN_POINT('Ctrl Pts',(81.9996906220771,-2.94123145262016E-14,
54.9197540038636));
#166950=CARTESIAN_POINT('Ctrl Pts',(81.9996543914623,-0.0191091568433552,
54.9195485298366));
#166951=CARTESIAN_POINT('Ctrl Pts',(81.9995617236469,-0.0382182903653823,
54.9193550169557));
#166952=CARTESIAN_POINT('Ctrl Pts',(81.9992250716837,-0.0813586940964622,
54.9189449652443));
#166953=CARTESIAN_POINT('Ctrl Pts',(81.998948257421,-0.105389644357322,
54.9187353385));
#166954=CARTESIAN_POINT('Ctrl Pts',(81.9976699366931,-0.189291046894798,
54.9180684917672));
#166955=CARTESIAN_POINT('Ctrl Pts',(81.9962033782377,-0.249153755475308,
54.9177083467591));
#166956=CARTESIAN_POINT('Ctrl Pts',(81.9765111417756,-0.832234119781761,
54.9153034916425));
#166957=CARTESIAN_POINT('Ctrl Pts',(81.916471825102,-1.35317638216592,54.9217658501432));
#166958=CARTESIAN_POINT('Ctrl Pts',(81.7467604813164,-2.20695625026125,
54.9444969621447));
#166959=CARTESIAN_POINT('Ctrl Pts',(81.6607438020665,-2.54341034204183,
54.9567229066047));
#166960=CARTESIAN_POINT('Ctrl Pts',(81.4957573764999,-3.06835540692492,
54.9806785851731));
#166961=CARTESIAN_POINT('Ctrl Pts',(81.4286432669879,-3.26032648788813,
54.990516751523));
#166962=CARTESIAN_POINT('Ctrl Pts',(81.3313881941951,-3.51244678510232,
55.0048560190491));
#166963=CARTESIAN_POINT('Ctrl Pts',(81.3066352655041,-3.57466324886592,
55.0085119394264));
#166964=CARTESIAN_POINT('Ctrl Pts',(81.2644378631296,-3.67756889565411,
55.0147540431852));
#166965=CARTESIAN_POINT('Ctrl Pts',(81.2473590268853,-3.71840882687804,
55.0172829427844));
#166966=CARTESIAN_POINT('Ctrl Pts',(81.213383603913,-3.79809440488792,55.0223184600511));
#166967=CARTESIAN_POINT('Ctrl Pts',(81.1965111046936,-3.83694943494383,
55.0248213091283));
#166968=CARTESIAN_POINT('Ctrl Pts',(81.1553419359743,-3.93005810722302,
55.0309334200571));
#166969=CARTESIAN_POINT('Ctrl Pts',(81.1307973304866,-3.98419758370011,
55.0345815198751));
#166970=CARTESIAN_POINT('Ctrl Pts',(81.048244816237,-4.16186306782704,55.0468651111836));
#166971=CARTESIAN_POINT('Ctrl Pts',(80.9881051081548,-4.28435615803449,
55.0558349363848));
#166972=CARTESIAN_POINT('Ctrl Pts',(80.6459579998245,-4.945075460852,55.1069994707986));
#166973=CARTESIAN_POINT('Ctrl Pts',(80.3159163833134,-5.45624295152242,
55.1567068571896));
#166974=CARTESIAN_POINT('Ctrl Pts',(79.8271913890805,-6.07474322030209,
55.23234459434));
#166975=CARTESIAN_POINT('Ctrl Pts',(79.7103117904494,-6.21423415781569,
55.2505666829455));
#166976=CARTESIAN_POINT('Ctrl Pts',(79.540903388712,-6.40502026328512,55.277238177257));
#166977=CARTESIAN_POINT('Ctrl Pts',(79.4916251198374,-6.45924054320261,
55.2850257121151));
#166978=CARTESIAN_POINT('Ctrl Pts',(79.4038210992298,-6.5536335452002,55.2989594850689));
#166979=CARTESIAN_POINT('Ctrl Pts',(79.3655558433369,-6.59405186600855,
55.3050506489884));
#166980=CARTESIAN_POINT('Ctrl Pts',(79.3071826448708,-6.65463391888389,
55.3143735982192));
#166981=CARTESIAN_POINT('Ctrl Pts',(79.2873312859905,-6.67505178618935,
55.31754942982));
#166982=CARTESIAN_POINT('Ctrl Pts',(79.2509923349751,-6.71209285138234,
55.323373061447));
#166983=CARTESIAN_POINT('Ctrl Pts',(79.2345341758204,-6.72874530394705,
55.3260143979054));
#166984=CARTESIAN_POINT('Ctrl Pts',(79.1969493636204,-6.76649338762336,
55.3320547916534));
#166985=CARTESIAN_POINT('Ctrl Pts',(79.175785211435,-6.78754975194111,55.335462149535));
#166986=CARTESIAN_POINT('Ctrl Pts',(79.1098791566091,-6.85250373441439,
55.3460902980748));
#166987=CARTESIAN_POINT('Ctrl Pts',(79.0648070478237,-6.89605196577429,
55.3533834840511));
#166988=CARTESIAN_POINT('Ctrl Pts',(78.677979981765,-7.2624456188471,55.4161606131424));
#166989=CARTESIAN_POINT('Ctrl Pts',(78.3134652438269,-7.55945831821165,
55.476492495436));
#166990=CARTESIAN_POINT('Ctrl Pts',(77.5452291460069,-8.09494620565633,
55.6038128585436));
#166991=CARTESIAN_POINT('Ctrl Pts',(77.1427291606947,-8.33288452715957,
55.6705895957359));
#166992=CARTESIAN_POINT('Ctrl Pts',(76.6518948370455,-8.57534623500454,
55.7514667654166));
#166993=CARTESIAN_POINT('Ctrl Pts',(76.5789499483404,-8.61020521221352,
55.7634738740725));
#166994=CARTESIAN_POINT('Ctrl Pts',(76.462946602241,-8.66379618776121,55.7825473341175));
#166995=CARTESIAN_POINT('Ctrl Pts',(76.4201793148645,-8.68316238197663,
55.7895746934616));
#166996=CARTESIAN_POINT('Ctrl Pts',(76.3394281967744,-8.71899471413204,
55.8028346722387));
#166997=CARTESIAN_POINT('Ctrl Pts',(76.3014768602568,-8.73553283198892,
55.8090629855396));
#166998=CARTESIAN_POINT('Ctrl Pts',(76.2155907037222,-8.77227929189866,
55.8231497824531));
#166999=CARTESIAN_POINT('Ctrl Pts',(76.1675952810867,-8.79233943306002,
55.8310160914402));
#167000=CARTESIAN_POINT('Ctrl Pts',(76.02490270769,-8.8505774199943,55.854385813728));
#167001=CARTESIAN_POINT('Ctrl Pts',(75.9297504065972,-8.88759574306452,
55.869947210255));
#167002=CARTESIAN_POINT('Ctrl Pts',(75.2751386841816,-9.12992603753234,
55.9768557513435));
#167003=CARTESIAN_POINT('Ctrl Pts',(74.6979562336475,-9.28244475646385,
56.0702707738278));
#167004=CARTESIAN_POINT('Ctrl Pts',(73.8233210946542,-9.4254961473837,56.2120285197604));
#167005=CARTESIAN_POINT('Ctrl Pts',(73.5341957873921,-9.45890297150018,
56.2589428223652));
#167006=CARTESIAN_POINT('Ctrl Pts',(73.1003189769933,-9.48842642732312,
56.3297599332903));
#167007=CARTESIAN_POINT('Ctrl Pts',(72.9563918679109,-9.49484976773475,
56.3533205160106));
#167008=CARTESIAN_POINT('Ctrl Pts',(72.7736558009451,-9.4987340790332,56.3833624766229));
#167009=CARTESIAN_POINT('Ctrl Pts',(72.734915541674,-9.49931412589773,56.3897387432393));
#167010=CARTESIAN_POINT('Ctrl Pts',(72.6726251672411,-9.4998554131959,56.4000039901323));
#167011=CARTESIAN_POINT('Ctrl Pts',(72.6490759894993,-9.49997011608609,
56.403887772357));
#167012=CARTESIAN_POINT('Ctrl Pts',(72.6037574946716,-9.50001778090229,
56.4113677781855));
#167013=CARTESIAN_POINT('Ctrl Pts',(72.5819883838354,-9.49996381921214,
56.4149635429323));
#167014=CARTESIAN_POINT('Ctrl Pts',(72.5338032426151,-9.49967424663347,
56.4229283235579));
#167015=CARTESIAN_POINT('Ctrl Pts',(72.5073877565322,-9.49940230610399,
56.4272984565549));
#167016=CARTESIAN_POINT('Ctrl Pts',(72.413289332745,-9.49803030629334,56.4428785749982));
#167017=CARTESIAN_POINT('Ctrl Pts',(72.3456206272278,-9.49630026944509,
56.4541059407717));
#167018=CARTESIAN_POINT('Ctrl Pts',(71.9000070444091,-9.48000900730683,
56.5281692111283));
#167019=CARTESIAN_POINT('Ctrl Pts',(71.5233031776256,-9.44300977489737,
56.5913762090154));
#167020=CARTESIAN_POINT('Ctrl Pts',(70.8271386592143,-9.33120543279843,
56.7082311688947));
#167021=CARTESIAN_POINT('Ctrl Pts',(70.5073361164754,-9.26229985036379,
56.761930867608));
#167022=CARTESIAN_POINT('Ctrl Pts',(69.9851626071795,-9.12051769081183,
56.8492191837797));
#167023=CARTESIAN_POINT('Ctrl Pts',(69.7805646262415,-9.05728830369756,
56.8833198619124));
#167024=CARTESIAN_POINT('Ctrl Pts',(69.4399526992648,-8.93898259000179,
56.9398470826378));
#167025=CARTESIAN_POINT('Ctrl Pts',(69.3027668991533,-8.88767220263716,
56.9625463825968));
#167026=CARTESIAN_POINT('Ctrl Pts',(69.1120095988285,-8.81114691545972,
56.9940040100372));
#167027=CARTESIAN_POINT('Ctrl Pts',(69.0574139907513,-8.78864005280026,
57.002995023854));
#167028=CARTESIAN_POINT('Ctrl Pts',(68.9639764294593,-8.74907747383411,
57.018361092331));
#167029=CARTESIAN_POINT('Ctrl Pts',(68.9250333609312,-8.73227418806761,
57.0247588878946));
#167030=CARTESIAN_POINT('Ctrl Pts',(68.850754637804,-8.69962119620557,57.0369492954803));
#167031=CARTESIAN_POINT('Ctrl Pts',(68.8154009484433,-8.68381623454716,
57.0427459629008));
#167032=CARTESIAN_POINT('Ctrl Pts',(68.732538644546,-8.64615160363277,57.0563193431114));
#167033=CARTESIAN_POINT('Ctrl Pts',(68.6851109532613,-8.62411069625395,
57.0640782656713));
#167034=CARTESIAN_POINT('Ctrl Pts',(68.5197760727363,-8.54557896337993,
57.0910912088325));
#167035=CARTESIAN_POINT('Ctrl Pts',(68.4028442360229,-8.48699813083125,
57.1101329793298));
#167036=CARTESIAN_POINT('Ctrl Pts',(67.7510073327286,-8.14314164054218,
57.2159440328911));
#167037=CARTESIAN_POINT('Ctrl Pts',(67.2428799584556,-7.80847175235973,
57.2970120852495));
#167038=CARTESIAN_POINT('Ctrl Pts',(66.627189069515,-7.31124077189001,57.3949564037384));
#167039=CARTESIAN_POINT('Ctrl Pts',(66.4876501584309,-7.19163359982041,
57.417142723216));
#167040=CARTESIAN_POINT('Ctrl Pts',(66.2971008723498,-7.01836649131229,
57.4475051916297));
#167041=CARTESIAN_POINT('Ctrl Pts',(66.2431203892434,-6.96811075817676,
57.4561143787328));
#167042=CARTESIAN_POINT('Ctrl Pts',(66.1492286410241,-6.87861501678154,
57.4711101711093));
#167043=CARTESIAN_POINT('Ctrl Pts',(66.1090689851143,-6.83964663452938,
57.4775312587777));
#167044=CARTESIAN_POINT('Ctrl Pts',(66.0489531754694,-6.78026439983104,
57.4871567023407));
#167045=CARTESIAN_POINT('Ctrl Pts',(66.0287412636062,-6.76011679026062,
57.4903952938556));
#167046=CARTESIAN_POINT('Ctrl Pts',(65.992116320494,-6.72327490259632,57.4962685598051));
#167047=CARTESIAN_POINT('Ctrl Pts',(65.9756738512513,-6.70661122162914,
57.4989071317947));
#167048=CARTESIAN_POINT('Ctrl Pts',(65.9384543237514,-6.66860858741753,
57.5048839392775));
#167049=CARTESIAN_POINT('Ctrl Pts',(65.9177157499812,-6.64723180845958,
57.5082170554009));
#167050=CARTESIAN_POINT('Ctrl Pts',(65.8539141451404,-6.58083989389841,
57.5184792056073));
#167051=CARTESIAN_POINT('Ctrl Pts',(65.8111922500503,-6.53549217524235,
57.525362048434));
#167052=CARTESIAN_POINT('Ctrl Pts',(65.4496562707306,-6.1440376390254,57.5836814772186));
#167053=CARTESIAN_POINT('Ctrl Pts',(65.1564237324558,-5.77466682140244,
57.6314437786339));
#167054=CARTESIAN_POINT('Ctrl Pts',(64.6271696504826,-4.99559301651045,
57.7166203379356));
#167055=CARTESIAN_POINT('Ctrl Pts',(64.3917609229367,-4.58707441697464,
57.7539296414042));
#167056=CARTESIAN_POINT('Ctrl Pts',(64.1517249399031,-4.08906171839117,
57.7905775941932));
#167057=CARTESIAN_POINT('Ctrl Pts',(64.1172450994925,-4.01513169422822,
57.7958021848038));
#167058=CARTESIAN_POINT('Ctrl Pts',(64.0642271782468,-3.89756843503945,
57.8037694993107));
#167059=CARTESIAN_POINT('Ctrl Pts',(64.0450664606938,-3.85422880773364,
57.8066343636464));
#167060=CARTESIAN_POINT('Ctrl Pts',(64.0096103182798,-3.77240039580295,
57.8119076001293));
#167061=CARTESIAN_POINT('Ctrl Pts',(63.9932442203614,-3.73394437312935,
57.8143298579128));
#167062=CARTESIAN_POINT('Ctrl Pts',(63.9568763421477,-3.64692001379552,
57.8196852868362));
#167063=CARTESIAN_POINT('Ctrl Pts',(63.9370199792312,-3.59829065424796,
57.822589957312));
#167064=CARTESIAN_POINT('Ctrl Pts',(63.8793667194219,-3.4537245527429,57.830965167705));
#167065=CARTESIAN_POINT('Ctrl Pts',(63.8427075241937,-3.35732966191139,
57.8362128357817));
#167066=CARTESIAN_POINT('Ctrl Pts',(63.6025406495692,-2.69394374354582,
57.8700416488785));
#167067=CARTESIAN_POINT('Ctrl Pts',(63.4508759665109,-2.10912859135389,
57.8884235627262));
#167068=CARTESIAN_POINT('Ctrl Pts',(63.3078994743928,-1.22309465822339,
57.9011693501972));
#167069=CARTESIAN_POINT('Ctrl Pts',(63.2743271865317,-0.930330914578197,
57.9030245152615));
#167070=CARTESIAN_POINT('Ctrl Pts',(63.2442955246402,-0.490899180369177,
57.902634895665));
#167071=CARTESIAN_POINT('Ctrl Pts',(63.2376615307871,-0.345101527986707,
57.9019874536953));
#167072=CARTESIAN_POINT('Ctrl Pts',(63.2334647197337,-0.159962073948043,
57.9005485740808));
#167073=CARTESIAN_POINT('Ctrl Pts',(63.2328158312106,-0.120706127649299,
57.9002083406172));
#167074=CARTESIAN_POINT('Ctrl Pts',(63.2321600363581,-0.0575831912739143,
57.8996057915336));
#167075=CARTESIAN_POINT('Ctrl Pts',(63.2320011701347,-0.0337180265013591,
57.8993652388043));
#167076=CARTESIAN_POINT('Ctrl Pts',(63.2318668976233,0.0122105293043752,
57.8988780519747));
#167077=CARTESIAN_POINT('Ctrl Pts',(63.2318785485024,0.034273637622909,
57.8986332777915));
#167078=CARTESIAN_POINT('Ctrl Pts',(63.2320728638578,0.0831114681549032,
57.8980674381057));
#167079=CARTESIAN_POINT('Ctrl Pts',(63.2322915224963,0.109885848235369,
57.8977412392575));
#167080=CARTESIAN_POINT('Ctrl Pts',(63.2334698568543,0.20527008881406,57.8965213928946));
#167081=CARTESIAN_POINT('Ctrl Pts',(63.2350535136951,0.273868947417529,
57.8955376158625));
#167082=CARTESIAN_POINT('Ctrl Pts',(63.2506255019945,0.73438064848014,57.8881935330277));
#167083=CARTESIAN_POINT('Ctrl Pts',(63.2878766102646,1.1250722932481,57.8783489777953));
#167084=CARTESIAN_POINT('Ctrl Pts',(63.4035972359396,1.86043661932604,57.8518033047862));
#167085=CARTESIAN_POINT('Ctrl Pts',(63.4774422076243,2.20520464142053,57.8359139645466));
#167086=CARTESIAN_POINT('Ctrl Pts',(63.6487563344907,2.83442980456629,57.7999334307641));
#167087=CARTESIAN_POINT('Ctrl Pts',(63.7410106299812,3.11990054383761,57.7808353102243));
#167088=CARTESIAN_POINT('Ctrl Pts',(63.8729625574057,3.47118158272536,57.7536996086356));
#167089=CARTESIAN_POINT('Ctrl Pts',(63.9003698276564,3.54160828277167,57.7480718247532));
#167090=CARTESIAN_POINT('Ctrl Pts',(63.9458134971997,3.6544228307231,57.7387527695002));
#167091=CARTESIAN_POINT('Ctrl Pts',(63.9633316139623,3.69702419853088,57.735163125661));
#167092=CARTESIAN_POINT('Ctrl Pts',(63.9973999085118,3.77820603078778,57.7281872559331));
#167093=CARTESIAN_POINT('Ctrl Pts',(64.0138982566356,3.81680792879478,57.7248112019246));
#167094=CARTESIAN_POINT('Ctrl Pts',(64.0521022480339,3.90459577177927,57.7169983783234));
#167095=CARTESIAN_POINT('Ctrl Pts',(64.0739682143242,3.95370754775727,57.7125301615332));
#167096=CARTESIAN_POINT('Ctrl Pts',(64.1333214779202,4.08405404421362,57.7004107319849));
#167097=CARTESIAN_POINT('Ctrl Pts',(64.171530506634,4.16494085057172,57.6926180815396));
#167098=CARTESIAN_POINT('Ctrl Pts',(64.4439995487114,4.72140993393359,57.6371173764298));
#167099=CARTESIAN_POINT('Ctrl Pts',(64.7159929997526,5.17671899593926,57.5819826842037));
#167100=CARTESIAN_POINT('Ctrl Pts',(65.2556278933211,5.92930167012332,57.4742239557703));
#167101=CARTESIAN_POINT('Ctrl Pts',(65.5070327918403,6.23699089422994,57.4245068846877));
#167102=CARTESIAN_POINT('Ctrl Pts',(65.8119182029589,6.56533159150481,57.3653750393213));
#167103=CARTESIAN_POINT('Ctrl Pts',(65.8472491391151,6.60275821621563,57.3585390883402));
#167104=CARTESIAN_POINT('Ctrl Pts',(65.9019726380357,6.65977974048592,57.3479782729481));
#167105=CARTESIAN_POINT('Ctrl Pts',(65.9211492056122,6.67958594173356,57.3442825375604));
#167106=CARTESIAN_POINT('Ctrl Pts',(65.9567826278662,6.71606578115462,57.3374249569922));
#167107=CARTESIAN_POINT('Ctrl Pts',(65.9732153167856,6.73276302986632,57.3342663509451));
#167108=CARTESIAN_POINT('Ctrl Pts',(66.011080373346,6.77095008647839,57.326996737532));
#167109=CARTESIAN_POINT('Ctrl Pts',(66.0325543152087,6.79239712079718,57.3228802417796));
#167110=CARTESIAN_POINT('Ctrl Pts',(66.1020262578688,6.8611108271439,57.3095815367732));
#167111=CARTESIAN_POINT('Ctrl Pts',(66.150424902648,6.9079589477878,57.3003455415892));
#167112=CARTESIAN_POINT('Ctrl Pts',(66.4452173369067,7.18721109030737,57.2442395016016));
#167113=CARTESIAN_POINT('Ctrl Pts',(66.7033999828718,7.40646837788407,57.1957148178854));
#167114=CARTESIAN_POINT('Ctrl Pts',(67.2016338024688,7.78507859305503,57.1024065185077));
#167115=CARTESIAN_POINT('Ctrl Pts',(67.4383506516803,7.94828523885839,57.058200187442));
#167116=CARTESIAN_POINT('Ctrl Pts',(67.8578043862365,8.2097551421779,56.9797654797525));
#167117=CARTESIAN_POINT('Ctrl Pts',(68.0370799036966,8.31336798873816,56.9462134805954));
#167118=CARTESIAN_POINT('Ctrl Pts',(68.34382173419,8.47724345363654,56.8886837590713));
#167119=CARTESIAN_POINT('Ctrl Pts',(68.4695267102784,8.54076784640929,56.8650750377454));
#167120=CARTESIAN_POINT('Ctrl Pts',(68.6489142397303,8.62635149445977,56.8313268052075));
#167121=CARTESIAN_POINT('Ctrl Pts',(68.7014701125895,8.65082272351403,56.8214326882021));
#167122=CARTESIAN_POINT('Ctrl Pts',(68.7925863317653,8.6922127478716,56.8042669976011));
#167123=CARTESIAN_POINT('Ctrl Pts',(68.8310423998376,8.70936626929446,56.7970184058439));
#167124=CARTESIAN_POINT('Ctrl Pts',(68.9099195534317,8.74390681295809,56.7821430558813));
#167125=CARTESIAN_POINT('Ctrl Pts',(68.9503499619508,8.76126896602064,56.7745141888425));
#167126=CARTESIAN_POINT('Ctrl Pts',(69.0531609805942,8.80455375859027,56.7551040152788));
#167127=CARTESIAN_POINT('Ctrl Pts',(69.1156987885475,8.83008036249795,56.7432873442472));
#167128=CARTESIAN_POINT('Ctrl Pts',(69.3601118387648,8.92673466386954,56.6970666396792));
#167129=CARTESIAN_POINT('Ctrl Pts',(69.5438719540856,8.99274928089602,56.6622327958355));
#167130=CARTESIAN_POINT('Ctrl Pts',(70.3045394493982,9.2390655768595,56.5177500921458));
#167131=CARTESIAN_POINT('Ctrl Pts',(70.8958147621585,9.36807306839831,56.4046620349361));
#167132=CARTESIAN_POINT('Ctrl Pts',(71.74764648053,9.46755482196796,56.2425827325765));
#167133=CARTESIAN_POINT('Ctrl Pts',(72.0011474928261,9.48653008343553,56.1944705996034));
#167134=CARTESIAN_POINT('Ctrl Pts',(72.3152302628538,9.49694909810163,56.135220467501));
#167135=CARTESIAN_POINT('Ctrl Pts',(72.3753375021582,9.4983517229637,56.1238979358385));
#167136=CARTESIAN_POINT('Ctrl Pts',(72.4633491342091,9.49954014093796,56.1073466339065));
#167137=CARTESIAN_POINT('Ctrl Pts',(72.4912432732057,9.49978958845323,56.1021049788767));
#167138=CARTESIAN_POINT('Ctrl Pts',(72.5405744468258,9.50000580127886,56.0928426752753));
#167139=CARTESIAN_POINT('Ctrl Pts',(72.5620106458844,9.50002465184133,56.0888204365761));
#167140=CARTESIAN_POINT('Ctrl Pts',(72.6086618487185,9.49990223857548,56.0800725951929));
#167141=CARTESIAN_POINT('Ctrl Pts',(72.6338765846449,9.49973217327249,56.0753479949009));
#167142=CARTESIAN_POINT('Ctrl Pts',(72.7044697574858,9.49896514963176,56.0621300369897));
#167143=CARTESIAN_POINT('Ctrl Pts',(72.7498464041002,9.49813557200794,56.053644536735));
#167144=CARTESIAN_POINT('Ctrl Pts',(73.0241877041815,9.49108494941575,56.0024010596379));
#167145=CARTESIAN_POINT('Ctrl Pts',(73.2529123496641,9.47663356441566,55.9599242027111));
#167146=CARTESIAN_POINT('Ctrl Pts',(73.9402989595516,9.40732134851028,55.832590466458));
#167147=CARTESIAN_POINT('Ctrl Pts',(74.3957579626969,9.3264294074589,55.7486248470616));
#167148=CARTESIAN_POINT('Ctrl Pts',(75.1665981452764,9.12874394520049,55.6057674057952));
#167149=CARTESIAN_POINT('Ctrl Pts',(75.4851651473643,9.02832480097397,55.5465053931756));
#167150=CARTESIAN_POINT('Ctrl Pts',(75.8873724343318,8.87708751583461,55.4711899113413));
#167151=CARTESIAN_POINT('Ctrl Pts',(75.9765188550052,8.84197274638609,55.4544654633048));
#167152=CARTESIAN_POINT('Ctrl Pts',(76.1113215854849,8.786434198187,55.4291254149382));
#167153=CARTESIAN_POINT('Ctrl Pts',(76.1573771759172,8.76702045639009,55.4204589323687));
#167154=CARTESIAN_POINT('Ctrl Pts',(76.2373811344034,8.73252895638724,55.4053882997191));
#167155=CARTESIAN_POINT('Ctrl Pts',(76.2713989404665,8.71761916185326,55.3989751798774));
#167156=CARTESIAN_POINT('Ctrl Pts',(76.3479817100524,8.68350134869854,55.3845261158146));
#167157=CARTESIAN_POINT('Ctrl Pts',(76.3904939261038,8.66417448904742,55.376497158438));
#167158=CARTESIAN_POINT('Ctrl Pts',(76.5055759959553,8.61079975804508,55.3547405493048));
#167159=CARTESIAN_POINT('Ctrl Pts',(76.577858328374,8.57612603714894,55.3410514585676));
#167160=CARTESIAN_POINT('Ctrl Pts',(77.0276679219405,8.35311292487585,55.2557174501453));
#167161=CARTESIAN_POINT('Ctrl Pts',(77.3926498052564,8.13994013275484,55.1857907711019));
#167162=CARTESIAN_POINT('Ctrl Pts',(77.9958719373521,7.73009805731332,55.0695013677019));
#167163=CARTESIAN_POINT('Ctrl Pts',(78.241058279384,7.54518352910079,55.0220138420851));
#167164=CARTESIAN_POINT('Ctrl Pts',(78.5968687876305,7.24827253993063,54.9530965697791));
#167165=CARTESIAN_POINT('Ctrl Pts',(78.7143576984184,7.14514031137337,54.9303407323003));
#167166=CARTESIAN_POINT('Ctrl Pts',(78.8780104389563,6.99408919902902,54.8986981688875));
#167167=CARTESIAN_POINT('Ctrl Pts',(78.9262795293674,6.94858191938103,54.8893723477172));
#167168=CARTESIAN_POINT('Ctrl Pts',(79.0111912884188,6.86681629702483,54.8729852347786));
#167169=CARTESIAN_POINT('Ctrl Pts',(79.0480209787864,6.83076416673249,54.8658837355163));
#167170=CARTESIAN_POINT('Ctrl Pts',(79.1041102809689,6.77495120781602,54.8550805941682));
#167171=CARTESIAN_POINT('Ctrl Pts',(79.1235774834283,6.75540924839076,54.8513333481908));
#167172=CARTESIAN_POINT('Ctrl Pts',(79.1594185899139,6.71911363903007,54.8444389105302));
#167173=CARTESIAN_POINT('Ctrl Pts',(79.1758157178529,6.70238450321822,54.8412865952095));
#167174=CARTESIAN_POINT('Ctrl Pts',(79.2132983974725,6.66385710712737,54.8340847475431));
#167175=CARTESIAN_POINT('Ctrl Pts',(79.2343423323037,6.64201714651654,54.8300443870573));
#167176=CARTESIAN_POINT('Ctrl Pts',(79.3016950774692,6.57143937040763,54.8171214459381));
#167177=CARTESIAN_POINT('Ctrl Pts',(79.3475969891558,6.52230001069604,54.8083273756248));
#167178=CARTESIAN_POINT('Ctrl Pts',(79.6180169411257,6.22654030109073,54.7565768455703));
#167179=CARTESIAN_POINT('Ctrl Pts',(79.8301018884544,5.96842381631564,54.7162228487968));
#167180=CARTESIAN_POINT('Ctrl Pts',(80.1960204684428,5.47168412008226,54.6463427308519));
#167181=CARTESIAN_POINT('Ctrl Pts',(80.353612814115,5.23640337575937,54.6161414988451));
#167182=CARTESIAN_POINT('Ctrl Pts',(80.612529467151,4.80972965763513,54.5660210859414));
#167183=CARTESIAN_POINT('Ctrl Pts',(80.7182460677757,4.62133224023602,54.5453806556852));
#167184=CARTESIAN_POINT('Ctrl Pts',(80.8844059838189,4.30003791327498,54.5125430232452));
#167185=CARTESIAN_POINT('Ctrl Pts',(80.9483537764292,4.16910516569654,54.4997911991359));
#167186=CARTESIAN_POINT('Ctrl Pts',(81.0340152048785,3.98300124835467,54.4825289181419));
#167187=CARTESIAN_POINT('Ctrl Pts',(81.0582434454874,3.92904737559927,54.4776243691093));
#167188=CARTESIAN_POINT('Ctrl Pts',(81.0990908996805,3.83577049978816,54.4693160546135));
#167189=CARTESIAN_POINT('Ctrl Pts',(81.1159498771867,3.79655782666367,54.4658747610282));
#167190=CARTESIAN_POINT('Ctrl Pts',(81.1477507323136,3.72120116370777,54.4593595772727));
#167191=CARTESIAN_POINT('Ctrl Pts',(81.162734497092,3.68507637194616,54.4562791438284));
#167192=CARTESIAN_POINT('Ctrl Pts',(81.2013504639087,3.59033391878792,54.4483119284538));
#167193=CARTESIAN_POINT('Ctrl Pts',(81.2246247789901,3.531567824447,54.4434812469245));
#167194=CARTESIAN_POINT('Ctrl Pts',(81.3048195903584,3.32305529302083,54.4267322493362));
#167195=CARTESIAN_POINT('Ctrl Pts',(81.3585664734141,3.1720780440009,54.4153122128391));
#167196=CARTESIAN_POINT('Ctrl Pts',(81.6153604679569,2.38895760027483,54.3597019091175));
#167197=CARTESIAN_POINT('Ctrl Pts',(81.7561565625459,1.73766512540865,54.3252901811299));
#167198=CARTESIAN_POINT('Ctrl Pts',(81.8569271514174,0.821510333654386,
54.2949775075885));
#167199=CARTESIAN_POINT('Ctrl Pts',(81.8748098085163,0.565284361092315,
54.288437205712));
#167200=CARTESIAN_POINT('Ctrl Pts',(81.8843188155679,0.247674584612399,
54.2829165930799));
#167201=CARTESIAN_POINT('Ctrl Pts',(81.8855682365754,0.186718236933947,
54.2819748184765));
#167202=CARTESIAN_POINT('Ctrl Pts',(81.8865564700108,0.0974115784321152,
54.2807709734858));
#167203=CARTESIAN_POINT('Ctrl Pts',(81.8867458609506,0.0690690495417933,
54.2804148714424));
#167204=CARTESIAN_POINT('Ctrl Pts',(81.8868423009076,0.0271505916043363,
54.279926941574));
#167205=CARTESIAN_POINT('Ctrl Pts',(81.8868450451571,0.0135753215422557,
54.2797749350526));
#167206=CARTESIAN_POINT('Ctrl Pts',(81.8868193065938,6.72938151241379E-11,
54.2796289644064));
#167207=CARTESIAN_POINT('Origin',(73.0915550886457,-4.33680868994202E-16,
59.1075264962884));
#167208=CARTESIAN_POINT('',(81.7660537076114,-5.44047451804188E-12,53.5947332184626));
#167209=CARTESIAN_POINT('',(81.7739479911102,2.25145191314116E-12,53.6395039249478));
#167210=CARTESIAN_POINT('',(82.4472287422617,-1.59709532818419E-15,57.4578688084528));
#167211=CARTESIAN_POINT('Ctrl Pts',(81.7660537076114,-1.08793519407556E-11,
53.5947332184626));
#167212=CARTESIAN_POINT('Ctrl Pts',(81.766089311675,0.0187786941596928,
53.594935139141));
#167213=CARTESIAN_POINT('Ctrl Pts',(81.7660697497931,0.0375572995376573,
53.5951448454953));
#167214=CARTESIAN_POINT('Ctrl Pts',(81.7658885063145,0.0831106075212402,
53.5956726299015));
#167215=CARTESIAN_POINT('Ctrl Pts',(81.7656698513442,0.109884855239771,
53.5959988267661));
#167216=CARTESIAN_POINT('Ctrl Pts',(81.7644915402974,0.205268114732128,
53.5972186589636));
#167217=CARTESIAN_POINT('Ctrl Pts',(81.7629079201996,0.273866125009716,
53.5982024213271));
#167218=CARTESIAN_POINT('Ctrl Pts',(81.747329218689,0.734581573566942,53.6055497270411));
#167219=CARTESIAN_POINT('Ctrl Pts',(81.7100462908909,1.12547632460795,53.6154012865544));
#167220=CARTESIAN_POINT('Ctrl Pts',(81.594204699406,1.8613059481231,53.6419721180145));
#167221=CARTESIAN_POINT('Ctrl Pts',(81.5202657075538,2.20633441514307,53.6578804072962));
#167222=CARTESIAN_POINT('Ctrl Pts',(81.3488968214419,2.83539203505383,53.6938704724558));
#167223=CARTESIAN_POINT('Ctrl Pts',(81.2567482905691,3.12045454484827,53.7129464508605));
#167224=CARTESIAN_POINT('Ctrl Pts',(81.1249480906405,3.47131279343958,53.7400508866665));
#167225=CARTESIAN_POINT('Ctrl Pts',(81.0975505357671,3.54171179529186,53.7456766669679));
#167226=CARTESIAN_POINT('Ctrl Pts',(81.0521192256183,3.65449288038163,53.7549931790221));
#167227=CARTESIAN_POINT('Ctrl Pts',(81.0346031953589,3.69708825898491,53.7585823925088));
#167228=CARTESIAN_POINT('Ctrl Pts',(81.0005361595372,3.77826559731044,53.7655579999387));
#167229=CARTESIAN_POINT('Ctrl Pts',(80.9840368793863,3.81686894571487,53.7689342424537));
#167230=CARTESIAN_POINT('Ctrl Pts',(80.945826599136,3.90466953481744,53.7767483469641));
#167231=CARTESIAN_POINT('Ctrl Pts',(80.9239551055655,3.95379252712304,53.7812176895887));
#167232=CARTESIAN_POINT('Ctrl Pts',(80.8645769792569,4.08418981395652,53.7933421840864));
#167233=CARTESIAN_POINT('Ctrl Pts',(80.8263476963176,4.16511574105258,53.8011389535829));
#167234=CARTESIAN_POINT('Ctrl Pts',(80.5541150543673,4.7210670533362,53.856591386042));
#167235=CARTESIAN_POINT('Ctrl Pts',(80.2824691179467,5.17586792222044,53.9116556106604));
#167236=CARTESIAN_POINT('Ctrl Pts',(79.7430125147178,5.92846932190368,54.0193818686345));
#167237=CARTESIAN_POINT('Ctrl Pts',(79.4913043740192,6.23658400322117,54.0691602503405));
#167238=CARTESIAN_POINT('Ctrl Pts',(79.1860624510275,6.56531110064247,54.1283613052804));
#167239=CARTESIAN_POINT('Ctrl Pts',(79.1507268808955,6.60274283164926,54.1351981583995));
#167240=CARTESIAN_POINT('Ctrl Pts',(79.0959976968593,6.65977045457835,54.1457600759643));
#167241=CARTESIAN_POINT('Ctrl Pts',(79.0768201504957,6.67957771830201,54.1494560015092));
#167242=CARTESIAN_POINT('Ctrl Pts',(79.0411858971306,6.71605848665225,54.1563137443743));
#167243=CARTESIAN_POINT('Ctrl Pts',(79.0247533660064,6.73275561183066,54.1594723212229));
#167244=CARTESIAN_POINT('Ctrl Pts',(78.9868899350406,6.7709411156073,54.1667416251171));
#167245=CARTESIAN_POINT('Ctrl Pts',(78.9654174739252,6.7923867337347,54.1708578388394));
#167246=CARTESIAN_POINT('Ctrl Pts',(78.8959552506888,6.86109107270506,54.1841546902176));
#167247=CARTESIAN_POINT('Ctrl Pts',(78.8475650007641,6.90793140714231,54.1933890926434));
#167248=CARTESIAN_POINT('Ctrl Pts',(78.5532008394214,7.18678090178326,54.2494136969507));
#167249=CARTESIAN_POINT('Ctrl Pts',(78.295479288909,7.40569001903707,54.2978527190256));
#167250=CARTESIAN_POINT('Ctrl Pts',(77.7981254176937,7.78378075038857,54.3909973997704));
#167251=CARTESIAN_POINT('Ctrl Pts',(77.5618137061987,7.94679912788598,54.4351283213659));
#167252=CARTESIAN_POINT('Ctrl Pts',(77.142293647711,8.20850395491835,54.5135747900315));
#167253=CARTESIAN_POINT('Ctrl Pts',(76.9625059866902,8.31246863880373,54.5472221954063));
#167254=CARTESIAN_POINT('Ctrl Pts',(76.6549779415856,8.47681683120888,54.6048989047051));
#167255=CARTESIAN_POINT('Ctrl Pts',(76.5290125853886,8.54048629379684,54.6285563795084));
#167256=CARTESIAN_POINT('Ctrl Pts',(76.3493178397523,8.62622472709793,54.6623623166521));
#167257=CARTESIAN_POINT('Ctrl Pts',(76.2967206130346,8.65071711526014,54.6722641967464));
#167258=CARTESIAN_POINT('Ctrl Pts',(76.2055557048802,8.69213170326657,54.6894390311634));
#167259=CARTESIAN_POINT('Ctrl Pts',(76.1670926140245,8.70928932300813,54.6966889350736));
#167260=CARTESIAN_POINT('Ctrl Pts',(76.0930125481498,8.74173094133538,54.710659586924));
#167261=CARTESIAN_POINT('Ctrl Pts',(76.0574133770316,8.75705506989795,54.7173763969815));
#167262=CARTESIAN_POINT('Ctrl Pts',(75.9636750452429,8.79671001447499,54.7350713680082));
#167263=CARTESIAN_POINT('Ctrl Pts',(75.9053871234054,8.8206689587982,54.7460829509784));
#167264=CARTESIAN_POINT('Ctrl Pts',(75.6963697012725,8.90409779949654,54.7856005397252));
#167265=CARTESIAN_POINT('Ctrl Pts',(75.544374851785,8.9601798693336,54.8143943173984));
#167266=CARTESIAN_POINT('Ctrl Pts',(74.7764584901133,9.2207778185887,54.9601245350163));
#167267=CARTESIAN_POINT('Ctrl Pts',(74.1423871569636,9.36365084070184,55.0814246755504));
#167268=CARTESIAN_POINT('Ctrl Pts',(73.2475224556367,9.46777148786138,55.2516873773412));
#167269=CARTESIAN_POINT('Ctrl Pts',(72.9951276850991,9.4866018652505,55.2995880089901));
#167270=CARTESIAN_POINT('Ctrl Pts',(72.6822831747417,9.49696017760314,55.3586040050923));
#167271=CARTESIAN_POINT('Ctrl Pts',(72.6223026888742,9.49835732872119,55.3699025822977));
#167272=CARTESIAN_POINT('Ctrl Pts',(72.534441515006,9.49954185362375,55.3864255298651));
#167273=CARTESIAN_POINT('Ctrl Pts',(72.5065710197733,9.49979060707295,55.3916627259293));
#167274=CARTESIAN_POINT('Ctrl Pts',(72.4572655253772,9.5000060442374,55.4009201855465));
#167275=CARTESIAN_POINT('Ctrl Pts',(72.4358313603421,9.50002461188377,55.4049420326747));
#167276=CARTESIAN_POINT('Ctrl Pts',(72.3891655357367,9.49990156374198,55.413692595416));
#167277=CARTESIAN_POINT('Ctrl Pts',(72.3639341443655,9.49973099490788,55.4184203034165));
#167278=CARTESIAN_POINT('Ctrl Pts',(72.2932499537031,9.49896169398094,55.4316552619596));
#167279=CARTESIAN_POINT('Ctrl Pts',(72.2477989566889,9.49812937607001,55.4401546226488));
#167280=CARTESIAN_POINT('Ctrl Pts',(71.9715978664719,9.49101920390794,55.4917451456631));
#167281=CARTESIAN_POINT('Ctrl Pts',(71.7410925927617,9.47637800073317,55.5345505785301));
#167282=CARTESIAN_POINT('Ctrl Pts',(71.0528728697567,9.40654687555473,55.662033176143));
#167283=CARTESIAN_POINT('Ctrl Pts',(70.5983499454807,9.32559737393371,55.7458276171454));
#167284=CARTESIAN_POINT('Ctrl Pts',(69.8292493820901,9.12808823030405,55.8883657059645));
#167285=CARTESIAN_POINT('Ctrl Pts',(69.5114867796251,9.02785437859029,55.947479454498));
#167286=CARTESIAN_POINT('Ctrl Pts',(69.1101656723436,8.87692203359165,56.0226295482308));
#167287=CARTESIAN_POINT('Ctrl Pts',(69.0211279174825,8.84184564459701,56.0393337001265));
#167288=CARTESIAN_POINT('Ctrl Pts',(68.8864545401026,8.78635656545091,56.0646495113161));
#167289=CARTESIAN_POINT('Ctrl Pts',(68.8404207899903,8.76695091906606,56.0733119070883));
#167290=CARTESIAN_POINT('Ctrl Pts',(68.7604407912212,8.73246816398617,56.0883780592396));
#167291=CARTESIAN_POINT('Ctrl Pts',(68.7264252370218,8.71755869347868,56.0947907683467));
#167292=CARTESIAN_POINT('Ctrl Pts',(68.6498294865343,8.68343362942294,56.1092423120975));
#167293=CARTESIAN_POINT('Ctrl Pts',(68.6073021534936,8.66409893527404,56.1172741445388));
#167294=CARTESIAN_POINT('Ctrl Pts',(68.4921337091477,8.61068113494746,56.1390471454897));
#167295=CARTESIAN_POINT('Ctrl Pts',(68.4197808882597,8.57597054021846,56.1527496490367));
#167296=CARTESIAN_POINT('Ctrl Pts',(67.9651233300583,8.35052706178557,56.2390039158279));
#167297=CARTESIAN_POINT('Ctrl Pts',(67.5957012389091,8.13430902447392,56.3097916254067));
#167298=CARTESIAN_POINT('Ctrl Pts',(66.9786628403738,7.71348127405852,56.4287629763096));
#167299=CARTESIAN_POINT('Ctrl Pts',(66.7243901780782,7.52022027008374,56.4780250396689));
#167300=CARTESIAN_POINT('Ctrl Pts',(66.3694688561866,7.22061335610846,56.5467679879914));
#167301=CARTESIAN_POINT('Ctrl Pts',(66.2608036355152,7.12447830648815,56.567810682016));
#167302=CARTESIAN_POINT('Ctrl Pts',(66.0867033385695,6.96311362972743,56.6014682042626));
#167303=CARTESIAN_POINT('Ctrl Pts',(66.0199535653995,6.8993958990753,56.6143581285272));
#167304=CARTESIAN_POINT('Ctrl Pts',(65.9293917436607,6.81036862447813,56.6318147587271));
#167305=CARTESIAN_POINT('Ctrl Pts',(65.9047843305848,6.78590964943391,56.6365547713395));
#167306=CARTESIAN_POINT('Ctrl Pts',(65.8633915620035,6.74431012431058,56.6445216818408));
#167307=CARTESIAN_POINT('Ctrl Pts',(65.8465370347348,6.72724175290705,56.6477638702909));
#167308=CARTESIAN_POINT('Ctrl Pts',(65.8117710044302,6.69176519442075,56.6544475018772));
#167309=CARTESIAN_POINT('Ctrl Pts',(65.7938690704714,6.67334768426026,56.6578868566572));
#167310=CARTESIAN_POINT('Ctrl Pts',(65.7463937169884,6.62410464340944,56.6670025242646));
#167311=CARTESIAN_POINT('Ctrl Pts',(65.7169512498564,6.59314839645086,56.6726501054801));
#167312=CARTESIAN_POINT('Ctrl Pts',(65.584423839207,6.45190047504579,56.6980497602557));
#167313=CARTESIAN_POINT('Ctrl Pts',(65.4837354091013,6.33929904271823,56.7172881251141));
#167314=CARTESIAN_POINT('Ctrl Pts',(65.0730914342873,5.85730632321677,56.7956588974026));
#167315=CARTESIAN_POINT('Ctrl Pts',(64.7885145284515,5.46645740968215,56.8497818266967));
#167316=CARTESIAN_POINT('Ctrl Pts',(64.4136755499147,4.85909413547504,56.9222177560214));
#167317=CARTESIAN_POINT('Ctrl Pts',(64.2997801843603,4.65857942921805,56.9444181941565));
#167318=CARTESIAN_POINT('Ctrl Pts',(64.1228253630042,4.31884181992413,56.9793513879912));
#167319=CARTESIAN_POINT('Ctrl Pts',(64.055650751179,4.18194362018412,56.9927359564357));
#167320=CARTESIAN_POINT('Ctrl Pts',(63.9665797219404,3.98882781585597,57.0106786875953));
#167321=CARTESIAN_POINT('Ctrl Pts',(63.9419006787588,3.93396074097829,57.0156729519043));
#167322=CARTESIAN_POINT('Ctrl Pts',(63.9005278980066,3.83960168641521,57.0240861126173));
#167323=CARTESIAN_POINT('Ctrl Pts',(63.8835793203608,3.80022707509067,57.0275448986472));
#167324=CARTESIAN_POINT('Ctrl Pts',(63.8517550363479,3.72489882762584,57.0340634388743));
#167325=CARTESIAN_POINT('Ctrl Pts',(63.8368329145727,3.68896638502454,57.0371304454779));
#167326=CARTESIAN_POINT('Ctrl Pts',(63.8024138836432,3.60463245713474,57.0442298263955));
#167327=CARTESIAN_POINT('Ctrl Pts',(63.7830925569564,3.55615838193804,57.0482346709695));
#167328=CARTESIAN_POINT('Ctrl Pts',(63.7176581611327,3.38799749356167,57.0618667765012));
#167329=CARTESIAN_POINT('Ctrl Pts',(63.6735517416903,3.26751974012838,57.0711790909016));
#167330=CARTESIAN_POINT('Ctrl Pts',(63.429555276041,2.55703805104296,57.1234470674421));
#167331=CARTESIAN_POINT('Ctrl Pts',(63.2851253917232,1.94897037145211,57.1577210353531));
#167332=CARTESIAN_POINT('Ctrl Pts',(63.1666622239508,1.08392075099097,57.1906794009407));
#167333=CARTESIAN_POINT('Ctrl Pts',(63.1424296648806,0.835760212641774,
57.1983452148013));
#167334=CARTESIAN_POINT('Ctrl Pts',(63.1200700971016,0.455255564289024,
57.2071683363034));
#167335=CARTESIAN_POINT('Ctrl Pts',(63.1150253214581,0.323459011811552,
57.2096890550143));
#167336=CARTESIAN_POINT('Ctrl Pts',(63.1119928394879,0.153636672107118,
57.2122182595312));
#167337=CARTESIAN_POINT('Ctrl Pts',(63.1115379645799,0.115676936922943,
57.21273737601));
#167338=CARTESIAN_POINT('Ctrl Pts',(63.1111617642863,0.054136416387556,
57.2135030922203));
#167339=CARTESIAN_POINT('Ctrl Pts',(63.1111035839216,0.0305572408797322,
57.2137784196053));
#167340=CARTESIAN_POINT('Ctrl Pts',(63.111157487027,-0.0152400383097263,
57.214277837288));
#167341=CARTESIAN_POINT('Ctrl Pts',(63.1112599297194,-0.0374578964485856,
57.214503944773));
#167342=CARTESIAN_POINT('Ctrl Pts',(63.1116591095197,-0.0870722029593554,
57.2149730047514));
#167343=CARTESIAN_POINT('Ctrl Pts',(63.1119955738653,-0.114468264310403,
57.2152075980197));
#167344=CARTESIAN_POINT('Ctrl Pts',(63.1135614728535,-0.209260586160049,
57.2159356541743));
#167345=CARTESIAN_POINT('Ctrl Pts',(63.115377369187,-0.27664605349559,57.2163068776385));
#167346=CARTESIAN_POINT('Ctrl Pts',(63.1321645750317,-0.725604601534028,
57.2178278532523));
#167347=CARTESIAN_POINT('Ctrl Pts',(63.1689751832739,-1.10602626318967,
57.214541776366));
#167348=CARTESIAN_POINT('Ctrl Pts',(63.2792496235438,-1.80799893656087,
57.2009627838911));
#167349=CARTESIAN_POINT('Ctrl Pts',(63.3468390394394,-2.12991371852061,
57.1917147605416));
#167350=CARTESIAN_POINT('Ctrl Pts',(63.4866173257163,-2.65909406999227,
57.1718431541107));
#167351=CARTESIAN_POINT('Ctrl Pts',(63.5496627790994,-2.8685318306424,57.1627182335516));
#167352=CARTESIAN_POINT('Ctrl Pts',(63.6676123373362,-3.21675006653548,
57.1454795911502));
#167353=CARTESIAN_POINT('Ctrl Pts',(63.7187068458715,-3.3567587597836,57.1379699564294));
#167354=CARTESIAN_POINT('Ctrl Pts',(63.7948446251956,-3.55117565991767,
57.1267346378981));
#167355=CARTESIAN_POINT('Ctrl Pts',(63.8171707819532,-3.60664853390628,
57.1234351441384));
#167356=CARTESIAN_POINT('Ctrl Pts',(63.8563852080932,-3.70150621018156,
57.1176319241774));
#167357=CARTESIAN_POINT('Ctrl Pts',(63.8730217131375,-3.74099549251064,
57.1151676336021));
#167358=CARTESIAN_POINT('Ctrl Pts',(63.9053281270779,-3.8162621156397,57.1103779572939));
#167359=CARTESIAN_POINT('Ctrl Pts',(63.9209531322106,-3.85205822088329,
57.10805960032));
#167360=CARTESIAN_POINT('Ctrl Pts',(63.9622185645461,-3.94503739716452,
57.1019321492266));
#167361=CARTESIAN_POINT('Ctrl Pts',(63.9882013443875,-4.0020628674108,57.0980694252641));
#167362=CARTESIAN_POINT('Ctrl Pts',(64.0813730043895,-4.20133348853111,
57.0842018467488));
#167363=CARTESIAN_POINT('Ctrl Pts',(64.1514990701253,-4.34214426541746,
57.073736295198));
#167364=CARTESIAN_POINT('Ctrl Pts',(64.5276242686246,-5.05284365776764,
57.0174305968665));
#167365=CARTESIAN_POINT('Ctrl Pts',(64.8872203712195,-5.59172393386763,
56.9631928403841));
#167366=CARTESIAN_POINT('Ctrl Pts',(65.3861799682201,-6.19628194310113,
56.8855119893723));
#167367=CARTESIAN_POINT('Ctrl Pts',(65.4767201862364,-6.30122230454004,
56.8713292366245));
#167368=CARTESIAN_POINT('Ctrl Pts',(65.6293416652474,-6.47049138706509,
56.8472395004043));
#167369=CARTESIAN_POINT('Ctrl Pts',(65.6901143975928,-6.53600984312842,
56.8376020928291));
#167370=CARTESIAN_POINT('Ctrl Pts',(65.7754878287027,-6.62548447115215,
56.8239915930124));
#167371=CARTESIAN_POINT('Ctrl Pts',(65.7993204352857,-6.65019225383117,
56.8201845630712));
#167372=CARTESIAN_POINT('Ctrl Pts',(65.8400185530687,-6.69192951249316,
56.8136699056959));
#167373=CARTESIAN_POINT('Ctrl Pts',(65.8568167251176,-6.70902655665234,
56.810977107473));
#167374=CARTESIAN_POINT('Ctrl Pts',(65.8919170522222,-6.7444817686687,56.8053421235555));
#167375=CARTESIAN_POINT('Ctrl Pts',(65.9102297572077,-6.76282865170696,
56.8023976128523));
#167376=CARTESIAN_POINT('Ctrl Pts',(65.9595498707783,-6.81183737592831,
56.7944556713425));
#167377=CARTESIAN_POINT('Ctrl Pts',(65.9906915295878,-6.84235840481285,
56.7894286498668));
#167378=CARTESIAN_POINT('Ctrl Pts',(66.1372954964266,-6.98407011312404,
56.7657105154106));
#167379=CARTESIAN_POINT('Ctrl Pts',(66.2553107171901,-7.09248843979961,
56.7464666034052));
#167380=CARTESIAN_POINT('Ctrl Pts',(66.6793857970444,-7.46262979858878,
56.6769599864269));
#167381=CARTESIAN_POINT('Ctrl Pts',(66.9991242809228,-7.70748361618338,
56.6239453297674));
#167382=CARTESIAN_POINT('Ctrl Pts',(67.6438958129781,-8.13844539967706,
56.5170596848018));
#167383=CARTESIAN_POINT('Ctrl Pts',(67.9663774915458,-8.32709835295906,
56.4636105473459));
#167384=CARTESIAN_POINT('Ctrl Pts',(68.3882118940512,-8.54100625152076,
56.3940461414255));
#167385=CARTESIAN_POINT('Ctrl Pts',(68.4780194289604,-8.58474515862727,
56.3792541317284));
#167386=CARTESIAN_POINT('Ctrl Pts',(68.6145962844914,-8.64856389684196,
56.3567896683141));
#167387=CARTESIAN_POINT('Ctrl Pts',(68.6608640935571,-8.66972315007258,
56.3491846781772));
#167388=CARTESIAN_POINT('Ctrl Pts',(68.7450108435647,-8.70737392981719,
56.3353634122024));
#167389=CARTESIAN_POINT('Ctrl Pts',(68.7828315981335,-8.7239950583187,56.3291548489606));
#167390=CARTESIAN_POINT('Ctrl Pts',(68.8646125220353,-8.75928728392246,
56.3157377244104));
#167391=CARTESIAN_POINT('Ctrl Pts',(68.9086077020988,-8.77787254010335,
56.3085246405678));
#167392=CARTESIAN_POINT('Ctrl Pts',(69.02884805874,-8.82757858244895,56.2888243443684));
#167393=CARTESIAN_POINT('Ctrl Pts',(69.1053617835307,-8.85802458593729,
56.2763027769185));
#167394=CARTESIAN_POINT('Ctrl Pts',(69.6280695734132,-9.05801385643573,
56.1908582245492));
#167395=CARTESIAN_POINT('Ctrl Pts',(70.0861417683028,-9.19389455685718,
56.1165060073459));
#167396=CARTESIAN_POINT('Ctrl Pts',(71.0323438312868,-9.39685184028539,
55.9631929772623));
#167397=CARTESIAN_POINT('Ctrl Pts',(71.519505702754,-9.46149162727628,55.8843905420308));
#167398=CARTESIAN_POINT('Ctrl Pts',(72.1119017796888,-9.49263414192549,
55.7874979223915));
#167399=CARTESIAN_POINT('Ctrl Pts',(72.2146127353695,-9.49631962096214,
55.7706580823399));
#167400=CARTESIAN_POINT('Ctrl Pts',(72.3529391211423,-9.49897699309798,
55.7479085197052));
#167401=CARTESIAN_POINT('Ctrl Pts',(72.3885266354459,-9.49945524949781,
55.7420494120179));
#167402=CARTESIAN_POINT('Ctrl Pts',(72.4447023201719,-9.49988596953694,
55.7327899514867));
#167403=CARTESIAN_POINT('Ctrl Pts',(72.4652898574265,-9.49997508678827,
55.7293942248832));
#167404=CARTESIAN_POINT('Ctrl Pts',(72.5079282331955,-9.50001729772026,
55.722356492773));
#167405=CARTESIAN_POINT('Ctrl Pts',(72.5299787883694,-9.49996026903604,
55.7187141574565));
#167406=CARTESIAN_POINT('Ctrl Pts',(72.5837046672675,-9.49962917292953,
55.7098332443231));
#167407=CARTESIAN_POINT('Ctrl Pts',(72.6153788156775,-9.49927122114843,
55.7045920701524));
#167408=CARTESIAN_POINT('Ctrl Pts',(72.7293895959455,-9.49739684630065,
55.6857084136771));
#167409=CARTESIAN_POINT('Ctrl Pts',(72.8117027750687,-9.49494330885159,
55.6720408700257));
#167410=CARTESIAN_POINT('Ctrl Pts',(73.333786850443,-9.47239647567461,55.5851795638939));
#167411=CARTESIAN_POINT('Ctrl Pts',(73.7716154456839,-9.42201164183068,
55.5115820349469));
#167412=CARTESIAN_POINT('Ctrl Pts',(74.7093058965669,-9.24561783447955,
55.354199663201));
#167413=CARTESIAN_POINT('Ctrl Pts',(75.2057357664216,-9.10869101437909,
55.2710584822521));
#167414=CARTESIAN_POINT('Ctrl Pts',(75.790445398465,-8.89384269090942,55.174243065176));
#167415=CARTESIAN_POINT('Ctrl Pts',(75.8915036496523,-8.85469288439399,
55.1575490123797));
#167416=CARTESIAN_POINT('Ctrl Pts',(76.0405337587023,-8.79394617656608,
55.1329921667997));
#167417=CARTESIAN_POINT('Ctrl Pts',(76.0890265413662,-8.77369980296775,
55.1250114572114));
#167418=CARTESIAN_POINT('Ctrl Pts',(76.1754596780747,-8.73675133555327,
55.110804562409));
#167419=CARTESIAN_POINT('Ctrl Pts',(76.2134628074514,-8.720205154257,55.1045642693147));
#167420=CARTESIAN_POINT('Ctrl Pts',(76.2939657059386,-8.68451466408779,
55.0913586319232));
#167421=CARTESIAN_POINT('Ctrl Pts',(76.3364357378043,-8.66530366954231,
55.0843998278683));
#167422=CARTESIAN_POINT('Ctrl Pts',(76.4507376762134,-8.612564761637,55.065692697827));
#167423=CARTESIAN_POINT('Ctrl Pts',(76.5222973009616,-8.57843498161289,
55.0540040559273));
#167424=CARTESIAN_POINT('Ctrl Pts',(76.9512176901878,-8.36711934902414,
54.9840809592697));
#167425=CARTESIAN_POINT('Ctrl Pts',(77.2976708617606,-8.16795873159066,
54.9282045165333));
#167426=CARTESIAN_POINT('Ctrl Pts',(77.9522518577298,-7.73382098625736,
54.8233966356192));
#167427=CARTESIAN_POINT('Ctrl Pts',(78.2606662805836,-7.50070914316503,
54.7743879784506));
#167428=CARTESIAN_POINT('Ctrl Pts',(78.6929658769925,-7.12999257225669,
54.7056076110398));
#167429=CARTESIAN_POINT('Ctrl Pts',(78.8284054257806,-7.00681721704554,
54.6840418389898));
#167430=CARTESIAN_POINT('Ctrl Pts',(78.9929135639126,-6.84819501800568,
54.6577482718694));
#167431=CARTESIAN_POINT('Ctrl Pts',(79.025393562022,-6.81642032567887,54.6525518781379));
#167432=CARTESIAN_POINT('Ctrl Pts',(79.0763263072911,-6.76586688962991,
54.6443935996856));
#167433=CARTESIAN_POINT('Ctrl Pts',(79.0949308817272,-6.74724537563443,
54.6414114951433));
#167434=CARTESIAN_POINT('Ctrl Pts',(79.1302104800646,-6.71163626877166,
54.6357522266302));
#167435=CARTESIAN_POINT('Ctrl Pts',(79.1468993974597,-6.69466324849478,
54.6330732100695));
#167436=CARTESIAN_POINT('Ctrl Pts',(79.1868167471057,-6.65375736669634,
54.6266610932853));
#167437=CARTESIAN_POINT('Ctrl Pts',(79.2099834345467,-6.62976338517252,
54.6229361964881));
#167438=CARTESIAN_POINT('Ctrl Pts',(79.2903049313384,-6.54568500892601,
54.6100107638819));
#167439=CARTESIAN_POINT('Ctrl Pts',(79.3468007618755,-6.48496263549507,
54.6009001541037));
#167440=CARTESIAN_POINT('Ctrl Pts',(79.7275711237563,-6.06473432874413,
54.5394083290304));
#167441=CARTESIAN_POINT('Ctrl Pts',(80.0248644545611,-5.68118573127458,
54.4909881299508));
#167442=CARTESIAN_POINT('Ctrl Pts',(80.5273632882508,-4.91925352939866,
54.4103218509623));
#167443=CARTESIAN_POINT('Ctrl Pts',(80.7387225627891,-4.54652323968196,
54.376931620969));
#167444=CARTESIAN_POINT('Ctrl Pts',(80.959850812974,-4.08747785067972,54.3431747723531));
#167445=CARTESIAN_POINT('Ctrl Pts',(80.9941542065315,-4.01389507305992,
54.33797744475));
#167446=CARTESIAN_POINT('Ctrl Pts',(81.0469660238515,-3.89675726489382,
54.3300416407751));
#167447=CARTESIAN_POINT('Ctrl Pts',(81.0660892781304,-3.85349208227253,
54.3271825545163));
#167448=CARTESIAN_POINT('Ctrl Pts',(81.099850286557,-3.77555981267128,54.3221617037155));
#167449=CARTESIAN_POINT('Ctrl Pts',(81.1146047699058,-3.74094587430185,
54.3199770211922));
#167450=CARTESIAN_POINT('Ctrl Pts',(81.1487385677232,-3.65954761405594,
54.3149457253764));
#167451=CARTESIAN_POINT('Ctrl Pts',(81.1679530919834,-3.6126934543398,54.3121314177833));
#167452=CARTESIAN_POINT('Ctrl Pts',(81.2229232410845,-3.47557751962789,
54.3041334370407));
#167453=CARTESIAN_POINT('Ctrl Pts',(81.2576882098913,-3.38491441259102,
54.2991438579255));
#167454=CARTESIAN_POINT('Ctrl Pts',(81.4074338600818,-2.97600506029438,
54.2779699511291));
#167455=CARTESIAN_POINT('Ctrl Pts',(81.5070221635251,-2.65223242719468,
54.2647958639422));
#167456=CARTESIAN_POINT('Ctrl Pts',(81.7035348461263,-1.86876789217715,
54.2410678371496));
#167457=CARTESIAN_POINT('Ctrl Pts',(81.7843698754555,-1.40586692489733,
54.2335295287399));
#167458=CARTESIAN_POINT('Ctrl Pts',(81.8543822587684,-0.706555442065941,
54.2306241735281));
#167459=CARTESIAN_POINT('Ctrl Pts',(81.8691810274887,-0.473448102637126,
54.2310382586001));
#167460=CARTESIAN_POINT('Ctrl Pts',(81.876709007879,-0.193869574515561,
54.2330369605984));
#167461=CARTESIAN_POINT('Ctrl Pts',(81.8776189721871,-0.147688661319497,
54.2334160562138));
#167462=CARTESIAN_POINT('Ctrl Pts',(81.8785155688848,-0.0758478686663873,
54.234080293023));
#167463=CARTESIAN_POINT('Ctrl Pts',(81.8787328285037,-0.0501912685364171,
54.2343322902245));
#167464=CARTESIAN_POINT('Ctrl Pts',(81.8788835494623,-0.0163561638718441,
54.2346838626483));
#167465=CARTESIAN_POINT('Ctrl Pts',(81.8789095176102,-0.00817807648179977,
54.2347703219472));
#167466=CARTESIAN_POINT('Ctrl Pts',(81.8789250230948,-6.6822534455389E-11,
54.2348582579198));
#167467=CARTESIAN_POINT('Ctrl Pts',(81.8868193065938,6.72938151241379E-11,
54.2796289644064));
#167468=CARTESIAN_POINT('Ctrl Pts',(81.8868037018699,-0.00823041824879308,
54.2795404656197));
#167469=CARTESIAN_POINT('Ctrl Pts',(81.8867776276105,-0.0164608554629298,
54.279454185466));
#167470=CARTESIAN_POINT('Ctrl Pts',(81.8866270604485,-0.0503705596085221,
54.2791078230115));
#167471=CARTESIAN_POINT('Ctrl Pts',(81.8864111104939,-0.0760494735295417,
54.278867068142));
#167472=CARTESIAN_POINT('Ctrl Pts',(81.885520170495,-0.148012085361578,
54.2782521807275));
#167473=CARTESIAN_POINT('Ctrl Pts',(81.8846158847755,-0.19429262809756,
54.2779260690182));
#167474=CARTESIAN_POINT('Ctrl Pts',(81.8770833769293,-0.476365369618101,
54.2763542287265));
#167475=CARTESIAN_POINT('Ctrl Pts',(81.8621834322366,-0.711863574058764,
54.2768118075317));
#167476=CARTESIAN_POINT('Ctrl Pts',(81.7920732767064,-1.41217311362647,
54.2830428280544));
#167477=CARTESIAN_POINT('Ctrl Pts',(81.7117187716005,-1.87369743422597,
54.2935659156048));
#167478=CARTESIAN_POINT('Ctrl Pts',(81.5161550782977,-2.65481791695313,
54.3211319109903));
#167479=CARTESIAN_POINT('Ctrl Pts',(81.417008554657,-2.97760906953024,54.3355337051005));
#167480=CARTESIAN_POINT('Ctrl Pts',(81.2677700727074,-3.38543212348313,
54.3574666876688));
#167481=CARTESIAN_POINT('Ctrl Pts',(81.2330738320505,-3.47596250547474,
54.3625807460449));
#167482=CARTESIAN_POINT('Ctrl Pts',(81.1781839095376,-3.61292005473898,
54.3706907744574));
#167483=CARTESIAN_POINT('Ctrl Pts',(81.1589838217342,-3.65974753090069,
54.3735309824325));
#167484=CARTESIAN_POINT('Ctrl Pts',(81.1248644977962,-3.74111646184618,
54.3785837473697));
#167485=CARTESIAN_POINT('Ctrl Pts',(81.1101107507902,-3.77572765707751,
54.3807703886754));
#167486=CARTESIAN_POINT('Ctrl Pts',(81.076338802895,-3.85367587452407,54.3857795520443));
#167487=CARTESIAN_POINT('Ctrl Pts',(81.0572027854896,-3.89695956210476,
54.3886205267855));
#167488=CARTESIAN_POINT('Ctrl Pts',(81.0043244696569,-4.01420333350509,
54.3964781202221));
#167489=CARTESIAN_POINT('Ctrl Pts',(80.9699613206163,-4.08787240278888,
54.4015920273012));
#167490=CARTESIAN_POINT('Ctrl Pts',(80.7443601195198,-4.55584599192918,
54.4352164696084));
#167491=CARTESIAN_POINT('Ctrl Pts',(80.527237583365,-4.93678840350033,54.4677687397645));
#167492=CARTESIAN_POINT('Ctrl Pts',(80.1017226532291,-5.57665300903674,
54.5324213539537));
#167493=CARTESIAN_POINT('Ctrl Pts',(79.9044194825698,-5.84223042498021,
54.5626589915195));
#167494=CARTESIAN_POINT('Ctrl Pts',(79.6067873758376,-6.20210705450477,
54.6090097342164));
#167495=CARTESIAN_POINT('Ctrl Pts',(79.5174760262113,-6.30547627230742,
54.6230032598172));
#167496=CARTESIAN_POINT('Ctrl Pts',(79.3667349052224,-6.47252939326779,
54.6467993287517));
#167497=CARTESIAN_POINT('Ctrl Pts',(79.3065681871575,-6.53736276963142,
54.6563414959228));
#167498=CARTESIAN_POINT('Ctrl Pts',(79.2219102082595,-6.6260698475448,54.6698384333121));
#167499=CARTESIAN_POINT('Ctrl Pts',(79.1981696492827,-6.65067833943088,
54.6736308719257));
#167500=CARTESIAN_POINT('Ctrl Pts',(79.1575802967885,-6.69229930409101,
54.6801282601002));
#167501=CARTESIAN_POINT('Ctrl Pts',(79.1407979339267,-6.70937843699708,
54.6828185798356));
#167502=CARTESIAN_POINT('Ctrl Pts',(79.1056760786384,-6.74485188006904,
54.688457126974));
#167503=CARTESIAN_POINT('Ctrl Pts',(79.0873256160593,-6.76323446730563,
54.691407772179));
#167504=CARTESIAN_POINT('Ctrl Pts',(79.0377971948921,-6.81244368777388,
54.6993834460056));
#167505=CARTESIAN_POINT('Ctrl Pts',(79.0064830248739,-6.84312743315383,
54.7044384949753));
#167506=CARTESIAN_POINT('Ctrl Pts',(78.8577788876661,-6.98682863128549,
54.7284974879095));
#167507=CARTESIAN_POINT('Ctrl Pts',(78.7377467747131,-7.09697545809167,
54.7480734480863));
#167508=CARTESIAN_POINT('Ctrl Pts',(78.2604321110614,-7.51275769315889,
54.8263212499131));
#167509=CARTESIAN_POINT('Ctrl Pts',(77.8837213471018,-7.79429326005309,
54.888888481178));
#167510=CARTESIAN_POINT('Ctrl Pts',(77.2952406566751,-8.16870785841258,
54.9864244522242));
#167511=CARTESIAN_POINT('Ctrl Pts',(77.0983037136312,-8.28410059184347,
55.0190409214751));
#167512=CARTESIAN_POINT('Ctrl Pts',(76.7644442175929,-8.46361131233401,
55.0741923601068));
#167513=CARTESIAN_POINT('Ctrl Pts',(76.629795718281,-8.53184688523183,55.0963993378599));
#167514=CARTESIAN_POINT('Ctrl Pts',(76.4397396027214,-8.62242491716268,
55.1276800750773));
#167515=CARTESIAN_POINT('Ctrl Pts',(76.3856613623745,-8.64756302150875,
55.1365735844978));
#167516=CARTESIAN_POINT('Ctrl Pts',(76.2926220992222,-8.68972937077951,
55.1518617802551));
#167517=CARTESIAN_POINT('Ctrl Pts',(76.2537770158542,-8.70701440027458,
55.1582410472903));
#167518=CARTESIAN_POINT('Ctrl Pts',(76.1794369346593,-8.7394850814779,55.1704421048029));
#167519=CARTESIAN_POINT('Ctrl Pts',(76.1439628269152,-8.75471737731974,
55.1762611373328));
#167520=CARTESIAN_POINT('Ctrl Pts',(76.060667530918,-8.78987106701651,55.1899171068255));
#167521=CARTESIAN_POINT('Ctrl Pts',(76.0127739782824,-8.80961403696841,
55.197763359345));
#167522=CARTESIAN_POINT('Ctrl Pts',(75.8464368736243,-8.87656163033207,
55.2249939961966));
#167523=CARTESIAN_POINT('Ctrl Pts',(75.7272031616995,-8.92172316593278,
55.2444785944213));
#167524=CARTESIAN_POINT('Ctrl Pts',(75.0259232068373,-9.17096521075283,
55.3588867249881));
#167525=CARTESIAN_POINT('Ctrl Pts',(74.4259354239074,-9.31900165167197,
55.4558785913282));
#167526=CARTESIAN_POINT('Ctrl Pts',(73.5724183466109,-9.44128635155178,
55.5943132607097));
#167527=CARTESIAN_POINT('Ctrl Pts',(73.3275401402027,-9.46646571011397,
55.634100334039));
#167528=CARTESIAN_POINT('Ctrl Pts',(72.9521054300962,-9.49000543493065,
55.6954207829239));
#167529=CARTESIAN_POINT('Ctrl Pts',(72.8220630485322,-9.49540910087137,
55.7167199876299));
#167530=CARTESIAN_POINT('Ctrl Pts',(72.6545134984376,-9.49883368609103,
55.7442694109516));
#167531=CARTESIAN_POINT('Ctrl Pts',(72.6170584157632,-9.49937169626509,
55.7504348799275));
#167532=CARTESIAN_POINT('Ctrl Pts',(72.5563369146072,-9.49987505736842,
55.7604423812777));
#167533=CARTESIAN_POINT('Ctrl Pts',(72.533071295167,-9.49998014100829,55.7642796773405));
#167534=CARTESIAN_POINT('Ctrl Pts',(72.4878830151827,-9.50001374574615,
55.7717386722315));
#167535=CARTESIAN_POINT('Ctrl Pts',(72.4659605421489,-9.49995210358764,
55.7753600209924));
#167536=CARTESIAN_POINT('Ctrl Pts',(72.4170057908746,-9.49964038424899,
55.7834525983054));
#167537=CARTESIAN_POINT('Ctrl Pts',(72.3899741255588,-9.49934972106651,
55.7879250733794));
#167538=CARTESIAN_POINT('Ctrl Pts',(72.2964396983423,-9.49793374924685,
55.8034134415145));
#167539=CARTESIAN_POINT('Ctrl Pts',(72.229950790923,-9.49620948254141,55.8144457275155));
#167540=CARTESIAN_POINT('Ctrl Pts',(71.7866313366997,-9.47992427102733,
55.8881297435857));
#167541=CARTESIAN_POINT('Ctrl Pts',(71.4110379251485,-9.44303607424208,
55.9511495569013));
#167542=CARTESIAN_POINT('Ctrl Pts',(70.7172642198884,-9.33174774183496,
56.0676029860616));
#167543=CARTESIAN_POINT('Ctrl Pts',(70.3987366952597,-9.26325038407453,
56.1210890401528));
#167544=CARTESIAN_POINT('Ctrl Pts',(69.8766655397566,-9.12184068168485,
56.2083646637515));
#167545=CARTESIAN_POINT('Ctrl Pts',(69.6709542908296,-9.05836433057767,
56.242652596755));
#167546=CARTESIAN_POINT('Ctrl Pts',(69.3287125709147,-8.93958729744622,
56.299452035826));
#167547=CARTESIAN_POINT('Ctrl Pts',(69.1909957221431,-8.8881029202051,56.322239704473));
#167548=CARTESIAN_POINT('Ctrl Pts',(68.9996358021361,-8.81135074198667,
56.3537970112849));
#167549=CARTESIAN_POINT('Ctrl Pts',(68.9449600838455,-8.78881425229208,
56.3628012879568));
#167550=CARTESIAN_POINT('Ctrl Pts',(68.8514281424868,-8.74921605380204,
56.3781829672609));
#167551=CARTESIAN_POINT('Ctrl Pts',(68.812470285213,-8.73240809088499,56.3845832277817));
#167552=CARTESIAN_POINT('Ctrl Pts',(68.7381919134569,-8.6997583007703,56.3967736410281));
#167553=CARTESIAN_POINT('Ctrl Pts',(68.702853200618,-8.68396160806406,56.4025678856032));
#167554=CARTESIAN_POINT('Ctrl Pts',(68.6200689469886,-8.64633643453006,
56.4161285633606));
#167555=CARTESIAN_POINT('Ctrl Pts',(68.5727039291519,-8.624327598275,56.423877293998));
#167556=CARTESIAN_POINT('Ctrl Pts',(68.4078159950103,-8.54602077316438,
56.4508174735786));
#167557=CARTESIAN_POINT('Ctrl Pts',(68.2912611519676,-8.48764796319075,
56.4697982471763));
#167558=CARTESIAN_POINT('Ctrl Pts',(67.5793662104695,-8.1122919378659,56.5853619099856));
#167559=CARTESIAN_POINT('Ctrl Pts',(67.0176567205434,-7.73366920555861,
56.6747601265172));
#167560=CARTESIAN_POINT('Ctrl Pts',(66.3936889914479,-7.20712609555206,
56.7740190118674));
#167561=CARTESIAN_POINT('Ctrl Pts',(66.2885975073678,-7.1143472560409,56.7907420525393));
#167562=CARTESIAN_POINT('Ctrl Pts',(66.1193907420373,-6.9581012129157,56.8177211283103));
#167563=CARTESIAN_POINT('Ctrl Pts',(66.0540595389005,-6.89601330030935,
56.8281516063107));
#167564=CARTESIAN_POINT('Ctrl Pts',(65.9649996469558,-6.80890678809975,
56.8424005375566));
#167565=CARTESIAN_POINT('Ctrl Pts',(65.9405099979431,-6.78469000345276,
56.8463219235067));
#167566=CARTESIAN_POINT('Ctrl Pts',(65.899188550292,-6.74337810233011,56.852944743338));
#167567=CARTESIAN_POINT('Ctrl Pts',(65.8822888792217,-6.72635272886875,
56.855655153581));
#167568=CARTESIAN_POINT('Ctrl Pts',(65.8472931773515,-6.69082622875994,
56.8612718896173));
#167569=CARTESIAN_POINT('Ctrl Pts',(65.8292079467307,-6.67231469713399,
56.8641767589549));
#167570=CARTESIAN_POINT('Ctrl Pts',(65.7809920204501,-6.62255371399367,
56.8719266870697));
#167571=CARTESIAN_POINT('Ctrl Pts',(65.7509991775424,-6.59116869957959,
56.8767532827162));
#167572=CARTESIAN_POINT('Ctrl Pts',(65.6128974275168,-6.44464405239583,
56.898999590071));
#167573=CARTESIAN_POINT('Ctrl Pts',(65.507447205033,-6.32697784859078,56.9160499571423));
#167574=CARTESIAN_POINT('Ctrl Pts',(65.1420317544909,-5.8980725068684,56.975210507752));
#167575=CARTESIAN_POINT('Ctrl Pts',(64.8990033414979,-5.57263290037703,
57.0146840597765));
#167576=CARTESIAN_POINT('Ctrl Pts',(64.4717379677446,-4.91695987548984,
57.083195157016));
#167577=CARTESIAN_POINT('Ctrl Pts',(64.2848892206694,-4.5893974135785,57.1127221172638));
#167578=CARTESIAN_POINT('Ctrl Pts',(64.0729657225697,-4.16105504507071,
57.1452644213271));
#167579=CARTESIAN_POINT('Ctrl Pts',(64.0296653390984,-4.06995170992162,
57.1518549610581));
#167580=CARTESIAN_POINT('Ctrl Pts',(63.966485534597,-3.93143776181582,57.1613762839153));
#167581=CARTESIAN_POINT('Ctrl Pts',(63.9455440509895,-3.884534038266,57.1645153554872));
#167582=CARTESIAN_POINT('Ctrl Pts',(63.908281739838,-3.7992463703181,57.1700694168243));
#167583=CARTESIAN_POINT('Ctrl Pts',(63.8918334329776,-3.76092119762157,
57.1725094374628));
#167584=CARTESIAN_POINT('Ctrl Pts',(63.85691038023,-3.67806662401944,57.1776644374106));
#167585=CARTESIAN_POINT('Ctrl Pts',(63.8385196576617,-3.63350205716523,
57.1803629549147));
#167586=CARTESIAN_POINT('Ctrl Pts',(63.789341906914,-3.5117477624044,57.1875340169673));
#167587=CARTESIAN_POINT('Ctrl Pts',(63.7592157228958,-3.43428818390488,
57.1918770682651));
#167588=CARTESIAN_POINT('Ctrl Pts',(63.5651731218812,-2.91559575363422,
57.2195078839532));
#167589=CARTESIAN_POINT('Ctrl Pts',(63.4326760499285,-2.46298503603752,
57.2366247678939));
#167590=CARTESIAN_POINT('Ctrl Pts',(63.2624592385337,-1.67037294422955,
57.2554586820962));
#167591=CARTESIAN_POINT('Ctrl Pts',(63.2087284589601,-1.33479508682692,
57.260140361922));
#167592=CARTESIAN_POINT('Ctrl Pts',(63.1459354028104,-0.743838779650244,
57.2631843828959));
#167593=CARTESIAN_POINT('Ctrl Pts',(63.1290859331298,-0.489639754540127,
57.2628367014751));
#167594=CARTESIAN_POINT('Ctrl Pts',(63.1211546198795,-0.189312912893192,
57.2606668808862));
#167595=CARTESIAN_POINT('Ctrl Pts',(63.1202733895077,-0.143535259063808,
57.2602880834199));
#167596=CARTESIAN_POINT('Ctrl Pts',(63.1194141866416,-0.0724641262934447,
57.2596269751481));
#167597=CARTESIAN_POINT('Ctrl Pts',(63.1192084689173,-0.0471737837894489,
57.2593773729443));
#167598=CARTESIAN_POINT('Ctrl Pts',(63.1190114576078,-2.04737978380578E-5,
57.2588855669708));
#167599=CARTESIAN_POINT('Ctrl Pts',(63.1189948859015,0.0218420668010453,
57.258646985011));
#167600=CARTESIAN_POINT('Ctrl Pts',(63.1191287671181,0.0721426862078172,
57.2580736336732));
#167601=CARTESIAN_POINT('Ctrl Pts',(63.1193309530555,0.100580271569169,
57.2577314917698));
#167602=CARTESIAN_POINT('Ctrl Pts',(63.1203626406985,0.189851770932978,
57.2566001002843));
#167603=CARTESIAN_POINT('Ctrl Pts',(63.1216443936129,0.250678078777477,
57.2557456106451));
#167604=CARTESIAN_POINT('Ctrl Pts',(63.1398670833702,0.846485663990278,
57.2465312803745));
#167605=CARTESIAN_POINT('Ctrl Pts',(63.2009344777738,1.37905493293315,57.2315717722661));
#167606=CARTESIAN_POINT('Ctrl Pts',(63.3721367094694,2.23521474306536,57.19415244763));
#167607=CARTESIAN_POINT('Ctrl Pts',(63.4558681992518,2.56305616835908,57.1765078746579));
#167608=CARTESIAN_POINT('Ctrl Pts',(63.6162260837168,3.07654082556368,57.1431967522594));
#167609=CARTESIAN_POINT('Ctrl Pts',(63.6817628196879,3.26547650233007,57.1296733286947));
#167610=CARTESIAN_POINT('Ctrl Pts',(63.7768620419819,3.51428634893736,57.1101308051765));
#167611=CARTESIAN_POINT('Ctrl Pts',(63.8012512260684,3.57616085275525,57.1051252604647));
#167612=CARTESIAN_POINT('Ctrl Pts',(63.8428872728525,3.67865519099926,57.0965897280603));
#167613=CARTESIAN_POINT('Ctrl Pts',(63.8597769870129,3.71942331897871,57.0931297844375));
#167614=CARTESIAN_POINT('Ctrl Pts',(63.8934234783828,3.799079935851,57.0862418687314));
#167615=CARTESIAN_POINT('Ctrl Pts',(63.9101578701817,3.83797713646599,57.0828182919277));
#167616=CARTESIAN_POINT('Ctrl Pts',(63.9510740761863,3.93137309794328,57.0744527097932));
#167617=CARTESIAN_POINT('Ctrl Pts',(63.9755061514997,3.98575581396697,57.0694616178568));
#167618=CARTESIAN_POINT('Ctrl Pts',(64.0581023064795,4.16510719833506,57.0526025334797));
#167619=CARTESIAN_POINT('Ctrl Pts',(64.1184410654669,4.2890143959922,57.0403084101541));
#167620=CARTESIAN_POINT('Ctrl Pts',(64.2755507193237,4.59467902619919,57.0083602819718));
#167621=CARTESIAN_POINT('Ctrl Pts',(64.375532197232,4.77463967360553,56.9880824776893));
#167622=CARTESIAN_POINT('Ctrl Pts',(64.6954363090397,5.30892404169094,56.9234490492815));
#167623=CARTESIAN_POINT('Ctrl Pts',(64.9327033558509,5.65186047291621,56.8758116710857));
#167624=CARTESIAN_POINT('Ctrl Pts',(65.344671843749,6.17046539751304,56.7943294858255));
#167625=CARTESIAN_POINT('Ctrl Pts',(65.505200084583,6.35705412738364,56.7628333922726));
#167626=CARTESIAN_POINT('Ctrl Pts',(65.7057654761593,6.5724566231778,56.7239498664319));
#167627=CARTESIAN_POINT('Ctrl Pts',(65.7390233081084,6.60762506407441,56.7175167827929));
#167628=CARTESIAN_POINT('Ctrl Pts',(65.7913953224537,6.66215368229698,56.7074109980558));
#167629=CARTESIAN_POINT('Ctrl Pts',(65.8103263047558,6.68169321299162,56.7037629774392));
#167630=CARTESIAN_POINT('Ctrl Pts',(65.8441090356111,6.71625937858891,56.6972621319641));
#167631=CARTESIAN_POINT('Ctrl Pts',(65.8589273230657,6.73131904240498,56.694413750271));
#167632=CARTESIAN_POINT('Ctrl Pts',(65.8949340311389,6.7676654769623,56.6874999179495));
#167633=CARTESIAN_POINT('Ctrl Pts',(65.9161734442222,6.78890001361772,56.683427749291));
#167634=CARTESIAN_POINT('Ctrl Pts',(65.9829086578959,6.85498119570882,56.6706508300068));
#167635=CARTESIAN_POINT('Ctrl Pts',(66.0287568461807,6.89946017657578,56.6618988260408));
#167636=CARTESIAN_POINT('Ctrl Pts',(66.2723156567597,7.13095611329834,56.6155245836703));
#167637=CARTESIAN_POINT('Ctrl Pts',(66.4775491862603,7.30965534968785,56.5768509225591));
#167638=CARTESIAN_POINT('Ctrl Pts',(67.0611866175379,7.77472479341755,56.467343245114));
#167639=CARTESIAN_POINT('Ctrl Pts',(67.4537952850087,8.04139391636132,56.3941515890003));
#167640=CARTESIAN_POINT('Ctrl Pts',(68.0457325045604,8.38067072794395,56.283313414584));
#167641=CARTESIAN_POINT('Ctrl Pts',(68.2303616987859,8.47837889630691,56.2486860473544));
#167642=CARTESIAN_POINT('Ctrl Pts',(68.4798890797847,8.59984288548275,56.2017691035976));
#167643=CARTESIAN_POINT('Ctrl Pts',(68.542071822468,8.62926063095005,56.1900680069379));
#167644=CARTESIAN_POINT('Ctrl Pts',(68.6447844275995,8.67646059939143,56.1707240003661));
#167645=CARTESIAN_POINT('Ctrl Pts',(68.6851307638111,8.69465212420425,56.163121438763));
#167646=CARTESIAN_POINT('Ctrl Pts',(68.7639912199249,8.7295311722847,56.1482534071613));
#167647=CARTESIAN_POINT('Ctrl Pts',(68.8024919634255,8.74624753131575,56.1409908776346));
#167648=CARTESIAN_POINT('Ctrl Pts',(68.8937018660945,8.78511422443546,56.123776641423));
#167649=CARTESIAN_POINT('Ctrl Pts',(68.9465019527323,8.80703767293152,56.1138045186464));
#167650=CARTESIAN_POINT('Ctrl Pts',(69.1249833024015,8.87921367193621,56.080071700581));
#167651=CARTESIAN_POINT('Ctrl Pts',(69.2515314724431,8.92718294011467,56.0561144137714));
#167652=CARTESIAN_POINT('Ctrl Pts',(69.80064677166,9.12164225637417,55.95199917272));
#167653=CARTESIAN_POINT('Ctrl Pts',(70.2321408548675,9.23996980639693,55.8697468278977));
#167654=CARTESIAN_POINT('Ctrl Pts',(71.1508633070926,9.4212387163456,55.6945325578907));
#167655=CARTESIAN_POINT('Ctrl Pts',(71.638024782268,9.47742375588013,55.6015764133996));
#167656=CARTESIAN_POINT('Ctrl Pts',(72.1908326194499,9.49665741169594,55.4972673125214));
#167657=CARTESIAN_POINT('Ctrl Pts',(72.2542511321458,9.49820558948042,55.4853189269724));
#167658=CARTESIAN_POINT('Ctrl Pts',(72.3458787538574,9.49949179646944,55.4680860472043));
#167659=CARTESIAN_POINT('Ctrl Pts',(72.3740758937811,9.49975762128033,55.4627870035779));
#167660=CARTESIAN_POINT('Ctrl Pts',(72.4237917534768,9.49999715168168,55.4534517388633));
#167661=CARTESIAN_POINT('Ctrl Pts',(72.4453096387934,9.5000251487393,55.4494138531572));
#167662=CARTESIAN_POINT('Ctrl Pts',(72.491531012897,9.49992273774942,55.4407459632756));
#167663=CARTESIAN_POINT('Ctrl Pts',(72.5162342458354,9.49976827473747,55.4361167980933));
#167664=CARTESIAN_POINT('Ctrl Pts',(72.5852147286712,9.49905847464713,55.4231995156892));
#167665=CARTESIAN_POINT('Ctrl Pts',(72.62949042129,9.49828248070331,55.4149188553773));
#167666=CARTESIAN_POINT('Ctrl Pts',(72.9067772803576,9.49141566200921,55.3631176637781));
#167667=CARTESIAN_POINT('Ctrl Pts',(73.1395460441066,9.47677302352543,55.3198897289655));
#167668=CARTESIAN_POINT('Ctrl Pts',(73.714024217922,9.41862243577074,55.2134743335685));
#167669=CARTESIAN_POINT('Ctrl Pts',(74.0543921880827,9.36473494312402,55.1506582099894));
#167670=CARTESIAN_POINT('Ctrl Pts',(74.8522560221838,9.19204550163891,55.003079553422));
#167671=CARTESIAN_POINT('Ctrl Pts',(75.3053294102451,9.05685050371174,54.9189857956076));
#167672=CARTESIAN_POINT('Ctrl Pts',(75.8228749248785,8.85802325338984,54.8219893753125));
#167673=CARTESIAN_POINT('Ctrl Pts',(75.8990736192657,8.82757748403866,54.8076851870293));
#167674=CARTESIAN_POINT('Ctrl Pts',(76.0188162574668,8.7778718603371,54.7851684786556));
#167675=CARTESIAN_POINT('Ctrl Pts',(76.0626289979602,8.75928665798209,54.7769216225474));
#167676=CARTESIAN_POINT('Ctrl Pts',(76.1440697956621,8.72399449429642,54.7615765659813));
#167677=CARTESIAN_POINT('Ctrl Pts',(76.1817328979715,8.70737335412838,54.7544738619917));
#167678=CARTESIAN_POINT('Ctrl Pts',(76.2655280858635,8.66972244998581,54.7386573540621));
#167679=CARTESIAN_POINT('Ctrl Pts',(76.3116019393107,8.64856309857459,54.729951296251));
#167680=CARTESIAN_POINT('Ctrl Pts',(76.4476050615252,8.58474361194902,54.7042241205318));
#167681=CARTESIAN_POINT('Ctrl Pts',(76.5370324288022,8.54100418656501,54.6872706193047));
#167682=CARTESIAN_POINT('Ctrl Pts',(76.9570752956643,8.32708935194492,54.6074694624332));
#167683=CARTESIAN_POINT('Ctrl Pts',(77.2781409908186,8.13843080712285,54.5459502410746));
#167684=CARTESIAN_POINT('Ctrl Pts',(77.9199689617395,7.70745538556204,54.4222790011362));
#167685=CARTESIAN_POINT('Ctrl Pts',(78.2381877487167,7.46258772423397,54.3605624114115));
#167686=CARTESIAN_POINT('Ctrl Pts',(78.6601071376136,7.09244599352062,54.2788758867884));
#167687=CARTESIAN_POINT('Ctrl Pts',(78.7774915188021,6.98404469276734,54.2561691872502));
#167688=CARTESIAN_POINT('Ctrl Pts',(78.9232985676954,6.84235126356615,54.2280441028623));
#167689=CARTESIAN_POINT('Ctrl Pts',(78.9542723123117,6.81183177091451,54.2220742713647));
#167690=CARTESIAN_POINT('Ctrl Pts',(79.0033254038192,6.7628248574842,54.212628962011));
#167691=CARTESIAN_POINT('Ctrl Pts',(79.0215389084019,6.74447831159453,54.2091239331579));
#167692=CARTESIAN_POINT('Ctrl Pts',(79.056448810804,6.70902326234618,54.20241013013));
#167693=CARTESIAN_POINT('Ctrl Pts',(79.0731557501983,6.69192604687947,54.1991990400479));
#167694=CARTESIAN_POINT('Ctrl Pts',(79.1136326149226,6.65018771908824,54.1914237735947));
#167695=CARTESIAN_POINT('Ctrl Pts',(79.1373352345226,6.62547899080174,54.1868744302463));
#167696=CARTESIAN_POINT('Ctrl Pts',(79.2222437045098,6.53599742631999,54.170589365341));
#167697=CARTESIAN_POINT('Ctrl Pts',(79.2826817300576,6.47047242462857,54.1590198552344));
#167698=CARTESIAN_POINT('Ctrl Pts',(79.4344526743067,6.3011824070846,54.1300031374128));
#167699=CARTESIAN_POINT('Ctrl Pts',(79.5244771109269,6.19622697916207,54.1128263089429));
#167700=CARTESIAN_POINT('Ctrl Pts',(80.0206649713991,5.59140006542065,54.018190898994));
#167701=CARTESIAN_POINT('Ctrl Pts',(80.3779607811106,5.05223054293846,53.9500616685561));
#167702=CARTESIAN_POINT('Ctrl Pts',(80.750991426542,4.34143940072097,53.8765038719716));
#167703=CARTESIAN_POINT('Ctrl Pts',(80.8203985614988,4.20085520762842,53.8626887079181));
#167704=CARTESIAN_POINT('Ctrl Pts',(80.9126072188179,4.00185272323795,53.8441292860633));
#167705=CARTESIAN_POINT('Ctrl Pts',(80.9383356633627,3.94486238842252,53.8389262188333));
#167706=CARTESIAN_POINT('Ctrl Pts',(80.9791963853384,3.85192488606166,53.8306215137677));
#167707=CARTESIAN_POINT('Ctrl Pts',(80.9946704502021,3.81613489613762,53.8274663613728));
#167708=CARTESIAN_POINT('Ctrl Pts',(81.0266659859806,3.74086827871907,53.8209207703901));
#167709=CARTESIAN_POINT('Ctrl Pts',(81.0431423895596,3.70137283544941,53.8175374060662));
#167710=CARTESIAN_POINT('Ctrl Pts',(81.0819831308973,3.60647589560421,53.8095306694711));
#167711=CARTESIAN_POINT('Ctrl Pts',(81.1040951324315,3.550969796042,53.8049468573553));
#167712=CARTESIAN_POINT('Ctrl Pts',(81.1795353537772,3.35630096280034,53.7892164874625));
#167713=CARTESIAN_POINT('Ctrl Pts',(81.2301365437784,3.21607092444481,53.7784979647761));
#167714=CARTESIAN_POINT('Ctrl Pts',(81.3468862685882,2.86717061425798,53.7533360673316));
#167715=CARTESIAN_POINT('Ctrl Pts',(81.4092041237738,2.65726679501057,53.7395013044267));
#167716=CARTESIAN_POINT('Ctrl Pts',(81.5467546317825,2.12815756493666,53.707921581553));
#167717=CARTESIAN_POINT('Ctrl Pts',(81.6129330712187,1.8068051040015,53.6916640158221));
#167718=CARTESIAN_POINT('Ctrl Pts',(81.7203516780883,1.1056104425334,53.6628695973415));
#167719=CARTESIAN_POINT('Ctrl Pts',(81.7556859612981,0.725389215569644,
53.6513930117048));
#167720=CARTESIAN_POINT('Ctrl Pts',(81.770762177904,0.276630689451335,53.6432577887107));
#167721=CARTESIAN_POINT('Ctrl Pts',(81.7723223054978,0.209249832552093,
53.6421796521692));
#167722=CARTESIAN_POINT('Ctrl Pts',(81.7735285954149,0.114462559547364,
53.6408690767072));
#167723=CARTESIAN_POINT('Ctrl Pts',(81.7737611497979,0.0870672968790157,
53.6405145014626));
#167724=CARTESIAN_POINT('Ctrl Pts',(81.7739622678791,0.0397810590504774,
53.6399446357702));
#167725=CARTESIAN_POINT('Ctrl Pts',(81.7739857033185,0.0198905954865054,
53.639717801509));
#167726=CARTESIAN_POINT('Ctrl Pts',(81.7739479911102,4.5045009216105E-12,
53.6395039249478));
#167727=CARTESIAN_POINT('Origin',(73.0915550886457,-4.33680868994202E-16,
59.1075264962884));
#167728=CARTESIAN_POINT('',(81.653182392128,-6.03303474316641E-13,52.9546081790047));
#167729=CARTESIAN_POINT('',(81.6610766756267,2.23549780027555E-12,52.9993788854899));
#167730=CARTESIAN_POINT('',(82.4472287422617,-1.59709532818419E-15,57.4578688084528));
#167731=CARTESIAN_POINT('Ctrl Pts',(81.653182392128,-1.2050098533051E-12,
52.9546081790047));
#167732=CARTESIAN_POINT('Ctrl Pts',(81.6531851088897,0.00143290493713799,
52.9546235865264));
#167733=CARTESIAN_POINT('Ctrl Pts',(81.6531875044535,0.00286581046897979,
52.9546390393913));
#167734=CARTESIAN_POINT('Ctrl Pts',(81.6532233539634,0.0276294538124026,
52.954906881751));
#167735=CARTESIAN_POINT('Ctrl Pts',(81.6531719782427,0.0509601047422428,
52.9551712533422));
#167736=CARTESIAN_POINT('Ctrl Pts',(81.6528199849092,0.111121506211944,
52.9558843734276));
#167737=CARTESIAN_POINT('Ctrl Pts',(81.6523923386346,0.147950905939667,
52.9563512783029));
#167738=CARTESIAN_POINT('Ctrl Pts',(81.6498429068614,0.294719037309852,
52.9583351952227));
#167739=CARTESIAN_POINT('Ctrl Pts',(81.6460434811885,0.404616702112234,
52.9600964744945));
#167740=CARTESIAN_POINT('Ctrl Pts',(81.6098997609032,1.1027383561785,52.973133326473));
#167741=CARTESIAN_POINT('Ctrl Pts',(81.5254093008345,1.68682274318137,52.9924731025717));
#167742=CARTESIAN_POINT('Ctrl Pts',(81.2976027997886,2.63757270516619,53.0409794735188));
#167743=CARTESIAN_POINT('Ctrl Pts',(81.1841234582634,3.00995384298833,53.0645334646489));
#167744=CARTESIAN_POINT('Ctrl Pts',(81.0204259219582,3.44964165566448,53.098210734284));
#167745=CARTESIAN_POINT('Ctrl Pts',(80.9913830923766,3.52474759383711,53.1041758701733));
#167746=CARTESIAN_POINT('Ctrl Pts',(80.9438527680212,3.64321128628823,53.113924298331));
#167747=CARTESIAN_POINT('Ctrl Pts',(80.9259811660577,3.68682177005464,53.1175868337448));
#167748=CARTESIAN_POINT('Ctrl Pts',(80.891670631995,3.76881967294016,53.1246130337504));
#167749=CARTESIAN_POINT('Ctrl Pts',(80.8753004837309,3.80723579936609,53.1279632004791));
#167750=CARTESIAN_POINT('Ctrl Pts',(80.8376866807841,3.8939302308394,53.1356561269352));
#167751=CARTESIAN_POINT('Ctrl Pts',(80.8162954086813,3.94214038937022,53.1400278423351));
#167752=CARTESIAN_POINT('Ctrl Pts',(80.7598177594276,4.06664304053919,53.151561553844));
#167753=CARTESIAN_POINT('Ctrl Pts',(80.7241284528481,4.14264589344325,53.1588417186191));
#167754=CARTESIAN_POINT('Ctrl Pts',(80.4294920360104,4.74922187462374,53.2188741527783));
#167755=CARTESIAN_POINT('Ctrl Pts',(80.1233338937517,5.25448783642775,53.2809444792974));
#167756=CARTESIAN_POINT('Ctrl Pts',(79.7237134958812,5.79358726663658,53.3605176287432));
#167757=CARTESIAN_POINT('Ctrl Pts',(79.6737511995805,5.85917659460431,53.3704424175489));
#167758=CARTESIAN_POINT('Ctrl Pts',(79.5097164749224,6.06876597478054,53.4029364910156));
#167759=CARTESIAN_POINT('Ctrl Pts',(79.3923383649786,6.21003971940025,53.4260516114764));
#167760=CARTESIAN_POINT('Ctrl Pts',(79.2222549390406,6.4029690782621,53.4592784642033));
#167761=CARTESIAN_POINT('Ctrl Pts',(79.1729177195201,6.45762496457932,53.4688869845655));
#167762=CARTESIAN_POINT('Ctrl Pts',(79.085047662333,6.55269508357314,53.4859407161347));
#167763=CARTESIAN_POINT('Ctrl Pts',(79.0467839236783,6.59335992723495,53.4933477937378));
#167764=CARTESIAN_POINT('Ctrl Pts',(78.9884701807746,6.65423423061991,53.5046046812826));
#167765=CARTESIAN_POINT('Ctrl Pts',(78.968684236537,6.67470151227817,53.5084187919373));
#167766=CARTESIAN_POINT('Ctrl Pts',(78.9325019982952,6.71178997853067,53.5153833973951));
#167767=CARTESIAN_POINT('Ctrl Pts',(78.9161360582504,6.72844083122991,53.5185298331574));
#167768=CARTESIAN_POINT('Ctrl Pts',(78.8788110506641,6.76613270619697,53.525697237507));
#167769=CARTESIAN_POINT('Ctrl Pts',(78.8578144476744,6.78713494028236,53.5297231581496));
#167770=CARTESIAN_POINT('Ctrl Pts',(78.7926005123424,6.85174885958812,53.5422099226398));
#167771=CARTESIAN_POINT('Ctrl Pts',(78.7480532683087,6.89501657676172,53.5507149788459));
#167772=CARTESIAN_POINT('Ctrl Pts',(78.3634704344591,7.26119087314628,53.6239564857326));
#167773=CARTESIAN_POINT('Ctrl Pts',(78.000380645464,7.55826585105626,53.6919215589871));
#167774=CARTESIAN_POINT('Ctrl Pts',(77.234534061211,8.0942693626051,53.835106201599));
#167775=CARTESIAN_POINT('Ctrl Pts',(76.8329440448213,8.33257751035838,53.9101169267169));
#167776=CARTESIAN_POINT('Ctrl Pts',(76.343472575379,8.57532840246176,54.0021007685567));
#167777=CARTESIAN_POINT('Ctrl Pts',(76.2708120141278,8.6101916243388,54.0157679207733));
#167778=CARTESIAN_POINT('Ctrl Pts',(76.155271077027,8.66378755544133,54.0375220799395));
#167779=CARTESIAN_POINT('Ctrl Pts',(76.1126777352058,8.68315465012804,54.0455461222872));
#167780=CARTESIAN_POINT('Ctrl Pts',(76.032259849134,8.71898781551311,54.0607046032667));
#167781=CARTESIAN_POINT('Ctrl Pts',(75.9944673254759,8.73552589656495,54.0678319717392));
#167782=CARTESIAN_POINT('Ctrl Pts',(75.9089458313919,8.77227123416493,54.0839689281252));
#167783=CARTESIAN_POINT('Ctrl Pts',(75.8611572540474,8.79233033312754,54.0929918860099));
#167784=CARTESIAN_POINT('Ctrl Pts',(75.7190935229166,8.85056209863549,54.1198321712684));
#167785=CARTESIAN_POINT('Ctrl Pts',(75.624370986828,8.88757564336336,54.137750648613));
#167786=CARTESIAN_POINT('Ctrl Pts',(74.9725214106413,9.12996767661181,54.2612083882653));
#167787=CARTESIAN_POINT('Ctrl Pts',(74.3980220324031,9.28251995801431,54.3708687689541));
#167788=CARTESIAN_POINT('Ctrl Pts',(73.5275810894262,9.42553785836264,54.5368158118696));
#167789=CARTESIAN_POINT('Ctrl Pts',(73.2399592872618,9.45892242627501,54.5915958444191));
#167790=CARTESIAN_POINT('Ctrl Pts',(72.8081745632571,9.48843030376819,54.6734161688691));
#167791=CARTESIAN_POINT('Ctrl Pts',(72.664902405294,9.49485110491601,54.7004961134848));
#167792=CARTESIAN_POINT('Ctrl Pts',(72.482947966746,9.49873430675822,54.7347584843411));
#167793=CARTESIAN_POINT('Ctrl Pts',(72.4443661336139,9.49931425703466,54.7420161527846));
#167794=CARTESIAN_POINT('Ctrl Pts',(72.3823249654886,9.49985545800877,54.7536738683831));
#167795=CARTESIAN_POINT('Ctrl Pts',(72.3588682885446,9.49997013932155,54.7580784785989));
#167796=CARTESIAN_POINT('Ctrl Pts',(72.313724850805,9.50001777306765,54.7665493474078));
#167797=CARTESIAN_POINT('Ctrl Pts',(72.2920384406394,9.49996379472975,54.7706159664307));
#167798=CARTESIAN_POINT('Ctrl Pts',(72.2440334840176,9.49967417479822,54.7796121120073));
#167799=CARTESIAN_POINT('Ctrl Pts',(72.217715066986,9.49940219454825,54.7845404023461));
#167800=CARTESIAN_POINT('Ctrl Pts',(72.1239530773142,9.49802993961756,54.8020852443306));
#167801=CARTESIAN_POINT('Ctrl Pts',(72.0565169371262,9.49629951400901,54.814680590286));
#167802=CARTESIAN_POINT('Ctrl Pts',(71.6037718665759,9.47968824177278,54.8991102449892));
#167803=CARTESIAN_POINT('Ctrl Pts',(71.2195600721447,9.44129098303147,54.9701334413135));
#167804=CARTESIAN_POINT('Ctrl Pts',(70.4963812153249,9.32270896029754,55.1037906958956));
#167805=CARTESIAN_POINT('Ctrl Pts',(70.1573210241772,9.24721904033253,55.1664448247529));
#167806=CARTESIAN_POINT('Ctrl Pts',(69.5386556079521,9.07225515070606,55.2813054512462));
#167807=CARTESIAN_POINT('Ctrl Pts',(69.2580380363048,8.97809467536674,55.3336168206133));
#167808=CARTESIAN_POINT('Ctrl Pts',(68.9127885771729,8.84344769595115,55.3983622716093));
#167809=CARTESIAN_POINT('Ctrl Pts',(68.8435699668383,8.81548034045728,55.4113624996697));
#167810=CARTESIAN_POINT('Ctrl Pts',(68.7326953078154,8.76910983180753,55.4322187747066));
#167811=CARTESIAN_POINT('Ctrl Pts',(68.6908272496663,8.75123468941025,55.4401019652083));
#167812=CARTESIAN_POINT('Ctrl Pts',(68.6110447637958,8.71647272437077,55.4551384770455));
#167813=CARTESIAN_POINT('Ctrl Pts',(68.573109055057,8.69963870183839,55.4622945180514));
#167814=CARTESIAN_POINT('Ctrl Pts',(68.4868379884985,8.66065792082803,55.4785828776011));
#167815=CARTESIAN_POINT('Ctrl Pts',(68.43857622262,8.63834780040543,55.4877053980935));
#167816=CARTESIAN_POINT('Ctrl Pts',(68.3104888284529,8.57778970720131,55.5119445636487));
#167817=CARTESIAN_POINT('Ctrl Pts',(68.2310082889168,8.53880633272851,55.5270145386497));
#167818=CARTESIAN_POINT('Ctrl Pts',(67.6843088897289,8.26085827462049,55.6308689310983));
#167819=CARTESIAN_POINT('Ctrl Pts',(67.2371836347527,7.98345115343855,55.7168833548564));
#167820=CARTESIAN_POINT('Ctrl Pts',(66.4981887656814,7.43331683276955,55.8597945435958));
#167821=CARTESIAN_POINT('Ctrl Pts',(66.1960621862242,7.177073485896,55.9184558384286));
#167822=CARTESIAN_POINT('Ctrl Pts',(65.8735982952597,6.86652298197054,55.9806877483495));
#167823=CARTESIAN_POINT('Ctrl Pts',(65.8368435243893,6.83054137601503,55.9877747665752));
#167824=CARTESIAN_POINT('Ctrl Pts',(65.7808436989398,6.77481492282599,55.9985606407082));
#167825=CARTESIAN_POINT('Ctrl Pts',(65.7613920790619,6.75528785333911,56.0023048766362));
#167826=CARTESIAN_POINT('Ctrl Pts',(65.7255646139728,6.71900490908967,56.0091966734451));
#167827=CARTESIAN_POINT('Ctrl Pts',(65.7091656909039,6.70227339623416,56.0123493255522));
#167828=CARTESIAN_POINT('Ctrl Pts',(65.6716603088655,6.66372137156733,56.0195555168211));
#167829=CARTESIAN_POINT('Ctrl Pts',(65.6505956575853,6.6418589651321,56.0235998419343));
#167830=CARTESIAN_POINT('Ctrl Pts',(65.5831059764369,6.57113394912269,56.0365490096215));
#167831=CARTESIAN_POINT('Ctrl Pts',(65.537090243409,6.52186745495794,56.0453648242135));
#167832=CARTESIAN_POINT('Ctrl Pts',(65.262819257121,6.2218473032735,56.0978518841695));
#167833=CARTESIAN_POINT('Ctrl Pts',(65.0474346617468,5.95920004815421,56.1388297521726));
#167834=CARTESIAN_POINT('Ctrl Pts',(64.6753177678137,5.45208819192811,56.2099029650843));
#167835=CARTESIAN_POINT('Ctrl Pts',(64.5148227683445,5.21098492136576,56.2406723360261));
#167836=CARTESIAN_POINT('Ctrl Pts',(64.2580418784646,4.78410875016397,56.2904254571182));
#167837=CARTESIAN_POINT('Ctrl Pts',(64.1564379179796,4.60188570289519,56.3102803457906));
#167838=CARTESIAN_POINT('Ctrl Pts',(63.9957790516098,4.29005225111126,56.3420492100451));
#167839=CARTESIAN_POINT('Ctrl Pts',(63.933509024626,4.16223635293633,56.3544717913713));
#167840=CARTESIAN_POINT('Ctrl Pts',(63.8496329315514,3.97980697350209,56.3713777272633));
#167841=CARTESIAN_POINT('Ctrl Pts',(63.8256469086816,3.9263440003003,56.3762340682647));
#167842=CARTESIAN_POINT('Ctrl Pts',(63.7850808955849,3.83364602727304,56.3844862270183));
#167843=CARTESIAN_POINT('Ctrl Pts',(63.7682691639683,3.79451761693966,56.3879183162862));
#167844=CARTESIAN_POINT('Ctrl Pts',(63.7364764881869,3.71913351153391,56.3944326297103));
#167845=CARTESIAN_POINT('Ctrl Pts',(63.7214561696865,3.68289590952451,56.3975210036219));
#167846=CARTESIAN_POINT('Ctrl Pts',(63.6825726451172,3.58742611533613,56.4055446456523));
#167847=CARTESIAN_POINT('Ctrl Pts',(63.6590781258552,3.52804111868332,56.4104221198305));
#167848=CARTESIAN_POINT('Ctrl Pts',(63.5771757609427,3.31479246837527,56.427532869769));
#167849=CARTESIAN_POINT('Ctrl Pts',(63.5221382824121,3.15962410510045,56.4392369569967));
#167850=CARTESIAN_POINT('Ctrl Pts',(63.2674918484385,2.37820455941616,56.4944640878441));
#167851=CARTESIAN_POINT('Ctrl Pts',(63.1286276081184,1.73338423843806,56.5284354258869));
#167852=CARTESIAN_POINT('Ctrl Pts',(63.0282874495021,0.823225331996955,
56.5585928568498));
#167853=CARTESIAN_POINT('Ctrl Pts',(63.0103206638125,0.56632020372454,56.565157902973));
#167854=CARTESIAN_POINT('Ctrl Pts',(63.0007772661167,0.247950331523532,
56.5706941076219));
#167855=CARTESIAN_POINT('Ctrl Pts',(62.9995247559059,0.186916016119687,
56.5716373966359));
#167856=CARTESIAN_POINT('Ctrl Pts',(62.9985343941073,0.0975168026113216,
56.5728427199189));
#167857=CARTESIAN_POINT('Ctrl Pts',(62.9983446195951,0.0691597164579145,
56.5731990650259));
#167858=CARTESIAN_POINT('Ctrl Pts',(62.9982288146377,0.0189951161409549,
56.5737830627965));
#167859=CARTESIAN_POINT('Ctrl Pts',(62.998251979729,-0.00281185154086295,
56.5740214044755));
#167860=CARTESIAN_POINT('Ctrl Pts',(62.9984624304569,-0.0502878787672504,
56.5745064116745));
#167861=CARTESIAN_POINT('Ctrl Pts',(62.9986780614881,-0.0759564992473333,
56.5747471189385));
#167862=CARTESIAN_POINT('Ctrl Pts',(62.9995675392294,-0.147862838647288,
56.5753616857521));
#167863=CARTESIAN_POINT('Ctrl Pts',(63.0004701053835,-0.194097413028669,
56.5756876445601));
#167864=CARTESIAN_POINT('Ctrl Pts',(63.0079647818126,-0.475015389661,56.5772544889009));
#167865=CARTESIAN_POINT('Ctrl Pts',(63.022748548414,-0.709408209651014,
56.576808494219));
#167866=CARTESIAN_POINT('Ctrl Pts',(63.0925551452664,-1.40929162176869,
56.570630574318));
#167867=CARTESIAN_POINT('Ctrl Pts',(63.1728982913727,-1.8714855318355,56.5601138616527));
#167868=CARTESIAN_POINT('Ctrl Pts',(63.3685960529682,-2.65369613980434,
56.5325322891673));
#167869=CARTESIAN_POINT('Ctrl Pts',(63.4678384230203,-2.97691385881897,
56.5181169486992));
#167870=CARTESIAN_POINT('Ctrl Pts',(63.6172343928597,-3.38520712801605,
56.496160960067));
#167871=CARTESIAN_POINT('Ctrl Pts',(63.6519504746455,-3.47579523215722,
56.4910439961187));
#167872=CARTESIAN_POINT('Ctrl Pts',(63.706865966957,-3.61282150503926,56.4829302051978));
#167873=CARTESIAN_POINT('Ctrl Pts',(63.7260702405749,-3.6596605882726,56.4800893823114));
#167874=CARTESIAN_POINT('Ctrl Pts',(63.7601940837421,-3.74104224742202,
56.47503595405));
#167875=CARTESIAN_POINT('Ctrl Pts',(63.7749479961465,-3.7756546334831,56.4728492906534));
#167876=CARTESIAN_POINT('Ctrl Pts',(63.8087161835238,-3.85359592043542,
56.4678406903297));
#167877=CARTESIAN_POINT('Ctrl Pts',(63.8278481407165,-3.89687154779444,
56.465000321757));
#167878=CARTESIAN_POINT('Ctrl Pts',(63.8807041312365,-4.01406926395532,
56.45714605628));
#167879=CARTESIAN_POINT('Ctrl Pts',(63.9150481660042,-4.08770074481185,
56.4520350041243));
#167880=CARTESIAN_POINT('Ctrl Pts',(64.1380401797386,-4.5502906750407,56.4187995378315));
#167881=CARTESIAN_POINT('Ctrl Pts',(64.3518546959585,-4.92626548755453,
56.3867447015043));
#167882=CARTESIAN_POINT('Ctrl Pts',(64.7679436043986,-5.55452725632516,
56.323546326405));
#167883=CARTESIAN_POINT('Ctrl Pts',(64.9590468267763,-5.81354188317332,
56.2942773865799));
#167884=CARTESIAN_POINT('Ctrl Pts',(65.2552181614526,-6.17510824662347,
56.2482168567204));
#167885=CARTESIAN_POINT('Ctrl Pts',(65.3502536701254,-6.28582711028667,
56.2333424992836));
#167886=CARTESIAN_POINT('Ctrl Pts',(65.5097323844737,-6.46319745322292,
56.2081822474878));
#167887=CARTESIAN_POINT('Ctrl Pts',(65.5726924888361,-6.53119281418251,
56.1982011833488));
#167888=CARTESIAN_POINT('Ctrl Pts',(65.6606438943671,-6.6234339050194,56.1841815056031));
#167889=CARTESIAN_POINT('Ctrl Pts',(65.6848026362384,-6.64849355766373,
56.1803227786715));
#167890=CARTESIAN_POINT('Ctrl Pts',(65.7258877429669,-6.69064443696378,
56.1737466721988));
#167891=CARTESIAN_POINT('Ctrl Pts',(65.7427435270944,-6.70780646726806,
56.1710448328442));
#167892=CARTESIAN_POINT('Ctrl Pts',(65.777775226757,-6.7432044849496,56.1654212360849));
#167893=CARTESIAN_POINT('Ctrl Pts',(65.7959602430942,-6.76143069855299,
56.162497473426));
#167894=CARTESIAN_POINT('Ctrl Pts',(65.8445767290485,-6.80976217323059,
56.1546694742757));
#167895=CARTESIAN_POINT('Ctrl Pts',(65.8751359114217,-6.83973353817258,
56.1497370796754));
#167896=CARTESIAN_POINT('Ctrl Pts',(66.014527895092,-6.97460362589823,56.1271892000794));
#167897=CARTESIAN_POINT('Ctrl Pts',(66.1256174938266,-7.07705554811865,
56.1090847317394));
#167898=CARTESIAN_POINT('Ctrl Pts',(66.6011782138914,-7.49497911654568,
56.0311925169791));
#167899=CARTESIAN_POINT('Ctrl Pts',(66.9866843808187,-7.78459586609376,
55.9671611342368));
#167900=CARTESIAN_POINT('Ctrl Pts',(67.5859016687395,-8.16636221186927,
55.867844530841));
#167901=CARTESIAN_POINT('Ctrl Pts',(67.7838182941223,-8.28244277363937,
55.8350649478133));
#167902=CARTESIAN_POINT('Ctrl Pts',(68.1191630341652,-8.4628544801865,55.7796672818617));
#167903=CARTESIAN_POINT('Ctrl Pts',(68.2542864395813,-8.53135611121289,
55.75738170233));
#167904=CARTESIAN_POINT('Ctrl Pts',(68.4448998313424,-8.62221424464514,
55.7260090837402));
#167905=CARTESIAN_POINT('Ctrl Pts',(68.4990495165836,-8.6473887957525,55.717103787401));
#167906=CARTESIAN_POINT('Ctrl Pts',(68.5921736776358,-8.68959768876844,
55.7018015936054));
#167907=CARTESIAN_POINT('Ctrl Pts',(68.6310316564608,-8.70689003262623,
55.6954201900798));
#167908=CARTESIAN_POINT('Ctrl Pts',(68.7053705143828,-8.73936296670161,
55.683219299872));
#167909=CARTESIAN_POINT('Ctrl Pts',(68.7408303490545,-8.75459055774761,
55.6774025913991));
#167910=CARTESIAN_POINT('Ctrl Pts',(68.8240529088259,-8.78971711156529,
55.6637585034054));
#167911=CARTESIAN_POINT('Ctrl Pts',(68.8718876798237,-8.80943844854408,
55.6559218490915));
#167912=CARTESIAN_POINT('Ctrl Pts',(69.0387102451521,-8.87659239012893,
55.6286116045841));
#167913=CARTESIAN_POINT('Ctrl Pts',(69.1584974517625,-8.92195827496836,
55.6090366256135));
#167914=CARTESIAN_POINT('Ctrl Pts',(69.860076405798,-9.1712007918962,55.4945809437024));
#167915=CARTESIAN_POINT('Ctrl Pts',(70.4597761055783,-9.31911243207795,
55.3976358060226));
#167916=CARTESIAN_POINT('Ctrl Pts',(71.312916881783,-9.44131278489087,55.2592619483569));
#167917=CARTESIAN_POINT('Ctrl Pts',(71.5577185115048,-9.46647872083246,
55.219487219222));
#167918=CARTESIAN_POINT('Ctrl Pts',(71.9330506369443,-9.49000828287909,
55.1581834452261));
#167919=CARTESIAN_POINT('Ctrl Pts',(72.063067470748,-9.49541013754424,55.1368884032225));
#167920=CARTESIAN_POINT('Ctrl Pts',(72.2305889448303,-9.49883387908354,
55.1093435881339));
#167921=CARTESIAN_POINT('Ctrl Pts',(72.2680415273798,-9.4993718082175,55.1031785292554));
#167922=CARTESIAN_POINT('Ctrl Pts',(72.3287599772102,-9.49987509549167,
55.0931715291942));
#167923=CARTESIAN_POINT('Ctrl Pts',(72.3520250457068,-9.49998016012502,
55.089334323441));
#167924=CARTESIAN_POINT('Ctrl Pts',(72.3972131050212,-9.500013736652,55.0818753640039));
#167925=CARTESIAN_POINT('Ctrl Pts',(72.4191359083683,-9.49995207878265,
55.0782539601697));
#167926=CARTESIAN_POINT('Ctrl Pts',(72.4680922735697,-9.49964031353047,
55.0701611148772));
#167927=CARTESIAN_POINT('Ctrl Pts',(72.4951252223416,-9.49934961123635,
55.0656884266296));
#167928=CARTESIAN_POINT('Ctrl Pts',(72.5886683472263,-9.4979334006619,55.0501986149061));
#167929=CARTESIAN_POINT('Ctrl Pts',(72.6551646646249,-9.49620878556374,
55.0391650947126));
#167930=CARTESIAN_POINT('Ctrl Pts',(73.0988234815666,-9.47990952994969,
54.9654246318891));
#167931=CARTESIAN_POINT('Ctrl Pts',(73.4747462493226,-9.4429671901786,54.9023490404419));
#167932=CARTESIAN_POINT('Ctrl Pts',(74.169641037568,-9.33141974889466,54.7857072993243));
#167933=CARTESIAN_POINT('Ctrl Pts',(74.4889513305227,-9.26267281084391,
54.7320900751759));
#167934=CARTESIAN_POINT('Ctrl Pts',(75.0110902310015,-9.12103469033791,
54.6448058161543));
#167935=CARTESIAN_POINT('Ctrl Pts',(75.216122770848,-9.05770880816632,54.6106320454121));
#167936=CARTESIAN_POINT('Ctrl Pts',(75.5573710626558,-8.93921899473136,
54.5539985361194));
#167937=CARTESIAN_POINT('Ctrl Pts',(75.6947643274422,-8.88784061888727,
54.5312647135036));
#167938=CARTESIAN_POINT('Ctrl Pts',(75.8857570873621,-8.81122667628798,
54.4997681387308));
#167939=CARTESIAN_POINT('Ctrl Pts',(75.9403840224649,-8.78870822776538,
54.4907719384913));
#167940=CARTESIAN_POINT('Ctrl Pts',(76.0338584860343,-8.74913172249382,
54.4753997662184));
#167941=CARTESIAN_POINT('Ctrl Pts',(76.0728073326654,-8.73232661046519,
54.4690010075488));
#167942=CARTESIAN_POINT('Ctrl Pts',(76.1470858955967,-8.69967488212756,
54.4568106014597));
#167943=CARTESIAN_POINT('Ctrl Pts',(76.1824337107016,-8.683873162942,54.4510148843723));
#167944=CARTESIAN_POINT('Ctrl Pts',(76.2652654183662,-8.64622399895604,
54.4374464836224));
#167945=CARTESIAN_POINT('Ctrl Pts',(76.3126685446303,-8.6241956621182,54.4296915558093));
#167946=CARTESIAN_POINT('Ctrl Pts',(76.4778281290465,-8.54575214227553,
54.4027071510864));
#167947=CARTESIAN_POINT('Ctrl Pts',(76.5946120932545,-8.48725291539084,
54.3836893058772));
#167948=CARTESIAN_POINT('Ctrl Pts',(77.2464981544172,-8.14343592709517,
54.277869002374));
#167949=CARTESIAN_POINT('Ctrl Pts',(77.7548048635759,-7.80868240634213,
54.1967720053534));
#167950=CARTESIAN_POINT('Ctrl Pts',(78.3706817865983,-7.3113176967463,54.0987980666803));
#167951=CARTESIAN_POINT('Ctrl Pts',(78.5102477533446,-7.19168995334135,
54.0766074567405));
#167952=CARTESIAN_POINT('Ctrl Pts',(78.7008295324219,-7.01839518237206,
54.0462398234681));
#167953=CARTESIAN_POINT('Ctrl Pts',(78.7548166020132,-6.96813372240287,
54.0376295895671));
#167954=CARTESIAN_POINT('Ctrl Pts',(78.8487185825342,-6.87862869911172,
54.0226321677738));
#167955=CARTESIAN_POINT('Ctrl Pts',(78.8888819606826,-6.83965684693043,
54.016210486688));
#167956=CARTESIAN_POINT('Ctrl Pts',(78.9490021813989,-6.78027037483051,
54.0065843383982));
#167957=CARTESIAN_POINT('Ctrl Pts',(78.9692148381762,-6.76012205677604,
54.0033456279937));
#167958=CARTESIAN_POINT('Ctrl Pts',(79.0058404977669,-6.72327949860582,
53.9974722478685));
#167959=CARTESIAN_POINT('Ctrl Pts',(79.0222829454009,-6.70661586250353,
53.9948336796945));
#167960=CARTESIAN_POINT('Ctrl Pts',(79.0595016347727,-6.66861413698908,
53.9888570075512));
#167961=CARTESIAN_POINT('Ctrl Pts',(79.0802393997811,-6.64723822955063,
53.9855240219263));
#167962=CARTESIAN_POINT('Ctrl Pts',(79.1440359318979,-6.58085173641304,
53.9752626894438));
#167963=CARTESIAN_POINT('Ctrl Pts',(79.186753643857,-6.53550864566605,53.968380522767));
#167964=CARTESIAN_POINT('Ctrl Pts',(79.5483377831547,-6.14400436424126,
53.9100533480883));
#167965=CARTESIAN_POINT('Ctrl Pts',(79.8416142209471,-5.77457148759858,
53.8622838239147));
#167966=CARTESIAN_POINT('Ctrl Pts',(80.3708586533091,-4.99547711129451,
53.7771091168074));
#167967=CARTESIAN_POINT('Ctrl Pts',(80.6062308265866,-4.58701194791107,
53.7398057883377));
#167968=CARTESIAN_POINT('Ctrl Pts',(80.8462381816745,-4.08905797442266,
53.7031622174816));
#167969=CARTESIAN_POINT('Ctrl Pts',(80.8807176040813,-4.0151287727142,53.6979376914601));
#167970=CARTESIAN_POINT('Ctrl Pts',(80.9337350371828,-3.89756652116829,
53.6899704515841));
#167971=CARTESIAN_POINT('Ctrl Pts',(80.9528956660566,-3.85422707012049,
53.687105600925));
#167972=CARTESIAN_POINT('Ctrl Pts',(80.9883517264494,-3.77239880783103,
53.6818323773236));
#167973=CARTESIAN_POINT('Ctrl Pts',(81.0047178280493,-3.73394275719147,
53.679410119329));
#167974=CARTESIAN_POINT('Ctrl Pts',(81.0410858170288,-3.646918087512,53.6740546748789));
#167975=CARTESIAN_POINT('Ctrl Pts',(81.0609422827981,-3.5982884438105,53.6711499899173));
#167976=CARTESIAN_POINT('Ctrl Pts',(81.1185961564571,-3.45372068577784,
53.6627746923882));
#167977=CARTESIAN_POINT('Ctrl Pts',(81.1552558234924,-3.35732440722175,
53.6575269593339));
#167978=CARTESIAN_POINT('Ctrl Pts',(81.3954166105477,-2.69395378083437,
53.6236990299759));
#167979=CARTESIAN_POINT('Ctrl Pts',(81.5470779541456,-2.1091564217122,53.6053174237616));
#167980=CARTESIAN_POINT('Ctrl Pts',(81.6900577174245,-1.22312945548832,
53.5925709806086));
#167981=CARTESIAN_POINT('Ctrl Pts',(81.7236322173041,-0.930354280515686,
53.5907155989023));
#167982=CARTESIAN_POINT('Ctrl Pts',(81.7536654417887,-0.490907646989111,
53.5911051470487));
#167983=CARTESIAN_POINT('Ctrl Pts',(81.7602996923846,-0.345106621283968,
53.5917525887928));
#167984=CARTESIAN_POINT('Ctrl Pts',(81.7644966198225,-0.159963493406468,
53.5931914921324));
#167985=CARTESIAN_POINT('Ctrl Pts',(81.7651455184341,-0.120707251723698,
53.5935317274066));
#167986=CARTESIAN_POINT('Ctrl Pts',(81.7658013224872,-0.0575839547028548,
53.5941342791524));
#167987=CARTESIAN_POINT('Ctrl Pts',(81.7659601909634,-0.0337187247201237,
53.5943748322806));
#167988=CARTESIAN_POINT('Ctrl Pts',(81.7660395656254,-0.00656885437556106,
53.5946628240841));
#167989=CARTESIAN_POINT('Ctrl Pts',(81.7660474803996,-0.00328442583511579,
53.5946979021895));
#167990=CARTESIAN_POINT('Ctrl Pts',(81.7660537076114,-1.08793519407556E-11,
53.5947332184626));
#167991=CARTESIAN_POINT('Ctrl Pts',(81.7739479911102,4.5045009216105E-12,
53.6395039249478));
#167992=CARTESIAN_POINT('Ctrl Pts',(81.7739435788723,-0.0023271519310627,
53.6394789019034));
#167993=CARTESIAN_POINT('Ctrl Pts',(81.7739383296181,-0.00465430567239209,
53.6394540562307));
#167994=CARTESIAN_POINT('Ctrl Pts',(81.7738705745845,-0.0305610931805376,
53.6391794376136));
#167995=CARTESIAN_POINT('Ctrl Pts',(81.7737229710217,-0.0541406115829586,
53.6389476853336));
#167996=CARTESIAN_POINT('Ctrl Pts',(81.7731133581065,-0.115682941145436,
53.6383899097105));
#167997=CARTESIAN_POINT('Ctrl Pts',(81.7725144821153,-0.153644232417719,
53.6380926315016));
#167998=CARTESIAN_POINT('Ctrl Pts',(81.7688374252251,-0.323482709412806,
53.6369690995888));
#167999=CARTESIAN_POINT('Ctrl Pts',(81.7632915785597,-0.455295166218249,
53.6366541539024));
#168000=CARTESIAN_POINT('Ctrl Pts',(81.7394807488555,-0.835862496200755,
53.6372823187662));
#168001=CARTESIAN_POINT('Ctrl Pts',(81.7142958664717,-1.08407074726912,
53.6395935649047));
#168002=CARTESIAN_POINT('Ctrl Pts',(81.5924716314608,-1.94936756526757,
53.6537996749283));
#168003=CARTESIAN_POINT('Ctrl Pts',(81.4456102316304,-2.55761463047674,
53.6747380167085));
#168004=CARTESIAN_POINT('Ctrl Pts',(81.1986495746275,-3.26826109240764,
53.7109029249683));
#168005=CARTESIAN_POINT('Ctrl Pts',(81.1540428298269,-3.38874829255497,
53.7174645646486));
#168006=CARTESIAN_POINT('Ctrl Pts',(81.087941795081,-3.55682559483755,53.7272210815887));
#168007=CARTESIAN_POINT('Ctrl Pts',(81.0684557847543,-3.60520834751748,
53.7301009338568));
#168008=CARTESIAN_POINT('Ctrl Pts',(81.0337331261786,-3.6894292577611,53.7352387300448));
#168009=CARTESIAN_POINT('Ctrl Pts',(81.0186708254145,-3.72533957941291,
53.7374693613516));
#168010=CARTESIAN_POINT('Ctrl Pts',(80.9865333797313,-3.8006662385055,53.7422326164722));
#168011=CARTESIAN_POINT('Ctrl Pts',(80.9694112848591,-3.84006112394793,
53.7447725953886));
#168012=CARTESIAN_POINT('Ctrl Pts',(80.9275832170625,-3.93455336022793,
53.7509828505172));
#168013=CARTESIAN_POINT('Ctrl Pts',(80.902620584541,-3.98953237409775,53.7546933318891));
#168014=CARTESIAN_POINT('Ctrl Pts',(80.8123136977879,-4.18352510474944,
53.7681318751447));
#168015=CARTESIAN_POINT('Ctrl Pts',(80.7441527510494,-4.32117009628719,
53.7783016409775));
#168016=CARTESIAN_POINT('Ctrl Pts',(80.5643579982684,-4.66324994061301,
53.8052075804389));
#168017=CARTESIAN_POINT('Ctrl Pts',(80.4485274313295,-4.8653104872372,53.8226098499921));
#168018=CARTESIAN_POINT('Ctrl Pts',(80.0798593958943,-5.4571323354101,53.8783380774478));
#168019=CARTESIAN_POINT('Ctrl Pts',(79.8059598832282,-5.83260429851963,
53.9201398194718));
#168020=CARTESIAN_POINT('Ctrl Pts',(79.3990001339462,-6.31256365636161,
53.9837484290553));
#168021=CARTESIAN_POINT('Ctrl Pts',(79.2886415813603,-6.43602604468151,
54.0011305791617));
#168022=CARTESIAN_POINT('Ctrl Pts',(79.1448752567326,-6.58864459546846,
54.0239966366722));
#168023=CARTESIAN_POINT('Ctrl Pts',(79.1143654252176,-6.62058356424803,
54.0288613989999));
#168024=CARTESIAN_POINT('Ctrl Pts',(79.0655146741229,-6.67101344014595,
54.0366712996995));
#168025=CARTESIAN_POINT('Ctrl Pts',(79.0473161370937,-6.68964619426383,
54.0395852455076));
#168026=CARTESIAN_POINT('Ctrl Pts',(79.0122623193101,-6.72524215981955,
54.0452070213877));
#168027=CARTESIAN_POINT('Ctrl Pts',(78.9954190497796,-6.74221713054289,
54.0479122341511));
#168028=CARTESIAN_POINT('Ctrl Pts',(78.954464104476,-6.78318141256307,54.0544992800625));
#168029=CARTESIAN_POINT('Ctrl Pts',(78.9302883451521,-6.80710395385358,
54.0583952896698));
#168030=CARTESIAN_POINT('Ctrl Pts',(78.8436411808546,-6.89192562861749,
54.0723843141305));
#168031=CARTESIAN_POINT('Ctrl Pts',(78.7804709522617,-6.95207928737868,
54.082629881807));
#168032=CARTESIAN_POINT('Ctrl Pts',(78.618253936078,-7.10232838853546,54.1090375827375));
#168033=CARTESIAN_POINT('Ctrl Pts',(78.5181286810934,-7.19119057019406,
54.1254268511999));
#168034=CARTESIAN_POINT('Ctrl Pts',(78.1629462060085,-7.49315467367921,
54.1837812503194));
#168035=CARTESIAN_POINT('Ctrl Pts',(77.8987140240129,-7.69472446669826,
54.2275599272912));
#168036=CARTESIAN_POINT('Ctrl Pts',(77.264300242671,-8.12742409278371,54.3327211296841));
#168037=CARTESIAN_POINT('Ctrl Pts',(76.8876626359836,-8.34744965195274,
54.3951721960963));
#168038=CARTESIAN_POINT('Ctrl Pts',(76.4250228660552,-8.5758891808143,54.4714026165396));
#168039=CARTESIAN_POINT('Ctrl Pts',(76.3523256671751,-8.61061911215167,
54.4833688334468));
#168040=CARTESIAN_POINT('Ctrl Pts',(76.2366258054512,-8.6640594022498,54.5023922734591));
#168041=CARTESIAN_POINT('Ctrl Pts',(76.1939116151177,-8.68339820377563,
54.5094108686884));
#168042=CARTESIAN_POINT('Ctrl Pts',(76.116987926664,-8.71752705457139,54.5220422921981));
#168043=CARTESIAN_POINT('Ctrl Pts',(76.0828313107758,-8.73243635728515,
54.5276481375869));
#168044=CARTESIAN_POINT('Ctrl Pts',(76.002530235741,-8.76691456812469,54.5408203550892));
#168045=CARTESIAN_POINT('Ctrl Pts',(75.9563166060691,-8.78631597794009,
54.5483956828099));
#168046=CARTESIAN_POINT('Ctrl Pts',(75.8211527954778,-8.84177934234442,
54.5705360162297));
#168047=CARTESIAN_POINT('Ctrl Pts',(75.7318054675107,-8.87683564604249,
54.5851517050483));
#168048=CARTESIAN_POINT('Ctrl Pts',(75.3293014073264,-9.0276104052791,54.650908246581));
#168049=CARTESIAN_POINT('Ctrl Pts',(75.0106843999781,-9.12774682512769,
54.7027176279918));
#168050=CARTESIAN_POINT('Ctrl Pts',(74.2396112397559,-9.3251214178566,54.8277914888407));
#168051=CARTESIAN_POINT('Ctrl Pts',(73.783972807736,-9.40608394327155,54.901438813675));
#168052=CARTESIAN_POINT('Ctrl Pts',(73.092669241097,-9.47622175434809,55.0138724992235));
#168053=CARTESIAN_POINT('Ctrl Pts',(72.8601880300136,-9.49097913818975,
55.0518073070235));
#168054=CARTESIAN_POINT('Ctrl Pts',(72.5817834234466,-9.49812562146044,
55.0975408063158));
#168055=CARTESIAN_POINT('Ctrl Pts',(72.5361119356159,-9.49895960144131,
55.1050531341384));
#168056=CARTESIAN_POINT('Ctrl Pts',(72.4650996505089,-9.49973028158489,
55.116750710549));
#168057=CARTESIAN_POINT('Ctrl Pts',(72.4397608132908,-9.49990115533811,
55.1209280512153));
#168058=CARTESIAN_POINT('Ctrl Pts',(72.3929060488989,-9.5000245869161,55.1286590755608));
#168059=CARTESIAN_POINT('Ctrl Pts',(72.3713904102209,-9.500006190287,55.1322117535819));
#168060=CARTESIAN_POINT('Ctrl Pts',(72.3219102349707,-9.49979122054929,
55.1403878330069));
#168061=CARTESIAN_POINT('Ctrl Pts',(72.2939465000311,-9.49954288575259,
55.1450128275175));
#168062=CARTESIAN_POINT('Ctrl Pts',(72.2058374496105,-9.49836070547216,
55.1595980445449));
#168063=CARTESIAN_POINT('Ctrl Pts',(72.145702023126,-9.49696685006281,55.1695711682019));
#168064=CARTESIAN_POINT('Ctrl Pts',(71.8323995737194,-9.48664504836688,
55.221613452924));
#168065=CARTESIAN_POINT('Ctrl Pts',(71.5796956094659,-9.46790170270744,
55.263869514766));
#168066=CARTESIAN_POINT('Ctrl Pts',(70.6761818374809,-9.36341453496009,
55.4153036215634));
#168067=CARTESIAN_POINT('Ctrl Pts',(70.0340001689457,-9.21881299824602,
55.523457096834));
#168068=CARTESIAN_POINT('Ctrl Pts',(69.2614117502248,-8.95628610894851,
55.651780029097));
#168069=CARTESIAN_POINT('Ctrl Pts',(69.1123853901585,-8.90135057236214,
55.6764546418972));
#168070=CARTESIAN_POINT('Ctrl Pts',(68.9065643467413,-8.81943700671664,
55.7104096977477));
#168071=CARTESIAN_POINT('Ctrl Pts',(68.8485657978985,-8.7956736413379,55.719964133609));
#168072=CARTESIAN_POINT('Ctrl Pts',(68.7550615019874,-8.75625629838545,
55.735344761527));
#168073=CARTESIAN_POINT('Ctrl Pts',(68.719410575645,-8.74096463309731,55.7412035936562));
#168074=CARTESIAN_POINT('Ctrl Pts',(68.6450439249085,-8.7085157178352,55.7534134745602));
#168075=CARTESIAN_POINT('Ctrl Pts',(68.6063469642528,-8.69131612870886,
55.7597603922748));
#168076=CARTESIAN_POINT('Ctrl Pts',(68.5143005003488,-8.64965144430281,
55.7748418241645));
#168077=CARTESIAN_POINT('Ctrl Pts',(68.4610588711095,-8.62494388705857,
55.7835526017649));
#168078=CARTESIAN_POINT('Ctrl Pts',(68.2774377262581,-8.53761763459406,
55.8135509717747));
#168079=CARTESIAN_POINT('Ctrl Pts',(68.1482483613159,-8.47245687800116,
55.8345796874533));
#168080=CARTESIAN_POINT('Ctrl Pts',(67.8312326484309,-8.303217406328,55.8860012949317));
#168081=CARTESIAN_POINT('Ctrl Pts',(67.6453277735364,-8.19559664811225,
55.9159932278355));
#168082=CARTESIAN_POINT('Ctrl Pts',(67.2239787149258,-7.9319341052037,55.9836725900661));
#168083=CARTESIAN_POINT('Ctrl Pts',(66.9914862156297,-7.77142214123729,
56.0207889067569));
#168084=CARTESIAN_POINT('Ctrl Pts',(66.5006882927859,-7.39881576768811,
56.0989483301185));
#168085=CARTESIAN_POINT('Ctrl Pts',(66.2456699050642,-7.18290369070718,
56.1394305134399));
#168086=CARTESIAN_POINT('Ctrl Pts',(65.9535117858883,-6.90755300798338,
56.1860614781161));
#168087=CARTESIAN_POINT('Ctrl Pts',(65.9049799446759,-6.8608196681872,56.1938168845393));
#168088=CARTESIAN_POINT('Ctrl Pts',(65.8352781908649,-6.7922438347912,56.204973657854));
#168089=CARTESIAN_POINT('Ctrl Pts',(65.8137101651539,-6.77081769195838,
56.2084285426796));
#168090=CARTESIAN_POINT('Ctrl Pts',(65.7756635704857,-6.73265350446117,
56.2145282533942));
#168091=CARTESIAN_POINT('Ctrl Pts',(65.7591436431825,-6.71595806535549,
56.2171785472124));
#168092=CARTESIAN_POINT('Ctrl Pts',(65.7233028979491,-6.67946447995962,
56.2229324986162));
#168093=CARTESIAN_POINT('Ctrl Pts',(65.7040063823056,-6.65964256163827,
56.2260329095319));
#168094=CARTESIAN_POINT('Ctrl Pts',(65.6488963048328,-6.60253091306488,
56.2348940548648));
#168095=CARTESIAN_POINT('Ctrl Pts',(65.6132996938343,-6.56502872188158,
56.2406255726365));
#168096=CARTESIAN_POINT('Ctrl Pts',(65.5325701330007,-6.47856449704637,
56.2536386882547));
#168097=CARTESIAN_POINT('Ctrl Pts',(65.4876414162638,-6.42941125399487,
56.2608915979324));
#168098=CARTESIAN_POINT('Ctrl Pts',(65.3385176849451,-6.26275979422972,
56.2849897995331));
#168099=CARTESIAN_POINT('Ctrl Pts',(65.2367084334307,-6.14311162624957,
56.3014835051011));
#168100=CARTESIAN_POINT('Ctrl Pts',(64.9435887003916,-5.78073977715671,
56.3489748009083));
#168101=CARTESIAN_POINT('Ctrl Pts',(64.7610302256386,-5.5310248850314,56.3785531895552));
#168102=CARTESIAN_POINT('Ctrl Pts',(64.3563075352983,-4.91675613630517,
56.4435176420691));
#168103=CARTESIAN_POINT('Ctrl Pts',(64.145710531136,-4.54517280094908,56.4767839281));
#168104=CARTESIAN_POINT('Ctrl Pts',(63.925193946218,-4.08738129239885,56.5104471382329));
#168105=CARTESIAN_POINT('Ctrl Pts',(63.8909012843529,-4.01381963946874,
56.515642807749));
#168106=CARTESIAN_POINT('Ctrl Pts',(63.8381020056929,-3.89670771459341,
56.5235766947342));
#168107=CARTESIAN_POINT('Ctrl Pts',(63.8189810319182,-3.85344706253765,
56.5264354292444));
#168108=CARTESIAN_POINT('Ctrl Pts',(63.7852221324119,-3.77551868167044,
56.5314559495459));
#168109=CARTESIAN_POINT('Ctrl Pts',(63.7704675525215,-3.74090406713161,
56.5336406385959));
#168110=CARTESIAN_POINT('Ctrl Pts',(63.7363311990189,-3.65949861945083,
56.5386722921987));
#168111=CARTESIAN_POINT('Ctrl Pts',(63.7171143098185,-3.61263790917291,
56.5414869325814));
#168112=CARTESIAN_POINT('Ctrl Pts',(63.6621297106346,-3.4754831692157,56.5494869678141));
#168113=CARTESIAN_POINT('Ctrl Pts',(63.6273535235925,-3.38478746534386,
56.5544780988672));
#168114=CARTESIAN_POINT('Ctrl Pts',(63.477518677162,-2.97561215049119,56.5756642310369));
#168115=CARTESIAN_POINT('Ctrl Pts',(63.3778759563504,-2.65159817599759,
56.5888443814968));
#168116=CARTESIAN_POINT('Ctrl Pts',(63.1813227904579,-1.86765951736082,
56.612572443422));
#168117=CARTESIAN_POINT('Ctrl Pts',(63.1005088166986,-1.40452708149557,
56.620103561528));
#168118=CARTESIAN_POINT('Ctrl Pts',(63.0306375983541,-0.705469652835039,
56.6229891492765));
#168119=CARTESIAN_POINT('Ctrl Pts',(63.0158903312778,-0.472850780734742,
56.6225728925549));
#168120=CARTESIAN_POINT('Ctrl Pts',(63.0083792183321,-0.193782659307004,
56.6205773809409));
#168121=CARTESIAN_POINT('Ctrl Pts',(63.0074700259392,-0.147622185050712,
56.6201983997499));
#168122=CARTESIAN_POINT('Ctrl Pts',(63.006574086225,-0.0758064158346538,
56.6195343448282));
#168123=CARTESIAN_POINT('Ctrl Pts',(63.0063569701409,-0.0501543953342147,
56.6192823776814));
#168124=CARTESIAN_POINT('Ctrl Pts',(63.0061457093478,-0.00269292086676632,
56.6187891942779));
#168125=CARTESIAN_POINT('Ctrl Pts',(63.0061230385094,0.0191160765268714,
56.618552061429));
#168126=CARTESIAN_POINT('Ctrl Pts',(63.0062420791469,0.0693062479474148,
56.6179820379973));
#168127=CARTESIAN_POINT('Ctrl Pts',(63.006435382794,0.0976869089277555,
56.617641795673));
#168128=CARTESIAN_POINT('Ctrl Pts',(63.0074427319032,0.187235856074897,
56.6165108651902));
#168129=CARTESIAN_POINT('Ctrl Pts',(63.008715915933,0.248396566000516,56.6156539759828));
#168130=CARTESIAN_POINT('Ctrl Pts',(63.0184259441006,0.567997460409354,
56.6107209291361));
#168131=CARTESIAN_POINT('Ctrl Pts',(63.0367170380479,0.826006183880536,
56.6051794327142));
#168132=CARTESIAN_POINT('Ctrl Pts',(63.1334101599791,1.69300303724305,56.5806779675544));
#168133=CARTESIAN_POINT('Ctrl Pts',(63.25963213391,2.29486024221408,56.5537057007334));
#168134=CARTESIAN_POINT('Ctrl Pts',(63.500892638895,3.06905337443102,56.5035814234627));
#168135=CARTESIAN_POINT('Ctrl Pts',(63.5655845641365,3.25611292617718,56.4902301950731));
#168136=CARTESIAN_POINT('Ctrl Pts',(63.6603134830605,3.50488340961284,56.4707607076978));
#168137=CARTESIAN_POINT('Ctrl Pts',(63.6853302238838,3.56852787414792,56.465625807306));
#168138=CARTESIAN_POINT('Ctrl Pts',(63.7277513709704,3.67315314557332,56.4569287111113));
#168139=CARTESIAN_POINT('Ctrl Pts',(63.7447670543967,3.71429508499674,56.4534427487512));
#168140=CARTESIAN_POINT('Ctrl Pts',(63.7786185223381,3.79455747131133,56.4465125044715));
#168141=CARTESIAN_POINT('Ctrl Pts',(63.7954298849918,3.83368748356148,56.443073017419));
#168142=CARTESIAN_POINT('Ctrl Pts',(63.8359941654029,3.92639666985897,56.4347790344227));
#168143=CARTESIAN_POINT('Ctrl Pts',(63.8599773790326,3.97986909359566,56.429879367455));
#168144=CARTESIAN_POINT('Ctrl Pts',(63.9438512138028,4.16236946002337,56.412758319666));
#168145=CARTESIAN_POINT('Ctrl Pts',(64.0061080455079,4.29024477489271,56.4000732153486));
#168146=CARTESIAN_POINT('Ctrl Pts',(64.1667180715454,4.60225824568439,56.3674150360299));
#168147=CARTESIAN_POINT('Ctrl Pts',(64.2682717164075,4.78459800433314,56.3468202175828));
#168148=CARTESIAN_POINT('Ctrl Pts',(64.5246663128105,5.21136054059977,56.2950271687821));
#168149=CARTESIAN_POINT('Ctrl Pts',(64.6847764424568,5.45225071430965,56.2628362507192));
#168150=CARTESIAN_POINT('Ctrl Pts',(65.0562216874646,5.95917156752946,56.1887981878117));
#168151=CARTESIAN_POINT('Ctrl Pts',(65.2713472417803,6.22183166709789,56.1463001040846));
#168152=CARTESIAN_POINT('Ctrl Pts',(65.5454901724754,6.52186677953113,56.0930068462174));
#168153=CARTESIAN_POINT('Ctrl Pts',(65.59148852512,6.57113338955384,56.0840919239196));
#168154=CARTESIAN_POINT('Ctrl Pts',(65.6589636675872,6.64185876114554,56.0710583318046));
#168155=CARTESIAN_POINT('Ctrl Pts',(65.6800251815459,6.66372118754364,56.0669961133184));
#168156=CARTESIAN_POINT('Ctrl Pts',(65.7175278111001,6.70227325825661,56.0597740556079));
#168157=CARTESIAN_POINT('Ctrl Pts',(65.7339264651989,6.71900477355933,56.0566198703855));
#168158=CARTESIAN_POINT('Ctrl Pts',(65.769755424473,6.75528769292943,56.0497366972799));
#168159=CARTESIAN_POINT('Ctrl Pts',(65.78920917177,6.77481475013885,56.0460046078108));
#168160=CARTESIAN_POINT('Ctrl Pts',(65.8452184814091,6.83054100844442,56.0352736823481));
#168161=CARTESIAN_POINT('Ctrl Pts',(65.8819837963559,6.86652255685391,56.02824685625));
#168162=CARTESIAN_POINT('Ctrl Pts',(66.2045633178061,7.17706385419258,55.9667269602566));
#168163=CARTESIAN_POINT('Ctrl Pts',(66.5070134402033,7.4333039653498,55.9099347347465));
#168164=CARTESIAN_POINT('Ctrl Pts',(67.2468054604889,7.98344971704667,55.7714739233163));
#168165=CARTESIAN_POINT('Ctrl Pts',(67.694384990695,8.2608602358875,55.6879930552982));
#168166=CARTESIAN_POINT('Ctrl Pts',(68.2412859584078,8.53880768467192,55.5852861202919));
#168167=CARTESIAN_POINT('Ctrl Pts',(68.3207880524256,8.57779076856391,55.570341393945));
#168168=CARTESIAN_POINT('Ctrl Pts',(68.4488976763201,8.63834839773323,55.5462337554238));
#168169=CARTESIAN_POINT('Ctrl Pts',(68.4971652485335,8.66065843933449,55.5371450293802));
#168170=CARTESIAN_POINT('Ctrl Pts',(68.5834417130519,8.69963910682542,55.5208886229814));
#168171=CARTESIAN_POINT('Ctrl Pts',(68.621378167446,8.71647311521148,55.5137369203664));
#168172=CARTESIAN_POINT('Ctrl Pts',(68.7011587395927,8.75123510638607,55.4986890876233));
#168173=CARTESIAN_POINT('Ctrl Pts',(68.7430237709636,8.76911027582995,55.4907882610334));
#168174=CARTESIAN_POINT('Ctrl Pts',(68.8538854190036,8.8154810367184,55.4698544469925));
#168175=CARTESIAN_POINT('Ctrl Pts',(68.9230903630514,8.8434485186948,55.4567745383863));
#168176=CARTESIAN_POINT('Ctrl Pts',(69.2682526784094,8.97809914497562,55.3914786174327));
#168177=CARTESIAN_POINT('Ctrl Pts',(69.548710500393,9.07226064872847,55.3382288845659));
#168178=CARTESIAN_POINT('Ctrl Pts',(70.1668832416476,9.24722317947999,55.2205736727544));
#168179=CARTESIAN_POINT('Ctrl Pts',(70.505588672187,9.32271153541284,55.1559278539401));
#168180=CARTESIAN_POINT('Ctrl Pts',(71.2280333597365,9.44129039968847,55.018196396144));
#168181=CARTESIAN_POINT('Ctrl Pts',(71.6118780328604,9.4796880791591,54.9451078323308));
#168182=CARTESIAN_POINT('Ctrl Pts',(72.064452436974,9.49629949500186,54.8596882082981));
#168183=CARTESIAN_POINT('Ctrl Pts',(72.1318693912012,9.49802993185262,54.8469839017132));
#168184=CARTESIAN_POINT('Ctrl Pts',(72.2256162144575,9.49940219307597,54.8293506638683));
#168185=CARTESIAN_POINT('Ctrl Pts',(72.2519314844745,9.49967417411436,54.8244045025594));
#168186=CARTESIAN_POINT('Ctrl Pts',(72.2999330840384,9.49996379432037,54.8153891609369));
#168187=CARTESIAN_POINT('Ctrl Pts',(72.3216188479708,9.50001777310287,54.8113188710497));
#168188=CARTESIAN_POINT('Ctrl Pts',(72.366762842118,9.49997013945874,54.802851213075));
#168189=CARTESIAN_POINT('Ctrl Pts',(72.3902208756095,9.49985545870245,54.7984543078638));
#168190=CARTESIAN_POINT('Ctrl Pts',(72.4522682021779,9.49931425883601,54.7868321513294));
#168191=CARTESIAN_POINT('Ctrl Pts',(72.4908566582702,9.49873431089071,54.7796120959425));
#168192=CARTESIAN_POINT('Ctrl Pts',(72.6728524530838,9.49485114642883,54.7455942552908));
#168193=CARTESIAN_POINT('Ctrl Pts',(72.8161928622921,9.48843043562868,54.7189019812377));
#168194=CARTESIAN_POINT('Ctrl Pts',(73.2482509079764,9.45892269217232,54.6386418160273));
#168195=CARTESIAN_POINT('Ctrl Pts',(73.5361475678402,9.4255384738796,54.5854222547199));
#168196=CARTESIAN_POINT('Ctrl Pts',(74.4074689976157,9.28251837826274,54.4243855960287));
#168197=CARTESIAN_POINT('Ctrl Pts',(74.9825551345731,9.12996383677311,54.3180520805766));
#168198=CARTESIAN_POINT('Ctrl Pts',(75.6346424247745,8.88757546275032,54.1959999981996));
#168199=CARTESIAN_POINT('Ctrl Pts',(75.7293912938865,8.85056189003455,54.1782307582996));
#168200=CARTESIAN_POINT('Ctrl Pts',(75.8714788050035,8.79233028683736,54.1515276443941));
#168201=CARTESIAN_POINT('Ctrl Pts',(75.9192728784128,8.77227118345709,54.142535833178));
#168202=CARTESIAN_POINT('Ctrl Pts',(76.0047993741645,8.73552586772809,54.1264275362523));
#168203=CARTESIAN_POINT('Ctrl Pts',(76.0425924403916,8.71898778531994,54.1193032450804));
#168204=CARTESIAN_POINT('Ctrl Pts',(76.1230079048321,8.68315460977871,54.1041308926769));
#168205=CARTESIAN_POINT('Ctrl Pts',(76.1655977719933,8.66378751482831,54.0960871671847));
#168206=CARTESIAN_POINT('Ctrl Pts',(76.2811236426335,8.61019148723119,54.0742463352153));
#168207=CARTESIAN_POINT('Ctrl Pts',(76.3537681635725,8.57532826400436,54.0604883251766));
#168208=CARTESIAN_POINT('Ctrl Pts',(76.8430959574678,8.33257438134261,53.9676542582478));
#168209=CARTESIAN_POINT('Ctrl Pts',(77.2443395148981,8.09426590044972,53.890688505867));
#168210=CARTESIAN_POINT('Ctrl Pts',(78.0093841367439,7.55827125933498,53.7430263679308));
#168211=CARTESIAN_POINT('Ctrl Pts',(78.3720343067702,7.26119636107946,53.6725580848276));
#168212=CARTESIAN_POINT('Ctrl Pts',(78.7564490765101,6.89501641006542,53.5983289894072));
#168213=CARTESIAN_POINT('Ctrl Pts',(78.8009811114762,6.85174880886952,53.5897383474476));
#168214=CARTESIAN_POINT('Ctrl Pts',(78.8661819108371,6.787134839058,53.5771768078695));
#168215=CARTESIAN_POINT('Ctrl Pts',(78.8871756400428,6.76613262704809,53.5731347171465));
#168216=CARTESIAN_POINT('Ctrl Pts',(78.9244982501218,6.72844076320482,53.5659537884372));
#168217=CARTESIAN_POINT('Ctrl Pts',(78.9408641104192,6.71178988869277,53.5628067745242));
#168218=CARTESIAN_POINT('Ctrl Pts',(78.9770482353132,6.6747014325592,53.5558529342696));
#168219=CARTESIAN_POINT('Ctrl Pts',(78.9968366417043,6.65423413168898,53.552052677177));
#168220=CARTESIAN_POINT('Ctrl Pts',(79.0551614614934,6.59335986069459,53.5408588098267));
#168221=CARTESIAN_POINT('Ctrl Pts',(79.0934376842599,6.55269492202907,53.5335219884846));
#168222=CARTESIAN_POINT('Ctrl Pts',(79.1813467109718,6.4576246267802,53.5166883797742));
#168223=CARTESIAN_POINT('Ctrl Pts',(79.2307137207254,6.40296857267175,53.5072479025901));
#168224=CARTESIAN_POINT('Ctrl Pts',(79.4009217115848,6.21003926904902,53.4747280630421));
#168225=CARTESIAN_POINT('Ctrl Pts',(79.5184267884624,6.0687648685244,53.4523294721632));
#168226=CARTESIAN_POINT('Ctrl Pts',(80.0069152335273,5.44539984906099,53.3591640048695));
#168227=CARTESIAN_POINT('Ctrl Pts',(80.3356543188246,4.93090226056861,53.2962266732256));
#168228=CARTESIAN_POINT('Ctrl Pts',(80.6730303960008,4.27059756054935,53.2294276028492));
#168229=CARTESIAN_POINT('Ctrl Pts',(80.7304863243917,4.15214632014954,53.2179566607241));
#168230=CARTESIAN_POINT('Ctrl Pts',(80.8074861057222,3.98464594931615,53.202436251855));
#168231=CARTESIAN_POINT('Ctrl Pts',(80.8290950047086,3.93659324884282,53.1980630778914));
#168232=CARTESIAN_POINT('Ctrl Pts',(80.8660164081746,3.85263510295497,53.1905593473035));
#168233=CARTESIAN_POINT('Ctrl Pts',(80.8815080047392,3.81681236055175,53.1874007537807));
#168234=CARTESIAN_POINT('Ctrl Pts',(80.9135102763582,3.74154525083389,53.1808540485433));
#168235=CARTESIAN_POINT('Ctrl Pts',(80.9299767197412,3.7020824303408,53.1774728802268));
#168236=CARTESIAN_POINT('Ctrl Pts',(80.968741686554,3.60739333612914,53.1694821560375));
#168237=CARTESIAN_POINT('Ctrl Pts',(80.9907906994876,3.55206361323786,53.1649117173043));
#168238=CARTESIAN_POINT('Ctrl Pts',(81.0657476691169,3.35872375019643,53.1492835296927));
#168239=CARTESIAN_POINT('Ctrl Pts',(81.115978782651,3.21966537406848,53.1386459342224));
#168240=CARTESIAN_POINT('Ctrl Pts',(81.2317263970142,2.8743652716097,53.1137102932119));
#168241=CARTESIAN_POINT('Ctrl Pts',(81.2935211652247,2.66692257399266,53.1000034635478));
#168242=CARTESIAN_POINT('Ctrl Pts',(81.4318744016013,2.13757404759784,53.0682844376273));
#168243=CARTESIAN_POINT('Ctrl Pts',(81.4989227246745,1.81338860362256,53.0518329643473));
#168244=CARTESIAN_POINT('Ctrl Pts',(81.6072433598528,1.1081318123274,53.022821058296));
#168245=CARTESIAN_POINT('Ctrl Pts',(81.6427654782644,0.72671346380171,53.0112929320736));
#168246=CARTESIAN_POINT('Ctrl Pts',(81.6578886087804,0.276722274049013,
53.0031342417759));
#168247=CARTESIAN_POINT('Ctrl Pts',(81.6594498991434,0.209314703980056,
53.0020555649737));
#168248=CARTESIAN_POINT('Ctrl Pts',(81.6606569610688,0.114496078260597,
53.0007444782374));
#168249=CARTESIAN_POINT('Ctrl Pts',(81.6608896428737,0.0870961888499821,
53.0003898246238));
#168250=CARTESIAN_POINT('Ctrl Pts',(81.6610909333258,0.0397972357573462,
52.9998197807963));
#168251=CARTESIAN_POINT('Ctrl Pts',(81.6611144031703,0.0198986838339381,
52.9995928490222));
#168252=CARTESIAN_POINT('Ctrl Pts',(81.6610766756267,4.47259269587928E-12,
52.9993788854899));
#168253=CARTESIAN_POINT('Origin',(73.035119430904,-4.33680868994202E-16,
58.7874639765594));
#168254=CARTESIAN_POINT('',(82.5462364603111,-3.03519734642508E-8,56.9158101410025));
#168255=CARTESIAN_POINT('',(82.39079308452,-1.59709532818419E-15,57.1378062887238));
#168256=CARTESIAN_POINT('',(82.39079308452,-1.59709532818419E-15,57.1378062887238));
#168257=CARTESIAN_POINT('Ctrl Pts',(82.5462364601441,-3.03547367494313E-8,
56.915810141241));
#168258=CARTESIAN_POINT('Ctrl Pts',(82.5394791927201,1.22772898505908,56.9254605240026));
#168259=CARTESIAN_POINT('Ctrl Pts',(82.3004566029504,2.36750148144016,56.9793265804536));
#168260=CARTESIAN_POINT('Ctrl Pts',(81.6097765366974,4.21810104194341,57.1158850602721));
#168261=CARTESIAN_POINT('Ctrl Pts',(81.1769289619715,5.0196562288422,57.1971869538061));
#168262=CARTESIAN_POINT('Ctrl Pts',(80.3683710665038,6.11649038759656,57.34709448945));
#168263=CARTESIAN_POINT('Ctrl Pts',(80.069467258252,6.46633420673903,57.4023163122276));
#168264=CARTESIAN_POINT('Ctrl Pts',(78.8544190108279,7.69413928944279,57.6284971380434));
#168265=CARTESIAN_POINT('Ctrl Pts',(77.7887687197478,8.40501154231076,57.8292098024945));
#168266=CARTESIAN_POINT('Ctrl Pts',(75.7162159760365,9.25735872008406,58.2099244804492));
#168267=CARTESIAN_POINT('Ctrl Pts',(74.7560968307291,9.48744079427912,58.3836063847351));
#168268=CARTESIAN_POINT('Ctrl Pts',(72.3919766058581,9.66844304883471,58.8140516484161));
#168269=CARTESIAN_POINT('Ctrl Pts',(71.1462539173082,9.44699055352527,59.0467388176038));
#168270=CARTESIAN_POINT('Ctrl Pts',(69.304796347293,8.82095876131073,59.3871655574635));
#168271=CARTESIAN_POINT('Ctrl Pts',(68.5394038610483,8.43938374434001,59.5275098223593));
#168272=CARTESIAN_POINT('Ctrl Pts',(67.4999205036203,7.73139162193156,59.7177539829203));
#168273=CARTESIAN_POINT('Ctrl Pts',(67.1788228698108,7.48086138733766,59.7765194114987));
#168274=CARTESIAN_POINT('Ctrl Pts',(66.1091496978421,6.52721452808879,59.9736525925835));
#168275=CARTESIAN_POINT('Ctrl Pts',(65.4640288365233,5.72283346920203,60.0969323016118));
#168276=CARTESIAN_POINT('Ctrl Pts',(64.5534632021598,4.12018849825052,60.2726887746335));
#168277=CARTESIAN_POINT('Ctrl Pts',(64.2398628362638,3.35652371332293,60.3336831026002));
#168278=CARTESIAN_POINT('Ctrl Pts',(64.0263520775731,2.56296981511781,60.375952723877));
#168279=CARTESIAN_POINT('Origin',(73.035119430904,-4.33680868994202E-16,
58.7874639765594));
#168280=CARTESIAN_POINT('Origin',(72.2537026314029,-4.33680868994202E-16,
54.3558290880045));
#168281=CARTESIAN_POINT('',(62.5686102705547,3.28094194101619E-11,57.0166456920447));
#168282=CARTESIAN_POINT('',(62.5638890606905,-3.07089118677747E-11,56.9898703803749));
#168283=CARTESIAN_POINT('',(62.4056251012807,-1.65832766814156E-15,56.0923108646735));
#168284=CARTESIAN_POINT('',(76.6496952865773,-8.99107646638512,54.0790152794585));
#168285=CARTESIAN_POINT('Ctrl Pts',(62.5686102705547,6.5620497147992E-11,
57.0166456920447));
#168286=CARTESIAN_POINT('Ctrl Pts',(62.5685931686666,0.00949481003547198,
57.0165487024174));
#168287=CARTESIAN_POINT('Ctrl Pts',(62.5685893034143,0.0189896258170846,
57.0164489074448));
#168288=CARTESIAN_POINT('Ctrl Pts',(62.5686245154731,0.0546590393284597,
57.0160634979369));
#168289=CARTESIAN_POINT('Ctrl Pts',(62.5687509591852,0.0808332025605581,
57.0157594299316));
#168290=CARTESIAN_POINT('Ctrl Pts',(62.5694109838782,0.156908809992044,
57.0148143792232));
#168291=CARTESIAN_POINT('Ctrl Pts',(62.5702097450935,0.206806476872946,
57.0141178915667));
#168292=CARTESIAN_POINT('Ctrl Pts',(62.5812022844503,0.677655472505252,
57.0068335645316));
#168293=CARTESIAN_POINT('Ctrl Pts',(62.6170777414993,1.09751123819944,56.9949813703744));
#168294=CARTESIAN_POINT('Ctrl Pts',(62.7772610752319,2.17611177745555,56.952210362231));
#168295=CARTESIAN_POINT('Ctrl Pts',(62.9409331099227,2.82662380432915,56.914370342928));
#168296=CARTESIAN_POINT('Ctrl Pts',(63.2028308187524,3.55301820666139,56.8593144038791));
#168297=CARTESIAN_POINT('Ctrl Pts',(63.2395042796987,3.6500064231196,56.851683891133));
#168298=CARTESIAN_POINT('Ctrl Pts',(63.2970458462827,3.79534464003068,56.8398263299778));
#168299=CARTESIAN_POINT('Ctrl Pts',(63.3168090952313,3.84413840190321,56.8357725971545));
#168300=CARTESIAN_POINT('Ctrl Pts',(63.3529324808322,3.9313471081286,56.8283962528255));
#168301=CARTESIAN_POINT('Ctrl Pts',(63.369151024419,3.96982121447812,56.8250958401242));
#168302=CARTESIAN_POINT('Ctrl Pts',(63.4041974662658,4.05153158218341,56.8179877955404));
#168303=CARTESIAN_POINT('Ctrl Pts',(63.4230906979521,4.09473781598478,56.814169950057));
#168304=CARTESIAN_POINT('Ctrl Pts',(63.4750952395725,4.21141774879543,56.8036982139025));
#168305=CARTESIAN_POINT('Ctrl Pts',(63.5087853591859,4.28462135804108,56.7969536717606));
#168306=CARTESIAN_POINT('Ctrl Pts',(63.7140831478127,4.71690802153265,56.7560762678939));
#168307=CARTESIAN_POINT('Ctrl Pts',(63.9059480925585,5.06566528059715,56.7187809113607));
#168308=CARTESIAN_POINT('Ctrl Pts',(64.2775530262497,5.65507833823716,56.6475024582404));
#168309=CARTESIAN_POINT('Ctrl Pts',(64.4484320726923,5.90088720053665,56.6150003138333));
#168310=CARTESIAN_POINT('Ctrl Pts',(64.7263329313838,6.26462888920473,56.5622352149397));
#168311=CARTESIAN_POINT('Ctrl Pts',(64.8256734777039,6.38841120222158,56.5433883991211));
#168312=CARTESIAN_POINT('Ctrl Pts',(65.0416190896722,6.64470626388179,56.5023733078897));
#168313=CARTESIAN_POINT('Ctrl Pts',(65.1588690692999,6.77658307013366,56.480077510073));
#168314=CARTESIAN_POINT('Ctrl Pts',(65.3103902693084,6.93814801427767,56.4511627079599));
#168315=CARTESIAN_POINT('Ctrl Pts',(65.341503665052,6.97087418729542,56.4452201255802));
#168316=CARTESIAN_POINT('Ctrl Pts',(65.3910395910919,7.02227228460847,56.4357491367867));
#168317=CARTESIAN_POINT('Ctrl Pts',(65.4093179219078,7.04108811820308,56.4322523557138));
#168318=CARTESIAN_POINT('Ctrl Pts',(65.4442560166114,7.07676996905371,56.4255641409131));
#168319=CARTESIAN_POINT('Ctrl Pts',(65.4609022407199,7.09364932422797,56.4223756724639));
#168320=CARTESIAN_POINT('Ctrl Pts',(65.500890200341,7.13390812031383,56.4147120269516));
#168321=CARTESIAN_POINT('Ctrl Pts',(65.5242873191044,7.15722984841443,56.4102245973399));
#168322=CARTESIAN_POINT('Ctrl Pts',(65.6054669157639,7.23734412275618,56.3946444049743));
#168323=CARTESIAN_POINT('Ctrl Pts',(65.6638160395522,7.29353376969087,56.3834278350622));
#168324=CARTESIAN_POINT('Ctrl Pts',(65.8104477559555,7.43131412919587,56.3552091290267));
#168325=CARTESIAN_POINT('Ctrl Pts',(65.8995224735566,7.51200847800988,56.3380395757951));
#168326=CARTESIAN_POINT('Ctrl Pts',(66.3097465810958,7.87023483209404,56.2589171939135));
#168327=CARTESIAN_POINT('Ctrl Pts',(66.6467668404386,8.12820303385394,56.1937991707027));
#168328=CARTESIAN_POINT('Ctrl Pts',(67.3507618757592,8.59804670772538,56.0586588105352));
#168329=CARTESIAN_POINT('Ctrl Pts',(67.7169564898264,8.8095210453915,55.9887881688906));
#168330=CARTESIAN_POINT('Ctrl Pts',(68.1676576844471,9.03211541989052,55.9035840143207));
#168331=CARTESIAN_POINT('Ctrl Pts',(68.2402913230476,9.06687398848686,55.8898752203572));
#168332=CARTESIAN_POINT('Ctrl Pts',(68.3562224385685,9.12059472436967,55.8680306475622));
#168333=CARTESIAN_POINT('Ctrl Pts',(68.3992468473656,9.1401520682891,55.8599314749069));
#168334=CARTESIAN_POINT('Ctrl Pts',(68.480039378945,9.17616936533186,55.8447371902219));
#168335=CARTESIAN_POINT('Ctrl Pts',(68.5177735984549,9.19270466941119,55.8376465899271));
#168336=CARTESIAN_POINT('Ctrl Pts',(68.6025437256243,9.22921096226979,55.8217306694835));
#168337=CARTESIAN_POINT('Ctrl Pts',(68.6496331977045,9.24905145350947,55.8128984482855));
#168338=CARTESIAN_POINT('Ctrl Pts',(68.7904402123359,9.30707550747282,55.7865148074635));
#168339=CARTESIAN_POINT('Ctrl Pts',(68.884591039805,9.34416392126299,55.7689081535047));
#168340=CARTESIAN_POINT('Ctrl Pts',(69.3246383188335,9.50961615068189,55.6867707097593));
#168341=CARTESIAN_POINT('Ctrl Pts',(69.6769592990388,9.61962438373294,55.621458900797));
#168342=CARTESIAN_POINT('Ctrl Pts',(70.5371960288035,9.83528754798808,55.4625864613907));
#168343=CARTESIAN_POINT('Ctrl Pts',(71.048908636252,9.92074096312156,55.3685832667829));
#168344=CARTESIAN_POINT('Ctrl Pts',(71.7627018734177,9.9817681495456,55.2366069271219));
#168345=CARTESIAN_POINT('Ctrl Pts',(71.9611017592097,9.99258891067112,55.1998277628777));
#168346=CARTESIAN_POINT('Ctrl Pts',(72.203599699639,9.99833155165266,55.1546549956625));
#168347=CARTESIAN_POINT('Ctrl Pts',(72.2475490442521,9.9990724239228,55.1464592656265));
#168348=CARTESIAN_POINT('Ctrl Pts',(72.3164058741999,9.99976338670872,55.1336034720334));
#168349=CARTESIAN_POINT('Ctrl Pts',(72.3413119942273,9.99991702651808,55.1289502857122));
#168350=CARTESIAN_POINT('Ctrl Pts',(72.3855259707677,10.0000188413299,55.1206839567672));
#168351=CARTESIAN_POINT('Ctrl Pts',(72.4048336877748,10.0000054342108,55.1170721372491));
#168352=CARTESIAN_POINT('Ctrl Pts',(72.451123325768,9.99983454951726,55.1084081491416));
#168353=CARTESIAN_POINT('Ctrl Pts',(72.4781044759894,9.999621919639,55.1033542587867));
#168354=CARTESIAN_POINT('Ctrl Pts',(72.5603302356578,9.99862944185504,55.0879412849576));
#168355=CARTESIAN_POINT('Ctrl Pts',(72.6155674512234,9.99748873097646,55.07757194825));
#168356=CARTESIAN_POINT('Ctrl Pts',(73.1223786800342,9.98267180163953,54.9823072472566));
#168357=CARTESIAN_POINT('Ctrl Pts',(73.5723841650235,9.93780530720776,54.8968391548794));
#168358=CARTESIAN_POINT('Ctrl Pts',(74.6122274687567,9.7598650388144,54.6991641364504));
#168359=CARTESIAN_POINT('Ctrl Pts',(75.1962568126423,9.60265922768935,54.5880604160712));
#168360=CARTESIAN_POINT('Ctrl Pts',(75.8642685014173,9.35412961381878,54.4619437842037));
#168361=CARTESIAN_POINT('Ctrl Pts',(75.9653346411857,9.31459158333285,54.4428868311959));
#168362=CARTESIAN_POINT('Ctrl Pts',(76.114319610202,9.25341560240702,54.4148306996414));
#168363=CARTESIAN_POINT('Ctrl Pts',(76.1627401318286,9.23307411184802,54.4057181318169));
#168364=CARTESIAN_POINT('Ctrl Pts',(76.2489646345519,9.19602816007876,54.3895012115302));
#168365=CARTESIAN_POINT('Ctrl Pts',(76.2868291479776,9.17947383065478,54.3823832852544));
#168366=CARTESIAN_POINT('Ctrl Pts',(76.3669161884763,9.14385162252252,54.3673356218294));
#168367=CARTESIAN_POINT('Ctrl Pts',(76.4091113546987,9.12472220695442,54.359411926295));
#168368=CARTESIAN_POINT('Ctrl Pts',(76.5222538670056,9.07245359044907,54.3381768175924));
#168369=CARTESIAN_POINT('Ctrl Pts',(76.5929497175994,9.0387559043459,54.324920629335));
#168370=CARTESIAN_POINT('Ctrl Pts',(76.9868495342344,8.84515095815546,54.2511247644129));
#168371=CARTESIAN_POINT('Ctrl Pts',(77.3016797901881,8.66816136434575,54.1924003023509));
#168372=CARTESIAN_POINT('Ctrl Pts',(77.9709902958771,8.2416025614237,54.0677152862301));
#168373=CARTESIAN_POINT('Ctrl Pts',(78.3203102234116,7.98506816980612,54.0027534996117));
#168374=CARTESIAN_POINT('Ctrl Pts',(78.8273338068105,7.55846796156511,53.907693947408));
#168375=CARTESIAN_POINT('Ctrl Pts',(78.9976561830876,7.40469695446938,53.8756072407743));
#168376=CARTESIAN_POINT('Ctrl Pts',(79.196823627565,7.21184006112934,53.8377489170521));
#168377=CARTESIAN_POINT('Ctrl Pts',(79.2308806640514,7.17837944237662,53.8312627113588));
#168378=CARTESIAN_POINT('Ctrl Pts',(79.2838709764714,7.12555516319683,53.8211490058739));
#168379=CARTESIAN_POINT('Ctrl Pts',(79.3029677609928,7.10636076056874,53.8174997318882));
#168380=CARTESIAN_POINT('Ctrl Pts',(79.3368221267231,7.07205185340416,53.8110220008779));
#168381=CARTESIAN_POINT('Ctrl Pts',(79.3516101682565,7.05696863452912,53.8081895358175));
#168382=CARTESIAN_POINT('Ctrl Pts',(79.3872954209661,7.02033641678031,53.8013475080595));
#168383=CARTESIAN_POINT('Ctrl Pts',(79.4081435121506,6.99873873800463,53.7973444558431));
#168384=CARTESIAN_POINT('Ctrl Pts',(79.472887103537,6.93105197815689,53.7848957028617));
#168385=CARTESIAN_POINT('Ctrl Pts',(79.5164398444057,6.88462875973907,53.7764964389036));
#168386=CARTESIAN_POINT('Ctrl Pts',(79.7397312256811,6.64196310873446,53.7333162623742));
#168387=CARTESIAN_POINT('Ctrl Pts',(79.9120338929608,6.43883812475559,53.6995973295178));
#168388=CARTESIAN_POINT('Ctrl Pts',(80.4910429915452,5.69778386465837,53.5854046058007));
#168389=CARTESIAN_POINT('Ctrl Pts',(80.8516218033384,5.1249567220635,53.5127439344644));
#168390=CARTESIAN_POINT('Ctrl Pts',(81.2045052046764,4.4145165200458,53.4413396392349));
#168391=CARTESIAN_POINT('Ctrl Pts',(81.2547358913952,4.30880570084298,53.4311620728742));
#168392=CARTESIAN_POINT('Ctrl Pts',(81.3253878608425,4.15318401133537,53.416829086828));
#168393=CARTESIAN_POINT('Ctrl Pts',(81.3472580920879,4.10396827141044,53.4123896352064));
#168394=CARTESIAN_POINT('Ctrl Pts',(81.3854810065323,4.01606350294559,53.4046259712041));
#168395=CARTESIAN_POINT('Ctrl Pts',(81.4019872345779,3.97744534865631,53.4012716403612));
#168396=CARTESIAN_POINT('Ctrl Pts',(81.4360602604884,3.89633100871155,53.39434391029));
#168397=CARTESIAN_POINT('Ctrl Pts',(81.4535790343089,3.8538149174761,53.3907799353671));
#168398=CARTESIAN_POINT('Ctrl Pts',(81.4989448627626,3.74154699526084,53.3815451884075));
#168399=CARTESIAN_POINT('Ctrl Pts',(81.526308285344,3.6715951766271,53.3759692528103));
#168400=CARTESIAN_POINT('Ctrl Pts',(81.6549014398985,3.33174312405532,53.3497343074538));
#168401=CARTESIAN_POINT('Ctrl Pts',(81.7453916640756,3.05776684845851,53.3311807258126));
#168402=CARTESIAN_POINT('Ctrl Pts',(82.0082139313181,2.1308095937197,53.276714972163));
#168403=CARTESIAN_POINT('Ctrl Pts',(82.1271784738995,1.46408438971074,53.2510864460441));
#168404=CARTESIAN_POINT('Ctrl Pts',(82.1931395076163,0.603094753541315,
53.2321347455033));
#168405=CARTESIAN_POINT('Ctrl Pts',(82.2022677019319,0.415597777414796,
53.2288426076628));
#168406=CARTESIAN_POINT('Ctrl Pts',(82.2070769805183,0.184138117262164,
53.2257262275492));
#168407=CARTESIAN_POINT('Ctrl Pts',(82.2077021702983,0.140325651796728,
53.225178143409));
#168408=CARTESIAN_POINT('Ctrl Pts',(82.2082371524422,0.0713779561209165,
53.2243800307341));
#168409=CARTESIAN_POINT('Ctrl Pts',(82.2083383205992,0.046245093079615,
53.2241025670669));
#168410=CARTESIAN_POINT('Ctrl Pts',(82.2083513337792,0.00143950189477805,
53.2236316253277));
#168411=CARTESIAN_POINT('Ctrl Pts',(82.2082995334347,-0.0182328740553303,
53.2234329773184));
#168412=CARTESIAN_POINT('Ctrl Pts',(82.2080361066515,-0.0656420563921209,
53.2229738974244));
#168413=CARTESIAN_POINT('Ctrl Pts',(82.2077676701436,-0.0933783996608032,
53.2227215509783));
#168414=CARTESIAN_POINT('Ctrl Pts',(82.2065890355628,-0.178794268618658,
53.2219950719772));
#168415=CARTESIAN_POINT('Ctrl Pts',(82.2052988794444,-0.236467836561447,
53.2215756707227));
#168416=CARTESIAN_POINT('Ctrl Pts',(82.1944060681179,-0.588546837825432,
53.2194608974788));
#168417=CARTESIAN_POINT('Ctrl Pts',(82.1724294942745,-0.88243790565272,
53.2196020910157));
#168418=CARTESIAN_POINT('Ctrl Pts',(82.0822731726419,-1.64151812111276,
53.2254919879159));
#168419=CARTESIAN_POINT('Ctrl Pts',(81.9944941765417,-2.10363409194026,
53.2345433800741));
#168420=CARTESIAN_POINT('Ctrl Pts',(81.785379399967,-2.89923456200442,53.2608445865819));
#168421=CARTESIAN_POINT('Ctrl Pts',(81.6779400874776,-3.23560135778612,
53.2754738746009));
#168422=CARTESIAN_POINT('Ctrl Pts',(81.5246116259184,-3.64133935041874,
53.2976187432487));
#168423=CARTESIAN_POINT('Ctrl Pts',(81.4950606031747,-3.71678883849265,
53.3019329823102));
#168424=CARTESIAN_POINT('Ctrl Pts',(81.4466581165149,-3.83613447830237,
53.3090708071552));
#168425=CARTESIAN_POINT('Ctrl Pts',(81.4283931195386,-3.88027139020126,
53.3117794605117));
#168426=CARTESIAN_POINT('Ctrl Pts',(81.3935834438828,-3.96273216800703,
53.3169694548881));
#168427=CARTESIAN_POINT('Ctrl Pts',(81.3771123605242,-4.0010868763655,53.3194363769157));
#168428=CARTESIAN_POINT('Ctrl Pts',(81.3396269055438,-4.08690797437958,
53.3250751795106));
#168429=CARTESIAN_POINT('Ctrl Pts',(81.3184842492748,-4.13431534304264,
53.3282722461304));
#168430=CARTESIAN_POINT('Ctrl Pts',(81.2541380793106,-4.27566213026408,
53.3380506897363));
#168431=CARTESIAN_POINT('Ctrl Pts',(81.2098637021002,-4.3690916563408,53.3448420829308));
#168432=CARTESIAN_POINT('Ctrl Pts',(80.9912583899368,-4.81268285252289,
53.3786559820135));
#168433=CARTESIAN_POINT('Ctrl Pts',(80.7982406709098,-5.15296585623734,
53.4093446978793));
#168434=CARTESIAN_POINT('Ctrl Pts',(80.3613417059943,-5.82824181038578,
53.4797969457659));
#168435=CARTESIAN_POINT('Ctrl Pts',(80.1155533618687,-6.16106793349038,
53.5199203502594));
#168436=CARTESIAN_POINT('Ctrl Pts',(79.7283107431263,-6.62248904205124,
53.5829706910569));
#168437=CARTESIAN_POINT('Ctrl Pts',(79.6025159653024,-6.76398184540343,
53.6034272604744));
#168438=CARTESIAN_POINT('Ctrl Pts',(79.4411707345731,-6.93533705453489,
53.6295502026618));
#168439=CARTESIAN_POINT('Ctrl Pts',(79.4093138900537,-6.96870113621365,
53.6347027001072));
#168440=CARTESIAN_POINT('Ctrl Pts',(79.3588027252295,-7.02086859285705,
53.6428623218664));
#168441=CARTESIAN_POINT('Ctrl Pts',(79.3403022211868,-7.03982318528284,
53.6458488290259));
#168442=CARTESIAN_POINT('Ctrl Pts',(79.3051007124267,-7.07560071712405,
53.6515270435608));
#168443=CARTESIAN_POINT('Ctrl Pts',(79.2884148380019,-7.09243837342628,
53.654216721746));
#168444=CARTESIAN_POINT('Ctrl Pts',(79.2485560113145,-7.13237222496328,
53.6606375865655));
#168445=CARTESIAN_POINT('Ctrl Pts',(79.2253293412192,-7.15541328442209,
53.6643758686284));
#168446=CARTESIAN_POINT('Ctrl Pts',(79.1458234574229,-7.23350661259238,
53.6771621491895));
#168447=CARTESIAN_POINT('Ctrl Pts',(79.0890084007561,-7.28799729217439,
53.6862823131678));
#168448=CARTESIAN_POINT('Ctrl Pts',(78.9472362368661,-7.42076340791128,
53.70901044749));
#168449=CARTESIAN_POINT('Ctrl Pts',(78.8615564050088,-7.49823271888026,
53.722720614747));
#168450=CARTESIAN_POINT('Ctrl Pts',(78.4928148849061,-7.82010270632613,
53.7816783144235));
#168451=CARTESIAN_POINT('Ctrl Pts',(78.1975549213685,-8.04971976131072,
53.8287842325848));
#168452=CARTESIAN_POINT('Ctrl Pts',(77.4946396176575,-8.53511901737442,
53.9415857835965));
#168453=CARTESIAN_POINT('Ctrl Pts',(77.0800086819011,-8.77880988180894,
54.0086030220957));
#168454=CARTESIAN_POINT('Ctrl Pts',(76.6496952865772,-8.99107646638516,
54.0790152794585));
#168455=CARTESIAN_POINT('',(77.9145171600383,-8.24294705479842,53.8559930573772));
#168456=CARTESIAN_POINT('Origin',(72.3389200802052,-4.33680868994202E-16,
54.8391212561108));
#168457=CARTESIAN_POINT('Ctrl Pts',(77.9145171600384,-8.24294705479845,
53.8559930573776));
#168458=CARTESIAN_POINT('Ctrl Pts',(78.3213525049871,-7.95968552154139,
53.7882909406893));
#168459=CARTESIAN_POINT('Ctrl Pts',(78.7066406568712,-7.64588391010058,
53.7242405516931));
#168460=CARTESIAN_POINT('Ctrl Pts',(79.1153143825233,-7.25872586587658,
53.6576053048667));
#168461=CARTESIAN_POINT('Ctrl Pts',(79.1628447870651,-7.21279207225363,
53.6498776832898));
#168462=CARTESIAN_POINT('Ctrl Pts',(79.2316566723277,-7.1449561476965,53.638727453146));
#168463=CARTESIAN_POINT('Ctrl Pts',(79.2532933544652,-7.12342974689743,
53.6352269656706));
#168464=CARTESIAN_POINT('Ctrl Pts',(79.2913755032853,-7.08519266371684,
53.6290761688813));
#168465=CARTESIAN_POINT('Ctrl Pts',(79.3078606857158,-7.06852344330279,
53.626417065223));
#168466=CARTESIAN_POINT('Ctrl Pts',(79.3437537073191,-7.03197327270077,
53.6206351724958));
#168467=CARTESIAN_POINT('Ctrl Pts',(79.3631378764722,-7.01206882310716,
53.61751757868));
#168468=CARTESIAN_POINT('Ctrl Pts',(79.41767310297,-6.95560051615191,53.6087599817631));
#168469=CARTESIAN_POINT('Ctrl Pts',(79.4526324307376,-6.91884619202492,
53.6031618804814));
#168470=CARTESIAN_POINT('Ctrl Pts',(79.7280591780775,-6.6248273401461,53.559174211131));
#168471=CARTESIAN_POINT('Ctrl Pts',(79.9552681604661,-6.35506292800244,
53.523594164842));
#168472=CARTESIAN_POINT('Ctrl Pts',(80.4054397376295,-5.75936374378995,
53.4538920402273));
#168473=CARTESIAN_POINT('Ctrl Pts',(80.6244033749147,-5.43106846241846,
53.4204820818717));
#168474=CARTESIAN_POINT('Ctrl Pts',(80.9688584891665,-4.84215658921231,
53.3682552409087));
#168475=CARTESIAN_POINT('Ctrl Pts',(81.1034470810526,-4.58755226200957,
53.3479645477279));
#168476=CARTESIAN_POINT('Ctrl Pts',(81.2590761590207,-4.25980281262834,
53.3245849008017));
#168477=CARTESIAN_POINT('Ctrl Pts',(81.2904303026423,-4.19182407550534,
53.3198798723704));
#168478=CARTESIAN_POINT('Ctrl Pts',(81.3398082712556,-4.08154844968708,
53.3124782783543));
#168479=CARTESIAN_POINT('Ctrl Pts',(81.3583041848338,-4.03947115945202,
53.3097077474962));
#168480=CARTESIAN_POINT('Ctrl Pts',(81.3931809781168,-3.9586295611547,53.3044872579642));
#168481=CARTESIAN_POINT('Ctrl Pts',(81.4096081113492,-3.91988674847484,
53.3020300536218));
#168482=CARTESIAN_POINT('Ctrl Pts',(81.4465963369226,-3.83110678990619,
53.2965012025719));
#168483=CARTESIAN_POINT('Ctrl Pts',(81.4669986327005,-3.78100338387256,
53.2934544259837));
#168484=CARTESIAN_POINT('Ctrl Pts',(81.5305771698515,-3.62119512750036,
53.2839696316962));
#168485=CARTESIAN_POINT('Ctrl Pts',(81.572236572607,-3.51088379625024,53.2777694512274));
#168486=CARTESIAN_POINT('Ctrl Pts',(81.8651240172146,-2.69216385682614,
53.2343112982109));
#168487=CARTESIAN_POINT('Ctrl Pts',(82.0385197218235,-1.95789195221018,
53.2091171996664));
#168488=CARTESIAN_POINT('Ctrl Pts',(82.1557779714219,-0.992821857504143,
53.1961360517622));
#168489=CARTESIAN_POINT('Ctrl Pts',(82.1752039634383,-0.773882537922454,
53.1945149798879));
#168490=CARTESIAN_POINT('Ctrl Pts',(82.194423697907,-0.432031790683103,
53.1941895029693));
#168491=CARTESIAN_POINT('Ctrl Pts',(82.199097873528,-0.309465939716292,
53.1945131090541));
#168492=CARTESIAN_POINT('Ctrl Pts',(82.2023080731677,-0.149763588622181,
53.1955318282972));
#168493=CARTESIAN_POINT('Ctrl Pts',(82.2028513961955,-0.112675467650475,
53.1958103295903));
#168494=CARTESIAN_POINT('Ctrl Pts',(82.2034079333408,-0.0521905018019316,
53.1963337441948));
#168495=CARTESIAN_POINT('Ctrl Pts',(82.2035428066805,-0.0287949156210848,
53.1965530888186));
#168496=CARTESIAN_POINT('Ctrl Pts',(82.2036492377446,0.0168896857020898,
53.1970146422514));
#168497=CARTESIAN_POINT('Ctrl Pts',(82.2036282217056,0.03917850045416,53.1972552920767));
#168498=CARTESIAN_POINT('Ctrl Pts',(82.2034176645911,0.089117039237505,
53.1978288885152));
#168499=CARTESIAN_POINT('Ctrl Pts',(82.2031887983291,0.11676636883879,53.1981701078976));
#168500=CARTESIAN_POINT('Ctrl Pts',(82.2019882750365,0.214051685765103,
53.199453157529));
#168501=CARTESIAN_POINT('Ctrl Pts',(82.2004164388026,0.283676631147189,
53.2005200694232));
#168502=CARTESIAN_POINT('Ctrl Pts',(82.1854431741609,0.739836407447927,
53.2084635920051));
#168503=CARTESIAN_POINT('Ctrl Pts',(82.1507781497542,1.12527542774975,53.2196531721575));
#168504=CARTESIAN_POINT('Ctrl Pts',(82.0472356809411,1.82541293831156,53.2473373839046));
#168505=CARTESIAN_POINT('Ctrl Pts',(81.9851889410471,2.14065632040254,53.262601494305));
#168506=CARTESIAN_POINT('Ctrl Pts',(81.8147773529143,2.83107629400283,53.3018785874066));
#168507=CARTESIAN_POINT('Ctrl Pts',(81.6994566408859,3.20393279213455,53.327027734262));
#168508=CARTESIAN_POINT('Ctrl Pts',(81.534409024631,3.645013793902,53.361444931191));
#168509=CARTESIAN_POINT('Ctrl Pts',(81.5050244062944,3.72073359133889,53.3675253981988));
#168510=CARTESIAN_POINT('Ctrl Pts',(81.4570803095161,3.83997159893516,53.3773740258539));
#168511=CARTESIAN_POINT('Ctrl Pts',(81.4391230893453,3.88373578376918,53.3810477506789));
#168512=CARTESIAN_POINT('Ctrl Pts',(81.4047440391612,3.96586499924193,53.388053381821));
#168513=CARTESIAN_POINT('Ctrl Pts',(81.3883905835414,4.00425844883778,53.3913745616527));
#168514=CARTESIAN_POINT('Ctrl Pts',(81.3509570056587,4.09064416497588,53.398951955667));
#168515=CARTESIAN_POINT('Ctrl Pts',(81.3297400306502,4.13857388585655,53.4032295829852));
#168516=CARTESIAN_POINT('Ctrl Pts',(81.2643845016779,4.28314263220271,53.416355706068));
#168517=CARTESIAN_POINT('Ctrl Pts',(81.2190916104298,4.37923486845521,53.4253850558867));
#168518=CARTESIAN_POINT('Ctrl Pts',(80.9515672387241,4.92418214483371,53.4783601702573));
#168519=CARTESIAN_POINT('Ctrl Pts',(80.6976545542606,5.356188667899,53.527248938));
#168520=CARTESIAN_POINT('Ctrl Pts',(80.3075667002764,5.91868773389435,53.6015669614577));
#168521=CARTESIAN_POINT('Ctrl Pts',(80.1981682730969,6.06744525204309,53.6223445870643));
#168522=CARTESIAN_POINT('Ctrl Pts',(79.9024844656567,6.44698191690618,53.6784726869544));
#168523=CARTESIAN_POINT('Ctrl Pts',(79.7099997632217,6.67252150865751,53.7149802152015));
#168524=CARTESIAN_POINT('Ctrl Pts',(79.4742736725412,6.92500277122591,53.7599509479243));
#168525=CARTESIAN_POINT('Ctrl Pts',(79.440355264385,6.9607946606352,53.7664277800239));
#168526=CARTESIAN_POINT('Ctrl Pts',(79.3873681495772,7.0158821806866,53.7765571260367));
#168527=CARTESIAN_POINT('Ctrl Pts',(79.3684806038538,7.03535822530672,53.7801699742222));
#168528=CARTESIAN_POINT('Ctrl Pts',(79.3331054726813,7.07153807419901,53.7869410716904));
#168529=CARTESIAN_POINT('Ctrl Pts',(79.3166377119049,7.08826153616138,53.7900949671569));
#168530=CARTESIAN_POINT('Ctrl Pts',(79.2784323070172,7.12678621626691,53.7974161046985));
#168531=CARTESIAN_POINT('Ctrl Pts',(79.2566531709839,7.14854412365631,53.801592526273));
#168532=CARTESIAN_POINT('Ctrl Pts',(79.1852675547447,7.21919989637126,53.8152903251426));
#168533=CARTESIAN_POINT('Ctrl Pts',(79.135256140556,7.26766846322225,53.8249003507436));
#168534=CARTESIAN_POINT('Ctrl Pts',(78.8156881144894,7.57091353084329,53.8863716156883));
#168535=CARTESIAN_POINT('Ctrl Pts',(78.5328018589116,7.81063953083945,53.9410611683261));
#168536=CARTESIAN_POINT('Ctrl Pts',(77.9736667631488,8.23267027361622,54.0488349431247));
#168537=CARTESIAN_POINT('Ctrl Pts',(77.700321763642,8.41811447270732,54.101392894075));
#168538=CARTESIAN_POINT('Ctrl Pts',(77.250526983879,8.69111022486983,54.1873553235274));
#168539=CARTESIAN_POINT('Ctrl Pts',(77.0797732891893,8.7878289353557,54.2198784292574));
#168540=CARTESIAN_POINT('Ctrl Pts',(76.785694745722,8.94287577886063,54.2756668084484));
#168541=CARTESIAN_POINT('Ctrl Pts',(76.6638197830142,9.00389919819087,54.2987246169373));
#168542=CARTESIAN_POINT('Ctrl Pts',(76.4889155403398,9.08692943818848,54.3317219233844));
#168543=CARTESIAN_POINT('Ctrl Pts',(76.4368897146813,9.11106585925497,54.3415256087708));
#168544=CARTESIAN_POINT('Ctrl Pts',(76.3463917995033,9.15208231039055,54.3585589846606));
#168545=CARTESIAN_POINT('Ctrl Pts',(76.3080161228249,9.16917655127408,54.3657758426482));
#168546=CARTESIAN_POINT('Ctrl Pts',(76.2338986411413,9.20161794471294,54.3797024288626));
#168547=CARTESIAN_POINT('Ctrl Pts',(76.1981727962142,9.21700046941069,54.3864100301935));
#168548=CARTESIAN_POINT('Ctrl Pts',(76.1036783887938,9.25701661837335,54.4041378260982));
#168549=CARTESIAN_POINT('Ctrl Pts',(76.0447613359343,9.28128620366111,54.415177129959));
#168550=CARTESIAN_POINT('Ctrl Pts',(75.8317856267572,9.36657683651875,54.4550333811033));
#168551=CARTESIAN_POINT('Ctrl Pts',(75.6764373842164,9.42422345570597,54.4840128765064));
#168552=CARTESIAN_POINT('Ctrl Pts',(74.8861778054217,9.69467707166735,54.6310206618911));
#168553=CARTESIAN_POINT('Ctrl Pts',(74.2322948513584,9.8452152704738,54.7511907050721));
#168554=CARTESIAN_POINT('Ctrl Pts',(73.3553891374439,9.95344756785505,54.9129267442595));
#168555=CARTESIAN_POINT('Ctrl Pts',(73.1414358637586,9.97265178972028,54.9524469832369));
#168556=CARTESIAN_POINT('Ctrl Pts',(72.8071601079025,9.99146775348171,55.0144367613227));
#168557=CARTESIAN_POINT('Ctrl Pts',(72.6871530679604,9.99598246383561,55.0367406512944));
#168558=CARTESIAN_POINT('Ctrl Pts',(72.5307022724023,9.99895120171713,55.0659064767255));
#168559=CARTESIAN_POINT('Ctrl Pts',(72.4942950130809,9.99943627525533,55.0726998440897));
#168560=CARTESIAN_POINT('Ctrl Pts',(72.4349003857445,9.99989195619382,55.0837936189728));
#168561=CARTESIAN_POINT('Ctrl Pts',(72.4119135490329,9.99998629424917,55.0880898326846));
#168562=CARTESIAN_POINT('Ctrl Pts',(72.3670090019568,10.0000103582077,55.0964880155532));
#168563=CARTESIAN_POINT('Ctrl Pts',(72.3450914454647,9.9999475308271,55.100589712496));
#168564=CARTESIAN_POINT('Ctrl Pts',(72.2959657850777,9.99963955696024,55.1097887977387));
#168565=CARTESIAN_POINT('Ctrl Pts',(72.2687583024436,9.99935404929783,55.1148874216539));
#168566=CARTESIAN_POINT('Ctrl Pts',(72.1729253539559,9.99794349796811,55.1328591367949));
#168567=CARTESIAN_POINT('Ctrl Pts',(72.1043141550645,9.99620210960415,55.1457490745891));
#168568=CARTESIAN_POINT('Ctrl Pts',(71.645274960245,9.97965440789786,55.2321211755954));
#168569=CARTESIAN_POINT('Ctrl Pts',(71.2561008595327,9.94190193294541,55.3059772517661));
#168570=CARTESIAN_POINT('Ctrl Pts',(70.4847514458789,9.81952100541946,55.4525715979359));
#168571=CARTESIAN_POINT('Ctrl Pts',(70.1032452753374,9.73505714580995,55.5251789894049));
#168572=CARTESIAN_POINT('Ctrl Pts',(69.4320850895938,9.54327503097831,55.652511085974));
#168573=CARTESIAN_POINT('Ctrl Pts',(69.1405515740728,9.44476816389429,55.7076831163667));
#168574=CARTESIAN_POINT('Ctrl Pts',(68.7833624712188,9.30486945645273,55.7750318353828));
#168575=CARTESIAN_POINT('Ctrl Pts',(68.7130477992302,9.27637724207569,55.7882779236005));
#168576=CARTESIAN_POINT('Ctrl Pts',(68.6008143123456,9.22936499221988,55.8094016020938));
#168577=CARTESIAN_POINT('Ctrl Pts',(68.5586882449006,9.21136904367418,55.817325852638));
#168578=CARTESIAN_POINT('Ctrl Pts',(68.4787057422203,9.17653225900244,55.8323629426998));
#168579=CARTESIAN_POINT('Ctrl Pts',(68.4408274936767,9.15974614989543,55.8394806768922));
#168580=CARTESIAN_POINT('Ctrl Pts',(68.3543291058352,9.12075216394802,55.8557266595136));
#168581=CARTESIAN_POINT('Ctrl Pts',(68.3057797977727,9.09838394398872,55.8648392750116));
#168582=CARTESIAN_POINT('Ctrl Pts',(68.1784093339627,9.03842665574957,55.8887316524423));
#168583=CARTESIAN_POINT('Ctrl Pts',(68.0998943524999,9.00017211488093,55.9034445281792));
#168584=CARTESIAN_POINT('Ctrl Pts',(67.4174763785686,8.6562795829925,56.0312022940559));
#168585=CARTESIAN_POINT('Ctrl Pts',(66.8453167095885,8.28921705592231,56.1373274536897));
#168586=CARTESIAN_POINT('Ctrl Pts',(66.0921755905048,7.68770791482057,56.27811528857));
#168587=CARTESIAN_POINT('Ctrl Pts',(65.8772541971612,7.500227094911,56.3184617932426));
#168588=CARTESIAN_POINT('Ctrl Pts',(65.6230393573239,7.25825490948418,56.3666777561398));
#168589=CARTESIAN_POINT('Ctrl Pts',(65.5758733348315,7.21245257664757,56.375645869119));
#168590=CARTESIAN_POINT('Ctrl Pts',(65.5075619195612,7.14477532374694,56.3886719304733));
#168591=CARTESIAN_POINT('Ctrl Pts',(65.4860585427239,7.12327357177135,56.3927778538137));
#168592=CARTESIAN_POINT('Ctrl Pts',(65.4481971095436,7.08506308867001,56.4000175881125));
#168593=CARTESIAN_POINT('Ctrl Pts',(65.4317989422668,7.06839559957553,56.4031566899719));
#168594=CARTESIAN_POINT('Ctrl Pts',(65.3960775986516,7.03182834483428,56.4100026170094));
#168595=CARTESIAN_POINT('Ctrl Pts',(65.3767786109534,7.01190491220764,56.4137062061511));
#168596=CARTESIAN_POINT('Ctrl Pts',(65.3224396491735,6.95533235989226,56.4241476894208));
#168597=CARTESIAN_POINT('Ctrl Pts',(65.2875953067392,6.91849167356383,56.4308592284819));
#168598=CARTESIAN_POINT('Ctrl Pts',(65.0075613497781,6.61780879386758,56.4849184093134));
#168599=CARTESIAN_POINT('Ctrl Pts',(64.7765038215339,6.34081331571827,56.5302699266778));
#168600=CARTESIAN_POINT('Ctrl Pts',(64.404975324249,5.8426753477537,56.6038621944375));
#168601=CARTESIAN_POINT('Ctrl Pts',(64.2573004463,5.62755015863068,56.6333328284688));
#168602=CARTESIAN_POINT('Ctrl Pts',(63.905344448837,5.06920505870918,56.7038769641504));
#168603=CARTESIAN_POINT('Ctrl Pts',(63.712735334331,4.71890369121622,56.7427704946597));
#168604=CARTESIAN_POINT('Ctrl Pts',(63.5067271573156,4.28490486719319,56.7845103748413));
#168605=CARTESIAN_POINT('Ctrl Pts',(63.4730211685367,4.21163965241819,56.7913457848994));
#168606=CARTESIAN_POINT('Ctrl Pts',(63.4209947451818,4.09488400238202,56.8019058025251));
#168607=CARTESIAN_POINT('Ctrl Pts',(63.4020981755873,4.05166448965373,56.8057433879861));
#168608=CARTESIAN_POINT('Ctrl Pts',(63.3670479653965,3.96994297956643,56.8128654431831));
#168609=CARTESIAN_POINT('Ctrl Pts',(63.3508292279652,3.93147113120173,56.8161626817023));
#168610=CARTESIAN_POINT('Ctrl Pts',(63.3147095875646,3.84428658170562,56.8235095826429));
#168611=CARTESIAN_POINT('Ctrl Pts',(63.2949489908331,3.79551479842813,56.8275317193774));
#168612=CARTESIAN_POINT('Ctrl Pts',(63.2361204593854,3.64699491858422,56.8395146673658));
#168613=CARTESIAN_POINT('Ctrl Pts',(63.1982501354834,3.54676204119937,56.8472407375714));
#168614=CARTESIAN_POINT('Ctrl Pts',(62.9432194224137,2.83789119790707,56.89937257243));
#168615=CARTESIAN_POINT('Ctrl Pts',(62.7829543507186,2.20960977442238,56.9325536750684));
#168616=CARTESIAN_POINT('Ctrl Pts',(62.6675377370273,1.46603257831083,56.9587000277526));
#168617=CARTESIAN_POINT('Ctrl Pts',(62.653025353269,1.36186430567599,56.9620734877445));
#168618=CARTESIAN_POINT('Ctrl Pts',(62.6008696196287,0.939452770540981,
56.9746222950362));
#168619=CARTESIAN_POINT('Ctrl Pts',(62.576706760898,0.61967254587812,56.9815288742265));
#168620=CARTESIAN_POINT('Ctrl Pts',(62.5661492407005,0.240484801933824,
56.9870292662832));
#168621=CARTESIAN_POINT('Ctrl Pts',(62.5650259598434,0.181705807685922,
56.9878057787459));
#168622=CARTESIAN_POINT('Ctrl Pts',(62.5641260848524,0.0949716285669506,
56.988842406409));
#168623=CARTESIAN_POINT('Ctrl Pts',(62.5639521579111,0.0670225197836035,
56.9891597235968));
#168624=CARTESIAN_POINT('Ctrl Pts',(62.5638673523048,0.0260486050623847,
56.9896007351212));
#168625=CARTESIAN_POINT('Ctrl Pts',(62.5638656015227,0.0130243126943486,
56.9897373368234));
#168626=CARTESIAN_POINT('Ctrl Pts',(62.5638890606905,-6.14161654078813E-11,
56.9898703803749));
#168627=CARTESIAN_POINT('Origin',(72.2537026314029,-4.33680868994202E-16,
54.3558290880045));
#168628=CARTESIAN_POINT('',(62.6814815860384,9.62546012605022E-15,57.6567707315034));
#168629=CARTESIAN_POINT('',(62.6767603761739,-1.97855053433324E-11,57.6299954198325));
#168630=CARTESIAN_POINT('',(62.4056251012807,-1.65832766814156E-15,56.0923108646735));
#168631=CARTESIAN_POINT('Ctrl Pts',(62.6814815860384,1.02164152390125E-14,
57.6567707315033));
#168632=CARTESIAN_POINT('Ctrl Pts',(62.6814467800136,0.0193239827663985,
57.6565733367276));
#168633=CARTESIAN_POINT('Ctrl Pts',(62.6814667819337,0.0386379061186494,
57.6563644329446));
#168634=CARTESIAN_POINT('Ctrl Pts',(62.6816358108951,0.0822795851394926,
57.6558663163279));
#168635=CARTESIAN_POINT('Ctrl Pts',(62.6818168480097,0.106597020978416,
57.6555704717971));
#168636=CARTESIAN_POINT('Ctrl Pts',(62.6827503906637,0.191328778297451,
57.6544763814131));
#168637=CARTESIAN_POINT('Ctrl Pts',(62.6839522664629,0.25173563754625,57.6535843353215));
#168638=CARTESIAN_POINT('Ctrl Pts',(62.6983697979476,0.752610954394169,
57.6452757657968));
#168639=CARTESIAN_POINT('Ctrl Pts',(62.7395768586216,1.19170326118966,57.6321602557347));
#168640=CARTESIAN_POINT('Ctrl Pts',(62.8721327213917,2.02001406534445,57.597587283528));
#168641=CARTESIAN_POINT('Ctrl Pts',(62.958223972576,2.40926975985943,57.5770725453641));
#168642=CARTESIAN_POINT('Ctrl Pts',(63.1185718279245,2.97360922428409,57.5414229492147));
#168643=CARTESIAN_POINT('Ctrl Pts',(63.1751777127269,3.15347783855469,57.5291430864392));
#168644=CARTESIAN_POINT('Ctrl Pts',(63.2806723227062,3.45850066534843,57.5067595373642));
#168645=CARTESIAN_POINT('Ctrl Pts',(63.3270884274095,3.58448352257791,57.4970475776677));
#168646=CARTESIAN_POINT('Ctrl Pts',(63.396953821441,3.76300576530805,57.4826159410961));
#168647=CARTESIAN_POINT('Ctrl Pts',(63.4183615824116,3.81635388271896,57.4782166045481));
#168648=CARTESIAN_POINT('Ctrl Pts',(63.4563555472384,3.90873254769104,57.4704473416695));
#168649=CARTESIAN_POINT('Ctrl Pts',(63.4727342466018,3.94784951390339,57.4671099446272));
#168650=CARTESIAN_POINT('Ctrl Pts',(63.5048385716458,4.02318046549636,57.4605906168753));
#168651=CARTESIAN_POINT('Ctrl Pts',(63.5205311644477,4.05940811246652,57.4574138738473));
#168652=CARTESIAN_POINT('Ctrl Pts',(63.5626945743402,4.15519228201309,57.4489042030205));
#168653=CARTESIAN_POINT('Ctrl Pts',(63.5895306704828,4.21458079301957,57.4435140775963));
#168654=CARTESIAN_POINT('Ctrl Pts',(63.689980181044,4.43122553157555,57.4234303374262));
#168655=CARTESIAN_POINT('Ctrl Pts',(63.7670758267679,4.58678145308591,57.4081909112725));
#168656=CARTESIAN_POINT('Ctrl Pts',(64.131180340086,5.27584275154966,57.3368970300171));
#168657=CARTESIAN_POINT('Ctrl Pts',(64.4619130310351,5.78405141775196,57.2739778488605));
#168658=CARTESIAN_POINT('Ctrl Pts',(64.9943877287862,6.45942005174256,57.1729082461595));
#168659=CARTESIAN_POINT('Ctrl Pts',(65.1603691071588,6.65403590688992,57.1414140701367));
#168660=CARTESIAN_POINT('Ctrl Pts',(65.3758470383112,6.88783488184467,57.1003384048787));
#168661=CARTESIAN_POINT('Ctrl Pts',(65.4185970285261,6.93335197496354,57.0921802957506));
#168662=CARTESIAN_POINT('Ctrl Pts',(65.4823633296937,6.99997734498814,57.0799947906232));
#168663=CARTESIAN_POINT('Ctrl Pts',(65.503056940761,7.02140516208031,57.0760377535803));
#168664=CARTESIAN_POINT('Ctrl Pts',(65.5385697534532,7.05784878325061,57.0692421329395));
#168665=CARTESIAN_POINT('Ctrl Pts',(65.5533419502679,7.07291192194743,57.0664139352711));
#168666=CARTESIAN_POINT('Ctrl Pts',(65.5872939540203,7.10731283037035,57.0599103117759));
#168667=CARTESIAN_POINT('Ctrl Pts',(65.6065047626977,7.12661822762156,57.056228017566));
#168668=CARTESIAN_POINT('Ctrl Pts',(65.6601141629369,7.18005022526594,57.0459461950387));
#168669=CARTESIAN_POINT('Ctrl Pts',(65.6946799705971,7.21400088796866,57.0393098887401));
#168670=CARTESIAN_POINT('Ctrl Pts',(65.9060084709376,7.41854867042736,56.9987022317964));
#168671=CARTESIAN_POINT('Ctrl Pts',(66.0886844941911,7.58265997151768,56.9634565764544));
#168672=CARTESIAN_POINT('Ctrl Pts',(66.6180849498278,8.02372293234134,56.8613030623954));
#168673=CARTESIAN_POINT('Ctrl Pts',(66.9773936236622,8.28408060060196,56.7919794088639));
#168674=CARTESIAN_POINT('Ctrl Pts',(67.5417517737355,8.63728005446337,56.6839593586341));
#168675=CARTESIAN_POINT('Ctrl Pts',(67.7346571205685,8.74901195980444,56.6471710870525));
#168676=CARTESIAN_POINT('Ctrl Pts',(68.0628420757879,8.9243694772397,56.584867931222));
#168677=CARTESIAN_POINT('Ctrl Pts',(68.1961067401817,8.99168665148801,56.5596432026462));
#168678=CARTESIAN_POINT('Ctrl Pts',(68.3844413331462,9.08144787319946,56.5241048839485));
#168679=CARTESIAN_POINT('Ctrl Pts',(68.4382747804767,9.10650320417762,56.5139589210525));
#168680=CARTESIAN_POINT('Ctrl Pts',(68.5309071191952,9.14858921091658,56.4965217049131));
#168681=CARTESIAN_POINT('Ctrl Pts',(68.5695964083469,9.16586300794149,56.4892450483959));
#168682=CARTESIAN_POINT('Ctrl Pts',(68.6436243857457,9.19833617415454,56.4753338204177));
#168683=CARTESIAN_POINT('Ctrl Pts',(68.6789432314978,9.21357990657319,56.4687018850815));
#168684=CARTESIAN_POINT('Ctrl Pts',(68.7618213270094,9.24876839856928,56.4531515140686));
#168685=CARTESIAN_POINT('Ctrl Pts',(68.8094492540546,9.26854449865722,56.4442242470775));
#168686=CARTESIAN_POINT('Ctrl Pts',(68.9505298397407,9.3258120072773,56.4178069543346));
#168687=CARTESIAN_POINT('Ctrl Pts',(69.0444016918334,9.36222751951755,56.4002636867578));
#168688=CARTESIAN_POINT('Ctrl Pts',(69.6558047166414,9.58853688578623,56.2862105400082));
#168689=CARTESIAN_POINT('Ctrl Pts',(70.1878539477727,9.73541835626262,56.1879955390148));
#168690=CARTESIAN_POINT('Ctrl Pts',(71.0320428635474,9.89268614298055,56.0324454695225));
#168691=CARTESIAN_POINT('Ctrl Pts',(71.3373159597415,9.93461146318714,55.976235148332));
#168692=CARTESIAN_POINT('Ctrl Pts',(71.8549439080666,9.98068700579617,55.8805567207322));
#168693=CARTESIAN_POINT('Ctrl Pts',(72.0664301929503,9.99253060617768,55.8413614375923));
#168694=CARTESIAN_POINT('Ctrl Pts',(72.3215090850681,9.99842424619325,55.7938407554123));
#168695=CARTESIAN_POINT('Ctrl Pts',(72.3649323706168,9.99913479020319,55.7857424549098));
#168696=CARTESIAN_POINT('Ctrl Pts',(72.432887762073,9.99978867791876,55.773054049421));
#168697=CARTESIAN_POINT('Ctrl Pts',(72.4574186235897,9.99993131373539,55.7684706799752));
#168698=CARTESIAN_POINT('Ctrl Pts',(72.503480422669,10.0000237508442,55.7598584095973));
#168699=CARTESIAN_POINT('Ctrl Pts',(72.5250111295909,9.99999499713105,55.7558302577256));
#168700=CARTESIAN_POINT('Ctrl Pts',(72.5748484602827,9.99976186526923,55.7465005807097));
#168701=CARTESIAN_POINT('Ctrl Pts',(72.6031543088402,9.9995050533136,55.7411974382303));
#168702=CARTESIAN_POINT('Ctrl Pts',(72.6953785541948,9.99826296194707,55.7239061389232));
#168703=CARTESIAN_POINT('Ctrl Pts',(72.7592857387396,9.99676768883518,55.7119037916169));
#168704=CARTESIAN_POINT('Ctrl Pts',(73.3631586405893,9.97663930622508,55.5983249562949));
#168705=CARTESIAN_POINT('Ctrl Pts',(73.9005638115575,9.91336745251767,55.4960442035739));
#168706=CARTESIAN_POINT('Ctrl Pts',(74.8768633421158,9.71444707239684,55.3104137122434));
#168707=CARTESIAN_POINT('Ctrl Pts',(75.3168347738604,9.59191334476979,55.2268252740692));
#168708=CARTESIAN_POINT('Ctrl Pts',(75.8784107693279,9.39192944166182,55.1206954970908));
#168709=CARTESIAN_POINT('Ctrl Pts',(76.0088951657422,9.34227184804425,55.0960739058512));
#168710=CARTESIAN_POINT('Ctrl Pts',(76.1920017064751,9.26803976442981,55.0615802157063));
#168711=CARTESIAN_POINT('Ctrl Pts',(76.2455092857734,9.24578954932307,55.0515074266961));
#168712=CARTESIAN_POINT('Ctrl Pts',(76.3375595192426,9.20654510345283,55.0341910332881));
#168713=CARTESIAN_POINT('Ctrl Pts',(76.3761931414785,9.18977740701081,55.0269270096716));
#168714=CARTESIAN_POINT('Ctrl Pts',(76.4549500204118,9.15498724871514,55.0121263329532));
#168715=CARTESIAN_POINT('Ctrl Pts',(76.4950627966062,9.13694247373873,55.0045919800011));
#168716=CARTESIAN_POINT('Ctrl Pts',(76.5963392560234,9.09055694127447,54.9855791726483));
#168717=CARTESIAN_POINT('Ctrl Pts',(76.6573393682436,9.06184997572337,54.9741367081107));
#168718=CARTESIAN_POINT('Ctrl Pts',(76.8922677544153,8.94830404035076,54.9301022631335));
#168719=CARTESIAN_POINT('Ctrl Pts',(77.0640274530913,8.85890034629599,54.8979810422508));
#168720=CARTESIAN_POINT('Ctrl Pts',(77.7374145588659,8.48257388663896,54.7722555659475));
#168721=CARTESIAN_POINT('Ctrl Pts',(78.2165102188141,8.15624541629679,54.6833471087575));
#168722=CARTESIAN_POINT('Ctrl Pts',(78.8583656904486,7.63052641390902,54.5632065506372));
#168723=CARTESIAN_POINT('Ctrl Pts',(79.046052664912,7.46445221040781,54.5279196865509));
#168724=CARTESIAN_POINT('Ctrl Pts',(79.2720183543039,7.24859130049152,54.4850424021632));
#168725=CARTESIAN_POINT('Ctrl Pts',(79.3163468927372,7.20543995417531,54.4766109761941));
#168726=CARTESIAN_POINT('Ctrl Pts',(79.3813404360577,7.14096981854607,54.4642153545348));
#168727=CARTESIAN_POINT('Ctrl Pts',(79.4023160899213,7.11997437835274,54.4602095796631));
#168728=CARTESIAN_POINT('Ctrl Pts',(79.4380331741083,7.08389931134314,54.4533790352111));
#168729=CARTESIAN_POINT('Ctrl Pts',(79.4528209754574,7.06886716787826,54.4505481602838));
#168730=CARTESIAN_POINT('Ctrl Pts',(79.4866531021275,7.03425466352652,54.4440649164889));
#168731=CARTESIAN_POINT('Ctrl Pts',(79.5056648237274,7.01464210125918,54.4404168734037));
#168732=CARTESIAN_POINT('Ctrl Pts',(79.5584179895339,6.95976763582236,54.4302814492293));
#168733=CARTESIAN_POINT('Ctrl Pts',(79.591981875593,6.92433171153357,54.4238179607748));
#168734=CARTESIAN_POINT('Ctrl Pts',(79.7965638588489,6.70510676467176,54.3843360198296));
#168735=CARTESIAN_POINT('Ctrl Pts',(79.9608722737452,6.51501149895175,54.3522593994892));
#168736=CARTESIAN_POINT('Ctrl Pts',(80.3920840311058,5.97604670194941,54.2674208018115));
#168737=CARTESIAN_POINT('Ctrl Pts',(80.6435519136396,5.61516681638907,54.2172019806512));
#168738=CARTESIAN_POINT('Ctrl Pts',(80.9869306171769,5.04581875844861,54.1482215178834));
#168739=CARTESIAN_POINT('Ctrl Pts',(81.0966814315515,4.84916834120332,54.1260910013853));
#168740=CARTESIAN_POINT('Ctrl Pts',(81.2688703318115,4.51471138620182,54.0912877876397));
#168741=CARTESIAN_POINT('Ctrl Pts',(81.3349463909953,4.37894758611579,54.0779082500981));
#168742=CARTESIAN_POINT('Ctrl Pts',(81.4230269647992,4.18713452960784,54.0600452865403));
#168743=CARTESIAN_POINT('Ctrl Pts',(81.4476006259695,4.13233514418333,54.0550583321794));
#168744=CARTESIAN_POINT('Ctrl Pts',(81.4888710938237,4.0380560613389,54.0466772699457));
#168745=CARTESIAN_POINT('Ctrl Pts',(81.5058068628168,3.99868699687575,54.0432362906741));
#168746=CARTESIAN_POINT('Ctrl Pts',(81.5376405790069,3.92336838247913,54.0367650370375));
#168747=CARTESIAN_POINT('Ctrl Pts',(81.5525821689485,3.88743887624623,54.0337262026295));
#168748=CARTESIAN_POINT('Ctrl Pts',(81.5870677441897,3.80314194692011,54.026708965883));
#168749=CARTESIAN_POINT('Ctrl Pts',(81.606446418411,3.75470544911803,54.0227629862458));
#168750=CARTESIAN_POINT('Ctrl Pts',(81.6720075827761,3.58708508545596,54.009403032506));
#168751=CARTESIAN_POINT('Ctrl Pts',(81.7163138801765,3.46715189529537,54.0003566798016));
#168752=CARTESIAN_POINT('Ctrl Pts',(81.9773108514265,2.71722016719636,53.9469288886632));
#168753=CARTESIAN_POINT('Ctrl Pts',(82.1338896365648,2.06726251322121,53.9143836481774));
#168754=CARTESIAN_POINT('Ctrl Pts',(82.2344304824298,1.34153292801883,53.8909616529434));
#168755=CARTESIAN_POINT('Ctrl Pts',(82.2427713639767,1.27671987125436,53.8889794911566));
#168756=CARTESIAN_POINT('Ctrl Pts',(82.276435657896,0.993503955104589,53.8807856555322));
#168757=CARTESIAN_POINT('Ctrl Pts',(82.295274739677,0.774361204337858,53.8756581196813));
#168758=CARTESIAN_POINT('Ctrl Pts',(82.3134708763828,0.432230905625216,
53.8693838702499));
#168759=CARTESIAN_POINT('Ctrl Pts',(82.3177570761235,0.309589852688239,
53.8674796615034));
#168760=CARTESIAN_POINT('Ctrl Pts',(82.3204274156931,0.149804214836417,
53.8654232416804));
#168761=CARTESIAN_POINT('Ctrl Pts',(82.3208429435044,0.112708087748638,
53.8649755926801));
#168762=CARTESIAN_POINT('Ctrl Pts',(82.3211871020456,0.0522133541867403,
53.8642932656695));
#168763=CARTESIAN_POINT('Ctrl Pts',(82.3212388760676,0.0288160074678149,
53.8640409935312));
#168764=CARTESIAN_POINT('Ctrl Pts',(82.3211811147386,-0.0168691787927078,
53.8635708552276));
#168765=CARTESIAN_POINT('Ctrl Pts',(82.3210791109962,-0.0391568177109596,
53.8633519112301));
#168766=CARTESIAN_POINT('Ctrl Pts',(82.3206852278142,-0.0890897477102007,
53.8628849579976));
#168767=CARTESIAN_POINT('Ctrl Pts',(82.3203535939649,-0.116734644783884,
53.8626426208118));
#168768=CARTESIAN_POINT('Ctrl Pts',(82.3187874928748,-0.213988775421065,
53.861847756271));
#168769=CARTESIAN_POINT('Ctrl Pts',(82.316946778117,-0.283586979177362,
53.8613828887352));
#168770=CARTESIAN_POINT('Ctrl Pts',(82.2991557836885,-0.767177079712734,
53.858897835677));
#168771=CARTESIAN_POINT('Ctrl Pts',(82.2584877935295,-1.17988250602676,
53.8605891197982));
#168772=CARTESIAN_POINT('Ctrl Pts',(82.1342429030406,-1.952558871361,53.872061384823));
#168773=CARTESIAN_POINT('Ctrl Pts',(82.0560162246229,-2.31271928743464,
53.8809158058714));
#168774=CARTESIAN_POINT('Ctrl Pts',(81.9017699440407,-2.87391172108804,
53.900710332764));
#168775=CARTESIAN_POINT('Ctrl Pts',(81.8386107044225,-3.07821613910783,
53.9092122342016));
#168776=CARTESIAN_POINT('Ctrl Pts',(81.721111382259,-3.41968091595709,53.9256720906166));
#168777=CARTESIAN_POINT('Ctrl Pts',(81.6701355540932,-3.55795232191926,
53.9329770022704));
#168778=CARTESIAN_POINT('Ctrl Pts',(81.5943301119312,-3.75053207398994,
53.9440603926201));
#168779=CARTESIAN_POINT('Ctrl Pts',(81.5719971627679,-3.80583035247125,
53.9473498912265));
#168780=CARTESIAN_POINT('Ctrl Pts',(81.532790358566,-3.90049376959742,53.9531654608353));
#168781=CARTESIAN_POINT('Ctrl Pts',(81.5161516705407,-3.93995733472288,
53.9556454338881));
#168782=CARTESIAN_POINT('Ctrl Pts',(81.483856586521,-4.01521730930301,53.9604813694123));
#168783=CARTESIAN_POINT('Ctrl Pts',(81.4682421529381,-4.05103138978655,
53.9628291141898));
#168784=CARTESIAN_POINT('Ctrl Pts',(81.4270320702046,-4.14407865101693,
53.969049873941));
#168785=CARTESIAN_POINT('Ctrl Pts',(81.4011128110954,-4.20116233767831,
53.9729863851572));
#168786=CARTESIAN_POINT('Ctrl Pts',(81.3086324816435,-4.39990860859872,
53.9871125532471));
#168787=CARTESIAN_POINT('Ctrl Pts',(81.239329630631,-4.54023130294979,53.9978397208571));
#168788=CARTESIAN_POINT('Ctrl Pts',(80.8760439399746,-5.2346670113602,54.0546953060607));
#168789=CARTESIAN_POINT('Ctrl Pts',(80.5344537815953,-5.76148972491485,
54.1101734092115));
#168790=CARTESIAN_POINT('Ctrl Pts',(79.9859644901883,-6.45510492963111,
54.1995242663509));
#168791=CARTESIAN_POINT('Ctrl Pts',(79.8178538190413,-6.65149857516524,
54.2269227678547));
#168792=CARTESIAN_POINT('Ctrl Pts',(79.5996556815575,-6.8871536861063,54.2622927574894));
#168793=CARTESIAN_POINT('Ctrl Pts',(79.5565196799058,-6.9328624728543,54.2692762472393));
#168794=CARTESIAN_POINT('Ctrl Pts',(79.4922205496177,-6.99971254116264,
54.2796691103541));
#168795=CARTESIAN_POINT('Ctrl Pts',(79.4713879305112,-7.02117646285454,
54.2830337910988));
#168796=CARTESIAN_POINT('Ctrl Pts',(79.4356553716273,-7.05766004312809,
54.2888001245902));
#168797=CARTESIAN_POINT('Ctrl Pts',(79.4208034451506,-7.07272732810432,
54.2911954217731));
#168798=CARTESIAN_POINT('Ctrl Pts',(79.386696360594,-7.1071080938456,54.2966928072899));
#168799=CARTESIAN_POINT('Ctrl Pts',(79.3674099458245,-7.12638943274464,
54.2997990151119));
#168800=CARTESIAN_POINT('Ctrl Pts',(79.3136539070021,-7.17968955146655,
54.3084507749134));
#168801=CARTESIAN_POINT('Ctrl Pts',(79.2790159480114,-7.2135338331821,54.3140187729977));
#168802=CARTESIAN_POINT('Ctrl Pts',(79.0719423924536,-7.41291726011599,
54.3472720541034));
#168803=CARTESIAN_POINT('Ctrl Pts',(78.8938754519389,-7.57236573321312,
54.3757324256153));
#168804=CARTESIAN_POINT('Ctrl Pts',(78.3618087989894,-8.01520743096129,
54.4607512174312));
#168805=CARTESIAN_POINT('Ctrl Pts',(77.9940960363526,-8.28074318692409,
54.5195051476434));
#168806=CARTESIAN_POINT('Ctrl Pts',(77.4201452423074,-8.63796573448676,
54.6121014683613));
#168807=CARTESIAN_POINT('Ctrl Pts',(77.2265779505194,-8.74950131171391,
54.6434634275847));
#168808=CARTESIAN_POINT('Ctrl Pts',(76.8973138924305,-8.92459729154222,
54.6970927062953));
#168809=CARTESIAN_POINT('Ctrl Pts',(76.7636018757933,-8.99183526526654,
54.71894516354));
#168810=CARTESIAN_POINT('Ctrl Pts',(76.5746385525104,-9.08151251093388,
54.7499368035909));
#168811=CARTESIAN_POINT('Ctrl Pts',(76.5206034625095,-9.10655673823455,
54.7588112586674));
#168812=CARTESIAN_POINT('Ctrl Pts',(76.427619709887,-9.14862977136467,54.77410350098));
#168813=CARTESIAN_POINT('Ctrl Pts',(76.3887788727589,-9.16590134471883,
54.7804975534351));
#168814=CARTESIAN_POINT('Ctrl Pts',(76.3144570255503,-9.19837386356399,
54.7927444144432));
#168815=CARTESIAN_POINT('Ctrl Pts',(76.2789955185052,-9.21361906807648,
54.7985929234747));
#168816=CARTESIAN_POINT('Ctrl Pts',(76.195774683438,-9.24881597525119,54.8123300449534));
#168817=CARTESIAN_POINT('Ctrl Pts',(76.1479477075382,-9.2685987854853,54.8202338683988));
#168818=CARTESIAN_POINT('Ctrl Pts',(76.0062493555896,-9.32590025881121,
54.8436771996773));
#168819=CARTESIAN_POINT('Ctrl Pts',(75.9119651267375,-9.36234106087739,
54.8593102153508));
#168820=CARTESIAN_POINT('Ctrl Pts',(75.3118761807926,-9.58366164047387,
54.9590132520356));
#168821=CARTESIAN_POINT('Ctrl Pts',(74.7925845473,-9.72782934484848,55.0462669218385));
#168822=CARTESIAN_POINT('Ctrl Pts',(74.0644117936631,-9.86642499906641,
55.1688941422367));
#168823=CARTESIAN_POINT('Ctrl Pts',(73.8633764656079,-9.89819553156769,
55.2027692482083));
#168824=CARTESIAN_POINT('Ctrl Pts',(73.4413329594399,-9.95138883419935,
55.2737825627323));
#168825=CARTESIAN_POINT('Ctrl Pts',(73.220287607698,-9.97159664074993,55.3109177917393));
#168826=CARTESIAN_POINT('Ctrl Pts',(72.8760764633516,-9.99122019912003,
55.3684894585483));
#168827=CARTESIAN_POINT('Ctrl Pts',(72.7532945491389,-9.99588891031017,
55.388975041455));
#168828=CARTESIAN_POINT('Ctrl Pts',(72.5936643706124,-9.99893268868906,
55.4155170311351));
#168829=CARTESIAN_POINT('Ctrl Pts',(72.5568768047025,-9.99942547234498,
55.42162744313));
#168830=CARTESIAN_POINT('Ctrl Pts',(72.4969617697601,-9.99988827267009,
55.4315681290353));
#168831=CARTESIAN_POINT('Ctrl Pts',(72.473836281552,-9.99998447862849,55.4354022329856));
#168832=CARTESIAN_POINT('Ctrl Pts',(72.4287486002363,-10.0000113655624,
55.4428720045041));
#168833=CARTESIAN_POINT('Ctrl Pts',(72.4067866556855,-9.99995013715283,
55.4465078942291));
#168834=CARTESIAN_POINT('Ctrl Pts',(72.3576527872722,-9.99964687954154,
55.4546366461243));
#168835=CARTESIAN_POINT('Ctrl Pts',(72.3304810170454,-9.99936540541892,
55.4591281662376));
#168836=CARTESIAN_POINT('Ctrl Pts',(72.236069194814,-9.99799207134238,55.4747220460726));
#168837=CARTESIAN_POINT('Ctrl Pts',(72.168836279222,-9.99631730448874,55.4858048194902));
#168838=CARTESIAN_POINT('Ctrl Pts',(71.6332099388321,-9.97742156908948,
55.5739475648411));
#168839=CARTESIAN_POINT('Ctrl Pts',(71.1664022631159,-9.92709917372414,
55.649874924514));
#168840=CARTESIAN_POINT('Ctrl Pts',(70.2990500426836,-9.76972412554119,
55.7908978432573));
#168841=CARTESIAN_POINT('Ctrl Pts',(69.8981505391108,-9.67039968655334,
55.8560566156195));
#168842=CARTESIAN_POINT('Ctrl Pts',(69.360426388242,-9.50038366337385,55.9438648269308));
#168843=CARTESIAN_POINT('Ctrl Pts',(69.2173034382342,-9.45144975200689,
55.9672747092599));
#168844=CARTESIAN_POINT('Ctrl Pts',(68.9688955928456,-9.36002750779578,
56.0079846396261));
#168845=CARTESIAN_POINT('Ctrl Pts',(68.863116536288,-9.31899384159476,56.025345613222));
#168846=CARTESIAN_POINT('Ctrl Pts',(68.7084819839311,-9.25589200635337,
56.0507639611599));
#168847=CARTESIAN_POINT('Ctrl Pts',(68.6590658553943,-9.23525193677671,
56.0588927447682));
#168848=CARTESIAN_POINT('Ctrl Pts',(68.571604027354,-9.19787496467867,56.0732903662859));
#168849=CARTESIAN_POINT('Ctrl Pts',(68.5334920325762,-9.18129991243966,
56.0795677664839));
#168850=CARTESIAN_POINT('Ctrl Pts',(68.4534208575969,-9.14586866114537,
56.092763620191));
#168851=CARTESIAN_POINT('Ctrl Pts',(68.4114862316701,-9.12695825300877,
56.0996788183473));
#168852=CARTESIAN_POINT('Ctrl Pts',(68.3003198882863,-9.07588229154613,
56.1180217880321));
#168853=CARTESIAN_POINT('Ctrl Pts',(68.2313240728367,-9.04319972476277,
56.1294180387994));
#168854=CARTESIAN_POINT('Ctrl Pts',(67.90868660651,-8.88572754178351,56.1827600856701));
#168855=CARTESIAN_POINT('Ctrl Pts',(67.6600492701548,-8.75076564379417,
56.2240219958622));
#168856=CARTESIAN_POINT('Ctrl Pts',(67.3490278159051,-8.5641259941554,56.2757336587115));
#168857=CARTESIAN_POINT('Ctrl Pts',(67.281081731324,-8.52221891537737,56.2870364344169));
#168858=CARTESIAN_POINT('Ctrl Pts',(66.8475450273114,-8.24748818106823,
56.3591748668246));
#168859=CARTESIAN_POINT('Ctrl Pts',(66.4968897155404,-7.9913824010402,56.4176380260284));
#168860=CARTESIAN_POINT('Ctrl Pts',(66.1388228350229,-7.69190120586487,
56.4768040865882));
#168861=CARTESIAN_POINT('Ctrl Pts',(66.1139167964462,-7.67086064018072,
56.4809164238193));
#168862=CARTESIAN_POINT('Ctrl Pts',(65.9345674453173,-7.51782555568169,
56.5105048782737));
#168863=CARTESIAN_POINT('Ctrl Pts',(65.784032712273,-7.38117650470982,56.5352075344276));
#168864=CARTESIAN_POINT('Ctrl Pts',(65.604254505522,-7.20765368370613,56.5644391530346));
#168865=CARTESIAN_POINT('Ctrl Pts',(65.5710237318134,-7.17512718210399,
56.5698305674089));
#168866=CARTESIAN_POINT('Ctrl Pts',(65.5189726379127,-7.123461954634,56.5782549195736));
#168867=CARTESIAN_POINT('Ctrl Pts',(65.5000027673707,-7.10448025204775,
56.5813207922665));
#168868=CARTESIAN_POINT('Ctrl Pts',(65.4644883849773,-7.06865608901523,
56.5870519399276));
#168869=CARTESIAN_POINT('Ctrl Pts',(65.4479270456507,-7.05183142572946,
56.5897209315517));
#168870=CARTESIAN_POINT('Ctrl Pts',(65.4090356116518,-7.0120404790486,56.5959802635103));
#168871=CARTESIAN_POINT('Ctrl Pts',(65.386755163371,-6.98902434700317,56.5995596607279));
#168872=CARTESIAN_POINT('Ctrl Pts',(65.3129436490221,-6.91203825063574,
56.6113969656744));
#168873=CARTESIAN_POINT('Ctrl Pts',(65.2618982686334,-6.85758993200706,
56.6195494011052));
#168874=CARTESIAN_POINT('Ctrl Pts',(65.1388223373986,-6.72332668785601,
56.6391321476672));
#168875=CARTESIAN_POINT('Ctrl Pts',(65.0674497246677,-6.64290133226429,
56.6504250103216));
#168876=CARTESIAN_POINT('Ctrl Pts',(64.7757628926427,-6.30334296580469,
56.696356036263));
#168877=CARTESIAN_POINT('Ctrl Pts',(64.567279703089,-6.03403361031762,56.728652476967));
#168878=CARTESIAN_POINT('Ctrl Pts',(64.0898352801356,-5.347693351677,56.8019553473707));
#168879=CARTESIAN_POINT('Ctrl Pts',(63.8371691512065,-4.92014170759687,
56.8401663806758));
#168880=CARTESIAN_POINT('Ctrl Pts',(63.5697093128545,-4.37985868116106,
56.8804099584722));
#168881=CARTESIAN_POINT('Ctrl Pts',(63.5239486482656,-4.28360130353994,
56.8872844017001));
#168882=CARTESIAN_POINT('Ctrl Pts',(63.4579255521113,-4.13883253849201,
56.8971878629492));
#168883=CARTESIAN_POINT('Ctrl Pts',(63.4365041515282,-4.09087068057834,
56.9003985406832));
#168884=CARTESIAN_POINT('Ctrl Pts',(63.3987144393805,-4.00444992785842,
56.9060579923265));
#168885=CARTESIAN_POINT('Ctrl Pts',(63.3822088239391,-3.96605384609136,
56.9085282719715));
#168886=CARTESIAN_POINT('Ctrl Pts',(63.3475157417985,-3.88394384615661,
56.9137169970989));
#168887=CARTESIAN_POINT('Ctrl Pts',(63.3293963000288,-3.84020162926648,
56.9164247921415));
#168888=CARTESIAN_POINT('Ctrl Pts',(63.2810364195707,-3.72108702589698,
56.9236456267113));
#168889=CARTESIAN_POINT('Ctrl Pts',(63.2513960239245,-3.64546930100763,
56.9280646315525));
#168890=CARTESIAN_POINT('Ctrl Pts',(63.0854956548177,-3.2066900231416,56.9527544844642));
#168891=CARTESIAN_POINT('Ctrl Pts',(62.969323373679,-2.83611714315204,56.9698823456802));
#168892=CARTESIAN_POINT('Ctrl Pts',(62.7617540923111,-2.01021801408222,
56.9996293841591));
#168893=CARTESIAN_POINT('Ctrl Pts',(62.6797801102224,-1.55339843102113,
57.0107007668451));
#168894=CARTESIAN_POINT('Ctrl Pts',(62.5986264616137,-0.81308586318316,
57.0190240053952));
#168895=CARTESIAN_POINT('Ctrl Pts',(62.5795904035836,-0.53250455818361,
57.0199893052929));
#168896=CARTESIAN_POINT('Ctrl Pts',(62.5709959477977,-0.207453005027223,
57.0183414650338));
#168897=CARTESIAN_POINT('Ctrl Pts',(62.5701165430882,-0.163395897912248,
57.0180593755872));
#168898=CARTESIAN_POINT('Ctrl Pts',(62.5691510877258,-0.0918065422875012,
57.0175041376516));
#168899=CARTESIAN_POINT('Ctrl Pts',(62.5688911701614,-0.0642769573281793,
57.0172673519341));
#168900=CARTESIAN_POINT('Ctrl Pts',(62.5686764252568,-0.0244979264229797,
57.0168912699599));
#168901=CARTESIAN_POINT('Ctrl Pts',(62.568632333185,-0.0122489680148922,
57.0167708154386));
#168902=CARTESIAN_POINT('Ctrl Pts',(62.5686102705547,6.5620497147992E-11,
57.0166456920447));
#168903=CARTESIAN_POINT('Ctrl Pts',(62.5638890606905,-6.14161654078813E-11,
56.9898703803749));
#168904=CARTESIAN_POINT('Ctrl Pts',(62.5639048106942,-0.00874425629257516,
56.9899597030843));
#168905=CARTESIAN_POINT('Ctrl Pts',(62.5639319241146,-0.0174885217134871,
56.9900474219547));
#168906=CARTESIAN_POINT('Ctrl Pts',(62.5640841001605,-0.0520730401625098,
56.9903879897772));
#168907=CARTESIAN_POINT('Ctrl Pts',(62.5642970225908,-0.0779128924089415,
56.9906283809511));
#168908=CARTESIAN_POINT('Ctrl Pts',(62.5651762302007,-0.15070063633938,
56.9912654398587));
#168909=CARTESIAN_POINT('Ctrl Pts',(62.5660707769559,-0.197645389445814,
56.9916293213419));
#168910=CARTESIAN_POINT('Ctrl Pts',(62.5736186133931,-0.487618141777484,
56.9935805014495));
#168911=CARTESIAN_POINT('Ctrl Pts',(62.5887144581143,-0.730354657305291,
56.9939254030249));
#168912=CARTESIAN_POINT('Ctrl Pts',(62.6602708834771,-1.45741667314123,
56.9907005442943));
#168913=CARTESIAN_POINT('Ctrl Pts',(62.7429552688184,-1.93841296625004,
56.9828230429895));
#168914=CARTESIAN_POINT('Ctrl Pts',(62.9483681114407,-2.77006385693597,
56.957743000169));
#168915=CARTESIAN_POINT('Ctrl Pts',(63.0564139232463,-3.12346042605179,
56.9432843019352));
#168916=CARTESIAN_POINT('Ctrl Pts',(63.2184791926907,-3.56570967861722,
56.9201024405613));
#168917=CARTESIAN_POINT('Ctrl Pts',(63.2549803027769,-3.6608505069661,56.9148064003663));
#168918=CARTESIAN_POINT('Ctrl Pts',(63.3121282485612,-3.80334462471342,
56.9064056031722));
#168919=CARTESIAN_POINT('Ctrl Pts',(63.331717051862,-3.85112708511771,56.9035081504862));
#168920=CARTESIAN_POINT('Ctrl Pts',(63.3677908177045,-3.93723865233663,
56.8981407074137));
#168921=CARTESIAN_POINT('Ctrl Pts',(63.3841494476181,-3.97562091678728,
56.8956954780285));
#168922=CARTESIAN_POINT('Ctrl Pts',(63.4198205618877,-4.05790219711481,
56.8903398536623));
#168923=CARTESIAN_POINT('Ctrl Pts',(63.4392083692609,-4.1017664498802,56.8874146633555));
#168924=CARTESIAN_POINT('Ctrl Pts',(63.4925678346612,-4.22020616114003,
56.8793260952426));
#168925=CARTESIAN_POINT('Ctrl Pts',(63.5271319264544,-4.29450261412776,
56.8740465054666));
#168926=CARTESIAN_POINT('Ctrl Pts',(63.7590275000885,-4.77752680016275,
56.8383760630443));
#168927=CARTESIAN_POINT('Ctrl Pts',(63.9826338898768,-5.17265936184192,
56.8028104026162));
#168928=CARTESIAN_POINT('Ctrl Pts',(64.4547827721841,-5.88924006652601,
56.7265466941171));
#168929=CARTESIAN_POINT('Ctrl Pts',(64.6977265994312,-6.21338701041532,
56.6868723392755));
#168930=CARTESIAN_POINT('Ctrl Pts',(65.0356423656362,-6.61131597155861,
56.6318696549662));
#168931=CARTESIAN_POINT('Ctrl Pts',(65.113356983297,-6.69961181644092,56.6192323398752));
#168932=CARTESIAN_POINT('Ctrl Pts',(65.2463560925697,-6.8454178625359,56.5976524902197));
#168933=CARTESIAN_POINT('Ctrl Pts',(65.3008083608359,-6.90368830470944,
56.588830066336));
#168934=CARTESIAN_POINT('Ctrl Pts',(65.3786909853988,-6.98504357620948,
56.5762367162863));
#168935=CARTESIAN_POINT('Ctrl Pts',(65.401548852792,-7.0086841747057,56.5725436880927));
#168936=CARTESIAN_POINT('Ctrl Pts',(65.4411028926908,-7.04918753222754,
56.5661589571686));
#168937=CARTESIAN_POINT('Ctrl Pts',(65.4577433836709,-7.06610545522635,
56.5634746450491));
#168938=CARTESIAN_POINT('Ctrl Pts',(65.4930300338297,-7.10172363384591,
56.5577864140044));
#168939=CARTESIAN_POINT('Ctrl Pts',(65.5116902391882,-7.12040918973532,
56.554780625295));
#168940=CARTESIAN_POINT('Ctrl Pts',(65.5628939954417,-7.17127433189184,
56.546538332892));
#168941=CARTESIAN_POINT('Ctrl Pts',(65.5955845506883,-7.20330184430556,
56.5412822664836));
#168942=CARTESIAN_POINT('Ctrl Pts',(65.7607424802654,-7.36288330519642,
56.5147536748528));
#168943=CARTESIAN_POINT('Ctrl Pts',(65.8964832888361,-7.48692321207819,
56.4930324849991));
#168944=CARTESIAN_POINT('Ctrl Pts',(66.4009042442753,-7.92274306796178,
56.4123979103522));
#168945=CARTESIAN_POINT('Ctrl Pts',(66.7885361015779,-8.21100398364867,
56.3505541015775));
#168946=CARTESIAN_POINT('Ctrl Pts',(67.5031435033192,-8.66532340663204,
56.2354021021567));
#168947=CARTESIAN_POINT('Ctrl Pts',(67.8214377641631,-8.84371012032256,
56.1837646318747));
#168948=CARTESIAN_POINT('Ctrl Pts',(68.2193241461475,-9.03851891805217,
56.1186290174417));
#168949=CARTESIAN_POINT('Ctrl Pts',(68.2904110854443,-9.07227142317338,
56.1069705707629));
#168950=CARTESIAN_POINT('Ctrl Pts',(68.4041374089743,-9.12460444621562,
56.0882849371297));
#168951=CARTESIAN_POINT('Ctrl Pts',(68.4465240490322,-9.14374564342729,
56.0813131965866));
#168952=CARTESIAN_POINT('Ctrl Pts',(68.5269485355556,-9.17937837010611,
56.0680708893829));
#168953=CARTESIAN_POINT('Ctrl Pts',(68.5649588266528,-9.19593181819053,
56.0618063860581));
#168954=CARTESIAN_POINT('Ctrl Pts',(68.6514798250429,-9.23296110311935,
56.0475334547496));
#168955=CARTESIAN_POINT('Ctrl Pts',(68.7000508742162,-9.25328742867254,
56.03951147355));
#168956=CARTESIAN_POINT('Ctrl Pts',(68.8493684080386,-9.31436638570483,
56.0148216675348));
#168957=CARTESIAN_POINT('Ctrl Pts',(68.950614579436,-9.35382920653745,55.9980408258301));
#168958=CARTESIAN_POINT('Ctrl Pts',(69.6239156277413,-9.60344000676977,
55.8861985455837));
#168959=CARTESIAN_POINT('Ctrl Pts',(70.2132461915203,-9.76124515803727,
55.7870277437451));
#168960=CARTESIAN_POINT('Ctrl Pts',(71.2518707369074,-9.93740617960594,
55.612090530215));
#168961=CARTESIAN_POINT('Ctrl Pts',(71.6950729655319,-9.9816310694202,55.5374264880331));
#168962=CARTESIAN_POINT('Ctrl Pts',(72.1989191972304,-9.9971887668825,55.4534789531029));
#168963=CARTESIAN_POINT('Ctrl Pts',(72.2580211260633,-9.9984747446368,55.4436466337144));
#168964=CARTESIAN_POINT('Ctrl Pts',(72.344917857463,-9.99957344353141,55.4292154920077));
#168965=CARTESIAN_POINT('Ctrl Pts',(72.3727040188649,-9.99980575215838,
55.4246047638297));
#168966=CARTESIAN_POINT('Ctrl Pts',(72.421983935016,-10.000006713663,55.4164345823164));
#168967=CARTESIAN_POINT('Ctrl Pts',(72.4434769586677,-10.0000231723034,
55.4128736532062));
#168968=CARTESIAN_POINT('Ctrl Pts',(72.4903076247572,-9.99990392767021,
55.4051202020519));
#168969=CARTESIAN_POINT('Ctrl Pts',(72.5156450036992,-9.9997404871866,55.4009286412189));
#168970=CARTESIAN_POINT('Ctrl Pts',(72.5866015198404,-9.99900574340614,
55.3891993138661));
#168971=CARTESIAN_POINT('Ctrl Pts',(72.6322189492257,-9.99821268572863,
55.3816690364506));
#168972=CARTESIAN_POINT('Ctrl Pts',(72.9050365506192,-9.99155150476078,
55.3366902802793));
#168973=CARTESIAN_POINT('Ctrl Pts',(73.1320239336223,-9.97805050031943,
55.299500524875));
#168974=CARTESIAN_POINT('Ctrl Pts',(73.8723630421821,-9.90795594389078,
55.1786006524985));
#168975=CARTESIAN_POINT('Ctrl Pts',(74.3819007130795,-9.81851031796833,
55.0959777979692));
#168976=CARTESIAN_POINT('Ctrl Pts',(75.2492126808648,-9.59414504533403,
54.9547787271946));
#168977=CARTESIAN_POINT('Ctrl Pts',(75.6105586599862,-9.47785607708538,
54.8957844722876));
#168978=CARTESIAN_POINT('Ctrl Pts',(76.039138866956,-9.31184736326088,54.8254460527912));
#168979=CARTESIAN_POINT('Ctrl Pts',(76.1135603183451,-9.28196303542946,
54.8132189354172));
#168980=CARTESIAN_POINT('Ctrl Pts',(76.2308611590211,-9.23317719069522,
54.7939259638552));
#168981=CARTESIAN_POINT('Ctrl Pts',(76.2739822738814,-9.21487874247212,
54.786829121736));
#168982=CARTESIAN_POINT('Ctrl Pts',(76.3549685073991,-9.17982407794511,
54.7734920087945));
#168983=CARTESIAN_POINT('Ctrl Pts',(76.3928614109974,-9.16313602837341,
54.7672481484521));
#168984=CARTESIAN_POINT('Ctrl Pts',(76.4782058085163,-9.12490215953699,
54.7531775854325));
#168985=CARTESIAN_POINT('Ctrl Pts',(76.5255945940612,-9.10321640661647,
54.7453591941456));
#168986=CARTESIAN_POINT('Ctrl Pts',(76.6688345474428,-9.0362802123121,54.7217107756027));
#168987=CARTESIAN_POINT('Ctrl Pts',(76.7641363743965,-8.98984686695501,
54.705954640819));
#168988=CARTESIAN_POINT('Ctrl Pts',(77.2461724703858,-8.74523439689092,
54.6261599702734));
#168989=CARTESIAN_POINT('Ctrl Pts',(77.620400450887,-8.52293752160539,54.5638520549711));
#168990=CARTESIAN_POINT('Ctrl Pts',(78.3814407573017,-7.99977242272465,
54.4371933896669));
#168991=CARTESIAN_POINT('Ctrl Pts',(78.7631499228351,-7.69334239791074,
54.3736980258993));
#168992=CARTESIAN_POINT('Ctrl Pts',(79.1833438484766,-7.30170514217075,
54.3050300703362));
#168993=CARTESIAN_POINT('Ctrl Pts',(79.2447723351254,-7.24296442069717,
54.2950260769044));
#168994=CARTESIAN_POINT('Ctrl Pts',(79.3295202093867,-7.15982482882853,
54.2812822949792));
#168995=CARTESIAN_POINT('Ctrl Pts',(79.3534667918142,-7.13609334314239,
54.277405419675));
#168996=CARTESIAN_POINT('Ctrl Pts',(79.3941592448955,-7.09535577787191,
54.2708294768964));
#168997=CARTESIAN_POINT('Ctrl Pts',(79.4109641753367,-7.07841117522327,
54.2681173388886));
#168998=CARTESIAN_POINT('Ctrl Pts',(79.4459815862858,-7.04284874296726,
54.2624736145624));
#168999=CARTESIAN_POINT('Ctrl Pts',(79.4641824196779,-7.02421949107003,
54.2595445691453));
#169000=CARTESIAN_POINT('Ctrl Pts',(79.513008143897,-6.97385198985392,54.2516984130922));
#169001=CARTESIAN_POINT('Ctrl Pts',(79.5434984041737,-6.94197945022565,
54.2468108204876));
#169002=CARTESIAN_POINT('Ctrl Pts',(79.6861602446116,-6.79085968815471,
54.2239955429386));
#169003=CARTESIAN_POINT('Ctrl Pts',(79.7956455858884,-6.66902459748612,
54.2066429991632));
#169004=CARTESIAN_POINT('Ctrl Pts',(80.2267826464556,-6.16487688083918,
54.1387986603288));
#169005=CARTESIAN_POINT('Ctrl Pts',(80.5229187285858,-5.76103577948711,
54.0933115275005));
#169006=CARTESIAN_POINT('Ctrl Pts',(80.9859758920753,-5.01893562440335,
54.0228232777364));
#169007=CARTESIAN_POINT('Ctrl Pts',(81.1662796979998,-4.6904340730106,53.9956134771049));
#169008=CARTESIAN_POINT('Ctrl Pts',(81.3622967684329,-4.28055019252815,
53.966158591484));
#169009=CARTESIAN_POINT('Ctrl Pts',(81.395833003133,-4.2082274332321,53.961125131984));
#169010=CARTESIAN_POINT('Ctrl Pts',(81.4477768954247,-4.09262701861121,
53.9533378873362));
#169011=CARTESIAN_POINT('Ctrl Pts',(81.4667446710304,-4.049610798616,53.9504963383642));
#169012=CARTESIAN_POINT('Ctrl Pts',(81.5020247955879,-3.96805749591278,
53.9452149160665));
#169013=CARTESIAN_POINT('Ctrl Pts',(81.518399363777,-3.92954906842659,53.9427652968102));
#169014=CARTESIAN_POINT('Ctrl Pts',(81.5549902306172,-3.84198567105462,
53.9372951733079));
#169015=CARTESIAN_POINT('Ctrl Pts',(81.5750603612961,-3.79286957566594,
53.9342975599772));
#169016=CARTESIAN_POINT('Ctrl Pts',(81.6352357774534,-3.64221830543486,
53.9253188579434));
#169017=CARTESIAN_POINT('Ctrl Pts',(81.6740835041807,-3.54017802959526,
53.9195349312583));
#169018=CARTESIAN_POINT('Ctrl Pts',(81.9237696760773,-2.85086037712017,
53.882460478916));
#169019=CARTESIAN_POINT('Ctrl Pts',(82.0814713195126,-2.2453733369779,53.8594438534479));
#169020=CARTESIAN_POINT('Ctrl Pts',(82.256746478396,-1.17615855835889,53.8368639699584));
#169021=CARTESIAN_POINT('Ctrl Pts',(82.3001946479318,-0.71871137215977,
53.8327602561505));
#169022=CARTESIAN_POINT('Ctrl Pts',(82.3140815183159,-0.209373276771355,
53.835255984522));
#169023=CARTESIAN_POINT('Ctrl Pts',(82.3150838110856,-0.158830585887076,
53.8355808789653));
#169024=CARTESIAN_POINT('Ctrl Pts',(82.3160370752743,-0.0819760675386363,
53.8361943511674));
#169025=CARTESIAN_POINT('Ctrl Pts',(82.3162617093688,-0.0556680090297576,
53.8364256253505));
#169026=CARTESIAN_POINT('Ctrl Pts',(82.3164863334048,-0.00762243364845737,
53.8368871971331));
#169027=CARTESIAN_POINT('Ctrl Pts',(82.3165185791312,0.0141146339893455,
53.8371107070966));
#169028=CARTESIAN_POINT('Ctrl Pts',(82.3164346784136,0.063224861308948,
53.837648825507));
#169029=CARTESIAN_POINT('Ctrl Pts',(82.3162778802675,0.0905975249978633,
53.8379719860563));
#169030=CARTESIAN_POINT('Ctrl Pts',(82.3155865374829,0.161507002415424,
53.8388687996983));
#169031=CARTESIAN_POINT('Ctrl Pts',(82.314883587652,0.205041158632895,53.8394776570823));
#169032=CARTESIAN_POINT('Ctrl Pts',(82.3079889008431,0.510802990607056,
53.8441577376328));
#169033=CARTESIAN_POINT('Ctrl Pts',(82.2919674719939,0.772677712118657,
53.8502504859091));
#169034=CARTESIAN_POINT('Ctrl Pts',(82.2177367663576,1.51415398010765,53.8729831907986));
#169035=CARTESIAN_POINT('Ctrl Pts',(82.135457198763,1.99047392445941,53.8941270711762));
#169036=CARTESIAN_POINT('Ctrl Pts',(81.9262807030074,2.83553129188075,53.9423026425108));
#169037=CARTESIAN_POINT('Ctrl Pts',(81.8114387948367,3.20636697051633,53.9673391598683));
#169038=CARTESIAN_POINT('Ctrl Pts',(81.6471251739613,3.64541629284319,54.0016021234051));
#169039=CARTESIAN_POINT('Ctrl Pts',(81.6177722627172,3.72104582720717,54.0076758855493));
#169040=CARTESIAN_POINT('Ctrl Pts',(81.5698686599173,3.84017489669624,54.0175160569567));
#169041=CARTESIAN_POINT('Ctrl Pts',(81.5519183455955,3.88391965542935,54.021188325486));
#169042=CARTESIAN_POINT('Ctrl Pts',(81.5175446855735,3.96603189838918,54.0281927897874));
#169043=CARTESIAN_POINT('Ctrl Pts',(81.5011894137835,4.00442767400094,54.0315143061468));
#169044=CARTESIAN_POINT('Ctrl Pts',(81.4637405211422,4.09084432015889,54.0390947269212));
#169045=CARTESIAN_POINT('Ctrl Pts',(81.4425096293239,4.13880245320339,54.0433751099671));
#169046=CARTESIAN_POINT('Ctrl Pts',(81.3770694274902,4.28354766761194,54.0565180611151));
#169047=CARTESIAN_POINT('Ctrl Pts',(81.3317015292353,4.37978590023679,54.0655621495879));
#169048=CARTESIAN_POINT('Ctrl Pts',(81.0663475117984,4.92020669174828,54.1181058290861));
#169049=CARTESIAN_POINT('Ctrl Pts',(80.8153664984999,5.34790961034214,54.1664424600943));
#169050=CARTESIAN_POINT('Ctrl Pts',(80.340863807801,6.03429225825351,54.2568583282166));
#169051=CARTESIAN_POINT('Ctrl Pts',(80.1336697962211,6.30350740048645,54.2961101599799));
#169052=CARTESIAN_POINT('Ctrl Pts',(79.8436844595481,6.64296231786595,54.3512072844235));
#169053=CARTESIAN_POINT('Ctrl Pts',(79.7727129014199,6.72337284533554,54.3647040892111));
#169054=CARTESIAN_POINT('Ctrl Pts',(79.650315335197,6.85761401006886,54.3880221602967));
#169055=CARTESIAN_POINT('Ctrl Pts',(79.5995467102453,6.91205498687755,54.3977057535891));
#169056=CARTESIAN_POINT('Ctrl Pts',(79.5261295227144,6.98903240629104,54.4117319905841));
#169057=CARTESIAN_POINT('Ctrl Pts',(79.5039662296407,7.01204730899201,54.415969143727));
#169058=CARTESIAN_POINT('Ctrl Pts',(79.4652776506389,7.05183683794212,54.4233711958869));
#169059=CARTESIAN_POINT('Ctrl Pts',(79.4488019709314,7.06866133000351,54.4265251517593));
#169060=CARTESIAN_POINT('Ctrl Pts',(79.4134698112614,7.10448596620821,54.4332927672804));
#169061=CARTESIAN_POINT('Ctrl Pts',(79.3945965053637,7.12346829623868,54.4369101356577));
#169062=CARTESIAN_POINT('Ctrl Pts',(79.3428075179754,7.1751370199094,54.4468421140114));
#169063=CARTESIAN_POINT('Ctrl Pts',(79.3097423312075,7.20766626817661,54.4531896283703));
#169064=CARTESIAN_POINT('Ctrl Pts',(79.1308126585927,7.38124353577852,54.4875672255652));
#169065=CARTESIAN_POINT('Ctrl Pts',(78.9809592267362,7.5179392764787,54.5164585031576));
#169066=CARTESIAN_POINT('Ctrl Pts',(78.7659132462544,7.70230324834318,54.5579463371169));
#169067=CARTESIAN_POINT('Ctrl Pts',(78.7041060083003,7.75399196895421,54.5698736847609));
#169068=CARTESIAN_POINT('Ctrl Pts',(78.3651033906683,8.03050374358188,54.6352864840647));
#169069=CARTESIAN_POINT('Ctrl Pts',(78.0767261091754,8.24069103972816,54.690895673929));
#169070=CARTESIAN_POINT('Ctrl Pts',(77.4559767767363,8.6432051992923,54.8099060922709));
#169071=CARTESIAN_POINT('Ctrl Pts',(77.1224530774971,8.83260080551398,54.8734731198974));
#169072=CARTESIAN_POINT('Ctrl Pts',(76.7077133980001,9.03679804891313,54.9518660116191));
#169073=CARTESIAN_POINT('Ctrl Pts',(76.6361534303869,9.0709509493595,54.965370282055));
#169074=CARTESIAN_POINT('Ctrl Pts',(76.5219475383449,9.12375354817043,54.9868873388191));
#169075=CARTESIAN_POINT('Ctrl Pts',(76.4795658829586,9.14298064343171,54.9948647314446));
#169076=CARTESIAN_POINT('Ctrl Pts',(76.3993259076638,9.17869067788625,55.0099538449014));
#169077=CARTESIAN_POINT('Ctrl Pts',(76.3614967980352,9.19523835344236,55.0170616746659));
#169078=CARTESIAN_POINT('Ctrl Pts',(76.2756299004896,9.2321495804909,55.0331821347635));
#169079=CARTESIAN_POINT('Ctrl Pts',(76.227532501316,9.25236785124801,55.0422024450543));
#169080=CARTESIAN_POINT('Ctrl Pts',(76.0805651359703,9.3127595752547,55.069736909107));
#169081=CARTESIAN_POINT('Ctrl Pts',(75.9812043418301,9.35168845087595,55.0883135700301));
#169082=CARTESIAN_POINT('Ctrl Pts',(75.2931596348921,9.60826605919751,55.2167002413699));
#169083=CARTESIAN_POINT('Ctrl Pts',(74.6855912582973,9.76989317578111,55.3286928604313));
#169084=CARTESIAN_POINT('Ctrl Pts',(73.6321391316903,9.94318768375844,55.522789014864));
#169085=CARTESIAN_POINT('Ctrl Pts',(73.1930053790114,9.98493428019243,55.6037117635221));
#169086=CARTESIAN_POINT('Ctrl Pts',(72.7029467250109,9.9979256930175,55.694960163832));
#169087=CARTESIAN_POINT('Ctrl Pts',(72.6531315046462,9.99886095488647,55.7042467602897));
#169088=CARTESIAN_POINT('Ctrl Pts',(72.5774259419976,9.99969682257542,55.7183787647901));
#169089=CARTESIAN_POINT('Ctrl Pts',(72.5515377852804,9.99987862366171,55.7232146832859));
#169090=CARTESIAN_POINT('Ctrl Pts',(72.5042828402994,10.0000205845329,55.7320484211217));
#169091=CARTESIAN_POINT('Ctrl Pts',(72.4829163066571,10.0000139057263,55.7360450880897));
#169092=CARTESIAN_POINT('Ctrl Pts',(72.4346726634354,9.99983880914977,55.7450747031514));
#169093=CARTESIAN_POINT('Ctrl Pts',(72.4077962778869,9.99962911452292,55.7501088994363));
#169094=CARTESIAN_POINT('Ctrl Pts',(72.3382258937914,9.99879598271771,55.7631494480421));
#169095=CARTESIAN_POINT('Ctrl Pts',(72.2955354281879,9.99800165579471,55.7711606540961));
#169096=CARTESIAN_POINT('Ctrl Pts',(71.9981023893323,9.99049448649122,55.8270343437193));
#169097=CARTESIAN_POINT('Ctrl Pts',(71.7437457656726,9.97398701442876,55.8751104491177));
#169098=CARTESIAN_POINT('Ctrl Pts',(71.017115524852,9.89786623642907,56.0128432983893));
#169099=CARTESIAN_POINT('Ctrl Pts',(70.5481352206956,9.81338292517933,56.1021881265229));
#169100=CARTESIAN_POINT('Ctrl Pts',(69.7147906404286,9.59883684736049,56.2604668434973));
#169101=CARTESIAN_POINT('Ctrl Pts',(69.3484224369646,9.48090110005274,56.3298824314981));
#169102=CARTESIAN_POINT('Ctrl Pts',(68.914951695536,9.31238457812526,56.4116298632164));
#169103=CARTESIAN_POINT('Ctrl Pts',(68.8405360341388,9.28239052189889,56.4256505178875));
#169104=CARTESIAN_POINT('Ctrl Pts',(68.723348061904,9.23346461477021,56.447708708801));
#169105=CARTESIAN_POINT('Ctrl Pts',(68.680335524265,9.21514227075404,56.4558003620636));
#169106=CARTESIAN_POINT('Ctrl Pts',(68.5996154173579,9.18006900149048,56.470977171782));
#169107=CARTESIAN_POINT('Ctrl Pts',(68.5618800883034,9.16338727445543,56.4780685528012));
#169108=CARTESIAN_POINT('Ctrl Pts',(68.4769738101259,9.1252065933094,56.4940166647823));
#169109=CARTESIAN_POINT('Ctrl Pts',(68.4298639917344,9.10356914712618,56.5028598990496));
#169110=CARTESIAN_POINT('Ctrl Pts',(68.2877655275524,9.03692717279299,56.5295178725263));
#169111=CARTESIAN_POINT('Ctrl Pts',(68.1933114847173,8.9907544385833,56.5472156600384));
#169112=CARTESIAN_POINT('Ctrl Pts',(67.6546182481865,8.71655948243433,56.6480378507247));
#169113=CARTESIAN_POINT('Ctrl Pts',(67.2271018241678,8.45602107943999,56.7275604431778));
#169114=CARTESIAN_POINT('Ctrl Pts',(66.5517277760748,7.9700333942638,56.8534110931146));
#169115=CARTESIAN_POINT('Ctrl Pts',(66.2923705569563,7.76273645738784,56.9018160669044));
#169116=CARTESIAN_POINT('Ctrl Pts',(65.9645120735511,7.47234456209885,56.9635291811305));
#169117=CARTESIAN_POINT('Ctrl Pts',(65.8863336212564,7.40081784720911,56.9782876158395));
#169118=CARTESIAN_POINT('Ctrl Pts',(65.7556739998463,7.27734528441009,57.0030475955759));
#169119=CARTESIAN_POINT('Ctrl Pts',(65.702603167529,7.22605357069181,57.0131318585195));
#169120=CARTESIAN_POINT('Ctrl Pts',(65.6274599925117,7.15177926468331,57.0274558840965));
#169121=CARTESIAN_POINT('Ctrl Pts',(65.6049212325227,7.12928424235837,57.0317582982299));
#169122=CARTESIAN_POINT('Ctrl Pts',(65.5659147023901,7.0899743725922,57.0392153422113));
#169123=CARTESIAN_POINT('Ctrl Pts',(65.5493980458749,7.07320966962676,57.0423764221574));
#169124=CARTESIAN_POINT('Ctrl Pts',(65.5141827325608,7.03720861808358,57.0491239349662));
#169125=CARTESIAN_POINT('Ctrl Pts',(65.4955021198739,7.01795468533027,57.0527079444153));
#169126=CARTESIAN_POINT('Ctrl Pts',(65.4445585189366,6.96501731238261,57.0624941354596));
#169127=CARTESIAN_POINT('Ctrl Pts',(65.41245347542,6.93117891323654,57.0686750931842));
#169128=CARTESIAN_POINT('Ctrl Pts',(65.2388941725803,6.7456338973516,57.1021584877965));
#169129=CARTESIAN_POINT('Ctrl Pts',(65.101948446706,6.58966703048029,57.1288306617375));
#169130=CARTESIAN_POINT('Ctrl Pts',(64.715974954414,6.12119937601435,57.2045269214451));
#169131=CARTESIAN_POINT('Ctrl Pts',(64.4806217066703,5.79761807739396,57.2513563251151));
#169132=CARTESIAN_POINT('Ctrl Pts',(64.0394473529066,5.10750264809855,57.3397137575542));
#169133=CARTESIAN_POINT('Ctrl Pts',(63.8359665871407,4.74035477580107,57.3807975050775));
#169134=CARTESIAN_POINT('Ctrl Pts',(63.6209177553964,4.28775468594752,57.4243679176016));
#169135=CARTESIAN_POINT('Ctrl Pts',(63.5869006210728,4.21386704673098,57.4312662880771));
#169136=CARTESIAN_POINT('Ctrl Pts',(63.5345098509273,4.09634855309728,57.4419001186997));
#169137=CARTESIAN_POINT('Ctrl Pts',(63.5155468574939,4.05299496798558,57.4457511486891));
#169138=CARTESIAN_POINT('Ctrl Pts',(63.4804355900086,3.97116021103539,57.4528855368321));
#169139=CARTESIAN_POINT('Ctrl Pts',(63.4642200661139,3.93271016472813,57.4561820861494));
#169140=CARTESIAN_POINT('Ctrl Pts',(63.4281854864458,3.84576416205288,57.4635116003861));
#169141=CARTESIAN_POINT('Ctrl Pts',(63.408503651082,3.79721041781361,57.4675176448319));
#169142=CARTESIAN_POINT('Ctrl Pts',(63.3501713437566,3.65003093824365,57.4793992832138));
#169143=CARTESIAN_POINT('Ctrl Pts',(63.3126866358481,3.55093299042886,57.4870463754278));
#169144=CARTESIAN_POINT('Ctrl Pts',(63.0121248439304,2.71696932840247,57.5484809650592));
#169145=CARTESIAN_POINT('Ctrl Pts',(62.8329579683888,1.95358456771351,57.5856285162755));
#169146=CARTESIAN_POINT('Ctrl Pts',(62.7095641700797,0.883623259656689,
57.6159490756503));
#169147=CARTESIAN_POINT('Ctrl Pts',(62.6885800130487,0.589144199610154,
57.6221186997156));
#169148=CARTESIAN_POINT('Ctrl Pts',(62.6789394557067,0.236476854729755,
57.627207924134));
#169149=CARTESIAN_POINT('Ctrl Pts',(62.6778570011712,0.178800735331424,
57.6279669991883));
#169150=CARTESIAN_POINT('Ctrl Pts',(62.6769860189733,0.0933820479571085,
57.6289857077668));
#169151=CARTESIAN_POINT('Ctrl Pts',(62.6768174887749,0.0656452109127856,
57.6293000326176));
#169152=CARTESIAN_POINT('Ctrl Pts',(62.6767385858228,0.0252719382420035,
57.6297339172685));
#169153=CARTESIAN_POINT('Ctrl Pts',(62.6767376164588,0.0126359830890657,
57.6298663430741));
#169154=CARTESIAN_POINT('Ctrl Pts',(62.6767603761739,-3.95693523589967E-11,
57.6299954198325));
#169155=CARTESIAN_POINT('Origin',(72.2537026314029,-4.33680868994202E-16,
54.3558290880045));
#169156=CARTESIAN_POINT('',(62.7943529015217,3.0501608000356E-11,58.2968957709606));
#169157=CARTESIAN_POINT('',(62.7896316916575,-2.89921316295001E-11,58.2701204592907));
#169158=CARTESIAN_POINT('',(62.4056251012807,-1.65832766814156E-15,56.0923108646735));
#169159=CARTESIAN_POINT('Ctrl Pts',(62.7943529015217,6.10048743283802E-11,
58.2968957709606));
#169160=CARTESIAN_POINT('Ctrl Pts',(62.7943293344815,0.0130842026143754,
58.2967621156339));
#169161=CARTESIAN_POINT('Ctrl Pts',(62.7943309036955,0.0261683656279026,
58.2966231335219));
#169162=CARTESIAN_POINT('Ctrl Pts',(62.7944147362689,0.0672353263688407,
58.2961702621673));
#169163=CARTESIAN_POINT('Ctrl Pts',(62.7945868500452,0.0952175476144742,
58.2958374185394));
#169164=CARTESIAN_POINT('Ctrl Pts',(62.7954790261329,0.182158258854861,
58.2947285382218));
#169165=CARTESIAN_POINT('Ctrl Pts',(62.7965947593984,0.241110378516977,
58.2938698386951));
#169166=CARTESIAN_POINT('Ctrl Pts',(62.8109561299922,0.761463163301568,
58.2853646196334));
#169167=CARTESIAN_POINT('Ctrl Pts',(62.8549919718124,1.2213647278526,58.2714431684893));
#169168=CARTESIAN_POINT('Ctrl Pts',(63.0289148515734,2.2744655743346,58.2265182963711));
#169169=CARTESIAN_POINT('Ctrl Pts',(63.1810736254434,2.86200269780546,58.191669630014));
#169170=CARTESIAN_POINT('Ctrl Pts',(63.4220714370871,3.53570538406769,58.1409193129469));
#169171=CARTESIAN_POINT('Ctrl Pts',(63.4609455944977,3.63898426690543,58.1328229898742));
#169172=CARTESIAN_POINT('Ctrl Pts',(63.5210776754935,3.79109434510471,58.1204277642212));
#169173=CARTESIAN_POINT('Ctrl Pts',(63.5410417054879,3.84044432826453,58.1163318334652));
#169174=CARTESIAN_POINT('Ctrl Pts',(63.5773843881548,3.92826654711039,58.1089093017307));
#169175=CARTESIAN_POINT('Ctrl Pts',(63.593613513274,3.96680124299856,58.1056061430119));
#169176=CARTESIAN_POINT('Ctrl Pts',(63.6285156588286,4.04824729677221,58.0985261637471));
#169177=CARTESIAN_POINT('Ctrl Pts',(63.6472487224153,4.09113100479396,58.0947399579927));
#169178=CARTESIAN_POINT('Ctrl Pts',(63.698377787519,4.20597898835893,58.0844423272796));
#169179=CARTESIAN_POINT('Ctrl Pts',(63.7313211842534,4.27768812336586,58.077845173602));
#169180=CARTESIAN_POINT('Ctrl Pts',(63.9189449681989,4.67370765463693,58.0404716424053));
#169181=CARTESIAN_POINT('Ctrl Pts',(64.0900305241596,4.98970407511549,58.0071314223973));
#169182=CARTESIAN_POINT('Ctrl Pts',(64.5050712194121,5.6666362814385,57.9273147193814));
#169183=CARTESIAN_POINT('Ctrl Pts',(64.7563347286539,6.02207380364771,57.8796449442551));
#169184=CARTESIAN_POINT('Ctrl Pts',(65.177562157959,6.5423027201162,57.7996877421493));
#169185=CARTESIAN_POINT('Ctrl Pts',(65.3318004113855,6.71957783593003,57.770397640488));
#169186=CARTESIAN_POINT('Ctrl Pts',(65.5249411939834,6.92632376194569,57.7335497497995));
#169187=CARTESIAN_POINT('Ctrl Pts',(65.5580849452905,6.96128937182639,57.7272207167366));
#169188=CARTESIAN_POINT('Ctrl Pts',(65.6103144474867,7.01559409779447,57.7172362668764));
#169189=CARTESIAN_POINT('Ctrl Pts',(65.6292310718141,7.03510161678302,57.713617878005));
#169190=CARTESIAN_POINT('Ctrl Pts',(65.6629829608783,7.06962348767211,57.7071575156229));
#169191=CARTESIAN_POINT('Ctrl Pts',(65.677787053521,7.08466913084751,57.7043224280844));
#169192=CARTESIAN_POINT('Ctrl Pts',(65.7136620417849,7.12089787138151,57.6974486524499));
#169193=CARTESIAN_POINT('Ctrl Pts',(65.7347797384007,7.14203225950021,57.6933995959993));
#169194=CARTESIAN_POINT('Ctrl Pts',(65.8006608754384,7.20737303200271,57.6807597907767));
#169195=CARTESIAN_POINT('Ctrl Pts',(65.8457426192756,7.25124273526741,57.6720992635608));
#169196=CARTESIAN_POINT('Ctrl Pts',(66.0790231114065,7.47396920349584,57.6272398867786));
#169197=CARTESIAN_POINT('Ctrl Pts',(66.273641838713,7.64567789291229,57.5896707955479));
#169198=CARTESIAN_POINT('Ctrl Pts',(66.9852626886022,8.22526528380116,57.4523596920884));
#169199=CARTESIAN_POINT('Ctrl Pts',(67.5354362690946,8.5881803337454,57.346430318815));
#169200=CARTESIAN_POINT('Ctrl Pts',(68.2295637926754,8.95152273838138,57.2148010286963));
#169201=CARTESIAN_POINT('Ctrl Pts',(68.3430123292046,9.00811476097755,57.1933418215872));
#169202=CARTESIAN_POINT('Ctrl Pts',(68.5041284454596,9.0845932463496,57.1629459012025));
#169203=CARTESIAN_POINT('Ctrl Pts',(68.5509168967525,9.10634851806559,57.15412814532));
#169204=CARTESIAN_POINT('Ctrl Pts',(68.6328905672464,9.14367379770937,57.1386956445957));
#169205=CARTESIAN_POINT('Ctrl Pts',(68.6680007905951,9.15940981475496,57.1320908966931));
#169206=CARTESIAN_POINT('Ctrl Pts',(68.7419714211186,9.192036972856,57.1181867589041));
#169207=CARTESIAN_POINT('Ctrl Pts',(68.7808503467378,9.20888312137265,57.1108849831111));
#169208=CARTESIAN_POINT('Ctrl Pts',(68.8744716352097,9.24872420912049,57.0933170042366));
#169209=CARTESIAN_POINT('Ctrl Pts',(68.9293148943754,9.27147192285284,57.0830378198933));
#169210=CARTESIAN_POINT('Ctrl Pts',(69.1222746074005,9.34944268669734,57.0469133533909));
#169211=CARTESIAN_POINT('Ctrl Pts',(69.2614260595878,9.40198714322001,57.0209371562456));
#169212=CARTESIAN_POINT('Ctrl Pts',(69.606914981838,9.52345520121727,56.9566090683839));
#169213=CARTESIAN_POINT('Ctrl Pts',(69.8144426648795,9.58866924081918,56.9181128988772));
#169214=CARTESIAN_POINT('Ctrl Pts',(70.3660865441529,9.74184751387493,56.8160554259573));
#169215=CARTESIAN_POINT('Ctrl Pts',(70.7130834328755,9.81795943782242,56.7521389818632));
#169216=CARTESIAN_POINT('Ctrl Pts',(71.4611692896431,9.93944803065652,56.6143037617848));
#169217=CARTESIAN_POINT('Ctrl Pts',(71.8624991917176,9.97913694636592,56.5403357430162));
#169218=CARTESIAN_POINT('Ctrl Pts',(72.3338195128043,9.99617727907689,56.4527018156264));
#169219=CARTESIAN_POINT('Ctrl Pts',(72.4026881310376,9.99793038223455,56.4398773694351));
#169220=CARTESIAN_POINT('Ctrl Pts',(72.498828970038,9.99934960489475,56.4219420978089));
#169221=CARTESIAN_POINT('Ctrl Pts',(72.5260938234216,9.99963669123889,56.4168521568661));
#169222=CARTESIAN_POINT('Ctrl Pts',(72.5752915408565,9.99994650746719,56.4076607194083));
#169223=CARTESIAN_POINT('Ctrl Pts',(72.597224265041,10.0000099567593,56.4035606085988));
#169224=CARTESIAN_POINT('Ctrl Pts',(72.6421217494904,9.99998698524796,56.3951621072308));
#169225=CARTESIAN_POINT('Ctrl Pts',(72.6650862724819,9.9998933663003,56.3908635256155));
#169226=CARTESIAN_POINT('Ctrl Pts',(72.724358031512,9.99944041524586,56.3797618043508));
#169227=CARTESIAN_POINT('Ctrl Pts',(72.7606632790489,9.99895828896922,56.3729549571492));
#169228=CARTESIAN_POINT('Ctrl Pts',(72.9160861014167,9.99601788440495,56.3437878713826));
#169229=CARTESIAN_POINT('Ctrl Pts',(73.0351460548074,9.99156084653281,56.3213770087204));
#169230=CARTESIAN_POINT('Ctrl Pts',(73.365918175375,9.97304476408488,56.2589742797523));
#169231=CARTESIAN_POINT('Ctrl Pts',(73.5772877629782,9.95421003460366,56.2189377542272));
#169232=CARTESIAN_POINT('Ctrl Pts',(74.5446760547878,9.83577703077049,56.0353602003182));
#169233=CARTESIAN_POINT('Ctrl Pts',(75.2882383596671,9.65380022996709,55.8935469931949));
#169234=CARTESIAN_POINT('Ctrl Pts',(76.1021830207998,9.34939493430575,55.7398984002603));
#169235=CARTESIAN_POINT('Ctrl Pts',(76.1999081944058,9.31103315447107,55.7214730661648));
#169236=CARTESIAN_POINT('Ctrl Pts',(76.3449530058481,9.25137097475403,55.6941602286289));
#169237=CARTESIAN_POINT('Ctrl Pts',(76.3927370477044,9.23126823608833,55.6851678015874));
#169238=CARTESIAN_POINT('Ctrl Pts',(76.4782612750357,9.19448216626113,55.6690830959504));
#169239=CARTESIAN_POINT('Ctrl Pts',(76.5160582416034,9.17793962010214,55.6619780861258));
#169240=CARTESIAN_POINT('Ctrl Pts',(76.5964565489322,9.14214199517785,55.6468723892491));
#169241=CARTESIAN_POINT('Ctrl Pts',(76.6390277839466,9.12281905823337,55.6388783511088));
#169242=CARTESIAN_POINT('Ctrl Pts',(76.7543073810453,9.06949133230654,55.6172429952161));
#169243=CARTESIAN_POINT('Ctrl Pts',(76.8267467978321,9.03489011645201,55.6036607149198));
#169244=CARTESIAN_POINT('Ctrl Pts',(77.2657555781029,8.81850531417105,55.521420489191));
#169245=CARTESIAN_POINT('Ctrl Pts',(77.6213831384325,8.61455960666906,55.4551361083359));
#169246=CARTESIAN_POINT('Ctrl Pts',(78.2850049499963,8.17656555069726,55.3315369244969));
#169247=CARTESIAN_POINT('Ctrl Pts',(78.5940060417588,7.94546023602887,55.2740240934562));
#169248=CARTESIAN_POINT('Ctrl Pts',(79.0606723178237,7.55162368283231,55.1865131385399));
#169249=CARTESIAN_POINT('Ctrl Pts',(79.2275311838521,7.40073428094589,55.1550728350098));
#169250=CARTESIAN_POINT('Ctrl Pts',(79.423277209432,7.21114332310874,55.1178636401614));
#169251=CARTESIAN_POINT('Ctrl Pts',(79.457168511617,7.17783958152459,55.1114088340873));
#169252=CARTESIAN_POINT('Ctrl Pts',(79.5099578575737,7.12520988486224,55.1013333215394));
#169253=CARTESIAN_POINT('Ctrl Pts',(79.5290174159989,7.10605110411441,55.0976911088358));
#169254=CARTESIAN_POINT('Ctrl Pts',(79.5628405344995,7.07177119001523,55.0912192771218));
#169255=CARTESIAN_POINT('Ctrl Pts',(79.5776342189003,7.05668099755745,55.0883856942888));
#169256=CARTESIAN_POINT('Ctrl Pts',(79.6133777293118,7.01998591484583,55.0815324063195));
#169257=CARTESIAN_POINT('Ctrl Pts',(79.6342779798912,6.99833188913727,55.0775192720024));
#169258=CARTESIAN_POINT('Ctrl Pts',(79.6993520310903,6.93029079258811,55.0650067299684));
#169259=CARTESIAN_POINT('Ctrl Pts',(79.7431778854462,6.88356457752861,55.056554470086));
#169260=CARTESIAN_POINT('Ctrl Pts',(79.9691590169313,6.63788276321501,55.012851795521));
#169261=CARTESIAN_POINT('Ctrl Pts',(80.1436651777642,6.43185179817786,54.9786944060639));
#169262=CARTESIAN_POINT('Ctrl Pts',(80.3847360351059,6.12249470125553,54.9311377423839));
#169263=CARTESIAN_POINT('Ctrl Pts',(80.4580475296599,6.02475451610943,54.9166201363671));
#169264=CARTESIAN_POINT('Ctrl Pts',(80.8639746050662,5.46229627324746,54.8359912114885));
#169265=CARTESIAN_POINT('Ctrl Pts',(81.1583945238756,4.97037240264469,54.7766231134293));
#169266=CARTESIAN_POINT('Ctrl Pts',(81.4498591380089,4.37300962317045,54.7176154916836));
#169267=CARTESIAN_POINT('Ctrl Pts',(81.4889241406627,4.29009331337702,54.7096985266908));
#169268=CARTESIAN_POINT('Ctrl Pts',(81.5493853819688,4.15708846364673,54.6974333486501));
#169269=CARTESIAN_POINT('Ctrl Pts',(81.5715111487678,4.10735064173061,54.6929421599415));
#169270=CARTESIAN_POINT('Ctrl Pts',(81.610026113258,4.01884891995319,54.685119365165));
#169271=CARTESIAN_POINT('Ctrl Pts',(81.6265763995364,3.9801594017487,54.681756161049));
#169272=CARTESIAN_POINT('Ctrl Pts',(81.6605962527342,3.89923597663324,54.6748394054917));
#169273=CARTESIAN_POINT('Ctrl Pts',(81.6780222419108,3.85698408309974,54.6712944060832));
#169274=CARTESIAN_POINT('Ctrl Pts',(81.7228403145991,3.7461886805504,54.6621714655065));
#169275=CARTESIAN_POINT('Ctrl Pts',(81.7497716814511,3.6774544648187,54.6566838692268));
#169276=CARTESIAN_POINT('Ctrl Pts',(81.8723984160978,3.3541031237216,54.6316682167266));
#169277=CARTESIAN_POINT('Ctrl Pts',(81.9585948862542,3.0958660756909,54.6140020814812));
#169278=CARTESIAN_POINT('Ctrl Pts',(82.1959543207427,2.27611767193012,54.5648906558562));
#169279=CARTESIAN_POINT('Ctrl Pts',(82.3094081381817,1.70455321714498,54.5407101351508));
#169280=CARTESIAN_POINT('Ctrl Pts',(82.4051349782228,0.836190511055383,
54.5168394758559));
#169281=CARTESIAN_POINT('Ctrl Pts',(82.4245618667854,0.544923089900452,
54.5109457745998));
#169282=CARTESIAN_POINT('Ctrl Pts',(82.4323856717708,0.208842427196565,
54.5062972627666));
#169283=CARTESIAN_POINT('Ctrl Pts',(82.4331260232878,0.164482173895023,
54.5057267287932));
#169284=CARTESIAN_POINT('Ctrl Pts',(82.4338528819693,0.0924989155547868,
54.5048692787617));
#169285=CARTESIAN_POINT('Ctrl Pts',(82.4340184471795,0.0648786374945988,
54.5045565971891));
#169286=CARTESIAN_POINT('Ctrl Pts',(82.4341117519754,0.0155095810496853,
54.50402648799));
#169287=CARTESIAN_POINT('Ctrl Pts',(82.4340825682918,-0.00623873017125077,
54.5038029233805));
#169288=CARTESIAN_POINT('Ctrl Pts',(82.4338637165141,-0.0540865559119959,
54.5033329252075));
#169289=CARTESIAN_POINT('Ctrl Pts',(82.4336431174273,-0.0801856147328861,
54.5030909120679));
#169290=CARTESIAN_POINT('Ctrl Pts',(82.4327104851214,-0.155825802968483,
54.5024316101472));
#169291=CARTESIAN_POINT('Ctrl Pts',(82.4317350194961,-0.205363242757256,
54.5020521751577));
#169292=CARTESIAN_POINT('Ctrl Pts',(82.419855199437,-0.644529275792791,
54.4991629057913));
#169293=CARTESIAN_POINT('Ctrl Pts',(82.3867795976834,-1.03325092763291,
54.4999298655147));
#169294=CARTESIAN_POINT('Ctrl Pts',(82.2347873349296,-2.0926359449325,54.5125266370394));
#169295=CARTESIAN_POINT('Ctrl Pts',(82.0706568649973,-2.75462038157244,
54.5322643312027));
#169296=CARTESIAN_POINT('Ctrl Pts',(81.8016976589154,-3.50690289598401,
54.5704295648089));
#169297=CARTESIAN_POINT('Ctrl Pts',(81.7596171380991,-3.61836617779735,
54.5765050728406));
#169298=CARTESIAN_POINT('Ctrl Pts',(81.6955103624837,-3.77951718314554,
54.5859068210986));
#169299=CARTESIAN_POINT('Ctrl Pts',(81.6750275000285,-3.82982511027735,
54.5889307125001));
#169300=CARTESIAN_POINT('Ctrl Pts',(81.6379481696952,-3.91883890119254,
54.5944393390176));
#169301=CARTESIAN_POINT('Ctrl Pts',(81.6215123252486,-3.9576121617823,54.5968925903749));
#169302=CARTESIAN_POINT('Ctrl Pts',(81.5866749558957,-4.03838963780071,
54.6021160251081));
#169303=CARTESIAN_POINT('Ctrl Pts',(81.5682291437554,-4.08037311971113,
54.6048949145853));
#169304=CARTESIAN_POINT('Ctrl Pts',(81.5191199552964,-4.19011629676324,
54.6123269809385));
#169305=CARTESIAN_POINT('Ctrl Pts',(81.4879960161064,-4.25766057610092,
54.6170705160356));
#169306=CARTESIAN_POINT('Ctrl Pts',(81.3346696993241,-4.58097316062581,
54.6405916395179));
#169307=CARTESIAN_POINT('Ctrl Pts',(81.2025488201186,-4.83174865825036,
54.6613157508934));
#169308=CARTESIAN_POINT('Ctrl Pts',(80.8848337654175,-5.37768182249967,
54.7119100517247));
#169309=CARTESIAN_POINT('Ctrl Pts',(80.6941551282675,-5.66935819423127,
54.7427551495191));
#169310=CARTESIAN_POINT('Ctrl Pts',(80.2677488282208,-6.25281247888802,
54.812092071968));
#169311=CARTESIAN_POINT('Ctrl Pts',(80.030029883529,-6.54241802822165,54.8509324155893));
#169312=CARTESIAN_POINT('Ctrl Pts',(79.729398638128,-6.86918597568535,54.8996853943373));
#169313=CARTESIAN_POINT('Ctrl Pts',(79.6815443567259,-6.92011125200681,
54.9074353950827));
#169314=CARTESIAN_POINT('Ctrl Pts',(79.6117819860961,-6.99279638261426,
54.9187133179158));
#169315=CARTESIAN_POINT('Ctrl Pts',(79.5902995076981,-7.01497071938764,
54.9221835250505));
#169316=CARTESIAN_POINT('Ctrl Pts',(79.5522621372452,-7.0538679235337,54.9283226737659));
#169317=CARTESIAN_POINT('Ctrl Pts',(79.5357502005065,-7.07063327665491,
54.9309859123285));
#169318=CARTESIAN_POINT('Ctrl Pts',(79.5000279104884,-7.10664637834109,
54.9367436990345));
#169319=CARTESIAN_POINT('Ctrl Pts',(79.480798068143,-7.1258738404656,54.939840833986));
#169320=CARTESIAN_POINT('Ctrl Pts',(79.4264072765182,-7.17981212388787,
54.9485948738223));
#169321=CARTESIAN_POINT('Ctrl Pts',(79.3910674668997,-7.21433757931758,
54.9542756243836));
#169322=CARTESIAN_POINT('Ctrl Pts',(79.1418332135287,-7.45421296459466,
54.9942981879214));
#169323=CARTESIAN_POINT('Ctrl Pts',(78.9191750005361,-7.65004089996804,
55.0298477965208));
#169324=CARTESIAN_POINT('Ctrl Pts',(78.5456971516658,-7.94991608812042,
55.0895301929499));
#169325=CARTESIAN_POINT('Ctrl Pts',(78.4000929857515,-8.06033423153442,
55.112809104865));
#169326=CARTESIAN_POINT('Ctrl Pts',(77.8449643651606,-8.45758730772135,
55.2017645334436));
#169327=CARTESIAN_POINT('Ctrl Pts',(77.4172790396777,-8.71700622504059,
55.2707390480504));
#169328=CARTESIAN_POINT('Ctrl Pts',(76.8779988768541,-8.99044595534622,
55.3588337402779));
#169329=CARTESIAN_POINT('Ctrl Pts',(76.782995899608,-9.03670711578353,55.3743908818577));
#169330=CARTESIAN_POINT('Ctrl Pts',(76.6401247635967,-9.10344911357804,
55.3978446687676));
#169331=CARTESIAN_POINT('Ctrl Pts',(76.5927939561801,-9.12510296840012,
55.4056238646237));
#169332=CARTESIAN_POINT('Ctrl Pts',(76.5075136666594,-9.16330172526239,
55.4196571761092));
#169333=CARTESIAN_POINT('Ctrl Pts',(76.4696255856313,-9.17998559055107,
55.4258977602181));
#169334=CARTESIAN_POINT('Ctrl Pts',(76.3886046501467,-9.21505247829252,
55.4392553398522));
#169335=CARTESIAN_POINT('Ctrl Pts',(76.3454441599627,-9.23336666764757,
55.4463785523404));
#169336=CARTESIAN_POINT('Ctrl Pts',(76.2279185402163,-9.28224467637531,
55.4657952017962));
#169337=CARTESIAN_POINT('Ctrl Pts',(76.1533138309441,-9.31220128856702,
55.4781426512809));
#169338=CARTESIAN_POINT('Ctrl Pts',(75.7204713969116,-9.47984949739519,
55.5499021176183));
#169339=CARTESIAN_POINT('Ctrl Pts',(75.3550051431997,-9.59721854715605,
55.6109876179549));
#169340=CARTESIAN_POINT('Ctrl Pts',(74.5475159396625,-9.80500481622996,
55.7465757420032));
#169341=CARTESIAN_POINT('Ctrl Pts',(74.1042568569665,-9.88685085552179,
55.8213983490645));
#169342=CARTESIAN_POINT('Ctrl Pts',(73.3746708383493,-9.96981270256432,
55.9440788354323));
#169343=CARTESIAN_POINT('Ctrl Pts',(73.0910954109453,-9.98953030366832,
55.9916394685481));
#169344=CARTESIAN_POINT('Ctrl Pts',(72.763363819548,-9.99792646581856,56.0461953891899));
#169345=CARTESIAN_POINT('Ctrl Pts',(72.7196999342711,-9.99875100568503,
56.0534554470616));
#169346=CARTESIAN_POINT('Ctrl Pts',(72.6488124556432,-9.99961233763443,
56.065226781678));
#169347=CARTESIAN_POINT('Ctrl Pts',(72.6215925147344,-9.99982886981166,
56.0697431882756));
#169348=CARTESIAN_POINT('Ctrl Pts',(72.5729163586274,-10.0000118731696,
56.0778127469671));
#169349=CARTESIAN_POINT('Ctrl Pts',(72.5514608518911,-10.000021597109,56.0813672247771));
#169350=CARTESIAN_POINT('Ctrl Pts',(72.5042304644808,-9.9998868466809,56.0891863598581));
#169351=CARTESIAN_POINT('Ctrl Pts',(72.478455856296,-9.99971094296779,56.0934499287059));
#169352=CARTESIAN_POINT('Ctrl Pts',(72.40368484573,-9.99890368887334,56.1058087321512));
#169353=CARTESIAN_POINT('Ctrl Pts',(72.3546906263827,-9.99800478995449,
56.1138949369193));
#169354=CARTESIAN_POINT('Ctrl Pts',(71.912449173706,-9.98655110407041,56.1867869673729));
#169355=CARTESIAN_POINT('Ctrl Pts',(71.5200327365673,-9.95254291377877,
56.2507850857573));
#169356=CARTESIAN_POINT('Ctrl Pts',(70.4483325154485,-9.79387743191931,
56.4251780552333));
#169357=CARTESIAN_POINT('Ctrl Pts',(69.7782597175951,-9.6207014238564,56.5339133418886));
#169358=CARTESIAN_POINT('Ctrl Pts',(69.0468560195961,-9.34638531395464,
56.653840627167));
#169359=CARTESIAN_POINT('Ctrl Pts',(68.9624800994791,-9.31339554115896,
56.6676920872827));
#169360=CARTESIAN_POINT('Ctrl Pts',(68.8285955541576,-9.25889269734186,
56.689697977193));
#169361=CARTESIAN_POINT('Ctrl Pts',(68.7787910001814,-9.23813602597271,
56.6978900881166));
#169362=CARTESIAN_POINT('Ctrl Pts',(68.6907696983954,-9.20059472937169,
56.7123788851772));
#169363=CARTESIAN_POINT('Ctrl Pts',(68.6524850944088,-9.18397607802619,
56.7186843296913));
#169364=CARTESIAN_POINT('Ctrl Pts',(68.5728256152086,-9.14879027356494,
56.7318115667791));
#169365=CARTESIAN_POINT('Ctrl Pts',(68.5314707345536,-9.13017931382513,
56.7386307051019));
#169366=CARTESIAN_POINT('Ctrl Pts',(68.4235923858018,-9.08072684503501,
56.7564298077484));
#169367=CARTESIAN_POINT('Ctrl Pts',(68.3572795579069,-9.04942268914026,
56.7673816508158));
#169368=CARTESIAN_POINT('Ctrl Pts',(68.0430277694203,-8.89673768247053,
56.8193296453327));
#169369=CARTESIAN_POINT('Ctrl Pts',(67.7998539091083,-8.76562020034719,
56.8596758587761));
#169370=CARTESIAN_POINT('Ctrl Pts',(66.9445219438104,-8.25676000969842,
57.0018635706515));
#169371=CARTESIAN_POINT('Ctrl Pts',(66.3681103195645,-7.82203377352227,
57.098363879586));
#169372=CARTESIAN_POINT('Ctrl Pts',(65.7902698355847,-7.27840340345619,
57.1926744948112));
#169373=CARTESIAN_POINT('Ctrl Pts',(65.738209353335,-7.22834704256752,57.2011454526931));
#169374=CARTESIAN_POINT('Ctrl Pts',(65.6657388188699,-7.15713548605935,
57.2128949691012));
#169375=CARTESIAN_POINT('Ctrl Pts',(65.6448796484374,-7.13645688375126,
57.216271787124));
#169376=CARTESIAN_POINT('Ctrl Pts',(65.6072517692323,-7.09882403141038,
57.2223535670278));
#169377=CARTESIAN_POINT('Ctrl Pts',(65.5904524614216,-7.08190171507522,
57.225065298698));
#169378=CARTESIAN_POINT('Ctrl Pts',(65.555800035577,-7.0467446771676,57.2306512449039));
#169379=CARTESIAN_POINT('Ctrl Pts',(65.5379557776114,-7.02850129585407,
57.2335235256053));
#169380=CARTESIAN_POINT('Ctrl Pts',(65.4911266166101,-6.98025630619024,
57.2410506583338));
#169381=CARTESIAN_POINT('Ctrl Pts',(65.4622573624889,-6.95013918773834,
57.2456801258759));
#169382=CARTESIAN_POINT('Ctrl Pts',(65.3279843769467,-6.80829484557587,
57.2671643013652));
#169383=CARTESIAN_POINT('Ctrl Pts',(65.2249381522968,-6.69428815491473,
57.28351301364));
#169384=CARTESIAN_POINT('Ctrl Pts',(64.9177665496709,-6.33828239680599,
57.3319147019146));
#169385=CARTESIAN_POINT('Ctrl Pts',(64.7223443702513,-6.08880373248865,
57.3622400323581));
#169386=CARTESIAN_POINT('Ctrl Pts',(64.233832824973,-5.4002286631775,57.4373804728273));
#169387=CARTESIAN_POINT('Ctrl Pts',(63.962819096328,-4.9462924518367,57.478369650224));
#169388=CARTESIAN_POINT('Ctrl Pts',(63.6816093985632,-4.37782800872695,
57.5206809355739));
#169389=CARTESIAN_POINT('Ctrl Pts',(63.63612695229,-4.28210804313245,57.5275134601793));
#169390=CARTESIAN_POINT('Ctrl Pts',(63.5704181624404,-4.1379889507939,57.5373696743691));
#169391=CARTESIAN_POINT('Ctrl Pts',(63.549048462097,-4.0901317839848,57.5405725753773));
#169392=CARTESIAN_POINT('Ctrl Pts',(63.5113156045274,-4.00382490312059,
57.5462234718173));
#169393=CARTESIAN_POINT('Ctrl Pts',(63.4948166842198,-3.96543729475209,
57.5486927316391));
#169394=CARTESIAN_POINT('Ctrl Pts',(63.4601033267713,-3.88326428312749,
57.553884451202));
#169395=CARTESIAN_POINT('Ctrl Pts',(63.4419580261639,-3.83945010877777,
57.556596086404));
#169396=CARTESIAN_POINT('Ctrl Pts',(63.3934465691909,-3.71993188910788,
57.5638394750176));
#169397=CARTESIAN_POINT('Ctrl Pts',(63.3636874357562,-3.64397971588759,
57.568276099263));
#169398=CARTESIAN_POINT('Ctrl Pts',(63.1950020529328,-3.19757304992833,
57.5933796870426));
#169399=CARTESIAN_POINT('Ctrl Pts',(63.0770087644234,-2.81940685612739,
57.6107719970196));
#169400=CARTESIAN_POINT('Ctrl Pts',(62.864374307043,-1.96433397259502,57.641195723081));
#169401=CARTESIAN_POINT('Ctrl Pts',(62.7812741321484,-1.48552760680555,
57.6523290080425));
#169402=CARTESIAN_POINT('Ctrl Pts',(62.7077436067178,-0.754835660743466,
57.6593095160525));
#169403=CARTESIAN_POINT('Ctrl Pts',(62.6919146816398,-0.506288995406827,
57.6599513901734));
#169404=CARTESIAN_POINT('Ctrl Pts',(62.6838799958966,-0.208933603431457,
57.658479443963));
#169405=CARTESIAN_POINT('Ctrl Pts',(62.6829155563255,-0.160440203136994,
57.6581682739325));
#169406=CARTESIAN_POINT('Ctrl Pts',(62.682036687821,-0.0915736068739256,
57.6576237272076));
#169407=CARTESIAN_POINT('Ctrl Pts',(62.6818376927526,-0.0712042632457356,
57.6574499112884));
#169408=CARTESIAN_POINT('Ctrl Pts',(62.6815847637954,-0.0338865066335313,
57.6571079514006));
#169409=CARTESIAN_POINT('Ctrl Pts',(62.6815121129508,-0.0169482591708172,
57.6569438582266));
#169410=CARTESIAN_POINT('Ctrl Pts',(62.6814815860384,1.77731069449741E-12,
57.6567707315033));
#169411=CARTESIAN_POINT('Ctrl Pts',(62.6767603761739,-3.95693523589967E-11,
57.6299954198325));
#169412=CARTESIAN_POINT('Ctrl Pts',(62.6767730501235,-0.00703645950903762,
57.6300672973722));
#169413=CARTESIAN_POINT('Ctrl Pts',(62.6767930822822,-0.0140729276535245,
57.6301381363992));
#169414=CARTESIAN_POINT('Ctrl Pts',(62.6769183030972,-0.0462422506144614,
57.6304572342398));
#169415=CARTESIAN_POINT('Ctrl Pts',(62.6771099999868,-0.0713747770162598,
57.6306932376319));
#169416=CARTESIAN_POINT('Ctrl Pts',(62.6778933222357,-0.140320776548243,
57.6313037681363));
#169417=CARTESIAN_POINT('Ctrl Pts',(62.6786763049084,-0.184131765194433,
57.6316508424258));
#169418=CARTESIAN_POINT('Ctrl Pts',(62.6843188444241,-0.415569757892112,
57.6332640333996));
#169419=CARTESIAN_POINT('Ctrl Pts',(62.6941211343586,-0.603044268526511,
57.6338051878891));
#169420=CARTESIAN_POINT('Ctrl Pts',(62.7549097502567,-1.36086732614974,
57.6326472034358));
#169421=CARTESIAN_POINT('Ctrl Pts',(62.8490070080706,-1.92666111061175,
57.6240183363885));
#169422=CARTESIAN_POINT('Ctrl Pts',(63.0842531293513,-2.8508970654349,57.5948732928638));
#169423=CARTESIAN_POINT('Ctrl Pts',(63.1990431153161,-3.21478480939138,
57.5793227096225));
#169424=CARTESIAN_POINT('Ctrl Pts',(63.3626097339909,-3.64683809530257,
57.5556861018641));
#169425=CARTESIAN_POINT('Ctrl Pts',(63.3921566667552,-3.72214948882659,
57.5513703062038));
#169426=CARTESIAN_POINT('Ctrl Pts',(63.4403925355549,-3.84089455160905,
57.5442538557541));
#169427=CARTESIAN_POINT('Ctrl Pts',(63.4584916697803,-3.88457080459729,
57.5415687923236));
#169428=CARTESIAN_POINT('Ctrl Pts',(63.4931688744478,-3.96662345095016,
57.5363969656386));
#169429=CARTESIAN_POINT('Ctrl Pts',(63.5096803785325,-4.00502768472232,
57.5339232427941));
#169430=CARTESIAN_POINT('Ctrl Pts',(63.5475184818785,-4.0915546575601,57.5282296993175));
#169431=CARTESIAN_POINT('Ctrl Pts',(63.5689828992801,-4.13961397596239,
57.5249828223105));
#169432=CARTESIAN_POINT('Ctrl Pts',(63.6352761143501,-4.28498869449471,
57.514904388037));
#169433=CARTESIAN_POINT('Ctrl Pts',(63.6812708393281,-4.3817478663855,57.5078441781412));
#169434=CARTESIAN_POINT('Ctrl Pts',(63.9435144839838,-4.91153746887167,
57.4672430703019));
#169435=CARTESIAN_POINT('Ctrl Pts',(64.1889419365388,-5.32895121696058,
57.4279643259112));
#169436=CARTESIAN_POINT('Ctrl Pts',(64.5757289448318,-5.88982000550573,
57.3652675553829));
#169437=CARTESIAN_POINT('Ctrl Pts',(64.6930072265174,-6.04952765619241,
57.3461782181847));
#169438=CARTESIAN_POINT('Ctrl Pts',(64.999649469371,-6.44208536917183,57.2962298659326));
#169439=CARTESIAN_POINT('Ctrl Pts',(65.1948499843389,-6.66999768867731,
57.2644001494803));
#169440=CARTESIAN_POINT('Ctrl Pts',(65.4338351124456,-6.92473448219735,
57.2256963327324));
#169441=CARTESIAN_POINT('Ctrl Pts',(65.4679825907577,-6.96059109360578,
57.2201721467679));
#169442=CARTESIAN_POINT('Ctrl Pts',(65.5213116107772,-7.01575626599036,
57.2115561379527));
#169443=CARTESIAN_POINT('Ctrl Pts',(65.540308519357,-7.03524604937448,57.2084891151116));
#169444=CARTESIAN_POINT('Ctrl Pts',(65.5758763149472,-7.07143727984411,
57.2027511984484));
#169445=CARTESIAN_POINT('Ctrl Pts',(65.5924269566033,-7.08815851063107,
57.2000830106152));
#169446=CARTESIAN_POINT('Ctrl Pts',(65.6308083503078,-7.12666035101376,
57.1938994484052));
#169447=CARTESIAN_POINT('Ctrl Pts',(65.6526810550493,-7.14839782912533,
57.1903785321577));
#169448=CARTESIAN_POINT('Ctrl Pts',(65.7243038983775,-7.21891656845933,
57.1788578299424));
#169449=CARTESIAN_POINT('Ctrl Pts',(65.7744626176174,-7.26727090969583,
57.1708031559143));
#169450=CARTESIAN_POINT('Ctrl Pts',(66.0837652592173,-7.55921828299814,
57.121195528919));
#169451=CARTESIAN_POINT('Ctrl Pts',(66.355212885337,-7.78910569840687,57.0779099055449));
#169452=CARTESIAN_POINT('Ctrl Pts',(66.8719892920037,-8.18105325811043,
56.9952505071063));
#169453=CARTESIAN_POINT('Ctrl Pts',(67.1133916303522,-8.34776397214705,
56.9565481634264));
#169454=CARTESIAN_POINT('Ctrl Pts',(67.5564042013422,-8.62543564657457,
56.8851046338728));
#169455=CARTESIAN_POINT('Ctrl Pts',(67.7552235805904,-8.74057935349551,
56.852902466124));
#169456=CARTESIAN_POINT('Ctrl Pts',(68.0899909044745,-8.91913077708268,
56.798386878696));
#169457=CARTESIAN_POINT('Ctrl Pts',(68.2237471176902,-8.98659394378869,
56.7765312617136));
#169458=CARTESIAN_POINT('Ctrl Pts',(68.4142150470329,-9.07726312014421,
56.745298513356));
#169459=CARTESIAN_POINT('Ctrl Pts',(68.4697173717242,-9.10305075499764,
56.7361843887784));
#169460=CARTESIAN_POINT('Ctrl Pts',(68.5640628649491,-9.14581825546213,
56.7206698024296));
#169461=CARTESIAN_POINT('Ctrl Pts',(68.6027852011337,-9.16306992197531,
56.7142959327222));
#169462=CARTESIAN_POINT('Ctrl Pts',(68.6812299869732,-9.19741154696185,
56.7013710800815));
#169463=CARTESIAN_POINT('Ctrl Pts',(68.7209559650063,-9.21449079724056,
56.6948192636759));
#169464=CARTESIAN_POINT('Ctrl Pts',(68.8191397166746,-9.25593565058751,
56.6786105951197));
#169465=CARTESIAN_POINT('Ctrl Pts',(68.8777191853321,-9.27999710972145,
56.6689263726862));
#169466=CARTESIAN_POINT('Ctrl Pts',(69.0997492156598,-9.36869139438358,
56.6321705461046));
#169467=CARTESIAN_POINT('Ctrl Pts',(69.2646475548105,-9.42947187737469,
56.6047695197724));
#169468=CARTESIAN_POINT('Ctrl Pts',(69.6916485949808,-9.57392626757734,
56.5335836406093));
#169469=CARTESIAN_POINT('Ctrl Pts',(69.9557365363162,-9.65101383200898,
56.4893352656871));
#169470=CARTESIAN_POINT('Ctrl Pts',(70.8356014495849,-9.86796891442351,
56.3414929518335));
#169471=CARTESIAN_POINT('Ctrl Pts',(71.4613113241799,-9.9591250245189,56.2356092294406));
#169472=CARTESIAN_POINT('Ctrl Pts',(72.1876940817472,-9.99361605449846,
56.1142743013188));
#169473=CARTESIAN_POINT('Ctrl Pts',(72.283925344515,-9.99675471409284,56.0982338824842));
#169474=CARTESIAN_POINT('Ctrl Pts',(72.4149306511492,-9.99908189827062,
56.0764566003539));
#169475=CARTESIAN_POINT('Ctrl Pts',(72.449671653634,-9.9995129522664,56.0706872254942));
#169476=CARTESIAN_POINT('Ctrl Pts',(72.5048409769384,-9.9999020204515,56.0615351398569));
#169477=CARTESIAN_POINT('Ctrl Pts',(72.5252675186006,-9.99998176874114,
56.0581486930192));
#169478=CARTESIAN_POINT('Ctrl Pts',(72.5678229536413,-10.0000139510908,
56.0510982084332));
#169479=CARTESIAN_POINT('Ctrl Pts',(72.5899517234821,-9.9999552273227,56.0474345980703));
#169480=CARTESIAN_POINT('Ctrl Pts',(72.6441556196297,-9.99962655807334,
56.0384668595446));
#169481=CARTESIAN_POINT('Ctrl Pts',(72.6762305024331,-9.99927353800509,
56.0331655474039));
#169482=CARTESIAN_POINT('Ctrl Pts',(72.7931227708354,-9.99740923360215,
56.0138637553239));
#169483=CARTESIAN_POINT('Ctrl Pts',(72.8779265259183,-9.99494796000027,
55.9998952290557));
#169484=CARTESIAN_POINT('Ctrl Pts',(73.4095317892232,-9.97256441822664,
55.9125101387846));
#169485=CARTESIAN_POINT('Ctrl Pts',(73.8547227937369,-9.92299041826608,
55.8400988035389));
#169486=CARTESIAN_POINT('Ctrl Pts',(74.8528913103704,-9.74166578596338,
55.6778068135957));
#169487=CARTESIAN_POINT('Ctrl Pts',(75.4010864551881,-9.59185145428424,
55.5886793896532));
#169488=CARTESIAN_POINT('Ctrl Pts',(76.0374947437299,-9.35677851018121,
55.4843722946892));
#169489=CARTESIAN_POINT('Ctrl Pts',(76.1408954633519,-9.31657285902152,
55.467400478894));
#169490=CARTESIAN_POINT('Ctrl Pts',(76.2927394307979,-9.25453735573563,
55.4424399376539));
#169491=CARTESIAN_POINT('Ctrl Pts',(76.3417150974251,-9.23406188663135,
55.4343833679096));
#169492=CARTESIAN_POINT('Ctrl Pts',(76.4286843997551,-9.19686817249914,
55.4200664881765));
#169493=CARTESIAN_POINT('Ctrl Pts',(76.4667416996277,-9.1803053120177,55.4137979545817));
#169494=CARTESIAN_POINT('Ctrl Pts',(76.5469888009104,-9.14477244002966,
55.4005728193999));
#169495=CARTESIAN_POINT('Ctrl Pts',(76.5891523047892,-9.12574425336534,
55.3936197031896));
#169496=CARTESIAN_POINT('Ctrl Pts',(76.7016163445618,-9.07402759935329,
55.3750620831016));
#169497=CARTESIAN_POINT('Ctrl Pts',(76.7716706835233,-9.04080000370248,
55.363490486311));
#169498=CARTESIAN_POINT('Ctrl Pts',(77.1479219861643,-8.85683837482425,
55.3012808761437));
#169499=CARTESIAN_POINT('Ctrl Pts',(77.4466151464932,-8.69095536332824,
55.251666818673));
#169500=CARTESIAN_POINT('Ctrl Pts',(77.9198684905862,-8.3948719008566,55.1729311343635));
#169501=CARTESIAN_POINT('Ctrl Pts',(78.099723584724,-8.27391124224535,55.1429790993635));
#169502=CARTESIAN_POINT('Ctrl Pts',(78.6302781537059,-7.89111577955463,
55.0547332519268));
#169503=CARTESIAN_POINT('Ctrl Pts',(78.9679416977988,-7.61163695975409,
54.998706525971));
#169504=CARTESIAN_POINT('Ctrl Pts',(79.3353174715195,-7.26424259857941,
54.938789279341));
#169505=CARTESIAN_POINT('Ctrl Pts',(79.383741018466,-7.21751477357013,54.9309146061299));
#169506=CARTESIAN_POINT('Ctrl Pts',(79.4536984442701,-7.14862654645227,
54.9195766008154));
#169507=CARTESIAN_POINT('Ctrl Pts',(79.4756014835507,-7.12685710512131,
54.9160323879038));
#169508=CARTESIAN_POINT('Ctrl Pts',(79.5140174351064,-7.08831954481476,
54.9098266532962));
#169509=CARTESIAN_POINT('Ctrl Pts',(79.5305719591037,-7.0715948130502,54.9071559190606));
#169510=CARTESIAN_POINT('Ctrl Pts',(79.5661251393491,-7.03542133399335,
54.9014278543103));
#169511=CARTESIAN_POINT('Ctrl Pts',(79.5851040282734,-7.0159530104727,54.8983748560151));
#169512=CARTESIAN_POINT('Ctrl Pts',(79.6383277509734,-6.96090901401687,
54.8898259702292));
#169513=CARTESIAN_POINT('Ctrl Pts',(79.6723917784638,-6.92515347902827,
54.8843696385213));
#169514=CARTESIAN_POINT('Ctrl Pts',(79.908219719632,-6.67391241297142,54.8466928559278));
#169515=CARTESIAN_POINT('Ctrl Pts',(80.1007629886276,-6.44967898789775,
54.8164323098566));
#169516=CARTESIAN_POINT('Ctrl Pts',(80.3753692817547,-6.09963621108647,
54.7737250646285));
#169517=CARTESIAN_POINT('Ctrl Pts',(80.4649169703354,-5.98007951967056,
54.7598797984591));
#169518=CARTESIAN_POINT('Ctrl Pts',(80.8667413674399,-5.41781870523989,
54.698029213528));
#169519=CARTESIAN_POINT('Ctrl Pts',(81.1457710342195,-4.95184374073563,
54.655829943058));
#169520=CARTESIAN_POINT('Ctrl Pts',(81.4315238242444,-4.37297496881559,
54.6128386239359));
#169521=CARTESIAN_POINT('Ctrl Pts',(81.4756575606616,-4.28000185518985,
54.6062089315844));
#169522=CARTESIAN_POINT('Ctrl Pts',(81.5401421580115,-4.13859566780366,
54.5965362729525));
#169523=CARTESIAN_POINT('Ctrl Pts',(81.5615490161417,-4.09066325865285,
54.5933277826855));
#169524=CARTESIAN_POINT('Ctrl Pts',(81.5993227252462,-4.00427456710424,
54.5876707390799));
#169525=CARTESIAN_POINT('Ctrl Pts',(81.6158264466846,-3.96588089874698,
54.5852007478941));
#169526=CARTESIAN_POINT('Ctrl Pts',(81.6505251769789,-3.88375331949801,
54.5800111886631));
#169527=CARTESIAN_POINT('Ctrl Pts',(81.668651849627,-3.83999097759006,54.5773023198099));
#169528=CARTESIAN_POINT('Ctrl Pts',(81.7170541125251,-3.72076351979598,
54.5700751788798));
#169529=CARTESIAN_POINT('Ctrl Pts',(81.746727711641,-3.64505228686216,54.5656512469584));
#169530=CARTESIAN_POINT('Ctrl Pts',(81.9133955697007,-3.20417084113407,
54.5408473783303));
#169531=CARTESIAN_POINT('Ctrl Pts',(82.0300710656479,-2.83150713910028,
54.523646427459));
#169532=CARTESIAN_POINT('Ctrl Pts',(82.2398850257726,-1.99423984355841,
54.4935909311738));
#169533=CARTESIAN_POINT('Ctrl Pts',(82.3225606237439,-1.52792548356179,
54.4824555261108));
#169534=CARTESIAN_POINT('Ctrl Pts',(82.3729798775079,-1.05279654130084,
54.4774256716504));
#169535=CARTESIAN_POINT('Ctrl Pts',(82.3734724356883,-1.04812404505824,
54.4773768217422));
#169536=CARTESIAN_POINT('Ctrl Pts',(82.4016060224843,-0.779458804999393,
54.4746033673291));
#169537=CARTESIAN_POINT('Ctrl Pts',(82.4189096750665,-0.514469882601093,
54.4738294657436));
#169538=CARTESIAN_POINT('Ctrl Pts',(82.4270068078351,-0.205490529190298,
54.4754107223865));
#169539=CARTESIAN_POINT('Ctrl Pts',(82.4278702324258,-0.161859226207651,
54.4756916412848));
#169540=CARTESIAN_POINT('Ctrl Pts',(82.4288204927573,-0.090823488374513,
54.4762442007747));
#169541=CARTESIAN_POINT('Ctrl Pts',(82.4290767380085,-0.0634216294130038,
54.476480406394));
#169542=CARTESIAN_POINT('Ctrl Pts',(82.4293385200686,-0.0142810983463323,
54.4769457332704));
#169543=CARTESIAN_POINT('Ctrl Pts',(82.4293849340598,0.00745710382980186,
54.4771662470542));
#169544=CARTESIAN_POINT('Ctrl Pts',(82.4293341863736,0.0554785326590305,
54.477685826653));
#169545=CARTESIAN_POINT('Ctrl Pts',(82.4292049693798,0.08176129124716,54.4779916296242));
#169546=CARTESIAN_POINT('Ctrl Pts',(82.4285316766892,0.158468487834349,
54.4789461576016));
#169547=CARTESIAN_POINT('Ctrl Pts',(82.4277155479953,0.208889019182937,
54.4796518192819));
#169548=CARTESIAN_POINT('Ctrl Pts',(82.4159105354718,0.70906493129357,54.4874161870165));
#169549=CARTESIAN_POINT('Ctrl Pts',(82.3755609864959,1.15752836349655,54.5004882693197));
#169550=CARTESIAN_POINT('Ctrl Pts',(82.2068610916447,2.22875953212481,54.5447081719204));
#169551=CARTESIAN_POINT('Ctrl Pts',(82.0494635512867,2.84478283087259,54.5809129284911));
#169552=CARTESIAN_POINT('Ctrl Pts',(81.7988418525356,3.54316768347523,54.6336528733453));
#169553=CARTESIAN_POINT('Ctrl Pts',(81.7606646779194,3.64438470872402,54.6416005012898));
#169554=CARTESIAN_POINT('Ctrl Pts',(81.7014303815819,3.79406607834721,54.6538080178078));
#169555=CARTESIAN_POINT('Ctrl Pts',(81.681607237855,3.84302578750983,54.657874339003));
#169556=CARTESIAN_POINT('Ctrl Pts',(81.6454187762078,3.93041684719629,54.6652643942841));
#169557=CARTESIAN_POINT('Ctrl Pts',(81.6291974172002,3.96890834370733,54.6685655588056));
#169558=CARTESIAN_POINT('Ctrl Pts',(81.5941956370286,4.05053645526604,54.6756649093197));
#169559=CARTESIAN_POINT('Ctrl Pts',(81.5753514938876,4.09364376750275,54.6794730565798));
#169560=CARTESIAN_POINT('Ctrl Pts',(81.5236156664912,4.20976142294565,54.6898913538235));
#169561=CARTESIAN_POINT('Ctrl Pts',(81.490154893451,4.28250630447755,54.696590631967));
#169562=CARTESIAN_POINT('Ctrl Pts',(81.2907477346504,4.70269672627653,54.7363000769308));
#169563=CARTESIAN_POINT('Ctrl Pts',(81.1058777324296,5.04051428627442,54.7722656345596));
#169564=CARTESIAN_POINT('Ctrl Pts',(80.7241133451485,5.65166074140487,54.8455535455307));
#169565=CARTESIAN_POINT('Ctrl Pts',(80.531901771641,5.92736136981478,54.8820932826333));
#169566=CARTESIAN_POINT('Ctrl Pts',(80.1413555983125,6.43134801659066,54.9562323536256));
#169567=CARTESIAN_POINT('Ctrl Pts',(79.9457641775941,6.66135402728018,54.9933232199854));
#169568=CARTESIAN_POINT('Ctrl Pts',(79.7057435020128,6.91893325193734,55.0391076960068));
#169569=CARTESIAN_POINT('Ctrl Pts',(79.6709871232328,6.95566642586564,55.045743818865));
#169570=CARTESIAN_POINT('Ctrl Pts',(79.6167601621197,7.01210909655683,55.0561092813358));
#169571=CARTESIAN_POINT('Ctrl Pts',(79.5974809254804,7.03200889466407,55.0597967666537));
#169572=CARTESIAN_POINT('Ctrl Pts',(79.5617772468385,7.06855487408178,55.0666302994487));
#169573=CARTESIAN_POINT('Ctrl Pts',(79.545376418575,7.08522452647522,55.0697711545597));
#169574=CARTESIAN_POINT('Ctrl Pts',(79.5074829122929,7.12346818551903,55.0770320322302));
#169575=CARTESIAN_POINT('Ctrl Pts',(79.4859504863666,7.14500065226707,55.0811608488297));
#169576=CARTESIAN_POINT('Ctrl Pts',(79.4174480730519,7.21287585899812,55.0943044366918));
#169577=CARTESIAN_POINT('Ctrl Pts',(79.3701224699737,7.25884203766398,55.1033971158815));
#169578=CARTESIAN_POINT('Ctrl Pts',(79.1141926749848,7.50250369588973,55.1526190067117));
#169579=CARTESIAN_POINT('Ctrl Pts',(78.8976913879561,7.69136418084092,55.1944298746371));
#169580=CARTESIAN_POINT('Ctrl Pts',(78.2838825101048,8.18129732708011,55.3128506456284));
#169581=CARTESIAN_POINT('Ctrl Pts',(77.8717753589995,8.46179792821496,55.3921978488658));
#169582=CARTESIAN_POINT('Ctrl Pts',(77.2462945219386,8.82100363719068,55.511396839619));
#169583=CARTESIAN_POINT('Ctrl Pts',(77.0483720389228,8.92577871084782,55.5489582229632));
#169584=CARTESIAN_POINT('Ctrl Pts',(76.783487209225,9.05451937528056,55.5989921319597));
#169585=CARTESIAN_POINT('Ctrl Pts',(76.7195603847006,9.0847328878724,55.611049850424));
#169586=CARTESIAN_POINT('Ctrl Pts',(76.6147074934559,9.13289832527706,55.6307983198773));
#169587=CARTESIAN_POINT('Ctrl Pts',(76.5739730013242,9.15127139462957,55.6384634717442));
#169588=CARTESIAN_POINT('Ctrl Pts',(76.4949112294838,9.18627816191814,55.6533273409854));
#169589=CARTESIAN_POINT('Ctrl Pts',(76.4566001647601,9.20294698566827,55.6605238815318));
#169590=CARTESIAN_POINT('Ctrl Pts',(76.3667529918049,9.24135197633555,55.6773871338504));
#169591=CARTESIAN_POINT('Ctrl Pts',(76.3151360383591,9.26289062336812,55.6870642553344));
#169592=CARTESIAN_POINT('Ctrl Pts',(76.1453233088867,9.33203509825228,55.7188659577552));
#169593=CARTESIAN_POINT('Ctrl Pts',(76.0263920632102,9.37775573475257,55.7410838746758));
#169594=CARTESIAN_POINT('Ctrl Pts',(75.4832938997748,9.57436478447919,55.842311186214));
#169595=CARTESIAN_POINT('Ctrl Pts',(75.0500308355795,9.69791212482701,55.9224049916045));
#169596=CARTESIAN_POINT('Ctrl Pts',(74.0737754918058,9.90416761000369,56.102387699057));
#169597=CARTESIAN_POINT('Ctrl Pts',(73.5291952782041,9.97170823125382,56.2024549930993));
#169598=CARTESIAN_POINT('Ctrl Pts',(72.9079695672571,9.99567491006911,56.3179217619057));
#169599=CARTESIAN_POINT('Ctrl Pts',(72.8337804531382,9.99768193755017,56.3317334082451));
#169600=CARTESIAN_POINT('Ctrl Pts',(72.728284389981,9.99932051509322,56.3514113699516));
#169601=CARTESIAN_POINT('Ctrl Pts',(72.6969865941856,9.99965457759026,56.3572540338713));
#169602=CARTESIAN_POINT('Ctrl Pts',(72.6439812619526,9.99996283038682,56.3671576897605));
#169603=CARTESIAN_POINT('Ctrl Pts',(72.6222738843087,10.0000159269599,56.3712160098394));
#169604=CARTESIAN_POINT('Ctrl Pts',(72.5772235176491,9.99997431923388,56.3796437543126));
#169605=CARTESIAN_POINT('Ctrl Pts',(72.5538808387964,9.99986817156351,56.3840134947001));
#169606=CARTESIAN_POINT('Ctrl Pts',(72.49251572356,9.99936673317937,56.3955083835053));
#169607=CARTESIAN_POINT('Ctrl Pts',(72.4544956172965,9.99883157127421,56.4026377265703));
#169608=CARTESIAN_POINT('Ctrl Pts',(72.2802833109216,9.99535057011472,56.4353365744532));
#169609=CARTESIAN_POINT('Ctrl Pts',(72.1441718469965,9.98974876820901,56.4609719204842));
#169610=CARTESIAN_POINT('Ctrl Pts',(71.7473587831863,9.96500015591874,56.5358905291706));
#169611=CARTESIAN_POINT('Ctrl Pts',(71.4872686788627,9.93814623553098,56.5852240625654));
#169612=CARTESIAN_POINT('Ctrl Pts',(70.580079533466,9.80709571539761,56.7575561715957));
#169613=CARTESIAN_POINT('Ctrl Pts',(69.9424640444626,9.64765091616599,56.8790159863435));
#169614=CARTESIAN_POINT('Ctrl Pts',(69.2054819054799,9.38166958775962,57.0182529712163));
#169615=CARTESIAN_POINT('Ctrl Pts',(69.0867697975335,9.3361763624801,57.0406491832489));
#169616=CARTESIAN_POINT('Ctrl Pts',(68.921054706971,9.26891833849636,57.0718657071906));
#169617=CARTESIAN_POINT('Ctrl Pts',(68.8733093509438,9.2490959576013,57.0808541581039));
#169618=CARTESIAN_POINT('Ctrl Pts',(68.790284730528,9.21384936594005,57.0964745278537));
#169619=CARTESIAN_POINT('Ctrl Pts',(68.7549373319765,9.1985954515273,57.103121750187));
#169620=CARTESIAN_POINT('Ctrl Pts',(68.6809070411261,9.1661266111272,57.1170370300208));
#169621=CARTESIAN_POINT('Ctrl Pts',(68.6422433720346,9.14886803357578,57.1243008328644));
#169622=CARTESIAN_POINT('Ctrl Pts',(68.5497815480908,9.10687096911078,57.1416630629036));
#169623=CARTESIAN_POINT('Ctrl Pts',(68.4960901972944,9.08189174982622,57.1517379490642));
#169624=CARTESIAN_POINT('Ctrl Pts',(68.3088635341918,8.9927051785819,57.1868461008762));
#169625=CARTESIAN_POINT('Ctrl Pts',(68.176525944269,8.92592930494475,57.2116183926266));
#169626=CARTESIAN_POINT('Ctrl Pts',(67.8511540812208,8.75235638610652,57.2724376206627));
#169627=CARTESIAN_POINT('Ctrl Pts',(67.6600578693407,8.64196238927888,57.3080782900684));
#169628=CARTESIAN_POINT('Ctrl Pts',(67.2175591210862,8.36599611620118,57.3905295534725));
#169629=CARTESIAN_POINT('Ctrl Pts',(66.9696341734787,8.19507159405754,57.4366609657191));
#169630=CARTESIAN_POINT('Ctrl Pts',(66.4438464427843,7.79574362683847,57.5347582742036));
#169631=CARTESIAN_POINT('Ctrl Pts',(66.1697767596987,7.56290386938635,57.5860676631683));
#169632=CARTESIAN_POINT('Ctrl Pts',(65.8583775761023,7.26753532360987,57.6451042854397));
#169633=CARTESIAN_POINT('Ctrl Pts',(65.8083895065521,7.21910494183,57.6546059483399));
#169634=CARTESIAN_POINT('Ctrl Pts',(65.7370365720214,7.14849520084388,57.6682097371229));
#169635=CARTESIAN_POINT('Ctrl Pts',(65.7152613999905,7.12674411985674,57.6723669140076));
#169636=CARTESIAN_POINT('Ctrl Pts',(65.6770611289512,7.08822709864953,57.6796703990337));
#169637=CARTESIAN_POINT('Ctrl Pts',(65.6605939355939,7.07150438459761,57.6828222612992));
#169638=CARTESIAN_POINT('Ctrl Pts',(65.6252167011947,7.03532073221709,57.6896013079857));
#169639=CARTESIAN_POINT('Ctrl Pts',(65.6063268311122,7.01584010477385,57.6932257874504));
#169640=CARTESIAN_POINT('Ctrl Pts',(65.5533240088667,6.96072658762479,57.7034085892717));
#169641=CARTESIAN_POINT('Ctrl Pts',(65.5193952313301,6.92491311339782,57.7099421413555));
#169642=CARTESIAN_POINT('Ctrl Pts',(65.283066071036,6.67168263224396,57.7555505508232));
#169643=CARTESIAN_POINT('Ctrl Pts',(65.0901732058478,6.44535836798946,57.7932889557165));
#169644=CARTESIAN_POINT('Ctrl Pts',(64.7885022084069,6.05739191205442,57.8528130777467));
#169645=CARTESIAN_POINT('Ctrl Pts',(64.6738607905233,5.90070242968286,57.8755715312986));
#169646=CARTESIAN_POINT('Ctrl Pts',(64.287253920152,5.33856541730202,57.9526423385588));
#169647=CARTESIAN_POINT('Ctrl Pts',(64.040221105445,4.91621195611723,58.0024542000079));
#169648=CARTESIAN_POINT('Ctrl Pts',(63.7775918557604,4.38120704456539,58.0556145728963));
#169649=CARTESIAN_POINT('Ctrl Pts',(63.7320559606948,4.28459179474932,58.064842932154));
#169650=CARTESIAN_POINT('Ctrl Pts',(63.6664199724308,4.13939055152813,58.078159961223));
#169651=CARTESIAN_POINT('Ctrl Pts',(63.6451582906387,4.09135915692004,58.0824763521399));
#169652=CARTESIAN_POINT('Ctrl Pts',(63.6076744457373,4.00486260710316,58.0900906373594));
#169653=CARTESIAN_POINT('Ctrl Pts',(63.5913148872551,3.96646073489049,58.0934154829661));
#169654=CARTESIAN_POINT('Ctrl Pts',(63.5569524441323,3.88439179869214,58.1004027326542));
#169655=CARTESIAN_POINT('Ctrl Pts',(63.5390163989046,3.84069674659609,58.1040520213532));
#169656=CARTESIAN_POINT('Ctrl Pts',(63.4912016664778,3.72184654249729,58.1137866322386));
#169657=CARTESIAN_POINT('Ctrl Pts',(63.461914474154,3.64644787228342,58.1197559777224));
#169658=CARTESIAN_POINT('Ctrl Pts',(63.2993237374074,3.21250580671838,58.1529389311906));
#169659=CARTESIAN_POINT('Ctrl Pts',(63.185448854058,2.8467383454678,58.176338518366));
#169660=CARTESIAN_POINT('Ctrl Pts',(62.9646140568515,1.96398543113634,58.2226196055605));
#169661=CARTESIAN_POINT('Ctrl Pts',(62.8766945410915,1.44324608427282,58.2419059869019));
#169662=CARTESIAN_POINT('Ctrl Pts',(62.8096001378845,0.692362390434222,
58.2599719580861));
#169663=CARTESIAN_POINT('Ctrl Pts',(62.7970198741906,0.46623249628501,58.2641754945589));
#169664=CARTESIAN_POINT('Ctrl Pts',(62.7910382678108,0.193820077886311,
58.2678904327133));
#169665=CARTESIAN_POINT('Ctrl Pts',(62.7903421927524,0.147778305705106,
58.2684720525722));
#169666=CARTESIAN_POINT('Ctrl Pts',(62.7897489103399,0.0760961461433343,
58.2693071413881));
#169667=CARTESIAN_POINT('Ctrl Pts',(62.7896343689182,0.0504585672256714,
58.2695917929293));
#169668=CARTESIAN_POINT('Ctrl Pts',(62.7896120602203,0.0165471062013723,
58.2699499944522));
#169669=CARTESIAN_POINT('Ctrl Pts',(62.789616789492,0.00827354424855654,
58.2700359449107));
#169670=CARTESIAN_POINT('Ctrl Pts',(62.7896316916575,-5.79826049313321E-11,
58.2701204592907));
#169671=CARTESIAN_POINT('Origin',(72.2537026314029,-4.33680868994202E-16,
54.3558290880045));
#169672=CARTESIAN_POINT('',(62.9072242170052,2.7021311761062E-11,58.9370208104186));
#169673=CARTESIAN_POINT('',(62.9025030071409,2.44438148519277E-14,58.910245498748));
#169674=CARTESIAN_POINT('',(62.4056251012807,-1.65832766814156E-15,56.0923108646735));
#169675=CARTESIAN_POINT('Ctrl Pts',(62.9072242170052,5.40442818497922E-11,
58.9370208104186));
#169676=CARTESIAN_POINT('Ctrl Pts',(62.9072099714203,0.00790901692578116,
58.9369400196918));
#169677=CARTESIAN_POINT('Ctrl Pts',(62.9072049102169,0.0158180443091237,
58.9368572823768));
#169678=CARTESIAN_POINT('Ctrl Pts',(62.9072223236603,0.0492122228663902,
58.9364997435817));
#169679=CARTESIAN_POINT('Ctrl Pts',(62.9073309856082,0.0746970095420169,
58.9362067275076));
#169680=CARTESIAN_POINT('Ctrl Pts',(62.9078983196514,0.145548068002589,
58.9353365036641));
#169681=CARTESIAN_POINT('Ctrl Pts',(62.9085639252973,0.19091154185888,58.9347159484371));
#169682=CARTESIAN_POINT('Ctrl Pts',(62.914083478072,0.449523595448512,58.930821944839));
#169683=CARTESIAN_POINT('Ctrl Pts',(62.9253196393055,0.662561934454989,
58.9262334789076));
#169684=CARTESIAN_POINT('Ctrl Pts',(62.9979891074459,1.52433953176591,58.9024195406952));
#169685=CARTESIAN_POINT('Ctrl Pts',(63.1149747013286,2.16649684139304,58.8726607003243));
#169686=CARTESIAN_POINT('Ctrl Pts',(63.3443570660399,2.97374699778817,58.821663746837));
#169687=CARTESIAN_POINT('Ctrl Pts',(63.4009550725885,3.1535826411818,58.8093857239716));
#169688=CARTESIAN_POINT('Ctrl Pts',(63.5064351023077,3.45855579379913,58.7870053930245));
#169689=CARTESIAN_POINT('Ctrl Pts',(63.5528456303677,3.58452159447197,58.7772946324959));
#169690=CARTESIAN_POINT('Ctrl Pts',(63.6227038128266,3.76302421421529,58.7628645056372));
#169691=CARTESIAN_POINT('Ctrl Pts',(63.6441105610017,3.81636952546874,58.758465381957));
#169692=CARTESIAN_POINT('Ctrl Pts',(63.6821033324133,3.90874492530129,58.7506963692028));
#169693=CARTESIAN_POINT('Ctrl Pts',(63.6984818927013,3.94786141543798,58.747359002905));
#169694=CARTESIAN_POINT('Ctrl Pts',(63.7305864134983,4.02319256790192,58.7408396397097));
#169695=CARTESIAN_POINT('Ctrl Pts',(63.7462793550074,4.05942088576101,58.7376628283205));
#169696=CARTESIAN_POINT('Ctrl Pts',(63.7884448525589,4.15520941778614,58.7291527424406));
#169697=CARTESIAN_POINT('Ctrl Pts',(63.8152827515735,4.21460159034845,58.7237622603097));
#169698=CARTESIAN_POINT('Ctrl Pts',(63.9157462712276,4.43127501901037,58.7036757439514));
#169699=CARTESIAN_POINT('Ctrl Pts',(63.9928553458238,4.58685535633015,58.6884337066871));
#169700=CARTESIAN_POINT('Ctrl Pts',(64.3299796384894,5.2248400448046,58.6224229689439));
#169701=CARTESIAN_POINT('Ctrl Pts',(64.6250941257276,5.68701860783708,58.5661299263498));
#169702=CARTESIAN_POINT('Ctrl Pts',(65.1409671780277,6.36513302978434,58.4681738755596));
#169703=CARTESIAN_POINT('Ctrl Pts',(65.3367536087514,6.59933673394019,58.4310616145545));
#169704=CARTESIAN_POINT('Ctrl Pts',(65.5886306731084,6.87397495057979,58.3830608139658));
#169705=CARTESIAN_POINT('Ctrl Pts',(65.6349741409503,6.92348032315649,58.3742189546327));
#169706=CARTESIAN_POINT('Ctrl Pts',(65.7030811716782,6.99475923142845,58.3612055093332));
#169707=CARTESIAN_POINT('Ctrl Pts',(65.7244532444699,7.01691964646535,58.3571191606363));
#169708=CARTESIAN_POINT('Ctrl Pts',(65.7621127677075,7.05560708156892,58.3499133524138));
#169709=CARTESIAN_POINT('Ctrl Pts',(65.7783566498744,7.07217784936632,58.3468035043139));
#169710=CARTESIAN_POINT('Ctrl Pts',(65.8138969522583,7.10818028216566,58.3399955198663));
#169711=CARTESIAN_POINT('Ctrl Pts',(65.833215376259,7.12758875897559,58.3362925247325));
#169712=CARTESIAN_POINT('Ctrl Pts',(65.8874094294959,7.18158694534945,58.3258983437606));
#169713=CARTESIAN_POINT('Ctrl Pts',(65.9224581545836,7.21599447354607,58.3191690945198));
#169714=CARTESIAN_POINT('Ctrl Pts',(66.1460933339935,7.43230066183781,58.2761949037771));
#169715=CARTESIAN_POINT('Ctrl Pts',(66.3414265066577,7.60678559789629,58.2384969884545));
#169716=CARTESIAN_POINT('Ctrl Pts',(66.96643879466,8.12189261756985,58.1178935357555));
#169717=CARTESIAN_POINT('Ctrl Pts',(67.4173223138905,8.43418822257564,58.0309712340087));
#169718=CARTESIAN_POINT('Ctrl Pts',(68.0868740326202,8.81918656896863,57.903365161378));
#169719=CARTESIAN_POINT('Ctrl Pts',(68.2860330616276,8.92469844476276,57.8655674196164));
#169720=CARTESIAN_POINT('Ctrl Pts',(68.5523425875103,9.05416498403435,57.815263723373));
#169721=CARTESIAN_POINT('Ctrl Pts',(68.6164147943805,9.08445319839993,57.8031784602715));
#169722=CARTESIAN_POINT('Ctrl Pts',(68.7214455199851,9.13270684668133,57.7833963626669));
#169723=CARTESIAN_POINT('Ctrl Pts',(68.7622111693946,9.15109621926484,57.7757253014748));
#169724=CARTESIAN_POINT('Ctrl Pts',(68.8412908242867,9.18611473125428,57.7608579913955));
#169725=CARTESIAN_POINT('Ctrl Pts',(68.8795883491662,9.20277960523408,57.7536639543031));
#169726=CARTESIAN_POINT('Ctrl Pts',(68.9693383521251,9.24114781486347,57.7368188421719));
#169727=CARTESIAN_POINT('Ctrl Pts',(69.020871161784,9.26265489952566,57.7271574233656));
#169728=CARTESIAN_POINT('Ctrl Pts',(69.1901106536621,9.33158027280642,57.6954627846869));
#169729=CARTESIAN_POINT('Ctrl Pts',(69.3085460544608,9.37713114827548,57.6733370777983));
#169730=CARTESIAN_POINT('Ctrl Pts',(69.8579557704563,9.57617069789906,57.5709306182368));
#169731=CARTESIAN_POINT('Ctrl Pts',(70.2983559506258,9.70132920320212,57.4895274646193));
#169732=CARTESIAN_POINT('Ctrl Pts',(71.2942694631327,9.90964150232231,57.305932341899));
#169733=CARTESIAN_POINT('Ctrl Pts',(71.8514694646905,9.9765227365849,57.2035482040618));
#169734=CARTESIAN_POINT('Ctrl Pts',(72.4728185408518,9.99685256945185,57.0879616226865));
#169735=CARTESIAN_POINT('Ctrl Pts',(72.5346505210121,9.99828181634118,57.0764431279122));
#169736=CARTESIAN_POINT('Ctrl Pts',(72.6248549170636,9.99950089481505,57.0596117595833));
#169737=CARTESIAN_POINT('Ctrl Pts',(72.6532223781713,9.9997593561708,57.0543146720848));
#169738=CARTESIAN_POINT('Ctrl Pts',(72.7031287002219,9.99999431123556,57.044988182496));
#169739=CARTESIAN_POINT('Ctrl Pts',(72.7246674202334,10.0000237023634,57.0409605807427));
#169740=CARTESIAN_POINT('Ctrl Pts',(72.770701546333,9.99993260503462,57.0323471199713));
#169741=CARTESIAN_POINT('Ctrl Pts',(72.7951964722171,9.99979098279492,57.0277606547346));
#169742=CARTESIAN_POINT('Ctrl Pts',(72.862952647179,9.99914155429355,57.0150654391661));
#169743=CARTESIAN_POINT('Ctrl Pts',(72.9062103478262,9.99843631372799,57.006950877971));
#169744=CARTESIAN_POINT('Ctrl Pts',(73.1581763788988,9.99263517906828,56.9596348577346));
#169745=CARTESIAN_POINT('Ctrl Pts',(73.3666532149147,9.98106536972207,56.9202842055288));
#169746=CARTESIAN_POINT('Ctrl Pts',(73.9664364500754,9.92823246739088,56.8067478861944));
#169747=CARTESIAN_POINT('Ctrl Pts',(74.3558284558308,9.86980459667376,56.7326488791205));
#169748=CARTESIAN_POINT('Ctrl Pts',(75.2413158291936,9.68110915818093,56.5642973908312));
#169749=CARTESIAN_POINT('Ctrl Pts',(75.7329741129178,9.53481733868083,56.4709626815177));
#169750=CARTESIAN_POINT('Ctrl Pts',(76.289398075909,9.32010056864745,56.3660078907599));
#169751=CARTESIAN_POINT('Ctrl Pts',(76.3671075955933,9.28895588853841,56.351364415483));
#169752=CARTESIAN_POINT('Ctrl Pts',(76.4887300842574,9.23838171984617,56.3284689807045));
#169753=CARTESIAN_POINT('Ctrl Pts',(76.5329079298455,9.21962723535497,56.3201573060205));
#169754=CARTESIAN_POINT('Ctrl Pts',(76.6143364945807,9.18434679062292,56.3048460498126));
#169755=CARTESIAN_POINT('Ctrl Pts',(76.6516242935245,9.1679127289542,56.2978381588468));
#169756=CARTESIAN_POINT('Ctrl Pts',(76.7344099097664,9.13080467554706,56.2822869316835));
#169757=CARTESIAN_POINT('Ctrl Pts',(76.7798558479759,9.11001298678257,56.2737550551609));
#169758=CARTESIAN_POINT('Ctrl Pts',(76.9118334746308,9.04840208803876,56.2489924428116));
#169759=CARTESIAN_POINT('Ctrl Pts',(76.9979413263648,9.00665194493683,56.2328545356675));
#169760=CARTESIAN_POINT('Ctrl Pts',(77.3841244304719,8.81234711301676,56.160552686014));
#169761=CARTESIAN_POINT('Ctrl Pts',(77.6770352127363,8.64550191482432,56.105929013356));
#169762=CARTESIAN_POINT('Ctrl Pts',(78.408644020972,8.17723440513523,55.9696435213792));
#169763=CARTESIAN_POINT('Ctrl Pts',(78.8328513716642,7.85444784033037,55.8907981797405));
#169764=CARTESIAN_POINT('Ctrl Pts',(79.3308440876463,7.4073590267506,55.7969444636213));
#169765=CARTESIAN_POINT('Ctrl Pts',(79.4305232913329,7.31405828729849,55.7780829839275));
#169766=CARTESIAN_POINT('Ctrl Pts',(79.5579481356863,7.18972030950491,55.7538366893383));
#169767=CARTESIAN_POINT('Ctrl Pts',(79.5874578565791,7.16055965952134,55.7482118641509));
#169768=CARTESIAN_POINT('Ctrl Pts',(79.6347572932563,7.11322593737397,55.7391791053005));
#169769=CARTESIAN_POINT('Ctrl Pts',(79.6526608714437,7.09517025378022,55.7357560694201));
#169770=CARTESIAN_POINT('Ctrl Pts',(79.6873827345013,7.05988143305583,55.7291093395206));
#169771=CARTESIAN_POINT('Ctrl Pts',(79.70420798506,7.04265570807208,55.7258847200167));
#169772=CARTESIAN_POINT('Ctrl Pts',(79.7454357550802,7.00013629364943,55.7179742160835));
#169773=CARTESIAN_POINT('Ctrl Pts',(79.769767428884,6.97477254054825,55.7132977570772));
#169774=CARTESIAN_POINT('Ctrl Pts',(79.8594096120248,6.88032337847043,55.6960411856496));
#169775=CARTESIAN_POINT('Ctrl Pts',(79.9238673893492,6.81041443214672,55.6835778309452));
#169776=CARTESIAN_POINT('Ctrl Pts',(80.0875772821118,6.62763857621036,55.6518011115764));
#169777=CARTESIAN_POINT('Ctrl Pts',(80.1853035867766,6.51339870097038,55.6327120356469));
#169778=CARTESIAN_POINT('Ctrl Pts',(80.4987040893437,6.12971420976461,55.5711894503913));
#169779=CARTESIAN_POINT('Ctrl Pts',(80.7030701859377,5.85107048554801,55.5305775026007));
#169780=CARTESIAN_POINT('Ctrl Pts',(81.1432751320225,5.18051551057712,55.4425525424328));
#169781=CARTESIAN_POINT('Ctrl Pts',(81.3676554092802,4.78174074339207,55.3972589895638));
#169782=CARTESIAN_POINT('Ctrl Pts',(81.5995376466848,4.2947398871361,55.3502808347035));
#169783=CARTESIAN_POINT('Ctrl Pts',(81.6338333089187,4.22039165055155,55.3433263560345));
#169784=CARTESIAN_POINT('Ctrl Pts',(81.6867568252709,4.10188772790358,55.332584928723));
#169785=CARTESIAN_POINT('Ctrl Pts',(81.7059781403745,4.05801179258908,55.3286816107324));
#169786=CARTESIAN_POINT('Ctrl Pts',(81.741332680708,3.97572000802668,55.3214980692558));
#169787=CARTESIAN_POINT('Ctrl Pts',(81.7575414059008,3.93733903303375,55.3182030361024));
#169788=CARTESIAN_POINT('Ctrl Pts',(81.7932735625761,3.851245334889,55.3109353486928));
#169789=CARTESIAN_POINT('Ctrl Pts',(81.8126709235696,3.80347950775275,55.3069874280684));
#169790=CARTESIAN_POINT('Ctrl Pts',(81.8692303245645,3.6610858909923,55.2954677385405));
#169791=CARTESIAN_POINT('Ctrl Pts',(81.9053367658428,3.56602944462098,55.2881028875509));
#169792=CARTESIAN_POINT('Ctrl Pts',(82.065473195865,3.12449460093883,55.255379535993));
#169793=CARTESIAN_POINT('Ctrl Pts',(82.1720534376146,2.77174544102934,55.2334384729471));
#169794=CARTESIAN_POINT('Ctrl Pts',(82.3758136352477,1.93510532764585,55.1906143018418));
#169795=CARTESIAN_POINT('Ctrl Pts',(82.457417863787,1.44827160084945,55.172657325847));
#169796=CARTESIAN_POINT('Ctrl Pts',(82.5253683923865,0.719948308188185,
55.1546675041677));
#169797=CARTESIAN_POINT('Ctrl Pts',(82.5391241014064,0.481884319809271,
55.1501660288107));
#169798=CARTESIAN_POINT('Ctrl Pts',(82.5454879615095,0.196801508651396,
55.1462630147488));
#169799=CARTESIAN_POINT('Ctrl Pts',(82.546206839377,0.150056984184883,55.1456707560209));
#169800=CARTESIAN_POINT('Ctrl Pts',(82.546818565591,0.0775143892891936,
55.1448240170581));
#169801=CARTESIAN_POINT('Ctrl Pts',(82.5469372335081,0.0517192751872206,
55.1445371285694));
#169802=CARTESIAN_POINT('Ctrl Pts',(82.5469737250037,0.00415092054648192,
55.1440339344148));
#169803=CARTESIAN_POINT('Ctrl Pts',(82.5469199774665,-0.0176219032436765,
55.1438135712789));
#169804=CARTESIAN_POINT('Ctrl Pts',(82.5466360218009,-0.0674037138328463,
55.1433325596077));
#169805=CARTESIAN_POINT('Ctrl Pts',(82.5463596861604,-0.0954122076489487,
55.1430784888024));
#169806=CARTESIAN_POINT('Ctrl Pts',(82.5451378539625,-0.182516811522682,
55.1423405096052));
#169807=CARTESIAN_POINT('Ctrl Pts',(82.5437900812275,-0.241606505921511,
55.1419145693536));
#169808=CARTESIAN_POINT('Ctrl Pts',(82.5282466003325,-0.733675716738335,
55.1390061573088));
#169809=CARTESIAN_POINT('Ctrl Pts',(82.486744801119,-1.16536485403954,55.140592691685));
#169810=CARTESIAN_POINT('Ctrl Pts',(82.3161439861218,-2.22354496998105,
55.1563809273633));
#169811=CARTESIAN_POINT('Ctrl Pts',(82.1552312645009,-2.84289423828583,
55.1762521081694));
#169812=CARTESIAN_POINT('Ctrl Pts',(81.9005478441486,-3.54413120966995,
55.2125774474713));
#169813=CARTESIAN_POINT('Ctrl Pts',(81.8620454506646,-3.64508381083524,
55.2181538028504));
#169814=CARTESIAN_POINT('Ctrl Pts',(81.8023248028915,-3.79445333689554,
55.2269250276648));
#169815=CARTESIAN_POINT('Ctrl Pts',(81.7823247749792,-3.84336265789555,
55.2298812216485));
#169816=CARTESIAN_POINT('Ctrl Pts',(81.7458112214872,-3.93069828419579,
55.2353111728736));
#169817=CARTESIAN_POINT('Ctrl Pts',(81.7294399786342,-3.96918443671297,
55.2377570416467));
#169818=CARTESIAN_POINT('Ctrl Pts',(81.6941074474136,-4.05083720985216,
55.2430592826185));
#169819=CARTESIAN_POINT('Ctrl Pts',(81.6750823900781,-4.09397430902961,
55.2459281832408));
#169820=CARTESIAN_POINT('Ctrl Pts',(81.6228218298127,-4.21026123399974,
55.2538454315186));
#169821=CARTESIAN_POINT('Ctrl Pts',(81.5890181752935,-4.28314420858446,
55.2590052344547));
#169822=CARTESIAN_POINT('Ctrl Pts',(81.3863203953756,-4.70686969538077,
55.2901599628658));
#169823=CARTESIAN_POINT('Ctrl Pts',(81.1982511699067,-5.04788308417159,
55.3199254042824));
#169824=CARTESIAN_POINT('Ctrl Pts',(80.7954080428616,-5.68761772188648,
55.3847075617269));
#169825=CARTESIAN_POINT('Ctrl Pts',(80.5830110594757,-5.98714289113689,
55.4192868711626));
#169826=CARTESIAN_POINT('Ctrl Pts',(80.2202137598613,-6.44331288287155,
55.478389073045));
#169827=CARTESIAN_POINT('Ctrl Pts',(80.0802347356817,-6.60803030250808,
55.5011971696345));
#169828=CARTESIAN_POINT('Ctrl Pts',(79.8784750202396,-6.83033916260853,
55.5339436495727));
#169829=CARTESIAN_POINT('Ctrl Pts',(79.8211125931903,-6.89195185312143,
55.543240172835));
#169830=CARTESIAN_POINT('Ctrl Pts',(79.7391358283428,-6.97778655058047,
55.5564980926484));
#169831=CARTESIAN_POINT('Ctrl Pts',(79.7151615050614,-7.00262820513807,
55.5603721350819));
#169832=CARTESIAN_POINT('Ctrl Pts',(79.6744629507664,-7.04436076701493,
55.5669424288867));
#169833=CARTESIAN_POINT('Ctrl Pts',(79.6578060748199,-7.06131839815295,
55.56962973432));
#169834=CARTESIAN_POINT('Ctrl Pts',(79.6230409417495,-7.09645750039703,
55.5752346088084));
#169835=CARTESIAN_POINT('Ctrl Pts',(79.604922928228,-7.11462871140889,55.5781534762829));
#169836=CARTESIAN_POINT('Ctrl Pts',(79.5567096977773,-7.16260941086454,
55.5859155760166));
#169837=CARTESIAN_POINT('Ctrl Pts',(79.5264948622572,-7.19229538279288,
55.590774695932));
#169838=CARTESIAN_POINT('Ctrl Pts',(79.3803538031251,-7.3340489100916,55.6142551348318));
#169839=CARTESIAN_POINT('Ctrl Pts',(79.2619225699825,-7.44344246608252,
55.6332183622152));
#169840=CARTESIAN_POINT('Ctrl Pts',(78.8816511477967,-7.77787932078961,
55.6940305091882));
#169841=CARTESIAN_POINT('Ctrl Pts',(78.6108053589414,-7.99204271404234,
55.7372408746047));
#169842=CARTESIAN_POINT('Ctrl Pts',(78.3039481208405,-8.20962589212828,
55.7864299336672));
#169843=CARTESIAN_POINT('Ctrl Pts',(78.2782804915427,-8.22764307286505,
55.7905460701455));
#169844=CARTESIAN_POINT('Ctrl Pts',(77.880172692812,-8.50427274301525,55.8544158078225));
#169845=CARTESIAN_POINT('Ctrl Pts',(77.4907942677911,-8.73684180465576,
55.9172955087661));
#169846=CARTESIAN_POINT('Ctrl Pts',(76.9925077600569,-8.98964335241288,
55.9986907256555));
#169847=CARTESIAN_POINT('Ctrl Pts',(76.8970699652099,-9.03613519547111,
56.014318683139));
#169848=CARTESIAN_POINT('Ctrl Pts',(76.753673447537,-9.10313756497479,56.0378584112176));
#169849=CARTESIAN_POINT('Ctrl Pts',(76.7062581816379,-9.12483413679376,
56.0456514046435));
#169850=CARTESIAN_POINT('Ctrl Pts',(76.6208858085757,-9.16307994958528,
56.0596997494516));
#169851=CARTESIAN_POINT('Ctrl Pts',(76.5829906678094,-9.17976942835726,
56.0659414448347));
#169852=CARTESIAN_POINT('Ctrl Pts',(76.5020194818393,-9.21481997950538,
56.0792907157792));
#169853=CARTESIAN_POINT('Ctrl Pts',(76.4589161739331,-9.23311312783332,
56.0864044248266));
#169854=CARTESIAN_POINT('Ctrl Pts',(76.3417111113945,-9.28186781259756,
56.1057679107776));
#169855=CARTESIAN_POINT('Ctrl Pts',(76.2673719603771,-9.31172780239573,
56.1180712060214));
#169856=CARTESIAN_POINT('Ctrl Pts',(75.8403759152482,-9.47718978747199,
56.1888598731825));
#169857=CARTESIAN_POINT('Ctrl Pts',(75.4807137943323,-9.59312044409277,
56.2489661600192));
#169858=CARTESIAN_POINT('Ctrl Pts',(74.5865826797033,-9.8250983877885,56.3990809817534));
#169859=CARTESIAN_POINT('Ctrl Pts',(74.047523912526,-9.91754541389785,56.4901918750426));
#169860=CARTESIAN_POINT('Ctrl Pts',(73.3031321300179,-9.98150847637653,
56.6150972981622));
#169861=CARTESIAN_POINT('Ctrl Pts',(73.102186028597,-9.99251000826106,56.6487182522762));
#169862=CARTESIAN_POINT('Ctrl Pts',(72.8567856408011,-9.99832056019788,
56.6895550734642));
#169863=CARTESIAN_POINT('Ctrl Pts',(72.8125438096882,-9.99906623277688,
56.6969084890224));
#169864=CARTESIAN_POINT('Ctrl Pts',(72.743271029061,-9.99976125388288,56.7084069744269));
#169865=CARTESIAN_POINT('Ctrl Pts',(72.7182437511166,-9.99991581248507,
56.7125580859481));
#169866=CARTESIAN_POINT('Ctrl Pts',(72.6718867547311,-10.0000232896589,
56.720240897245));
#169867=CARTESIAN_POINT('Ctrl Pts',(72.6505575666984,-10.0000026347173,
56.7237733825021));
#169868=CARTESIAN_POINT('Ctrl Pts',(72.6011101604298,-9.99979223162048,
56.7319571946038));
#169869=CARTESIAN_POINT('Ctrl Pts',(72.5729921321942,-9.99955075840802,
56.7366067565296));
#169870=CARTESIAN_POINT('Ctrl Pts',(72.4839986005901,-9.9984009009029,56.7513102993948));
#169871=CARTESIAN_POINT('Ctrl Pts',(72.4231278486966,-9.99704331373609,
56.7613491502423));
#169872=CARTESIAN_POINT('Ctrl Pts',(72.1056434015103,-9.98698291980609,
56.8136258094129));
#169873=CARTESIAN_POINT('Ctrl Pts',(71.8493801283175,-9.96870393054267,
56.8555406635842));
#169874=CARTESIAN_POINT('Ctrl Pts',(71.0099468825211,-9.87537234423317,
56.9924295681601));
#169875=CARTESIAN_POINT('Ctrl Pts',(70.4325720674018,-9.7576990451472,57.0860028999719));
#169876=CARTESIAN_POINT('Ctrl Pts',(69.6163526445126,-9.51290734268113,
57.2191566602303));
#169877=CARTESIAN_POINT('Ctrl Pts',(69.3667475312224,-9.42688894167878,
57.2599856399268));
#169878=CARTESIAN_POINT('Ctrl Pts',(69.0506988897274,-9.30344679008716,
57.311868061212));
#169879=CARTESIAN_POINT('Ctrl Pts',(68.9808489382277,-9.27523072093014,
57.3233461932567));
#169880=CARTESIAN_POINT('Ctrl Pts',(68.8690716619505,-9.22856941639705,
57.3417328252203));
#169881=CARTESIAN_POINT('Ctrl Pts',(68.8269395603865,-9.21063318741089,
57.3486676069018));
#169882=CARTESIAN_POINT('Ctrl Pts',(68.7467644712484,-9.17583496517369,
57.3618722991207));
#169883=CARTESIAN_POINT('Ctrl Pts',(68.7087004656476,-9.15902494469959,
57.3681449208736));
#169884=CARTESIAN_POINT('Ctrl Pts',(68.6215222449076,-9.11985887408198,
57.3825191540077));
#169885=CARTESIAN_POINT('Ctrl Pts',(68.5724820082497,-9.09733789313285,
57.3906109538339));
#169886=CARTESIAN_POINT('Ctrl Pts',(68.418729997444,-9.02518523672881,57.4159983973812));
#169887=CARTESIAN_POINT('Ctrl Pts',(68.3146989662436,-8.97409471314912,
57.4332023172028));
#169888=CARTESIAN_POINT('Ctrl Pts',(68.0716026032028,-8.84931051705981,
57.4734580635512));
#169889=CARTESIAN_POINT('Ctrl Pts',(67.9333420559465,-8.77408341770417,
57.4963963839914));
#169890=CARTESIAN_POINT('Ctrl Pts',(67.3908779586117,-8.4618010403139,57.5865107307297));
#169891=CARTESIAN_POINT('Ctrl Pts',(67.0017752889355,-8.19912903618128,
57.6514419458594));
#169892=CARTESIAN_POINT('Ctrl Pts',(66.4873295702514,-7.7957371799568,57.7367781668038));
#169893=CARTESIAN_POINT('Ctrl Pts',(66.3453773571203,-7.67787966963978,
57.7602608272079));
#169894=CARTESIAN_POINT('Ctrl Pts',(66.0855607086834,-7.44963538898656,
57.8030108968417));
#169895=CARTESIAN_POINT('Ctrl Pts',(65.9669543169776,-7.34021392474407,
57.8224299541468));
#169896=CARTESIAN_POINT('Ctrl Pts',(65.8194810921125,-7.19737679803652,
57.8463957810109));
#169897=CARTESIAN_POINT('Ctrl Pts',(65.7881517100808,-7.1666288793118,57.8514764132685));
#169898=CARTESIAN_POINT('Ctrl Pts',(65.7385891572439,-7.11734004022096,
57.8594953144461));
#169899=CARTESIAN_POINT('Ctrl Pts',(65.7202261268116,-7.09893519843986,
57.862462217087));
#169900=CARTESIAN_POINT('Ctrl Pts',(65.6851318310884,-7.06348522795356,
57.8681240855368));
#169901=CARTESIAN_POINT('Ctrl Pts',(65.668389702301,-7.04645168386884,57.8708214471548));
#169902=CARTESIAN_POINT('Ctrl Pts',(65.6280839667193,-7.00514915834031,
57.8773065011249));
#169903=CARTESIAN_POINT('Ctrl Pts',(65.6045811208325,-6.98081914027601,
57.8810808029697));
#169904=CARTESIAN_POINT('Ctrl Pts',(65.521961844959,-6.8944183850771,57.8943242595585));
#169905=CARTESIAN_POINT('Ctrl Pts',(65.463509824559,-6.83169549597652,57.9036494685014));
#169906=CARTESIAN_POINT('Ctrl Pts',(65.0759533240894,-6.40494408738154,
57.9652173088012));
#169907=CARTESIAN_POINT('Ctrl Pts',(64.7728440328764,-6.01744829571551,
58.0121126516977));
#169908=CARTESIAN_POINT('Ctrl Pts',(64.2340391880073,-5.21310548434183,
58.0945659873071));
#169909=CARTESIAN_POINT('Ctrl Pts',(63.9972270022942,-4.79858339243606,
58.1303310412948));
#169910=CARTESIAN_POINT('Ctrl Pts',(63.7551287009896,-4.29463608264552,
58.1667166652259));
#169911=CARTESIAN_POINT('Ctrl Pts',(63.7205342260945,-4.22031053671581,
58.1719096723079));
#169912=CARTESIAN_POINT('Ctrl Pts',(63.6671421450482,-4.10183465636789,
58.1799149056046));
#169913=CARTESIAN_POINT('Ctrl Pts',(63.6477475544268,-4.0579638398674,58.1828206796472));
#169914=CARTESIAN_POINT('Ctrl Pts',(63.6120706817561,-3.97567664707459,
58.1881619551793));
#169915=CARTESIAN_POINT('Ctrl Pts',(63.5957124681839,-3.93729510868763,
58.190609350044));
#169916=CARTESIAN_POINT('Ctrl Pts',(63.5596467454594,-3.85119360855982,
58.196001488352));
#169917=CARTESIAN_POINT('Ctrl Pts',(63.540066267015,-3.80342049946292,58.1989263388992));
#169918=CARTESIAN_POINT('Ctrl Pts',(63.4829614504212,-3.66098305369202,
58.20744826568));
#169919=CARTESIAN_POINT('Ctrl Pts',(63.4465008112283,-3.56588967069123,
58.2128785897505));
#169920=CARTESIAN_POINT('Ctrl Pts',(63.284725431708,-3.12404434226735,58.2369140044108));
#169921=CARTESIAN_POINT('Ctrl Pts',(63.1770057764588,-2.7710119260063,58.2527577501688));
#169922=CARTESIAN_POINT('Ctrl Pts',(62.9715179067535,-1.93655821366227,
58.2821140804204));
#169923=CARTESIAN_POINT('Ctrl Pts',(62.8889917412337,-1.45228515243556,
58.2931139426145));
#169924=CARTESIAN_POINT('Ctrl Pts',(62.8185609419714,-0.724513613636625,
58.2995354572268));
#169925=CARTESIAN_POINT('Ctrl Pts',(62.8038869612924,-0.484400027867834,
58.3000313765559));
#169926=CARTESIAN_POINT('Ctrl Pts',(62.796504011387,-0.197173501351806,
58.2985317688595));
#169927=CARTESIAN_POINT('Ctrl Pts',(62.7956227610553,-0.150340766037461,
58.2982208256383));
#169928=CARTESIAN_POINT('Ctrl Pts',(62.7947556468869,-0.077690223885297,
58.2976337926366));
#169929=CARTESIAN_POINT('Ctrl Pts',(62.7945454341098,-0.0518753922316298,
58.2974047057229));
#169930=CARTESIAN_POINT('Ctrl Pts',(62.7943952737771,-0.0173734758123369,
58.297070893174));
#169931=CARTESIAN_POINT('Ctrl Pts',(62.7943685479087,-0.00868672916154148,
58.2969845060308));
#169932=CARTESIAN_POINT('Ctrl Pts',(62.7943529015217,6.10048743283802E-11,
58.2968957709606));
#169933=CARTESIAN_POINT('Ctrl Pts',(62.7896316916575,-5.79826049313321E-11,
58.2701204592907));
#169934=CARTESIAN_POINT('Ctrl Pts',(62.7896560368138,-0.0135162054405685,
58.2702585275327));
#169935=CARTESIAN_POINT('Ctrl Pts',(62.7897075319756,-0.0270323637277315,
58.2703927630781));
#169936=CARTESIAN_POINT('Ctrl Pts',(62.7899503939444,-0.068773338415487,
58.2707954032247));
#169937=CARTESIAN_POINT('Ctrl Pts',(62.7902329888609,-0.0969975643424201,
58.2710508411162));
#169938=CARTESIAN_POINT('Ctrl Pts',(62.7914895794682,-0.185455098057772,
58.2717980112957));
#169939=CARTESIAN_POINT('Ctrl Pts',(62.7928842060982,-0.245681608635885,
58.27222911253));
#169940=CARTESIAN_POINT('Ctrl Pts',(62.8027670692509,-0.553516669642862,
58.2740250870666));
#169941=CARTESIAN_POINT('Ctrl Pts',(62.8198196832118,-0.800772308294341,
58.27411742739));
#169942=CARTESIAN_POINT('Ctrl Pts',(62.9161211585352,-1.7099521352087,58.2689787452707));
#169943=CARTESIAN_POINT('Ctrl Pts',(63.051523057112,-2.36415209218552,58.2543781182925));
#169944=CARTESIAN_POINT('Ctrl Pts',(63.3153768788678,-3.21011419768726,
58.2187127907996));
#169945=CARTESIAN_POINT('Ctrl Pts',(63.387727563575,-3.41803155528467,58.2085425026169));
#169946=CARTESIAN_POINT('Ctrl Pts',(63.4923558529088,-3.68986808904647,
58.1933466223143));
#169947=CARTESIAN_POINT('Ctrl Pts',(63.5186488455654,-3.75608876051431,
58.1894926708313));
#169948=CARTESIAN_POINT('Ctrl Pts',(63.562754995827,-3.86384528002755,58.1829716491946));
#169949=CARTESIAN_POINT('Ctrl Pts',(63.5801533094643,-3.90555303718801,
58.1803858908014));
#169950=CARTESIAN_POINT('Ctrl Pts',(63.6143958323984,-3.9861182813017,58.1752711946906));
#169951=CARTESIAN_POINT('Ctrl Pts',(63.6312059858349,-4.02498961629921,
58.1727489205827));
#169952=CARTESIAN_POINT('Ctrl Pts',(63.6711531772115,-4.11579397581618,
58.1667289253965));
#169953=CARTESIAN_POINT('Ctrl Pts',(63.6944839343718,-4.16763762685056,
58.1631931816089));
#169954=CARTESIAN_POINT('Ctrl Pts',(63.7728269862209,-4.33787576642266,
58.1512571571044));
#169955=CARTESIAN_POINT('Ctrl Pts',(63.8296847425617,-4.45538035961212,
58.1424950101607));
#169956=CARTESIAN_POINT('Ctrl Pts',(63.9721197247251,-4.73575072890804,
58.1203273884186));
#169957=CARTESIAN_POINT('Ctrl Pts',(64.0598888902517,-4.89741464014061,
58.1064945944065));
#169958=CARTESIAN_POINT('Ctrl Pts',(64.3181870159524,-5.34360087564587,
58.0653929460286));
#169959=CARTESIAN_POINT('Ctrl Pts',(64.498346247756,-5.62209543137918,58.0362848249265));
#169960=CARTESIAN_POINT('Ctrl Pts',(64.9253738032989,-6.2154764448889,57.9668946164429));
#169961=CARTESIAN_POINT('Ctrl Pts',(65.177942228068,-6.52543110269897,57.9256078756775));
#169962=CARTESIAN_POINT('Ctrl Pts',(65.4953116409186,-6.87025982320277,
57.8741417670288));
#169963=CARTESIAN_POINT('Ctrl Pts',(65.5428770849662,-6.92086489077495,
57.8664386989642));
#169964=CARTESIAN_POINT('Ctrl Pts',(65.6122928724757,-6.99318002316199,
57.8552169205603));
#169965=CARTESIAN_POINT('Ctrl Pts',(65.6337236303911,-7.01529876158576,
57.8517550988664));
#169966=CARTESIAN_POINT('Ctrl Pts',(65.6717032212638,-7.05413388840991,
57.8456253189166));
#169967=CARTESIAN_POINT('Ctrl Pts',(65.6882095547363,-7.07089230610177,
57.8429630033498));
#169968=CARTESIAN_POINT('Ctrl Pts',(65.7239608618288,-7.10693207814124,
57.8372005780922));
#169969=CARTESIAN_POINT('Ctrl Pts',(65.7432256460699,-7.12619281617151,
57.83409783931));
#169970=CARTESIAN_POINT('Ctrl Pts',(65.7978140033004,-7.18032156117973,
57.8253120762596));
#169971=CARTESIAN_POINT('Ctrl Pts',(65.8333185047889,-7.21500203850099,
57.8196049279966));
#169972=CARTESIAN_POINT('Ctrl Pts',(66.0884019481187,-7.46044856141768,
57.778643750801));
#169973=CARTESIAN_POINT('Ctrl Pts',(66.3172220096294,-7.66116574850118,
57.742115642975));
#169974=CARTESIAN_POINT('Ctrl Pts',(66.6741355235429,-7.94627937940034,
57.6850776785341));
#169975=CARTESIAN_POINT('Ctrl Pts',(66.795656771984,-8.0388274737182,57.6656484067713));
#169976=CARTESIAN_POINT('Ctrl Pts',(67.3416239536575,-8.43499482220052,
57.5782050164547));
#169977=CARTESIAN_POINT('Ctrl Pts',(67.7871769411349,-8.707259616821,57.5063956464762));
#169978=CARTESIAN_POINT('Ctrl Pts',(68.3458602876401,-8.99052198928067,
57.4151310169165));
#169979=CARTESIAN_POINT('Ctrl Pts',(68.4408221271113,-9.03676133096291,
57.3995805752955));
#169980=CARTESIAN_POINT('Ctrl Pts',(68.5836435478361,-9.1034786918692,57.3761349207657));
#169981=CARTESIAN_POINT('Ctrl Pts',(68.6309663536374,-9.12512849953856,
57.3683570320917));
#169982=CARTESIAN_POINT('Ctrl Pts',(68.7162379291058,-9.16332280182636,
57.3543251432075));
#169983=CARTESIAN_POINT('Ctrl Pts',(68.7541253512455,-9.18000613894365,
57.3480846627265));
#169984=CARTESIAN_POINT('Ctrl Pts',(68.835151048409,-9.21507459321868,57.3347262879021));
#169985=CARTESIAN_POINT('Ctrl Pts',(68.8783169946911,-9.23339079067513,
57.327602168644));
#169986=CARTESIAN_POINT('Ctrl Pts',(68.9958732099315,-9.28228056989534,
57.3081804450102));
#169987=CARTESIAN_POINT('Ctrl Pts',(69.0705032674212,-9.31224640300566,
57.2958287808511));
#169988=CARTESIAN_POINT('Ctrl Pts',(69.5039131815365,-9.48010684238259,
57.2239750843428));
#169989=CARTESIAN_POINT('Ctrl Pts',(69.8699434368651,-9.59761507769309,
57.1627944174484));
#169990=CARTESIAN_POINT('Ctrl Pts',(70.7046977800549,-9.81224566180213,
57.0226261791118));
#169991=CARTESIAN_POINT('Ctrl Pts',(71.1754823451742,-9.89702135037369,
56.943127860477));
#169992=CARTESIAN_POINT('Ctrl Pts',(71.9065629451082,-9.97374118967351,
56.8202660712687));
#169993=CARTESIAN_POINT('Ctrl Pts',(72.1635544045455,-9.99043491188369,
56.7771960619146));
#169994=CARTESIAN_POINT('Ctrl Pts',(72.4638390016225,-9.99799638053454,
56.7272129036606));
#169995=CARTESIAN_POINT('Ctrl Pts',(72.5067434441473,-9.99879282025211,
56.7200795451036));
#169996=CARTESIAN_POINT('Ctrl Pts',(72.5766435179477,-9.99962793240755,
56.7084726298045));
#169997=CARTESIAN_POINT('Ctrl Pts',(72.6036356969778,-9.99983810934053,
56.7039941645786));
#169998=CARTESIAN_POINT('Ctrl Pts',(72.6520740561749,-10.0000137668606,
56.6959642467719));
#169999=CARTESIAN_POINT('Ctrl Pts',(72.6735194957356,-10.0000206630978,
56.6924115360003));
#170000=CARTESIAN_POINT('Ctrl Pts',(72.7209331498144,-9.99987922188316,
56.6845622711482));
#170001=CARTESIAN_POINT('Ctrl Pts',(72.7469010484595,-9.99969784750455,
56.6802668674492));
#170002=CARTESIAN_POINT('Ctrl Pts',(72.8227959306771,-9.99886406543161,
56.6677227668892));
#170003=CARTESIAN_POINT('Ctrl Pts',(72.8727205695597,-9.99793146535694,
56.6594835245592));
#170004=CARTESIAN_POINT('Ctrl Pts',(73.3758435726986,-9.98466117497393,
56.576563725556));
#170005=CARTESIAN_POINT('Ctrl Pts',(73.8278499941925,-9.94106877638808,
56.5029639906997));
#170006=CARTESIAN_POINT('Ctrl Pts',(74.8830774561407,-9.76438491859643,
56.3313547789217));
#170007=CARTESIAN_POINT('Ctrl Pts',(75.4801487879644,-9.60520653377018,
56.2343562112766));
#170008=CARTESIAN_POINT('Ctrl Pts',(76.1599006764834,-9.35309385969277,
56.1229326415212));
#170009=CARTESIAN_POINT('Ctrl Pts',(76.2606488274134,-9.31381502937074,
56.1063948971864));
#170010=CARTESIAN_POINT('Ctrl Pts',(76.4093722967137,-9.25297269280181,
56.0819462958496));
#170011=CARTESIAN_POINT('Ctrl Pts',(76.4578493448498,-9.23268351977169,
56.0739714743553));
#170012=CARTESIAN_POINT('Ctrl Pts',(76.5442655521862,-9.19569490465986,
56.0597452573067));
#170013=CARTESIAN_POINT('Ctrl Pts',(76.582265400249,-9.17914354506159,56.0534860212888));
#170014=CARTESIAN_POINT('Ctrl Pts',(76.662733897872,-9.14348473599334,56.0402240603206));
#170015=CARTESIAN_POINT('Ctrl Pts',(76.7051741766732,-9.12431440210388,
56.0332250944577));
#170016=CARTESIAN_POINT('Ctrl Pts',(76.8192088606804,-9.07182229533657,
56.0144076765153));
#170017=CARTESIAN_POINT('Ctrl Pts',(76.8905443574619,-9.03793411881336,
56.0026238439549));
#170018=CARTESIAN_POINT('Ctrl Pts',(77.294379380416,-8.8400726263574,55.9358490144783));
#170019=CARTESIAN_POINT('Ctrl Pts',(77.6179324326154,-8.65812295719163,
55.8820784201954));
#170020=CARTESIAN_POINT('Ctrl Pts',(78.3568205450506,-8.18570995922695,
55.7591205998082));
#170021=CARTESIAN_POINT('Ctrl Pts',(78.7617517939312,-7.88053094833642,
55.691587052926));
#170022=CARTESIAN_POINT('Ctrl Pts',(79.2595628825674,-7.44176684154383,
55.6097044574082));
#170023=CARTESIAN_POINT('Ctrl Pts',(79.3746489419549,-7.33539418497803,
55.5908668217293));
#170024=CARTESIAN_POINT('Ctrl Pts',(79.5184516421845,-7.19604766322438,
55.5674992029213));
#170025=CARTESIAN_POINT('Ctrl Pts',(79.5494841927515,-7.16558071303746,
55.5624669976062));
#170026=CARTESIAN_POINT('Ctrl Pts',(79.5986880010373,-7.11663802463973,
55.5545064441688));
#170027=CARTESIAN_POINT('Ctrl Pts',(79.6169859080969,-7.09829497280259,
55.5515501662155));
#170028=CARTESIAN_POINT('Ctrl Pts',(79.6520420155991,-7.06287781121129,
55.5458946322542));
#170029=CARTESIAN_POINT('Ctrl Pts',(79.6688103981895,-7.0458145758536,55.5431931310169));
#170030=CARTESIAN_POINT('Ctrl Pts',(79.7092992155928,-7.00431669816306,
55.5366788472391));
#170031=CARTESIAN_POINT('Ctrl Pts',(79.7329574480326,-6.97981957529539,
55.5328797719419));
#170032=CARTESIAN_POINT('Ctrl Pts',(79.8167546461673,-6.89215860614009,
55.5194482893337));
#170033=CARTESIAN_POINT('Ctrl Pts',(79.8762029944654,-6.82831717449719,
55.5099654624862));
#170034=CARTESIAN_POINT('Ctrl Pts',(80.2654567943855,-6.39917042824931,
55.4481406223644));
#170035=CARTESIAN_POINT('Ctrl Pts',(80.5691244801292,-6.01030280750111,
55.4011696219501));
#170036=CARTESIAN_POINT('Ctrl Pts',(81.1059286353248,-5.20715384881265,
55.3190374995395));
#170037=CARTESIAN_POINT('Ctrl Pts',(81.3407739365141,-4.79559158778963,
55.2835699601268));
#170038=CARTESIAN_POINT('Ctrl Pts',(81.5813692407573,-4.29480132520669,
55.2474101480165));
#170039=CARTESIAN_POINT('Ctrl Pts',(81.6159819879548,-4.22043965619088,
55.2422143900577));
#170040=CARTESIAN_POINT('Ctrl Pts',(81.6693956263758,-4.10191913313227,
55.2342059164948));
#170041=CARTESIAN_POINT('Ctrl Pts',(81.6887942776036,-4.05804016770877,
55.2312995314776));
#170042=CARTESIAN_POINT('Ctrl Pts',(81.7244750411608,-3.9757456640287,55.2259576692539));
#170043=CARTESIAN_POINT('Ctrl Pts',(81.7408332130592,-3.9373650215457,55.2235102786188));
#170044=CARTESIAN_POINT('Ctrl Pts',(81.776894506749,-3.85127593701282,55.2181187978181));
#170045=CARTESIAN_POINT('Ctrl Pts',(81.7964707630272,-3.80351441661973,
55.2151945746701));
#170046=CARTESIAN_POINT('Ctrl Pts',(81.8535494830644,-3.66114671806651,
55.2066765301363));
#170047=CARTESIAN_POINT('Ctrl Pts',(81.8899898239298,-3.56611211345595,
55.2012492136946));
#170048=CARTESIAN_POINT('Ctrl Pts',(82.0515992273742,-3.12476080096068,
55.1772383375035));
#170049=CARTESIAN_POINT('Ctrl Pts',(82.1592191029732,-2.77217906562558,
55.1614089315373));
#170050=CARTESIAN_POINT('Ctrl Pts',(82.36570613699,-1.93426587403167,55.1319065367559));
#170051=CARTESIAN_POINT('Ctrl Pts',(82.4487044914181,-1.44593827026146,
55.1208490837898));
#170052=CARTESIAN_POINT('Ctrl Pts',(82.5184624369535,-0.717290300203294,
55.1145636378729));
#170053=CARTESIAN_POINT('Ctrl Pts',(82.5328076145551,-0.480419027492485,
55.1141011166423));
#170054=CARTESIAN_POINT('Ctrl Pts',(82.5400830901692,-0.196583885451342,
55.1155871992899));
#170055=CARTESIAN_POINT('Ctrl Pts',(82.5409593326823,-0.149890911920435,
55.1158977099975));
#170056=CARTESIAN_POINT('Ctrl Pts',(82.5418222043871,-0.0774114079091971,
55.1164838218244));
#170057=CARTESIAN_POINT('Ctrl Pts',(82.542031498269,-0.0516278227723996,
55.1167127713156));
#170058=CARTESIAN_POINT('Ctrl Pts',(82.5422374743968,-0.00406986241077593,
55.117173116348));
#170059=CARTESIAN_POINT('Ctrl Pts',(82.5422621641968,0.0177040968224466,
55.1173986213876));
#170060=CARTESIAN_POINT('Ctrl Pts',(82.5421594085252,0.067502478009366,
55.1179480115738));
#170061=CARTESIAN_POINT('Ctrl Pts',(82.5419862478804,0.0955264069625877,
55.1182815174849));
#170062=CARTESIAN_POINT('Ctrl Pts',(82.5410884065857,0.182727385267187,
55.1193943434771));
#170063=CARTESIAN_POINT('Ctrl Pts',(82.5399646040612,0.24189799222242,55.1202570439598));
#170064=CARTESIAN_POINT('Ctrl Pts',(82.5284537721331,0.657481339120658,
55.127058210742));
#170065=CARTESIAN_POINT('Ctrl Pts',(82.4999028638073,1.01307791450742,55.1367050025745));
#170066=CARTESIAN_POINT('Ctrl Pts',(82.3693581444211,1.99061937926038,55.1727907434886));
#170067=CARTESIAN_POINT('Ctrl Pts',(82.2280915529031,2.60540559057014,55.2062710267115));
#170068=CARTESIAN_POINT('Ctrl Pts',(81.9790179784828,3.35843425536561,55.2596607528521));
#170069=CARTESIAN_POINT('Ctrl Pts',(81.9236286927221,3.51308753212645,55.2713228690378));
#170070=CARTESIAN_POINT('Ctrl Pts',(81.8414556958688,3.72594593875938,55.2883452535917));
#170071=CARTESIAN_POINT('Ctrl Pts',(81.8178529871186,3.7853900947735,55.2932061671777));
#170072=CARTESIAN_POINT('Ctrl Pts',(81.7788519556088,3.88094466827754,55.3011935461263));
#170073=CARTESIAN_POINT('Ctrl Pts',(81.7638051168413,3.91720114435001,55.3042649178868));
#170074=CARTESIAN_POINT('Ctrl Pts',(81.7320016400795,3.9925823682761,55.3107357674994));
#170075=CARTESIAN_POINT('Ctrl Pts',(81.7152081887932,4.03169022845718,55.3141409961434));
#170076=CARTESIAN_POINT('Ctrl Pts',(81.6747815137863,4.12420665607056,55.3223113736718));
#170077=CARTESIAN_POINT('Ctrl Pts',(81.6509308844624,4.17751547634108,55.3271105516552));
#170078=CARTESIAN_POINT('Ctrl Pts',(81.5682003551724,4.35817921792623,55.3436879950985));
#170079=CARTESIAN_POINT('Ctrl Pts',(81.5071263502993,4.48447901614293,55.355810095591));
#170080=CARTESIAN_POINT('Ctrl Pts',(81.3511528490271,4.79046998160984,55.3865136163936));
#170081=CARTESIAN_POINT('Ctrl Pts',(81.2534157799658,4.96859735987704,55.4055433672032));
#170082=CARTESIAN_POINT('Ctrl Pts',(80.9851819307598,5.42402265031676,55.4573442314821));
#170083=CARTESIAN_POINT('Ctrl Pts',(80.8065134062264,5.69606906909182,55.4914455289004));
#170084=CARTESIAN_POINT('Ctrl Pts',(80.3967337304052,6.25818605272208,55.5693431935936));
#170085=CARTESIAN_POINT('Ctrl Pts',(80.1621039954986,6.5449929738467,55.6137668227995));
#170086=CARTESIAN_POINT('Ctrl Pts',(79.8652577993506,6.86921362961989,55.6703321294969));
#170087=CARTESIAN_POINT('Ctrl Pts',(79.8176462414156,6.9201306466871,55.6794152288931));
#170088=CARTESIAN_POINT('Ctrl Pts',(79.7482426718977,6.99280623729642,55.692675888029));
#170089=CARTESIAN_POINT('Ctrl Pts',(79.7268701895026,7.01497914300828,55.6967621478398));
#170090=CARTESIAN_POINT('Ctrl Pts',(79.689028522474,7.05387474754867,55.7040024995843));
#170091=CARTESIAN_POINT('Ctrl Pts',(79.6726016416218,7.07063992037553,55.7071472615729));
#170092=CARTESIAN_POINT('Ctrl Pts',(79.6370636557936,7.10665370053121,55.7139545963237));
#170093=CARTESIAN_POINT('Ctrl Pts',(79.6179333442399,7.12588201297431,55.717621405733));
#170094=CARTESIAN_POINT('Ctrl Pts',(79.5638236424908,7.17982516049554,55.7279990097966));
#170095=CARTESIAN_POINT('Ctrl Pts',(79.5286679709258,7.21435457459367,55.7347485820397));
#170096=CARTESIAN_POINT('Ctrl Pts',(79.2806318909866,7.45436781747725,55.7824104906476));
#170097=CARTESIAN_POINT('Ctrl Pts',(79.0590916404481,7.65031679717258,55.8251877210789));
#170098=CARTESIAN_POINT('Ctrl Pts',(78.6855425032289,7.95191588266032,55.8972625421681));
#170099=CARTESIAN_POINT('Ctrl Pts',(78.5386494144109,8.06383570001938,55.9255934010245));
#170100=CARTESIAN_POINT('Ctrl Pts',(77.9857252992693,8.46098497094117,56.0320252309737));
#170101=CARTESIAN_POINT('Ctrl Pts',(77.5617691642608,8.71914883231862,56.1131883450019));
#170102=CARTESIAN_POINT('Ctrl Pts',(77.0270211150753,8.99132431623913,56.214442476174));
#170103=CARTESIAN_POINT('Ctrl Pts',(76.9328991340914,9.03733379015971,56.232226779589));
#170104=CARTESIAN_POINT('Ctrl Pts',(76.7911937366267,9.10379148725305,56.2589442000974));
#170105=CARTESIAN_POINT('Ctrl Pts',(76.744148715745,9.12539858463339,56.2678048108245));
#170106=CARTESIAN_POINT('Ctrl Pts',(76.6593118972396,9.16354591623723,56.2837664202998));
#170107=CARTESIAN_POINT('Ctrl Pts',(76.6215817979544,9.18022371872653,56.2908592176795));
#170108=CARTESIAN_POINT('Ctrl Pts',(76.5408231107731,9.21530890529264,56.306028269109));
#170109=CARTESIAN_POINT('Ctrl Pts',(76.4977660082422,9.23364645062245,56.3141081874362));
#170110=CARTESIAN_POINT('Ctrl Pts',(76.3803325595405,9.28266137018431,56.3361248906341));
#170111=CARTESIAN_POINT('Ctrl Pts',(76.3057101334162,9.31272522592874,56.3500931761443));
#170112=CARTESIAN_POINT('Ctrl Pts',(75.8677429585852,9.48288271822146,56.4319498893773));
#170113=CARTESIAN_POINT('Ctrl Pts',(75.4967672066577,9.60189231068149,56.5007695016574));
#170114=CARTESIAN_POINT('Ctrl Pts',(74.6190035087891,9.82627414220338,56.6629255858309));
#170115=CARTESIAN_POINT('Ctrl Pts',(74.1090010404577,9.9139791814594,56.7566193574042));
#170116=CARTESIAN_POINT('Ctrl Pts',(73.3821043927746,9.97982027830171,56.8909620903642));
#170117=CARTESIAN_POINT('Ctrl Pts',(73.1689767994582,9.99203300209417,56.9304551465251));
#170118=CARTESIAN_POINT('Ctrl Pts',(72.9108781725562,9.99826499384839,56.9785305129153));
#170119=CARTESIAN_POINT('Ctrl Pts',(72.8660864449013,9.9990350127156,56.9868828604909));
#170120=CARTESIAN_POINT('Ctrl Pts',(72.7961966441963,9.9997505189866,56.9999310520931));
#170121=CARTESIAN_POINT('Ctrl Pts',(72.7711000501385,9.99990968278211,57.0046196784292));
#170122=CARTESIAN_POINT('Ctrl Pts',(72.7245706896034,10.000023516907,57.0133186662311));
#170123=CARTESIAN_POINT('Ctrl Pts',(72.7031381657225,10.0000046453583,57.017328106088));
#170124=CARTESIAN_POINT('Ctrl Pts',(72.6538099972462,9.99979709104262,57.0265616795334));
#170125=CARTESIAN_POINT('Ctrl Pts',(72.6259151227576,9.99955890718432,57.031787332499));
#170126=CARTESIAN_POINT('Ctrl Pts',(72.5380082847686,9.99842753651006,57.0482674696931));
#170127=CARTESIAN_POINT('Ctrl Pts',(72.4780056813453,9.99709594715378,57.0595342623081));
#170128=CARTESIAN_POINT('Ctrl Pts',(72.1678310260054,9.9873196631852,57.1178574717189));
#170129=CARTESIAN_POINT('Ctrl Pts',(71.9180754197389,9.96971219509977,57.1650910686456));
#170130=CARTESIAN_POINT('Ctrl Pts',(71.0949147371838,9.87942124999785,57.3211753669735));
#170131=CARTESIAN_POINT('Ctrl Pts',(70.5272285833151,9.76499279507884,57.4294072747857));
#170132=CARTESIAN_POINT('Ctrl Pts',(69.709555302367,9.52242286805878,57.5844563228087));
#170133=CARTESIAN_POINT('Ctrl Pts',(69.449809219873,9.43322358138652,57.6335928422547));
#170134=CARTESIAN_POINT('Ctrl Pts',(69.123153735291,9.30534335455554,57.6951851272823));
#170135=CARTESIAN_POINT('Ctrl Pts',(69.0525869852108,9.27675857013407,57.708478823019));
#170136=CARTESIAN_POINT('Ctrl Pts',(68.9400487320975,9.22962860307571,57.7296599863014));
#170137=CARTESIAN_POINT('Ctrl Pts',(68.8978680044398,9.21161260570685,57.737594559924));
#170138=CARTESIAN_POINT('Ctrl Pts',(68.8178424315244,9.17676250994397,57.7526398146157));
#170139=CARTESIAN_POINT('Ctrl Pts',(68.7799753955317,9.159984054687,57.7597554747274));
#170140=CARTESIAN_POINT('Ctrl Pts',(68.6935870036067,9.12104602755132,57.7759808751572));
#170141=CARTESIAN_POINT('Ctrl Pts',(68.6451358145953,9.09872760615646,57.7850751287797));
#170142=CARTESIAN_POINT('Ctrl Pts',(68.4945579049635,9.02786332643967,57.8133210033127));
#170143=CARTESIAN_POINT('Ctrl Pts',(68.3930688989171,8.97792949421522,57.8323332394945));
#170144=CARTESIAN_POINT('Ctrl Pts',(68.156792612989,8.85653796600411,57.8765433841998));
#170145=CARTESIAN_POINT('Ctrl Pts',(68.0227424250005,8.7836544029474,57.9015848552352));
#170146=CARTESIAN_POINT('Ctrl Pts',(67.5529805814227,8.5138251428777,57.9892385214302));
#170147=CARTESIAN_POINT('Ctrl Pts',(67.2270851262614,8.2998876278944,58.0498458996509));
#170148=CARTESIAN_POINT('Ctrl Pts',(66.6024224090205,7.83440640497587,58.166329045405));
#170149=CARTESIAN_POINT('Ctrl Pts',(66.3041566991107,7.58333536755529,58.2221142573581));
#170150=CARTESIAN_POINT('Ctrl Pts',(65.9709412225519,7.26723809998258,58.2852877854289));
#170151=CARTESIAN_POINT('Ctrl Pts',(65.9210449741039,7.21889309525724,58.2947720915488));
#170152=CARTESIAN_POINT('Ctrl Pts',(65.8497981041605,7.14838578179475,58.3083557289708));
#170153=CARTESIAN_POINT('Ctrl Pts',(65.8280388590372,7.12664997538445,58.3125098834334));
#170154=CARTESIAN_POINT('Ctrl Pts',(65.7898563794477,7.08815002738781,58.3198099923265));
#170155=CARTESIAN_POINT('Ctrl Pts',(65.7733911826969,7.07142897802047,58.3229614834389));
#170156=CARTESIAN_POINT('Ctrl Pts',(65.7380063528217,7.03523680009847,58.3297420081264));
#170157=CARTESIAN_POINT('Ctrl Pts',(65.7191069858698,7.01574588818218,58.3333683241492));
#170158=CARTESIAN_POINT('Ctrl Pts',(65.6660498163799,6.96057423594438,58.3435616133775));
#170159=CARTESIAN_POINT('Ctrl Pts',(65.6320768112236,6.92471230592477,58.3501037315673));
#170160=CARTESIAN_POINT('Ctrl Pts',(65.3941801561929,6.66978454220652,58.3960151122375));
#170161=CARTESIAN_POINT('Ctrl Pts',(65.1999126399328,6.44167428638077,58.4340268129339));
#170162=CARTESIAN_POINT('Ctrl Pts',(64.8953545935545,6.0494185559447,58.494129225884));
#170163=CARTESIAN_POINT('Ctrl Pts',(64.7791764599942,5.89024522052992,58.5171977332535));
#170164=CARTESIAN_POINT('Ctrl Pts',(64.3949240343878,5.32963174731759,58.5938173902111));
#170165=CARTESIAN_POINT('Ctrl Pts',(64.1510011920082,4.91187413749828,58.6430027651904));
#170166=CARTESIAN_POINT('Ctrl Pts',(63.8907038042634,4.38171435947856,58.6956908542953));
#170167=CARTESIAN_POINT('Ctrl Pts',(63.8450986501178,4.28496424950862,58.7049332183592));
#170168=CARTESIAN_POINT('Ctrl Pts',(63.7793845204544,4.13960006292655,58.7182660761189));
#170169=CARTESIAN_POINT('Ctrl Pts',(63.7581100322123,4.09154250133929,58.722585059913));
#170170=CARTESIAN_POINT('Ctrl Pts',(63.7206120703256,4.00501739563649,58.7302022026168));
#170171=CARTESIAN_POINT('Ctrl Pts',(63.7042508187716,3.96661331139702,58.7335273878648));
#170172=CARTESIAN_POINT('Ctrl Pts',(63.6698932217707,3.8845596669075,58.7405136426863));
#170173=CARTESIAN_POINT('Ctrl Pts',(63.651963444165,3.84088223479076,58.7441616501512));
#170174=CARTESIAN_POINT('Ctrl Pts',(63.6041854470681,3.72213077575406,58.7538887626634));
#170175=CARTESIAN_POINT('Ctrl Pts',(63.5749270371223,3.64681390896773,58.7598522213024));
#170176=CARTESIAN_POINT('Ctrl Pts',(63.4129784474172,3.21464798949199,58.7929039423211));
#170177=CARTESIAN_POINT('Ctrl Pts',(63.2995269445804,2.85064300111895,58.8162156015133));
#170178=CARTESIAN_POINT('Ctrl Pts',(63.0919972856453,2.02311697307081,58.8596972888563));
#170179=CARTESIAN_POINT('Ctrl Pts',(63.0092314806177,1.55759522967024,58.8777327922444));
#170180=CARTESIAN_POINT('Ctrl Pts',(62.9302613801214,0.815305549533786,
58.8976634002474));
#170181=CARTESIAN_POINT('Ctrl Pts',(62.9123390074276,0.541662011403782,
58.903155357785));
#170182=CARTESIAN_POINT('Ctrl Pts',(62.9043127956501,0.216805783682938,
58.9077169601091));
#170183=CARTESIAN_POINT('Ctrl Pts',(62.9034409778222,0.165998276538289,
58.9083738091881));
#170184=CARTESIAN_POINT('Ctrl Pts',(62.902750607283,0.0941525551497413,
58.9092245670084));
#170185=CARTESIAN_POINT('Ctrl Pts',(62.9026142197142,0.0731187293514479,
58.9094641778581));
#170186=CARTESIAN_POINT('Ctrl Pts',(62.9024852494696,0.0347198170549746,
58.9098845147619));
#170187=CARTESIAN_POINT('Ctrl Pts',(62.9024717297551,0.0173649150417452,
58.9100681158787));
#170188=CARTESIAN_POINT('Ctrl Pts',(62.9025030071408,2.40572005160039E-14,
58.910245498748));
#170189=CARTESIAN_POINT('Origin',(72.2537026314029,-4.33680868994202E-16,
54.3558290880045));
#170190=CARTESIAN_POINT('',(63.0200955324887,3.15100886788204E-11,59.5771458498765));
#170191=CARTESIAN_POINT('',(63.0153743226244,-1.95014612637774E-11,59.5503705382064));
#170192=CARTESIAN_POINT('',(62.4056251012807,-1.65832766814156E-15,56.0923108646735));
#170193=CARTESIAN_POINT('Ctrl Pts',(63.0200955324887,6.3021835685309E-11,
59.5771458498765));
#170194=CARTESIAN_POINT('Ctrl Pts',(63.0200725474665,0.0127610715955115,
59.5770154953381));
#170195=CARTESIAN_POINT('Ctrl Pts',(63.0200734724794,0.0255221090800886,
59.576880073832));
#170196=CARTESIAN_POINT('Ctrl Pts',(63.0201524332212,0.066088450096215,
59.5764335355938));
#170197=CARTESIAN_POINT('Ctrl Pts',(63.0203200911363,0.0938931878456895,
59.5761035105159));
#170198=CARTESIAN_POINT('Ctrl Pts',(63.0210563120057,0.166679807240136,
59.5751773968722));
#170199=CARTESIAN_POINT('Ctrl Pts',(63.0218085748546,0.211658719543653,
59.5745429231689));
#170200=CARTESIAN_POINT('Ctrl Pts',(63.0318781755434,0.643092600572684,
59.567868938244));
#170201=CARTESIAN_POINT('Ctrl Pts',(63.0628517303118,1.02865278076536,59.5573874701675));
#170202=CARTESIAN_POINT('Ctrl Pts',(63.1244481546801,1.47466085631702,59.5405490389491));
#170203=CARTESIAN_POINT('Ctrl Pts',(63.1337863823996,1.53786632840428,59.5380510306884));
#170204=CARTESIAN_POINT('Ctrl Pts',(63.2020388676492,1.97144933253191,59.5201581944454));
#170205=CARTESIAN_POINT('Ctrl Pts',(63.2808465391425,2.33825051061519,59.501233195767));
#170206=CARTESIAN_POINT('Ctrl Pts',(63.4345194487925,2.89938029904544,59.4667508594033));
#170207=CARTESIAN_POINT('Ctrl Pts',(63.4953438866782,3.09733408131394,59.4534788043003));
#170208=CARTESIAN_POINT('Ctrl Pts',(63.60869344673,3.42939836644478,59.4293569762587));
#170209=CARTESIAN_POINT('Ctrl Pts',(63.6580860047928,3.5645425751919,59.4190040033843));
#170210=CARTESIAN_POINT('Ctrl Pts',(63.731804417628,3.75355983427328,59.4037655723795));
#170211=CARTESIAN_POINT('Ctrl Pts',(63.7537414668091,3.8083751020046,59.3992549797151));
#170212=CARTESIAN_POINT('Ctrl Pts',(63.7923640705684,3.90246997818028,59.3913540242616));
#170213=CARTESIAN_POINT('Ctrl Pts',(63.8088201902371,3.94184501349841,59.3879996285045));
#170214=CARTESIAN_POINT('Ctrl Pts',(63.8408413783315,4.01711071388268,59.3814950190118));
#170215=CARTESIAN_POINT('Ctrl Pts',(63.8563664103702,4.05301809162716,59.3783510896961));
#170216=CARTESIAN_POINT('Ctrl Pts',(63.8934289989786,4.13738156008773,59.3708681323689));
#170217=CARTESIAN_POINT('Ctrl Pts',(63.9151406080702,4.18575744968697,59.3665018551243));
#170218=CARTESIAN_POINT('Ctrl Pts',(63.9927705024863,4.35511838983164,59.3509491532393));
#170219=CARTESIAN_POINT('Ctrl Pts',(64.0507046718079,4.47513439168626,59.3394467526492));
#170220=CARTESIAN_POINT('Ctrl Pts',(64.4036239622151,5.17047517097404,59.2699285699411));
#170221=CARTESIAN_POINT('Ctrl Pts',(64.7510267557267,5.71661901636454,59.2037523954328));
#170222=CARTESIAN_POINT('Ctrl Pts',(65.2702382611678,6.38104844216386,59.105195547197));
#170223=CARTESIAN_POINT('Ctrl Pts',(65.3970616580142,6.53371361209762,59.0811330238426));
#170224=CARTESIAN_POINT('Ctrl Pts',(65.6043998917974,6.76865856833162,59.0416941892472));
#170225=CARTESIAN_POINT('Ctrl Pts',(65.6819806544808,6.85355585452661,59.0269163799176));
#170226=CARTESIAN_POINT('Ctrl Pts',(65.786912671263,6.96446143353585,59.0068804632743));
#170227=CARTESIAN_POINT('Ctrl Pts',(65.8129905191862,6.99171158349314,59.0018972686762));
#170228=CARTESIAN_POINT('Ctrl Pts',(65.8563328032513,7.03648948561407,58.9936077571816));
#170229=CARTESIAN_POINT('Ctrl Pts',(65.8735101909773,7.05410449957666,58.9903206007854));
#170230=CARTESIAN_POINT('Ctrl Pts',(65.9060294875375,7.0872055493029,58.9840937279618));
#170231=CARTESIAN_POINT('Ctrl Pts',(65.9213575821644,7.10270551488825,58.981157091306));
#170232=CARTESIAN_POINT('Ctrl Pts',(65.9578844696464,7.1393996360552,58.9741555977358));
#170233=CARTESIAN_POINT('Ctrl Pts',(65.9791275021735,7.16054758509237,58.9700809589307));
#170234=CARTESIAN_POINT('Ctrl Pts',(66.054620891919,7.2350253742697,58.9555917550626));
#170235=CARTESIAN_POINT('Ctrl Pts',(66.1093774784722,7.28781675062998,58.9450666102771));
#170236=CARTESIAN_POINT('Ctrl Pts',(66.5271055983632,7.68137623445971,58.8646861741246));
#170237=CARTESIAN_POINT('Ctrl Pts',(66.9141798820333,7.99448239303505,58.7897578417173));
#170238=CARTESIAN_POINT('Ctrl Pts',(67.6560476066799,8.50668288704805,58.6471537347899));
#170239=CARTESIAN_POINT('Ctrl Pts',(68.0029144129277,8.71567093317399,58.5808209125774));
#170240=CARTESIAN_POINT('Ctrl Pts',(68.4721288828255,8.96000116052806,58.4918673758555));
#170241=CARTESIAN_POINT('Ctrl Pts',(68.5838254793688,9.01546452084471,58.4707447128195));
#170242=CARTESIAN_POINT('Ctrl Pts',(68.746635960045,9.09244628268166,58.4400352861272));
#170243=CARTESIAN_POINT('Ctrl Pts',(68.7969337125674,9.11570503057861,58.4305587995762));
#170244=CARTESIAN_POINT('Ctrl Pts',(68.8854225510539,9.15571012431528,58.4139056431212));
#170245=CARTESIAN_POINT('Ctrl Pts',(68.9235294953462,9.17264369028485,58.4067401664302));
#170246=CARTESIAN_POINT('Ctrl Pts',(69.0028875627831,9.20729858224362,58.391830532333));
#170247=CARTESIAN_POINT('Ctrl Pts',(69.0441545719024,9.22498019748003,58.3840843505093));
#170248=CARTESIAN_POINT('Ctrl Pts',(69.1515952660724,9.27013693690292,58.3639347322885));
#170249=CARTESIAN_POINT('Ctrl Pts',(69.2179491666316,9.29716580507235,58.3515081798939));
#170250=CARTESIAN_POINT('Ctrl Pts',(69.4977224032043,9.40753849723099,58.2991848456211));
#170251=CARTESIAN_POINT('Ctrl Pts',(69.7137035787971,9.48403241842706,58.2589680535346));
#170252=CARTESIAN_POINT('Ctrl Pts',(70.4659955958567,9.72086709788736,58.1193759273193));
#170253=CARTESIAN_POINT('Ctrl Pts',(71.0131274055265,9.84233992992407,58.0187520952213));
#170254=CARTESIAN_POINT('Ctrl Pts',(71.9076142730117,9.96105120379876,57.853835515361));
#170255=CARTESIAN_POINT('Ctrl Pts',(72.2499154079977,9.98806845090927,57.7906110908165));
#170256=CARTESIAN_POINT('Ctrl Pts',(72.6408216794739,9.99806751111475,57.717814278986));
#170257=CARTESIAN_POINT('Ctrl Pts',(72.6888405749281,9.99893776090644,57.7088615752299));
#170258=CARTESIAN_POINT('Ctrl Pts',(72.7623751522576,9.99972226265001,57.6951339437845));
#170259=CARTESIAN_POINT('Ctrl Pts',(72.7878889425738,9.99989341218551,57.6903676886638));
#170260=CARTESIAN_POINT('Ctrl Pts',(72.834791906369,10.0000222929586,57.6815993378657));
#170261=CARTESIAN_POINT('Ctrl Pts',(72.8561808303874,10.0000100498126,57.6775982866506));
#170262=CARTESIAN_POINT('Ctrl Pts',(72.9048981475929,9.99982040624204,57.668479578266));
#170263=CARTESIAN_POINT('Ctrl Pts',(72.9322257985338,9.99959807913916,57.6633605519435));
#170264=CARTESIAN_POINT('Ctrl Pts',(73.0037561063897,9.99871261001218,57.6499516970127));
#170265=CARTESIAN_POINT('Ctrl Pts',(73.0479548171807,9.99786201729911,57.6416565741571));
#170266=CARTESIAN_POINT('Ctrl Pts',(73.4099763817827,9.98840867005868,57.5736404734468));
#170267=CARTESIAN_POINT('Ctrl Pts',(73.7271459028565,9.96442351984042,57.5135977983781));
#170268=CARTESIAN_POINT('Ctrl Pts',(74.4504101346565,9.87365868581348,57.3763235104288));
#170269=CARTESIAN_POINT('Ctrl Pts',(74.8546426124419,9.79649047268983,57.2993521284652));
#170270=CARTESIAN_POINT('Ctrl Pts',(75.624078641156,9.59810386722078,57.1532135676406));
#170271=CARTESIAN_POINT('Ctrl Pts',(75.9894061101993,9.48042539736496,57.0839962767843));
#170272=CARTESIAN_POINT('Ctrl Pts',(76.421830377561,9.31230178869978,57.0024463705009));
#170273=CARTESIAN_POINT('Ctrl Pts',(76.4961996639025,9.28232466602108,56.9884344754596));
#170274=CARTESIAN_POINT('Ctrl Pts',(76.6133316644212,9.2334203758568,56.9663868419319));
#170275=CARTESIAN_POINT('Ctrl Pts',(76.6563342218514,9.21510171964711,56.9582970731907));
#170276=CARTESIAN_POINT('Ctrl Pts',(76.7370456058939,9.18003133349796,56.9431219147273));
#170277=CARTESIAN_POINT('Ctrl Pts',(76.7747821271544,9.16334864282998,56.9360303150169));
#170278=CARTESIAN_POINT('Ctrl Pts',(76.8597042814401,9.12515981145408,56.9200792332432));
#170279=CARTESIAN_POINT('Ctrl Pts',(76.9068286858055,9.10351495763508,56.9112332694498));
#170280=CARTESIAN_POINT('Ctrl Pts',(77.0490177255479,9.03682791653516,56.8845583340145));
#170281=CARTESIAN_POINT('Ctrl Pts',(77.1435467068324,8.99061527782845,56.866846542855));
#170282=CARTESIAN_POINT('Ctrl Pts',(77.6834509451405,8.71577609037926,56.7657979866849));
#170283=CARTESIAN_POINT('Ctrl Pts',(78.112011588744,8.4544617415982,56.6860828841022));
#170284=CARTESIAN_POINT('Ctrl Pts',(78.6646071992033,8.05645938193661,56.5831095517263));
#170285=CARTESIAN_POINT('Ctrl Pts',(78.8071940338766,7.94772210851001,56.5565151880089));
#170286=CARTESIAN_POINT('Ctrl Pts',(79.1765177655816,7.64975983644815,56.4874419441431));
#170287=CARTESIAN_POINT('Ctrl Pts',(79.3979494635795,7.45405364147757,56.4458325825213));
#170288=CARTESIAN_POINT('Ctrl Pts',(79.6457820614942,7.21432026774304,56.3987302495511));
#170289=CARTESIAN_POINT('Ctrl Pts',(79.6809386501648,7.17979880808279,56.3920351807516));
#170290=CARTESIAN_POINT('Ctrl Pts',(79.7350467617612,7.12586553635874,56.381708283254));
#170291=CARTESIAN_POINT('Ctrl Pts',(79.7541771939084,7.10663893262867,56.378052626661));
#170292=CARTESIAN_POINT('Ctrl Pts',(79.7897149771513,7.07062652718713,56.3712528637551));
#170293=CARTESIAN_POINT('Ctrl Pts',(79.8061418208554,7.05386099147639,56.3681061779679));
#170294=CARTESIAN_POINT('Ctrl Pts',(79.8439836437523,7.01496214691912,56.3608491094447));
#170295=CARTESIAN_POINT('Ctrl Pts',(79.8653556327152,6.99278636367774,56.3567444428635));
#170296=CARTESIAN_POINT('Ctrl Pts',(79.9347623082586,6.92009136902349,56.3433953463245));
#170297=CARTESIAN_POINT('Ctrl Pts',(79.982371018843,6.86915774106412,56.3342087701811));
#170298=CARTESIAN_POINT('Ctrl Pts',(80.2831316796237,6.54048824753826,56.2760020315854));
#170299=CARTESIAN_POINT('Ctrl Pts',(80.5210075049209,6.24879826543211,56.2291860027564));
#170300=CARTESIAN_POINT('Ctrl Pts',(80.98578074023,5.60788510940501,56.1369044189581));
#170301=CARTESIAN_POINT('Ctrl Pts',(81.208562615949,5.25645545567287,56.0921734593324));
#170302=CARTESIAN_POINT('Ctrl Pts',(81.4807659378698,4.7615137759443,56.0372790041854));
#170303=CARTESIAN_POINT('Ctrl Pts',(81.5495638146891,4.62956491761264,56.0233770716545));
#170304=CARTESIAN_POINT('Ctrl Pts',(81.6647007485787,4.39626213774363,56.000075169186));
#170305=CARTESIAN_POINT('Ctrl Pts',(81.7123217058328,4.29559588105244,55.9904252154799));
#170306=CARTESIAN_POINT('Ctrl Pts',(81.7803023764543,4.14550752139422,55.976633242519));
#170307=CARTESIAN_POINT('Ctrl Pts',(81.8019443117779,4.09669899714031,55.9722398626085));
#170308=CARTESIAN_POINT('Ctrl Pts',(81.8398498885169,4.00934711780903,55.9645402070295));
#170309=CARTESIAN_POINT('Ctrl Pts',(81.8562622940335,3.97087230805014,55.9612047501161));
#170310=CARTESIAN_POINT('Ctrl Pts',(81.890494070927,3.88922221549536,55.9542443416167));
#170311=CARTESIAN_POINT('Ctrl Pts',(81.908254331894,3.84602225758879,55.9506309892101));
#170312=CARTESIAN_POINT('Ctrl Pts',(81.9550388206692,3.72994120115857,55.9411066696293));
#170313=CARTESIAN_POINT('Ctrl Pts',(81.9835180311332,3.65683531215262,55.935302570212));
#170314=CARTESIAN_POINT('Ctrl Pts',(82.1162483636415,3.30402955169802,55.9082178837333));
#170315=CARTESIAN_POINT('Ctrl Pts',(82.2089887140146,3.01999254132958,55.8891936318053));
#170316=CARTESIAN_POINT('Ctrl Pts',(82.4410812536873,2.1857865052157,55.8410243035325));
#170317=CARTESIAN_POINT('Ctrl Pts',(82.5470843234707,1.62722091554012,55.8182696649173));
#170318=CARTESIAN_POINT('Ctrl Pts',(82.631757366863,0.811817315023689,55.7967190249472));
#170319=CARTESIAN_POINT('Ctrl Pts',(82.6484237067625,0.560224074816844,
55.7916328816616));
#170320=CARTESIAN_POINT('Ctrl Pts',(82.6574089882071,0.247521183882508,
55.7870555173154));
#170321=CARTESIAN_POINT('Ctrl Pts',(82.6586062479302,0.186777458460161,
55.7862477569346));
#170322=CARTESIAN_POINT('Ctrl Pts',(82.6595577826136,0.0977054394520253,
55.7851792375336));
#170323=CARTESIAN_POINT('Ctrl Pts',(82.6597411744399,0.0693838653862917,
55.7848566701605));
#170324=CARTESIAN_POINT('Ctrl Pts',(82.6598547850039,0.0192637541456681,
55.7843158126665));
#170325=CARTESIAN_POINT('Ctrl Pts',(82.6598335891773,-0.00253431925762405,
55.7840906022901));
#170326=CARTESIAN_POINT('Ctrl Pts',(82.6596340842985,-0.0499017624191425,
55.783622892004));
#170327=CARTESIAN_POINT('Ctrl Pts',(82.6594292367648,-0.0754707138692689,
55.7833841888325));
#170328=CARTESIAN_POINT('Ctrl Pts',(82.6585870595155,-0.146779261889534,
55.7827573272739));
#170329=CARTESIAN_POINT('Ctrl Pts',(82.6577360359873,-0.192515982101173,
55.7823998490237));
#170330=CARTESIAN_POINT('Ctrl Pts',(82.6509775435299,-0.458580943742663,
55.7805850650758));
#170331=CARTESIAN_POINT('Ctrl Pts',(82.638172332812,-0.678681116301826,
55.7801415042764));
#170332=CARTESIAN_POINT('Ctrl Pts',(82.5707444230845,-1.41962827553383,
55.7825446168574));
#170333=CARTESIAN_POINT('Ctrl Pts',(82.4829396886288,-1.93657489927633,
55.7907945584611));
#170334=CARTESIAN_POINT('Ctrl Pts',(82.2602112022678,-2.82560554272926,
55.8181788564529));
#170335=CARTESIAN_POINT('Ctrl Pts',(82.1426446438464,-3.20094752095467,
55.8340593003786));
#170336=CARTESIAN_POINT('Ctrl Pts',(81.974866658571,-3.64452544456632,55.858297746295));
#170337=CARTESIAN_POINT('Ctrl Pts',(81.9451355384252,-3.72035487614268,
55.8626396257654));
#170338=CARTESIAN_POINT('Ctrl Pts',(81.8966646676697,-3.83972519316476,
55.8697899598124));
#170339=CARTESIAN_POINT('Ctrl Pts',(81.8785254264841,-3.88351296676275,
55.8724807253108));
#170340=CARTESIAN_POINT('Ctrl Pts',(81.8438169628446,-3.9656628343147,55.8776568236605));
#170341=CARTESIAN_POINT('Ctrl Pts',(81.8273160220162,-4.0040535019679,55.8801287796844));
#170342=CARTESIAN_POINT('Ctrl Pts',(81.7895669762948,-4.09040186860476,
55.8858085047255));
#170343=CARTESIAN_POINT('Ctrl Pts',(81.7681834501694,-4.13829725373535,
55.8890428598873));
#170344=CARTESIAN_POINT('Ctrl Pts',(81.7023829678875,-4.28265291114649,
55.8990453721285));
#170345=CARTESIAN_POINT('Ctrl Pts',(81.6568245220118,-4.3785688757584,55.9060373910911));
#170346=CARTESIAN_POINT('Ctrl Pts',(81.3835434119711,-4.93127178930689,
55.9483376159127));
#170347=CARTESIAN_POINT('Ctrl Pts',(81.1231888358869,-5.37057415499867,
55.9900688843047));
#170348=CARTESIAN_POINT('Ctrl Pts',(80.7292983129638,-5.93276455048374,
56.0539816715363));
#170349=CARTESIAN_POINT('Ctrl Pts',(80.6239193981101,-6.07498988223039,
56.0711371189249));
#170350=CARTESIAN_POINT('Ctrl Pts',(80.3320179476734,-6.44782483159188,
56.1186854656449));
#170351=CARTESIAN_POINT('Ctrl Pts',(80.1389714699411,-6.67295649371278,
56.1501612972022));
#170352=CARTESIAN_POINT('Ctrl Pts',(79.9024408413115,-6.92504963604771,
56.1884673012694));
#170353=CARTESIAN_POINT('Ctrl Pts',(79.8683631238069,-6.96083022844835,
56.193980166324));
#170354=CARTESIAN_POINT('Ctrl Pts',(79.8151198219738,-7.01590419345922,
56.2025822919177));
#170355=CARTESIAN_POINT('Ctrl Pts',(79.7961378948207,-7.0353778390989,56.2056468850472));
#170356=CARTESIAN_POINT('Ctrl Pts',(79.7605820696068,-7.0715557042717,56.2113828529844));
#170357=CARTESIAN_POINT('Ctrl Pts',(79.744028267514,-7.08827955947311,56.2140515415401));
#170358=CARTESIAN_POINT('Ctrl Pts',(79.7056187609149,-7.12680824350938,
56.2202396132705));
#170359=CARTESIAN_POINT('Ctrl Pts',(79.6837208962468,-7.14856973018169,
56.2237645656928));
#170360=CARTESIAN_POINT('Ctrl Pts',(79.6119304288914,-7.21924953091756,
56.235312178609));
#170361=CARTESIAN_POINT('Ctrl Pts',(79.5616265976128,-7.26773812871635,
56.2433900861627));
#170362=CARTESIAN_POINT('Ctrl Pts',(79.2355482633924,-7.57546565443415,
56.2956877548929));
#170363=CARTESIAN_POINT('Ctrl Pts',(78.9457912405974,-7.81910045546643,
56.3418781368217));
#170364=CARTESIAN_POINT('Ctrl Pts',(78.3672991887962,-8.25151230180316,
56.4344443943366));
#170365=CARTESIAN_POINT('Ctrl Pts',(78.0811664485325,-8.44295338347043,
56.4803742384066));
#170366=CARTESIAN_POINT('Ctrl Pts',(77.5457400236712,-8.76202861299789,
56.5669744605854));
#170367=CARTESIAN_POINT('Ctrl Pts',(77.2997999197313,-8.89475760749457,
56.6069819412294));
#170368=CARTESIAN_POINT('Ctrl Pts',(76.9825100957221,-9.04893325464078,
56.6589472236596));
#170369=CARTESIAN_POINT('Ctrl Pts',(76.9159770924969,-9.08034395136983,
56.669862493727));
#170370=CARTESIAN_POINT('Ctrl Pts',(76.8078320754716,-9.12992211309388,
56.687634927693));
#170371=CARTESIAN_POINT('Ctrl Pts',(76.7664296728167,-9.14855628087697,
56.694446068824));
#170372=CARTESIAN_POINT('Ctrl Pts',(76.6867387936664,-9.18376037520967,
56.7075697147214));
#170373=CARTESIAN_POINT('Ctrl Pts',(76.648470388933,-9.20037492912495,56.7138778127472));
#170374=CARTESIAN_POINT('Ctrl Pts',(76.560570212029,-9.23787310215429,56.7283807479796));
#170375=CARTESIAN_POINT('Ctrl Pts',(76.5108722087848,-9.25859223283021,
56.73659046701));
#170376=CARTESIAN_POINT('Ctrl Pts',(76.3774642447571,-9.31292474763031,
56.7586544405836));
#170377=CARTESIAN_POINT('Ctrl Pts',(76.2934661056771,-9.34578995117681,
56.7725739189794));
#170378=CARTESIAN_POINT('Ctrl Pts',(75.5598594453791,-9.62120188052528,
56.8943670593408));
#170379=CARTESIAN_POINT('Ctrl Pts',(74.8874651900091,-9.7949782855156,57.0077064878314));
#170380=CARTESIAN_POINT('Ctrl Pts',(73.8159504270238,-9.95296389788093,
57.1881339633459));
#170381=CARTESIAN_POINT('Ctrl Pts',(73.4262027288345,-9.98662173994688,
57.2536810591757));
#170382=CARTESIAN_POINT('Ctrl Pts',(72.9864642559843,-9.99800712030206,
57.3268856743326));
#170383=CARTESIAN_POINT('Ctrl Pts',(72.9375097698522,-9.99890495110155,
57.335024665605));
#170384=CARTESIAN_POINT('Ctrl Pts',(72.8627839308599,-9.99971136128126,
57.3474301279833));
#170385=CARTESIAN_POINT('Ctrl Pts',(72.8370175548178,-9.99988708951038,
57.3517043836381));
#170386=CARTESIAN_POINT('Ctrl Pts',(72.7897945616622,-10.0000216248123,
57.3595315739047));
#170387=CARTESIAN_POINT('Ctrl Pts',(72.768338554275,-10.0000118088889,57.3630854475909));
#170388=CARTESIAN_POINT('Ctrl Pts',(72.7196523502409,-9.9998285654065,57.3711440875481));
#170389=CARTESIAN_POINT('Ctrl Pts',(72.6924223931206,-9.99961182395552,
57.3756473663842));
#170390=CARTESIAN_POINT('Ctrl Pts',(72.6214924366245,-9.99874962547304,
57.387368176853));
#170391=CARTESIAN_POINT('Ctrl Pts',(72.5777942269155,-9.99792415229429,
57.3945796331145));
#170392=CARTESIAN_POINT('Ctrl Pts',(72.2467762095126,-9.9894414168373,57.4491420010951));
#170393=CARTESIAN_POINT('Ctrl Pts',(71.9598441461565,-9.9693595767181,57.4960695289819));
#170394=CARTESIAN_POINT('Ctrl Pts',(71.6635196628818,-9.93539699957304,
57.5443796562413));
#170395=CARTESIAN_POINT('Ctrl Pts',(71.6528759737561,-9.93415931643981,
57.5461146976422));
#170396=CARTESIAN_POINT('Ctrl Pts',(71.2098765387747,-9.88190558132804,
57.6183202116018));
#170397=CARTESIAN_POINT('Ctrl Pts',(70.7812687173686,-9.80198862539112,
57.6878730205509));
#170398=CARTESIAN_POINT('Ctrl Pts',(69.9866093302135,-9.59800776372879,
57.8172338909326));
#170399=CARTESIAN_POINT('Ctrl Pts',(69.6197771053583,-9.4803630262814,57.8771180451826));
#170400=CARTESIAN_POINT('Ctrl Pts',(69.1856772115836,-9.31229090273862,
57.9483614319441));
#170401=CARTESIAN_POINT('Ctrl Pts',(69.1110067137023,-9.28231600601225,
57.9606293486214));
#170402=CARTESIAN_POINT('Ctrl Pts',(68.9934052907492,-9.23341455738645,
57.979971641371));
#170403=CARTESIAN_POINT('Ctrl Pts',(68.9502305585652,-9.21509638594357,
57.9870772703113));
#170404=CARTESIAN_POINT('Ctrl Pts',(68.8691976078222,-9.18002637846326,
58.0004220169187));
#170405=CARTESIAN_POINT('Ctrl Pts',(68.83131124957,-9.16334356079774,58.0066647701045));
#170406=CARTESIAN_POINT('Ctrl Pts',(68.7460528387754,-9.1251536564957,58.0207210911115));
#170407=CARTESIAN_POINT('Ctrl Pts',(68.6987429589574,-9.10350782765388,
58.028526418776));
#170408=CARTESIAN_POINT('Ctrl Pts',(68.5559936329689,-9.03681485324046,
58.0520936745828));
#170409=CARTESIAN_POINT('Ctrl Pts',(68.4610977555133,-8.99059696045416,
58.0677824928345));
#170410=CARTESIAN_POINT('Ctrl Pts',(67.9212161944057,-8.7167801821928,58.1571511796786));
#170411=CARTESIAN_POINT('Ctrl Pts',(67.4931056969342,-8.45680223914048,
58.2285056107748));
#170412=CARTESIAN_POINT('Ctrl Pts',(66.9384837795892,-8.05928162019742,
58.3207656067462));
#170413=CARTESIAN_POINT('Ctrl Pts',(66.7936749935322,-7.94931667603692,
58.3448302420551));
#170414=CARTESIAN_POINT('Ctrl Pts',(66.4212284288528,-7.64995766362703,
58.4065325495347));
#170415=CARTESIAN_POINT('Ctrl Pts',(66.1988104994536,-7.45416468378645,
58.4431848207273));
#170416=CARTESIAN_POINT('Ctrl Pts',(65.9497103543362,-7.2143324758635,58.483703747417));
#170417=CARTESIAN_POINT('Ctrl Pts',(65.9143811001581,-7.17980817286902,
58.4894371950452));
#170418=CARTESIAN_POINT('Ctrl Pts',(65.8600004773793,-7.12587140748161,
58.4982397389804));
#170419=CARTESIAN_POINT('Ctrl Pts',(65.840772802175,-7.10664419298143,58.5013476431137));
#170420=CARTESIAN_POINT('Ctrl Pts',(65.8050520235847,-7.07063130034372,
58.5071126807602));
#170421=CARTESIAN_POINT('Ctrl Pts',(65.7885397150802,-7.05386589427028,
58.5097740585185));
#170422=CARTESIAN_POINT('Ctrl Pts',(65.7504990403371,-7.01496819926987,
58.5158971397634));
#170423=CARTESIAN_POINT('Ctrl Pts',(65.7290130184311,-6.9927934443895,58.5193495129907));
#170424=CARTESIAN_POINT('Ctrl Pts',(65.659232842176,-6.92010530581626,58.5305429206518));
#170425=CARTESIAN_POINT('Ctrl Pts',(65.6113586508592,-6.86917761357063,
58.5381926513893));
#170426=CARTESIAN_POINT('Ctrl Pts',(65.3100123645777,-6.54179691289175,
58.5861739248146));
#170427=CARTESIAN_POINT('Ctrl Pts',(65.0715038219831,-6.25152202094488,
58.6233820631894));
#170428=CARTESIAN_POINT('Ctrl Pts',(64.6031266231701,-5.611218264681,58.6956468107223));
#170429=CARTESIAN_POINT('Ctrl Pts',(64.3776621958961,-5.25876457416573,
58.7299350072359));
#170430=CARTESIAN_POINT('Ctrl Pts',(64.1022822245504,-4.76250883216498,
58.7715743728875));
#170431=CARTESIAN_POINT('Ctrl Pts',(64.0327518383694,-4.6303510035834,58.7820603105359));
#170432=CARTESIAN_POINT('Ctrl Pts',(63.9164034921777,-4.39671328034927,
58.7995708322651));
#170433=CARTESIAN_POINT('Ctrl Pts',(63.8682899648765,-4.29592408523252,
58.8067998110784));
#170434=CARTESIAN_POINT('Ctrl Pts',(63.7996201879395,-4.14568765497114,
58.8171011345529));
#170435=CARTESIAN_POINT('Ctrl Pts',(63.7777692979185,-4.09685583444628,
58.8203764152899));
#170436=CARTESIAN_POINT('Ctrl Pts',(63.7395034391521,-4.00947809550287,
58.8261075068487));
#170437=CARTESIAN_POINT('Ctrl Pts',(63.7229383537878,-3.97100088051133,
58.8285868303989));
#170438=CARTESIAN_POINT('Ctrl Pts',(63.6883939566803,-3.88936227511663,
58.8337536198343));
#170439=CARTESIAN_POINT('Ctrl Pts',(63.6704739346249,-3.84617630472271,
58.8364318033698));
#170440=CARTESIAN_POINT('Ctrl Pts',(63.6232827182517,-3.73017334220863,
58.8434787435992));
#170441=CARTESIAN_POINT('Ctrl Pts',(63.5945589276684,-3.6571320789314,58.8477617194265));
#170442=CARTESIAN_POINT('Ctrl Pts',(63.4609496468839,-3.30536745325955,
58.8676504444353));
#170443=CARTESIAN_POINT('Ctrl Pts',(63.3675671683697,-3.02233787327736,
58.8814528823321));
#170444=CARTESIAN_POINT('Ctrl Pts',(63.1327154912277,-2.18824256650017,
58.9156148795403));
#170445=CARTESIAN_POINT('Ctrl Pts',(63.0250208122757,-1.62869950712594,
58.9305342332453));
#170446=CARTESIAN_POINT('Ctrl Pts',(62.9379234590289,-0.812159226565499,
58.9392625583131));
#170447=CARTESIAN_POINT('Ctrl Pts',(62.9205065379399,-0.5604315408587,58.9401852381982));
#170448=CARTESIAN_POINT('Ctrl Pts',(62.9104905284351,-0.247577749753939,
58.9389569323095));
#170449=CARTESIAN_POINT('Ctrl Pts',(62.9090885448431,-0.186818084566122,
58.93860734116));
#170450=CARTESIAN_POINT('Ctrl Pts',(62.9078284563691,-0.0977271282440349,
58.937928606089));
#170451=CARTESIAN_POINT('Ctrl Pts',(62.9075457140133,-0.0694025620102268,
58.9376882019774));
#170452=CARTESIAN_POINT('Ctrl Pts',(62.9073010701311,-0.0273849857570098,
58.9372947144178));
#170453=CARTESIAN_POINT('Ctrl Pts',(62.9072488797159,-0.0136925086044199,
58.9371606796013));
#170454=CARTESIAN_POINT('Ctrl Pts',(62.9072242170052,5.40442818497922E-11,
58.9370208104186));
#170455=CARTESIAN_POINT('Ctrl Pts',(62.9025030071408,2.40572005160039E-14,
58.910245498748));
#170456=CARTESIAN_POINT('Ctrl Pts',(62.9025342912689,-0.0173686582679938,
58.9104229198545));
#170457=CARTESIAN_POINT('Ctrl Pts',(62.9026103556841,-0.0347272718981202,
58.9105939150937));
#170458=CARTESIAN_POINT('Ctrl Pts',(62.9028777641638,-0.0731358798131149,
58.9109581633259));
#170459=CARTESIAN_POINT('Ctrl Pts',(62.9030900274107,-0.0941756765552429,
58.9111483321575));
#170460=CARTESIAN_POINT('Ctrl Pts',(62.9040397921087,-0.166048601348156,
58.9117656646191));
#170461=CARTESIAN_POINT('Ctrl Pts',(62.9050954046548,-0.216877140292341,
58.9121470526904));
#170462=CARTESIAN_POINT('Ctrl Pts',(62.9143026604179,-0.5419980837562,58.9142254053892));
#170463=CARTESIAN_POINT('Ctrl Pts',(62.9332410441641,-0.815880099105862,
58.9143284989985));
#170464=CARTESIAN_POINT('Ctrl Pts',(63.014969794944,-1.55827244014797,58.9096275643017));
#170465=CARTESIAN_POINT('Ctrl Pts',(63.09943809618,-2.02366545558728,58.9012098442081));
#170466=CARTESIAN_POINT('Ctrl Pts',(63.3100048167335,-2.85092599920466,
58.8751221496162));
#170467=CARTESIAN_POINT('Ctrl Pts',(63.4247916158072,-3.21480069270942,
58.8595719467266));
#170468=CARTESIAN_POINT('Ctrl Pts',(63.5883534277162,-3.64684082200208,
58.8359360258491));
#170469=CARTESIAN_POINT('Ctrl Pts',(63.6179001438503,-3.72215160646429,
58.8316202608708));
#170470=CARTESIAN_POINT('Ctrl Pts',(63.6661357363112,-3.84089593402397,
58.824503850265));
#170471=CARTESIAN_POINT('Ctrl Pts',(63.6842348233695,-3.8845720558084,58.8218187935395));
#170472=CARTESIAN_POINT('Ctrl Pts',(63.7189119915818,-3.96662458840719,
58.81664697183));
#170473=CARTESIAN_POINT('Ctrl Pts',(63.7354235084024,-4.00502883876494,
58.8141732468591));
#170474=CARTESIAN_POINT('Ctrl Pts',(63.7732617179863,-4.09155602479526,
58.8084796869005));
#170475=CARTESIAN_POINT('Ctrl Pts',(63.7947262317453,-4.13961553848542,
58.8052327949778));
#170476=CARTESIAN_POINT('Ctrl Pts',(63.8610200350821,-4.28499147354866,
58.7951542700602));
#170477=CARTESIAN_POINT('Ctrl Pts',(63.9070152812988,-4.38175165236982,
58.7880939786866));
#170478=CARTESIAN_POINT('Ctrl Pts',(64.1692392423258,-4.91150078674183,
58.7474959071995));
#170479=CARTESIAN_POINT('Ctrl Pts',(64.4146406270562,-5.32887623782263,
58.7082214426276));
#170480=CARTESIAN_POINT('Ctrl Pts',(64.8018013773615,-5.89030287614121,
58.6454642095547));
#170481=CARTESIAN_POINT('Ctrl Pts',(64.9195192906061,-6.05057757157698,
58.6263030524046));
#170482=CARTESIAN_POINT('Ctrl Pts',(65.2262870571687,-6.44313245235599,
58.5763340352565));
#170483=CARTESIAN_POINT('Ctrl Pts',(65.4210945266854,-6.67053695085696,
58.5445688959729));
#170484=CARTESIAN_POINT('Ctrl Pts',(65.6596317011368,-6.92479128899727,
58.5059376810256));
#170485=CARTESIAN_POINT('Ctrl Pts',(65.6937665975725,-6.96063418930786,
58.5004155368764));
#170486=CARTESIAN_POINT('Ctrl Pts',(65.747080158213,-7.01578291223961,58.4918020319176));
#170487=CARTESIAN_POINT('Ctrl Pts',(65.7660743654856,-7.03526978587571,
58.4887354471778));
#170488=CARTESIAN_POINT('Ctrl Pts',(65.8016399989601,-7.07145860285653,
58.4829978824889));
#170489=CARTESIAN_POINT('Ctrl Pts',(65.8181912067245,-7.08818030322966,
58.4803296049725));
#170490=CARTESIAN_POINT('Ctrl Pts',(65.8565776532105,-7.12668696804056,
58.4741452322619));
#170491=CARTESIAN_POINT('Ctrl Pts',(65.8784548819281,-7.1484287631162,58.4706235902747));
#170492=CARTESIAN_POINT('Ctrl Pts',(65.95010784568,-7.21897644402316,58.4590980524618));
#170493=CARTESIAN_POINT('Ctrl Pts',(66.0002926365253,-7.26735490810976,
58.4510392041551));
#170494=CARTESIAN_POINT('Ctrl Pts',(66.3264422016386,-7.5751941552042,58.3987296727815));
#170495=CARTESIAN_POINT('Ctrl Pts',(66.6164150449733,-7.81902438452433,
58.3525050495425));
#170496=CARTESIAN_POINT('Ctrl Pts',(67.2394907643446,-8.28474647656219,
58.2528047338209));
#170497=CARTESIAN_POINT('Ctrl Pts',(67.5735397682636,-8.5041999340286,58.1991521789296));
#170498=CARTESIAN_POINT('Ctrl Pts',(68.0540499006501,-8.77970114605355,
58.121252280052));
#170499=CARTESIAN_POINT('Ctrl Pts',(68.1901935791239,-8.85354907957623,
58.0991073914919));
#170500=CARTESIAN_POINT('Ctrl Pts',(68.4298920273864,-8.97633916261201,
58.0599758389674));
#170501=CARTESIAN_POINT('Ctrl Pts',(68.5326856563159,-9.02675085809725,
58.0431502382624));
#170502=CARTESIAN_POINT('Ctrl Pts',(68.6849427005484,-9.09814817447399,
58.0181611935353));
#170503=CARTESIAN_POINT('Ctrl Pts',(68.7337542152503,-9.12055066262303,
58.0101400960207));
#170504=CARTESIAN_POINT('Ctrl Pts',(68.8206739087486,-9.15958321890219,
57.9958390581626));
#170505=CARTESIAN_POINT('Ctrl Pts',(68.8587107372246,-9.17637463661734,
57.9895748390962));
#170506=CARTESIAN_POINT('Ctrl Pts',(68.9389814253069,-9.21120246816204,
57.9763427089367));
#170507=CARTESIAN_POINT('Ctrl Pts',(68.9812368555633,-9.22918479117664,
57.9693699374593));
#170508=CARTESIAN_POINT('Ctrl Pts',(69.0937049371064,-9.2761169259097,57.9507920647203));
#170509=CARTESIAN_POINT('Ctrl Pts',(69.1641236765312,-9.30454619076747,
57.939140528811));
#170510=CARTESIAN_POINT('Ctrl Pts',(69.4862920862339,-9.4302768968974,57.8857481274107));
#170511=CARTESIAN_POINT('Ctrl Pts',(69.7415477202365,-9.51792282889497,
57.843202957748));
#170512=CARTESIAN_POINT('Ctrl Pts',(70.5578155419666,-9.76094538690896,
57.7065771209657));
#170513=CARTESIAN_POINT('Ctrl Pts',(71.128860984443,-9.87668951302964,57.6100967183394));
#170514=CARTESIAN_POINT('Ctrl Pts',(71.960673633025,-9.96891279633525,57.4702511870423));
#170515=CARTESIAN_POINT('Ctrl Pts',(72.2156418465909,-9.98705241367056,
57.4274908907429));
#170516=CARTESIAN_POINT('Ctrl Pts',(72.5317680219692,-9.99705410672111,
57.3748134266249));
#170517=CARTESIAN_POINT('Ctrl Pts',(72.5924940441712,-9.9984063538746,57.3647099715857));
#170518=CARTESIAN_POINT('Ctrl Pts',(72.6813205044352,-9.99955242324994,
57.3499576255916));
#170519=CARTESIAN_POINT('Ctrl Pts',(72.7094116097431,-9.99979322436574,
57.3452961000567));
#170520=CARTESIAN_POINT('Ctrl Pts',(72.7588299662828,-10.0000028811811,
57.3371026915096));
#170521=CARTESIAN_POINT('Ctrl Pts',(72.7801564671796,-10.0000232682167,
57.3335692093946));
#170522=CARTESIAN_POINT('Ctrl Pts',(72.8265282793482,-9.99991520040572,
57.3258913849486));
#170523=CARTESIAN_POINT('Ctrl Pts',(72.8515733429144,-9.99976017905586,
57.3217479627198));
#170524=CARTESIAN_POINT('Ctrl Pts',(72.9209407289911,-9.99906311135047,
57.3102806329203));
#170525=CARTESIAN_POINT('Ctrl Pts',(72.9652615313968,-9.99831501398692,
57.3029636869536));
#170526=CARTESIAN_POINT('Ctrl Pts',(73.2120407645548,-9.99246377887463,
57.2622726676503));
#170527=CARTESIAN_POINT('Ctrl Pts',(73.4143411697187,-9.98134760084399,
57.2291019584791));
#170528=CARTESIAN_POINT('Ctrl Pts',(74.1590739731057,-9.91708696058708,
57.1073832542155));
#170529=CARTESIAN_POINT('Ctrl Pts',(74.6973353667004,-9.82477421979976,
57.0201282859161));
#170530=CARTESIAN_POINT('Ctrl Pts',(75.5909101085944,-9.5931600653227,56.8746506189172));
#170531=CARTESIAN_POINT('Ctrl Pts',(75.9508635486133,-9.47721678910531,
56.8158822677019));
#170532=CARTESIAN_POINT('Ctrl Pts',(76.3780410405796,-9.31173238424783,
56.7457738262313));
#170533=CARTESIAN_POINT('Ctrl Pts',(76.4523980563466,-9.28187149455451,
56.7335572648992));
#170534=CARTESIAN_POINT('Ctrl Pts',(76.5696211207097,-9.23311556292462,
56.7142770553058));
#170535=CARTESIAN_POINT('Ctrl Pts',(76.6127283574853,-9.21482221852788,
56.7071824875156));
#170536=CARTESIAN_POINT('Ctrl Pts',(76.6937025395623,-9.17977150395332,
56.6938473437002));
#170537=CARTESIAN_POINT('Ctrl Pts',(76.73159717781,-9.1630820797026,56.687603190084));
#170538=CARTESIAN_POINT('Ctrl Pts',(76.816964030267,-9.12483673414464,56.6735289078984));
#170539=CARTESIAN_POINT('Ctrl Pts',(76.8643733963188,-9.10314056843571,
56.6657071093106));
#170540=CARTESIAN_POINT('Ctrl Pts',(77.0077414827794,-9.03614085080102,
56.6420374941345));
#170541=CARTESIAN_POINT('Ctrl Pts',(77.1031493495533,-8.98965120953712,
56.6262637751262));
#170542=CARTESIAN_POINT('Ctrl Pts',(77.5995124876066,-8.73773245868233,
56.5440970859348));
#170543=CARTESIAN_POINT('Ctrl Pts',(77.9869522615415,-8.50627838538123,
56.4795728407288));
#170544=CARTESIAN_POINT('Ctrl Pts',(78.7331529385745,-7.98789563464108,
56.3553938402558));
#170545=CARTESIAN_POINT('Ctrl Pts',(79.0905424923617,-7.70087001339288,
56.2959741793573));
#170546=CARTESIAN_POINT('Ctrl Pts',(79.497765681327,-7.3247033024308,56.2293483485337));
#170547=CARTESIAN_POINT('Ctrl Pts',(79.5673634584594,-7.25852205814219,
56.2180040886079));
#170548=CARTESIAN_POINT('Ctrl Pts',(79.661262058269,-7.16661355164451,56.2027705859959));
#170549=CARTESIAN_POINT('Ctrl Pts',(79.6863834015439,-7.14176196039425,
56.1987022587048));
#170550=CARTESIAN_POINT('Ctrl Pts',(79.7284587820362,-7.09969401349658,
56.1919012511977));
#170551=CARTESIAN_POINT('Ctrl Pts',(79.745482044774,-7.08254977254455,56.1891532579657));
#170552=CARTESIAN_POINT('Ctrl Pts',(79.7803160489608,-7.04721272956597,
56.1835379142265));
#170553=CARTESIAN_POINT('Ctrl Pts',(79.7981198422834,-7.02901321619789,
56.1806720728125));
#170554=CARTESIAN_POINT('Ctrl Pts',(79.8447223321716,-6.98100920131469,
56.1731811584525));
#170555=CARTESIAN_POINT('Ctrl Pts',(79.8734074602198,-6.95109124997033,
56.1685810166465));
#170556=CARTESIAN_POINT('Ctrl Pts',(79.9950222400842,-6.82265977258022,
56.1491210942092));
#170557=CARTESIAN_POINT('Ctrl Pts',(80.0861598640805,-6.72241096163732,
56.1346461392179));
#170558=CARTESIAN_POINT('Ctrl Pts',(80.2544239170646,-6.52959413168857,
56.108086301528));
#170559=CARTESIAN_POINT('Ctrl Pts',(80.3319657344929,-6.4374320396065,56.0959170707031));
#170560=CARTESIAN_POINT('Ctrl Pts',(80.6939541038447,-5.99107850162928,
56.0393791190158));
#170561=CARTESIAN_POINT('Ctrl Pts',(80.9559994147831,-5.61888201167553,
55.9992509737802));
#170562=CARTESIAN_POINT('Ctrl Pts',(81.3664075105566,-4.94253295842123,
55.9368895665563));
#170563=CARTESIAN_POINT('Ctrl Pts',(81.5263213812908,-4.64644750119736,
55.9127664942475));
#170564=CARTESIAN_POINT('Ctrl Pts',(81.7046442838395,-4.2725370286962,55.8859732357997));
#170565=CARTESIAN_POINT('Ctrl Pts',(81.7373219096174,-4.20192092644069,
55.8810690142608));
#170566=CARTESIAN_POINT('Ctrl Pts',(81.7882576277528,-4.08841272845341,
55.8734332952313));
#170567=CARTESIAN_POINT('Ctrl Pts',(81.8070405218673,-4.04576526252089,
55.8706195698855));
#170568=CARTESIAN_POINT('Ctrl Pts',(81.842157498107,-3.96450525574626,55.8653627814097));
#170569=CARTESIAN_POINT('Ctrl Pts',(81.858547666924,-3.92591861480768,55.8629109327281));
#170570=CARTESIAN_POINT('Ctrl Pts',(81.895408490312,-3.83761013362202,55.8574007039593));
#170571=CARTESIAN_POINT('Ctrl Pts',(81.9157233945547,-3.7878231849306,55.854366716022));
#170572=CARTESIAN_POINT('Ctrl Pts',(81.9774692159133,-3.63296552248592,
55.8451544209256));
#170573=CARTESIAN_POINT('Ctrl Pts',(82.0175368826061,-3.52734839105768,
55.8391898560533));
#170574=CARTESIAN_POINT('Ctrl Pts',(82.24592031167,-2.89341059449705,55.8052889603103));
#170575=CARTESIAN_POINT('Ctrl Pts',(82.3917567001461,-2.35051118530748,
55.7839872145028));
#170576=CARTESIAN_POINT('Ctrl Pts',(82.525349966207,-1.613847614769,55.7661776652224));
#170577=CARTESIAN_POINT('Ctrl Pts',(82.5536618620599,-1.42865788028523,
55.7626177888971));
#170578=CARTESIAN_POINT('Ctrl Pts',(82.6179492638532,-0.913142139990253,
55.7553792079458));
#170579=CARTESIAN_POINT('Ctrl Pts',(82.6428772281945,-0.581656744058186,
55.7537386626833));
#170580=CARTESIAN_POINT('Ctrl Pts',(82.6528669907766,-0.201084493584069,
55.7556829203826));
#170581=CARTESIAN_POINT('Ctrl Pts',(82.6537938996066,-0.152604633247536,
55.7560017346494));
#170582=CARTESIAN_POINT('Ctrl Pts',(82.6546859107789,-0.0782442591020743,
55.7566016435419));
#170583=CARTESIAN_POINT('Ctrl Pts',(82.6548979563943,-0.0523670315677803,
55.7568310053257));
#170584=CARTESIAN_POINT('Ctrl Pts',(82.6551073110461,-0.0047241958240891,
55.7572915357648));
#170585=CARTESIAN_POINT('Ctrl Pts',(82.6551333942184,0.0170409902828053,
55.7575166520411));
#170586=CARTESIAN_POINT('Ctrl Pts',(82.6550341790086,0.0667067804927853,
55.758063890045));
#170587=CARTESIAN_POINT('Ctrl Pts',(82.6548641264406,0.0946068915860172,
55.7583954297706));
#170588=CARTESIAN_POINT('Ctrl Pts',(82.6541178920338,0.167809949977412,
55.7593280552602));
#170589=CARTESIAN_POINT('Ctrl Pts',(82.6533545310646,0.213109855960252,
55.7599682495316));
#170590=CARTESIAN_POINT('Ctrl Pts',(82.6442066695507,0.602154718065384,
55.7660004390248));
#170591=CARTESIAN_POINT('Ctrl Pts',(82.6187540126702,0.945218316972891,
55.7748949510362));
#170592=CARTESIAN_POINT('Ctrl Pts',(82.5265690674369,1.68002181989931,55.8009209666152));
#170593=CARTESIAN_POINT('Ctrl Pts',(82.4541356262684,2.07043194606314,55.8190848664116));
#170594=CARTESIAN_POINT('Ctrl Pts',(82.2656140061652,2.8331892824714,55.8625205332722));
#170595=CARTESIAN_POINT('Ctrl Pts',(82.1505203141465,3.20508695669689,55.8876162658754));
#170596=CARTESIAN_POINT('Ctrl Pts',(81.9858209027212,3.64520415645675,55.9219602953549));
#170597=CARTESIAN_POINT('Ctrl Pts',(81.9564512836613,3.72088125281246,55.9280375905523));
#170598=CARTESIAN_POINT('Ctrl Pts',(81.9085263432233,3.84006772535572,55.9378822178392));
#170599=CARTESIAN_POINT('Ctrl Pts',(81.8905723899394,3.8838227207945,55.9415552537532));
#170600=CARTESIAN_POINT('Ctrl Pts',(81.8561958915566,3.96594390355726,55.9485603325315));
#170601=CARTESIAN_POINT('Ctrl Pts',(81.8398415787454,4.00433844950523,55.951881671172));
#170602=CARTESIAN_POINT('Ctrl Pts',(81.8024007654925,4.09073877751059,55.9594604951477));
#170603=CARTESIAN_POINT('Ctrl Pts',(81.7811772146922,4.13868192326703,55.9637394245656));
#170604=CARTESIAN_POINT('Ctrl Pts',(81.7157816854263,4.28333403556716,55.9768734974031));
#170605=CARTESIAN_POINT('Ctrl Pts',(81.6704533624586,4.37949524045373,55.9859098094996));
#170606=CARTESIAN_POINT('Ctrl Pts',(81.392405257031,4.94582714483263,56.0409680083436));
#170607=CARTESIAN_POINT('Ctrl Pts',(81.1247994764948,5.39740610865565,56.0924276399303));
#170608=CARTESIAN_POINT('Ctrl Pts',(80.6404665156884,6.08525149804973,56.1846295327195));
#170609=CARTESIAN_POINT('Ctrl Pts',(80.4453478688704,6.33600141878482,56.2215985093296));
#170610=CARTESIAN_POINT('Ctrl Pts',(80.1714611855094,6.65529223623627,56.2736431613594));
#170611=CARTESIAN_POINT('Ctrl Pts',(80.102938218998,6.73270132713967,56.2866761225027));
#170612=CARTESIAN_POINT('Ctrl Pts',(79.9843873274947,6.862496079063,56.3092635089353));
#170613=CARTESIAN_POINT('Ctrl Pts',(79.934958889108,6.91543947332063,56.3186922082157));
#170614=CARTESIAN_POINT('Ctrl Pts',(79.863145954515,6.99069466959353,56.3324124766871));
#170615=CARTESIAN_POINT('Ctrl Pts',(79.8412172630735,7.01345618253948,56.3366049154377));
#170616=CARTESIAN_POINT('Ctrl Pts',(79.8027936208427,7.05296039309222,56.3439564659895));
#170617=CARTESIAN_POINT('Ctrl Pts',(79.7863461709483,7.06975082341103,56.3471050992447));
#170618=CARTESIAN_POINT('Ctrl Pts',(79.750903870796,7.10567641210136,56.353893973126));
#170619=CARTESIAN_POINT('Ctrl Pts',(79.7318908918214,7.12479239867154,56.3575382113221));
#170620=CARTESIAN_POINT('Ctrl Pts',(79.6793508285267,7.17718868482272,56.3676145299479));
#170621=CARTESIAN_POINT('Ctrl Pts',(79.645667040466,7.21030420375505,56.3740810894789));
#170622=CARTESIAN_POINT('Ctrl Pts',(79.4548278975932,7.39526226663255,56.4107488422979));
#170623=CARTESIAN_POINT('Ctrl Pts',(79.2930236368102,7.54202220522219,56.4419529715292));
#170624=CARTESIAN_POINT('Ctrl Pts',(78.7665629883177,7.98863151605013,56.5435304744943));
#170625=CARTESIAN_POINT('Ctrl Pts',(78.3855367794655,8.26741933616086,56.6170888762217));
#170626=CARTESIAN_POINT('Ctrl Pts',(77.7968388750445,8.63609731930965,56.7297712509923));
#170627=CARTESIAN_POINT('Ctrl Pts',(77.6034414638665,8.74816817762196,56.7666543607519));
#170628=CARTESIAN_POINT('Ctrl Pts',(77.2745049814969,8.92397698378391,56.8291011340283));
#170629=CARTESIAN_POINT('Ctrl Pts',(77.1409947007258,8.99143070836977,56.8543726086862));
#170630=CARTESIAN_POINT('Ctrl Pts',(76.952371607933,9.08133667158602,56.8899655143526));
#170631=CARTESIAN_POINT('Ctrl Pts',(76.8985005769538,9.10641111998939,56.9001185940377));
#170632=CARTESIAN_POINT('Ctrl Pts',(76.805823573605,9.14851946610285,56.9175642600107));
#170633=CARTESIAN_POINT('Ctrl Pts',(76.7671274819039,9.16579709438249,56.9248422123066));
#170634=CARTESIAN_POINT('Ctrl Pts',(76.6884239565763,9.20032273338006,56.9396320930603));
#170635=CARTESIAN_POINT('Ctrl Pts',(76.6484111517669,9.21755583147009,56.9471446752639));
#170636=CARTESIAN_POINT('Ctrl Pts',(76.5480441732338,9.25998543610024,56.9659727030585));
#170637=CARTESIAN_POINT('Ctrl Pts',(76.487551860372,9.2848416693542,56.9773058947809));
#170638=CARTESIAN_POINT('Ctrl Pts',(76.2623402264916,9.37473478142222,57.0194460009106));
#170639=CARTESIAN_POINT('Ctrl Pts',(76.0961338266892,9.43586305753576,57.0504400432094));
#170640=CARTESIAN_POINT('Ctrl Pts',(75.3537733601903,9.68606621061228,57.1884688740469));
#170641=CARTESIAN_POINT('Ctrl Pts',(74.7626083962399,9.8253428950092,57.2972227740556));
#170642=CARTESIAN_POINT('Ctrl Pts',(73.8202296514385,9.95589747587143,57.4709356885238));
#170643=CARTESIAN_POINT('Ctrl Pts',(73.4755939287353,9.98495018454923,57.534560246781));
#170644=CARTESIAN_POINT('Ctrl Pts',(73.0723052086547,9.99726578219294,57.6096063145284));
#170645=CARTESIAN_POINT('Ctrl Pts',(73.0143360141412,9.99851414849793,57.6204080133131));
#170646=CARTESIAN_POINT('Ctrl Pts',(72.928852687366,9.99958566903191,57.6363611368264));
#170647=CARTESIAN_POINT('Ctrl Pts',(72.9013423823041,9.99981302850819,57.6414989355973));
#170648=CARTESIAN_POINT('Ctrl Pts',(72.8524306804665,10.0000083972134,57.6506407332592));
#170649=CARTESIAN_POINT('Ctrl Pts',(72.831029474739,10.0000227845603,57.6546431420296));
#170650=CARTESIAN_POINT('Ctrl Pts',(72.7842542195342,9.99989883465852,57.663396355502));
#170651=CARTESIAN_POINT('Ctrl Pts',(72.7588807622356,9.99973164448181,57.6681480084801));
#170652=CARTESIAN_POINT('Ctrl Pts',(72.6874783543683,9.99897986318256,57.681528608682));
#170653=CARTESIAN_POINT('Ctrl Pts',(72.6414537367366,9.99816626338632,57.6901642078766));
#170654=CARTESIAN_POINT('Ctrl Pts',(72.3593295425278,9.99116158729582,57.7431586657038));
#170655=CARTESIAN_POINT('Ctrl Pts',(72.1235500244626,9.97664267091837,57.78770167283));
#170656=CARTESIAN_POINT('Ctrl Pts',(71.40840498152,9.90620628550892,57.9231933128778));
#170657=CARTESIAN_POINT('Ctrl Pts',(70.9324299634483,9.82299931367809,58.0138736950315));
#170658=CARTESIAN_POINT('Ctrl Pts',(70.1123819100195,9.61548347920324,58.1696493579154));
#170659=CARTESIAN_POINT('Ctrl Pts',(69.7655146378595,9.50665367784475,58.2353987178575));
#170660=CARTESIAN_POINT('Ctrl Pts',(69.3313178194179,9.34316708616744,58.3173486902701));
#170661=CARTESIAN_POINT('Ctrl Pts',(69.2378662466272,9.30631822157649,58.3349661940586));
#170662=CARTESIAN_POINT('Ctrl Pts',(69.0978815446895,9.2486020191161,58.3613244872542));
#170663=CARTESIAN_POINT('Ctrl Pts',(69.0509298242328,9.2288112867636,58.3701598043824));
#170664=CARTESIAN_POINT('Ctrl Pts',(68.9663066816261,9.19235730439304,58.3860743533869));
#170665=CARTESIAN_POINT('Ctrl Pts',(68.9285833913971,9.17582262596013,58.3931652134119));
#170666=CARTESIAN_POINT('Ctrl Pts',(68.8477058310117,9.1397601199923,58.4083603275334));
#170667=CARTESIAN_POINT('Ctrl Pts',(68.8045855847042,9.12015543506491,58.4164570663256));
#170668=CARTESIAN_POINT('Ctrl Pts',(68.6881339287258,9.06618364624091,58.4383111863728));
#170669=CARTESIAN_POINT('Ctrl Pts',(68.6150755822808,9.03121226622456,58.4520086564608));
#170670=CARTESIAN_POINT('Ctrl Pts',(68.1381466699981,8.7955792971828,58.5413464457309));
#170671=CARTESIAN_POINT('Ctrl Pts',(67.74771901752,8.56785444753638,58.6140683772073));
#170672=CARTESIAN_POINT('Ctrl Pts',(67.0970598350584,8.12548011414788,58.7352523955257));
#170673=CARTESIAN_POINT('Ctrl Pts',(66.829725500545,7.92301211440147,58.7850494681557));
#170674=CARTESIAN_POINT('Ctrl Pts',(66.3951885895302,7.55752403764773,58.8665169981539));
#170675=CARTESIAN_POINT('Ctrl Pts',(66.222574790196,7.40158626085029,58.8990365033695));
#170676=CARTESIAN_POINT('Ctrl Pts',(66.0219453491944,7.20700544304562,58.9371807612201));
#170677=CARTESIAN_POINT('Ctrl Pts',(65.988554097954,7.17415594591082,58.9435413493771));
#170678=CARTESIAN_POINT('Ctrl Pts',(65.9365678098929,7.12227888855382,58.9534649532022));
#170679=CARTESIAN_POINT('Ctrl Pts',(65.9178155000774,7.10341394175211,58.9570488906134));
#170680=CARTESIAN_POINT('Ctrl Pts',(65.8825753950237,7.06767407712765,58.9637925633479));
#170681=CARTESIAN_POINT('Ctrl Pts',(65.8660716930858,7.05081574958995,58.9669544065797));
#170682=CARTESIAN_POINT('Ctrl Pts',(65.8271370088832,7.01075796502635,58.97442210123));
#170683=CARTESIAN_POINT('Ctrl Pts',(65.8047584130837,6.98750667247541,58.9787209915102));
#170684=CARTESIAN_POINT('Ctrl Pts',(65.7298378535979,6.90889642073338,58.9931344948668));
#170685=CARTESIAN_POINT('Ctrl Pts',(65.6778174513365,6.85303114838828,59.0031780994776));
#170686=CARTESIAN_POINT('Ctrl Pts',(65.5518046664728,6.71452149583707,59.0275854351167));
#170687=CARTESIAN_POINT('Ctrl Pts',(65.478536450389,6.63121385909819,59.0418446087248));
#170688=CARTESIAN_POINT('Ctrl Pts',(65.1725478769838,6.27128075288447,59.1016355963843));
#170689=CARTESIAN_POINT('Ctrl Pts',(64.9534804948299,5.98306163370636,59.1450434458933));
#170690=CARTESIAN_POINT('Ctrl Pts',(64.489757352552,5.29864141497704,59.2375827581187));
#170691=CARTESIAN_POINT('Ctrl Pts',(64.2559932066147,4.89581537161776,59.2847227242312));
#170692=CARTESIAN_POINT('Ctrl Pts',(64.0036093063675,4.38178642825061,59.3358089667328));
#170693=CARTESIAN_POINT('Ctrl Pts',(63.9579943076422,4.28501715074904,59.3450533214539));
#170694=CARTESIAN_POINT('Ctrl Pts',(63.8922690722984,4.13962980658163,59.3583884288315));
#170695=CARTESIAN_POINT('Ctrl Pts',(63.8709927647128,4.09156852755386,59.3627077809818));
#170696=CARTESIAN_POINT('Ctrl Pts',(63.8334927967838,4.00503936356984,59.370325329739));
#170697=CARTESIAN_POINT('Ctrl Pts',(63.8171313041858,3.96663496362141,59.373650563344));
#170698=CARTESIAN_POINT('Ctrl Pts',(63.7827743929955,3.88458348448609,59.3806366773712));
#170699=CARTESIAN_POINT('Ctrl Pts',(63.7648455037303,3.84090854991692,59.3842845032402));
#170700=CARTESIAN_POINT('Ctrl Pts',(63.7170727132223,3.72217108621557,59.3940105529897));
#170701=CARTESIAN_POINT('Ctrl Pts',(63.687818382829,3.64686581329855,59.3999731772421));
#170702=CARTESIAN_POINT('Ctrl Pts',(63.5259603331888,3.21495033141412,59.4330063950098));
#170703=CARTESIAN_POINT('Ctrl Pts',(63.4125685846242,2.85119376599921,59.4563056449456));
#170704=CARTESIAN_POINT('Ctrl Pts',(63.180119070049,1.92462129514176,59.50500681965));
#170705=CARTESIAN_POINT('Ctrl Pts',(63.0878540298603,1.35626728101101,59.525342480917));
#170706=CARTESIAN_POINT('Ctrl Pts',(63.0303100530313,0.597995224837442,
59.5419459594712));
#170707=CARTESIAN_POINT('Ctrl Pts',(63.0213609437474,0.41265721398558,59.5451892306214));
#170708=CARTESIAN_POINT('Ctrl Pts',(63.0166172310532,0.18350400315967,59.5482719701468));
#170709=CARTESIAN_POINT('Ctrl Pts',(63.0159965172689,0.139834677949024,
59.5488179121082));
#170710=CARTESIAN_POINT('Ctrl Pts',(63.0154652684897,0.0710627943937142,
59.5496136497237));
#170711=CARTESIAN_POINT('Ctrl Pts',(63.0153649747804,0.0459625763126578,
59.5498906471691));
#170712=CARTESIAN_POINT('Ctrl Pts',(63.0153564584608,0.0139080571565023,
59.5502274527843));
#170713=CARTESIAN_POINT('Ctrl Pts',(63.0153617971604,0.0069540216278127,
59.55029950277));
#170714=CARTESIAN_POINT('Ctrl Pts',(63.0153743226244,-3.90012641998867E-11,
59.5503705382064));
#170715=CARTESIAN_POINT('Origin',(69.7358040552328,0.,40.0761166693274));
#170716=CARTESIAN_POINT('',(59.9621915011161,6.55335890299524E-10,43.6746029314002));
#170717=CARTESIAN_POINT('',(59.9459911121981,-3.64320804018464E-10,43.5827259602593));
#170718=CARTESIAN_POINT('',(59.6415245868576,-1.25526296912604E-15,41.8560104904131));
#170719=CARTESIAN_POINT('',(72.9974833261205,-9.75859007406187,40.5164212233382));
#170720=CARTESIAN_POINT('Ctrl Pts',(59.9621915011161,1.31067303586202E-9,
43.6746029314002));
#170721=CARTESIAN_POINT('Ctrl Pts',(59.9621173489605,0.0228571466064858,
43.6741823936118));
#170722=CARTESIAN_POINT('Ctrl Pts',(59.9621180799651,0.0457142985922821,
43.6737462492041));
#170723=CARTESIAN_POINT('Ctrl Pts',(59.9624078920643,0.133296489368093,
43.6720156346674));
#170724=CARTESIAN_POINT('Ctrl Pts',(59.9632226967352,0.198015867431952,
43.6706124157896));
#170725=CARTESIAN_POINT('Ctrl Pts',(59.9678600120166,0.409967523361952,
43.6656166008375));
#170726=CARTESIAN_POINT('Ctrl Pts',(59.9741929074607,0.557114709600572,
43.6615153088182));
#170727=CARTESIAN_POINT('Ctrl Pts',(59.998364587665,0.933224609434551,43.6494724853576));
#170728=CARTESIAN_POINT('Ctrl Pts',(60.0206520657771,1.16179318812559,43.6406704381945));
#170729=CARTESIAN_POINT('Ctrl Pts',(60.1378106502567,2.05585624406351,43.6007067186337));
#170730=CARTESIAN_POINT('Ctrl Pts',(60.289511129006,2.71176638524539,43.5593668052642));
#170731=CARTESIAN_POINT('Ctrl Pts',(60.5523720615392,3.49255424417903,43.4964316546202));
#170732=CARTESIAN_POINT('Ctrl Pts',(60.604378853226,3.63636565434677,43.4842343271781));
#170733=CARTESIAN_POINT('Ctrl Pts',(60.6958366926319,3.87267630363641,43.4631817307161));
#170734=CARTESIAN_POINT('Ctrl Pts',(60.7334847405298,3.96587194680139,43.4546131709443));
#170735=CARTESIAN_POINT('Ctrl Pts',(60.8113679101905,4.15081525954715,43.4370735516841));
#170736=CARTESIAN_POINT('Ctrl Pts',(60.8515905937239,4.24255632784152,43.4281047483983));
#170737=CARTESIAN_POINT('Ctrl Pts',(60.9560112778985,4.47155784408085,43.4050345898634));
#170738=CARTESIAN_POINT('Ctrl Pts',(61.0219073827158,4.60798972713239,43.3906642933388));
#170739=CARTESIAN_POINT('Ctrl Pts',(61.1741302317573,4.90611503719396,43.3578454249194));
#170740=CARTESIAN_POINT('Ctrl Pts',(61.2618115080646,5.06703334461495,43.3391809161984));
#170741=CARTESIAN_POINT('Ctrl Pts',(61.5805617291279,5.61643215419288,43.2720333696092));
#170742=CARTESIAN_POINT('Ctrl Pts',(61.8328107441819,5.99156763586135,43.2200948034707));
#170743=CARTESIAN_POINT('Ctrl Pts',(62.2780025896807,6.56733504541906,43.1292253869409));
#170744=CARTESIAN_POINT('Ctrl Pts',(62.4560175662718,6.77914880064797,43.0930538146435));
#170745=CARTESIAN_POINT('Ctrl Pts',(62.6974675926512,7.04378963482971,43.0439565774247));
#170746=CARTESIAN_POINT('Ctrl Pts',(62.7533793669096,7.10360488459081,43.0325847604572));
#170747=CARTESIAN_POINT('Ctrl Pts',(62.8481893238609,7.20261070306342,43.0132885449785));
#170748=CARTESIAN_POINT('Ctrl Pts',(62.8867037413048,7.24217909369355,43.0054462307965));
#170749=CARTESIAN_POINT('Ctrl Pts',(62.9716333422471,7.32802212488346,42.9881426304937));
#170750=CARTESIAN_POINT('Ctrl Pts',(63.0181746133971,7.37416200354657,42.9786543938634));
#170751=CARTESIAN_POINT('Ctrl Pts',(63.1646921582297,7.51662816108502,42.9487733654001));
#170752=CARTESIAN_POINT('Ctrl Pts',(63.2661683042383,7.6113220524863,42.9280627144475));
#170753=CARTESIAN_POINT('Ctrl Pts',(63.683676641712,7.98515581457783,42.842875281147));
#170754=CARTESIAN_POINT('Ctrl Pts',(64.0147467484473,8.2461738564164,42.7753930960578));
#170755=CARTESIAN_POINT('Ctrl Pts',(64.7129166745861,8.72869804795411,42.6341409547654));
#170756=CARTESIAN_POINT('Ctrl Pts',(65.0798374146058,8.94897057827151,42.560428361568));
#170757=CARTESIAN_POINT('Ctrl Pts',(65.5759815949015,9.20500908177388,42.4617082015838));
#170758=CARTESIAN_POINT('Ctrl Pts',(65.6936460591498,9.26281810691175,42.4383603462147));
#170759=CARTESIAN_POINT('Ctrl Pts',(65.8993561053364,9.35888780248268,42.3976544996312));
#170760=CARTESIAN_POINT('Ctrl Pts',(65.9868888909456,9.39823419833073,42.3803680453632));
#170761=CARTESIAN_POINT('Ctrl Pts',(66.1707762926584,9.47771320147651,42.3441237481254));
#170762=CARTESIAN_POINT('Ctrl Pts',(66.2672193832234,9.5176065801842,42.3251546585356));
#170763=CARTESIAN_POINT('Ctrl Pts',(66.5303000012563,9.62160599451012,42.2735135941002));
#170764=CARTESIAN_POINT('Ctrl Pts',(66.6980417425985,9.6827402026475,42.2406984428086));
#170765=CARTESIAN_POINT('Ctrl Pts',(67.2057678737193,9.85241545738296,42.1416605022513));
#170766=CARTESIAN_POINT('Ctrl Pts',(67.5499555697635,9.94713706253093,42.0749112681763));
#170767=CARTESIAN_POINT('Ctrl Pts',(68.3729831188539,10.1265021802317,41.9156916451335));
#170768=CARTESIAN_POINT('Ctrl Pts',(68.8543582772232,10.1948356872893,41.8228819554522));
#170769=CARTESIAN_POINT('Ctrl Pts',(69.4770026780229,10.2368873557742,41.7020779247071));
#170770=CARTESIAN_POINT('Ctrl Pts',(69.6155866148857,10.2433197476081,41.6751401055884));
#170771=CARTESIAN_POINT('Ctrl Pts',(69.8168134430169,10.2484171668224,41.635915800564));
#170772=CARTESIAN_POINT('Ctrl Pts',(69.879394580317,10.2494074474648,41.6237016685943));
#170773=CARTESIAN_POINT('Ctrl Pts',(69.9868439031305,10.2500863515925,41.6026997239521));
#170774=CARTESIAN_POINT('Ctrl Pts',(70.031709362798,10.2500640897533,41.5939209213597));
#170775=CARTESIAN_POINT('Ctrl Pts',(70.1410862974038,10.249264419133,41.5724962519277));
#170776=CARTESIAN_POINT('Ctrl Pts',(70.2055911165958,10.2481605107784,41.559842056356));
#170777=CARTESIAN_POINT('Ctrl Pts',(70.4209209722125,10.242363872947,41.5175440429169));
#170778=CARTESIAN_POINT('Ctrl Pts',(70.571638512008,10.2348455628059,41.4878467799212));
#170779=CARTESIAN_POINT('Ctrl Pts',(70.9625450467684,10.2063487386924,41.4106583962023));
#170780=CARTESIAN_POINT('Ctrl Pts',(71.2022447629782,10.1800199987766,41.3631666522352));
#170781=CARTESIAN_POINT('Ctrl Pts',(72.0951777882295,10.0486995648725,41.1860129444652));
#170782=CARTESIAN_POINT('Ctrl Pts',(72.7386402484642,9.88690701672744,41.0579901983043));
#170783=CARTESIAN_POINT('Ctrl Pts',(73.4925478435304,9.6147721265457,40.9087845182055));
#170784=CARTESIAN_POINT('Ctrl Pts',(73.6221561785561,9.56489518654855,40.8831577982836));
#170785=CARTESIAN_POINT('Ctrl Pts',(73.839744805898,9.47588736436761,40.8401767898018));
#170786=CARTESIAN_POINT('Ctrl Pts',(73.9282588973938,9.43817299578687,40.8227041079641));
#170787=CARTESIAN_POINT('Ctrl Pts',(74.1089292205463,9.35808061597936,40.7870625206487));
#170788=CARTESIAN_POINT('Ctrl Pts',(74.2010154417043,9.31556553328432,40.7689086618338));
#170789=CARTESIAN_POINT('Ctrl Pts',(74.4396917085287,9.20092390472612,40.7218838042689));
#170790=CARTESIAN_POINT('Ctrl Pts',(74.5852233809284,9.12657320745118,40.6932386751481));
#170791=CARTESIAN_POINT('Ctrl Pts',(74.8250778081425,8.99651990887481,40.6460542819881));
#170792=CARTESIAN_POINT('Ctrl Pts',(74.9203958179086,8.94279552140334,40.6273102682133));
#170793=CARTESIAN_POINT('Ctrl Pts',(75.3158959460101,8.71125304821846,40.5495440028411));
#170794=CARTESIAN_POINT('Ctrl Pts',(75.6078006929296,8.51923709816489,40.492174775107));
#170795=CARTESIAN_POINT('Ctrl Pts',(76.2045070451203,8.08049044573636,40.3744386786407));
#170796=CARTESIAN_POINT('Ctrl Pts',(76.5061781490616,7.83033589013045,40.3146322624727));
#170797=CARTESIAN_POINT('Ctrl Pts',(76.8632764293588,7.49723871979224,40.2428515583412));
#170798=CARTESIAN_POINT('Ctrl Pts',(76.9328689371494,7.43043143693812,40.228811623474));
#170799=CARTESIAN_POINT('Ctrl Pts',(77.0425255134659,7.32209786669668,40.2065927027049));
#170800=CARTESIAN_POINT('Ctrl Pts',(77.0832019609948,7.28121728359858,40.1983288871604));
#170801=CARTESIAN_POINT('Ctrl Pts',(77.1655949510218,7.19697848608749,40.1815412153398));
#170802=CARTESIAN_POINT('Ctrl Pts',(77.2072791305238,7.15359121425286,40.1730220518778));
#170803=CARTESIAN_POINT('Ctrl Pts',(77.3235043901774,7.03043367865424,40.1492000300661));
#170804=CARTESIAN_POINT('Ctrl Pts',(77.3971561861542,6.94981120634495,40.1340231108469));
#170805=CARTESIAN_POINT('Ctrl Pts',(77.5671917963301,6.75752477627966,40.0988159294102));
#170806=CARTESIAN_POINT('Ctrl Pts',(77.6624851149221,6.64489896507505,40.0789512984824));
#170807=CARTESIAN_POINT('Ctrl Pts',(78.0451683691847,6.17208490725915,39.9987104549053));
#170808=CARTESIAN_POINT('Ctrl Pts',(78.3106477829238,5.79426324545742,39.9419343747953));
#170809=CARTESIAN_POINT('Ctrl Pts',(78.709895369505,5.13555485717968,39.85538209849));
#170810=CARTESIAN_POINT('Ctrl Pts',(78.8579202449703,4.86447867345772,39.8229392144116));
#170811=CARTESIAN_POINT('Ctrl Pts',(79.0485049951672,4.47475917324987,39.7807255571288));
#170812=CARTESIAN_POINT('Ctrl Pts',(79.1013419507587,4.36154850676487,39.7689653621557));
#170813=CARTESIAN_POINT('Ctrl Pts',(79.1913152696655,4.15926374257341,39.7488361141225));
#170814=CARTESIAN_POINT('Ctrl Pts',(79.2292776224757,4.0705900938065,39.7403067915342));
#170815=CARTESIAN_POINT('Ctrl Pts',(79.3071811106906,3.88134112494089,39.7227233478217));
#170816=CARTESIAN_POINT('Ctrl Pts',(79.3467983331995,3.78063946443114,39.7137322934617));
#170817=CARTESIAN_POINT('Ctrl Pts',(79.4532281947511,3.49713415511864,39.6894306405052));
#170818=CARTESIAN_POINT('Ctrl Pts',(79.5164959258718,3.31299144033201,39.6748074869594));
#170819=CARTESIAN_POINT('Ctrl Pts',(79.6515049216347,2.88078099934798,39.6431138485946));
#170820=CARTESIAN_POINT('Ctrl Pts',(79.7192630951612,2.6315539187254,39.6268063790029));
#170821=CARTESIAN_POINT('Ctrl Pts',(79.8553469381881,2.04542344578551,39.5928183428281));
#170822=CARTESIAN_POINT('Ctrl Pts',(79.9164083023191,1.70707918399919,39.5764822130061));
#170823=CARTESIAN_POINT('Ctrl Pts',(80.0029096504755,1.0396177494775,39.5501129407671));
#170824=CARTESIAN_POINT('Ctrl Pts',(80.0296829682864,0.711099854667932,
39.5398580952606));
#170825=CARTESIAN_POINT('Ctrl Pts',(80.0435161808942,0.299867631964759,
39.5300357774177));
#170826=CARTESIAN_POINT('Ctrl Pts',(80.0453000397251,0.217898369552569,
39.5282267562018));
#170827=CARTESIAN_POINT('Ctrl Pts',(80.046624549247,0.0838834065347642,
39.5255040730306));
#170828=CARTESIAN_POINT('Ctrl Pts',(80.0467466390509,0.0318487197293709,
39.5245047644598));
#170829=CARTESIAN_POINT('Ctrl Pts',(80.0461810446212,-0.0770421743425323,
39.5225320751962));
#170830=CARTESIAN_POINT('Ctrl Pts',(80.0454173465967,-0.133896045883498,
39.5215700085654));
#170831=CARTESIAN_POINT('Ctrl Pts',(80.0419445200657,-0.294171634927588,
39.5190534947571));
#170832=CARTESIAN_POINT('Ctrl Pts',(80.0381542087308,-0.397565684268229,
39.5176598488733));
#170833=CARTESIAN_POINT('Ctrl Pts',(80.0257175206212,-0.638351979015838,
39.5149697493917));
#170834=CARTESIAN_POINT('Ctrl Pts',(80.015881642578,-0.775665347584725,
39.5138579199797));
#170835=CARTESIAN_POINT('Ctrl Pts',(79.9681294730664,-1.29673392045101,
39.5113161000226));
#170836=CARTESIAN_POINT('Ctrl Pts',(79.9115848938906,-1.67847948944964,
39.5129326313413));
#170837=CARTESIAN_POINT('Ctrl Pts',(79.7453491137976,-2.4878330276729,39.5245408991904));
#170838=CARTESIAN_POINT('Ctrl Pts',(79.6293893604218,-2.91336111157483,
39.5356926267131));
#170839=CARTESIAN_POINT('Ctrl Pts',(79.436317815401,-3.47799802302839,39.5577336475775));
#170840=CARTESIAN_POINT('Ctrl Pts',(79.3824275799282,-3.62471565578979,
39.564145826349));
#170841=CARTESIAN_POINT('Ctrl Pts',(79.2881949465286,-3.86442988438599,
39.5757625243229));
#170842=CARTESIAN_POINT('Ctrl Pts',(79.2497561460365,-3.95816437331337,
39.5805982594267));
#170843=CARTESIAN_POINT('Ctrl Pts',(79.1706894388021,-4.14321512524139,
39.5907297015011));
#170844=CARTESIAN_POINT('Ctrl Pts',(79.1301017712287,-4.2345369342463,39.5960178770899));
#170845=CARTESIAN_POINT('Ctrl Pts',(79.0256927379774,-4.46060257360602,
39.6098281622912));
#170846=CARTESIAN_POINT('Ctrl Pts',(78.9602813570908,-4.59456726527603,
39.6186593835295));
#170847=CARTESIAN_POINT('Ctrl Pts',(78.6993617524911,-5.10093193980778,
39.6545086894478));
#170848=CARTESIAN_POINT('Ctrl Pts',(78.4842466923207,-5.46248288743085,
39.6853245395268));
#170849=CARTESIAN_POINT('Ctrl Pts',(77.9759743733251,-6.20885361409864,
39.7598038940904));
#170850=CARTESIAN_POINT('Ctrl Pts',(77.6765978230205,-6.58808349054391,
39.8046077311431));
#170851=CARTESIAN_POINT('Ctrl Pts',(77.290641866474,-7.01159944329429,39.8623364442698));
#170852=CARTESIAN_POINT('Ctrl Pts',(77.2285883757945,-7.07789256832334,
39.8716162406021));
#170853=CARTESIAN_POINT('Ctrl Pts',(77.130166503438,-7.1802627397015,39.8863211949434));
#170854=CARTESIAN_POINT('Ctrl Pts',(77.0943915823113,-7.21691568138124,
39.891663501156));
#170855=CARTESIAN_POINT('Ctrl Pts',(77.0161053098073,-7.29592220348143,
39.9033454419194));
#170856=CARTESIAN_POINT('Ctrl Pts',(76.9734940530889,-7.33817187992911,
39.9096986641105));
#170857=CARTESIAN_POINT('Ctrl Pts',(76.8535436084434,-7.45502044706939,
39.9275733209952));
#170858=CARTESIAN_POINT('Ctrl Pts',(76.7754017126208,-7.52876698255031,
39.9392068607575));
#170859=CARTESIAN_POINT('Ctrl Pts',(76.4817043189845,-7.79728526459952,
39.9829276972726));
#170860=CARTESIAN_POINT('Ctrl Pts',(76.2590915117683,-7.98396200446055,
40.0160619804401));
#170861=CARTESIAN_POINT('Ctrl Pts',(75.5494288559673,-8.52909754940981,
40.1221845041652));
#170862=CARTESIAN_POINT('Ctrl Pts',(75.0385395243456,-8.8535292413592,40.1993245473084));
#170863=CARTESIAN_POINT('Ctrl Pts',(74.3812162984507,-9.19277637038211,
40.3003980655456));
#170864=CARTESIAN_POINT('Ctrl Pts',(74.2587588269137,-9.25286941293378,
40.319296020266));
#170865=CARTESIAN_POINT('Ctrl Pts',(74.0470333520821,-9.35149847965907,
40.3520884572869));
#170866=CARTESIAN_POINT('Ctrl Pts',(73.9583410299252,-9.39126526229129,
40.3658600374334));
#170867=CARTESIAN_POINT('Ctrl Pts',(73.7874146030616,-9.46495489953998,
40.3924658912069));
#170868=CARTESIAN_POINT('Ctrl Pts',(73.7052763221112,-9.49908431976494,
40.4052797349676));
#170869=CARTESIAN_POINT('Ctrl Pts',(73.5306247219921,-9.56895706967644,
40.4325841311828));
#170870=CARTESIAN_POINT('Ctrl Pts',(73.4380164429053,-9.60442909177834,
40.4470962130776));
#170871=CARTESIAN_POINT('Ctrl Pts',(73.2298227428336,-9.68066566216209,
40.4797924347375));
#170872=CARTESIAN_POINT('Ctrl Pts',(73.1139937762474,-9.7206951460624,40.4980316609364));
#170873=CARTESIAN_POINT('Ctrl Pts',(72.9974833261205,-9.75859007406187,
40.5164212233382));
#170874=CARTESIAN_POINT('',(76.8678595013252,-7.42547303891629,39.8339694781585));
#170875=CARTESIAN_POINT('Origin',(69.9094522328998,0.,41.0609244223396));
#170876=CARTESIAN_POINT('Ctrl Pts',(76.8678595013252,-7.42547303891629,
39.8339694781584));
#170877=CARTESIAN_POINT('Ctrl Pts',(76.8990285746249,-7.39548789751561,
39.8292694255059));
#170878=CARTESIAN_POINT('Ctrl Pts',(76.9300033038781,-7.36530950731916,
39.8246101125015));
#170879=CARTESIAN_POINT('Ctrl Pts',(76.9890950918522,-7.3070029802757,39.8157448866622));
#170880=CARTESIAN_POINT('Ctrl Pts',(77.0172338774585,-7.27891310035191,
39.811533799747));
#170881=CARTESIAN_POINT('Ctrl Pts',(77.0856086872409,-7.20985852939954,
39.8013283125404));
#170882=CARTESIAN_POINT('Ctrl Pts',(77.1256682594321,-7.16871548356406,
39.7953724164883));
#170883=CARTESIAN_POINT('Ctrl Pts',(77.2311477720555,-7.05854733117038,
39.7797484782629));
#170884=CARTESIAN_POINT('Ctrl Pts',(77.295966387408,-6.98893604171636,39.7702080620901));
#170885=CARTESIAN_POINT('Ctrl Pts',(77.6305655574832,-6.61942870337986,
39.7212469538832));
#170886=CARTESIAN_POINT('Ctrl Pts',(77.8836889316479,-6.30448353077214,
39.6851960134421));
#170887=CARTESIAN_POINT('Ctrl Pts',(78.4029737335433,-5.57414804881995,
39.6126427073769));
#170888=CARTESIAN_POINT('Ctrl Pts',(78.6592508879664,-5.15278013234336,
39.57783655874));
#170889=CARTESIAN_POINT('Ctrl Pts',(78.9516653474975,-4.58383576110372,
39.5390626495023));
#170890=CARTESIAN_POINT('Ctrl Pts',(79.0160016307363,-4.45180144374981,
39.530607907952));
#170891=CARTESIAN_POINT('Ctrl Pts',(79.1191926701759,-4.2280246383929,39.5171765521302));
#170892=CARTESIAN_POINT('Ctrl Pts',(79.1595712596385,-4.13702419646794,
39.5119580218592));
#170893=CARTESIAN_POINT('Ctrl Pts',(79.2385572431532,-3.95184115846412,
39.5018279559135));
#170894=CARTESIAN_POINT('Ctrl Pts',(79.2771013330322,-3.85764308504231,
39.4969263200327));
#170895=CARTESIAN_POINT('Ctrl Pts',(79.3722209894594,-3.61501995471575,
39.4849435078869));
#170896=CARTESIAN_POINT('Ctrl Pts',(79.4267846515862,-3.4658199729671,39.4781815291744));
#170897=CARTESIAN_POINT('Ctrl Pts',(79.6393390113098,-2.84033980478241,
39.4523692131195));
#170898=CARTESIAN_POINT('Ctrl Pts',(79.7660895075844,-2.35398540594275,
39.4382963459358));
#170899=CARTESIAN_POINT('Ctrl Pts',(79.918371690702,-1.5290448733026,39.4251794611873));
#170900=CARTESIAN_POINT('Ctrl Pts',(79.963395685683,-1.1950133641786,39.4227322356103));
#170901=CARTESIAN_POINT('Ctrl Pts',(80.0080462612809,-0.674516161978915,
39.4237578630503));
#170902=CARTESIAN_POINT('Ctrl Pts',(80.0189721768199,-0.489257118968895,
39.4250665478881));
#170903=CARTESIAN_POINT('Ctrl Pts',(80.0272276639154,-0.23370677680595,
39.4282457473849));
#170904=CARTESIAN_POINT('Ctrl Pts',(80.0287868895687,-0.163577834301707,
39.4292606182179));
#170905=CARTESIAN_POINT('Ctrl Pts',(80.0302602635132,-0.0425597037715466,
39.4312630645013));
#170906=CARTESIAN_POINT('Ctrl Pts',(80.0305085519828,0.00832354220289945,
39.4321818150966));
#170907=CARTESIAN_POINT('Ctrl Pts',(80.0302337913538,0.122148487738307,
39.4344098758722));
#170908=CARTESIAN_POINT('Ctrl Pts',(80.0295138785973,0.185086082590115,
39.4357595574041));
#170909=CARTESIAN_POINT('Ctrl Pts',(80.0254343796904,0.384367694243806,
39.4403996303459));
#170910=CARTESIAN_POINT('Ctrl Pts',(80.0199751212635,0.520644196063558,
39.4441161654749));
#170911=CARTESIAN_POINT('Ctrl Pts',(79.9820996429936,1.15498961354795,39.4638611414359));
#170912=CARTESIAN_POINT('Ctrl Pts',(79.9166508322399,1.6502162462987,39.4862837367131));
#170913=CARTESIAN_POINT('Ctrl Pts',(79.7371277022152,2.52022778367019,39.5369688694709));
#170914=CARTESIAN_POINT('Ctrl Pts',(79.6369242658023,2.89701110402737,39.5628547848345));
#170915=CARTESIAN_POINT('Ctrl Pts',(79.4636815455327,3.42597023401457,39.6046748539072));
#170916=CARTESIAN_POINT('Ctrl Pts',(79.4077692912873,3.58360973267206,39.6178607972264));
#170917=CARTESIAN_POINT('Ctrl Pts',(79.3112175035052,3.83613493849726,39.6401589588782));
#170918=CARTESIAN_POINT('Ctrl Pts',(79.272933952288,3.93192072117163,39.6488964259421));
#170919=CARTESIAN_POINT('Ctrl Pts',(79.1958155300578,4.11675596164734,39.6663043427833));
#170920=CARTESIAN_POINT('Ctrl Pts',(79.1571451961852,4.20586455879665,39.6749484356336));
#170921=CARTESIAN_POINT('Ctrl Pts',(79.0690856502033,4.40115295012384,39.6944543856953));
#170922=CARTESIAN_POINT('Ctrl Pts',(79.0191353558858,4.50705563096255,39.7054049367983));
#170923=CARTESIAN_POINT('Ctrl Pts',(78.8056406730932,4.94033148362395,39.7517720560935));
#170924=CARTESIAN_POINT('Ctrl Pts',(78.6265591937485,5.25947349456486,39.7896551829451));
#170925=CARTESIAN_POINT('Ctrl Pts',(78.2116804948403,5.91409987506177,39.8759311392482));
#170926=CARTESIAN_POINT('Ctrl Pts',(77.9720229012634,6.24628086098109,39.9249606399178));
#170927=CARTESIAN_POINT('Ctrl Pts',(77.6246178158771,6.67146949341581,39.9956966378726));
#170928=CARTESIAN_POINT('Ctrl Pts',(77.5336591481646,6.77821698227307,40.0141911967846));
#170929=CARTESIAN_POINT('Ctrl Pts',(77.3705838108441,6.96178471729201,40.0473476947724));
#170930=CARTESIAN_POINT('Ctrl Pts',(77.2994058850546,7.0394439411327,40.0618191768485));
#170931=CARTESIAN_POINT('Ctrl Pts',(77.1862350714393,7.15913500881618,40.0848449318188));
#170932=CARTESIAN_POINT('Ctrl Pts',(77.1450411747064,7.20194430764065,40.0932295683592));
#170933=CARTESIAN_POINT('Ctrl Pts',(77.0676782118854,7.28094345440789,40.1089860008795));
#170934=CARTESIAN_POINT('Ctrl Pts',(77.0316043901696,7.31722787839537,40.1163371104082));
#170935=CARTESIAN_POINT('Ctrl Pts',(76.9302526726861,7.41764188748027,40.1369984532148));
#170936=CARTESIAN_POINT('Ctrl Pts',(76.8643922015006,7.48115089376309,40.1504336311935));
#170937=CARTESIAN_POINT('Ctrl Pts',(76.3980520662467,7.91880977020058,40.2455832329278));
#170938=CARTESIAN_POINT('Ctrl Pts',(75.9692665279844,8.26020280735344,40.3331178885577));
#170939=CARTESIAN_POINT('Ctrl Pts',(75.2985069547894,8.70999833087118,40.4686098847352));
#170940=CARTESIAN_POINT('Ctrl Pts',(75.0761544622313,8.84680697144869,40.5133230576833));
#170941=CARTESIAN_POINT('Ctrl Pts',(74.7695648199348,9.01926273357357,40.5746330733728));
#170942=CARTESIAN_POINT('Ctrl Pts',(74.6897242445181,9.06274676450101,40.5905692816809));
#170943=CARTESIAN_POINT('Ctrl Pts',(74.4822279790979,9.17210369399836,40.6319057495574));
#170944=CARTESIAN_POINT('Ctrl Pts',(74.3537413525391,9.23630923447455,40.6574253326405));
#170945=CARTESIAN_POINT('Ctrl Pts',(74.1354185870535,9.3395650965652,40.7006561014693));
#170946=CARTESIAN_POINT('Ctrl Pts',(74.0462972422509,9.38011621502275,40.7182673050036));
#170947=CARTESIAN_POINT('Ctrl Pts',(73.8753841785891,9.45485715834273,40.7519737138198));
#170948=CARTESIAN_POINT('Ctrl Pts',(73.7937028210593,9.4892827629088,40.7680535087685));
#170949=CARTESIAN_POINT('Ctrl Pts',(73.5757808526759,9.57771432433733,40.8108794385776));
#170950=CARTESIAN_POINT('Ctrl Pts',(73.4388036548674,9.62979930375277,40.837721877349));
#170951=CARTESIAN_POINT('Ctrl Pts',(72.674124477842,9.90134916431078,40.9871888510873));
#170952=CARTESIAN_POINT('Ctrl Pts',(72.0271611616332,10.0601723356113,41.1121153475183));
#170953=CARTESIAN_POINT('Ctrl Pts',(71.1425330131848,10.1850166898584,41.2830892933127));
#170954=CARTESIAN_POINT('Ctrl Pts',(70.9144637961712,10.2091524228976,41.3271956911357));
#170955=CARTESIAN_POINT('Ctrl Pts',(70.5400256272296,10.2356556234102,41.3998228763409));
#170956=CARTESIAN_POINT('Ctrl Pts',(70.394049029545,10.2427390308062,41.4281904026554));
#170957=CARTESIAN_POINT('Ctrl Pts',(70.1842294733845,10.2482598716852,41.4690843290307));
#170958=CARTESIAN_POINT('Ctrl Pts',(70.1204592708199,10.2493199595284,41.4815290851168));
#170959=CARTESIAN_POINT('Ctrl Pts',(70.0068811527501,10.2501078748424,41.5037268454323));
#170960=CARTESIAN_POINT('Ctrl Pts',(69.9570765267565,10.2500766201812,41.5134723015878));
#170961=CARTESIAN_POINT('Ctrl Pts',(69.8420581847569,10.2491342981117,41.5360050517938));
#170962=CARTESIAN_POINT('Ctrl Pts',(69.7768509474777,10.2479538840617,41.5487988724902));
#170963=CARTESIAN_POINT('Ctrl Pts',(69.5665371123725,10.2420616783078,41.5901176442255));
#170964=CARTESIAN_POINT('Ctrl Pts',(69.4215302454519,10.234795177056,41.6186899135523));
#170965=CARTESIAN_POINT('Ctrl Pts',(68.4696077886515,10.1660138608211,41.8066451880225));
#170966=CARTESIAN_POINT('Ctrl Pts',(67.6725851893531,10.0086501410841,41.9655895428828));
#170967=CARTESIAN_POINT('Ctrl Pts',(66.7236348913335,9.69686408548901,42.1536230990952));
#170968=CARTESIAN_POINT('Ctrl Pts',(66.5464194445875,9.63300004668673,42.1886978194846));
#170969=CARTESIAN_POINT('Ctrl Pts',(66.2722638634957,9.52530485355145,42.2428876051179));
#170970=CARTESIAN_POINT('Ctrl Pts',(66.1740777165832,9.48490985429102,42.262280687351));
#170971=CARTESIAN_POINT('Ctrl Pts',(65.9888791377432,9.40523036584957,42.2988334914227));
#170972=CARTESIAN_POINT('Ctrl Pts',(65.9017526755059,9.36625267307211,42.3160184288552));
#170973=CARTESIAN_POINT('Ctrl Pts',(65.7020464373638,9.27344606329649,42.3553853881296));
#170974=CARTESIAN_POINT('Ctrl Pts',(65.5898759105557,9.21873771633629,42.3774794533091));
#170975=CARTESIAN_POINT('Ctrl Pts',(65.2014965573261,9.02021804661125,42.4539324068031));
#170976=CARTESIAN_POINT('Ctrl Pts',(64.9308299837578,8.86552166540736,42.5071262200063));
#170977=CARTESIAN_POINT('Ctrl Pts',(64.2866946003729,8.4563710629904,42.6338073921607));
#170978=CARTESIAN_POINT('Ctrl Pts',(63.9221101920738,8.18870661371439,42.7055779139455));
#170979=CARTESIAN_POINT('Ctrl Pts',(63.464653865196,7.80286662160835,42.7965793118998));
#170980=CARTESIAN_POINT('Ctrl Pts',(63.3549227002082,7.70614968893859,42.818489265235));
#170981=CARTESIAN_POINT('Ctrl Pts',(63.1674400891867,7.53350670885597,42.8561159797199));
#170982=CARTESIAN_POINT('Ctrl Pts',(63.0887526019016,7.45866379174902,42.8719701145718));
#170983=CARTESIAN_POINT('Ctrl Pts',(62.9684381653949,7.34046815037003,42.8963277451624));
#170984=CARTESIAN_POINT('Ctrl Pts',(62.9259756637275,7.29800195607488,42.9049475465382));
#170985=CARTESIAN_POINT('Ctrl Pts',(62.8434240876446,7.21395562638395,42.9217555361425));
#170986=CARTESIAN_POINT('Ctrl Pts',(62.8033082706967,7.17240601497427,42.9299474042846));
#170987=CARTESIAN_POINT('Ctrl Pts',(62.696834408525,7.06021662695402,42.9517506682705));
#170988=CARTESIAN_POINT('Ctrl Pts',(62.6311236833974,6.98895283042766,42.9652709750419));
#170989=CARTESIAN_POINT('Ctrl Pts',(62.2192988284285,6.52924229277284,43.0503751758264));
#170990=CARTESIAN_POINT('Ctrl Pts',(61.9021320626343,6.11509303133995,43.1175762416949));
#170991=CARTESIAN_POINT('Ctrl Pts',(61.4684418428818,5.44882528130082,43.210900835275));
#170992=CARTESIAN_POINT('Ctrl Pts',(61.3284373037179,5.21365403011963,43.2413240604058));
#170993=CARTESIAN_POINT('Ctrl Pts',(61.1031071075094,4.7982550081286,43.2907177272806));
#170994=CARTESIAN_POINT('Ctrl Pts',(61.0133551765301,4.62070523803238,43.3105333202156));
#170995=CARTESIAN_POINT('Ctrl Pts',(60.8825753724263,4.34225659141649,43.3396217908423));
#170996=CARTESIAN_POINT('Ctrl Pts',(60.8379382180383,4.24318147026431,43.3495942591852));
#170997=CARTESIAN_POINT('Ctrl Pts',(60.7566758520312,4.05493621894353,43.3678352123577));
#170998=CARTESIAN_POINT('Ctrl Pts',(60.7197204517938,3.96592785976959,43.376167717492));
#170999=CARTESIAN_POINT('Ctrl Pts',(60.6380742271444,3.76124565852801,43.3946662102358));
#171000=CARTESIAN_POINT('Ctrl Pts',(60.5942028810397,3.64524710709357,43.4046729206937));
#171001=CARTESIAN_POINT('Ctrl Pts',(60.4537665704898,3.25275197961635,43.4369514375245));
#171002=CARTESIAN_POINT('Ctrl Pts',(60.3667968015805,2.97282680911703,43.4573653843859));
#171003=CARTESIAN_POINT('Ctrl Pts',(60.2748146619763,2.62545634078586,43.4796507789828));
#171004=CARTESIAN_POINT('Ctrl Pts',(60.2584787769182,2.56128895432738,43.4836423840945));
#171005=CARTESIAN_POINT('Ctrl Pts',(60.1234629266166,2.00888984379493,43.5169456414411));
#171006=CARTESIAN_POINT('Ctrl Pts',(60.0396715483063,1.51245742901374,43.5397563499562));
#171007=CARTESIAN_POINT('Ctrl Pts',(59.9708782351334,0.786683988483576,
43.5641630169089));
#171008=CARTESIAN_POINT('Ctrl Pts',(59.9569046242807,0.561003863913369,
43.570523119053));
#171009=CARTESIAN_POINT('Ctrl Pts',(59.9481523568033,0.260411614599621,
43.5774956935159));
#171010=CARTESIAN_POINT('Ctrl Pts',(59.9467861842967,0.18577909152811,43.5791043272761));
#171011=CARTESIAN_POINT('Ctrl Pts',(59.9459496143772,0.0740918169188201,
43.5813340252946));
#171012=CARTESIAN_POINT('Ctrl Pts',(59.9458709289595,0.0370460643766788,
43.5820443672582));
#171013=CARTESIAN_POINT('Ctrl Pts',(59.9459911121981,-7.28640352773959E-10,
43.5827259602593));
#171014=CARTESIAN_POINT('Origin',(69.7358040552328,0.,40.0761166693274));
#171015=CARTESIAN_POINT('',(60.1705693073443,2.15049072447686E-6,44.8563721954731));
#171016=CARTESIAN_POINT('',(60.1543689253998,-5.77418479642888E-10,44.7644952638818));
#171017=CARTESIAN_POINT('',(59.6415245868576,-1.25526296912604E-15,41.8560104904131));
#171018=CARTESIAN_POINT('Ctrl Pts',(60.1705693073443,2.15049072447686E-6,
44.8563721954731));
#171019=CARTESIAN_POINT('Ctrl Pts',(60.1704255439564,0.044319522617042,
44.8555568192404));
#171020=CARTESIAN_POINT('Ctrl Pts',(60.1705632383758,0.0886262742527372,
44.8546829874787));
#171021=CARTESIAN_POINT('Ctrl Pts',(60.1715249939329,0.190262826338394,
44.8525455399988));
#171022=CARTESIAN_POINT('Ctrl Pts',(60.1725386634808,0.24757857132914,44.851243168513));
#171023=CARTESIAN_POINT('Ctrl Pts',(60.1780873034733,0.461678724818797,
44.846021289225));
#171024=CARTESIAN_POINT('Ctrl Pts',(60.1856796859077,0.618347621851348,
44.8414849048274));
#171025=CARTESIAN_POINT('Ctrl Pts',(60.2352514242262,1.31563187889683,44.8182311328369));
#171026=CARTESIAN_POINT('Ctrl Pts',(60.3158132347216,1.85239267216816,44.7921429505985));
#171027=CARTESIAN_POINT('Ctrl Pts',(60.496083572513,2.63157607779585,44.7433425718599));
#171028=CARTESIAN_POINT('Ctrl Pts',(60.5636603217285,2.88079739688011,44.72601359766));
#171029=CARTESIAN_POINT('Ctrl Pts',(60.6984329542329,3.31300003676053,44.6929898169196));
#171030=CARTESIAN_POINT('Ctrl Pts',(60.7616251099477,3.49713991596297,44.6779436237939));
#171031=CARTESIAN_POINT('Ctrl Pts',(60.867985974017,3.78064376844652,44.6532527619124));
#171032=CARTESIAN_POINT('Ctrl Pts',(60.9075878649764,3.88134492149082,44.6441757815022));
#171033=CARTESIAN_POINT('Ctrl Pts',(60.9854807615025,4.07059365435046,44.6265322693778));
#171034=CARTESIAN_POINT('Ctrl Pts',(61.0234457822407,4.15926739726915,44.618017701498));
#171035=CARTESIAN_POINT('Ctrl Pts',(61.1134425585809,4.3615526780029,44.5980194586427));
#171036=CARTESIAN_POINT('Ctrl Pts',(61.1663055552607,4.47476422131632,44.5864043415833));
#171037=CARTESIAN_POINT('Ctrl Pts',(61.3570238261799,4.86449146664188,44.5449234402758));
#171038=CARTESIAN_POINT('Ctrl Pts',(61.5052200292013,5.1355786498999,44.5134151024511));
#171039=CARTESIAN_POINT('Ctrl Pts',(61.9049887878862,5.79429098218372,44.4297809731763));
#171040=CARTESIAN_POINT('Ctrl Pts',(62.1708670338384,6.17210203586741,44.375301394302));
#171041=CARTESIAN_POINT('Ctrl Pts',(62.5539340471743,6.64490599185717,44.297280985997));
#171042=CARTESIAN_POINT('Ctrl Pts',(62.6493093980692,6.75753047789234,44.2778868575379));
#171043=CARTESIAN_POINT('Ctrl Pts',(62.8194514240044,6.94981479463985,44.2432933370539));
#171044=CARTESIAN_POINT('Ctrl Pts',(62.8931372911015,7.0304365990296,44.228312610868));
#171045=CARTESIAN_POINT('Ctrl Pts',(63.0093911900475,7.1535927499084,44.2046604536838));
#171046=CARTESIAN_POINT('Ctrl Pts',(63.051081244933,7.1969798918094,44.1961751949651));
#171047=CARTESIAN_POINT('Ctrl Pts',(63.133475470328,7.28121862649367,44.1793947693533));
#171048=CARTESIAN_POINT('Ctrl Pts',(63.1741476806585,7.32209928440839,44.1711063476643));
#171049=CARTESIAN_POINT('Ctrl Pts',(63.2837819804715,7.43043383051258,44.1487550811757));
#171050=CARTESIAN_POINT('Ctrl Pts',(63.3533481592734,7.49724151193889,44.1345629000235));
#171051=CARTESIAN_POINT('Ctrl Pts',(63.7102379452026,7.8303157962833,44.0617423766876));
#171052=CARTESIAN_POINT('Ctrl Pts',(64.0115750148459,8.08044522957783,44.0002314552037));
#171053=CARTESIAN_POINT('Ctrl Pts',(64.6076836801177,8.51918299615302,43.8792630898112));
#171054=CARTESIAN_POINT('Ctrl Pts',(64.8993390431828,8.71121564743694,43.8203647594883));
#171055=CARTESIAN_POINT('Ctrl Pts',(65.2946093242197,8.94277663363288,43.7411317988175));
#171056=CARTESIAN_POINT('Ctrl Pts',(65.389876630923,8.99650370569618,43.7220771734533));
#171057=CARTESIAN_POINT('Ctrl Pts',(65.6296224175688,9.12656163676907,43.6742358849136));
#171058=CARTESIAN_POINT('Ctrl Pts',(65.7751076266834,9.20091494725499,43.6453029153465));
#171059=CARTESIAN_POINT('Ctrl Pts',(66.0137429955704,9.31555992474666,43.5980099606362));
#171060=CARTESIAN_POINT('Ctrl Pts',(66.1058202200845,9.35807551534762,43.5798006983418));
#171061=CARTESIAN_POINT('Ctrl Pts',(66.2864886000496,9.43816827008255,43.5441461631412));
#171062=CARTESIAN_POINT('Ctrl Pts',(66.3750087861485,9.47588256072015,43.5267111117354));
#171063=CARTESIAN_POINT('Ctrl Pts',(66.5926281127583,9.56488892941394,43.4839294927927));
#171064=CARTESIAN_POINT('Ctrl Pts',(66.7222701492106,9.61476500451744,43.4585120757762));
#171065=CARTESIAN_POINT('Ctrl Pts',(67.4764781670717,9.88690200561605,43.3110061088934));
#171066=CARTESIAN_POINT('Ctrl Pts',(68.1205943078348,10.0487024228311,43.186575724765));
#171067=CARTESIAN_POINT('Ctrl Pts',(69.0143425374277,10.1800240126983,43.0138548861445));
#171068=CARTESIAN_POINT('Ctrl Pts',(69.2542296819376,10.2063509474823,42.9674745222301));
#171069=CARTESIAN_POINT('Ctrl Pts',(69.6004044869966,10.2315711849265,42.9003410817753));
#171070=CARTESIAN_POINT('Ctrl Pts',(69.7061292514836,10.2375676435575,42.8798105480313));
#171071=CARTESIAN_POINT('Ctrl Pts',(69.8967200090483,10.2453073872475,42.8427303618961));
#171072=CARTESIAN_POINT('Ctrl Pts',(69.9815547331096,10.2476581851155,42.8262005905712));
#171073=CARTESIAN_POINT('Ctrl Pts',(70.1188155339306,10.2496923204523,42.7994057882111));
#171074=CARTESIAN_POINT('Ctrl Pts',(70.1712314968081,10.2500517997528,42.7891618178983));
#171075=CARTESIAN_POINT('Ctrl Pts',(70.2783408274154,10.2499336729321,42.76820175232));
#171076=CARTESIAN_POINT('Ctrl Pts',(70.3330320179782,10.2494189562434,42.7574850875006));
#171077=CARTESIAN_POINT('Ctrl Pts',(70.4837238492593,10.2467484629841,42.7279219820349));
#171078=CARTESIAN_POINT('Ctrl Pts',(70.5796976098612,10.243646539479,42.7090541965003));
#171079=CARTESIAN_POINT('Ctrl Pts',(71.2343127941338,10.2129229516261,42.580143329448));
#171080=CARTESIAN_POINT('Ctrl Pts',(71.7897217646185,10.1392630019662,42.4697373880899));
#171081=CARTESIAN_POINT('Ctrl Pts',(72.6774250788273,9.94381380994694,42.2934205579085));
#171082=CARTESIAN_POINT('Ctrl Pts',(73.0145363486329,9.8506409414843,42.2264858167201));
#171083=CARTESIAN_POINT('Ctrl Pts',(73.5156923673857,9.68315989648576,42.1272022106212));
#171084=CARTESIAN_POINT('Ctrl Pts',(73.6836442204659,9.62194670070529,42.0939665145021));
#171085=CARTESIAN_POINT('Ctrl Pts',(73.9469871844002,9.51784016813432,42.0419191438102));
#171086=CARTESIAN_POINT('Ctrl Pts',(74.0434680579532,9.47793239236348,42.0228645502519));
#171087=CARTESIAN_POINT('Ctrl Pts',(74.2273835720304,9.39844897974591,41.9865676574354));
#171088=CARTESIAN_POINT('Ctrl Pts',(74.314905967817,9.35911469835312,41.9693059225534));
#171089=CARTESIAN_POINT('Ctrl Pts',(74.5205123278379,9.26312021661874,41.9287788807951));
#171090=CARTESIAN_POINT('Ctrl Pts',(74.6380926422076,9.20537831638721,41.9056217376954));
#171091=CARTESIAN_POINT('Ctrl Pts',(75.106018253574,8.96404741834731,41.8135204116345));
#171092=CARTESIAN_POINT('Ctrl Pts',(75.4467689884151,8.76189028604758,41.7465923191755));
#171093=CARTESIAN_POINT('Ctrl Pts',(76.0869348626083,8.32889507682514,41.6205837505826));
#171094=CARTESIAN_POINT('Ctrl Pts',(76.3870566723647,8.10031556226049,41.561374723565));
#171095=CARTESIAN_POINT('Ctrl Pts',(76.7765438108752,7.76749541067642,41.4838081207003));
#171096=CARTESIAN_POINT('Ctrl Pts',(76.8774633495982,7.67768718311102,41.4636368981732));
#171097=CARTESIAN_POINT('Ctrl Pts',(77.0518293647839,7.51612138903478,41.428616315608));
#171098=CARTESIAN_POINT('Ctrl Pts',(77.1260310612677,7.44523216914281,41.4136567295806));
#171099=CARTESIAN_POINT('Ctrl Pts',(77.2410925400592,7.33189808863244,41.3903532688205));
#171100=CARTESIAN_POINT('Ctrl Pts',(77.2826744187369,7.29021725883324,41.3819091198612));
#171101=CARTESIAN_POINT('Ctrl Pts',(77.3599430814493,7.21139676583721,41.3661715975547));
#171102=CARTESIAN_POINT('Ctrl Pts',(77.3957139398822,7.17434443853985,41.3588669591122));
#171103=CARTESIAN_POINT('Ctrl Pts',(77.4956308479103,7.06925111262193,41.3384123581069));
#171104=CARTESIAN_POINT('Ctrl Pts',(77.5591268084516,7.00058144592475,41.325353646242));
#171105=CARTESIAN_POINT('Ctrl Pts',(77.9195724797514,6.599756598571,41.2509104659163));
#171106=CARTESIAN_POINT('Ctrl Pts',(78.1955792805213,6.24883939102378,41.1926748869468));
#171107=CARTESIAN_POINT('Ctrl Pts',(78.7098957651985,5.49845019218121,41.0826207823401));
#171108=CARTESIAN_POINT('Ctrl Pts',(78.9458107585613,5.09851772952473,41.031258550513));
#171109=CARTESIAN_POINT('Ctrl Pts',(79.2174723675086,4.55742509420517,40.9712472424416));
#171110=CARTESIAN_POINT('Ctrl Pts',(79.2782138090284,4.42997847584416,40.9577570927977));
#171111=CARTESIAN_POINT('Ctrl Pts',(79.3768412566637,4.21161040246182,40.9357285122937));
#171112=CARTESIAN_POINT('Ctrl Pts',(79.4160675084637,4.1213432053878,40.9269300458601));
#171113=CARTESIAN_POINT('Ctrl Pts',(79.4936301304731,3.93564231489199,40.9094535020662));
#171114=CARTESIAN_POINT('Ctrl Pts',(79.5318451999104,3.84016787462365,40.900799126533));
#171115=CARTESIAN_POINT('Ctrl Pts',(79.6278364120737,3.58958159601358,40.8789389978898));
#171116=CARTESIAN_POINT('Ctrl Pts',(79.6833396296783,3.43359367398906,40.8661743422649));
#171117=CARTESIAN_POINT('Ctrl Pts',(79.9416392350219,2.64857230428485,40.8060544529767));
#171118=CARTESIAN_POINT('Ctrl Pts',(80.0879373965521,2.00181501077962,40.7696638583571));
#171119=CARTESIAN_POINT('Ctrl Pts',(80.1995400765391,1.12657467356358,40.735399786807));
#171120=CARTESIAN_POINT('Ctrl Pts',(80.2204452889702,0.907197634177053,
40.7280260479068));
#171121=CARTESIAN_POINT('Ctrl Pts',(80.2433907346824,0.544223252651627,
40.7176810132585));
#171122=CARTESIAN_POINT('Ctrl Pts',(80.2494678294453,0.400973136692729,
40.71407258984));
#171123=CARTESIAN_POINT('Ctrl Pts',(80.2539563570033,0.193552747041624,
40.7094954915821));
#171124=CARTESIAN_POINT('Ctrl Pts',(80.2547483208994,0.129459205751225,
40.7081705364979));
#171125=CARTESIAN_POINT('Ctrl Pts',(80.255100920087,0.0145775709653826,
40.7059514906647));
#171126=CARTESIAN_POINT('Ctrl Pts',(80.2548831092962,-0.0362062436283323,
40.7050247949784));
#171127=CARTESIAN_POINT('Ctrl Pts',(80.2535063607505,-0.154416988821826,
40.7029943333017));
#171128=CARTESIAN_POINT('Ctrl Pts',(80.2520624162441,-0.221838426712053,
40.7019326063345));
#171129=CARTESIAN_POINT('Ctrl Pts',(80.2451677638437,-0.442935493740978,
40.6987748722631));
#171130=CARTESIAN_POINT('Ctrl Pts',(80.2369549850655,-0.596510272815278,
40.6970953967244));
#171131=CARTESIAN_POINT('Ctrl Pts',(80.1634693289375,-1.56610449762325,
40.6899144716912));
#171132=CARTESIAN_POINT('Ctrl Pts',(80.0053183119484,-2.37226317618852,
40.6995494146783));
#171133=CARTESIAN_POINT('Ctrl Pts',(79.6963960163447,-3.332170090917,40.7334733134641));
#171134=CARTESIAN_POINT('Ctrl Pts',(79.6331912676002,-3.51155099444106,
40.7408180233016));
#171135=CARTESIAN_POINT('Ctrl Pts',(79.5265981742277,-3.78951510215392,
40.7537952416134));
#171136=CARTESIAN_POINT('Ctrl Pts',(79.4865245648172,-3.88935231860143,
40.7587859707903));
#171137=CARTESIAN_POINT('Ctrl Pts',(79.407419779681,-4.07790713533195,40.7688409796));
#171138=CARTESIAN_POINT('Ctrl Pts',(79.368681742007,-4.1667380292011,40.7738486070063));
#171139=CARTESIAN_POINT('Ctrl Pts',(79.2763176601259,-4.37069828847553,
40.7859726570874));
#171140=CARTESIAN_POINT('Ctrl Pts',(79.2218144948323,-4.48540258671413,
40.7932597806484));
#171141=CARTESIAN_POINT('Ctrl Pts',(79.0189807899978,-4.892797214755,40.8208200787647));
#171142=CARTESIAN_POINT('Ctrl Pts',(78.8589425892462,-5.17927701523856,
40.8433637815059));
#171143=CARTESIAN_POINT('Ctrl Pts',(78.4503012656289,-5.83533564463955,
40.9023110919439));
#171144=CARTESIAN_POINT('Ctrl Pts',(78.1909464253384,-6.19723727250574,
40.940731406425));
#171145=CARTESIAN_POINT('Ctrl Pts',(77.8167151048648,-6.65359690702007,
40.9965870950902));
#171146=CARTESIAN_POINT('Ctrl Pts',(77.721926373189,-6.7642804461397,41.0107638368156));
#171147=CARTESIAN_POINT('Ctrl Pts',(77.5525577052348,-6.95369539142955,
41.0360980070918));
#171148=CARTESIAN_POINT('Ctrl Pts',(77.4790197265573,-7.03334720038034,
41.0470987407664));
#171149=CARTESIAN_POINT('Ctrl Pts',(77.3627047132826,-7.15537022968237,
41.0644818265892));
#171150=CARTESIAN_POINT('Ctrl Pts',(77.3207898736863,-7.19856925942343,
41.0707426482386));
#171151=CARTESIAN_POINT('Ctrl Pts',(77.2376487384254,-7.28275170342843,
41.0831509789572));
#171152=CARTESIAN_POINT('Ctrl Pts',(77.1964493257227,-7.32375875748218,
41.089294665291));
#171153=CARTESIAN_POINT('Ctrl Pts',(77.0849042211385,-7.43289809342019,
41.1059190680632));
#171154=CARTESIAN_POINT('Ctrl Pts',(77.0139293706916,-7.50036556454618,
41.1164872961157));
#171155=CARTESIAN_POINT('Ctrl Pts',(76.6864070774697,-7.8028312059972,41.1652458625602));
#171156=CARTESIAN_POINT('Ctrl Pts',(76.4190165354946,-8.02548914234972,
41.2050323975225));
#171157=CARTESIAN_POINT('Ctrl Pts',(75.8366534024342,-8.46191632817427,
41.2922309507865));
#171158=CARTESIAN_POINT('Ctrl Pts',(75.5200232683736,-8.67253465312376,
41.3399444956717));
#171159=CARTESIAN_POINT('Ctrl Pts',(75.0932027642936,-8.92307973147675,
41.4049407542926));
#171160=CARTESIAN_POINT('Ctrl Pts',(74.992869920202,-8.97969578241385,41.4202646474527));
#171161=CARTESIAN_POINT('Ctrl Pts',(74.7424448216935,-9.11542310643498,
41.4586313394939));
#171162=CARTESIAN_POINT('Ctrl Pts',(74.591312786796,-9.19248002066406,41.4818896101064));
#171163=CARTESIAN_POINT('Ctrl Pts',(74.3454482934272,-9.31013546457496,
41.5198996829357));
#171164=CARTESIAN_POINT('Ctrl Pts',(74.2518781354646,-9.35316518107523,
41.5344045342761));
#171165=CARTESIAN_POINT('Ctrl Pts',(74.0695810462862,-9.43363974854203,
41.562738448414));
#171166=CARTESIAN_POINT('Ctrl Pts',(73.9809416416488,-9.47126169519278,
41.5765490803664));
#171167=CARTESIAN_POINT('Ctrl Pts',(73.7653626751441,-9.55913766853745,
41.6102166631081));
#171168=CARTESIAN_POINT('Ctrl Pts',(73.6379291640151,-9.60808632132263,
41.6301836765182));
#171169=CARTESIAN_POINT('Ctrl Pts',(73.073123924773,-9.81195026239119,41.7189444567463));
#171170=CARTESIAN_POINT('Ctrl Pts',(72.6266323311036,-9.93898254185201,
41.7898282484404));
#171171=CARTESIAN_POINT('Ctrl Pts',(71.7919835398247,-10.1150082328428,
41.9228213438546));
#171172=CARTESIAN_POINT('Ctrl Pts',(71.4065734074098,-10.1730658266453,
41.9844078439595));
#171173=CARTESIAN_POINT('Ctrl Pts',(70.8819130618401,-10.221009383761,42.0678801835785));
#171174=CARTESIAN_POINT('Ctrl Pts',(70.744805929142,-10.2306934508472,42.0896588226559));
#171175=CARTESIAN_POINT('Ctrl Pts',(70.5046670019219,-10.2426865429399,
42.1277015338923));
#171176=CARTESIAN_POINT('Ctrl Pts',(70.4017199527197,-10.2462348543771,
42.1439776443847));
#171177=CARTESIAN_POINT('Ctrl Pts',(70.2424081672662,-10.2492634056236,
42.1690983386118));
#171178=CARTESIAN_POINT('Ctrl Pts',(70.1860758048906,-10.2498583874661,
42.1779680568265));
#171179=CARTESIAN_POINT('Ctrl Pts',(70.0784109730032,-10.2500862104176,
42.1948921933579));
#171180=CARTESIAN_POINT('Ctrl Pts',(70.0270811673423,-10.249799880826,42.202948428152));
#171181=CARTESIAN_POINT('Ctrl Pts',(69.8952185046746,-10.2480497692699,
42.2236150272714));
#171182=CARTESIAN_POINT('Ctrl Pts',(69.8146939112116,-10.2460087084472,
42.2362075318369));
#171183=CARTESIAN_POINT('Ctrl Pts',(69.4311997185964,-10.2316554002495,
42.2960661450067));
#171184=CARTESIAN_POINT('Ctrl Pts',(69.1288032560586,-10.2065539130263,
42.3429353815764));
#171185=CARTESIAN_POINT('Ctrl Pts',(68.3448741127029,-10.1054881116976,
42.4641052211933));
#171186=CARTESIAN_POINT('Ctrl Pts',(67.8667957127787,-10.0080528806127,
42.5376930843337));
#171187=CARTESIAN_POINT('Ctrl Pts',(67.210734278808,-9.82373831792741,42.6389832248867));
#171188=CARTESIAN_POINT('Ctrl Pts',(67.0254614860757,-9.76584396775118,
42.6676183412889));
#171189=CARTESIAN_POINT('Ctrl Pts',(66.6914602635536,-9.65074918116083,
42.7193214625833));
#171190=CARTESIAN_POINT('Ctrl Pts',(66.5422011822621,-9.59531431834851,
42.7424566756313));
#171191=CARTESIAN_POINT('Ctrl Pts',(66.3003003397803,-9.4988739277754,42.780003460665));
#171192=CARTESIAN_POINT('Ctrl Pts',(66.206864161016,-9.45997862245632,42.7945190799848));
#171193=CARTESIAN_POINT('Ctrl Pts',(66.0247675191537,-9.38093144995062,
42.8228323310797));
#171194=CARTESIAN_POINT('Ctrl Pts',(65.9360716464283,-9.34089050952548,
42.8366345313369));
#171195=CARTESIAN_POINT('Ctrl Pts',(65.7183198397622,-9.23876254125689,
42.8705441520899));
#171196=CARTESIAN_POINT('Ctrl Pts',(65.5899689257589,-9.17519101207616,
42.8905536483184));
#171197=CARTESIAN_POINT('Ctrl Pts',(65.0019901980299,-8.86819225514824,
42.982285489555));
#171198=CARTESIAN_POINT('Ctrl Pts',(64.5599807279445,-8.5920108761144,43.0514825197807));
#171199=CARTESIAN_POINT('Ctrl Pts',(63.8385401500208,-8.05988720219786,
43.1636036880936));
#171200=CARTESIAN_POINT('Ctrl Pts',(63.548724571481,-7.82022914357439,43.2083693712019));
#171201=CARTESIAN_POINT('Ctrl Pts',(63.2010465706138,-7.49880992345238,
43.2611688632362));
#171202=CARTESIAN_POINT('Ctrl Pts',(63.1304731108674,-7.4316715860082,43.2718352988815));
#171203=CARTESIAN_POINT('Ctrl Pts',(63.019390249814,-7.32293441139376,43.2885280859276));
#171204=CARTESIAN_POINT('Ctrl Pts',(62.9782678448442,-7.28199058140089,
43.2946859857017));
#171205=CARTESIAN_POINT('Ctrl Pts',(62.8951149025589,-7.197781174401,43.3070894314852));
#171206=CARTESIAN_POINT('Ctrl Pts',(62.8531136598361,-7.15448927420012,
43.3133288946496));
#171207=CARTESIAN_POINT('Ctrl Pts',(62.7362667739382,-7.03190687389094,
43.3306194702127));
#171208=CARTESIAN_POINT('Ctrl Pts',(62.6622864964652,-6.95177688158209,
43.3414875602269));
#171209=CARTESIAN_POINT('Ctrl Pts',(62.4916563702286,-6.76094917609823,
43.3663886209964));
#171210=CARTESIAN_POINT('Ctrl Pts',(62.3960632753648,-6.64931087552116,
43.3802091111123));
#171211=CARTESIAN_POINT('Ctrl Pts',(62.0154123502092,-6.18495979641894,
43.4347904284973));
#171212=CARTESIAN_POINT('Ctrl Pts',(61.7512251719933,-5.81534570084265,
43.4716146726948));
#171213=CARTESIAN_POINT('Ctrl Pts',(61.3448960495976,-5.1591306179987,43.5271123087567));
#171214=CARTESIAN_POINT('Ctrl Pts',(61.1901527276195,-4.88130754176526,
43.547879498298));
#171215=CARTESIAN_POINT('Ctrl Pts',(60.9919903885807,-4.48330927718824,
43.5740179079228));
#171216=CARTESIAN_POINT('Ctrl Pts',(60.9376309207981,-4.36890195438882,
43.5811307878231));
#171217=CARTESIAN_POINT('Ctrl Pts',(60.8454328724955,-4.16527582899965,
43.5930913611281));
#171218=CARTESIAN_POINT('Ctrl Pts',(60.806722155446,-4.07647757889274,43.5980774865959));
#171219=CARTESIAN_POINT('Ctrl Pts',(60.7276048238023,-3.8877922035273,43.6081895033886));
#171220=CARTESIAN_POINT('Ctrl Pts',(60.6874990306224,-3.78778913082878,
43.6132678560022));
#171221=CARTESIAN_POINT('Ctrl Pts',(60.5806290917482,-3.50876749973317,
43.626658658446));
#171222=CARTESIAN_POINT('Ctrl Pts',(60.5172424990888,-3.32847745506082,
43.6344346924671));
#171223=CARTESIAN_POINT('Ctrl Pts',(60.2076167799292,-2.36324238070314,
43.671375970447));
#171224=CARTESIAN_POINT('Ctrl Pts',(60.0504624715391,-1.55243489538217,
43.6864193700675));
#171225=CARTESIAN_POINT('Ctrl Pts',(59.9792450557694,-0.582489999898303,
43.6822138483795));
#171226=CARTESIAN_POINT('Ctrl Pts',(59.9715017252469,-0.433189199583286,
43.6809465333485));
#171227=CARTESIAN_POINT('Ctrl Pts',(59.9649354564718,-0.217092509485996,
43.6781744434392));
#171228=CARTESIAN_POINT('Ctrl Pts',(59.9635474472644,-0.150387540702407,
43.6771896383154));
#171229=CARTESIAN_POINT('Ctrl Pts',(59.9624839812393,-0.0557842688263437,
43.6756060404254));
#171230=CARTESIAN_POINT('Ctrl Pts',(59.9622819875824,-0.0278921387390975,
43.675116105672));
#171231=CARTESIAN_POINT('Ctrl Pts',(59.9621915011161,1.31067303586202E-9,
43.6746029314002));
#171232=CARTESIAN_POINT('Ctrl Pts',(59.9459911121981,-7.28640352773959E-10,
43.5827259602593));
#171233=CARTESIAN_POINT('Ctrl Pts',(59.9460375900799,-0.0143266460599373,
43.5829895494194));
#171234=CARTESIAN_POINT('Ctrl Pts',(59.946113810169,-0.0286533381359354,
43.5832488390263));
#171235=CARTESIAN_POINT('Ctrl Pts',(59.9466646997059,-0.103139137788873,
43.5845744266029));
#171236=CARTESIAN_POINT('Ctrl Pts',(59.9476339701448,-0.163294614590786,
43.585568729974));
#171237=CARTESIAN_POINT('Ctrl Pts',(59.9521211302597,-0.344036513006118,
43.588321807074));
#171238=CARTESIAN_POINT('Ctrl Pts',(59.957221110632,-0.464576916028509,
43.5898441921207));
#171239=CARTESIAN_POINT('Ctrl Pts',(59.9952440979856,-1.10044949754627,
43.5961474971593));
#171240=CARTESIAN_POINT('Ctrl Pts',(60.0644986283257,-1.61293018088451,
43.5951938415123));
#171241=CARTESIAN_POINT('Ctrl Pts',(60.2491038566319,-2.48481286991128,
43.5817148185854));
#171242=CARTESIAN_POINT('Ctrl Pts',(60.3464892490603,-2.84703270485521,
43.5724493086601));
#171243=CARTESIAN_POINT('Ctrl Pts',(60.5191319917585,-3.37397908844107,
43.5532653883163));
#171244=CARTESIAN_POINT('Ctrl Pts',(60.5795257731593,-3.543349290979,43.5461983962768));
#171245=CARTESIAN_POINT('Ctrl Pts',(60.6823277489088,-3.80962222417279,
43.5336394321642));
#171246=CARTESIAN_POINT('Ctrl Pts',(60.7218859029594,-3.90761074021264,
43.5286993712111));
#171247=CARTESIAN_POINT('Ctrl Pts',(60.800796383866,-4.09480154908873,43.5186475891421));
#171248=CARTESIAN_POINT('Ctrl Pts',(60.8399245364853,-4.18408823367254,
43.513579128566));
#171249=CARTESIAN_POINT('Ctrl Pts',(60.9356783573457,-4.3944786241219,43.5009853742053));
#171250=CARTESIAN_POINT('Ctrl Pts',(60.9933931351928,-4.51505409487973,
43.4932481998287));
#171251=CARTESIAN_POINT('Ctrl Pts',(61.3342139881777,-5.19309496507027,
43.4467919855794));
#171252=CARTESIAN_POINT('Ctrl Pts',(61.6646959979008,-5.72460664695023,
43.3988158979195));
#171253=CARTESIAN_POINT('Ctrl Pts',(62.1758565580389,-6.40081490004067,
43.3229576775345));
#171254=CARTESIAN_POINT('Ctrl Pts',(62.3165378614139,-6.57478569882454,
43.3019529901831));
#171255=CARTESIAN_POINT('Ctrl Pts',(62.5574355865755,-6.85348034838193,
43.2659333134321));
#171256=CARTESIAN_POINT('Ctrl Pts',(62.6544107220027,-6.96096753278267,
43.2514209122878));
#171257=CARTESIAN_POINT('Ctrl Pts',(62.799353378053,-7.11490539940208,43.2297523322832));
#171258=CARTESIAN_POINT('Ctrl Pts',(62.8455598722524,-7.16302442308203,
43.2228477554537));
#171259=CARTESIAN_POINT('Ctrl Pts',(62.9309109399163,-7.25017857204365,
43.2101047413057));
#171260=CARTESIAN_POINT('Ctrl Pts',(62.9699081272575,-7.2893563376217,43.2042869120689));
#171261=CARTESIAN_POINT('Ctrl Pts',(63.0665960901053,-7.38492314733817,
43.1898717121464));
#171262=CARTESIAN_POINT('Ctrl Pts',(63.1246379911191,-7.44094407153647,
43.1812257756037));
#171263=CARTESIAN_POINT('Ctrl Pts',(63.3731532484376,-7.675167396915,43.1442206188697));
#171264=CARTESIAN_POINT('Ctrl Pts',(63.5697038420368,-7.84664015300446,
43.114984867416));
#171265=CARTESIAN_POINT('Ctrl Pts',(64.1352126644439,-8.30296019081711,
43.0306020645529));
#171266=CARTESIAN_POINT('Ctrl Pts',(64.5172977653965,-8.57011422427541,
42.9732714676007));
#171267=CARTESIAN_POINT('Ctrl Pts',(65.0745654338905,-8.90522790379286,
42.8885664899947));
#171268=CARTESIAN_POINT('Ctrl Pts',(65.2356545641202,-8.99618558198695,
42.8639666151387));
#171269=CARTESIAN_POINT('Ctrl Pts',(65.5336148410308,-9.15381648743382,
42.8182344431816));
#171270=CARTESIAN_POINT('Ctrl Pts',(65.6696924087366,-9.22191951265763,
42.7972643415207));
#171271=CARTESIAN_POINT('Ctrl Pts',(65.8974898533498,-9.32956159898774,
42.7620168084714));
#171272=CARTESIAN_POINT('Ctrl Pts',(65.9883735920149,-9.3708692046486,42.7479174718631));
#171273=CARTESIAN_POINT('Ctrl Pts',(66.1711273838748,-9.45068162080295,
42.7194933426395));
#171274=CARTESIAN_POINT('Ctrl Pts',(66.2629851798873,-9.48918732474518,
42.705170595965));
#171275=CARTESIAN_POINT('Ctrl Pts',(66.4949577457651,-9.58240888751211,
42.6689138259321));
#171276=CARTESIAN_POINT('Ctrl Pts',(66.6357353503896,-9.63535125544396,
42.6468318910217));
#171277=CARTESIAN_POINT('Ctrl Pts',(67.3100766137265,-9.87183714434973,
42.5407200531307));
#171278=CARTESIAN_POINT('Ctrl Pts',(67.8568336237306,-10.0132608371559,
42.4536330517418));
#171279=CARTESIAN_POINT('Ctrl Pts',(68.8275881304431,-10.1786493093381,
42.2987866733099));
#171280=CARTESIAN_POINT('Ctrl Pts',(69.2467769037161,-10.223093001542,42.2318708571912));
#171281=CARTESIAN_POINT('Ctrl Pts',(69.7566209836434,-10.2447623578791,
42.1511825076571));
#171282=CARTESIAN_POINT('Ctrl Pts',(69.8457224560884,-10.2473567790266,
42.1371075889581));
#171283=CARTESIAN_POINT('Ctrl Pts',(69.9883517930055,-10.2496024647024,
42.1146302327215));
#171284=CARTESIAN_POINT('Ctrl Pts',(70.0418599869951,-10.2500156234435,
42.1062096836316));
#171285=CARTESIAN_POINT('Ctrl Pts',(70.149518156792,-10.2499832824638,42.0892946883698));
#171286=CARTESIAN_POINT('Ctrl Pts',(70.2036663937296,-10.2495275185122,
42.0808007840563));
#171287=CARTESIAN_POINT('Ctrl Pts',(70.3500372849288,-10.2471074464185,
42.0578739302752));
#171288=CARTESIAN_POINT('Ctrl Pts',(70.4422449880518,-10.2443076647194,
42.0434668380879));
#171289=CARTESIAN_POINT('Ctrl Pts',(71.022766247079,-10.2186465656209,41.9529479927956));
#171290=CARTESIAN_POINT('Ctrl Pts',(71.5090751876544,-10.1613175233665,
41.8779170190555));
#171291=CARTESIAN_POINT('Ctrl Pts',(72.4346805892153,-9.98283080432906,
41.7351742488077));
#171292=CARTESIAN_POINT('Ctrl Pts',(72.8737854201792,-9.86683159229917,
41.6674861722385));
#171293=CARTESIAN_POINT('Ctrl Pts',(73.4640988682087,-9.66724560127392,
41.5761341899508));
#171294=CARTESIAN_POINT('Ctrl Pts',(73.6231304500029,-9.60895774775429,
41.5514904435393));
#171295=CARTESIAN_POINT('Ctrl Pts',(73.8764955096983,-9.50876261489964,
41.512170585656));
#171296=CARTESIAN_POINT('Ctrl Pts',(73.971772300336,-9.4693801852802,41.4973711659113));
#171297=CARTESIAN_POINT('Ctrl Pts',(74.1557884221983,-9.38998415419588,
41.4687630291964));
#171298=CARTESIAN_POINT('Ctrl Pts',(74.2445848466483,-9.35013427435378,
41.4549468436074));
#171299=CARTESIAN_POINT('Ctrl Pts',(74.4571581255323,-9.25100800216019,
41.4218473526083));
#171300=CARTESIAN_POINT('Ctrl Pts',(74.580338722039,-9.19047211405968,41.4026467156689));
#171301=CARTESIAN_POINT('Ctrl Pts',(75.2248689893672,-8.85721022430065,
41.3021063109763));
#171302=CARTESIAN_POINT('Ctrl Pts',(75.7232208935052,-8.54154437581208,
41.2240334446168));
#171303=CARTESIAN_POINT('Ctrl Pts',(76.3797857300465,-8.04063741825332,
41.1221956496918));
#171304=CARTESIAN_POINT('Ctrl Pts',(76.5627223540064,-7.89069744434567,
41.0939557778104));
#171305=CARTESIAN_POINT('Ctrl Pts',(76.8529490302931,-7.63543627012667,
41.0495539337904));
#171306=CARTESIAN_POINT('Ctrl Pts',(76.9633673714707,-7.53392065665673,
41.0327627421851));
#171307=CARTESIAN_POINT('Ctrl Pts',(77.1202509238951,-7.38318789238706,
41.0091001727908));
#171308=CARTESIAN_POINT('Ctrl Pts',(77.1684938332366,-7.33590959851867,
41.0018515246761));
#171309=CARTESIAN_POINT('Ctrl Pts',(77.2552570340658,-7.24918325001962,
40.9888712799995));
#171310=CARTESIAN_POINT('Ctrl Pts',(77.2939302737214,-7.20989801632789,
40.9831068009904));
#171311=CARTESIAN_POINT('Ctrl Pts',(77.3874447105696,-7.11335930622603,
40.9692187416404));
#171312=CARTESIAN_POINT('Ctrl Pts',(77.4419476727918,-7.05577317682132,
40.9611673409808));
#171313=CARTESIAN_POINT('Ctrl Pts',(77.6587057174443,-6.82137060509613,
40.9293059857636));
#171314=CARTESIAN_POINT('Ctrl Pts',(77.8154820958198,-6.6394385941867,40.9066261575104));
#171315=CARTESIAN_POINT('Ctrl Pts',(78.1833153722474,-6.18102325609108,
40.8540994115583));
#171316=CARTESIAN_POINT('Ctrl Pts',(78.3870793060089,-5.89891689248128,
40.8256083292068));
#171317=CARTESIAN_POINT('Ctrl Pts',(78.7407995616609,-5.35289045722612,
40.7769456644645));
#171318=CARTESIAN_POINT('Ctrl Pts',(78.8941341991853,-5.09165831176914,
40.7561986658561));
#171319=CARTESIAN_POINT('Ctrl Pts',(79.114079668581,-4.67603162253496,40.726895501663));
#171320=CARTESIAN_POINT('Ctrl Pts',(79.1887622655494,-4.52619813869404,
40.7170439350763));
#171321=CARTESIAN_POINT('Ctrl Pts',(79.3035589219681,-4.28112993192916,
40.7020599920552));
#171322=CARTESIAN_POINT('Ctrl Pts',(79.3459375623717,-4.18701268434998,
40.6965679481115));
#171323=CARTESIAN_POINT('Ctrl Pts',(79.4255869180075,-4.00279687151226,
40.6863253375304));
#171324=CARTESIAN_POINT('Ctrl Pts',(79.4630065666425,-3.912776019988,40.6815510433645));
#171325=CARTESIAN_POINT('Ctrl Pts',(79.5510186649322,-3.69229658560822,
40.6704188464459));
#171326=CARTESIAN_POINT('Ctrl Pts',(79.6002509572031,-3.56130564516457,
40.6642765731327));
#171327=CARTESIAN_POINT('Ctrl Pts',(79.8734219276251,-2.78716581397686,
40.630750261085));
#171328=CARTESIAN_POINT('Ctrl Pts',(80.036199019137,-2.12385049578148,40.6130137092608));
#171329=CARTESIAN_POINT('Ctrl Pts',(80.1674515416969,-1.2091924592492,40.6050775418096));
#171330=CARTESIAN_POINT('Ctrl Pts',(80.1935067487899,-0.967989845444839,
40.6045162377913));
#171331=CARTESIAN_POINT('Ctrl Pts',(80.2189222227205,-0.619335059196382,
40.606063448969));
#171332=CARTESIAN_POINT('Ctrl Pts',(80.2250626423124,-0.512455059801902,
40.6068558946787));
#171333=CARTESIAN_POINT('Ctrl Pts',(80.2331722425514,-0.31960774339719,
40.6088780251448));
#171334=CARTESIAN_POINT('Ctrl Pts',(80.2357243293705,-0.233673779241834,
40.6099908389222));
#171335=CARTESIAN_POINT('Ctrl Pts',(80.2381424332421,-0.0944225953100012,
40.6121463084135));
#171336=CARTESIAN_POINT('Ctrl Pts',(80.2386605338121,-0.0411186812615804,
40.6130549964071));
#171337=CARTESIAN_POINT('Ctrl Pts',(80.2388875538814,0.068039035736405,
40.615089812499));
#171338=CARTESIAN_POINT('Ctrl Pts',(80.2385565526446,0.123890759317233,
40.6162240313559));
#171339=CARTESIAN_POINT('Ctrl Pts',(80.2364058055572,0.278197784409159,
40.6196109858607));
#171340=CARTESIAN_POINT('Ctrl Pts',(80.2336427929077,0.37662978697222,40.6220565484951));
#171341=CARTESIAN_POINT('Ctrl Pts',(80.2103218164168,0.928889356995538,
40.6373367883457));
#171342=CARTESIAN_POINT('Ctrl Pts',(80.1615626044225,1.38087278303248,40.6557394214364));
#171343=CARTESIAN_POINT('Ctrl Pts',(80.0199125654128,2.19143526620157,40.6984158437578));
#171344=CARTESIAN_POINT('Ctrl Pts',(79.9370832874237,2.55108783377926,40.7209201867642));
#171345=CARTESIAN_POINT('Ctrl Pts',(79.7881175342793,3.06943055637364,40.75837518173));
#171346=CARTESIAN_POINT('Ctrl Pts',(79.736912265311,3.23227915737716,40.7708918470471));
#171347=CARTESIAN_POINT('Ctrl Pts',(79.634702643799,3.5311982057483,40.7952517888642));
#171348=CARTESIAN_POINT('Ctrl Pts',(79.5848110211136,3.66761744394733,40.8069160276739));
#171349=CARTESIAN_POINT('Ctrl Pts',(79.496038160898,3.89529874403081,40.8273101327712));
#171350=CARTESIAN_POINT('Ctrl Pts',(79.4586850379013,3.98715464255901,40.8357970317134));
#171351=CARTESIAN_POINT('Ctrl Pts',(79.385012852756,4.16107311123714,40.852364021814));
#171352=CARTESIAN_POINT('Ctrl Pts',(79.3489345058583,4.2432311709102,40.8604057255209));
#171353=CARTESIAN_POINT('Ctrl Pts',(79.2502716536176,4.46014513185474,40.8822163440565));
#171354=CARTESIAN_POINT('Ctrl Pts',(79.1858424905868,4.59400837202528,40.8962775208754));
#171355=CARTESIAN_POINT('Ctrl Pts',(78.9381167390807,5.08134239878733,40.9497345341578));
#171356=CARTESIAN_POINT('Ctrl Pts',(78.7373149201773,5.42519801935659,40.9919164317268));
#171357=CARTESIAN_POINT('Ctrl Pts',(78.3217323578381,6.05019069970159,41.077833175774));
#171358=CARTESIAN_POINT('Ctrl Pts',(78.1113059835995,6.33361571499208,41.1208130307063));
#171359=CARTESIAN_POINT('Ctrl Pts',(77.8034569838703,6.70627120459286,41.1834732485849));
#171360=CARTESIAN_POINT('Ctrl Pts',(77.7181519512505,6.80557187567079,41.2008167853645));
#171361=CARTESIAN_POINT('Ctrl Pts',(77.5641791857886,6.97797051420906,41.232122576725));
#171362=CARTESIAN_POINT('Ctrl Pts',(77.4962853560562,7.05176390492606,41.2459272234256));
#171363=CARTESIAN_POINT('Ctrl Pts',(77.3871513568511,7.166917943456,41.2681328440385));
#171364=CARTESIAN_POINT('Ctrl Pts',(77.3466117927354,7.20896209254216,41.2763848102507));
#171365=CARTESIAN_POINT('Ctrl Pts',(77.2694152287003,7.28765533835146,41.2921083239062));
#171366=CARTESIAN_POINT('Ctrl Pts',(77.2328340306705,7.32437933958338,41.2995632703786));
#171367=CARTESIAN_POINT('Ctrl Pts',(77.1280766959687,7.42794721872118,41.3209200009373));
#171368=CARTESIAN_POINT('Ctrl Pts',(77.0592505971471,7.49409711798191,41.3349609988095));
#171369=CARTESIAN_POINT('Ctrl Pts',(76.6173294068665,7.90698117658797,41.4251309402652));
#171370=CARTESIAN_POINT('Ctrl Pts',(76.2199922768251,8.22560935912857,41.5062352773913));
#171371=CARTESIAN_POINT('Ctrl Pts',(75.4832917644561,8.72959773806129,41.6552044139016));
#171372=CARTESIAN_POINT('Ctrl Pts',(75.1538759892047,8.92812337330524,41.7213883313959));
#171373=CARTESIAN_POINT('Ctrl Pts',(74.6875133322545,9.17366615781197,41.814289648415));
#171374=CARTESIAN_POINT('Ctrl Pts',(74.5595694582691,9.237549914246,41.8397002935372));
#171375=CARTESIAN_POINT('Ctrl Pts',(74.3418879498715,9.34044343571355,41.8828027581011));
#171376=CARTESIAN_POINT('Ctrl Pts',(74.2528545331535,9.38093242200543,41.9003960884452));
#171377=CARTESIAN_POINT('Ctrl Pts',(74.0819289368364,9.45564015737336,41.9341041063845));
#171378=CARTESIAN_POINT('Ctrl Pts',(74.000144760869,9.49008927924609,41.9502037038238));
#171379=CARTESIAN_POINT('Ctrl Pts',(73.781501364439,9.57875718641313,41.9931701847553));
#171380=CARTESIAN_POINT('Ctrl Pts',(73.6438965685247,9.63103035949489,42.0201345343597));
#171381=CARTESIAN_POINT('Ctrl Pts',(72.9410820168122,9.88027937791589,42.1575026697587));
#171382=CARTESIAN_POINT('Ctrl Pts',(72.3603789891852,10.028767605135,42.2697834155235));
#171383=CARTESIAN_POINT('Ctrl Pts',(71.502079616051,10.1671413440725,42.4356364628139));
#171384=CARTESIAN_POINT('Ctrl Pts',(71.2323799028694,10.1993012234798,42.4877518500749));
#171385=CARTESIAN_POINT('Ctrl Pts',(70.8487744119882,10.2290971665373,42.5621153328345));
#171386=CARTESIAN_POINT('Ctrl Pts',(70.7356517164443,10.2359292629871,42.584074144077));
#171387=CARTESIAN_POINT('Ctrl Pts',(70.5332716509214,10.2446623340606,42.6234364358077));
#171388=CARTESIAN_POINT('Ctrl Pts',(70.4440540624603,10.2473017608102,42.640815805587));
#171389=CARTESIAN_POINT('Ctrl Pts',(70.3015238058131,10.2495859655522,42.6686344253381));
#171390=CARTESIAN_POINT('Ctrl Pts',(70.2482238541103,10.2500086536731,42.6790494262501));
#171391=CARTESIAN_POINT('Ctrl Pts',(70.1412820663025,10.2499910209053,42.6999735552205));
#171392=CARTESIAN_POINT('Ctrl Pts',(70.0876419906215,10.2495450902793,42.7104824859471));
#171393=CARTESIAN_POINT('Ctrl Pts',(69.9431202514993,10.2471657637742,42.7388299870026));
#171394=CARTESIAN_POINT('Ctrl Pts',(69.852260865597,10.2444143332145,42.7566873966239));
#171395=CARTESIAN_POINT('Ctrl Pts',(69.2578523779148,10.2181930521271,42.8737033210349));
#171396=CARTESIAN_POINT('Ctrl Pts',(68.7567501112307,10.1574351896112,42.9732171057245));
#171397=CARTESIAN_POINT('Ctrl Pts',(67.7885712796517,9.96402834930255,43.16551229296));
#171398=CARTESIAN_POINT('Ctrl Pts',(67.3221959485919,9.83476678771789,43.2581496903659));
#171399=CARTESIAN_POINT('Ctrl Pts',(66.7318003060275,9.62363010938942,43.3750098951206));
#171400=CARTESIAN_POINT('Ctrl Pts',(66.5979465520151,9.57247178701405,43.4014788638174));
#171401=CARTESIAN_POINT('Ctrl Pts',(66.3745381330922,9.48150719916644,43.4456127821913));
#171402=CARTESIAN_POINT('Ctrl Pts',(66.2844032180224,9.44324792314643,43.4634065243943));
#171403=CARTESIAN_POINT('Ctrl Pts',(66.1137386736809,9.36781801758265,43.4970758814441));
#171404=CARTESIAN_POINT('Ctrl Pts',(66.0331157095046,9.33089108775091,43.5129720104634));
#171405=CARTESIAN_POINT('Ctrl Pts',(65.8202489540236,9.22993809552489,43.5549199188208));
#171406=CARTESIAN_POINT('Ctrl Pts',(65.6888786706006,9.16404454290439,43.5807846723764));
#171407=CARTESIAN_POINT('Ctrl Pts',(65.2085602447716,8.90970766782227,43.675296153065));
#171408=CARTESIAN_POINT('Ctrl Pts',(64.8691603666153,8.70329799202075,43.7419543654796));
#171409=CARTESIAN_POINT('Ctrl Pts',(64.1985032119731,8.23877372854175,43.8740335738653));
#171410=CARTESIAN_POINT('Ctrl Pts',(63.8693083531321,7.97893375500673,43.9390700456032));
#171411=CARTESIAN_POINT('Ctrl Pts',(63.4548230651222,7.60752724362429,44.0219980900755));
#171412=CARTESIAN_POINT('Ctrl Pts',(63.3545087620615,7.51387866073428,44.0421584804766));
#171413=CARTESIAN_POINT('Ctrl Pts',(63.2093224476735,7.37268393367582,44.0715075251689));
#171414=CARTESIAN_POINT('Ctrl Pts',(63.1629719911126,7.32672431201815,44.0809038283794));
#171415=CARTESIAN_POINT('Ctrl Pts',(63.0781916190838,7.24101109611234,44.0981454549373));
#171416=CARTESIAN_POINT('Ctrl Pts',(63.0396383023116,7.2013875802826,44.1060078610015));
#171417=CARTESIAN_POINT('Ctrl Pts',(62.9444561668407,7.10194209022563,44.1254717352569));
#171418=CARTESIAN_POINT('Ctrl Pts',(62.8882245884188,7.04173459229395,44.1370176684737));
#171419=CARTESIAN_POINT('Ctrl Pts',(62.6389037039307,6.76815901836654,44.1884040771738));
#171420=CARTESIAN_POINT('Ctrl Pts',(62.4541192736215,6.5471721156624,44.2270191408352));
#171421=CARTESIAN_POINT('Ctrl Pts',(62.0101297946349,5.96786206652741,44.3207776041163));
#171422=CARTESIAN_POINT('Ctrl Pts',(61.7642248934756,5.59973148773273,44.3736457813584));
#171423=CARTESIAN_POINT('Ctrl Pts',(61.4517708519255,5.05926852203045,44.4417054306874));
#171424=CARTESIAN_POINT('Ctrl Pts',(61.3650571102148,4.89965697625828,44.4607139226006));
#171425=CARTESIAN_POINT('Ctrl Pts',(61.2142568371581,4.6036621360204,44.4939773213363));
#171426=CARTESIAN_POINT('Ctrl Pts',(61.1488601915217,4.46803248006192,44.5084840868057));
#171427=CARTESIAN_POINT('Ctrl Pts',(61.0449929553346,4.23998572462094,44.531661998768));
#171428=CARTESIAN_POINT('Ctrl Pts',(61.004866833588,4.14838192684605,44.5406543052984));
#171429=CARTESIAN_POINT('Ctrl Pts',(60.9270231008684,3.96341078168895,44.5581787743077));
#171430=CARTESIAN_POINT('Ctrl Pts',(60.8893267034365,3.87004614627509,44.5667066831668));
#171431=CARTESIAN_POINT('Ctrl Pts',(60.7974910126167,3.6326660703553,44.5875938759801));
#171432=CARTESIAN_POINT('Ctrl Pts',(60.7451781959886,3.48794028136869,44.599598575301));
#171433=CARTESIAN_POINT('Ctrl Pts',(60.5279615902703,2.84235242295893,44.6499801348749));
#171434=CARTESIAN_POINT('Ctrl Pts',(60.3980370108493,2.33005966651555,44.6815814004138));
#171435=CARTESIAN_POINT('Ctrl Pts',(60.252064560178,1.49022692120604,44.7212881957219));
#171436=CARTESIAN_POINT('Ctrl Pts',(60.2115056883058,1.16814721753628,44.7337442901996));
#171437=CARTESIAN_POINT('Ctrl Pts',(60.1718904704918,0.663491986028091,
44.7493674512558));
#171438=CARTESIAN_POINT('Ctrl Pts',(60.1624315563092,0.48200272453448,44.7542083558063));
#171439=CARTESIAN_POINT('Ctrl Pts',(60.1559568484478,0.230712323472897,
44.7599097471535));
#171440=CARTESIAN_POINT('Ctrl Pts',(60.1548649575305,0.161064386341852,
44.7613837534939));
#171441=CARTESIAN_POINT('Ctrl Pts',(60.1543057576669,0.0609395441185803,
44.763354614216));
#171442=CARTESIAN_POINT('Ctrl Pts',(60.1542700764961,0.0304698290536312,
44.7639346639111));
#171443=CARTESIAN_POINT('Ctrl Pts',(60.1543689253998,-1.15483570402281E-9,
44.7644952638818));
#171444=CARTESIAN_POINT('Origin',(69.7358040552328,0.,40.0761166693274));
#171445=CARTESIAN_POINT('',(60.3789471275204,6.59340593767212E-11,46.0381415386512));
#171446=CARTESIAN_POINT('',(60.3627467385963,-5.75426767521213E-14,45.9462645674752));
#171447=CARTESIAN_POINT('',(59.6415245868576,-1.25526296912604E-15,41.8560104904131));
#171448=CARTESIAN_POINT('Ctrl Pts',(60.3789471275204,1.31869374016412E-10,
46.0381415386512));
#171449=CARTESIAN_POINT('Ctrl Pts',(60.378925330733,0.00671878418599705,
46.0380179229264));
#171450=CARTESIAN_POINT('Ctrl Pts',(60.3789100041966,0.0134375803992449,
46.03789295849));
#171451=CARTESIAN_POINT('Ctrl Pts',(60.3788262141627,0.0770085414268258,
46.0366978518554));
#171452=CARTESIAN_POINT('Ctrl Pts',(60.3792145896087,0.133858539604107,
46.0355327241613));
#171453=CARTESIAN_POINT('Ctrl Pts',(60.3816162978435,0.294110881741993,
46.0319808432064));
#171454=CARTESIAN_POINT('Ctrl Pts',(60.3847000954561,0.397485575382497,
46.0293755110242));
#171455=CARTESIAN_POINT('Ctrl Pts',(60.3954619430938,0.6382170946337,46.0225960466755));
#171456=CARTESIAN_POINT('Ctrl Pts',(60.4043200761219,0.775495110568486,
46.0181887322636));
#171457=CARTESIAN_POINT('Ctrl Pts',(60.448292680914,1.29632651977757,45.9994785111034));
#171458=CARTESIAN_POINT('Ctrl Pts',(60.5019329936339,1.67787306614414,45.9816710352204));
#171459=CARTESIAN_POINT('Ctrl Pts',(60.6620634989202,2.48730663859187,45.9357303979089));
#171460=CARTESIAN_POINT('Ctrl Pts',(60.7748970488261,2.91310231641818,45.90653366641));
#171461=CARTESIAN_POINT('Ctrl Pts',(60.9639494315895,3.47799654954706,45.861190457982));
#171462=CARTESIAN_POINT('Ctrl Pts',(61.0167828669662,3.62471447983636,45.8487843676519));
#171463=CARTESIAN_POINT('Ctrl Pts',(61.1093058311519,3.86442905708134,45.8274710075018));
#171464=CARTESIAN_POINT('Ctrl Pts',(61.1470804203344,3.95816360141092,45.8188682644958));
#171465=CARTESIAN_POINT('Ctrl Pts',(61.2248439682433,4.1432143670693,45.8013463007918));
#171466=CARTESIAN_POINT('Ctrl Pts',(61.2647925358388,4.23453613561547,45.7924337659594));
#171467=CARTESIAN_POINT('Ctrl Pts',(61.3676281751315,4.46060148906893,45.7697012294424));
#171468=CARTESIAN_POINT('Ctrl Pts',(61.432115085293,4.59456594006168,45.7556278819492));
#171469=CARTESIAN_POINT('Ctrl Pts',(61.6895592808755,5.10092843623557,45.7000757073256));
#171470=CARTESIAN_POINT('Ctrl Pts',(61.9022396526794,5.46247757645872,45.6554597151197));
#171471=CARTESIAN_POINT('Ctrl Pts',(62.4053327784477,6.2088495327472,45.5516080363524));
#171472=CARTESIAN_POINT('Ctrl Pts',(62.7019803653381,6.58808203293475,45.4913166879943));
#171473=CARTESIAN_POINT('Ctrl Pts',(63.0844067574181,7.0116001530841,45.4135588062441));
#171474=CARTESIAN_POINT('Ctrl Pts',(63.1458917128634,7.07789312758018,45.4010554448187));
#171475=CARTESIAN_POINT('Ctrl Pts',(63.2434072577435,7.18026312697839,45.3812113500679));
#171476=CARTESIAN_POINT('Ctrl Pts',(63.2788518431567,7.2169160438872,45.3739957362542));
#171477=CARTESIAN_POINT('Ctrl Pts',(63.3564123569383,7.29592258117983,45.3581976830808));
#171478=CARTESIAN_POINT('Ctrl Pts',(63.398626813907,7.33817229649872,45.3495938420671));
#171479=CARTESIAN_POINT('Ctrl Pts',(63.5174571149938,7.4550211050397,45.3253650037492));
#171480=CARTESIAN_POINT('Ctrl Pts',(63.5948656056335,7.5287678368704,45.3095708072905));
#171481=CARTESIAN_POINT('Ctrl Pts',(63.7785695622404,7.69831509588369,45.2720858636952));
#171482=CARTESIAN_POINT('Ctrl Pts',(63.8857392206877,7.79309526280672,45.2502159904983));
#171483=CARTESIAN_POINT('Ctrl Pts',(64.3223182430656,8.16297009745149,45.1612032877917));
#171484=CARTESIAN_POINT('Ctrl Pts',(64.6667790051496,8.41889901779289,45.0911652196799));
#171485=CARTESIAN_POINT('Ctrl Pts',(65.0571008875175,8.67177745263827,45.0124694009763));
#171486=CARTESIAN_POINT('Ctrl Pts',(65.0880919473385,8.69161382469961,45.0062252464144));
#171487=CARTESIAN_POINT('Ctrl Pts',(65.3784028575049,8.87518222957974,44.947773431553));
#171488=CARTESIAN_POINT('Ctrl Pts',(65.64485274034,9.02697212853524,44.8944340943857));
#171489=CARTESIAN_POINT('Ctrl Pts',(66.0278319447423,9.22234577828469,44.8182809434756));
#171490=CARTESIAN_POINT('Ctrl Pts',(66.1389521851639,9.27645011243593,44.7962426803298));
#171491=CARTESIAN_POINT('Ctrl Pts',(66.3374874012046,9.36858307229529,44.7569697563452));
#171492=CARTESIAN_POINT('Ctrl Pts',(66.4245047088404,9.40745464770424,44.7397905606299));
#171493=CARTESIAN_POINT('Ctrl Pts',(66.6101971756299,9.48722343313728,44.7032013747657));
#171494=CARTESIAN_POINT('Ctrl Pts',(66.7089973473114,9.52779175354907,44.6837752751633));
#171495=CARTESIAN_POINT('Ctrl Pts',(66.9870644186293,9.63676335449365,44.629212788059));
#171496=CARTESIAN_POINT('Ctrl Pts',(67.1676578649076,9.70156431617021,44.5939047391021));
#171497=CARTESIAN_POINT('Ctrl Pts',(67.5914784360616,9.83991033498591,44.5112939379681));
#171498=CARTESIAN_POINT('Ctrl Pts',(67.8358538125961,9.90941510406354,44.4638492042291));
#171499=CARTESIAN_POINT('Ctrl Pts',(68.4110612650839,10.0493690707769,44.3524360082622));
#171500=CARTESIAN_POINT('Ctrl Pts',(68.7433312152032,10.1124040850863,44.288277909562));
#171501=CARTESIAN_POINT('Ctrl Pts',(69.3993086443484,10.2023622571703,44.1614856735944));
#171502=CARTESIAN_POINT('Ctrl Pts',(69.7224336102066,10.2305863885849,44.0989673307257));
#171503=CARTESIAN_POINT('Ctrl Pts',(70.1267142570285,10.2459391287521,44.0202884472602));
#171504=CARTESIAN_POINT('Ctrl Pts',(70.2071940450906,10.2480107407359,44.0046030102669));
#171505=CARTESIAN_POINT('Ctrl Pts',(70.3387607935062,10.2497885692975,43.9789148654675));
#171506=CARTESIAN_POINT('Ctrl Pts',(70.3898397882226,10.2500825110509,43.9689304457918));
#171507=CARTESIAN_POINT('Ctrl Pts',(70.4967202203022,10.2498683828308,43.9480121670586));
#171508=CARTESIAN_POINT('Ctrl Pts',(70.5525190016502,10.2492835853794,43.9370766897919));
#171509=CARTESIAN_POINT('Ctrl Pts',(70.7098017635962,10.2463015868333,43.9062151002667));
#171510=CARTESIAN_POINT('Ctrl Pts',(70.8112534132081,10.2428122278487,43.8862648617424));
#171511=CARTESIAN_POINT('Ctrl Pts',(71.047492832534,10.2310366352245,43.8397276179595));
#171512=CARTESIAN_POINT('Ctrl Pts',(71.1821986972139,10.2215477550215,43.8131299529958));
#171513=CARTESIAN_POINT('Ctrl Pts',(71.6932438072268,10.174994197067,43.7120622472136));
#171514=CARTESIAN_POINT('Ctrl Pts',(72.0675660000018,10.1190765654494,43.6377099036488));
#171515=CARTESIAN_POINT('Ctrl Pts',(72.8616746715027,9.95340129435716,43.4799818104551));
#171516=CARTESIAN_POINT('Ctrl Pts',(73.2794109686977,9.83721198043801,43.3970224981221));
#171517=CARTESIAN_POINT('Ctrl Pts',(73.8336696704474,9.64315796272915,43.2872835621363));
#171518=CARTESIAN_POINT('Ctrl Pts',(73.977630182317,9.58897289097414,43.2588093095473));
#171519=CARTESIAN_POINT('Ctrl Pts',(74.212848065994,9.49415453236284,43.212334985081));
#171520=CARTESIAN_POINT('Ctrl Pts',(74.3048264595144,9.45545997342302,43.1941746489131));
#171521=CARTESIAN_POINT('Ctrl Pts',(74.4864143138544,9.37583517147386,43.158345658732));
#171522=CARTESIAN_POINT('Ctrl Pts',(74.5760291630246,9.33494586695202,43.1406756184265));
#171523=CARTESIAN_POINT('Ctrl Pts',(74.7978734570424,9.22972506855056,43.0969586451437));
#171524=CARTESIAN_POINT('Ctrl Pts',(74.9293405211179,9.16377404830954,43.0710748893434));
#171525=CARTESIAN_POINT('Ctrl Pts',(75.4262731441858,8.90059447464323,42.9732944433866));
#171526=CARTESIAN_POINT('Ctrl Pts',(75.7811128544655,8.68339770983549,42.9036119242478));
#171527=CARTESIAN_POINT('Ctrl Pts',(76.5135561745785,8.16991404432632,42.7593196181868));
#171528=CARTESIAN_POINT('Ctrl Pts',(76.8856618724111,7.8673037180736,42.6857229689564));
#171529=CARTESIAN_POINT('Ctrl Pts',(77.3009799864684,7.47718472773244,42.6021653891796));
#171530=CARTESIAN_POINT('Ctrl Pts',(77.3659816192516,7.41446268098955,42.5890419426571));
#171531=CARTESIAN_POINT('Ctrl Pts',(77.4663433017434,7.3149827254597,42.5686959970545));
#171532=CARTESIAN_POINT('Ctrl Pts',(77.5022742208761,7.27882364475396,42.5613946294845));
#171533=CARTESIAN_POINT('Ctrl Pts',(77.5797175807923,7.19969814631131,42.5456172336984));
#171534=CARTESIAN_POINT('Ctrl Pts',(77.6211270061647,7.1566309804866,42.5371553414755));
#171535=CARTESIAN_POINT('Ctrl Pts',(77.7356404153824,7.03539868506445,42.513687687667));
#171536=CARTESIAN_POINT('Ctrl Pts',(77.8078999535786,6.9564235699023,42.4988013904465));
#171537=CARTESIAN_POINT('Ctrl Pts',(77.9740004579499,6.7690012970359,42.4644204104341));
#171538=CARTESIAN_POINT('Ctrl Pts',(78.0668322931986,6.65966212288598,42.4450786823118));
#171539=CARTESIAN_POINT('Ctrl Pts',(78.429030297644,6.21425882325532,42.3691813599199));
#171540=CARTESIAN_POINT('Ctrl Pts',(78.6794806304577,5.86286921127467,42.315719866957));
#171541=CARTESIAN_POINT('Ctrl Pts',(78.9268291409886,5.46481180979472,42.2622341112299));
#171542=CARTESIAN_POINT('Ctrl Pts',(78.946230835509,5.43320728767722,42.2580334744581));
#171543=CARTESIAN_POINT('Ctrl Pts',(79.1257685198872,5.13715680139019,42.2191139680423));
#171544=CARTESIAN_POINT('Ctrl Pts',(79.2741652723773,4.8654926123219,42.1865905829128));
#171545=CARTESIAN_POINT('Ctrl Pts',(79.4650960376256,4.47510786674353,42.1443007534294));
#171546=CARTESIAN_POINT('Ctrl Pts',(79.5179603256464,4.36184888822867,42.1325345864788));
#171547=CARTESIAN_POINT('Ctrl Pts',(79.6079640825577,4.15951019654728,42.1123986869945));
#171548=CARTESIAN_POINT('Ctrl Pts',(79.6459311887863,4.070831741312,42.1038683651965));
#171549=CARTESIAN_POINT('Ctrl Pts',(79.7238303008384,3.88160671489311,42.0862860561136));
#171550=CARTESIAN_POINT('Ctrl Pts',(79.763439428332,3.78093423302513,42.0772969346177));
#171551=CARTESIAN_POINT('Ctrl Pts',(79.8698095191329,3.49761694886707,42.0530092576846));
#171552=CARTESIAN_POINT('Ctrl Pts',(79.9330335353391,3.31363594446031,42.0383966059595));
#171553=CARTESIAN_POINT('Ctrl Pts',(80.0679302422039,2.88190894499843,42.0067308774697));
#171554=CARTESIAN_POINT('Ctrl Pts',(80.1356343696011,2.63300748796762,41.9904380516688));
#171555=CARTESIAN_POINT('Ctrl Pts',(80.2717539694384,2.04719203069956,41.9564478910252));
#171556=CARTESIAN_POINT('Ctrl Pts',(80.3328788241228,1.70882907080785,41.940099988337));
#171557=CARTESIAN_POINT('Ctrl Pts',(80.4195677198545,1.04080017210136,41.9136886806186));
#171558=CARTESIAN_POINT('Ctrl Pts',(80.4464152069194,0.711728004257093,
41.9034120510381));
#171559=CARTESIAN_POINT('Ctrl Pts',(80.4602703761031,0.299926844175113,
41.8935757132368));
#171560=CARTESIAN_POINT('Ctrl Pts',(80.4620549104904,0.21794597738313,41.8917663727201));
#171561=CARTESIAN_POINT('Ctrl Pts',(80.4633800212526,0.0839173239754168,
41.8890433426507));
#171562=CARTESIAN_POINT('Ctrl Pts',(80.4635022811982,0.031880557681116,
41.8880439701639));
#171563=CARTESIAN_POINT('Ctrl Pts',(80.4629370090956,-0.0770085414591912,
41.8860712680392));
#171564=CARTESIAN_POINT('Ctrl Pts',(80.4621735584137,-0.133858539639717,
41.8851092383684));
#171565=CARTESIAN_POINT('Ctrl Pts',(80.4587018760738,-0.294110881801409,
41.8825929946396));
#171566=CARTESIAN_POINT('Ctrl Pts',(80.4549129781255,-0.397485575460832,
41.8811995041147));
#171567=CARTESIAN_POINT('Ctrl Pts',(80.4424814359409,-0.638217094768553,
41.8785096601645));
#171568=CARTESIAN_POINT('Ctrl Pts',(80.432650123389,-0.775495110739907,
41.8773977992621));
#171569=CARTESIAN_POINT('Ctrl Pts',(80.3849301185938,-1.29632652018824,
41.8748554590984));
#171570=CARTESIAN_POINT('Ctrl Pts',(80.3284341970514,-1.67787306675583,
41.8764679728648));
#171571=CARTESIAN_POINT('Ctrl Pts',(80.1622481194629,-2.48730663912413,
41.8880657533685));
#171572=CARTESIAN_POINT('Ctrl Pts',(80.0462333950024,-2.91310231668167,
41.899221147135));
#171573=CARTESIAN_POINT('Ctrl Pts',(79.8530739754205,-3.47799654955143,
41.9212721918112));
#171574=CARTESIAN_POINT('Ctrl Pts',(79.7991836532735,-3.62471447984029,
41.9276843794151));
#171575=CARTESIAN_POINT('Ctrl Pts',(79.7049509080823,-3.86442905708363,
41.9393010896296));
#171576=CARTESIAN_POINT('Ctrl Pts',(79.6665120939782,-3.95816360141368,
41.9441368259146));
#171577=CARTESIAN_POINT('Ctrl Pts',(79.5874453973038,-4.14321436707407,
41.9542682657217));
#171578=CARTESIAN_POINT('Ctrl Pts',(79.5468577566825,-4.23453613561992,
41.9595564373218));
#171579=CARTESIAN_POINT('Ctrl Pts',(79.4424488798874,-4.46060148907393,
41.973366700595));
#171580=CARTESIAN_POINT('Ctrl Pts',(79.377037637944,-4.59456594006752,41.982197902062));
#171581=CARTESIAN_POINT('Ctrl Pts',(79.116119264361,-5.10092843624674,42.0180470341715));
#171582=CARTESIAN_POINT('Ctrl Pts',(78.9010055203383,-5.46247757647484,
42.0488626867741));
#171583=CARTESIAN_POINT('Ctrl Pts',(78.3927332564295,-6.20884953275891,
42.1233420135616));
#171584=CARTESIAN_POINT('Ctrl Pts',(78.0933548524537,-6.58808203293845,
42.1681461285969));
#171585=CARTESIAN_POINT('Ctrl Pts',(77.7073968319673,-7.01160015308173,
42.225875150338));
#171586=CARTESIAN_POINT('Ctrl Pts',(77.645343471579,-7.07789312757804,42.2351549271454));
#171587=CARTESIAN_POINT('Ctrl Pts',(77.5469217535134,-7.1802631269752,42.2498598583782));
#171588=CARTESIAN_POINT('Ctrl Pts',(77.5111468528833,-7.2169160438839,42.2552021615061));
#171589=CARTESIAN_POINT('Ctrl Pts',(77.4328605580079,-7.29592258117641,
42.2668841055561));
#171590=CARTESIAN_POINT('Ctrl Pts',(77.3902492573673,-7.3381722964953,42.273237334268));
#171591=CARTESIAN_POINT('Ctrl Pts',(77.2702985495597,-7.45502110503297,
42.2911120302992));
#171592=CARTESIAN_POINT('Ctrl Pts',(77.1921564287853,-7.52876783686154,
42.3027456034984));
#171593=CARTESIAN_POINT('Ctrl Pts',(77.0067105705779,-7.69831509586957,
42.3303517321786));
#171594=CARTESIAN_POINT('Ctrl Pts',(76.8985240962022,-7.79309526278899,
42.3464549556596));
#171595=CARTESIAN_POINT('Ctrl Pts',(76.4578298731816,-8.16297009740647,
42.4121291955713));
#171596=CARTESIAN_POINT('Ctrl Pts',(76.110188206841,-8.41889901772776,42.4641274590054));
#171597=CARTESIAN_POINT('Ctrl Pts',(75.7164900589895,-8.67177745262435,
42.5236755250436));
#171598=CARTESIAN_POINT('Ctrl Pts',(75.6852323620228,-8.69161382475175,
42.5284075058163));
#171599=CARTESIAN_POINT('Ctrl Pts',(75.3924376438511,-8.87518222965952,
42.5727729458325));
#171600=CARTESIAN_POINT('Ctrl Pts',(75.1238135274487,-9.02697212858223,
42.6137815914077));
#171601=CARTESIAN_POINT('Ctrl Pts',(74.7378848836248,-9.2223457783011,42.6732076398196));
#171602=CARTESIAN_POINT('Ctrl Pts',(74.6259284837652,-9.2764501124498,42.6905038071214));
#171603=CARTESIAN_POINT('Ctrl Pts',(74.4259342752012,-9.36858307230592,
42.7215023733009));
#171604=CARTESIAN_POINT('Ctrl Pts',(74.3382891223546,-9.40745464771453,
42.7351208818856));
#171605=CARTESIAN_POINT('Ctrl Pts',(74.1512810429809,-9.48722343314812,
42.7642488580347));
#171606=CARTESIAN_POINT('Ctrl Pts',(74.0517951333466,-9.5277917535606,42.7797859444671));
#171607=CARTESIAN_POINT('Ctrl Pts',(73.7718360886688,-9.63676335451079,
42.8236185175525));
#171608=CARTESIAN_POINT('Ctrl Pts',(73.5900576958591,-9.70156431619152,
42.8522064008754));
#171609=CARTESIAN_POINT('Ctrl Pts',(73.1635420745201,-9.83991033501786,
42.9195328131501));
#171610=CARTESIAN_POINT('Ctrl Pts',(72.9176772818257,-9.90941510410055,
42.9585306482728));
#171611=CARTESIAN_POINT('Ctrl Pts',(72.3390535260209,-10.0493690708103,
43.0505690255109));
#171612=CARTESIAN_POINT('Ctrl Pts',(72.0048785436739,-10.1124040851137,
43.103923149561));
#171613=CARTESIAN_POINT('Ctrl Pts',(71.3450958954378,-10.2023622571799,
43.2091349153755));
#171614=CARTESIAN_POINT('Ctrl Pts',(71.0200752168912,-10.2305863885873,
43.2609021370449));
#171615=CARTESIAN_POINT('Ctrl Pts',(70.6132659133987,-10.2459391287523,
43.3252402956022));
#171616=CARTESIAN_POINT('Ctrl Pts',(70.5322749150267,-10.248010740736,43.3380265148535));
#171617=CARTESIAN_POINT('Ctrl Pts',(70.3998567494346,-10.2497885692975,
43.3588860328936));
#171618=CARTESIAN_POINT('Ctrl Pts',(70.3484433223744,-10.2500825110509,
43.3669737924953));
#171619=CARTESIAN_POINT('Ctrl Pts',(70.240854096352,-10.2498683828307,43.3838723010288));
#171620=CARTESIAN_POINT('Ctrl Pts',(70.1846802397678,-10.2492835853794,
43.3926806209306));
#171621=CARTESIAN_POINT('Ctrl Pts',(70.0263275037152,-10.2463015868331,
43.4174740857719));
#171622=CARTESIAN_POINT('Ctrl Pts',(69.9241707537666,-10.2428122278484,
43.4334255015889));
#171623=CARTESIAN_POINT('Ctrl Pts',(69.6862616398917,-10.2310366352235,
43.4704934370725));
#171624=CARTESIAN_POINT('Ctrl Pts',(69.5505825956879,-10.2215477550199,
43.4915719267213));
#171625=CARTESIAN_POINT('Ctrl Pts',(69.0357900856737,-10.1749941970615,
43.571387071175));
#171626=CARTESIAN_POINT('Ctrl Pts',(68.6586122840996,-10.1190765654379,
43.6295444526155));
#171627=CARTESIAN_POINT('Ctrl Pts',(67.858448040357,-9.95340129433929,43.7529296889922));
#171628=CARTESIAN_POINT('Ctrl Pts',(67.4375305685867,-9.83721198042683,
43.8178476636013));
#171629=CARTESIAN_POINT('Ctrl Pts',(66.8791648299632,-9.64315796272882,
43.9042944358496));
#171630=CARTESIAN_POINT('Ctrl Pts',(66.7341474313231,-9.58897289097375,
43.9267747857123));
#171631=CARTESIAN_POINT('Ctrl Pts',(66.4972197666391,-9.49415453236207,
43.9635524602433));
#171632=CARTESIAN_POINT('Ctrl Pts',(66.4045771481974,-9.45545997342227,
43.9779457896901));
#171633=CARTESIAN_POINT('Ctrl Pts',(66.221686145093,-9.37583517147317,44.0063842559742));
#171634=CARTESIAN_POINT('Ctrl Pts',(66.131432222897,-9.33494586695127,44.0204299330474));
#171635=CARTESIAN_POINT('Ctrl Pts',(65.9080146913774,-9.22972506854991,
44.0552246330863));
#171636=CARTESIAN_POINT('Ctrl Pts',(65.775623295521,-9.16377404830908,44.0758662428602));
#171637=CARTESIAN_POINT('Ctrl Pts',(65.2752164944573,-8.90059447464353,
44.1539436463021));
#171638=CARTESIAN_POINT('Ctrl Pts',(64.9179434119637,-8.68339770983664,
44.2098258258369));
#171639=CARTESIAN_POINT('Ctrl Pts',(64.1803209537105,-8.16991404432835,
44.324745779918));
#171640=CARTESIAN_POINT('Ctrl Pts',(63.8054844387862,-7.86730371807531,
44.3828551958267));
#171641=CARTESIAN_POINT('Ctrl Pts',(63.3866346963149,-7.47718472773274,
44.4463839155955));
#171642=CARTESIAN_POINT('Ctrl Pts',(63.3210646585895,-7.4144626809903,44.4562837774999));
#171643=CARTESIAN_POINT('Ctrl Pts',(63.2197968029131,-7.3149827254624,44.4714905595842));
#171644=CARTESIAN_POINT('Ctrl Pts',(63.1835355685625,-7.27882364475602,
44.4769186164687));
#171645=CARTESIAN_POINT('Ctrl Pts',(63.1053664275514,-7.19969814631249,
44.4885799031316));
#171646=CARTESIAN_POINT('Ctrl Pts',(63.0635601585069,-7.15663098048755,
44.4947911830527));
#171647=CARTESIAN_POINT('Ctrl Pts',(62.9479263425654,-7.03539868506595,
44.5119046945751));
#171648=CARTESIAN_POINT('Ctrl Pts',(62.8749331742322,-6.95642356990395,
44.5226303685366));
#171649=CARTESIAN_POINT('Ctrl Pts',(62.7070907682543,-6.7690012970378,44.547132533635));
#171650=CARTESIAN_POINT('Ctrl Pts',(62.6132421170728,-6.65966212288828,
44.5607076120422));
#171651=CARTESIAN_POINT('Ctrl Pts',(62.2469289119509,-6.21425882325954,
44.6132664716456));
#171652=CARTESIAN_POINT('Ctrl Pts',(61.9932976748477,-5.86286921128045,
44.6486881599369));
#171653=CARTESIAN_POINT('Ctrl Pts',(61.7425728988971,-5.46481180979694,
44.6830261629865));
#171654=CARTESIAN_POINT('Ctrl Pts',(61.722904567331,-5.43320728767347,44.6857146259506));
#171655=CARTESIAN_POINT('Ctrl Pts',(61.5408830750034,-5.13715680138255,
44.7105477575107));
#171656=CARTESIAN_POINT('Ctrl Pts',(61.3903120888982,-4.86549261231695,
44.7307404510571));
#171657=CARTESIAN_POINT('Ctrl Pts',(61.1964318841738,-4.47510786674152,
44.7563031780524));
#171658=CARTESIAN_POINT('Ctrl Pts',(61.1427314367107,-4.36184888822653,
44.7633272491598));
#171659=CARTESIAN_POINT('Ctrl Pts',(61.0512686872711,-4.15951019654608,
44.77518879084));
#171660=CARTESIAN_POINT('Ctrl Pts',(61.0126737358313,-4.0708317413104,44.7801584255075));
#171661=CARTESIAN_POINT('Ctrl Pts',(60.9334590111974,-3.88160671489095,
44.7902795248749));
#171662=CARTESIAN_POINT('Ctrl Pts',(60.8931641457534,-3.78093423302279,
44.7953796332002));
#171663=CARTESIAN_POINT('Ctrl Pts',(60.7849020816094,-3.49761694886339,
44.8089373961114));
#171664=CARTESIAN_POINT('Ctrl Pts',(60.7204931188863,-3.31363594445542,
44.8168298821998));
#171665=CARTESIAN_POINT('Ctrl Pts',(60.58290136188,-2.88190894499112,44.8332112218223));
#171666=CARTESIAN_POINT('Ctrl Pts',(60.513707818352,-2.63300748795805,44.8410571490016));
#171667=CARTESIAN_POINT('Ctrl Pts',(60.3283602700609,-1.85486038514426,
44.8604709180007));
#171668=CARTESIAN_POINT('Ctrl Pts',(60.2442547230065,-1.3188352359329,44.8666826188784));
#171669=CARTESIAN_POINT('Ctrl Pts',(60.1898644273114,-0.621316886541912,
44.864268571302));
#171670=CARTESIAN_POINT('Ctrl Pts',(60.1811636672246,-0.463675701607057,
44.8630346952966));
#171671=CARTESIAN_POINT('Ctrl Pts',(60.1741655665948,-0.248381985595741,
44.8603650018948));
#171672=CARTESIAN_POINT('Ctrl Pts',(60.1727707935746,-0.190844644938373,
44.8595556628521));
#171673=CARTESIAN_POINT('Ctrl Pts',(60.1711405545296,-0.088864956530352,
44.8579482502389));
#171674=CARTESIAN_POINT('Ctrl Pts',(60.1707134643357,-0.0444365562647033,
44.8571898040892));
#171675=CARTESIAN_POINT('Ctrl Pts',(60.1705693073443,2.15049072447686E-6,
44.8563721954731));
#171676=CARTESIAN_POINT('Ctrl Pts',(60.1543689253998,-1.15483570402281E-9,
44.7644952638818));
#171677=CARTESIAN_POINT('Ctrl Pts',(60.1544335380298,-0.0199166192528812,
44.7648617003024));
#171678=CARTESIAN_POINT('Ctrl Pts',(60.1545556301466,-0.0398332865460885,
44.765219826651));
#171679=CARTESIAN_POINT('Ctrl Pts',(60.1553035651452,-0.122792370642498,
44.7666766472281));
#171680=CARTESIAN_POINT('Ctrl Pts',(60.1564477107353,-0.185829839162329,
44.767699708579));
#171681=CARTESIAN_POINT('Ctrl Pts',(60.1619033127762,-0.385803791935395,
44.7706725481338));
#171682=CARTESIAN_POINT('Ctrl Pts',(60.1683551897962,-0.522671862930262,
44.7723013594263));
#171683=CARTESIAN_POINT('Ctrl Pts',(60.2108588050916,-1.15698867587593,
44.7778759236443));
#171684=CARTESIAN_POINT('Ctrl Pts',(60.2800257466418,-1.65159608120817,
44.7765486489021));
#171685=CARTESIAN_POINT('Ctrl Pts',(60.4606916331271,-2.49619847305522,
44.7631669203097));
#171686=CARTESIAN_POINT('Ctrl Pts',(60.5557456738136,-2.84881779514516,
44.7540996937084));
#171687=CARTESIAN_POINT('Ctrl Pts',(60.7253863733359,-3.36792906345627,
44.7352808831733));
#171688=CARTESIAN_POINT('Ctrl Pts',(60.7861804439288,-3.53871633551991,
44.7281741386553));
#171689=CARTESIAN_POINT('Ctrl Pts',(60.8895195636392,-3.80664699843975,
44.7155559443905));
#171690=CARTESIAN_POINT('Ctrl Pts',(60.9291505531237,-3.90489943795874,
44.7106087880791));
#171691=CARTESIAN_POINT('Ctrl Pts',(61.0080817819441,-4.09227342619886,
44.7005575550456));
#171692=CARTESIAN_POINT('Ctrl Pts',(61.0471477319428,-4.18148362684842,
44.695498703219));
#171693=CARTESIAN_POINT('Ctrl Pts',(61.1425166787578,-4.3911861099131,44.6829592667386));
#171694=CARTESIAN_POINT('Ctrl Pts',(61.1998873183109,-4.51116079544422,
44.6752709696757));
#171695=CARTESIAN_POINT('Ctrl Pts',(61.4522052578221,-5.01373677828991,
44.640891948042));
#171696=CARTESIAN_POINT('Ctrl Pts',(61.6684024320991,-5.3848894393157,44.6100734139114));
#171697=CARTESIAN_POINT('Ctrl Pts',(62.1063892874136,-6.03926454968155,
44.5460656424816));
#171698=CARTESIAN_POINT('Ctrl Pts',(62.3211695503718,-6.32647943306077,
44.5141402096601));
#171699=CARTESIAN_POINT('Ctrl Pts',(62.635049775427,-6.70328554143873,44.4672598906789));
#171700=CARTESIAN_POINT('Ctrl Pts',(62.7216254629264,-6.80321365569073,
44.4543092542136));
#171701=CARTESIAN_POINT('Ctrl Pts',(62.8778004195768,-6.97655883481724,
44.4309484982464));
#171702=CARTESIAN_POINT('Ctrl Pts',(62.946605206381,-7.05068289042323,44.4206570104763));
#171703=CARTESIAN_POINT('Ctrl Pts',(63.057100811273,-7.16622502557467,44.4041452694206));
#171704=CARTESIAN_POINT('Ctrl Pts',(63.0980739954297,-7.20833445731159,
44.3980258062601));
#171705=CARTESIAN_POINT('Ctrl Pts',(63.1760015825637,-7.28704883316404,
44.3863968985025));
#171706=CARTESIAN_POINT('Ctrl Pts',(63.2128773424897,-7.32373044764001,
44.3808980271677));
#171707=CARTESIAN_POINT('Ctrl Pts',(63.3182970546813,-7.42700060747211,
44.365185922196));
#171708=CARTESIAN_POINT('Ctrl Pts',(63.3874928474175,-7.49290220592788,
44.3548821316821));
#171709=CARTESIAN_POINT('Ctrl Pts',(63.8336274340093,-7.90598092875223,
44.2884643332931));
#171710=CARTESIAN_POINT('Ctrl Pts',(64.2351126276922,-8.22498923683794,
44.228726166918));
#171711=CARTESIAN_POINT('Ctrl Pts',(64.9788572543902,-8.72938955394705,
44.1166671640505));
#171712=CARTESIAN_POINT('Ctrl Pts',(65.3111565060333,-8.92799775556546,
44.0661759639856));
#171713=CARTESIAN_POINT('Ctrl Pts',(65.7813052853928,-9.17361945482924,
43.9939483178637));
#171714=CARTESIAN_POINT('Ctrl Pts',(65.9102404697575,-9.23751280379088,
43.9740646488257));
#171715=CARTESIAN_POINT('Ctrl Pts',(66.1295558638234,-9.34041736638353,
43.9401132340323));
#171716=CARTESIAN_POINT('Ctrl Pts',(66.2192395628354,-9.38090806588518,
43.926193975315));
#171717=CARTESIAN_POINT('Ctrl Pts',(66.4024019950372,-9.46039777279593,
43.8976951514502));
#171718=CARTESIAN_POINT('Ctrl Pts',(66.4959048809363,-9.4993129734784,43.8831097263679));
#171719=CARTESIAN_POINT('Ctrl Pts',(66.738235768412,-9.59590946159948,43.8452170096186));
#171720=CARTESIAN_POINT('Ctrl Pts',(66.8878527562691,-9.65146434570958,
43.8217335110625));
#171721=CARTESIAN_POINT('Ctrl Pts',(67.2228099917319,-9.76684812705613,
43.7689854471539));
#171722=CARTESIAN_POINT('Ctrl Pts',(67.40867777952,-9.82489103648375,43.7395994111689));
#171723=CARTESIAN_POINT('Ctrl Pts',(68.0691778471187,-10.0102543626263,
43.6348639168474));
#171724=CARTESIAN_POINT('Ctrl Pts',(68.5510961498953,-10.1080158997696,
43.5578620979039));
#171725=CARTESIAN_POINT('Ctrl Pts',(69.3333075600327,-10.2075532106292,
43.4331625120587));
#171726=CARTESIAN_POINT('Ctrl Pts',(69.629973381005,-10.2319216640304,43.3859415000183));
#171727=CARTESIAN_POINT('Ctrl Pts',(70.0076417257142,-10.2460289865898,
43.3262154485403));
#171728=CARTESIAN_POINT('Ctrl Pts',(70.0880040421732,-10.2480611409662,
43.3135291019613));
#171729=CARTESIAN_POINT('Ctrl Pts',(70.2196813255477,-10.2498031702913,
43.2927870270688));
#171730=CARTESIAN_POINT('Ctrl Pts',(70.2709829635795,-10.2500872636329,
43.284717136905));
#171731=CARTESIAN_POINT('Ctrl Pts',(70.3786740949611,-10.249855408428,43.2678031644929));
#171732=CARTESIAN_POINT('Ctrl Pts',(70.4350616130504,-10.2492574044026,
43.258961666125));
#171733=CARTESIAN_POINT('Ctrl Pts',(70.5946988596947,-10.2462150053732,
43.2339680875963));
#171734=CARTESIAN_POINT('Ctrl Pts',(70.6979255942784,-10.2426490761611,
43.2178506375705));
#171735=CARTESIAN_POINT('Ctrl Pts',(70.9388687218488,-10.2305910133748,
43.1803129051586));
#171736=CARTESIAN_POINT('Ctrl Pts',(71.0765081765009,-10.2208484336994,
43.158932150096));
#171737=CARTESIAN_POINT('Ctrl Pts',(71.6046269993583,-10.1724837301423,
43.0770600611678));
#171738=CARTESIAN_POINT('Ctrl Pts',(71.9930125237041,-10.113772390402,43.0171864013352));
#171739=CARTESIAN_POINT('Ctrl Pts',(72.8272572909885,-9.93706629584623,
42.8885466787075));
#171740=CARTESIAN_POINT('Ctrl Pts',(73.2705258626672,-9.81080340615027,
42.8201634146415));
#171741=CARTESIAN_POINT('Ctrl Pts',(73.8321843902975,-9.60817022279217,
42.7331506611185));
#171742=CARTESIAN_POINT('Ctrl Pts',(73.9596903722518,-9.55921025997451,
42.7133744091333));
#171743=CARTESIAN_POINT('Ctrl Pts',(74.1753462646005,-9.47132024709691,
42.6798864231748));
#171744=CARTESIAN_POINT('Ctrl Pts',(74.2639976999074,-9.43369728463362,
42.6661086584929));
#171745=CARTESIAN_POINT('Ctrl Pts',(74.4462863326864,-9.35322791833252,
42.6377558402625));
#171746=CARTESIAN_POINT('Ctrl Pts',(74.5398352423263,-9.31020493537004,
42.6231929538129));
#171747=CARTESIAN_POINT('Ctrl Pts',(74.7855769951801,-9.19258952491959,
42.5849098230035));
#171748=CARTESIAN_POINT('Ctrl Pts',(74.9365956910636,-9.11556821643338,
42.5613538173131));
#171749=CARTESIAN_POINT('Ctrl Pts',(75.186782754201,-8.97991513765112,42.5223029891664));
#171750=CARTESIAN_POINT('Ctrl Pts',(75.2869998209127,-8.92333752135874,
42.50665324063));
#171751=CARTESIAN_POINT('Ctrl Pts',(75.7131453799762,-8.6730549016473,42.4401020361524));
#171752=CARTESIAN_POINT('Ctrl Pts',(76.0291662229347,-8.46269522764463,
42.3907249940435));
#171753=CARTESIAN_POINT('Ctrl Pts',(76.6112096133001,-8.02625244617443,
42.3003501661901));
#171754=CARTESIAN_POINT('Ctrl Pts',(76.8788179653258,-7.80324216687985,
42.25906021943));
#171755=CARTESIAN_POINT('Ctrl Pts',(77.206602026039,-7.50038007347266,42.2092774195641));
#171756=CARTESIAN_POINT('Ctrl Pts',(77.2775531196989,-7.43290933024477,
42.1985531037319));
#171757=CARTESIAN_POINT('Ctrl Pts',(77.3890782390824,-7.32376650238012,
42.1817929999155));
#171758=CARTESIAN_POINT('Ctrl Pts',(77.4302738884402,-7.28275881709131,
42.1756238312646));
#171759=CARTESIAN_POINT('Ctrl Pts',(77.5134159955473,-7.19857660824525,
42.1632214523772));
#171760=CARTESIAN_POINT('Ctrl Pts',(77.5553358622813,-7.15537847828065,
42.1569937530078));
#171761=CARTESIAN_POINT('Ctrl Pts',(77.671675823996,-7.03336027321952,42.1397771701164));
#171762=CARTESIAN_POINT('Ctrl Pts',(77.7452435670081,-6.95371309507588,
42.1289685943587));
#171763=CARTESIAN_POINT('Ctrl Pts',(77.914706706801,-6.76431168256126,42.1042345012843));
#171764=CARTESIAN_POINT('Ctrl Pts',(78.009569098743,-6.6536373863326,42.0905167864875));
#171765=CARTESIAN_POINT('Ctrl Pts',(78.3841168538635,-6.19735516804941,
42.0367963263584));
#171766=CARTESIAN_POINT('Ctrl Pts',(78.6438141651905,-5.83552764715924,
42.000568059813));
#171767=CARTESIAN_POINT('Ctrl Pts',(79.0530090012289,-5.17947451038125,
41.9446143542519));
#171768=CARTESIAN_POINT('Ctrl Pts',(79.2132833316153,-4.89290933682466,
41.9230923896796));
#171769=CARTESIAN_POINT('Ctrl Pts',(79.4163045905892,-4.48541768054737,
41.8963101480454));
#171770=CARTESIAN_POINT('Ctrl Pts',(79.4708356116372,-4.37071142343845,
41.8891741498132));
#171771=CARTESIAN_POINT('Ctrl Pts',(79.5632254819026,-4.16674846523351,
41.8771877520599));
#171772=CARTESIAN_POINT('Ctrl Pts',(79.6019667746226,-4.07791736080481,
41.8721972843117));
#171773=CARTESIAN_POINT('Ctrl Pts',(79.6810616419954,-3.88936357596394,
41.8620872847738));
#171774=CARTESIAN_POINT('Ctrl Pts',(79.7211204682305,-3.7895274661613,41.8570143291583));
#171775=CARTESIAN_POINT('Ctrl Pts',(79.8276449335569,-3.51157212168754,
41.8436649582457));
#171776=CARTESIAN_POINT('Ctrl Pts',(79.8907772006661,-3.33219725453737,
41.8359179284451));
#171777=CARTESIAN_POINT('Ctrl Pts',(80.1991808156335,-2.37232788355457,
41.7991032088621));
#171778=CARTESIAN_POINT('Ctrl Pts',(80.356369193319,-1.56619826433015,41.7839983275279));
#171779=CARTESIAN_POINT('Ctrl Pts',(80.4292834038212,-0.596598155405868,
41.7878709014643));
#171780=CARTESIAN_POINT('Ctrl Pts',(80.4374262264858,-0.442995382190262,
41.7891395160404));
#171781=CARTESIAN_POINT('Ctrl Pts',(80.4442617473451,-0.221867699396258,
41.7919526294067));
#171782=CARTESIAN_POINT('Ctrl Pts',(80.445693233636,-0.15444170199019,41.7929422484627));
#171783=CARTESIAN_POINT('Ctrl Pts',(80.4470597942346,-0.0362263074402389,
41.7949133209436));
#171784=CARTESIAN_POINT('Ctrl Pts',(80.447277108525,0.0145575883017807,
41.7958366534171));
#171785=CARTESIAN_POINT('Ctrl Pts',(80.44693244556,0.129435886879059,41.7980992895404));
#171786=CARTESIAN_POINT('Ctrl Pts',(80.446151160613,0.19352556587406,41.7994835927479));
#171787=CARTESIAN_POINT('Ctrl Pts',(80.441715190715,0.400920069772679,41.8043513192942));
#171788=CARTESIAN_POINT('Ctrl Pts',(80.4357023297616,0.544146405024124,
41.8083128592234));
#171789=CARTESIAN_POINT('Ctrl Pts',(80.4129703810276,0.907042064359414,
41.8198170930238));
#171790=CARTESIAN_POINT('Ctrl Pts',(80.3922414766065,1.12636372738025,41.828136807102));
#171791=CARTESIAN_POINT('Ctrl Pts',(80.281410250048,2.00147495859493,41.8665419581647));
#171792=CARTESIAN_POINT('Ctrl Pts',(80.1357966959054,2.64819629436514,41.9066161249942));
#171793=CARTESIAN_POINT('Ctrl Pts',(79.8778890351759,3.43325423914305,41.9688167868748));
#171794=CARTESIAN_POINT('Ctrl Pts',(79.8224190979191,3.58931492827038,41.9818904577881));
#171795=CARTESIAN_POINT('Ctrl Pts',(79.7264514199753,3.8399877714725,42.0040459577929));
#171796=CARTESIAN_POINT('Ctrl Pts',(79.6882438704159,3.93547592931995,42.0127635132903));
#171797=CARTESIAN_POINT('Ctrl Pts',(79.6106865597225,4.12118350218499,42.0302662368209));
#171798=CARTESIAN_POINT('Ctrl Pts',(79.571459500868,4.21144386550842,42.0390316734453));
#171799=CARTESIAN_POINT('Ctrl Pts',(79.4728282003867,4.42975916261849,42.0608696029861));
#171800=CARTESIAN_POINT('Ctrl Pts',(79.4120769241394,4.55716142752468,42.0741553278741));
#171801=CARTESIAN_POINT('Ctrl Pts',(79.1414639165277,5.09578921273117,42.132690549279));
#171802=CARTESIAN_POINT('Ctrl Pts',(78.9067731816421,5.49348743263157,42.1818781498277));
#171803=CARTESIAN_POINT('Ctrl Pts',(78.3914111492602,6.24571825266891,42.2880802973488));
#171804=CARTESIAN_POINT('Ctrl Pts',(78.1123826943308,6.60014221682026,42.3447970372081));
#171805=CARTESIAN_POINT('Ctrl Pts',(77.749182457666,7.00343540193265,42.4186447482027));
#171806=CARTESIAN_POINT('Ctrl Pts',(77.6861947713095,7.07148195498237,42.4314532254602));
#171807=CARTESIAN_POINT('Ctrl Pts',(77.5868937593087,7.17585961097028,42.4516600036497));
#171808=CARTESIAN_POINT('Ctrl Pts',(77.5512072335956,7.21280575164807,42.458924599158));
#171809=CARTESIAN_POINT('Ctrl Pts',(77.4738726114266,7.29166523002439,42.4746760507925));
#171810=CARTESIAN_POINT('Ctrl Pts',(77.4321377248062,7.33348695929728,42.4831818331765));
#171811=CARTESIAN_POINT('Ctrl Pts',(77.3161658017376,7.44768876893271,42.5068270905542));
#171812=CARTESIAN_POINT('Ctrl Pts',(77.2411969166165,7.51928299708685,42.5221229295825));
#171813=CARTESIAN_POINT('Ctrl Pts',(77.0646167606054,7.68280642087837,42.5581539268041));
#171814=CARTESIAN_POINT('Ctrl Pts',(76.9622280836394,7.77383121131077,42.5790487425704));
#171815=CARTESIAN_POINT('Ctrl Pts',(76.5620669725293,8.11525953956883,42.6606474011505));
#171816=CARTESIAN_POINT('Ctrl Pts',(76.2520344130197,8.35020244765254,42.7237241647739));
#171817=CARTESIAN_POINT('Ctrl Pts',(75.6125317189732,8.7787379928646,42.8528974961526));
#171818=CARTESIAN_POINT('Ctrl Pts',(75.284008834267,8.97264397171745,42.9188173197737));
#171819=CARTESIAN_POINT('Ctrl Pts',(74.8294841094273,9.20691745409177,43.0092499321159));
#171820=CARTESIAN_POINT('Ctrl Pts',(74.712406871467,9.2643803176519,43.0324799664187));
#171821=CARTESIAN_POINT('Ctrl Pts',(74.5073672723046,9.36006333071543,43.0730514916028));
#171822=CARTESIAN_POINT('Ctrl Pts',(74.4199072395709,9.3993474965955,43.0903229149195));
#171823=CARTESIAN_POINT('Ctrl Pts',(74.235829748319,9.47885030221642,43.1266033819154));
#171824=CARTESIAN_POINT('Ctrl Pts',(74.1391195066904,9.5188192075385,43.1456242467234));
#171825=CARTESIAN_POINT('Ctrl Pts',(73.8743575531548,9.62337594965442,43.1975930507576));
#171826=CARTESIAN_POINT('Ctrl Pts',(73.705177513008,9.68492391296871,43.2306872600623));
#171827=CARTESIAN_POINT('Ctrl Pts',(73.2111234426127,9.84958967443477,43.3270501243312));
#171828=CARTESIAN_POINT('Ctrl Pts',(72.8825749904206,9.94058132118908,43.3907794376997));
#171829=CARTESIAN_POINT('Ctrl Pts',(71.9934711344537,10.138121872299,43.5628122627297));
#171830=CARTESIAN_POINT('Ctrl Pts',(71.4274635072994,10.2134351550852,43.6718527906004));
#171831=CARTESIAN_POINT('Ctrl Pts',(70.7642427952375,10.2439126278387,43.8008064812598));
#171832=CARTESIAN_POINT('Ctrl Pts',(70.6700033746303,10.2468924228968,43.8191591167497));
#171833=CARTESIAN_POINT('Ctrl Pts',(70.5214125154391,10.2494625531567,43.8481553665839));
#171834=CARTESIAN_POINT('Ctrl Pts',(70.46707699971,10.2499539351324,43.8587709118182));
#171835=CARTESIAN_POINT('Ctrl Pts',(70.3600499035572,10.2500385885598,43.8797085143961));
#171836=CARTESIAN_POINT('Ctrl Pts',(70.3073600924855,10.2496585372523,43.8900295141274));
#171837=CARTESIAN_POINT('Ctrl Pts',(70.1684414773438,10.2475444433968,43.9172730483735));
#171838=CARTESIAN_POINT('Ctrl Pts',(70.0822310083332,10.2451022628853,43.934212238722));
#171839=CARTESIAN_POINT('Ctrl Pts',(69.5892208234616,10.2246678286397,44.031235834295));
#171840=CARTESIAN_POINT('Ctrl Pts',(69.1838579249568,10.1826483000773,44.111596314172));
#171841=CARTESIAN_POINT('Ctrl Pts',(68.2126659171701,10.0208103096813,44.30439220126));
#171842=CARTESIAN_POINT('Ctrl Pts',(67.6522807306225,9.87612814579876,44.415812418359));
#171843=CARTESIAN_POINT('Ctrl Pts',(66.967048277767,9.63371740256559,44.5514642782997));
#171844=CARTESIAN_POINT('Ctrl Pts',(66.8281030064351,9.58102982810751,44.5789434180771));
#171845=CARTESIAN_POINT('Ctrl Pts',(66.5987556340911,9.48813281509504,44.624254362307));
#171846=CARTESIAN_POINT('Ctrl Pts',(66.5077033647201,9.44966427277173,44.6422305836622));
#171847=CARTESIAN_POINT('Ctrl Pts',(66.3262623846365,9.36980452747353,44.678028393732));
#171848=CARTESIAN_POINT('Ctrl Pts',(66.2358896088186,9.32840357396158,44.6958467144927));
#171849=CARTESIAN_POINT('Ctrl Pts',(66.0087730412191,9.22022208857846,44.7405997219895));
#171850=CARTESIAN_POINT('Ctrl Pts',(65.8728808341264,9.15163883679588,44.7673523152967));
#171851=CARTESIAN_POINT('Ctrl Pts',(65.5749640871962,8.99264085785811,44.8259679838072));
#171852=CARTESIAN_POINT('Ctrl Pts',(65.413755523149,8.90075613378588,44.857662750292));
#171853=CARTESIAN_POINT('Ctrl Pts',(64.8510116982668,8.55894524525192,44.9683121631765));
#171854=CARTESIAN_POINT('Ctrl Pts',(64.4643023879459,8.28490780011079,45.0443422507495));
#171855=CARTESIAN_POINT('Ctrl Pts',(63.9069027295949,7.82753809667824,45.1549880735582));
#171856=CARTESIAN_POINT('Ctrl Pts',(63.7215775920452,7.66370094881584,45.1919813961789));
#171857=CARTESIAN_POINT('Ctrl Pts',(63.4847302524726,7.43825287285645,45.2397158903179));
#171858=CARTESIAN_POINT('Ctrl Pts',(63.4277276403445,7.38269324179563,45.2512413843217));
#171859=CARTESIAN_POINT('Ctrl Pts',(63.3324928269611,7.28764519533255,45.270568735491));
#171860=CARTESIAN_POINT('Ctrl Pts',(63.293919648172,7.24851364405408,45.2784175710745));
#171861=CARTESIAN_POINT('Ctrl Pts',(63.2091527102532,7.16110306387053,45.2957138604662));
#171862=CARTESIAN_POINT('Ctrl Pts',(63.1631131201746,7.11267495385704,45.305139627345));
#171863=CARTESIAN_POINT('Ctrl Pts',(63.0175902577066,6.95653002081841,45.3350268681521));
#171864=CARTESIAN_POINT('Ctrl Pts',(62.9199433224521,6.84707698346953,45.3552245466701));
#171865=CARTESIAN_POINT('Ctrl Pts',(62.6760478551066,6.56144424658541,45.4059852125525));
#171866=CARTESIAN_POINT('Ctrl Pts',(62.5332773196419,6.38230638959384,45.4360027255352));
#171867=CARTESIAN_POINT('Ctrl Pts',(62.0350798095629,5.71198144882276,45.5416088721145));
#171868=CARTESIAN_POINT('Ctrl Pts',(61.717113197429,5.19351337138165,45.6106580551813));
#171869=CARTESIAN_POINT('Ctrl Pts',(61.3859971935355,4.52782309721815,45.683872127209));
#171870=CARTESIAN_POINT('Ctrl Pts',(61.3280118748508,4.40524110317338,45.6967601643282));
#171871=CARTESIAN_POINT('Ctrl Pts',(61.2324813075535,4.19254000294612,45.7181100338742));
#171872=CARTESIAN_POINT('Ctrl Pts',(61.1937748110581,4.10298566251397,45.726797188772));
#171873=CARTESIAN_POINT('Ctrl Pts',(61.1162215581349,3.91633815426279,45.7442822848895));
#171874=CARTESIAN_POINT('Ctrl Pts',(61.0775665003081,3.81917415623401,45.7530428458193));
#171875=CARTESIAN_POINT('Ctrl Pts',(60.9782459576933,3.55806321443092,45.7756819122062));
#171876=CARTESIAN_POINT('Ctrl Pts',(60.9202342389636,3.39310032082398,45.789045543741));
#171877=CARTESIAN_POINT('Ctrl Pts',(60.7347617478341,2.81970978904979,45.8323332666847));
#171878=CARTESIAN_POINT('Ctrl Pts',(60.6283272193907,2.40465593321471,45.8582081005878));
#171879=CARTESIAN_POINT('Ctrl Pts',(60.4505135006237,1.47581028769749,45.9050809027698));
#171880=CARTESIAN_POINT('Ctrl Pts',(60.3912855530988,0.96078511143066,45.9238727462837));
#171881=CARTESIAN_POINT('Ctrl Pts',(60.3671377522047,0.3507955582706,45.9389994618556));
#171882=CARTESIAN_POINT('Ctrl Pts',(60.3647148433716,0.258213846078,45.9411038164074));
#171883=CARTESIAN_POINT('Ctrl Pts',(60.3628372297609,0.110963761724782,
45.9441578451942));
#171884=CARTESIAN_POINT('Ctrl Pts',(60.3625729586119,0.0563133755297087,
45.9452271959814));
#171885=CARTESIAN_POINT('Ctrl Pts',(60.3627431879399,0.00110819107845439,
45.9462441719599));
#171886=CARTESIAN_POINT('Ctrl Pts',(60.3627449410238,0.000554095481200964,
45.9462543729349));
#171887=CARTESIAN_POINT('Ctrl Pts',(60.3627467385963,-1.13830090535116E-13,
45.9462645674752));
#171888=CARTESIAN_POINT('Origin',(69.7358040552328,0.,40.0761166693274));
#171889=CARTESIAN_POINT('',(60.5873249407211,2.12028922040352E-12,47.2199108422682));
#171890=CARTESIAN_POINT('',(60.571124584323,-1.00246535761107E-5,47.128034055528));
#171891=CARTESIAN_POINT('',(59.6415245868576,-1.25526296912604E-15,41.8560104904131));
#171892=CARTESIAN_POINT('Ctrl Pts',(60.5873249407211,4.24183370377617E-12,
47.2199108422682));
#171893=CARTESIAN_POINT('Ctrl Pts',(60.5871564475275,0.0519374417576126,
47.2189552698825));
#171894=CARTESIAN_POINT('Ctrl Pts',(60.5873745952724,0.103873817754455,
47.217919139388));
#171895=CARTESIAN_POINT('Ctrl Pts',(60.5890147051784,0.244664900100287,
47.2148949648136));
#171896=CARTESIAN_POINT('Ctrl Pts',(60.5911823537611,0.333503310376602,
47.2127540973366));
#171897=CARTESIAN_POINT('Ctrl Pts',(60.5986397676944,0.534130867503647,
47.2074058867246));
#171898=CARTESIAN_POINT('Ctrl Pts',(60.6045932141645,0.645880780145617,
47.2040663378404));
#171899=CARTESIAN_POINT('Ctrl Pts',(60.6304768520209,1.01870811056277,47.1917537198258));
#171900=CARTESIAN_POINT('Ctrl Pts',(60.6584366639251,1.27907486694412,47.1812349816448));
#171901=CARTESIAN_POINT('Ctrl Pts',(60.7880120193026,2.16808233850058,47.1390937889102));
#171902=CARTESIAN_POINT('Ctrl Pts',(60.9374985460543,2.78786671149221,47.0990072009642));
#171903=CARTESIAN_POINT('Ctrl Pts',(61.1900215853618,3.52748128373783,47.0387965184134));
#171904=CARTESIAN_POINT('Ctrl Pts',(61.2401114909548,3.66459092317205,47.0270823680358));
#171905=CARTESIAN_POINT('Ctrl Pts',(61.3255306601509,3.88382929836638,47.007454930536));
#171906=CARTESIAN_POINT('Ctrl Pts',(61.3590542006774,3.96666480758704,46.9998286393197));
#171907=CARTESIAN_POINT('Ctrl Pts',(61.4321884305318,4.14081609533997,46.9833470018634));
#171908=CARTESIAN_POINT('Ctrl Pts',(61.4720532157607,4.23201124356125,46.9744516285704));
#171909=CARTESIAN_POINT('Ctrl Pts',(61.5744035817512,4.45717904801317,46.9518224235189));
#171910=CARTESIAN_POINT('Ctrl Pts',(61.6384592545527,4.59038750526218,46.9378399665963));
#171911=CARTESIAN_POINT('Ctrl Pts',(61.8921155097484,5.0899640530361,46.8830904450713));
#171912=CARTESIAN_POINT('Ctrl Pts',(62.1007438273467,5.4458847515296,46.839296717377));
#171913=CARTESIAN_POINT('Ctrl Pts',(62.6031325361139,6.19534142306503,46.7355277545459));
#171914=CARTESIAN_POINT('Ctrl Pts',(62.9048803410925,6.58207761561037,46.6741998497982));
#171915=CARTESIAN_POINT('Ctrl Pts',(63.293271610961,7.01212801484634,46.5952290695433));
#171916=CARTESIAN_POINT('Ctrl Pts',(63.3546606214733,7.07830913213025,46.5827451887376));
#171917=CARTESIAN_POINT('Ctrl Pts',(63.4520625791018,7.18055135714168,46.5629241663619));
#171918=CARTESIAN_POINT('Ctrl Pts',(63.4874920916229,7.2171858876578,46.555711603057));
#171919=CARTESIAN_POINT('Ctrl Pts',(63.5650691999907,7.29620384287648,46.5399101309933));
#171920=CARTESIAN_POINT('Ctrl Pts',(63.6073161003812,7.33848254909956,46.5312996565791));
#171921=CARTESIAN_POINT('Ctrl Pts',(63.7263408827705,7.45551145249706,46.5070311125269));
#171922=CARTESIAN_POINT('Ctrl Pts',(63.8039156271988,7.52940467225742,46.4912029541305));
#171923=CARTESIAN_POINT('Ctrl Pts',(63.9881085295817,7.6993645425123,46.4536182221693));
#171924=CARTESIAN_POINT('Ctrl Pts',(64.0956077657255,7.794402565646,46.4316811394151));
#171925=CARTESIAN_POINT('Ctrl Pts',(64.5348417557687,8.16634727674466,46.3421279905083));
#171926=CARTESIAN_POINT('Ctrl Pts',(64.8818441192843,8.4237997354602,46.2715763734489));
#171927=CARTESIAN_POINT('Ctrl Pts',(65.2700328272329,8.67467908947449,46.1933213604471));
#171928=CARTESIAN_POINT('Ctrl Pts',(65.2961334872847,8.69137610097679,46.1880627096418));
#171929=CARTESIAN_POINT('Ctrl Pts',(65.5828359801181,8.87291260119502,46.1303329060429));
#171930=CARTESIAN_POINT('Ctrl Pts',(65.8506843749084,9.02563123887694,46.076710619746));
#171931=CARTESIAN_POINT('Ctrl Pts',(66.2352631706985,9.22187963702733,46.0002380995568));
#171932=CARTESIAN_POINT('Ctrl Pts',(66.3465147266043,9.27606144512495,45.9781734877417));
#171933=CARTESIAN_POINT('Ctrl Pts',(66.5451966231694,9.36828070798211,45.9388711386241));
#171934=CARTESIAN_POINT('Ctrl Pts',(66.6322270728671,9.4071657652942,45.9216891775339));
#171935=CARTESIAN_POINT('Ctrl Pts',(66.8178548917409,9.48692223649771,45.8851123870488));
#171936=CARTESIAN_POINT('Ctrl Pts',(66.9165760963242,9.52746766906352,45.8657016045507));
#171937=CARTESIAN_POINT('Ctrl Pts',(67.1941347364996,9.63627045143624,45.8112382341993));
#171938=CARTESIAN_POINT('Ctrl Pts',(67.3742908986744,9.70094777096812,45.7760149853913));
#171939=CARTESIAN_POINT('Ctrl Pts',(67.7968053742221,9.83897598914569,45.6936568011168));
#171940=CARTESIAN_POINT('Ctrl Pts',(68.040301335604,9.90832710885732,45.6463811983437));
#171941=CARTESIAN_POINT('Ctrl Pts',(68.6146589195713,10.0483790543752,45.5351293205157));
#171942=CARTESIAN_POINT('Ctrl Pts',(68.9469805374208,10.1115920792684,45.4709604920435));
#171943=CARTESIAN_POINT('Ctrl Pts',(69.6044930380109,10.2020797536131,45.3438728708097));
#171944=CARTESIAN_POINT('Ctrl Pts',(69.9291162995728,10.2305157759936,45.2810663848514));
#171945=CARTESIAN_POINT('Ctrl Pts',(70.3349339806519,10.2459346665038,45.2020885532685));
#171946=CARTESIAN_POINT('Ctrl Pts',(70.4154447647139,10.2480082394494,45.1863971062708));
#171947=CARTESIAN_POINT('Ctrl Pts',(70.5470480816301,10.2497878425927,45.160701858097));
#171948=CARTESIAN_POINT('Ctrl Pts',(70.5981326345252,10.2500822701963,45.1507163660395));
#171949=CARTESIAN_POINT('Ctrl Pts',(70.7050082934605,10.2498690109389,45.1297990482548));
#171950=CARTESIAN_POINT('Ctrl Pts',(70.7607967475691,10.2492848580112,45.1188656108937));
#171951=CARTESIAN_POINT('Ctrl Pts',(70.9180175300403,10.2463057933422,45.0880162319155));
#171952=CARTESIAN_POINT('Ctrl Pts',(71.0194175813151,10.2428201418387,45.0680761907018));
#171953=CARTESIAN_POINT('Ctrl Pts',(71.2555110077228,10.2310581916697,45.0215678482867));
#171954=CARTESIAN_POINT('Ctrl Pts',(71.3901226643612,10.2215815350339,44.9949888957795));
#171955=CARTESIAN_POINT('Ctrl Pts',(71.9005363163362,10.1751141686502,44.8940465128647));
#171956=CARTESIAN_POINT('Ctrl Pts',(72.2743287847078,10.1193283777581,44.8197999528818));
#171957=CARTESIAN_POINT('Ctrl Pts',(73.0686513712459,9.95379079981624,44.6620294481148));
#171958=CARTESIAN_POINT('Ctrl Pts',(73.4871007991411,9.83745271014495,44.5789280180757));
#171959=CARTESIAN_POINT('Ctrl Pts',(74.0420450640677,9.64315886050844,44.4690533444287));
#171960=CARTESIAN_POINT('Ctrl Pts',(74.1860060644551,9.58897364333637,44.4405789949054));
#171961=CARTESIAN_POINT('Ctrl Pts',(74.421224520611,9.4941550969204,44.394104556992));
#171962=CARTESIAN_POINT('Ctrl Pts',(74.5132030050931,9.45546051520291,44.3759442027451));
#171963=CARTESIAN_POINT('Ctrl Pts',(74.6947908819492,9.37583573131703,44.3401152079155));
#171964=CARTESIAN_POINT('Ctrl Pts',(74.7844056646576,9.33494647237442,44.3224451806072));
#171965=CARTESIAN_POINT('Ctrl Pts',(75.0062494890913,9.22972593820227,44.2787282995957));
#171966=CARTESIAN_POINT('Ctrl Pts',(75.1377161578585,9.16377515270088,44.2528446214116));
#171967=CARTESIAN_POINT('Ctrl Pts',(75.6346452031636,8.90059765838181,44.1550648786954));
#171968=CARTESIAN_POINT('Ctrl Pts',(75.9894819445791,8.68340312009844,44.0853829409446));
#171969=CARTESIAN_POINT('Ctrl Pts',(76.7219272858651,8.16991955358759,43.9410902482714));
#171970=CARTESIAN_POINT('Ctrl Pts',(77.0940372937178,7.86730609168436,43.8674927572876));
#171971=CARTESIAN_POINT('Ctrl Pts',(77.5093589639703,7.47718361018491,43.7839344578914));
#171972=CARTESIAN_POINT('Ctrl Pts',(77.5743603497403,7.41446178376609,43.7708110606936));
#171973=CARTESIAN_POINT('Ctrl Pts',(77.6747217500709,7.31498208913852,43.7504651716978));
#171974=CARTESIAN_POINT('Ctrl Pts',(77.7106526285462,7.2788230430956,43.7431638121824));
#171975=CARTESIAN_POINT('Ctrl Pts',(77.7880960133048,7.19969750684008,43.7273864109151));
#171976=CARTESIAN_POINT('Ctrl Pts',(77.8295055023672,7.15663026675921,43.7189245054143));
#171977=CARTESIAN_POINT('Ctrl Pts',(77.9440193072145,7.03539752640193,43.6954567697067));
#171978=CARTESIAN_POINT('Ctrl Pts',(78.0162791671139,6.95642203091557,43.6805704053421));
#171979=CARTESIAN_POINT('Ctrl Pts',(78.1823805770609,6.76899864007856,43.6461892352308));
#171980=CARTESIAN_POINT('Ctrl Pts',(78.2752129779155,6.65965871258256,43.6268473869962));
#171981=CARTESIAN_POINT('Ctrl Pts',(78.6374155050432,6.21424936763742,43.5509491057436));
#171982=CARTESIAN_POINT('Ctrl Pts',(78.8878691627596,5.86285397478378,43.4974868806145));
#171983=CARTESIAN_POINT('Ctrl Pts',(79.1352093193116,5.46480783062019,43.4440029010219));
#171984=CARTESIAN_POINT('Ctrl Pts',(79.1546002497502,5.43322088197864,43.4398045953535));
#171985=CARTESIAN_POINT('Ctrl Pts',(79.3341334925697,5.13718010259645,43.400886083636));
#171986=CARTESIAN_POINT('Ctrl Pts',(79.482535628112,4.8655074135214,43.3683615333574));
#171987=CARTESIAN_POINT('Ctrl Pts',(79.6734714121739,4.47511303312139,43.3260705991843));
#171988=CARTESIAN_POINT('Ctrl Pts',(79.7263361053394,4.36185333848243,43.314304343712));
#171989=CARTESIAN_POINT('Ctrl Pts',(79.816340313465,4.15951384729163,43.2941683456253));
#171990=CARTESIAN_POINT('Ctrl Pts',(79.8543074901914,4.07083532066365,43.2856380090069));
#171991=CARTESIAN_POINT('Ctrl Pts',(79.9322065376245,3.88161064836288,43.2680557166844));
#171992=CARTESIAN_POINT('Ctrl Pts',(79.9718155453191,3.78093859836991,43.2590666237938));
#171993=CARTESIAN_POINT('Ctrl Pts',(80.0781847516176,3.49762409667531,43.2347791536815));
#171994=CARTESIAN_POINT('Ctrl Pts',(80.1414081208651,3.3136454852178,43.2201666573747));
#171995=CARTESIAN_POINT('Ctrl Pts',(80.2763031662515,2.88192563767089,43.1885013418342));
#171996=CARTESIAN_POINT('Ctrl Pts',(80.3440064937989,2.63302899713405,43.1722087327176));
#171997=CARTESIAN_POINT('Ctrl Pts',(80.4801266227141,2.04721819758891,43.1382185405716));
#171998=CARTESIAN_POINT('Ctrl Pts',(80.541252417161,1.70885495919348,43.1218704635874));
#171999=CARTESIAN_POINT('Ctrl Pts',(80.627944089206,1.04081766298725,43.0954585336299));
#172000=CARTESIAN_POINT('Ctrl Pts',(80.6547926742552,0.711737294504319,
43.0851815816499));
#172001=CARTESIAN_POINT('Ctrl Pts',(80.6686481681964,0.299927717328372,
43.0753450364434));
#172002=CARTESIAN_POINT('Ctrl Pts',(80.6704327125468,0.217946679402327,
43.0735356912178));
#172003=CARTESIAN_POINT('Ctrl Pts',(80.6717578321756,0.0839178240909962,
43.0708126560324));
#172004=CARTESIAN_POINT('Ctrl Pts',(80.67188009463,0.0318810271266049,43.0698132826031));
#172005=CARTESIAN_POINT('Ctrl Pts',(80.6713148272797,-0.0770080455644929,
43.0678405802884));
#172006=CARTESIAN_POINT('Ctrl Pts',(80.6705513802445,-0.133857986641344,
43.0668785511626));
#172007=CARTESIAN_POINT('Ctrl Pts',(80.667079714772,-0.294109986102082,
43.0643623114152));
#172008=CARTESIAN_POINT('Ctrl Pts',(80.6632908376584,-0.397484394424257,
43.0629688231807));
#172009=CARTESIAN_POINT('Ctrl Pts',(80.6508593713272,-0.638215106263754,
43.0602789829982));
#172010=CARTESIAN_POINT('Ctrl Pts',(80.6410281260701,-0.775492601098059,
43.0591671216325));
#172011=CARTESIAN_POINT('Ctrl Pts',(80.5933085952772,-1.29632051534599,
43.0566247738066));
#172012=CARTESIAN_POINT('Ctrl Pts',(80.536813390687,-1.67786412892185,43.0582372283862));
#172013=CARTESIAN_POINT('Ctrl Pts',(80.3706280454606,-2.48729888203156,
43.0698348543323));
#172014=CARTESIAN_POINT('Ctrl Pts',(80.2546125106642,-2.91309850439924,
43.0809903021381));
#172015=CARTESIAN_POINT('Ctrl Pts',(80.0614517956559,-3.47799653012537,
43.1030414945953));
#172016=CARTESIAN_POINT('Ctrl Pts',(80.0075614723663,-3.62471446433682,
43.1094536823156));
#172017=CARTESIAN_POINT('Ctrl Pts',(79.913328725701,-3.8644290461771,43.1210703926915));
#172018=CARTESIAN_POINT('Ctrl Pts',(79.8748899114175,-3.95816359123738,
43.1259061289921));
#172019=CARTESIAN_POINT('Ctrl Pts',(79.7958232148824,-4.1432143570785,43.1360375687693));
#172020=CARTESIAN_POINT('Ctrl Pts',(79.7552355746164,-4.23453612509113,
43.1413257403168));
#172021=CARTESIAN_POINT('Ctrl Pts',(79.6508266998838,-4.46060147477623,
43.155136003301));
#172022=CARTESIAN_POINT('Ctrl Pts',(79.5854154597721,-4.59456592259702,
43.1639672045073));
#172023=CARTESIAN_POINT('Ctrl Pts',(79.3244971024167,-5.10092839006078,
43.1998163343256));
#172024=CARTESIAN_POINT('Ctrl Pts',(79.1093833757438,-5.46247750646331,
43.230631984325));
#172025=CARTESIAN_POINT('Ctrl Pts',(78.6011111125618,-6.20884947895576,
43.3051113107463));
#172026=CARTESIAN_POINT('Ctrl Pts',(78.3017326841511,-6.58808201372149,
43.3499154294459));
#172027=CARTESIAN_POINT('Ctrl Pts',(77.9157746364577,-7.01160016243578,
43.4076444552552));
#172028=CARTESIAN_POINT('Ctrl Pts',(77.8537212777866,-7.07789313494804,
43.4169242318052));
#172029=CARTESIAN_POINT('Ctrl Pts',(77.7552995617537,-7.1802631320795,43.4316291627336));
#172030=CARTESIAN_POINT('Ctrl Pts',(77.7195246613939,-7.21691604866152,
43.4369714658208));
#172031=CARTESIAN_POINT('Ctrl Pts',(77.6412383662243,-7.29592258615367,
43.4486534099141));
#172032=CARTESIAN_POINT('Ctrl Pts',(77.5986270650052,-7.33817230198449,
43.4550066387119));
#172033=CARTESIAN_POINT('Ctrl Pts',(77.4786763537277,-7.45502111370519,
43.4728813352592));
#172034=CARTESIAN_POINT('Ctrl Pts',(77.4005342299879,-7.52876784812212,
43.4845149088992));
#172035=CARTESIAN_POINT('Ctrl Pts',(77.2150883630637,-7.69831511441796,
43.5121210388767));
#172036=CARTESIAN_POINT('Ctrl Pts',(77.1069018828138,-7.79309528589141,
43.5282242632328));
#172037=CARTESIAN_POINT('Ctrl Pts',(76.6662076126637,-8.16297015691732,
43.5938985101831));
#172038=CARTESIAN_POINT('Ctrl Pts',(76.3185659012665,-8.41889910404204,
43.6458967804122));
#172039=CARTESIAN_POINT('Ctrl Pts',(75.9248678412809,-8.67177747161641,
43.7054448333481));
#172040=CARTESIAN_POINT('Ctrl Pts',(75.8936102813695,-8.69161375696135,
43.7101767933696));
#172041=CARTESIAN_POINT('Ctrl Pts',(75.6008156388286,-8.87518212604365,
43.7545422217171));
#172042=CARTESIAN_POINT('Ctrl Pts',(75.3321914560878,-9.02697206838936,
43.7955508772855));
#172043=CARTESIAN_POINT('Ctrl Pts',(74.9462627371051,-9.22234575861689,
43.8549769372163));
#172044=CARTESIAN_POINT('Ctrl Pts',(74.8343063316602,-9.27645009603366,
43.8722731053681));
#172045=CARTESIAN_POINT('Ctrl Pts',(74.6343121168603,-9.36858305952962,
43.903271672497));
#172046=CARTESIAN_POINT('Ctrl Pts',(74.5466669634561,-9.40745463550601,
43.9168901811612));
#172047=CARTESIAN_POINT('Ctrl Pts',(74.3596588868407,-9.48722342041452,
43.9460181568663));
#172048=CARTESIAN_POINT('Ctrl Pts',(74.2601729805711,-9.52779173985729,
43.9615552427644));
#172049=CARTESIAN_POINT('Ctrl Pts',(73.9802139575753,-9.63676333365362,
44.0053878124279));
#172050=CARTESIAN_POINT('Ctrl Pts',(73.7984355834092,-9.70156429009606,
44.0339756927895));
#172051=CARTESIAN_POINT('Ctrl Pts',(73.3719200177862,-9.83991029545085,
44.1013020961864));
#172052=CARTESIAN_POINT('Ctrl Pts',(73.1260552626071,-9.90941505802381,
44.1402999252907));
#172053=CARTESIAN_POINT('Ctrl Pts',(72.5474315430654,-10.0493690288865,
44.232338296622));
#172054=CARTESIAN_POINT('Ctrl Pts',(72.2132565585436,-10.1124040507284,
44.2856924209878));
#172055=CARTESIAN_POINT('Ctrl Pts',(71.5534738449002,-10.202362245212,44.3909041972888));
#172056=CARTESIAN_POINT('Ctrl Pts',(71.2284531024807,-10.2305863855897,
44.4426714292048));
#172057=CARTESIAN_POINT('Ctrl Pts',(70.8216437334047,-10.2459391285614,
44.5070095981421));
#172058=CARTESIAN_POINT('Ctrl Pts',(70.7406527336991,-10.248010740629,44.5197958176052));
#172059=CARTESIAN_POINT('Ctrl Pts',(70.608234566533,-10.2497885692664,44.5406553358949));
#172060=CARTESIAN_POINT('Ctrl Pts',(70.5568211392339,-10.2500825110406,
44.5487430955347));
#172061=CARTESIAN_POINT('Ctrl Pts',(70.4492319134183,-10.2498683828576,
44.5656416040368));
#172062=CARTESIAN_POINT('Ctrl Pts',(70.3930580572796,-10.2492835854339,
44.5744499238695));
#172063=CARTESIAN_POINT('Ctrl Pts',(70.2347053238982,-10.2463015870132,
44.5992433882946));
#172064=CARTESIAN_POINT('Ctrl Pts',(70.1325485761743,-10.2428122281872,
44.6151948037664));
#172065=CARTESIAN_POINT('Ctrl Pts',(69.8946394685958,-10.2310366361465,
44.652262738275));
#172066=CARTESIAN_POINT('Ctrl Pts',(69.7589604284561,-10.2215477564663,
44.6733412272971));
#172067=CARTESIAN_POINT('Ctrl Pts',(69.2441679456989,-10.174994202201,44.7531563675436));
#172068=CARTESIAN_POINT('Ctrl Pts',(68.8669901670021,-10.1190765762285,
44.8113137454806));
#172069=CARTESIAN_POINT('Ctrl Pts',(68.066825914051,-9.95340131103121,44.9346989832805));
#172070=CARTESIAN_POINT('Ctrl Pts',(67.6459084115125,-9.83721199074886,
44.9996169626139));
#172071=CARTESIAN_POINT('Ctrl Pts',(67.0875426433126,-9.64315796278377,
45.0860637394411));
#172072=CARTESIAN_POINT('Ctrl Pts',(66.942525244642,-9.58897289101964,45.1085440893086));
#172073=CARTESIAN_POINT('Ctrl Pts',(66.7055975799226,-9.49415453239639,
45.1453217638451));
#172074=CARTESIAN_POINT('Ctrl Pts',(66.6129549614752,-9.45545997345516,
45.1597150932927));
#172075=CARTESIAN_POINT('Ctrl Pts',(66.4300639583688,-9.3758351715069,45.1881535595771));
#172076=CARTESIAN_POINT('Ctrl Pts',(66.339810036177,-9.3349458669878,45.2021992366496));
#172077=CARTESIAN_POINT('Ctrl Pts',(66.1163925046861,-9.22972506860246,
45.2369939366841));
#172078=CARTESIAN_POINT('Ctrl Pts',(65.9840011088537,-9.16377404837579,
45.2576355464542));
#172079=CARTESIAN_POINT('Ctrl Pts',(65.4835943080076,-8.90059447483589,
45.3357129498621));
#172080=CARTESIAN_POINT('Ctrl Pts',(65.1263212256947,-8.68339771016354,
45.3915951293686));
#172081=CARTESIAN_POINT('Ctrl Pts',(64.3886987673181,-8.16991404466073,
45.5065150834696));
#172082=CARTESIAN_POINT('Ctrl Pts',(64.0138622521309,-7.86730371821761,
45.5646244994196));
#172083=CARTESIAN_POINT('Ctrl Pts',(63.5950125094422,-7.47718472766329,
45.6281532192212));
#172084=CARTESIAN_POINT('Ctrl Pts',(63.5294424717323,-7.41446268093463,
45.6380530811232));
#172085=CARTESIAN_POINT('Ctrl Pts',(63.4281746160734,-7.31498272542267,
45.6532598632049));
#172086=CARTESIAN_POINT('Ctrl Pts',(63.3919133817252,-7.27882364471826,
45.658687920089));
#172087=CARTESIAN_POINT('Ctrl Pts',(63.3137442407122,-7.19969814627209,
45.6703492067521));
#172088=CARTESIAN_POINT('Ctrl Pts',(63.2719379716636,-7.15663098044244,
45.6765604866738));
#172089=CARTESIAN_POINT('Ctrl Pts',(63.1563041556976,-7.03539868499352,
45.6936739981997));
#172090=CARTESIAN_POINT('Ctrl Pts',(63.0833109873441,-6.95642356980787,
45.7043996721642));
#172091=CARTESIAN_POINT('Ctrl Pts',(62.9154685813085,-6.76900129687135,
45.7289018372709));
#172092=CARTESIAN_POINT('Ctrl Pts',(62.8216199300911,-6.65966212267454,
45.7424769156831));
#172093=CARTESIAN_POINT('Ctrl Pts',(62.4553067246819,-6.21425882266641,
45.795035775327));
#172094=CARTESIAN_POINT('Ctrl Pts',(62.2016754873669,-5.86286921032458,
45.8304574636465));
#172095=CARTESIAN_POINT('Ctrl Pts',(61.9509507119463,-5.46481180954629,
45.8647954666217));
#172096=CARTESIAN_POINT('Ctrl Pts',(61.9312823810656,-5.43320728852651,
45.8674839294922));
#172097=CARTESIAN_POINT('Ctrl Pts',(61.7492608890216,-5.13715680284549,
45.8923170610155));
#172098=CARTESIAN_POINT('Ctrl Pts',(61.5986899025736,-4.86549261324594,
45.9125097546087));
#172099=CARTESIAN_POINT('Ctrl Pts',(61.4048096975294,-4.47510786706544,
45.9380724816467));
#172100=CARTESIAN_POINT('Ctrl Pts',(61.3511092500408,-4.3618488885061,45.9450965527575));
#172101=CARTESIAN_POINT('Ctrl Pts',(61.2596465005726,-4.15951019677586,
45.9569580944416));
#172102=CARTESIAN_POINT('Ctrl Pts',(61.2210515491285,-4.07083174153613,
45.9619277291097));
#172103=CARTESIAN_POINT('Ctrl Pts',(61.1418368244989,-3.88160671513911,
45.9720488284767));
#172104=CARTESIAN_POINT('Ctrl Pts',(61.1015419590627,-3.78093423329831,
45.9771489368012));
#172105=CARTESIAN_POINT('Ctrl Pts',(60.9932798949756,-3.49761694931462,
45.9907066997055));
#172106=CARTESIAN_POINT('Ctrl Pts',(60.9288709322941,-3.31363594505769,
45.9985991857891));
#172107=CARTESIAN_POINT('Ctrl Pts',(60.791279175395,-2.88190894604371,46.0149805254003));
#172108=CARTESIAN_POINT('Ctrl Pts',(60.7220856319191,-2.63300748931425,
46.0228264525751));
#172109=CARTESIAN_POINT('Ctrl Pts',(60.582549728761,-2.04719203233801,46.0374417944943));
#172110=CARTESIAN_POINT('Ctrl Pts',(60.5195198417882,-1.70882907243014,
46.0429857225426));
#172111=CARTESIAN_POINT('Ctrl Pts',(60.4290257267372,-1.04080017320016,
46.0478165601401));
#172112=CARTESIAN_POINT('Ctrl Pts',(60.4002825268621,-0.711728004843181,
46.0473420685351));
#172113=CARTESIAN_POINT('Ctrl Pts',(60.3838987009321,-0.299926844234377,
46.0428376814325));
#172114=CARTESIAN_POINT('Ctrl Pts',(60.3816029562331,-0.21794597743042,
46.0417478042074));
#172115=CARTESIAN_POINT('Ctrl Pts',(60.3795355269043,-0.0906355194028028,
46.0397477506953));
#172116=CARTESIAN_POINT('Ctrl Pts',(60.3790941463259,-0.0453180362328119,
46.0389753237333));
#172117=CARTESIAN_POINT('Ctrl Pts',(60.3789471275204,1.31869374016412E-10,
46.0381415386512));
#172118=CARTESIAN_POINT('Ctrl Pts',(60.3627467385963,-1.13830090535116E-13,
45.9462645674752));
#172119=CARTESIAN_POINT('Ctrl Pts',(60.3629210969066,-0.0537453435861863,
45.9472534025903));
#172120=CARTESIAN_POINT('Ctrl Pts',(60.3635140173742,-0.107489596541202,
45.9481816946506));
#172121=CARTESIAN_POINT('Ctrl Pts',(60.3662357203024,-0.252129721537147,
45.9505137108538));
#172122=CARTESIAN_POINT('Ctrl Pts',(60.3691429658746,-0.343008082848155,
45.9518021386462));
#172123=CARTESIAN_POINT('Ctrl Pts',(60.3784525920476,-0.549144354899051,
45.9543100815123));
#172124=CARTESIAN_POINT('Ctrl Pts',(60.3855850233311,-0.664358651866915,
45.9554172690278));
#172125=CARTESIAN_POINT('Ctrl Pts',(60.4163177143643,-1.05503640493196,
45.9581327905588));
#172126=CARTESIAN_POINT('Ctrl Pts',(60.4489978372468,-1.32967619768264,
45.9582819908947));
#172127=CARTESIAN_POINT('Ctrl Pts',(60.5885132993943,-2.20373001633204,
45.9526845389634));
#172128=CARTESIAN_POINT('Ctrl Pts',(60.7369835307299,-2.79513263192651,
45.9395791997444));
#172129=CARTESIAN_POINT('Ctrl Pts',(60.9850572371069,-3.51115661396042,
45.9110331525872));
#172130=CARTESIAN_POINT('Ctrl Pts',(61.0370396938302,-3.65135059926042,
45.9048159910799));
#172131=CARTESIAN_POINT('Ctrl Pts',(61.1251537700211,-3.87413141348213,
45.8939207614984));
#172132=CARTESIAN_POINT('Ctrl Pts',(61.1593746367891,-3.95746834551078,
45.8896130140066));
#172133=CARTESIAN_POINT('Ctrl Pts',(61.2335610766254,-4.13165034516851,
45.8801200764335));
#172134=CARTESIAN_POINT('Ctrl Pts',(61.2737528242459,-4.22238656688466,
45.8748907015453));
#172135=CARTESIAN_POINT('Ctrl Pts',(61.3758566536567,-4.44424755395228,
45.8614036960955));
#172136=CARTESIAN_POINT('Ctrl Pts',(61.4392213392701,-4.57466247116494,
45.8528636219607));
#172137=CARTESIAN_POINT('Ctrl Pts',(61.6826735746847,-5.05008549496835,
45.81947997045));
#172138=CARTESIAN_POINT('Ctrl Pts',(61.879326184238,-5.38600561318496,45.7914280866291));
#172139=CARTESIAN_POINT('Ctrl Pts',(62.3783059639627,-6.13745551539409,
45.7186009764369));
#172140=CARTESIAN_POINT('Ctrl Pts',(62.6935772200122,-6.54287847846962,
45.6714425313701));
#172141=CARTESIAN_POINT('Ctrl Pts',(63.1020705535991,-6.99373713347628,
45.6103407892075));
#172142=CARTESIAN_POINT('Ctrl Pts',(63.1674870136203,-7.06392324356832,
45.6005570398216));
#172143=CARTESIAN_POINT('Ctrl Pts',(63.2699187681363,-7.1707596524641,45.5852515637908));
#172144=CARTESIAN_POINT('Ctrl Pts',(63.3062476940756,-7.20807396295211,
45.5798259531585));
#172145=CARTESIAN_POINT('Ctrl Pts',(63.3841084912721,-7.28682911761619,
45.5682062473634));
#172146=CARTESIAN_POINT('Ctrl Pts',(63.4257148039169,-7.3281921431653,45.5620021934324));
#172147=CARTESIAN_POINT('Ctrl Pts',(63.5396952313653,-7.43956450023324,
45.5450155661601));
#172148=CARTESIAN_POINT('Ctrl Pts',(63.6127471497991,-7.50885650709635,
45.5341386032939));
#172149=CARTESIAN_POINT('Ctrl Pts',(63.7834338217886,-7.66601574938943,
45.5087287945943));
#172150=CARTESIAN_POINT('Ctrl Pts',(63.8817580485864,-7.75309171207928,
45.4940945493024));
#172151=CARTESIAN_POINT('Ctrl Pts',(64.2509400991073,-8.06750558799496,
45.4390971857092));
#172152=CARTESIAN_POINT('Ctrl Pts',(64.5317749777085,-8.28246482312865,
45.3971575890294));
#172153=CARTESIAN_POINT('Ctrl Pts',(65.1796830971222,-8.72683161959794,
45.2996129541909));
#172154=CARTESIAN_POINT('Ctrl Pts',(65.5513081540276,-8.94820225798396,
45.2431427454616));
#172155=CARTESIAN_POINT('Ctrl Pts',(66.0530038921372,-9.20510060597355,
45.1659548702342));
#172156=CARTESIAN_POINT('Ctrl Pts',(66.1715292554078,-9.26289296654748,
45.1476553991507));
#172157=CARTESIAN_POINT('Ctrl Pts',(66.3787231055926,-9.35894403805032,
45.1155543724818));
#172158=CARTESIAN_POINT('Ctrl Pts',(66.466885753228,-9.39828742775446,45.1018608747481));
#172159=CARTESIAN_POINT('Ctrl Pts',(66.6520886273164,-9.47776749994737,
45.0730247213876));
#172160=CARTESIAN_POINT('Ctrl Pts',(66.7492160415553,-9.5176644533488,45.0578623295626));
#172161=CARTESIAN_POINT('Ctrl Pts',(67.0141733890003,-9.62169026337531,
45.0163975351537));
#172162=CARTESIAN_POINT('Ctrl Pts',(67.1830910319922,-9.68284408437236,
44.9898517591112));
#172163=CARTESIAN_POINT('Ctrl Pts',(67.6926848912736,-9.85203783106043,
44.9094825471871));
#172164=CARTESIAN_POINT('Ctrl Pts',(68.0374421943896,-9.94641933020242,
44.8547273931204));
#172165=CARTESIAN_POINT('Ctrl Pts',(68.8606804526575,-10.1251489765166,
44.7235902363861));
#172166=CARTESIAN_POINT('Ctrl Pts',(69.3416223638702,-10.1934737053383,
44.6466678097345));
#172167=CARTESIAN_POINT('Ctrl Pts',(69.9679911044351,-10.2363736959526,
44.5472219732214));
#172168=CARTESIAN_POINT('Ctrl Pts',(70.110543023416,-10.2430760478758,44.5246408207548));
#172169=CARTESIAN_POINT('Ctrl Pts',(70.3166748660034,-10.2483506458548,
44.4921015816188));
#172170=CARTESIAN_POINT('Ctrl Pts',(70.3801664949231,-10.2493705227098,
44.4820945678289));
#172171=CARTESIAN_POINT('Ctrl Pts',(70.4938303869501,-10.2501140724956,
44.4642121487561));
#172172=CARTESIAN_POINT('Ctrl Pts',(70.5439972620434,-10.2500649704298,
44.4563311322078));
#172173=CARTESIAN_POINT('Ctrl Pts',(70.6617756049254,-10.2490640284763,
44.4378555056053));
#172174=CARTESIAN_POINT('Ctrl Pts',(70.7293829254277,-10.2478042331192,
44.427270433084));
#172175=CARTESIAN_POINT('Ctrl Pts',(70.9673230379516,-10.240958181047,44.390079295044));
#172176=CARTESIAN_POINT('Ctrl Pts',(71.1375391116156,-10.2317072888623,
44.3635860777138));
#172177=CARTESIAN_POINT('Ctrl Pts',(71.5995033240834,-10.1947550182515,
44.2918838205177));
#172178=CARTESIAN_POINT('Ctrl Pts',(71.8904490470167,-10.1585882197607,
44.2469404631009));
#172179=CARTESIAN_POINT('Ctrl Pts',(72.7395208250848,-10.0150058563067,
44.1159379662807));
#172180=CARTESIAN_POINT('Ctrl Pts',(73.2907769626046,-9.87283043966821,
44.0310331869294));
#172181=CARTESIAN_POINT('Ctrl Pts',(73.9690212236715,-9.63498248067833,
43.9260107583852));
#172182=CARTESIAN_POINT('Ctrl Pts',(74.1096484363916,-9.58209792534047,
43.9042082570258));
#172183=CARTESIAN_POINT('Ctrl Pts',(74.3414367412509,-9.48894970069511,
43.8682253495136));
#172184=CARTESIAN_POINT('Ctrl Pts',(74.4332675145068,-9.45045248926828,
43.8539570690286));
#172185=CARTESIAN_POINT('Ctrl Pts',(74.6160189034456,-9.37062962594823,
43.8255384242235));
#172186=CARTESIAN_POINT('Ctrl Pts',(74.7069263835331,-9.32930112281805,
43.8113900396457));
#172187=CARTESIAN_POINT('Ctrl Pts',(74.9349003330417,-9.22153850265106,
43.775883228647));
#172188=CARTESIAN_POINT('Ctrl Pts',(75.0711172754451,-9.15332794471267,
43.7546431175649));
#172189=CARTESIAN_POINT('Ctrl Pts',(75.3694320448253,-8.99539122241514,
43.708093592273));
#172190=CARTESIAN_POINT('Ctrl Pts',(75.5307236640642,-8.9042263174588,43.6829023872182));
#172191=CARTESIAN_POINT('Ctrl Pts',(76.0897573432447,-8.56763067672749,
43.5955982706218));
#172192=CARTESIAN_POINT('Ctrl Pts',(76.4731412819818,-8.29896087700861,
43.5357170139515));
#172193=CARTESIAN_POINT('Ctrl Pts',(77.037456562796,-7.84235692315833,43.4485821656145));
#172194=CARTESIAN_POINT('Ctrl Pts',(77.2317809219798,-7.67251750957461,
43.4187906970589));
#172195=CARTESIAN_POINT('Ctrl Pts',(77.478104087099,-7.44020544823845,43.3815107049779));
#172196=CARTESIAN_POINT('Ctrl Pts',(77.5359859775027,-7.38431155568068,
43.3727877092191));
#172197=CARTESIAN_POINT('Ctrl Pts',(77.6325014416984,-7.28888816280562,
43.3583141346835));
#172198=CARTESIAN_POINT('Ctrl Pts',(77.6714789556455,-7.24972346637005,
43.3524894778163));
#172199=CARTESIAN_POINT('Ctrl Pts',(77.756893509239,-7.16250023184012,43.3397729638602));
#172200=CARTESIAN_POINT('Ctrl Pts',(77.8031830606127,-7.11429737354174,
43.3329124263439));
#172201=CARTESIAN_POINT('Ctrl Pts',(77.9487082318632,-6.95976294760169,
43.3114361643479));
#172202=CARTESIAN_POINT('Ctrl Pts',(78.0461819095162,-6.85174566132742,
43.2971894866158));
#172203=CARTESIAN_POINT('Ctrl Pts',(78.2887357799658,-6.57118963592098,
43.2620388806591));
#172204=CARTESIAN_POINT('Ctrl Pts',(78.4305347328856,-6.39583619833343,
43.241778663432));
#172205=CARTESIAN_POINT('Ctrl Pts',(78.9402590384094,-5.72125868764573,
43.169795660147));
#172206=CARTESIAN_POINT('Ctrl Pts',(79.2689273126923,-5.19329707652492,
43.1250781316381));
#172207=CARTESIAN_POINT('Ctrl Pts',(79.6086844404968,-4.518604276133,43.0801780059318));
#172208=CARTESIAN_POINT('Ctrl Pts',(79.6667461609775,-4.3974766723292,43.0725691258047));
#172209=CARTESIAN_POINT('Ctrl Pts',(79.7628822454898,-4.18645187756787,
43.0600836221655));
#172210=CARTESIAN_POINT('Ctrl Pts',(79.8020721324873,-4.09709336258671,
43.0550299401882));
#172211=CARTESIAN_POINT('Ctrl Pts',(79.8809588588637,-3.91006239615493,
43.0449353168022));
#172212=CARTESIAN_POINT('Ctrl Pts',(79.9204394425517,-3.812309287656,43.0399285118045));
#172213=CARTESIAN_POINT('Ctrl Pts',(80.0227041100148,-3.54751383887044,
43.0270899072709));
#172214=CARTESIAN_POINT('Ctrl Pts',(80.0826786602154,-3.37940479590762,
43.0197041501388));
#172215=CARTESIAN_POINT('Ctrl Pts',(80.2738526992248,-2.79633897034405,
42.9967365023146));
#172216=CARTESIAN_POINT('Ctrl Pts',(80.3832694847052,-2.37460581584302,
42.9846450180873));
#172217=CARTESIAN_POINT('Ctrl Pts',(80.5618018003175,-1.45150579628832,
42.9685699092611));
#172218=CARTESIAN_POINT('Ctrl Pts',(80.6214510966608,-0.949445864507903,
42.9662086504445));
#172219=CARTESIAN_POINT('Ctrl Pts',(80.6488332517447,-0.352236933514285,
42.9720192689296));
#172220=CARTESIAN_POINT('Ctrl Pts',(80.6518514835544,-0.259336887938741,
42.9731696689341));
#172221=CARTESIAN_POINT('Ctrl Pts',(80.6546790942502,-0.111702451308424,
42.9754008249226));
#172222=CARTESIAN_POINT('Ctrl Pts',(80.6552975981326,-0.056986277958104,
42.9763156374376));
#172223=CARTESIAN_POINT('Ctrl Pts',(80.6556746885256,0.0519676945265764,
42.9783153064823));
#172224=CARTESIAN_POINT('Ctrl Pts',(80.6554407689613,0.106203715414807,
42.9793986064886));
#172225=CARTESIAN_POINT('Ctrl Pts',(80.6536895151984,0.251031796056709,
42.9825226610243));
#172226=CARTESIAN_POINT('Ctrl Pts',(80.6514167543075,0.341606701826619,
42.9847181540605));
#172227=CARTESIAN_POINT('Ctrl Pts',(80.6330993184868,0.82220059335519,42.9976203926994));
#172228=CARTESIAN_POINT('Ctrl Pts',(80.5963815172592,1.21100446686805,43.0124318899873));
#172229=CARTESIAN_POINT('Ctrl Pts',(80.4464285729306,2.20025734822541,43.0603767248664));
#172230=CARTESIAN_POINT('Ctrl Pts',(80.3019601354889,2.79416722331763,43.0989821326822));
#172231=CARTESIAN_POINT('Ctrl Pts',(80.0582437363962,3.51232919463471,43.1571964434274));
#172232=CARTESIAN_POINT('Ctrl Pts',(80.0073340152638,3.65229881537172,43.1691170888978));
#172233=CARTESIAN_POINT('Ctrl Pts',(79.9208882618855,3.87482165377092,43.188995938758));
#172234=CARTESIAN_POINT('Ctrl Pts',(79.8872658527491,3.95812179729244,43.1966499761715));
#172235=CARTESIAN_POINT('Ctrl Pts',(79.8142953100193,4.1322990173888,43.2131045870906));
#172236=CARTESIAN_POINT('Ctrl Pts',(79.7747176624397,4.22306641842177,43.2219412926025));
#172237=CARTESIAN_POINT('Ctrl Pts',(79.6740350787655,4.44515511869587,43.2442155063629));
#172238=CARTESIAN_POINT('Ctrl Pts',(79.6114611227259,4.57576285996777,43.2578856011995));
#172239=CARTESIAN_POINT('Ctrl Pts',(79.5048986406616,4.78661651051017,43.2809079168193));
#172240=CARTESIAN_POINT('Ctrl Pts',(79.4625506151416,4.86769677599351,43.2899966564355));
#172241=CARTESIAN_POINT('Ctrl Pts',(79.2948212238833,5.17862443130876,43.3257779641757));
#172242=CARTESIAN_POINT('Ctrl Pts',(79.1617957323111,5.40408866030519,43.3537046588196));
#172243=CARTESIAN_POINT('Ctrl Pts',(78.83262293428,5.91609954628576,43.4220320630696));
#172244=CARTESIAN_POINT('Ctrl Pts',(78.6302871003758,6.19813365337136,43.4634750166297));
#172245=CARTESIAN_POINT('Ctrl Pts',(78.2713525315724,6.64818542212518,43.5366264382315));
#172246=CARTESIAN_POINT('Ctrl Pts',(78.1225994869778,6.8223182383764,43.5668544867521));
#172247=CARTESIAN_POINT('Ctrl Pts',(77.9140611953691,7.0504050650835,43.6092602171263));
#172248=CARTESIAN_POINT('Ctrl Pts',(77.8592226037651,7.10897730187663,43.6204141512894));
#172249=CARTESIAN_POINT('Ctrl Pts',(77.7656306047343,7.20660055735756,43.6394630792646));
#172250=CARTESIAN_POINT('Ctrl Pts',(77.7272352903052,7.24600426098306,43.6472814578416));
#172251=CARTESIAN_POINT('Ctrl Pts',(77.6417639963485,7.33230720410671,43.6646959930862));
#172252=CARTESIAN_POINT('Ctrl Pts',(77.5945474634561,7.37905645851623,43.6743222202586));
#172253=CARTESIAN_POINT('Ctrl Pts',(77.4432997607954,7.52589357013387,43.7051688088887));
#172254=CARTESIAN_POINT('Ctrl Pts',(77.3376254047933,7.6241898842825,43.7267370479436));
#172255=CARTESIAN_POINT('Ctrl Pts',(77.0633341659678,7.86859514650933,43.7827008928775));
#172256=CARTESIAN_POINT('Ctrl Pts',(76.8919759487901,8.01138531900531,43.8176446406624));
#172257=CARTESIAN_POINT('Ctrl Pts',(76.2301027931177,8.52665885219056,43.9522653118987));
#172258=CARTESIAN_POINT('Ctrl Pts',(75.7110952982463,8.85899961456718,44.0570519771855));
#172259=CARTESIAN_POINT('Ctrl Pts',(75.0479580644837,9.20189918723911,44.1890145874175));
#172260=CARTESIAN_POINT('Ctrl Pts',(74.9293268917585,9.2602782148456,44.2125564061781));
#172261=CARTESIAN_POINT('Ctrl Pts',(74.7225091505826,9.3569854333983,44.2534841448613));
#172262=CARTESIAN_POINT('Ctrl Pts',(74.6348527110893,9.39643524604626,44.2707960936901));
#172263=CARTESIAN_POINT('Ctrl Pts',(74.4512566615219,9.47588217732843,44.3069850517531));
#172264=CARTESIAN_POINT('Ctrl Pts',(74.3552354874421,9.51565687875646,44.3258723855551));
#172265=CARTESIAN_POINT('Ctrl Pts',(74.0948032159035,9.61877876741822,44.3769972229015));
#172266=CARTESIAN_POINT('Ctrl Pts',(73.9293254733919,9.6792599627662,44.4093730810716));
#172267=CARTESIAN_POINT('Ctrl Pts',(73.4166713731958,9.85130809364957,44.5093858144987));
#172268=CARTESIAN_POINT('Ctrl Pts',(73.0649864042846,9.94813044846011,44.577587149333));
#172269=CARTESIAN_POINT('Ctrl Pts',(72.2261774860944,10.1299897403704,44.7398524944165));
#172270=CARTESIAN_POINT('Ctrl Pts',(71.7365088094433,10.1983438376698,44.8342561796209));
#172271=CARTESIAN_POINT('Ctrl Pts',(71.1135125218988,10.2381934697919,44.9551674741933));
#172272=CARTESIAN_POINT('Ctrl Pts',(70.9828739377346,10.2439495431846,44.9805682283276));
#172273=CARTESIAN_POINT('Ctrl Pts',(70.7909403808074,10.2485924268276,45.0179867540857));
#172274=CARTESIAN_POINT('Ctrl Pts',(70.7296964534421,10.2495040933913,45.0299415410962));
#172275=CARTESIAN_POINT('Ctrl Pts',(70.6184403884264,10.2501252936398,45.0516900179658));
#172276=CARTESIAN_POINT('Ctrl Pts',(70.5684310298726,10.2500246503311,45.0614777686095));
#172277=CARTESIAN_POINT('Ctrl Pts',(70.4488203392759,10.2488753040572,45.0849152377932));
#172278=CARTESIAN_POINT('Ctrl Pts',(70.3792271322961,10.2474704627822,45.0985737273884));
#172279=CARTESIAN_POINT('Ctrl Pts',(70.1214640977061,10.2395393724093,45.1492329203671));
#172280=CARTESIAN_POINT('Ctrl Pts',(69.9334926394964,10.2283665196997,45.1863137924143));
#172281=CARTESIAN_POINT('Ctrl Pts',(69.3958588721882,10.1809444913754,45.2926155751259));
#172282=CARTESIAN_POINT('Ctrl Pts',(69.0476403642592,10.1313857049403,45.3617557807614));
#172283=CARTESIAN_POINT('Ctrl Pts',(68.2421753444426,9.97252878900785,45.5217306327631));
#172284=CARTESIAN_POINT('Ctrl Pts',(67.7884573143866,9.84897258228748,45.611862846335));
#172285=CARTESIAN_POINT('Ctrl Pts',(67.1998728434787,9.64282427306771,45.7283974456558));
#172286=CARTESIAN_POINT('Ctrl Pts',(67.0560937525458,9.58869321103137,45.7568356997508));
#172287=CARTESIAN_POINT('Ctrl Pts',(66.8210884633804,9.49394458976434,45.803267894746));
#172288=CARTESIAN_POINT('Ctrl Pts',(66.7291438420976,9.4552584806206,45.8214215184769));
#172289=CARTESIAN_POINT('Ctrl Pts',(66.5475642482472,9.37562691060056,45.8572488022389));
#172290=CARTESIAN_POINT('Ctrl Pts',(66.457924625181,9.33472062605483,45.8749236873815));
#172291=CARTESIAN_POINT('Ctrl Pts',(66.2359053963485,9.22940140113565,45.9186750347101));
#172292=CARTESIAN_POINT('Ctrl Pts',(66.104291083856,9.16336293784568,45.9445877017524));
#172293=CARTESIAN_POINT('Ctrl Pts',(65.6060235529111,8.89940750163991,46.0426305356261));
#172294=CARTESIAN_POINT('Ctrl Pts',(65.2500760480114,8.68137953927731,46.1125299907108));
#172295=CARTESIAN_POINT('Ctrl Pts',(64.5185634190718,8.1679834078953,46.2566432754873));
#172296=CARTESIAN_POINT('Ctrl Pts',(64.1482245484443,7.86669262032007,46.3298943287175));
#172297=CARTESIAN_POINT('Ctrl Pts',(63.7342857131744,7.47797554740454,46.4131714854007));
#172298=CARTESIAN_POINT('Ctrl Pts',(63.6691090366818,7.41509738375306,46.4263298851424));
#172299=CARTESIAN_POINT('Ctrl Pts',(63.5685473570574,7.31543249169649,46.4467159541363));
#172300=CARTESIAN_POINT('Ctrl Pts',(63.5325875742219,7.27924878646794,46.4540230405205));
#172301=CARTESIAN_POINT('Ctrl Pts',(63.455161497815,7.20014972570824,46.4697966184252));
#172302=CARTESIAN_POINT('Ctrl Pts',(63.41379694177,7.15713487938176,46.4782491562529));
#172303=CARTESIAN_POINT('Ctrl Pts',(63.2995621216697,7.03621589125165,46.5016591393423));
#172304=CARTESIAN_POINT('Ctrl Pts',(63.2275291092484,6.95750854247805,46.5164981584575));
#172305=CARTESIAN_POINT('Ctrl Pts',(63.0620658426728,6.77087280472048,46.550745372892));
#172306=CARTESIAN_POINT('Ctrl Pts',(62.9696319172445,6.66206340482518,46.5700026055298));
#172307=CARTESIAN_POINT('Ctrl Pts',(62.6105961049359,6.22088612783867,46.6452295182885));
#172308=CARTESIAN_POINT('Ctrl Pts',(62.3624711536996,5.87353238193372,46.6981790684783));
#172309=CARTESIAN_POINT('Ctrl Pts',(62.1060842513098,5.46251119810423,46.7535972737332));
#172310=CARTESIAN_POINT('Ctrl Pts',(62.0760609759145,5.41346544106682,46.7600995648005));
#172311=CARTESIAN_POINT('Ctrl Pts',(61.8933508275054,5.10927361376937,46.7997454523949));
#172312=CARTESIAN_POINT('Ctrl Pts',(61.7512935358652,4.84765245666622,46.8308963519295));
#172313=CARTESIAN_POINT('Ctrl Pts',(61.566313278203,4.46867822573259,46.8718765570834));
#172314=CARTESIAN_POINT('Ctrl Pts',(61.5139492009717,4.35630335929961,46.8835334313065));
#172315=CARTESIAN_POINT('Ctrl Pts',(61.4245016956969,4.15494833510534,46.9035477964139));
#172316=CARTESIAN_POINT('Ctrl Pts',(61.3866207472589,4.06635466372642,46.912060032723));
#172317=CARTESIAN_POINT('Ctrl Pts',(61.3086361935644,3.87667471311965,46.9296643567785));
#172318=CARTESIAN_POINT('Ctrl Pts',(61.2688747724967,3.77545451536933,46.9386898284297));
#172319=CARTESIAN_POINT('Ctrl Pts',(61.1613788985319,3.48859620573651,46.9632407414657));
#172320=CARTESIAN_POINT('Ctrl Pts',(61.0973327171974,3.3015675145769,46.9780509811067));
#172321=CARTESIAN_POINT('Ctrl Pts',(60.9603164140632,2.86068557313158,47.0102439523115));
#172322=CARTESIAN_POINT('Ctrl Pts',(60.8915956994273,2.60560186705304,47.0268130095019));
#172323=CARTESIAN_POINT('Ctrl Pts',(60.7089553747825,1.80753641260781,47.0725950268692));
#172324=CARTESIAN_POINT('Ctrl Pts',(60.6286562534582,1.25756617858406,47.0955803210865));
#172325=CARTESIAN_POINT('Ctrl Pts',(60.5837428466699,0.564422640247255,
47.1155101252095));
#172326=CARTESIAN_POINT('Ctrl Pts',(60.577532758024,0.425075990803095,47.1190668737045));
#172327=CARTESIAN_POINT('Ctrl Pts',(60.5728429545518,0.232437560486106,
47.1233962230586));
#172328=CARTESIAN_POINT('Ctrl Pts',(60.5719577001284,0.179227946904613,
47.1245301965381));
#172329=CARTESIAN_POINT('Ctrl Pts',(60.5711076850732,0.0840102689892994,
47.1264512370528));
#172330=CARTESIAN_POINT('Ctrl Pts',(60.5709882801534,0.0420052607569114,
47.1272610361969));
#172331=CARTESIAN_POINT('Ctrl Pts',(60.5711245517966,-1.29611701639584E-15,
47.1280338710899));
#172332=CARTESIAN_POINT('Origin',(69.7358040552328,0.,40.0761166693274));
#172333=CARTESIAN_POINT('',(60.7795023650012,-6.55271312842658E-10,48.3098031747286));
#172334=CARTESIAN_POINT('Ctrl Pts',(60.571124584323,-1.00246535761108E-5,
47.128034055528));
#172335=CARTESIAN_POINT('Ctrl Pts',(60.5712148032041,-0.0278113824378972,
47.1285455556463));
#172336=CARTESIAN_POINT('Ctrl Pts',(60.5714169343916,-0.0556025639840617,
47.1290406821915));
#172337=CARTESIAN_POINT('Ctrl Pts',(60.5720858854301,-0.11480023329174,
47.1300604955834));
#172338=CARTESIAN_POINT('Ctrl Pts',(60.5725834899719,-0.146196177168539,
47.1305804830234));
#172339=CARTESIAN_POINT('Ctrl Pts',(60.575032242565,-0.266248040290342,
47.1324880221005));
#172340=CARTESIAN_POINT('Ctrl Pts',(60.5779789971853,-0.35488218316995,
47.133727828746));
#172341=CARTESIAN_POINT('Ctrl Pts',(60.6092552542877,-1.0334123568815,47.1418865635819));
#172342=CARTESIAN_POINT('Ctrl Pts',(60.6867863375073,-1.62004253220283,
47.1411617285872));
#172343=CARTESIAN_POINT('Ctrl Pts',(60.8874434000863,-2.53283045702649,
47.1257427289583));
#172344=CARTESIAN_POINT('Ctrl Pts',(60.9779031647833,-2.86492265784167,
47.117028961743));
#172345=CARTESIAN_POINT('Ctrl Pts',(61.1410732466115,-3.36487994114951,
47.0989433042988));
#172346=CARTESIAN_POINT('Ctrl Pts',(61.2020699062065,-3.53638546197852,
47.0918164663893));
#172347=CARTESIAN_POINT('Ctrl Pts',(61.3056812367078,-3.80515603437629,
47.0791682513928));
#172348=CARTESIAN_POINT('Ctrl Pts',(61.3453491786462,-3.90354199471231,
47.074217486293));
#172349=CARTESIAN_POINT('Ctrl Pts',(61.424291867263,-4.09101024679259,47.0641663919241));
#172350=CARTESIAN_POINT('Ctrl Pts',(61.4633272452909,-4.18018332693093,
47.0591122739339));
#172351=CARTESIAN_POINT('Ctrl Pts',(61.5585061688121,-4.38954657088156,
47.0465996654256));
#172352=CARTESIAN_POINT('Ctrl Pts',(61.6157067757008,-4.50922437742387,
47.0389355170984));
#172353=CARTESIAN_POINT('Ctrl Pts',(61.9586335262266,-5.19268799918991,
46.9922200214171));
#172354=CARTESIAN_POINT('Ctrl Pts',(62.2928722184951,-5.72993047556373,
46.943685630173));
#172355=CARTESIAN_POINT('Ctrl Pts',(62.8073668453159,-6.40877746633383,
46.8673143615842));
#172356=CARTESIAN_POINT('Ctrl Pts',(62.9465139892635,-6.58054681578012,
46.8465372175401));
#172357=CARTESIAN_POINT('Ctrl Pts',(63.1850727850178,-6.85627088397663,
46.8108665824421));
#172358=CARTESIAN_POINT('Ctrl Pts',(63.2813415000775,-6.96290790738683,
46.7964600198185));
#172359=CARTESIAN_POINT('Ctrl Pts',(63.4254277181341,-7.11588985339365,
46.7749196304762));
#172360=CARTESIAN_POINT('Ctrl Pts',(63.4715158877616,-7.16387366600094,
46.7680327961607));
#172361=CARTESIAN_POINT('Ctrl Pts',(63.556775656516,-7.25091744339383,46.7553035211773));
#172362=CARTESIAN_POINT('Ctrl Pts',(63.5958028082764,-7.2901171656847,46.7494812824883));
#172363=CARTESIAN_POINT('Ctrl Pts',(63.6927496964427,-7.3859189542384,46.7350275964303));
#172364=CARTESIAN_POINT('Ctrl Pts',(63.7510252740847,-7.44214793288821,
46.7263469290494));
#172365=CARTESIAN_POINT('Ctrl Pts',(63.9986631721268,-7.67545018964536,
46.6894726448285));
#172366=CARTESIAN_POINT('Ctrl Pts',(64.1940153141472,-7.845888334824,46.6604148077498));
#172367=CARTESIAN_POINT('Ctrl Pts',(64.7586916046057,-8.30178340996116,
46.5761579625035));
#172368=CARTESIAN_POINT('Ctrl Pts',(65.1412784408068,-8.56938334510254,
46.5187538767455));
#172369=CARTESIAN_POINT('Ctrl Pts',(65.6991825987615,-8.90493236734765,
46.4339531611846));
#172370=CARTESIAN_POINT('Ctrl Pts',(65.8603597593676,-8.9959511205643,46.4093400838637));
#172371=CARTESIAN_POINT('Ctrl Pts',(66.1584632334814,-9.15367217966799,
46.3635862445074));
#172372=CARTESIAN_POINT('Ctrl Pts',(66.2945944560027,-9.22180691583146,
46.3426079832871));
#172373=CARTESIAN_POINT('Ctrl Pts',(66.5224559358261,-9.32948465021821,
46.3073506625335));
#172374=CARTESIAN_POINT('Ctrl Pts',(66.6133489666176,-9.37079842131573,
46.2932499279432));
#172375=CARTESIAN_POINT('Ctrl Pts',(66.7961017713411,-9.45061390581593,
46.2648260300776));
#172376=CARTESIAN_POINT('Ctrl Pts',(66.8879490377325,-9.48911710502249,
46.250504967349));
#172377=CARTESIAN_POINT('Ctrl Pts',(67.1198544806631,-9.58231688646064,
46.2142588005508));
#172378=CARTESIAN_POINT('Ctrl Pts',(67.2605746935562,-9.63524219942648,
46.192185963904));
#172379=CARTESIAN_POINT('Ctrl Pts',(68.0376430613358,-9.90778602276534,
46.0699100043904));
#172380=CARTESIAN_POINT('Ctrl Pts',(68.6929573644766,-10.0660067363506,
45.9652586327518));
#172381=CARTESIAN_POINT('Ctrl Pts',(69.5808601216022,-10.1877346382761,
45.8236671205603));
#172382=CARTESIAN_POINT('Ctrl Pts',(69.8037204760739,-10.2106946458299,
45.7881576587774));
#172383=CARTESIAN_POINT('Ctrl Pts',(70.1711086181769,-10.2361102646359,
45.7298248138721));
#172384=CARTESIAN_POINT('Ctrl Pts',(70.3152502964532,-10.2429519182616,
45.7069903189383));
#172385=CARTESIAN_POINT('Ctrl Pts',(70.523230246374,-10.2483170465695,45.6741582330827));
#172386=CARTESIAN_POINT('Ctrl Pts',(70.5869773276538,-10.2493518294266,
45.6641106521459));
#172387=CARTESIAN_POINT('Ctrl Pts',(70.7008828351484,-10.2501118898927,
45.6461897745921));
#172388=CARTESIAN_POINT('Ctrl Pts',(70.7510357683067,-10.2500694791727,
45.6383107340837));
#172389=CARTESIAN_POINT('Ctrl Pts',(70.8673239408612,-10.2490969264566,
45.6200684001011));
#172390=CARTESIAN_POINT('Ctrl Pts',(70.933455253354,-10.2478882161687,45.6097137388107));
#172391=CARTESIAN_POINT('Ctrl Pts',(71.1484918722356,-10.2418254652421,
45.5760992976301));
#172392=CARTESIAN_POINT('Ctrl Pts',(71.2973149936773,-10.2343026359673,
45.5529215986974));
#172393=CARTESIAN_POINT('Ctrl Pts',(72.2558405027365,-10.1643783646006,
45.4040288101855));
#172394=CARTESIAN_POINT('Ctrl Pts',(73.0560702454888,-10.0069883564334,
45.2812576116335));
#172395=CARTESIAN_POINT('Ctrl Pts',(74.0085779719508,-9.69602214883924,
45.1339341707801));
#172396=CARTESIAN_POINT('Ctrl Pts',(74.1865130200952,-9.63232441115741,
45.1063732880928));
#172397=CARTESIAN_POINT('Ctrl Pts',(74.4619826268559,-9.52485547428383,
45.0636344637706));
#172398=CARTESIAN_POINT('Ctrl Pts',(74.560772876472,-9.48449120277262,45.0482929323982));
#172399=CARTESIAN_POINT('Ctrl Pts',(74.7472193492221,-9.4048265966382,45.0193127493898));
#172400=CARTESIAN_POINT('Ctrl Pts',(74.8349897316404,-9.36582906736572,
45.0056590074803));
#172401=CARTESIAN_POINT('Ctrl Pts',(75.0363308297293,-9.27289785179124,
44.9743147558886));
#172402=CARTESIAN_POINT('Ctrl Pts',(75.1494836782866,-9.21807801207909,
44.9566820144759));
#172403=CARTESIAN_POINT('Ctrl Pts',(75.5449595466918,-9.01725522478599,
44.8950087976443));
#172404=CARTESIAN_POINT('Ctrl Pts',(75.8214737807829,-8.85998224334017,
44.8517979763908));
#172405=CARTESIAN_POINT('Ctrl Pts',(76.4698789015359,-8.44954028808022,
44.7505688507741));
#172406=CARTESIAN_POINT('Ctrl Pts',(76.8333495250869,-8.1840296067559,44.6938965114066));
#172407=CARTESIAN_POINT('Ctrl Pts',(77.2905427321294,-7.80112343946986,
44.6235401114811));
#172408=CARTESIAN_POINT('Ctrl Pts',(77.4007012998642,-7.70475351910916,
44.6066682609185));
#172409=CARTESIAN_POINT('Ctrl Pts',(77.5890830040765,-7.532664726504,44.5780052686678));
#172410=CARTESIAN_POINT('Ctrl Pts',(77.6682231850741,-7.45801752128144,
44.5660249995239));
#172411=CARTESIAN_POINT('Ctrl Pts',(77.7893504880082,-7.34006242190119,
44.5478036059522));
#172412=CARTESIAN_POINT('Ctrl Pts',(77.8321568309724,-7.29763479756387,
44.541387207907));
#172413=CARTESIAN_POINT('Ctrl Pts',(77.9154656299549,-7.21359399412603,
44.5289494435067));
#172414=CARTESIAN_POINT('Ctrl Pts',(77.9559932322748,-7.17201005074573,
44.5229226526456));
#172415=CARTESIAN_POINT('Ctrl Pts',(78.0636894564502,-7.05961310135321,
44.5069676192112));
#172416=CARTESIAN_POINT('Ctrl Pts',(78.1302143806874,-6.98817199927902,
44.4971760707883));
#172417=CARTESIAN_POINT('Ctrl Pts',(78.4461193230978,-6.6390657861382,44.450957322891));
#172418=CARTESIAN_POINT('Ctrl Pts',(78.6814420171409,-6.34868604587716,
44.4173747315025));
#172419=CARTESIAN_POINT('Ctrl Pts',(79.1149602139214,-5.74976439653213,
44.3566175617764));
#172420=CARTESIAN_POINT('Ctrl Pts',(79.3135402069697,-5.44217813132996,
44.3293619421705));
#172421=CARTESIAN_POINT('Ctrl Pts',(79.6129935773734,-4.91917326217556,
44.2889637400265));
#172422=CARTESIAN_POINT('Ctrl Pts',(79.7234985966133,-4.70977652232714,
44.2742531957818));
#172423=CARTESIAN_POINT('Ctrl Pts',(79.8768559283336,-4.39325204051632,
44.2541179920027));
#172424=CARTESIAN_POINT('Ctrl Pts',(79.9252539433013,-4.28895629647708,
44.2478114452241));
#172425=CARTESIAN_POINT('Ctrl Pts',(80.0108619709941,-4.09610496024231,
44.2367467145892));
#172426=CARTESIAN_POINT('Ctrl Pts',(80.0485961480015,-4.00780112245531,
44.2319053178921));
#172427=CARTESIAN_POINT('Ctrl Pts',(80.1299350222782,-3.80986632484421,
44.2215527338582));
#172428=CARTESIAN_POINT('Ctrl Pts',(80.1729064929177,-3.6999847728598,44.216141788707));
#172429=CARTESIAN_POINT('Ctrl Pts',(80.3019749275425,-3.3525371606697,44.2000886228256));
#172430=CARTESIAN_POINT('Ctrl Pts',(80.3812706981692,-3.11249779706675,
44.1905278482389));
#172431=CARTESIAN_POINT('Ctrl Pts',(80.4905516205075,-2.73598656892681,
44.1779459418813));
#172432=CARTESIAN_POINT('Ctrl Pts',(80.526681023091,-2.60143807971074,44.1739177365803));
#172433=CARTESIAN_POINT('Ctrl Pts',(80.6787136901535,-1.98605398938358,
44.1576652541872));
#172434=CARTESIAN_POINT('Ctrl Pts',(80.7628924573915,-1.49793652580564,
44.1507276544172));
#172435=CARTESIAN_POINT('Ctrl Pts',(80.827446997135,-0.852294322658078,
44.1502701775411));
#172436=CARTESIAN_POINT('Ctrl Pts',(80.839380454511,-0.698605869535761,
44.1508038580746));
#172437=CARTESIAN_POINT('Ctrl Pts',(80.8541193166427,-0.432663225378754,
44.1528885103362));
#172438=CARTESIAN_POINT('Ctrl Pts',(80.858523369788,-0.320522586653946,
44.1541233691532));
#172439=CARTESIAN_POINT('Ctrl Pts',(80.8624785355301,-0.149774858189465,
44.1565639634004));
#172440=CARTESIAN_POINT('Ctrl Pts',(80.8633430127721,-0.0912030828018238,
44.1575014640504));
#172441=CARTESIAN_POINT('Ctrl Pts',(80.8640419151073,0.0186491112984646,
44.1594513223032));
#172442=CARTESIAN_POINT('Ctrl Pts',(80.8639912768604,0.0699268206422241,
44.1604400821254));
#172443=CARTESIAN_POINT('Ctrl Pts',(80.8629174979052,0.198673804398144,
44.1631179089744));
#172444=CARTESIAN_POINT('Ctrl Pts',(80.861410638048,0.276133945101377,44.1649063761142));
#172445=CARTESIAN_POINT('Ctrl Pts',(80.8516318630623,0.595906695800077,
44.1730070544069));
#172446=CARTESIAN_POINT('Ctrl Pts',(80.8357897122155,0.83787206041321,44.1808377488813));
#172447=CARTESIAN_POINT('Ctrl Pts',(80.7567641370625,1.62332390246877,44.2114772410717));
#172448=CARTESIAN_POINT('Ctrl Pts',(80.6592196732919,2.16215553067159,44.2406474350728));
#172449=CARTESIAN_POINT('Ctrl Pts',(80.4675369104719,2.88777777805181,44.2902009737457));
#172450=CARTESIAN_POINT('Ctrl Pts',(80.4095582262334,3.08356688755194,44.3046436770043));
#172451=CARTESIAN_POINT('Ctrl Pts',(80.2941959382061,3.43453529807525,44.3324615995049));
#172452=CARTESIAN_POINT('Ctrl Pts',(80.2388034243116,3.59031997843296,44.3455156265546));
#172453=CARTESIAN_POINT('Ctrl Pts',(80.1429378206459,3.84066897455588,44.3676461927745));
#172454=CARTESIAN_POINT('Ctrl Pts',(80.1047434918303,3.93610510796475,44.3763602786074));
#172455=CARTESIAN_POINT('Ctrl Pts',(80.0276132484011,4.12075847331712,44.3937658733821));
#172456=CARTESIAN_POINT('Ctrl Pts',(79.9888269187536,4.21002848816928,44.4024333955731));
#172457=CARTESIAN_POINT('Ctrl Pts',(79.9002264450712,4.40627470334876,44.422053521333));
#172458=CARTESIAN_POINT('Ctrl Pts',(79.8498283935279,4.51296253986985,44.4330984400104));
#172459=CARTESIAN_POINT('Ctrl Pts',(79.5126187776257,5.19606077186552,44.5063059973374));
#172460=CARTESIAN_POINT('Ctrl Pts',(79.1742821913063,5.74451787765544,44.5765677906907));
#172461=CARTESIAN_POINT('Ctrl Pts',(78.6583567644974,6.42757934270093,44.6820229833376));
#172462=CARTESIAN_POINT('Ctrl Pts',(78.5240629578254,6.594202497137,44.7093601643086));
#172463=CARTESIAN_POINT('Ctrl Pts',(78.2931446207121,6.86294764063671,44.7563219597435));
#172464=CARTESIAN_POINT('Ctrl Pts',(78.1994176618604,6.96756726847844,44.7753722742591));
#172465=CARTESIAN_POINT('Ctrl Pts',(78.0586718524208,7.11827615544848,44.804001183889));
#172466=CARTESIAN_POINT('Ctrl Pts',(78.0132891658441,7.16593536585266,44.8132356381705));
#172467=CARTESIAN_POINT('Ctrl Pts',(77.9290299288515,7.2527187679944,44.8303916092196));
#172468=CARTESIAN_POINT('Ctrl Pts',(77.8902890125125,7.29197574467653,44.838284212732));
#172469=CARTESIAN_POINT('Ctrl Pts',(77.7936066872988,7.38836303068299,44.8579904287636));
#172470=CARTESIAN_POINT('Ctrl Pts',(77.7353024820702,7.44510788266909,44.8698819765888));
#172471=CARTESIAN_POINT('Ctrl Pts',(77.4816047554304,7.68614265782594,44.9216393160743));
#172472=CARTESIAN_POINT('Ctrl Pts',(77.27975271499,7.86318703315804,44.962852134825));
#172473=CARTESIAN_POINT('Ctrl Pts',(76.7174670584843,8.31798736759351,45.0773622019873));
#172474=CARTESIAN_POINT('Ctrl Pts',(76.3451364867638,8.5794828862537,45.1528650960693));
#172475=CARTESIAN_POINT('Ctrl Pts',(75.8005420867777,8.90905104515565,45.2622380173261));
#172476=CARTESIAN_POINT('Ctrl Pts',(75.641880387846,8.99922098860143,45.2939889082202));
#172477=CARTESIAN_POINT('Ctrl Pts',(75.3480817719023,9.15568800037619,45.3525535375993));
#172478=CARTESIAN_POINT('Ctrl Pts',(75.2137265059827,9.22338111647456,45.3792512183673));
#172479=CARTESIAN_POINT('Ctrl Pts',(74.9884325573904,9.33056232199089,45.423876488021));
#172480=CARTESIAN_POINT('Ctrl Pts',(74.8983263053219,9.37179022542599,45.4416874644431));
#172481=CARTESIAN_POINT('Ctrl Pts',(74.7168568222614,9.45156372102435,45.4774850288662));
#172482=CARTESIAN_POINT('Ctrl Pts',(74.625502504406,9.49010249204443,45.4954697936684));
#172483=CARTESIAN_POINT('Ctrl Pts',(74.3942440458679,9.58360991023536,45.5409093207623));
#172484=CARTESIAN_POINT('Ctrl Pts',(74.2536557864928,9.63677584874654,45.5684531735549));
#172485=CARTESIAN_POINT('Ctrl Pts',(73.5959464807408,9.86857373579511,45.6969766515089));
#172486=CARTESIAN_POINT('Ctrl Pts',(73.0661039440133,10.0073371192394,45.7995116645105));
#172487=CARTESIAN_POINT('Ctrl Pts',(72.2301899963443,10.1537701536665,45.961048660037));
#172488=CARTESIAN_POINT('Ctrl Pts',(71.9304177825758,10.192238742476,46.0189475407777));
#172489=CARTESIAN_POINT('Ctrl Pts',(71.5096073395762,10.2267524012556,46.100496468681));
#172490=CARTESIAN_POINT('Ctrl Pts',(71.3896196493146,10.2343929861575,46.1237802463463));
#172491=CARTESIAN_POINT('Ctrl Pts',(71.1763879444469,10.2440694253526,46.1652427215803));
#172492=CARTESIAN_POINT('Ctrl Pts',(71.0831928121456,10.2469775845504,46.183392984091));
#172493=CARTESIAN_POINT('Ctrl Pts',(70.9358614690237,10.2494883115732,46.2121444938566));
#172494=CARTESIAN_POINT('Ctrl Pts',(70.8817404909017,10.2499657004367,46.2227184841259));
#172495=CARTESIAN_POINT('Ctrl Pts',(70.7747509104128,10.2500299837307,46.2436493857298));
#172496=CARTESIAN_POINT('Ctrl Pts',(70.7218840565727,10.2496371808114,46.2540054154293));
#172497=CARTESIAN_POINT('Ctrl Pts',(70.5819074259259,10.2474728267927,46.2814574155939));
#172498=CARTESIAN_POINT('Ctrl Pts',(70.4948167023751,10.2449727678598,46.2985704526487));
#172499=CARTESIAN_POINT('Ctrl Pts',(69.8631186230343,10.2184660167189,46.4228952904468));
#172500=CARTESIAN_POINT('Ctrl Pts',(69.321364176781,10.1505355790661,46.5305412933948));
#172501=CARTESIAN_POINT('Ctrl Pts',(68.4015272723725,9.95691999091736,46.7132424322025));
#172502=CARTESIAN_POINT('Ctrl Pts',(68.0203930196076,9.85255851926371,46.7889333508227));
#172503=CARTESIAN_POINT('Ctrl Pts',(67.4847246744987,9.67088274177677,46.8950349661311));
#172504=CARTESIAN_POINT('Ctrl Pts',(67.3246142255615,9.61194108129113,46.9267142040233));
#172505=CARTESIAN_POINT('Ctrl Pts',(67.0704531729611,9.51087667780468,46.9769422299198));
#172506=CARTESIAN_POINT('Ctrl Pts',(66.9754389415886,9.47137853925105,46.9957056332596));
#172507=CARTESIAN_POINT('Ctrl Pts',(66.7924881954681,9.39197736983452,47.0318096220627));
#172508=CARTESIAN_POINT('Ctrl Pts',(66.7044881493277,9.352255994829,47.0491643235425));
#172509=CARTESIAN_POINT('Ctrl Pts',(66.4947638623784,9.25389988261604,47.0905001495394));
#172510=CARTESIAN_POINT('Ctrl Pts',(66.3736070676214,9.19404974525078,47.1143595211593));
#172511=CARTESIAN_POINT('Ctrl Pts',(65.7258228253963,8.85752883569113,47.2418509639892));
#172512=CARTESIAN_POINT('Ctrl Pts',(65.2227263756756,8.53633246810886,47.3405117912805));
#172513=CARTESIAN_POINT('Ctrl Pts',(64.5675028067047,8.03073720708396,47.470078292076));
#172514=CARTESIAN_POINT('Ctrl Pts',(64.3893799651125,7.88323492718028,47.5054349807229));
#172515=CARTESIAN_POINT('Ctrl Pts',(64.106046092681,7.63166795566416,47.5620681211979));
#172516=CARTESIAN_POINT('Ctrl Pts',(63.9978167774939,7.53123808994899,47.5838019397277));
#172517=CARTESIAN_POINT('Ctrl Pts',(63.8437240938318,7.38181862714292,47.614938242529));
#172518=CARTESIAN_POINT('Ctrl Pts',(63.7961073795064,7.33471712411558,47.6245876173148));
#172519=CARTESIAN_POINT('Ctrl Pts',(63.7103039766681,7.24813463892236,47.6420318291885));
#172520=CARTESIAN_POINT('Ctrl Pts',(63.671966467166,7.20881216751893,47.6498475097459));
#172521=CARTESIAN_POINT('Ctrl Pts',(63.5790330997845,7.11192197836666,47.668844864131));
#172522=CARTESIAN_POINT('Ctrl Pts',(63.5247863902146,7.05401519000976,47.6799777541437));
#172523=CARTESIAN_POINT('Ctrl Pts',(63.3065223651301,6.81545795282461,47.7249355548842));
#172524=CARTESIAN_POINT('Ctrl Pts',(63.1483043268279,6.62945212943957,47.7579092172451));
#172525=CARTESIAN_POINT('Ctrl Pts',(62.700039465136,6.06223290556525,47.8521989594965));
#172526=CARTESIAN_POINT('Ctrl Pts',(62.4297615124453,5.66570545217994,47.9102024273087));
#172527=CARTESIAN_POINT('Ctrl Pts',(62.0934208371174,5.0891486175109,47.9833990808422));
#172528=CARTESIAN_POINT('Ctrl Pts',(62.0033051966152,4.92446444490717,48.0031395705416));
#172529=CARTESIAN_POINT('Ctrl Pts',(61.8474786200503,4.62021065602418,48.0374935143791));
#172530=CARTESIAN_POINT('Ctrl Pts',(61.7803114853395,4.48148172601328,48.0523867790885));
#172531=CARTESIAN_POINT('Ctrl Pts',(61.674453929789,4.24973781162177,48.076001485579));
#172532=CARTESIAN_POINT('Ctrl Pts',(61.6339834657458,4.15759935959977,48.0850682207215));
#172533=CARTESIAN_POINT('Ctrl Pts',(61.5559721933895,3.97270128857706,48.1026252343321));
#172534=CARTESIAN_POINT('Ctrl Pts',(61.5184190479317,3.87995913646557,48.1111177785738));
#172535=CARTESIAN_POINT('Ctrl Pts',(61.4278217225578,3.64653817106006,48.1317147872399));
#172536=CARTESIAN_POINT('Ctrl Pts',(61.3764764397989,3.50519678930873,48.143489395866));
#172537=CARTESIAN_POINT('Ctrl Pts',(61.1384690317617,2.80271719503812,48.1986344324567));
#172538=CARTESIAN_POINT('Ctrl Pts',(60.9967884040585,2.2268672065966,48.2332713097903));
#172539=CARTESIAN_POINT('Ctrl Pts',(60.8607433709496,1.36008477544737,48.2716507968488));
#172540=CARTESIAN_POINT('Ctrl Pts',(60.8281471100261,1.07670858810491,48.2820955947034));
#172541=CARTESIAN_POINT('Ctrl Pts',(60.7949289875252,0.624213451717764,
48.2957313806341));
#172542=CARTESIAN_POINT('Ctrl Pts',(60.7866872932901,0.455842228828194,
48.3001405576672));
#172543=CARTESIAN_POINT('Ctrl Pts',(60.7808939206339,0.219462490995435,
48.3054587822185));
#172544=CARTESIAN_POINT('Ctrl Pts',(60.7798976545732,0.151577621009194,
48.3068853995553));
#172545=CARTESIAN_POINT('Ctrl Pts',(60.7794341281953,0.0557908786371534,
48.3087604010123));
#172546=CARTESIAN_POINT('Ctrl Pts',(60.779411867806,0.0278954436961792,
48.3092899396518));
#172547=CARTESIAN_POINT('Ctrl Pts',(60.7795023650012,-1.31054137042235E-9,
48.3098031747286));
#172548=CARTESIAN_POINT('',(60.7957027539178,5.63053972823762E-10,48.4016801458623));
#172549=CARTESIAN_POINT('',(59.6415245868576,-1.25526296912604E-15,41.8560104904131));
#172550=CARTESIAN_POINT('Ctrl Pts',(60.7957027539178,1.12610920091049E-9,
48.4016801458622));
#172551=CARTESIAN_POINT('Ctrl Pts',(60.7956407021154,0.0191272543263107,
48.4013282325916));
#172552=CARTESIAN_POINT('Ctrl Pts',(60.7956310882385,0.0382545525903811,
48.4009653897912));
#172553=CARTESIAN_POINT('Ctrl Pts',(60.7958141432303,0.119992421931868,
48.3993683697433));
#172554=CARTESIAN_POINT('Ctrl Pts',(60.7965163606537,0.182598288115929,
48.3980286631963));
#172555=CARTESIAN_POINT('Ctrl Pts',(60.8004959192312,0.379594606971077,
48.3934526272087));
#172556=CARTESIAN_POINT('Ctrl Pts',(60.8058029680528,0.513920459702991,
48.3898042296417));
#172557=CARTESIAN_POINT('Ctrl Pts',(60.8431551615082,1.14837467604115,48.3701598674042));
#172558=CARTESIAN_POINT('Ctrl Pts',(60.9086010446192,1.64565792010428,48.3476930150286));
#172559=CARTESIAN_POINT('Ctrl Pts',(61.0834588810541,2.49413586098243,48.2983014301159));
#172560=CARTESIAN_POINT('Ctrl Pts',(61.1761499579601,2.84798882452612,48.274236671391));
#172561=CARTESIAN_POINT('Ctrl Pts',(61.3423766118459,3.36822335352085,48.2338091552142));
#172562=CARTESIAN_POINT('Ctrl Pts',(61.4019159928038,3.53894144694612,48.2196993707237));
#172563=CARTESIAN_POINT('Ctrl Pts',(61.5033130501057,3.80679120184683,48.19621878482));
#172564=CARTESIAN_POINT('Ctrl Pts',(61.5422425634555,3.90503077212232,48.1873138850712));
#172565=CARTESIAN_POINT('Ctrl Pts',(61.619850380846,4.09239573051365,48.1697632677733));
#172566=CARTESIAN_POINT('Ctrl Pts',(61.6582935509874,4.18160956398272,48.161155106083));
#172567=CARTESIAN_POINT('Ctrl Pts',(61.7522180430712,4.39134505081754,48.1403163522377));
#172568=CARTESIAN_POINT('Ctrl Pts',(61.8087746987146,4.51134859732828,48.1279156262983));
#172569=CARTESIAN_POINT('Ctrl Pts',(62.0562625820615,5.0111248034433,48.074221795361));
#172570=CARTESIAN_POINT('Ctrl Pts',(62.2682268076956,5.37963653237417,48.0295943522921));
#172571=CARTESIAN_POINT('Ctrl Pts',(62.7006251459201,6.03367683168163,47.9401421565941));
#172572=CARTESIAN_POINT('Ctrl Pts',(62.9145602433688,6.32283840416465,47.8964375255591));
#172573=CARTESIAN_POINT('Ctrl Pts',(63.2271517103667,6.70177190310662,47.8328093486643));
#172574=CARTESIAN_POINT('Ctrl Pts',(63.3131788514659,6.80201893769789,47.8153188273904));
#172575=CARTESIAN_POINT('Ctrl Pts',(63.4683178614429,6.9758448396921,47.7837759384149));
#172576=CARTESIAN_POINT('Ctrl Pts',(63.5366358111993,7.05013661455441,47.7698851748001));
#172577=CARTESIAN_POINT('Ctrl Pts',(63.6462902192209,7.16587563302743,47.7475738291046));
#172578=CARTESIAN_POINT('Ctrl Pts',(63.6869136656239,7.20801822301824,47.7393048586609));
#172579=CARTESIAN_POINT('Ctrl Pts',(63.7641238605713,7.28674374510451,47.7235786997223));
#172580=CARTESIAN_POINT('Ctrl Pts',(63.8006322275545,7.32340423822185,47.7161386550899));
#172581=CARTESIAN_POINT('Ctrl Pts',(63.9049076078787,7.42652561564756,47.6948803313079));
#172582=CARTESIAN_POINT('Ctrl Pts',(63.9733149022665,7.4923030583153,47.6809248867538));
#172583=CARTESIAN_POINT('Ctrl Pts',(64.3640529058159,7.85759510535715,47.6011986993135));
#172584=CARTESIAN_POINT('Ctrl Pts',(64.7043143139839,8.1364320630722,47.5317394437224));
#172585=CARTESIAN_POINT('Ctrl Pts',(65.4373550479627,8.66082627983858,47.3831787401561));
#172586=CARTESIAN_POINT('Ctrl Pts',(65.8311129601765,8.90321252224248,47.3039413422658));
#172587=CARTESIAN_POINT('Ctrl Pts',(66.3636434756009,9.18208987898382,47.1978919938694));
#172588=CARTESIAN_POINT('Ctrl Pts',(66.4887097590223,9.24426954336362,47.1730588781052));
#172589=CARTESIAN_POINT('Ctrl Pts',(66.7030038505289,9.3452446399822,47.1306342748845));
#172590=CARTESIAN_POINT('Ctrl Pts',(66.7915826926268,9.38540632480728,47.1131334825956));
#172591=CARTESIAN_POINT('Ctrl Pts',(66.9738078620823,9.46482588748011,47.0772021479379));
#172592=CARTESIAN_POINT('Ctrl Pts',(67.0674945295657,9.50396062911089,47.0587667980213));
#172593=CARTESIAN_POINT('Ctrl Pts',(67.3133700258608,9.6022697012904,47.0104791394805));
#172594=CARTESIAN_POINT('Ctrl Pts',(67.466427738063,9.6591312259943,46.9805139053764));
#172595=CARTESIAN_POINT('Ctrl Pts',(68.2370084144984,9.92396536405127,46.8300649497402));
#172596=CARTESIAN_POINT('Ctrl Pts',(68.8721621277378,10.0743849098331,46.7074752020394));
#172597=CARTESIAN_POINT('Ctrl Pts',(69.7316861643122,10.1902689570851,46.5413312233425));
#172598=CARTESIAN_POINT('Ctrl Pts',(69.9471387215376,10.2121438629284,46.4996529095671));
#172599=CARTESIAN_POINT('Ctrl Pts',(70.3035773732664,10.2365435675069,46.4305030817386));
#172600=CARTESIAN_POINT('Ctrl Pts',(70.4442341038064,10.2431563971155,46.4031643516186));
#172601=CARTESIAN_POINT('Ctrl Pts',(70.6478754054477,10.2483724969894,46.3634708957887));
#172602=CARTESIAN_POINT('Ctrl Pts',(70.710795239774,10.2493826647817,46.3511910729874));
#172603=CARTESIAN_POINT('Ctrl Pts',(70.8235652607529,10.2501154181836,46.3291497587947));
#172604=CARTESIAN_POINT('Ctrl Pts',(70.8734123378434,10.2500619082221,46.3193952783228));
#172605=CARTESIAN_POINT('Ctrl Pts',(70.9894350708341,10.2490588628604,46.2966641919293));
#172606=CARTESIAN_POINT('Ctrl Pts',(71.0556039137051,10.2478214124625,46.2836805737815));
#172607=CARTESIAN_POINT('Ctrl Pts',(71.2725712001932,10.2415810330529,46.2410504157295));
#172608=CARTESIAN_POINT('Ctrl Pts',(71.4232583116735,10.2337865047158,46.2113530303485));
#172609=CARTESIAN_POINT('Ctrl Pts',(72.3746796013367,10.1626722109809,46.0234534774516));
#172610=CARTESIAN_POINT('Ctrl Pts',(73.1654907719064,10.0052509963959,45.8657602557628));
#172611=CARTESIAN_POINT('Ctrl Pts',(74.1073249453324,9.69512549840155,45.67914149771));
#172612=CARTESIAN_POINT('Ctrl Pts',(74.2833350222481,9.63160437773884,45.644306086122));
#172613=CARTESIAN_POINT('Ctrl Pts',(74.5560861964528,9.52437557358169,45.5903945680753));
#172614=CARTESIAN_POINT('Ctrl Pts',(74.6540525278367,9.48404392001777,45.5710451142434));
#172615=CARTESIAN_POINT('Ctrl Pts',(74.8390775828875,9.40439477664596,45.534526891957));
#172616=CARTESIAN_POINT('Ctrl Pts',(74.9262470416164,9.36537583794669,45.5173336333379));
#172617=CARTESIAN_POINT('Ctrl Pts',(75.1263953366559,9.27231057064868,45.4778798904959));
#172618=CARTESIAN_POINT('Ctrl Pts',(75.2389583300217,9.2173708539392,45.4557087705101));
#172619=CARTESIAN_POINT('Ctrl Pts',(75.6386962047256,9.01286644033033,45.3770207602173));
#172620=CARTESIAN_POINT('Ctrl Pts',(75.9197933067054,8.85138375494903,45.3217815902134));
#172621=CARTESIAN_POINT('Ctrl Pts',(76.5636429013016,8.43873533544804,45.195146427409));
#172622=CARTESIAN_POINT('Ctrl Pts',(76.918847927094,8.17661833087698,45.1252023031759));
#172623=CARTESIAN_POINT('Ctrl Pts',(77.3665955832659,7.79833137928525,45.0361197754086));
#172624=CARTESIAN_POINT('Ctrl Pts',(77.4751702165876,7.70251587293689,45.0144379332026));
#172625=CARTESIAN_POINT('Ctrl Pts',(77.6609424390612,7.53131297011153,44.9771509681051));
#172626=CARTESIAN_POINT('Ctrl Pts',(77.73905120902,7.45697907637112,44.9614122133987));
#172627=CARTESIAN_POINT('Ctrl Pts',(77.8586895954159,7.33940908681387,44.9371902559852));
#172628=CARTESIAN_POINT('Ctrl Pts',(77.9010397445653,7.29704328186987,44.928592871904));
#172629=CARTESIAN_POINT('Ctrl Pts',(77.983558384167,7.21301049474357,44.9117909136498));
#172630=CARTESIAN_POINT('Ctrl Pts',(78.023750330805,7.17137067001636,44.9035831216388));
#172631=CARTESIAN_POINT('Ctrl Pts',(78.1307082735172,7.05863650086592,44.8816796267686));
#172632=CARTESIAN_POINT('Ctrl Pts',(78.1968156176301,6.98690742133993,44.8680766381385));
#172633=CARTESIAN_POINT('Ctrl Pts',(78.4928853110067,6.65618915672465,44.8068871295681));
#172634=CARTESIAN_POINT('Ctrl Pts',(78.7106709243835,6.38627106067666,44.7611327084919));
#172635=CARTESIAN_POINT('Ctrl Pts',(79.1378138970357,5.79776604854028,44.6703309407971));
#172636=CARTESIAN_POINT('Ctrl Pts',(79.3440141469304,5.47745183160361,44.6258493945515));
#172637=CARTESIAN_POINT('Ctrl Pts',(79.589169016565,5.04556607541324,44.5723515634568));
#172638=CARTESIAN_POINT('Ctrl Pts',(79.6445452754241,4.94405802254751,44.5602187527157));
#172639=CARTESIAN_POINT('Ctrl Pts',(79.777269572704,4.69069679162793,44.5310239019012));
#172640=CARTESIAN_POINT('Ctrl Pts',(79.8525993070769,4.53778182874249,44.5143498814705));
#172641=CARTESIAN_POINT('Ctrl Pts',(79.967579539728,4.28900376493974,44.4887321738162));
#172642=CARTESIAN_POINT('Ctrl Pts',(80.0096189256019,4.19432912719339,44.4793252236839));
#172643=CARTESIAN_POINT('Ctrl Pts',(80.0882227485604,4.00987807881692,44.4616551540784));
#172644=CARTESIAN_POINT('Ctrl Pts',(80.1249614132303,3.92019121743338,44.4533583100141));
#172645=CARTESIAN_POINT('Ctrl Pts',(80.2107503757952,3.70207041534065,44.4338871232293));
#172646=CARTESIAN_POINT('Ctrl Pts',(80.2585199403275,3.57313125421282,44.4229615588669));
#172647=CARTESIAN_POINT('Ctrl Pts',(80.4581007480095,2.99961265964152,44.3769045866386));
#172648=CARTESIAN_POINT('Ctrl Pts',(80.5822739415818,2.5456011955061,44.3471333409612));
#172649=CARTESIAN_POINT('Ctrl Pts',(80.7528314314767,1.69989962469362,44.3028742635563));
#172650=CARTESIAN_POINT('Ctrl Pts',(80.8085692791001,1.31109515934199,44.286697083169));
#172651=CARTESIAN_POINT('Ctrl Pts',(80.8540160308513,0.781627644295828,
44.2696724388824));
#172652=CARTESIAN_POINT('Ctrl Pts',(80.8631120487898,0.643072813701096,
44.2656755941091));
#172653=CARTESIAN_POINT('Ctrl Pts',(80.874153401148,0.400364665669781,44.2594349753772));
#172654=CARTESIAN_POINT('Ctrl Pts',(80.8773178009215,0.29629222971149,44.2570031128034));
#172655=CARTESIAN_POINT('Ctrl Pts',(80.8797853678576,0.135202963460496,
44.2536006461113));
#172656=CARTESIAN_POINT('Ctrl Pts',(80.8801879312855,0.0782135254226426,
44.2524669349703));
#172657=CARTESIAN_POINT('Ctrl Pts',(80.8800578296401,-0.030741306703425,
44.2504299779556));
#172658=CARTESIAN_POINT('Ctrl Pts',(80.8796044925397,-0.0827043997496042,
44.2495150116257));
#172659=CARTESIAN_POINT('Ctrl Pts',(80.8774342689301,-0.216246525200686,
44.2473114193674));
#172660=CARTESIAN_POINT('Ctrl Pts',(80.8751443945932,-0.297814272844059,
44.2461073780376));
#172661=CARTESIAN_POINT('Ctrl Pts',(80.859229190897,-0.696762037044488,
44.2409337106242));
#172662=CARTESIAN_POINT('Ctrl Pts',(80.831984558409,-1.0134545438031,44.2390474765423));
#172663=CARTESIAN_POINT('Ctrl Pts',(80.7452105349251,-1.66884695902908,
44.2402311211581));
#172664=CARTESIAN_POINT('Ctrl Pts',(80.6832998391857,-2.00684548315895,
44.2437162865044));
#172665=CARTESIAN_POINT('Ctrl Pts',(80.5440555254029,-2.59994400080739,
44.2553124037534));
#172666=CARTESIAN_POINT('Ctrl Pts',(80.4734081546615,-2.85631448270343,
44.2621957986621));
#172667=CARTESIAN_POINT('Ctrl Pts',(80.3329511489704,-3.29909646664805,
44.2774697691701));
#172668=CARTESIAN_POINT('Ctrl Pts',(80.2674520612435,-3.48675357479172,
44.2850386108823));
#172669=CARTESIAN_POINT('Ctrl Pts',(80.1577340117372,-3.77434325417801,
44.2983608575186));
#172670=CARTESIAN_POINT('Ctrl Pts',(80.1172360159011,-3.87567580319108,
44.3033939398344));
#172671=CARTESIAN_POINT('Ctrl Pts',(80.0379033032512,-4.06545065503559,
44.3134617818319));
#172672=CARTESIAN_POINT('Ctrl Pts',(79.9994149115417,-4.1540283220643,44.318429563002));
#172673=CARTESIAN_POINT('Ctrl Pts',(79.9086507796542,-4.35518839907081,
44.3303263837583));
#172674=CARTESIAN_POINT('Ctrl Pts',(79.8555834491748,-4.46738769859569,
44.3374095135131));
#172675=CARTESIAN_POINT('Ctrl Pts',(79.6688597075322,-4.84450684769502,
44.3627336945338));
#172676=CARTESIAN_POINT('Ctrl Pts',(79.5258984371408,-5.1045276194319,44.3827790337421));
#172677=CARTESIAN_POINT('Ctrl Pts',(79.3406140704187,-5.40964398127828,
44.4093653935485));
#172678=CARTESIAN_POINT('Ctrl Pts',(79.3087489438537,-5.4610923568507,44.4139570169332));
#172679=CARTESIAN_POINT('Ctrl Pts',(79.0478189849678,-5.87421542838934,
44.4517002556594));
#172680=CARTESIAN_POINT('Ctrl Pts',(78.7970661222546,-6.2213117667756,44.4888720436358));
#172681=CARTESIAN_POINT('Ctrl Pts',(78.4345178552781,-6.66221925756195,
44.5429909868608));
#172682=CARTESIAN_POINT('Ctrl Pts',(78.3411765096075,-6.77099455615806,
44.5569517329799));
#172683=CARTESIAN_POINT('Ctrl Pts',(78.1741232844086,-6.95757949211454,
44.5819396297114));
#172684=CARTESIAN_POINT('Ctrl Pts',(78.101406859692,-7.03626957578673,44.5928172589728));
#172685=CARTESIAN_POINT('Ctrl Pts',(77.9861018551028,-7.15716778611019,
44.6100491219602));
#172686=CARTESIAN_POINT('Ctrl Pts',(77.9443495293131,-7.20017925531297,
44.6162855521785));
#172687=CARTESIAN_POINT('Ctrl Pts',(77.8661999123292,-7.27927653233073,
44.6279487108804));
#172688=CARTESIAN_POINT('Ctrl Pts',(77.8299041858663,-7.31546183368558,
44.633361592367));
#172689=CARTESIAN_POINT('Ctrl Pts',(77.7284017317043,-7.41513917151991,
44.6484910985241));
#172690=CARTESIAN_POINT('Ctrl Pts',(77.6626204554461,-7.47802743249217,
44.6582873623916));
#172691=CARTESIAN_POINT('Ctrl Pts',(77.2450302830985,-7.8666739804324,44.7204585636653));
#172692=CARTESIAN_POINT('Ctrl Pts',(76.8716682127879,-8.16788997248872,
44.775996631079));
#172693=CARTESIAN_POINT('Ctrl Pts',(76.1343684641899,-8.68126788593136,
44.8868874150028));
#172694=CARTESIAN_POINT('Ctrl Pts',(75.7756326123108,-8.89934071476048,
44.9413135934751));
#172695=CARTESIAN_POINT('Ctrl Pts',(75.2735911890999,-9.16334040808751,
45.0184035461415));
#172696=CARTESIAN_POINT('Ctrl Pts',(75.141003759556,-9.22938356001108,45.0388428221052));
#172697=CARTESIAN_POINT('Ctrl Pts',(74.9173626519533,-9.33470837874229,
45.0734551423237));
#172698=CARTESIAN_POINT('Ctrl Pts',(74.8270754120788,-9.37561558374381,
45.0874648399649));
#172699=CARTESIAN_POINT('Ctrl Pts',(74.6441953046535,-9.45524750118546,
45.1159138546512));
#172700=CARTESIAN_POINT('Ctrl Pts',(74.5515978879351,-9.49393319005151,
45.1303547941148));
#172701=CARTESIAN_POINT('Ctrl Pts',(74.3149414988765,-9.5886777241126,45.1673513814753));
#172702=CARTESIAN_POINT('Ctrl Pts',(74.1701633832244,-9.6428060246807,45.1900675671839));
#172703=CARTESIAN_POINT('Ctrl Pts',(73.5791515094535,-9.8483773786203,45.2830999932603));
#172704=CARTESIAN_POINT('Ctrl Pts',(73.1240704257277,-9.97159930842423,
45.3554491140219));
#172705=CARTESIAN_POINT('Ctrl Pts',(72.3137077236981,-10.1307999853763,
45.4846431810268));
#172706=CARTESIAN_POINT('Ctrl Pts',(71.9619082670843,-10.1806572951188,
45.5408358972255));
#172707=CARTESIAN_POINT('Ctrl Pts',(71.419063013793,-10.2283015198731,45.6271766377918));
#172708=CARTESIAN_POINT('Ctrl Pts',(71.2294789563311,-10.2395124908403,
45.6572604419998));
#172709=CARTESIAN_POINT('Ctrl Pts',(70.9696001391121,-10.2474643850277,
45.6983167703373));
#172710=CARTESIAN_POINT('Ctrl Pts',(70.8995021632802,-10.2488718573973,
45.709372866089));
#172711=CARTESIAN_POINT('Ctrl Pts',(70.7790523440288,-10.2500238663365,
45.7283336507061));
#172712=CARTESIAN_POINT('Ctrl Pts',(70.7287083677262,-10.250125400347,45.7362473225106));
#172713=CARTESIAN_POINT('Ctrl Pts',(70.6167431657534,-10.2495062547478,
45.7538210177922));
#172714=CARTESIAN_POINT('Ctrl Pts',(70.5551248958887,-10.2485963603833,
45.7634752051308));
#172715=CARTESIAN_POINT('Ctrl Pts',(70.3621285679459,-10.2439634854918,
45.7936656451819));
#172716=CARTESIAN_POINT('Ctrl Pts',(70.2308030065516,-10.2382220100505,
45.8141397337392));
#172717=CARTESIAN_POINT('Ctrl Pts',(69.603662278349,-10.1984209701417,45.9116693665396));
#172718=CARTESIAN_POINT('Ctrl Pts',(69.1105498406412,-10.1300647358911,
45.9876580424967));
#172719=CARTESIAN_POINT('Ctrl Pts',(68.269598150233,-9.94898088705509,46.1173325602242));
#172720=CARTESIAN_POINT('Ctrl Pts',(67.9191065053259,-9.85336098913091,
46.1713972467541));
#172721=CARTESIAN_POINT('Ctrl Pts',(67.4042453606154,-9.68241751761035,
46.2510503813024));
#172722=CARTESIAN_POINT('Ctrl Pts',(67.2355450232222,-9.62134447903006,
46.2771863361049));
#172723=CARTESIAN_POINT('Ctrl Pts',(66.9708554109246,-9.51742658013076,
46.3182577645633));
#172724=CARTESIAN_POINT('Ctrl Pts',(66.8737671284838,-9.47754434971928,
46.3333366431497));
#172725=CARTESIAN_POINT('Ctrl Pts',(66.6885929406964,-9.39806857571963,
46.3621217097281));
#172726=CARTESIAN_POINT('Ctrl Pts',(66.6004193911351,-9.35871280994671,
46.3758394525262));
#172727=CARTESIAN_POINT('Ctrl Pts',(66.3931188524541,-9.26258522860232,
46.4081144016209));
#172728=CARTESIAN_POINT('Ctrl Pts',(66.2745057386477,-9.20472423152712,
46.426600485627));
#172729=CARTESIAN_POINT('Ctrl Pts',(65.7831394063063,-8.95296304978737,
46.5032382722179));
#172730=CARTESIAN_POINT('Ctrl Pts',(65.4213712997427,-8.73808896840144,
46.5598214397522));
#172731=CARTESIAN_POINT('Ctrl Pts',(64.7752916217732,-8.29771000806215,
46.6605449161024));
#172732=CARTESIAN_POINT('Ctrl Pts',(64.4877218187872,-8.07831618324674,
46.7052358856107));
#172733=CARTESIAN_POINT('Ctrl Pts',(64.1111484677427,-7.75791190049661,
46.7630848549705));
#172734=CARTESIAN_POINT('Ctrl Pts',(64.0117379420787,-7.66992676327865,
46.7782859186802));
#172735=CARTESIAN_POINT('Ctrl Pts',(63.8394005405125,-7.51129971534814,
46.8044762360614));
#172736=CARTESIAN_POINT('Ctrl Pts',(63.7657699365944,-7.44147409507387,
46.8156113359947));
#172737=CARTESIAN_POINT('Ctrl Pts',(63.6511017124594,-7.32944738852989,
46.8328498123164));
#172738=CARTESIAN_POINT('Ctrl Pts',(63.6093801447359,-7.28797873600959,
46.8390998043601));
#172739=CARTESIAN_POINT('Ctrl Pts',(63.5314791545818,-7.20920587032642,
46.8507238423054));
#172740=CARTESIAN_POINT('Ctrl Pts',(63.4952231208372,-7.17198263228146,
46.8561147467794));
#172741=CARTESIAN_POINT('Ctrl Pts',(63.393311076075,-7.06574880299513,46.8712168930763));
#172742=CARTESIAN_POINT('Ctrl Pts',(63.3283208608638,-6.9960868238204,46.8807865736354));
#172743=CARTESIAN_POINT('Ctrl Pts',(62.9058078137151,-6.53036755962993,
46.9426366692795));
#172744=CARTESIAN_POINT('Ctrl Pts',(62.5782585329474,-6.10742215544912,
46.9888705721308));
#172745=CARTESIAN_POINT('Ctrl Pts',(62.1111184685539,-5.39605665124973,
47.0532787316343));
#172746=CARTESIAN_POINT('Ctrl Pts',(61.9496191976245,-5.12354854216499,
47.0751609016335));
#172747=CARTESIAN_POINT('Ctrl Pts',(61.7203636854676,-4.69261631022918,
47.1057304556297));
#172748=CARTESIAN_POINT('Ctrl Pts',(61.6436342145201,-4.53929301461325,
47.1158587132025));
#172749=CARTESIAN_POINT('Ctrl Pts',(61.5265598997261,-4.2900231366227,47.1311471143641));
#172750=CARTESIAN_POINT('Ctrl Pts',(61.4837931720625,-4.19527456183938,
47.136691942056));
#172751=CARTESIAN_POINT('Ctrl Pts',(61.4038513012846,-4.01078933828968,
47.1469765956848));
#172752=CARTESIAN_POINT('Ctrl Pts',(61.3664974894336,-3.92114377790846,
47.1517448612107));
#172753=CARTESIAN_POINT('Ctrl Pts',(61.2793149775345,-3.70331901729009,
47.1627785320664));
#172754=CARTESIAN_POINT('Ctrl Pts',(61.2307659198831,-3.57463799286622,
47.1688410958831));
#172755=CARTESIAN_POINT('Ctrl Pts',(61.0402420148368,-3.03746267321418,
47.1922564120649));
#172756=CARTESIAN_POINT('Ctrl Pts',(60.9213279926237,-2.62111073909064,
47.2059429267996));
#172757=CARTESIAN_POINT('Ctrl Pts',(60.7030599179109,-1.62509682914602,
47.2276317923128));
#172758=CARTESIAN_POINT('Ctrl Pts',(60.6262083473102,-1.04199845955352,
47.2318458860108));
#172759=CARTESIAN_POINT('Ctrl Pts',(60.594289766227,-0.360824028936842,
47.2253546100265));
#172760=CARTESIAN_POINT('Ctrl Pts',(60.5911399959984,-0.266007535216332,
47.2241945180865));
#172761=CARTESIAN_POINT('Ctrl Pts',(60.5881999181426,-0.116060049539068,
47.2219423547029));
#172762=CARTESIAN_POINT('Ctrl Pts',(60.5875550318019,-0.0609487046800113,
47.2210254656653));
#172763=CARTESIAN_POINT('Ctrl Pts',(60.5873381061323,-0.00389096929625129,
47.2199823173059));
#172764=CARTESIAN_POINT('Ctrl Pts',(60.5873312521756,-0.0019454838982729,
47.2199466363049));
#172765=CARTESIAN_POINT('Ctrl Pts',(60.5873249407211,4.24183370377617E-12,
47.2199108422682));
#172766=CARTESIAN_POINT('Origin',(69.7358040552328,0.,40.0761166693274));
#172767=CARTESIAN_POINT('',(61.0040805671216,1.7419825273942E-11,49.583449449497));
#172768=CARTESIAN_POINT('',(60.9878801781973,-1.65377492662557E-11,49.4915724783198));
#172769=CARTESIAN_POINT('',(59.6415245868576,-1.25526296912604E-15,41.8560104904131));
#172770=CARTESIAN_POINT('Ctrl Pts',(61.0040805671216,3.48409058108532E-11,
49.583449449497));
#172771=CARTESIAN_POINT('Ctrl Pts',(61.0040673449976,0.00407567382671532,
49.5833744631057));
#172772=CARTESIAN_POINT('Ctrl Pts',(61.0040565037605,0.00815135186697398,
49.5832989804273));
#172773=CARTESIAN_POINT('Ctrl Pts',(61.0039320934917,0.0680854659092492,
49.5821816953104));
#172774=CARTESIAN_POINT('Ctrl Pts',(61.0042633855356,0.123942179426902,
49.5810473211021));
#172775=CARTESIAN_POINT('Ctrl Pts',(61.0064153766429,0.278278712675812,
49.5776595482583));
#172776=CARTESIAN_POINT('Ctrl Pts',(61.0091799556003,0.376735212894865,
49.5752131984396));
#172777=CARTESIAN_POINT('Ctrl Pts',(61.0325051331097,0.928931211202058,
49.5599333442491));
#172778=CARTESIAN_POINT('Ctrl Pts',(61.0812548371948,1.38082706604539,49.5415343461584));
#172779=CARTESIAN_POINT('Ctrl Pts',(61.2228842771604,2.1913329685438,49.4988628223748));
#172780=CARTESIAN_POINT('Ctrl Pts',(61.3057167948855,2.55101398941332,49.4763572651825));
#172781=CARTESIAN_POINT('Ctrl Pts',(61.4546898524297,3.0693911988267,49.4389002220721));
#172782=CARTESIAN_POINT('Ctrl Pts',(61.5058965644992,3.23224647348887,49.4263831544526));
#172783=CARTESIAN_POINT('Ctrl Pts',(61.6081089505079,3.53117622055814,49.4020224914558));
#172784=CARTESIAN_POINT('Ctrl Pts',(61.6580017427047,3.6675995294168,49.3903579582932));
#172785=CARTESIAN_POINT('Ctrl Pts',(61.7467760692201,3.89528556576239,49.3699634930242));
#172786=CARTESIAN_POINT('Ctrl Pts',(61.7841293413855,3.98714218525543,49.3614765517485));
#172787=CARTESIAN_POINT('Ctrl Pts',(61.8578013224181,4.16106077273271,49.3449095933209));
#172788=CARTESIAN_POINT('Ctrl Pts',(61.8938792801003,4.24321824562081,49.336867969315));
#172789=CARTESIAN_POINT('Ctrl Pts',(61.9925396913437,4.46012767106206,49.3150578710357));
#172790=CARTESIAN_POINT('Ctrl Pts',(62.0569666463966,4.59398704125687,49.3009971595692));
#172791=CARTESIAN_POINT('Ctrl Pts',(62.3072820697831,5.08641890005117,49.2469812440128));
#172792=CARTESIAN_POINT('Ctrl Pts',(62.5112633589193,5.43505031105863,49.2041469361923));
#172793=CARTESIAN_POINT('Ctrl Pts',(62.9680010973421,6.11945136653108,49.1097604168948));
#172794=CARTESIAN_POINT('Ctrl Pts',(63.2219657960189,6.45345669783525,49.0580132218942));
#172795=CARTESIAN_POINT('Ctrl Pts',(63.5844536915174,6.87376348966324,48.9842977375232));
#172796=CARTESIAN_POINT('Ctrl Pts',(63.6755211219381,6.97516563609575,48.9657874925067));
#172797=CARTESIAN_POINT('Ctrl Pts',(63.8130351868757,7.12223551365012,48.9378153233543));
#172798=CARTESIAN_POINT('Ctrl Pts',(63.8579595653611,7.16936601315166,48.9286738759781));
#172799=CARTESIAN_POINT('Ctrl Pts',(63.9418884873431,7.25574017831345,48.9115847144845));
#172800=CARTESIAN_POINT('Ctrl Pts',(63.980768980659,7.29510509796929,48.9036634249084));
#172801=CARTESIAN_POINT('Ctrl Pts',(64.0785657922458,7.39251549112169,48.8837295587852));
#172802=CARTESIAN_POINT('Ctrl Pts',(64.1378651062253,7.45015389406024,48.8716347212945));
#172803=CARTESIAN_POINT('Ctrl Pts',(64.411617338533,7.70980090357732,48.8157849989339));
#172804=CARTESIAN_POINT('Ctrl Pts',(64.633937889923,7.90295376069808,48.7703915764291));
#172805=CARTESIAN_POINT('Ctrl Pts',(65.2039994328685,8.355997590601,48.6543618629463));
#172806=CARTESIAN_POINT('Ctrl Pts',(65.5605220899802,8.60347392592059,48.5821199313326));
#172807=CARTESIAN_POINT('Ctrl Pts',(66.0373040097512,8.89045490370289,48.4863960877223));
#172808=CARTESIAN_POINT('Ctrl Pts',(66.1441201423704,8.95208296464464,48.465002566873));
#172809=CARTESIAN_POINT('Ctrl Pts',(66.4072739254099,9.09747761472091,48.4124339267184));
#172810=CARTESIAN_POINT('Ctrl Pts',(66.5647318969057,9.17906924168856,48.3810947704945));
#172811=CARTESIAN_POINT('Ctrl Pts',(66.8177909835845,9.30174309763282,48.3309186507373));
#172812=CARTESIAN_POINT('Ctrl Pts',(66.9120334108321,9.34561836260671,48.3122730847958));
#172813=CARTESIAN_POINT('Ctrl Pts',(67.0947067281429,9.42720445646798,48.2762093529906));
#172814=CARTESIAN_POINT('Ctrl Pts',(67.1830334651035,9.46512658565578,48.2588059541097));
#172815=CARTESIAN_POINT('Ctrl Pts',(67.3939087302974,9.55206306608089,48.2173351258885));
#172816=CARTESIAN_POINT('Ctrl Pts',(67.5169013683719,9.59992415779027,48.1932097203439));
#172817=CARTESIAN_POINT('Ctrl Pts',(67.9941691234116,9.7747762603445,48.0998136719632));
#172818=CARTESIAN_POINT('Ctrl Pts',(68.3544683888514,9.88398260549235,48.0297837993292));
#172819=CARTESIAN_POINT('Ctrl Pts',(69.1670658385735,10.0806001285614,47.8724017458725));
#172820=CARTESIAN_POINT('Ctrl Pts',(69.6209786021461,10.1574667226971,47.7848657854983));
#172821=CARTESIAN_POINT('Ctrl Pts',(70.2924683811773,10.2235468767787,47.6548774426344));
#172822=CARTESIAN_POINT('Ctrl Pts',(70.5071330688254,10.2376195699303,47.6132445907046));
#172823=CARTESIAN_POINT('Ctrl Pts',(70.7945972563735,10.247059916598,47.5572647245332));
#172824=CARTESIAN_POINT('Ctrl Pts',(70.8671705467532,10.248642782147,47.5431125370581));
#172825=CARTESIAN_POINT('Ctrl Pts',(70.9900854424749,10.2499684817613,47.5191039792565));
#172826=CARTESIAN_POINT('Ctrl Pts',(71.0404220177089,10.2501265509135,47.5092605390517));
#172827=CARTESIAN_POINT('Ctrl Pts',(71.1501771497844,10.2496320682669,47.4877711481412));
#172828=CARTESIAN_POINT('Ctrl Pts',(71.2095916633332,10.2488280277085,47.4761217045659));
#172829=CARTESIAN_POINT('Ctrl Pts',(71.3893848618278,10.2447713860716,47.4408253099966));
#172830=CARTESIAN_POINT('Ctrl Pts',(71.5097081370372,10.2398526698203,47.4171438904982));
#172831=CARTESIAN_POINT('Ctrl Pts',(72.2218386726454,10.1976779810612,47.2767165395426));
#172832=CARTESIAN_POINT('Ctrl Pts',(72.8093933424619,10.1093534062066,47.1598201382924));
#172833=CARTESIAN_POINT('Ctrl Pts',(73.6319342458763,9.9088108181989,46.9964779357895));
#172834=CARTESIAN_POINT('Ctrl Pts',(73.8756408755417,9.83939181932036,46.94811084902));
#172835=CARTESIAN_POINT('Ctrl Pts',(74.2985017592521,9.70122238367633,46.8643160550229));
#172836=CARTESIAN_POINT('Ctrl Pts',(74.478777627586,9.6364903737699,46.8286337095392));
#172837=CARTESIAN_POINT('Ctrl Pts',(74.7564952780868,9.527611975536,46.773738141561));
#172838=CARTESIAN_POINT('Ctrl Pts',(74.8552364332674,9.48705641825705,46.7542349072487));
#172839=CARTESIAN_POINT('Ctrl Pts',(75.0408825763764,9.40729442242711,46.7175929386025));
#172840=CARTESIAN_POINT('Ctrl Pts',(75.1279098115385,9.36841538698938,46.7004271791125));
#172841=CARTESIAN_POINT('Ctrl Pts',(75.326549230017,9.2762347133933,46.6612696420596));
#172842=CARTESIAN_POINT('Ctrl Pts',(75.43776808863,9.22208740524928,46.6393624207116));
#172843=CARTESIAN_POINT('Ctrl Pts',(75.821807746146,9.02620659869566,46.5637616523185));
#172844=CARTESIAN_POINT('Ctrl Pts',(76.0892452106587,8.87387365141424,46.5112004349527));
#172845=CARTESIAN_POINT('Ctrl Pts',(76.3787138015798,8.6908378026982,46.4542731138968));
#172846=CARTESIAN_POINT('Ctrl Pts',(76.4078917222599,8.67217584096392,46.4485344420631));
#172847=CARTESIAN_POINT('Ctrl Pts',(76.7974269107242,8.42017968097085,46.3719114593987));
#172848=CARTESIAN_POINT('Ctrl Pts',(77.1429246859792,8.16385253383278,46.3038580152475));
#172849=CARTESIAN_POINT('Ctrl Pts',(77.5805623123211,7.79343683031798,46.216773717417));
#172850=CARTESIAN_POINT('Ctrl Pts',(77.6878976081256,7.69858906245689,46.1953363510994));
#172851=CARTESIAN_POINT('Ctrl Pts',(77.8718332748722,7.52893390483562,46.1584142256097));
#172852=CARTESIAN_POINT('Ctrl Pts',(77.9493185650653,7.45514875292869,46.1427997842708));
#172853=CARTESIAN_POINT('Ctrl Pts',(78.0682280501083,7.33825333994719,46.118724105806));
#172854=CARTESIAN_POINT('Ctrl Pts',(78.1104567232221,7.29599601915857,46.1101509572733));
#172855=CARTESIAN_POINT('Ctrl Pts',(78.1880223212825,7.21698660172601,46.0943568138957));
#172856=CARTESIAN_POINT('Ctrl Pts',(78.2234594561265,7.18033851698227,46.0871222645864));
#172857=CARTESIAN_POINT('Ctrl Pts',(78.3209263338557,7.0780016391432,46.0671749591857));
#172858=CARTESIAN_POINT('Ctrl Pts',(78.3823628801202,7.01173804498451,46.054545300444));
#172859=CARTESIAN_POINT('Ctrl Pts',(78.7649939098359,6.58778962157157,45.975564355603));
#172860=CARTESIAN_POINT('Ctrl Pts',(79.0615942226491,6.20804358575574,45.912903385635));
#172861=CARTESIAN_POINT('Ctrl Pts',(79.5639827856835,5.46144651148204,45.8051828536768));
#172862=CARTESIAN_POINT('Ctrl Pts',(79.7761220919811,5.10025123361291,45.7589905416315));
#172863=CARTESIAN_POINT('Ctrl Pts',(80.0331196361417,4.59430834000802,45.7022853161928));
#172864=CARTESIAN_POINT('Ctrl Pts',(80.0975399315968,4.46039098638363,45.6879917243836));
#172865=CARTESIAN_POINT('Ctrl Pts',(80.2003085921771,4.23438069341351,45.6650548598083));
#172866=CARTESIAN_POINT('Ctrl Pts',(80.2402449340321,4.14306684354109,45.6561035219449));
#172867=CARTESIAN_POINT('Ctrl Pts',(80.3134291800371,3.96891087806438,45.6396251955236));
#172868=CARTESIAN_POINT('Ctrl Pts',(80.3469360602918,3.88619247319618,45.6320479987425));
#172869=CARTESIAN_POINT('Ctrl Pts',(80.4321304936543,3.66779165715199,45.612691673642));
#172870=CARTESIAN_POINT('Ctrl Pts',(80.4820506691022,3.53141165359496,45.6012556823369));
#172871=CARTESIAN_POINT('Ctrl Pts',(80.7368300530287,2.7872369657385,45.5423178865471));
#172872=CARTESIAN_POINT('Ctrl Pts',(80.8880433326182,2.16179213325184,45.5052564431246));
#172873=CARTESIAN_POINT('Ctrl Pts',(81.0177905568147,1.26957861901464,45.4675592930169));
#172874=CARTESIAN_POINT('Ctrl Pts',(81.0454722871623,1.01185257793934,45.4583846578112));
#172875=CARTESIAN_POINT('Ctrl Pts',(81.0711989342334,0.642344008651511,
45.4474748180109));
#172876=CARTESIAN_POINT('Ctrl Pts',(81.0771397391497,0.531250048812504,
45.4444827765273));
#172877=CARTESIAN_POINT('Ctrl Pts',(81.0845918423905,0.331668168683652,
45.4396025589623));
#172878=CARTESIAN_POINT('Ctrl Pts',(81.086760798445,0.243218453805301,45.4376139966441));
#172879=CARTESIAN_POINT('Ctrl Pts',(81.0884256696655,0.100950184485942,
45.4346853926625));
#172880=CARTESIAN_POINT('Ctrl Pts',(81.0886360100655,0.04714661561525,45.4336398879946));
#172881=CARTESIAN_POINT('Ctrl Pts',(81.0882122583059,-0.0618632610171435,
45.4316444081162));
#172882=CARTESIAN_POINT('Ctrl Pts',(81.0875560498093,-0.117067658097874,
45.4306977765404));
#172883=CARTESIAN_POINT('Ctrl Pts',(81.0845637515103,-0.267561747610409,
45.4282950839628));
#172884=CARTESIAN_POINT('Ctrl Pts',(81.0813537485863,-0.362830713523165,
45.4269686598293));
#172885=CARTESIAN_POINT('Ctrl Pts',(81.0545999128149,-0.926020272110199,
45.420318260754));
#172886=CARTESIAN_POINT('Ctrl Pts',(81.000684497016,-1.39200765978234,45.4197044297711));
#172887=CARTESIAN_POINT('Ctrl Pts',(80.8188730207129,-2.37623753026221,
45.4302640098083));
#172888=CARTESIAN_POINT('Ctrl Pts',(80.6821727652902,-2.89146758284856,
45.4430574296226));
#172889=CARTESIAN_POINT('Ctrl Pts',(80.4587877575335,-3.53120381771839,
45.4688826648455));
#172890=CARTESIAN_POINT('Ctrl Pts',(80.4079158694468,-3.66762201686016,
45.474985774153));
#172891=CARTESIAN_POINT('Ctrl Pts',(80.3175218561777,-3.8953021079917,45.4861836488402));
#172892=CARTESIAN_POINT('Ctrl Pts',(80.2795187512148,-3.98715782249328,
45.4909840901436));
#172893=CARTESIAN_POINT('Ctrl Pts',(80.2046232464102,-4.16107626087176,
45.5006135933442));
#172894=CARTESIAN_POINT('Ctrl Pts',(80.1679701650797,-4.24323447034296,
45.505396399953));
#172895=CARTESIAN_POINT('Ctrl Pts',(80.0677971090229,-4.46014958911488,
45.5186458938487));
#172896=CARTESIAN_POINT('Ctrl Pts',(80.002443723957,-4.59401381721281,45.5274688624765));
#172897=CARTESIAN_POINT('Ctrl Pts',(79.751162691718,-5.0817577254656,45.5619919879664));
#172898=CARTESIAN_POINT('Ctrl Pts',(79.5477861608664,-5.42599629684176,
45.5910702757448));
#172899=CARTESIAN_POINT('Ctrl Pts',(79.1277308350556,-6.05103096487884,
45.6524973395758));
#172900=CARTESIAN_POINT('Ctrl Pts',(78.9154748071413,-6.33416543875234,
45.6840531754701));
#172901=CARTESIAN_POINT('Ctrl Pts',(78.6050034727639,-6.70650223929368,
45.7304262038561));
#172902=CARTESIAN_POINT('Ctrl Pts',(78.518948475767,-6.80575444824079,45.7432990708961));
#172903=CARTESIAN_POINT('Ctrl Pts',(78.3636145420426,-6.9780799359613,45.7665340086848));
#172904=CARTESIAN_POINT('Ctrl Pts',(78.2951157155577,-7.05184774857841,
45.7767796490357));
#172905=CARTESIAN_POINT('Ctrl Pts',(78.1849954796973,-7.16697177031707,
45.7932351821164));
#172906=CARTESIAN_POINT('Ctrl Pts',(78.1440827458378,-7.2090108747292,45.7993455669863));
#172907=CARTESIAN_POINT('Ctrl Pts',(78.0661645735939,-7.28770253355853,
45.8109729767454));
#172908=CARTESIAN_POINT('Ctrl Pts',(78.0292359088352,-7.32442985533583,
45.8164796948654));
#172909=CARTESIAN_POINT('Ctrl Pts',(77.9234664203589,-7.42802101044722,
45.8322438236062));
#172910=CARTESIAN_POINT('Ctrl Pts',(77.8539667060724,-7.49419031439474,
45.8425927886614));
#172911=CARTESIAN_POINT('Ctrl Pts',(77.5682993208651,-7.7585728062715,45.8851210559512));
#172912=CARTESIAN_POINT('Ctrl Pts',(77.3446354325167,-7.94830257061248,
45.9184003312349));
#172913=CARTESIAN_POINT('Ctrl Pts',(76.7812530010548,-8.38581214569848,
46.0026037301126));
#172914=CARTESIAN_POINT('Ctrl Pts',(76.4338656154348,-8.62258577781445,
46.0548437426379));
#172915=CARTESIAN_POINT('Ctrl Pts',(75.9684924311167,-8.8991457156002,46.1256443746958));
#172916=CARTESIAN_POINT('Ctrl Pts',(75.8627909874382,-8.95941092458015,
46.1417753481643));
#172917=CARTESIAN_POINT('Ctrl Pts',(75.601515544903,-9.10219761974323,46.1817793704878));
#172918=CARTESIAN_POINT('Ctrl Pts',(75.4448505766269,-9.18257529397102,
46.2058779471163));
#172919=CARTESIAN_POINT('Ctrl Pts',(75.1923206429091,-9.30390972558562,
46.2449075485867));
#172920=CARTESIAN_POINT('Ctrl Pts',(75.0977487456319,-9.34756089790883,
46.2595640749589));
#172921=CARTESIAN_POINT('Ctrl Pts',(74.9139616327435,-9.42896336502099,
46.2881235568065));
#172922=CARTESIAN_POINT('Ctrl Pts',(74.8248421693073,-9.46690960124373,
46.3020063189872));
#172923=CARTESIAN_POINT('Ctrl Pts',(74.6112610035641,-9.55423571487202,
46.3353561484672));
#172924=CARTESIAN_POINT('Ctrl Pts',(74.4863482214221,-9.60242456899424,
46.3549237400397));
#172925=CARTESIAN_POINT('Ctrl Pts',(74.0018405292962,-9.77831688357989,
46.431045166004));
#172926=CARTESIAN_POINT('Ctrl Pts',(73.6362463788273,-9.88794313063175,
46.4889643887945));
#172927=CARTESIAN_POINT('Ctrl Pts',(72.6900682040399,-10.1138034185437,
46.6394991502311));
#172928=CARTESIAN_POINT('Ctrl Pts',(72.1040200846467,-10.199863110892,46.7333637028918));
#172929=CARTESIAN_POINT('Ctrl Pts',(71.3961233553964,-10.2403862161788,
46.8456107995423));
#172930=CARTESIAN_POINT('Ctrl Pts',(71.2783702210663,-10.2450410236952,
46.8642425538667));
#172931=CARTESIAN_POINT('Ctrl Pts',(71.1013799408687,-10.2489068919668,
46.8921642895165));
#172932=CARTESIAN_POINT('Ctrl Pts',(71.0421925221178,-10.2496742327309,
46.9014876775396));
#172933=CARTESIAN_POINT('Ctrl Pts',(70.9321765080428,-10.2501241729304,
46.9187880549125));
#172934=CARTESIAN_POINT('Ctrl Pts',(70.8813516080021,-10.2499448116025,
46.9267683086871));
#172935=CARTESIAN_POINT('Ctrl Pts',(70.7682154402204,-10.2486836542141,
46.9445069059908));
#172936=CARTESIAN_POINT('Ctrl Pts',(70.7059074734182,-10.2474070288422,
46.9542591770138));
#172937=CARTESIAN_POINT('Ctrl Pts',(70.4727739729375,-10.2404518933631,
46.9906926394535));
#172938=CARTESIAN_POINT('Ctrl Pts',(70.3020721738944,-10.2309804072448,
47.0172573077076));
#172939=CARTESIAN_POINT('Ctrl Pts',(69.6109075697902,-10.1748539933539,
47.1245199710389));
#172940=CARTESIAN_POINT('Ctrl Pts',(69.0940392714917,-10.091870712187,47.2040885696753));
#172941=CARTESIAN_POINT('Ctrl Pts',(68.3378409925298,-9.90894490389436,
47.3207241779582));
#172942=CARTESIAN_POINT('Ctrl Pts',(68.0921800517385,-9.83950696932494,
47.3586433244153));
#172943=CARTESIAN_POINT('Ctrl Pts',(67.6659992383484,-9.70129836716088,
47.4245538850417));
#172944=CARTESIAN_POINT('Ctrl Pts',(67.4843369957254,-9.63655111956149,
47.4526897972642));
#172945=CARTESIAN_POINT('Ctrl Pts',(67.204529284537,-9.52765191535149,47.4960996270251));
#172946=CARTESIAN_POINT('Ctrl Pts',(67.1050626524839,-9.48709353734558,
47.5115455581197));
#172947=CARTESIAN_POINT('Ctrl Pts',(66.9180720306105,-9.40733002369934,
47.5406093233296));
#172948=CARTESIAN_POINT('Ctrl Pts',(66.8304237779518,-9.36845264967769,
47.5542435923924));
#172949=CARTESIAN_POINT('Ctrl Pts',(66.6303893284162,-9.2762826114878,47.5853833759914));
#172950=CARTESIAN_POINT('Ctrl Pts',(66.5184013821207,-9.22214485084536,
47.6028338605937));
#172951=CARTESIAN_POINT('Ctrl Pts',(66.1318650337091,-9.02637248821874,
47.6631104716653));
#172952=CARTESIAN_POINT('Ctrl Pts',(65.862753936375,-8.87415475948891,47.7051606732697));
#172953=CARTESIAN_POINT('Ctrl Pts',(65.5747679244819,-8.69334486471779,
47.7501248446212));
#172954=CARTESIAN_POINT('Ctrl Pts',(65.5486983017096,-8.67681035273505,
47.7541947891571));
#172955=CARTESIAN_POINT('Ctrl Pts',(65.1566726098513,-8.42564649642074,
47.8153889121942));
#172956=CARTESIAN_POINT('Ctrl Pts',(64.8058745255349,-8.16761862304484,
47.8700587382125));
#172957=CARTESIAN_POINT('Ctrl Pts',(64.3618560895901,-7.79489198067989,
47.9383709197026));
#172958=CARTESIAN_POINT('Ctrl Pts',(64.2532917614047,-7.6997570588825,47.9549947846071));
#172959=CARTESIAN_POINT('Ctrl Pts',(64.0672715067216,-7.52964245613763,
47.9832936984406));
#172960=CARTESIAN_POINT('Ctrl Pts',(63.9889319965957,-7.45569423181673,
47.9951511011832));
#172961=CARTESIAN_POINT('Ctrl Pts',(63.8687408377713,-7.33859834064117,
48.0132300411273));
#172962=CARTESIAN_POINT('Ctrl Pts',(63.8260902515492,-7.29630875339498,
48.0196225586124));
#172963=CARTESIAN_POINT('Ctrl Pts',(63.7477818472157,-7.21728656679977,
48.0313129081549));
#172964=CARTESIAN_POINT('Ctrl Pts',(63.7120243632958,-7.18065888316707,
48.0366324598717));
#172965=CARTESIAN_POINT('Ctrl Pts',(63.6137404304597,-7.07846387164977,
48.051205179706));
#172966=CARTESIAN_POINT('Ctrl Pts',(63.5517969709913,-7.01232448132923,
48.0603341479518));
#172967=CARTESIAN_POINT('Ctrl Pts',(63.1629037520539,-6.58590725616973,
48.1173268257431));
#172968=CARTESIAN_POINT('Ctrl Pts',(62.86070431903,-6.20322789384647,48.160169970309));
#172969=CARTESIAN_POINT('Ctrl Pts',(62.3519059843458,-5.4553149670522,48.2307302784892));
#172970=CARTESIAN_POINT('Ctrl Pts',(62.1382797499242,-5.09620297619264,
48.2596688955328));
#172971=CARTESIAN_POINT('Ctrl Pts',(61.87880738257,-4.59277142093952,48.2940905470742));
#172972=CARTESIAN_POINT('Ctrl Pts',(61.8135444332031,-4.45913267275824,
48.3026702813829));
#172973=CARTESIAN_POINT('Ctrl Pts',(61.7093099052031,-4.23345325529348,
48.3162413593808));
#172974=CARTESIAN_POINT('Ctrl Pts',(61.6687517275544,-4.14218615668145,
48.3214845925173));
#172975=CARTESIAN_POINT('Ctrl Pts',(61.5897014039152,-3.95711622997738,
48.3316257876471));
#172976=CARTESIAN_POINT('Ctrl Pts',(61.5512534577513,-3.86330619699858,
48.3365168769265));
#172977=CARTESIAN_POINT('Ctrl Pts',(61.4569139993982,-3.62311778127344,
48.3484063768129));
#172978=CARTESIAN_POINT('Ctrl Pts',(61.402952818374,-3.47599465238431,48.3550985570037));
#172979=CARTESIAN_POINT('Ctrl Pts',(61.1945207709509,-2.86515841778187,
48.3804403696506));
#172980=CARTESIAN_POINT('Ctrl Pts',(61.0695872723964,-2.39186309715017,
48.3943840153022));
#172981=CARTESIAN_POINT('Ctrl Pts',(60.913282447589,-1.56823970016767,48.4082143148684));
#172982=CARTESIAN_POINT('Ctrl Pts',(60.8654794912693,-1.2219533567363,48.4109596393889));
#172983=CARTESIAN_POINT('Ctrl Pts',(60.8186903445414,-0.685333999625466,
48.4100457573896));
#172984=CARTESIAN_POINT('Ctrl Pts',(60.8073814968257,-0.49633910944873,
48.4087430698905));
#172985=CARTESIAN_POINT('Ctrl Pts',(60.7989069574862,-0.236577787073999,
48.4055282221811));
#172986=CARTESIAN_POINT('Ctrl Pts',(60.7973195590584,-0.165983077583135,
48.4045102554311));
#172987=CARTESIAN_POINT('Ctrl Pts',(60.7960539259737,-0.0635873302775755,
48.402819863519));
#172988=CARTESIAN_POINT('Ctrl Pts',(60.7958058977463,-0.0317937268324048,
48.4022651036016));
#172989=CARTESIAN_POINT('Ctrl Pts',(60.7957027539178,1.12610920091049E-9,
48.4016801458622));
#172990=CARTESIAN_POINT('Ctrl Pts',(60.7795023650012,-1.31054137042235E-9,
48.3098031747286));
#172991=CARTESIAN_POINT('Ctrl Pts',(60.7795765067117,-0.0228539252004177,
48.310223653247));
#172992=CARTESIAN_POINT('Ctrl Pts',(60.779726332016,-0.0457078558460972,
48.3106331887275));
#172993=CARTESIAN_POINT('Ctrl Pts',(60.7805904389733,-0.133284916798912,
48.3121602353422));
#172994=CARTESIAN_POINT('Ctrl Pts',(60.7818359190101,-0.198002387172251,
48.313200131041));
#172995=CARTESIAN_POINT('Ctrl Pts',(60.7879015251552,-0.409940099125638,
48.3163084488624));
#172996=CARTESIAN_POINT('Ctrl Pts',(60.7952541481782,-0.557075269763786,
48.3179963592047));
#172997=CARTESIAN_POINT('Ctrl Pts',(60.8404923029711,-1.19121275142366,
48.32313819393));
#172998=CARTESIAN_POINT('Ctrl Pts',(60.9095924263722,-1.67539614495611,
48.3215957730452));
#172999=CARTESIAN_POINT('Ctrl Pts',(61.1003678533738,-2.56147117870582,
48.3073380182831));
#173000=CARTESIAN_POINT('Ctrl Pts',(61.2128476043723,-2.96433645223241,
48.2962826415568));
#173001=CARTESIAN_POINT('Ctrl Pts',(61.398553863287,-3.50223277365923,48.2749583044959));
#173002=CARTESIAN_POINT('Ctrl Pts',(61.4510412238349,-3.64414850080823,
48.2686894151225));
#173003=CARTESIAN_POINT('Ctrl Pts',(61.5434753960353,-3.87824169459329,
48.2572693516743));
#173004=CARTESIAN_POINT('Ctrl Pts',(61.5817012772225,-3.97108886448879,
48.2524515988262));
#173005=CARTESIAN_POINT('Ctrl Pts',(61.6609814697912,-4.1559933543047,48.2422774476391));
#173006=CARTESIAN_POINT('Ctrl Pts',(61.7020421679011,-4.2480357948693,48.2369195213534));
#173007=CARTESIAN_POINT('Ctrl Pts',(61.8091920736398,-4.47911947043774,
48.2227253218519));
#173008=CARTESIAN_POINT('Ctrl Pts',(61.8770391485022,-4.61729653443926,
48.2135473656859));
#173009=CARTESIAN_POINT('Ctrl Pts',(62.0341735558332,-4.92007396352988,
48.1919096692745));
#173010=CARTESIAN_POINT('Ctrl Pts',(62.1248900566577,-5.08385006970712,
48.1791737231482));
#173011=CARTESIAN_POINT('Ctrl Pts',(62.4610459019524,-5.65365218217333,
48.1312508599801));
#173012=CARTESIAN_POINT('Ctrl Pts',(62.729773664739,-6.0448432735838,48.0916520591102));
#173013=CARTESIAN_POINT('Ctrl Pts',(63.1818130027412,-6.61407985057535,
48.0243061433485));
#173014=CARTESIAN_POINT('Ctrl Pts',(63.3465240915125,-6.80640192010735,
47.99964841869));
#173015=CARTESIAN_POINT('Ctrl Pts',(63.5726427126616,-7.05137667845077,
47.9658316321619));
#173016=CARTESIAN_POINT('Ctrl Pts',(63.6278321061735,-7.10976894082202,
47.9575805133412));
#173017=CARTESIAN_POINT('Ctrl Pts',(63.7221183976014,-7.2071933640807,47.9434967595932));
#173018=CARTESIAN_POINT('Ctrl Pts',(63.7608563329749,-7.2465745887425,47.93771408191));
#173019=CARTESIAN_POINT('Ctrl Pts',(63.847215518413,-7.33295073186859,47.9248326965077));
#173020=CARTESIAN_POINT('Ctrl Pts',(63.8949813477333,-7.37979336047445,
47.9177138690443));
#173021=CARTESIAN_POINT('Ctrl Pts',(64.0484015995225,-7.52731112026731,
47.8948597582135));
#173022=CARTESIAN_POINT('Ctrl Pts',(64.1557422862191,-7.62616921198454,
47.8788860377963));
#173023=CARTESIAN_POINT('Ctrl Pts',(64.434965097946,-7.87244812078303,47.8373141111808));
#173024=CARTESIAN_POINT('Ctrl Pts',(64.6096757214068,-8.01646917727984,
47.811283157596));
#173025=CARTESIAN_POINT('Ctrl Pts',(65.2756754166724,-8.52913912498367,
47.7117002912856));
#173026=CARTESIAN_POINT('Ctrl Pts',(65.7948079728654,-8.85851727020266,
47.6333162159989));
#173027=CARTESIAN_POINT('Ctrl Pts',(66.4589108091594,-9.19974337699546,
47.5311669373846));
#173028=CARTESIAN_POINT('Ctrl Pts',(66.5791222396116,-9.25852181227756,
47.512610830095));
#173029=CARTESIAN_POINT('Ctrl Pts',(66.7882505634683,-9.35567628070652,
47.4802147169227));
#173030=CARTESIAN_POINT('Ctrl Pts',(66.8766319308123,-9.39519920322599,
47.4664890813355));
#173031=CARTESIAN_POINT('Ctrl Pts',(67.0613433228089,-9.47462864696736,
47.4377330021541));
#173032=CARTESIAN_POINT('Ctrl Pts',(67.1577488796595,-9.51432418937986,
47.4226853845674));
#173033=CARTESIAN_POINT('Ctrl Pts',(67.4181775626633,-9.61685917212951,
47.3819354344702));
#173034=CARTESIAN_POINT('Ctrl Pts',(67.5832258774511,-9.6769025253189,47.3560038010921));
#173035=CARTESIAN_POINT('Ctrl Pts',(68.5231633857349,-9.99122789578273,
47.2078059431948));
#173036=CARTESIAN_POINT('Ctrl Pts',(69.3242013150811,-10.1544651041615,
47.0792845889112));
#173037=CARTESIAN_POINT('Ctrl Pts',(70.300930718175,-10.231830670227,46.9240490764136));
#173038=CARTESIAN_POINT('Ctrl Pts',(70.4660935905049,-10.2407978935956,
46.8978590670135));
#173039=CARTESIAN_POINT('Ctrl Pts',(70.6931994158643,-10.2474851876242,
46.8619867841994));
#173040=CARTESIAN_POINT('Ctrl Pts',(70.7550012084679,-10.2487318002441,
46.8522392027246));
#173041=CARTESIAN_POINT('Ctrl Pts',(70.8675396507649,-10.2499585566647,
46.8345194279285));
#173042=CARTESIAN_POINT('Ctrl Pts',(70.9182714022317,-10.2501257164091,
46.826542739719));
#173043=CARTESIAN_POINT('Ctrl Pts',(71.0285527484569,-10.2496504113759,
46.8092292506485));
#173044=CARTESIAN_POINT('Ctrl Pts',(71.0880997877005,-10.2488622430712,
46.7998969368915));
#173045=CARTESIAN_POINT('Ctrl Pts',(71.2673852523826,-10.2448886739982,
46.7718423936476));
#173046=CARTESIAN_POINT('Ctrl Pts',(71.3870850143546,-10.2400853917182,
46.7531700244064));
#173047=CARTESIAN_POINT('Ctrl Pts',(71.676335623008,-10.2232755867876,46.7081560565961));
#173048=CARTESIAN_POINT('Ctrl Pts',(71.845734425581,-10.2090980345999,46.6818828075499));
#173049=CARTESIAN_POINT('Ctrl Pts',(72.6720047468749,-10.1187230726835,
46.5539914500252));
#173050=CARTESIAN_POINT('Ctrl Pts',(73.3209135840049,-9.98190993035056,
46.4542482860221));
#173051=CARTESIAN_POINT('Ctrl Pts',(74.1468086644587,-9.72042310977867,
46.3265632297974));
#173052=CARTESIAN_POINT('Ctrl Pts',(74.3398113943093,-9.65276896211922,
46.2966799600512));
#173053=CARTESIAN_POINT('Ctrl Pts',(74.6338574990111,-9.53950702820404,
46.2510703679023));
#173054=CARTESIAN_POINT('Ctrl Pts',(74.7364095851474,-9.49804989607294,
46.2351481012261));
#173055=CARTESIAN_POINT('Ctrl Pts',(74.9260928779884,-9.41770454404923,
46.2056700648824));
#173056=CARTESIAN_POINT('Ctrl Pts',(75.013392237616,-9.37925356836793,46.1920920337707));
#173057=CARTESIAN_POINT('Ctrl Pts',(75.2103546523868,-9.28913706849641,
46.1614347658374));
#173058=CARTESIAN_POINT('Ctrl Pts',(75.3196639282275,-9.23671762433628,
46.1444043088575));
#173059=CARTESIAN_POINT('Ctrl Pts',(75.6864127941312,-9.05262898091877,
46.0872217634099));
#173060=CARTESIAN_POINT('Ctrl Pts',(75.9392036797019,-8.91181887450907,
46.0477308214453));
#173061=CARTESIAN_POINT('Ctrl Pts',(76.6767679350914,-8.45842479205521,
45.932554552414));
#173062=CARTESIAN_POINT('Ctrl Pts',(77.1415427806757,-8.11484095676641,
45.8599950243703));
#173063=CARTESIAN_POINT('Ctrl Pts',(77.6874925401928,-7.6344926605228,45.7764740508071));
#173064=CARTESIAN_POINT('Ctrl Pts',(77.7975887495404,-7.53324960471619,
45.7597325125078));
#173065=CARTESIAN_POINT('Ctrl Pts',(77.9541122691709,-7.38284642989016,
45.7361247359689));
#173066=CARTESIAN_POINT('Ctrl Pts',(78.0023057619755,-7.3356123599928,45.7288836468148));
#173067=CARTESIAN_POINT('Ctrl Pts',(78.0890267165177,-7.24892221062687,
45.7159099220155));
#173068=CARTESIAN_POINT('Ctrl Pts',(78.1277061043518,-7.20962787585481,
45.7101446249022));
#173069=CARTESIAN_POINT('Ctrl Pts',(78.2212976394699,-7.11300224490283,
45.6962453540441));
#173070=CARTESIAN_POINT('Ctrl Pts',(78.2758699332725,-7.05533670756435,
45.688183904982));
#173071=CARTESIAN_POINT('Ctrl Pts',(78.5019693615782,-6.81079866175594,
45.6549504512769));
#173072=CARTESIAN_POINT('Ctrl Pts',(78.6672957519092,-6.61814177749665,
45.6310570574329));
#173073=CARTESIAN_POINT('Ctrl Pts',(79.0218762056326,-6.17254607224269,
45.5805028126085));
#173074=CARTESIAN_POINT('Ctrl Pts',(79.2070040643538,-5.91656513488964,
45.5546030126715));
#173075=CARTESIAN_POINT('Ctrl Pts',(79.5963033328536,-5.32250060373993,
45.5009455273585));
#173076=CARTESIAN_POINT('Ctrl Pts',(79.7934587919346,-4.98031078968498,
45.4743623312877));
#173077=CARTESIAN_POINT('Ctrl Pts',(80.0300897822527,-4.50900087827087,
45.4431062222859));
#173078=CARTESIAN_POINT('Ctrl Pts',(80.0873002315768,-4.38935747080625,
45.4356120499775));
#173079=CARTESIAN_POINT('Ctrl Pts',(80.1824841991048,-4.18003291620887,
45.4232544199594));
#173080=CARTESIAN_POINT('Ctrl Pts',(80.2215198621933,-4.09086411410551,
45.4182223792946));
#173081=CARTESIAN_POINT('Ctrl Pts',(80.3004557227389,-3.90338492548337,
45.4081250951556));
#173082=CARTESIAN_POINT('Ctrl Pts',(80.3401146218821,-3.80498337922563,
45.4030979567488));
#173083=CARTESIAN_POINT('Ctrl Pts',(80.443696349993,-3.53611623083272,45.3901014555969));
#173084=CARTESIAN_POINT('Ctrl Pts',(80.5046517516113,-3.36452678420184,
45.3826032536093));
#173085=CARTESIAN_POINT('Ctrl Pts',(80.666437599643,-2.86795784159947,45.3632047048561));
#173086=CARTESIAN_POINT('Ctrl Pts',(80.7558440426525,-2.53944392706786,
45.3531400102567));
#173087=CARTESIAN_POINT('Ctrl Pts',(80.9560349573233,-1.62961664659101,
45.3331920979815));
#173088=CARTESIAN_POINT('Ctrl Pts',(81.0335854643708,-1.04224134504529,
45.3289171756853));
#173089=CARTESIAN_POINT('Ctrl Pts',(81.0654036824948,-0.357498360043161,
45.3354955571808));
#173090=CARTESIAN_POINT('Ctrl Pts',(81.0685020617527,-0.263428123826516,
45.3366519086648));
#173091=CARTESIAN_POINT('Ctrl Pts',(81.0713983569315,-0.114381144895917,
45.3388958921633));
#173092=CARTESIAN_POINT('Ctrl Pts',(81.0720330285175,-0.0594234856816828,
45.3398119639789));
#173093=CARTESIAN_POINT('Ctrl Pts',(81.0724330554443,0.0495516206740589,
45.3418072576274));
#173094=CARTESIAN_POINT('Ctrl Pts',(81.0722131288569,0.103567233911748,
45.3428834527681));
#173095=CARTESIAN_POINT('Ctrl Pts',(81.0705168013786,0.247095979922438,
45.3459714278223));
#173096=CARTESIAN_POINT('Ctrl Pts',(81.0683094374653,0.336592762322675,
45.348132978835));
#173097=CARTESIAN_POINT('Ctrl Pts',(81.0487431222813,0.85794588733079,45.3620684487564));
#173098=CARTESIAN_POINT('Ctrl Pts',(81.0057467068751,1.28827508982859,45.3789321079492));
#173099=CARTESIAN_POINT('Ctrl Pts',(80.8451122782092,2.2716567509323,45.4286899802784));
#173100=CARTESIAN_POINT('Ctrl Pts',(80.7088560351132,2.82010142128822,45.4648015379234));
#173101=CARTESIAN_POINT('Ctrl Pts',(80.4801141151906,3.49803540474294,45.5195318653395));
#173102=CARTESIAN_POINT('Ctrl Pts',(80.4284144257382,3.64076963704903,45.531651699219));
#173103=CARTESIAN_POINT('Ctrl Pts',(80.3373501983133,3.87581996887589,45.5526078744458));
#173104=CARTESIAN_POINT('Ctrl Pts',(80.2997477373566,3.9688172657719,45.5611640196031));
#173105=CARTESIAN_POINT('Ctrl Pts',(80.2218120562113,4.15373527800768,45.5787119087024));
#173106=CARTESIAN_POINT('Ctrl Pts',(80.18148057449,4.24564472473005,45.5877030919483));
#173107=CARTESIAN_POINT('Ctrl Pts',(80.0764314682381,4.47581208897823,45.6109071506257));
#173108=CARTESIAN_POINT('Ctrl Pts',(80.0099762993214,4.61322156272542,45.6253952272206));
#173109=CARTESIAN_POINT('Ctrl Pts',(79.8561674963407,4.91395000955456,45.6585449214192));
#173110=CARTESIAN_POINT('Ctrl Pts',(79.7674132832127,5.07646659247095,45.6774298717117));
#173111=CARTESIAN_POINT('Ctrl Pts',(79.4412025781533,5.63712244572356,45.7461175224448));
#173112=CARTESIAN_POINT('Ctrl Pts',(79.1813617184851,6.02110686093215,45.7995737219165));
#173113=CARTESIAN_POINT('Ctrl Pts',(78.7349486830617,6.59295783336683,45.8906457718601));
#173114=CARTESIAN_POINT('Ctrl Pts',(78.5653234364098,6.79372679985372,45.9251128520068));
#173115=CARTESIAN_POINT('Ctrl Pts',(78.3336419229699,7.0473711167071,45.9722242433797));
#173116=CARTESIAN_POINT('Ctrl Pts',(78.278314298823,7.10650961381684,45.9834774628389));
#173117=CARTESIAN_POINT('Ctrl Pts',(78.1841694864696,7.20476075566679,46.0026386278442));
#173118=CARTESIAN_POINT('Ctrl Pts',(78.1457220480855,7.2442375080533,46.0104674737798));
#173119=CARTESIAN_POINT('Ctrl Pts',(78.0605077734062,7.33032133851806,46.0278293798582));
#173120=CARTESIAN_POINT('Ctrl Pts',(78.0136071090963,7.37678551210205,46.0373910596379));
#173121=CARTESIAN_POINT('Ctrl Pts',(77.8645888000426,7.52156273312126,46.0677825675462));
#173122=CARTESIAN_POINT('Ctrl Pts',(77.7608963602562,7.61816022583092,46.0889459516062));
#173123=CARTESIAN_POINT('Ctrl Pts',(77.4935181638413,7.85695106124518,46.1435002377902));
#173124=CARTESIAN_POINT('Ctrl Pts',(77.327278905375,7.99606068848886,46.1774025615863));
#173125=CARTESIAN_POINT('Ctrl Pts',(76.6592271683617,8.51938645610865,46.3133102269626));
#173126=CARTESIAN_POINT('Ctrl Pts',(76.1268313275312,8.86077207538095,46.4208209273963));
#173127=CARTESIAN_POINT('Ctrl Pts',(75.462403552005,9.20284155474791,46.5530073484307));
#173128=CARTESIAN_POINT('Ctrl Pts',(75.3574780453199,9.25454314075059,46.5738307837529));
#173129=CARTESIAN_POINT('Ctrl Pts',(75.1646140895626,9.34538758918787,46.6120120458151));
#173130=CARTESIAN_POINT('Ctrl Pts',(75.0769653843334,9.3851291014514,46.6293291046125));
#173131=CARTESIAN_POINT('Ctrl Pts',(74.8958182444689,9.46411517545122,46.6650486821665));
#173132=CARTESIAN_POINT('Ctrl Pts',(74.8022693298654,9.50321325397977,46.6834573866458));
#173133=CARTESIAN_POINT('Ctrl Pts',(74.55725120225,9.6012396066345,46.731577959967));
#173134=CARTESIAN_POINT('Ctrl Pts',(74.4049243066894,9.6578862018402,46.7614013117085));
#173135=CARTESIAN_POINT('Ctrl Pts',(74.0620045155435,9.77591051812833,46.8283565648095));
#173136=CARTESIAN_POINT('Ctrl Pts',(73.8708186192574,9.83530448577064,46.865561653675));
#173137=CARTESIAN_POINT('Ctrl Pts',(73.1665268381982,10.0309318259124,47.0022829474601));
#173138=CARTESIAN_POINT('Ctrl Pts',(72.6447153605288,10.1316131573217,47.1028989262433));
#173139=CARTESIAN_POINT('Ctrl Pts',(71.8729498075118,10.217053602988,47.2522040395169));
#173140=CARTESIAN_POINT('Ctrl Pts',(71.6274133368779,10.234991285751,47.2997855656282));
#173141=CARTESIAN_POINT('Ctrl Pts',(71.304819022534,10.2464759571301,47.362585122641));
#173142=CARTESIAN_POINT('Ctrl Pts',(71.2280947672074,10.2483126486633,47.3775423261758));
#173143=CARTESIAN_POINT('Ctrl Pts',(71.1009233288507,10.2498746063893,47.4023767836586));
#173144=CARTESIAN_POINT('Ctrl Pts',(71.0504825350468,10.2501077034053,47.4122382398805));
#173145=CARTESIAN_POINT('Ctrl Pts',(70.9428405032955,10.2497804659859,47.4333090402214));
#173146=CARTESIAN_POINT('Ctrl Pts',(70.8856424746946,10.2491095297945,47.4445208632596));
#173147=CARTESIAN_POINT('Ctrl Pts',(70.7198533539539,10.2457237335422,47.4770582848146));
#173148=CARTESIAN_POINT('Ctrl Pts',(70.611302479733,10.2417137813799,47.498411763524));
#173149=CARTESIAN_POINT('Ctrl Pts',(70.3547050221152,10.2279909974161,47.5489798691584));
#173150=CARTESIAN_POINT('Ctrl Pts',(70.206769271889,10.2167300939211,47.5782061388832));
#173151=CARTESIAN_POINT('Ctrl Pts',(69.59759798258,10.1565221055004,47.6987496720323));
#173152=CARTESIAN_POINT('Ctrl Pts',(69.1397770362672,10.0784273250427,47.7897815199368));
#173153=CARTESIAN_POINT('Ctrl Pts',(68.3282021921214,9.88042003111095,47.9509456965582));
#173154=CARTESIAN_POINT('Ctrl Pts',(67.9725823638028,9.77215906398969,48.0214959853037));
#173155=CARTESIAN_POINT('Ctrl Pts',(67.5002261775576,9.59885585308983,48.1149582809414));
#173156=CARTESIAN_POINT('Ctrl Pts',(67.3777217985953,9.55113345464636,48.1391757396126));
#173157=CARTESIAN_POINT('Ctrl Pts',(67.1673956328049,9.46436065962865,48.1807164467912));
#173158=CARTESIAN_POINT('Ctrl Pts',(67.0791430534159,9.42644795762594,48.1981351450922));
#173159=CARTESIAN_POINT('Ctrl Pts',(66.8963717601802,9.34478028907606,48.2341865470601));
#173160=CARTESIAN_POINT('Ctrl Pts',(66.8019588753419,9.30080693839525,48.2527964444137));
#173161=CARTESIAN_POINT('Ctrl Pts',(66.5477857521161,9.17754497026199,48.302867360851));
#173162=CARTESIAN_POINT('Ctrl Pts',(66.3893879552261,9.09541895339749,48.3340382871065));
#173163=CARTESIAN_POINT('Ctrl Pts',(65.8623604432592,8.80400872937472,48.4376981096682));
#173164=CARTESIAN_POINT('Ctrl Pts',(65.5045247173482,8.57538502364424,48.5079726220249));
#173165=CARTESIAN_POINT('Ctrl Pts',(64.8404989780704,8.08925542286462,48.6389697326557));
#173166=CARTESIAN_POINT('Ctrl Pts',(64.5330668281248,7.83484634717865,48.6999045323923));
#173167=CARTESIAN_POINT('Ctrl Pts',(64.1708356628121,7.49692398147681,48.7727180106483));
#173168=CARTESIAN_POINT('Ctrl Pts',(64.1013176395154,7.43018282468968,48.7867430798592));
#173169=CARTESIAN_POINT('Ctrl Pts',(63.9917481908598,7.32192982248355,48.8089445196392));
#173170=CARTESIAN_POINT('Ctrl Pts',(63.951086108794,7.28106182924346,48.8172054779518));
#173171=CARTESIAN_POINT('Ctrl Pts',(63.8686903595205,7.1968168791224,48.8339938244213));
#173172=CARTESIAN_POINT('Ctrl Pts',(63.8269896091492,7.15341031518989,48.8425164414961));
#173173=CARTESIAN_POINT('Ctrl Pts',(63.710660762785,7.03013627658631,48.8663599065718));
#173174=CARTESIAN_POINT('Ctrl Pts',(63.6369246993532,6.94941400674899,48.8815544183621));
#173175=CARTESIAN_POINT('Ctrl Pts',(63.4666498777151,6.75683149706457,48.9168118329063));
#173176=CARTESIAN_POINT('Ctrl Pts',(63.3712066905908,6.64400505344512,48.9367083126948));
#173177=CARTESIAN_POINT('Ctrl Pts',(62.9872207515609,6.16944616795585,49.0172253903589));
#173178=CARTESIAN_POINT('Ctrl Pts',(62.7207879085076,5.78992719006603,49.0742120869994));
#173179=CARTESIAN_POINT('Ctrl Pts',(62.3220330195843,5.1309880476925,49.1606714854087));
#173180=CARTESIAN_POINT('Ctrl Pts',(62.175076564144,4.86160630276654,49.1928830293485));
#173181=CARTESIAN_POINT('Ctrl Pts',(61.9854827624297,4.47379724987402,49.2348784796164));
#173182=CARTESIAN_POINT('Ctrl Pts',(61.9327210855891,4.36071964276109,49.2466222266294));
#173183=CARTESIAN_POINT('Ctrl Pts',(61.8428315735787,4.15858330130247,49.2667331614468));
#173184=CARTESIAN_POINT('Ctrl Pts',(61.8048822860286,4.06992278890669,49.2752597384238));
#173185=CARTESIAN_POINT('Ctrl Pts',(61.726966573758,3.8806073417182,49.2928463471193));
#173186=CARTESIAN_POINT('Ctrl Pts',(61.6873269232175,3.7798248783761,49.3018427562414));
#173187=CARTESIAN_POINT('Ctrl Pts',(61.5807314244082,3.49579852618635,49.3261831395961));
#173188=CARTESIAN_POINT('Ctrl Pts',(61.5173425880186,3.311207621457,49.3408353891317));
#173189=CARTESIAN_POINT('Ctrl Pts',(61.3820222761095,2.87765594773114,49.3726064190893));
#173190=CARTESIAN_POINT('Ctrl Pts',(61.3141143725114,2.62752498594417,49.3889544822805));
#173191=CARTESIAN_POINT('Ctrl Pts',(61.1886093822549,2.08575666178515,49.4203178232803));
#173192=CARTESIAN_POINT('Ctrl Pts',(61.1340113166221,1.79363551635217,49.4347771311325));
#173193=CARTESIAN_POINT('Ctrl Pts',(61.0434859330599,1.15967815393985,49.461271835961));
#173194=CARTESIAN_POINT('Ctrl Pts',(61.0118289147671,0.817566344443593,
49.472565466228));
#173195=CARTESIAN_POINT('Ctrl Pts',(60.9930270032638,0.37617628195623,49.4837164374098));
#173196=CARTESIAN_POINT('Ctrl Pts',(60.9902398662939,0.277849304918228,
49.485983528557));
#173197=CARTESIAN_POINT('Ctrl Pts',(60.988067133047,0.123669582752043,49.4892119583869));
#173198=CARTESIAN_POINT('Ctrl Pts',(60.9877318234734,0.0678392566848939,
49.4903139558446));
#173199=CARTESIAN_POINT('Ctrl Pts',(60.9878565297257,0.00800513799957859,
49.4914248599193));
#173200=CARTESIAN_POINT('Ctrl Pts',(60.9878671932475,0.00400256564559759,
49.4914988370101));
#173201=CARTESIAN_POINT('Ctrl Pts',(60.9878801781973,-3.30742432695422E-11,
49.4915724783198));
#173202=CARTESIAN_POINT('Origin',(69.7358040552328,8.67361737988404E-16,
40.0761166693274));
#173203=CARTESIAN_POINT('',(62.9451177993176,1.47451495458029E-14,41.4621534271586));
#173204=CARTESIAN_POINT('',(66.3565919271274,-6.,40.860618494437));
#173205=CARTESIAN_POINT('Ctrl Pts',(62.9451177993323,1.18985499391726E-10,
41.4621534276372));
#173206=CARTESIAN_POINT('Ctrl Pts',(64.8245030414636,-2.99999999999997,
42.1461937170664));
#173207=CARTESIAN_POINT('Ctrl Pts',(66.3565919272773,-6.00000000011892,
40.8606184948917));
#173208=CARTESIAN_POINT('',(73.179540182747,-6.,39.6575486289937));
#173209=CARTESIAN_POINT('Ctrl Pts',(66.3565919270745,-5.99999999999999,
40.8606184949275));
#173210=CARTESIAN_POINT('Ctrl Pts',(69.9417142331783,-6.00000000000001,
41.2438913179839));
#173211=CARTESIAN_POINT('Ctrl Pts',(73.1795401829645,-6.00000000000002,
39.6575486294364));
#173212=CARTESIAN_POINT('',(76.5910143105568,4.44197482702742E-16,39.056013696272));
#173213=CARTESIAN_POINT('Ctrl Pts',(73.1795401827616,-6.00000000011894,
39.6575486294722));
#173214=CARTESIAN_POINT('Ctrl Pts',(75.058925424893,-2.99999999999999,40.3415889189015));
#173215=CARTESIAN_POINT('Ctrl Pts',(76.5910143107067,1.1897463431604E-10,
39.0560136967267));
#173216=CARTESIAN_POINT('',(76.8756602645714,-2.05071913934279E-17,38.8171673812424));
#173217=CARTESIAN_POINT('',(76.8756602645714,-2.05071913934274E-17,38.8171673812424));
#173218=CARTESIAN_POINT('Origin',(69.7358040552328,8.67361737988404E-16,
40.0761166693274));
#173219=CARTESIAN_POINT('',(73.179540182747,6.,39.6575486289937));
#173220=CARTESIAN_POINT('Ctrl Pts',(76.5910143107067,-1.18906507354984E-10,
39.0560136967267));
#173221=CARTESIAN_POINT('Ctrl Pts',(75.058925424893,3.00000000000003,40.3415889189014));
#173222=CARTESIAN_POINT('Ctrl Pts',(73.1795401827617,6.00000000011895,39.6575486294722));
#173223=CARTESIAN_POINT('',(66.3565919271274,6.,40.860618494437));
#173224=CARTESIAN_POINT('Ctrl Pts',(73.1795401829645,6.,39.6575486294364));
#173225=CARTESIAN_POINT('Ctrl Pts',(69.9417142331783,6.00000000000001,41.2438913179839));
#173226=CARTESIAN_POINT('Ctrl Pts',(66.3565919270744,6.00000000000001,40.8606184949274));
#173227=CARTESIAN_POINT('Ctrl Pts',(66.3565919272774,6.0000000001189,40.8606184948917));
#173228=CARTESIAN_POINT('Ctrl Pts',(64.8245030414637,2.99999999999997,42.1461937170664));
#173229=CARTESIAN_POINT('Ctrl Pts',(62.9451177993323,-1.18964943843131E-10,
41.4621534276372));
#173230=CARTESIAN_POINT('Origin',(69.7358040552328,0.,40.0761166693274));
#173231=CARTESIAN_POINT('',(64.637845022461,-7.86451166255212,49.0198937666656));
#173232=CARTESIAN_POINT('Ctrl Pts',(60.9878801781973,-3.30742432695422E-11,
49.4915724783198));
#173233=CARTESIAN_POINT('Ctrl Pts',(60.9880401713394,-0.0493173303693729,
49.4924798445168));
#173234=CARTESIAN_POINT('Ctrl Pts',(60.9885525976134,-0.0986336473097226,
49.4933362314723));
#173235=CARTESIAN_POINT('Ctrl Pts',(60.9909257253593,-0.233976944592225,
49.4955439724581));
#173236=CARTESIAN_POINT('Ctrl Pts',(60.9935061966073,-0.31998919131596,
49.4967889330294));
#173237=CARTESIAN_POINT('Ctrl Pts',(61.001704578084,-0.513045452919115,
49.4992170694476));
#173238=CARTESIAN_POINT('Ctrl Pts',(61.0079122741947,-0.620055759686851,
49.500309829454));
#173239=CARTESIAN_POINT('Ctrl Pts',(61.0336081579724,-0.969346204667657,
49.5030194112285));
#173240=CARTESIAN_POINT('Ctrl Pts',(61.0599480389006,-1.21104866590326,
49.5035425669253));
#173241=CARTESIAN_POINT('Ctrl Pts',(61.1922679292548,-2.1261924181685,49.5000167941384));
#173242=CARTESIAN_POINT('Ctrl Pts',(61.3558488408635,-2.78950458864437,
49.4859063527375));
#173243=CARTESIAN_POINT('Ctrl Pts',(61.6293995057569,-3.56328691890951,
49.4540514957178));
#173244=CARTESIAN_POINT('Ctrl Pts',(61.6785649297539,-3.69393067546807,
49.4481242973407));
#173245=CARTESIAN_POINT('Ctrl Pts',(61.766486128001,-3.91401106741436,49.4371998973908));
#173246=CARTESIAN_POINT('Ctrl Pts',(61.8039016441018,-4.00397473164329,
49.4324624103401));
#173247=CARTESIAN_POINT('Ctrl Pts',(61.8835893431142,-4.18822590447127,
49.422197881793));
#173248=CARTESIAN_POINT('Ctrl Pts',(61.9260138406176,-4.2824338436548,49.4166409609042));
#173249=CARTESIAN_POINT('Ctrl Pts',(62.0410890950622,-4.52810486397312,
49.4013386018796));
#173250=CARTESIAN_POINT('Ctrl Pts',(62.1160134027525,-4.678440273996,49.3911514393713));
#173251=CARTESIAN_POINT('Ctrl Pts',(62.2634238141401,-4.95703732795004,
49.3707333809413));
#173252=CARTESIAN_POINT('Ctrl Pts',(62.3350625756721,-5.08571015610324,
49.3606639102153));
#173253=CARTESIAN_POINT('Ctrl Pts',(62.4388006637816,-5.26301523477087,
49.345903663078));
#173254=CARTESIAN_POINT('Ctrl Pts',(62.4686149550707,-5.312998716639,49.3416422986169));
#173255=CARTESIAN_POINT('Ctrl Pts',(62.5072139561134,-5.37648344525029,
49.3361022797283));
#173256=CARTESIAN_POINT('Ctrl Pts',(62.51561262016,-5.39022439117882,49.3348954770061));
#173257=CARTESIAN_POINT('Ctrl Pts',(62.691009452068,-5.67568523459674,49.3096649194389));
#173258=CARTESIAN_POINT('Ctrl Pts',(62.8703876086604,-5.93938633574773,
49.2833333046337));
#173259=CARTESIAN_POINT('Ctrl Pts',(63.2498229223662,-6.44493318261301,
49.2270615686531));
#173260=CARTESIAN_POINT('Ctrl Pts',(63.4493038913084,-6.68678916115698,
49.1972166504444));
#173261=CARTESIAN_POINT('Ctrl Pts',(63.7244571744634,-6.99077316725946,
49.1560595277977));
#173262=CARTESIAN_POINT('Ctrl Pts',(63.7904476578538,-7.06162529942621,
49.1461897604786));
#173263=CARTESIAN_POINT('Ctrl Pts',(63.8975013770108,-7.17333252315719,
49.1301934309612));
#173264=CARTESIAN_POINT('Ctrl Pts',(63.9379276847023,-7.21480264918602,
49.1241561256065));
#173265=CARTESIAN_POINT('Ctrl Pts',(64.0142732844073,-7.29179467432231,
49.1127641635071));
#173266=CARTESIAN_POINT('Ctrl Pts',(64.0501081576586,-7.32739909170935,
49.1074207417009));
#173267=CARTESIAN_POINT('Ctrl Pts',(64.1302141795215,-7.4058142832196,49.0954817591005));
#173268=CARTESIAN_POINT('Ctrl Pts',(64.1746105550878,-7.44849170397798,
49.0888687980882));
#173269=CARTESIAN_POINT('Ctrl Pts',(64.3554553547475,-7.61920543577403,
49.0619394356935));
#173270=CARTESIAN_POINT('Ctrl Pts',(64.4949922116416,-7.74383224910817,
49.0411787461335));
#173271=CARTESIAN_POINT('Ctrl Pts',(64.637845022461,-7.86451166255217,49.0198937666656));
#173272=CARTESIAN_POINT('',(61.9506556875214,-4.30478031493663,49.4937177486874));
#173273=CARTESIAN_POINT('Origin',(71.1115577432812,0.,47.8784035486295));
#173274=CARTESIAN_POINT('Ctrl Pts',(61.9506598557337,-4.30478938863868,
49.4937172065276));
#173275=CARTESIAN_POINT('Ctrl Pts',(61.9294009716217,-4.25851127052955,
49.4964823507224));
#173276=CARTESIAN_POINT('Ctrl Pts',(61.9084833788973,-4.21207392643947,
49.4991933391632));
#173277=CARTESIAN_POINT('Ctrl Pts',(61.8674561497903,-4.11916380707771,
49.5044907771788));
#173278=CARTESIAN_POINT('Ctrl Pts',(61.8473429944743,-4.07269417580616,
49.5070778015142));
#173279=CARTESIAN_POINT('Ctrl Pts',(61.7914021009595,-3.94079672650919,
49.5142441877163));
#173280=CARTESIAN_POINT('Ctrl Pts',(61.7563777950916,-3.85502670269385,
49.5186962557556));
#173281=CARTESIAN_POINT('Ctrl Pts',(61.667277166826,-3.62816619246239,49.5299253978876));
#173282=CARTESIAN_POINT('Ctrl Pts',(61.615126883088,-3.48632894604623,49.5363968482329));
#173283=CARTESIAN_POINT('Ctrl Pts',(61.3816664441308,-2.80571450758912,
49.564824352624));
#173284=CARTESIAN_POINT('Ctrl Pts',(61.2417600627997,-2.25353444009203,
49.5802036917875));
#173285=CARTESIAN_POINT('Ctrl Pts',(61.0762492875393,-1.26672398661516,
49.5929998798764));
#173286=CARTESIAN_POINT('Ctrl Pts',(61.0313922556877,-0.836811029042843,
49.5938184905104));
#173287=CARTESIAN_POINT('Ctrl Pts',(61.0096444362259,-0.319519193756273,
49.5883932902413));
#173288=CARTESIAN_POINT('Ctrl Pts',(61.0070935436993,-0.233603440773108,
49.5872805795056));
#173289=CARTESIAN_POINT('Ctrl Pts',(61.004747258745,-0.0984492968550968,
49.5851883899502));
#173290=CARTESIAN_POINT('Ctrl Pts',(61.0042402605943,-0.0492249582819704,
49.5843551161851));
#173291=CARTESIAN_POINT('Ctrl Pts',(61.0040805671216,3.48409058108532E-11,
49.583449449497));
#173292=CARTESIAN_POINT('Origin',(71.2118135654015,4.33680868994202E-16,
48.4469825699312));
#173293=CARTESIAN_POINT('',(62.4496382053723,-6.991174202171E-16,52.0228437193745));
#173294=CARTESIAN_POINT('Origin',(71.5591099207353,4.33680868994202E-16,
50.4165980759556));
#173295=CARTESIAN_POINT('',(62.1023418500385,-6.991174202171E-16,50.0532282133501));
#173296=CARTESIAN_POINT('',(62.1023418500385,-6.991174202171E-16,50.0532282133501));
#173297=CARTESIAN_POINT('',(80.3212852807645,1.19403062916867E-15,46.8407369265124));
#173298=CARTESIAN_POINT('Origin',(71.2118135654015,4.33680868994202E-16,
48.4469825699312));
#173299=CARTESIAN_POINT('Origin',(71.2118135654015,4.33680868994202E-16,
48.4469825699312));
#173300=CARTESIAN_POINT('Origin',(71.5591099207353,0.,50.4165980759556));
#173301=CARTESIAN_POINT('',(61.0735209929348,-1.34711147906209E-15,54.2963435363159));
#173302=CARTESIAN_POINT('Origin',(71.9064062760691,0.,52.38621358198));
#173303=CARTESIAN_POINT('',(60.726224637601,-1.34711147906209E-15,52.3267280302915));
#173304=CARTESIAN_POINT('',(60.726224637601,-1.34711147906209E-15,52.3267280302915));
#173305=CARTESIAN_POINT('Origin',(71.5591099207353,0.,50.4165980759556));
#173306=CARTESIAN_POINT('Origin',(71.9064062760691,0.,52.38621358198));
#173307=CARTESIAN_POINT('',(63.2427116913412,-1.12055182121983E-15,55.9447099136567));
#173308=CARTESIAN_POINT('Origin',(72.2537026314029,0.,54.3558290880045));
#173309=CARTESIAN_POINT('',(62.8954153360073,-1.12055182121983E-15,53.9750944076322));
#173310=CARTESIAN_POINT('',(62.8954153360073,-1.12055182121983E-15,53.9750944076322));
#173311=CARTESIAN_POINT('Origin',(71.9064062760691,0.,52.38621358198));
#173312=CARTESIAN_POINT('Origin',(72.2537026314029,-4.33680868994202E-16,
54.3558290880045));
#173313=CARTESIAN_POINT('',(72.8461248809557,9.99946181761383,58.3130755089793));
#173314=CARTESIAN_POINT('Ctrl Pts',(63.0153743226244,-3.90012641998867E-11,
59.5503705382064));
#173315=CARTESIAN_POINT('Ctrl Pts',(63.0153972406607,-0.0127238816044014,
59.5505005128487));
#173316=CARTESIAN_POINT('Ctrl Pts',(63.015444218918,-0.025447716762289,
59.5506270909235));
#173317=CARTESIAN_POINT('Ctrl Pts',(63.015670373446,-0.0659565906910079,
59.5510192008863));
#173318=CARTESIAN_POINT('Ctrl Pts',(63.0159402079255,-0.0937410855028063,
59.5512718523828));
#173319=CARTESIAN_POINT('Ctrl Pts',(63.017126433562,-0.179454306078677,
59.5520003585878));
#173320=CARTESIAN_POINT('Ctrl Pts',(63.0184266650033,-0.237376994939163,
59.5524209190357));
#173321=CARTESIAN_POINT('Ctrl Pts',(63.0311791315022,-0.648040738871901,
59.554880622942));
#173322=CARTESIAN_POINT('Ctrl Pts',(63.060603601808,-0.999995108331238,
59.5542488690691));
#173323=CARTESIAN_POINT('Ctrl Pts',(63.1914958773353,-1.9594219188347,59.543981049886));
#173324=CARTESIAN_POINT('Ctrl Pts',(63.3299820083306,-2.56022648173973,
59.5279430870644));
#173325=CARTESIAN_POINT('Ctrl Pts',(63.577938413814,-3.31532630551769,59.4937772209545));
#173326=CARTESIAN_POINT('Ctrl Pts',(63.6385814296694,-3.48467194886097,
59.4851690595328));
#173327=CARTESIAN_POINT('Ctrl Pts',(63.7276922896354,-3.71409752939761,
59.4721915985195));
#173328=CARTESIAN_POINT('Ctrl Pts',(63.7523091857069,-3.77567839889446,
59.4685762666482));
#173329=CARTESIAN_POINT('Ctrl Pts',(63.7943152147813,-3.87783776628032,
59.4623578939484));
#173330=CARTESIAN_POINT('Ctrl Pts',(63.8113696545304,-3.91855553505762,
59.4598204580738));
#173331=CARTESIAN_POINT('Ctrl Pts',(63.8455275209278,-3.99863449379825,
59.4547135931825));
#173332=CARTESIAN_POINT('Ctrl Pts',(63.8626161277331,-4.03800115895169,
59.4521470542971));
#173333=CARTESIAN_POINT('Ctrl Pts',(63.9042491226319,-4.13226440080662,
59.445866798204));
#173334=CARTESIAN_POINT('Ctrl Pts',(63.9290322945844,-4.18705052954745,
59.442106218525));
#173335=CARTESIAN_POINT('Ctrl Pts',(64.0178223892747,-4.37876096587211,
59.428558368047));
#173336=CARTESIAN_POINT('Ctrl Pts',(64.0843950554685,-4.51443814573505,
59.4182680211522));
#173337=CARTESIAN_POINT('Ctrl Pts',(64.2577840528361,-4.84862924827669,
59.3911736943488));
#173338=CARTESIAN_POINT('Ctrl Pts',(64.3682301684812,-5.04510610853753,
59.3736634282429));
#173339=CARTESIAN_POINT('Ctrl Pts',(64.7157075033443,-5.61738396006518,
59.3180188526635));
#173340=CARTESIAN_POINT('Ctrl Pts',(64.9709856154607,-5.98109874914044,
59.2764334550044));
#173341=CARTESIAN_POINT('Ctrl Pts',(65.4055645901478,-6.52006368772027,
59.2056383501741));
#173342=CARTESIAN_POINT('Ctrl Pts',(65.5688871659162,-6.70777928239044,
59.1790381863562));
#173343=CARTESIAN_POINT('Ctrl Pts',(65.7724134155743,-6.92469182104557,
59.1460772755362));
#173344=CARTESIAN_POINT('Ctrl Pts',(65.8060762427447,-6.96004241693961,
59.140631466992));
#173345=CARTESIAN_POINT('Ctrl Pts',(65.8590087100124,-7.01481347859254,
59.1320793091153));
#173346=CARTESIAN_POINT('Ctrl Pts',(65.8781019561053,-7.03440701784639,
59.1289966624021));
#173347=CARTESIAN_POINT('Ctrl Pts',(65.9120948662297,-7.06900296197743,
59.1235127045085));
#173348=CARTESIAN_POINT('Ctrl Pts',(65.9269621141047,-7.08403741921878,
59.1211156858566));
#173349=CARTESIAN_POINT('Ctrl Pts',(65.9628921482931,-7.12013975848987,
59.1153261899299));
#173350=CARTESIAN_POINT('Ctrl Pts',(65.9840014881413,-7.14115991619729,
59.1119275771374));
#173351=CARTESIAN_POINT('Ctrl Pts',(66.0494881321774,-7.20578455083538,
59.1013919552325));
#173352=CARTESIAN_POINT('Ctrl Pts',(66.0941781085156,-7.24906319306956,
59.0942130436402));
#173353=CARTESIAN_POINT('Ctrl Pts',(66.3225891886383,-7.4661314114206,59.0575643349633));
#173354=CARTESIAN_POINT('Ctrl Pts',(66.5124360680845,-7.63319524967299,
59.0272396712087));
#173355=CARTESIAN_POINT('Ctrl Pts',(67.1810548013945,-8.17764157613828,
58.9204019059097));
#173356=CARTESIAN_POINT('Ctrl Pts',(67.687749069195,-8.51764354585437,58.839288498054));
#173357=CARTESIAN_POINT('Ctrl Pts',(68.3717923878515,-8.89008177659352,
58.7280371590308));
#173358=CARTESIAN_POINT('Ctrl Pts',(68.523824359906,-8.96779965280919,58.703216448197));
#173359=CARTESIAN_POINT('Ctrl Pts',(68.7358647752087,-9.06931987054389,
58.6684580987205));
#173360=CARTESIAN_POINT('Ctrl Pts',(68.7942463895949,-9.09656908715674,
58.6588737037093));
#173361=CARTESIAN_POINT('Ctrl Pts',(68.8884982994032,-9.13943631771255,
58.6433774281439));
#173362=CARTESIAN_POINT('Ctrl Pts',(68.9242060720533,-9.1554198934331,58.6375013119101));
#173363=CARTESIAN_POINT('Ctrl Pts',(68.9985283346228,-9.18815626502272,
58.6252598037237));
#173364=CARTESIAN_POINT('Ctrl Pts',(69.0371565514239,-9.20487475187628,
58.6188913202396));
#173365=CARTESIAN_POINT('Ctrl Pts',(69.1285119656597,-9.24371779764268,
58.6038156489328));
#173366=CARTESIAN_POINT('Ctrl Pts',(69.1813247014005,-9.26562972817009,
58.5950892397882));
#173367=CARTESIAN_POINT('Ctrl Pts',(69.3586907108283,-9.33740673626942,
58.5657459079227));
#173368=CARTESIAN_POINT('Ctrl Pts',(69.4840492563005,-9.38516584059354,
58.5449464070969));
#173369=CARTESIAN_POINT('Ctrl Pts',(69.7880668066933,-9.49389191081518,
58.4943704100662));
#173370=CARTESIAN_POINT('Ctrl Pts',(69.9675568819216,-9.55228305330136,
58.4644011635447));
#173371=CARTESIAN_POINT('Ctrl Pts',(70.7867530700148,-9.79278136731914,
58.3272347957418));
#173372=CARTESIAN_POINT('Ctrl Pts',(71.4417459459794,-9.91427382230702,
58.2163822146416));
#173373=CARTESIAN_POINT('Ctrl Pts',(72.2909494508674,-9.98325294556837,
58.073953998191));
#173374=CARTESIAN_POINT('Ctrl Pts',(72.4783440086267,-9.99302939405581,
58.0426137861576));
#173375=CARTESIAN_POINT('Ctrl Pts',(72.7092993085787,-9.99838801357882,
58.0041839749464));
#173376=CARTESIAN_POINT('Ctrl Pts',(72.7526810991047,-9.99910430876741,
57.9969739744684));
#173377=CARTESIAN_POINT('Ctrl Pts',(72.8208982492309,-9.99977439078064,
57.985651176986));
#173378=CARTESIAN_POINT('Ctrl Pts',(72.8457301582975,-9.99992326850401,
57.9815326198913));
#173379=CARTESIAN_POINT('Ctrl Pts',(72.8899657043635,-10.0000191893599,
57.974201626971));
#173380=CARTESIAN_POINT('Ctrl Pts',(72.9093687778549,-10.0000032472533,
57.9709880394958));
#173381=CARTESIAN_POINT('Ctrl Pts',(72.9560850226036,-9.99982518655341,
57.9632555469892));
#173382=CARTESIAN_POINT('Ctrl Pts',(72.9833980664459,-9.99960612928655,
57.95873858226));
#173383=CARTESIAN_POINT('Ctrl Pts',(73.0673484280767,-9.99857949922355,
57.9448664145709));
#173384=CARTESIAN_POINT('Ctrl Pts',(73.1239820394017,-9.99739259086614,
57.9355239956593));
#173385=CARTESIAN_POINT('Ctrl Pts',(73.6369106535519,-9.98216442695471,
57.8510368702289));
#173386=CARTESIAN_POINT('Ctrl Pts',(74.0918896743786,-9.93654433063337,
57.776979615097));
#173387=CARTESIAN_POINT('Ctrl Pts',(75.1339980204783,-9.75747861245336,
57.6075192203945));
#173388=CARTESIAN_POINT('Ctrl Pts',(75.7155099326642,-9.60128775932434,
57.5130253832674));
#173389=CARTESIAN_POINT('Ctrl Pts',(76.3817355004841,-9.35460524953656,
57.4038240322294));
#173390=CARTESIAN_POINT('Ctrl Pts',(76.4835659284401,-9.31494784018957,
57.3871091765992));
#173391=CARTESIAN_POINT('Ctrl Pts',(76.6335636359693,-9.25361818247504,
57.3624515261964));
#173392=CARTESIAN_POINT('Ctrl Pts',(76.6822450676087,-9.23325265268029,
57.3544431961951));
#173393=CARTESIAN_POINT('Ctrl Pts',(76.7688873856061,-9.1961802856855,57.3401799165044));
#173394=CARTESIAN_POINT('Ctrl Pts',(76.8069101801534,-9.17962452221205,
57.3339169693134));
#173395=CARTESIAN_POINT('Ctrl Pts',(76.8872849321029,-9.14401880221152,
57.3206705985712));
#173396=CARTESIAN_POINT('Ctrl Pts',(76.9296093820722,-9.12490792130417,
57.3136908201104));
#173397=CARTESIAN_POINT('Ctrl Pts',(77.0429865065423,-9.07274046470455,
57.294982168038));
#173398=CARTESIAN_POINT('Ctrl Pts',(77.1137856280795,-9.03912897268019,
57.2832871923927));
#173399=CARTESIAN_POINT('Ctrl Pts',(77.5054901203791,-8.84737815138417,
57.2185199911168));
#173400=CARTESIAN_POINT('Ctrl Pts',(77.8181007715108,-8.67253810194579,
57.1665794757874));
#173401=CARTESIAN_POINT('Ctrl Pts',(78.4865875535025,-8.24917525748617,
57.0553471649651));
#173402=CARTESIAN_POINT('Ctrl Pts',(78.8370898372806,-7.99335053134205,
56.9969090578562));
#173403=CARTESIAN_POINT('Ctrl Pts',(79.3494357490841,-7.56514391086097,
56.9122457696215));
#173404=CARTESIAN_POINT('Ctrl Pts',(79.523584019982,-7.40881765385398,56.8836243759743));
#173405=CARTESIAN_POINT('Ctrl Pts',(79.7268934068559,-7.21294877118822,
56.8505570511511));
#173406=CARTESIAN_POINT('Ctrl Pts',(79.761381174521,-7.17923736371063,56.8449604366153));
#173407=CARTESIAN_POINT('Ctrl Pts',(79.8149575964137,-7.12610208360609,
56.8362879582245));
#173408=CARTESIAN_POINT('Ctrl Pts',(79.8342105098096,-7.10685082368393,
56.8331759397018));
#173409=CARTESIAN_POINT('Ctrl Pts',(79.8682893117592,-7.0724951025603,56.8276758506217));
#173410=CARTESIAN_POINT('Ctrl Pts',(79.8831457204213,-7.05742247501516,
56.825281011699));
#173411=CARTESIAN_POINT('Ctrl Pts',(79.9189277391044,-7.02088820525327,
56.8195198916435));
#173412=CARTESIAN_POINT('Ctrl Pts',(79.9398056652184,-6.99937859483033,
56.8161641379583));
#173413=CARTESIAN_POINT('Ctrl Pts',(80.0043851385759,-6.93224333926219,
56.8058011541814));
#173414=CARTESIAN_POINT('Ctrl Pts',(80.0477566006229,-6.88629127384611,
56.7988658139896));
#173415=CARTESIAN_POINT('Ctrl Pts',(80.2681868436911,-6.64826358789515,
56.7637317615667));
#173416=CARTESIAN_POINT('Ctrl Pts',(80.4382129438355,-6.44959649984763,
56.7370123858501));
#173417=CARTESIAN_POINT('Ctrl Pts',(81.0118714857229,-5.72354607914022,
56.6477165955925));
#173418=CARTESIAN_POINT('Ctrl Pts',(81.3711484916976,-5.16233930121776,
56.593297712963));
#173419=CARTESIAN_POINT('Ctrl Pts',(81.7301171758017,-4.45584920586747,
56.5392293896068));
#173420=CARTESIAN_POINT('Ctrl Pts',(81.7855469201543,-4.34143560350729,
56.5308967250654));
#173421=CARTESIAN_POINT('Ctrl Pts',(81.8606013483149,-4.17872253269041,
56.5196337823115));
#173422=CARTESIAN_POINT('Ctrl Pts',(81.8820352272707,-4.13129108731475,
56.5164198239708));
#173423=CARTESIAN_POINT('Ctrl Pts',(81.9188526854303,-4.04810309294576,
56.5109034407096));
#173424=CARTESIAN_POINT('Ctrl Pts',(81.9343980121356,-4.01242106548909,
56.5085756772287));
#173425=CARTESIAN_POINT('Ctrl Pts',(81.9666698308304,-3.93715668223187,
56.5037462684997));
#173426=CARTESIAN_POINT('Ctrl Pts',(81.983350805942,-3.89755521620216,56.5012517488476));
#173427=CARTESIAN_POINT('Ctrl Pts',(82.0228732947852,-3.80202205813339,
56.4953457956932));
#173428=CARTESIAN_POINT('Ctrl Pts',(82.0454668398663,-3.74598724189699,
56.4919732041538));
#173429=CARTESIAN_POINT('Ctrl Pts',(82.1232852072188,-3.54786746878617,
56.4803707974395));
#173430=CARTESIAN_POINT('Ctrl Pts',(82.1757966107307,-3.40471499598959,
56.4725665516287));
#173431=CARTESIAN_POINT('Ctrl Pts',(82.2974089349353,-3.04839754066916,
56.4545746395008));
#173432=CARTESIAN_POINT('Ctrl Pts',(82.362702218747,-2.83399194437994,56.4449903211823));
#173433=CARTESIAN_POINT('Ctrl Pts',(82.5133755507188,-2.27292092536084,
56.4231974807356));
#173434=CARTESIAN_POINT('Ctrl Pts',(82.5876402737568,-1.92353356160316,
56.4128057182158));
#173435=CARTESIAN_POINT('Ctrl Pts',(82.6717518192979,-1.39111488943614,
56.4021240616837));
#173436=CARTESIAN_POINT('Ctrl Pts',(82.6953154067304,-1.21059315410368,
56.3993835526276));
#173437=CARTESIAN_POINT('Ctrl Pts',(82.7408522150387,-0.769879807381216,
56.3949493823501));
#173438=CARTESIAN_POINT('Ctrl Pts',(82.7576795567097,-0.50928211026459,
56.3942270198793));
#173439=CARTESIAN_POINT('Ctrl Pts',(82.7656342431276,-0.204847392485989,
56.3957898248367));
#173440=CARTESIAN_POINT('Ctrl Pts',(82.7664924732408,-0.161355025493206,
56.3960703577545));
#173441=CARTESIAN_POINT('Ctrl Pts',(82.7674377811045,-0.0905000121902342,
56.3966220412924));
#173442=CARTESIAN_POINT('Ctrl Pts',(82.767692825144,-0.0631399135396372,
56.3968580573713));
#173443=CARTESIAN_POINT('Ctrl Pts',(82.7679532228835,-0.0140427354381262,
56.3973232171349));
#173444=CARTESIAN_POINT('Ctrl Pts',(82.7679991279918,0.00769383312288637,
56.3975438216474));
#173445=CARTESIAN_POINT('Ctrl Pts',(82.7679472374795,0.0557499153964174,
56.3980640098788));
#173446=CARTESIAN_POINT('Ctrl Pts',(82.7678170962327,0.0820689182735145,
56.3983703916125));
#173447=CARTESIAN_POINT('Ctrl Pts',(82.7671393580162,0.158987447891594,
56.3993280919463));
#173448=CARTESIAN_POINT('Ctrl Pts',(82.7663173891197,0.209583024122863,
56.4000368302565));
#173449=CARTESIAN_POINT('Ctrl Pts',(82.7542402509525,0.719447650404466,
56.4079605514154));
#173450=CARTESIAN_POINT('Ctrl Pts',(82.7123557420851,1.17735529161294,56.4214469228521));
#173451=CARTESIAN_POINT('Ctrl Pts',(82.540832122938,2.24635608924051,56.4661470751882));
#173452=CARTESIAN_POINT('Ctrl Pts',(82.3854851470434,2.85121668799052,56.501820406516));
#173453=CARTESIAN_POINT('Ctrl Pts',(82.1386395300699,3.54000434630717,56.553781145612));
#173454=CARTESIAN_POINT('Ctrl Pts',(82.1001676646831,3.64209240272902,56.5617916307335));
#173455=CARTESIAN_POINT('Ctrl Pts',(82.0405538098305,3.79280040737901,56.5740785028626));
#173456=CARTESIAN_POINT('Ctrl Pts',(82.0206709476821,3.84192555607953,56.5781573750507));
#173457=CARTESIAN_POINT('Ctrl Pts',(81.9844173075688,3.92949900162393,56.5855611586151));
#173458=CARTESIAN_POINT('Ctrl Pts',(81.9681928481918,3.968008425401,56.5888631306304));
#173459=CARTESIAN_POINT('Ctrl Pts',(81.9332342088384,4.04955745250443,56.5959540893212));
#173460=CARTESIAN_POINT('Ctrl Pts',(81.9144378849117,4.09256846232226,56.5997527901644));
#173461=CARTESIAN_POINT('Ctrl Pts',(81.8629634791182,4.20813908897189,56.6101190986596));
#173462=CARTESIAN_POINT('Ctrl Pts',(81.829725698529,4.28043771285296,56.6167743630153));
#173463=CARTESIAN_POINT('Ctrl Pts',(81.635620859875,4.68974778331293,56.6554326229452));
#173464=CARTESIAN_POINT('Ctrl Pts',(81.456987925288,5.01773594004858,56.6902110873017));
#173465=CARTESIAN_POINT('Ctrl Pts',(81.0153001055961,5.73075077929968,56.7750684403635));
#173466=CARTESIAN_POINT('Ctrl Pts',(80.7428502346743,6.10872866637621,56.8266866698138));
#173467=CARTESIAN_POINT('Ctrl Pts',(80.3215825979059,6.61457358668624,56.9066799010964));
#173468=CARTESIAN_POINT('Ctrl Pts',(80.1935151813372,6.75954443633545,56.9310229636541));
#173469=CARTESIAN_POINT('Ctrl Pts',(80.0297244066458,6.93441398475723,56.9622766104188));
#173470=CARTESIAN_POINT('Ctrl Pts',(79.9978327158827,6.967989670514,56.9683674412743));
#173471=CARTESIAN_POINT('Ctrl Pts',(79.9473384010373,7.02041215847785,56.9780212550551));
#173472=CARTESIAN_POINT('Ctrl Pts',(79.9288898550424,7.03941263564539,56.9815504623455));
#173473=CARTESIAN_POINT('Ctrl Pts',(79.8938406783404,7.07522297942018,56.9882597139624));
#173474=CARTESIAN_POINT('Ctrl Pts',(79.8772554062885,7.09204801206173,56.9914363915921));
#173475=CARTESIAN_POINT('Ctrl Pts',(79.8377102518846,7.13187970416904,56.9990149017995));
#173476=CARTESIAN_POINT('Ctrl Pts',(79.8146982451438,7.1548320385734,57.0034282669222));
#173477=CARTESIAN_POINT('Ctrl Pts',(79.7362675129167,7.23229489000526,57.0184800924012));
#173478=CARTESIAN_POINT('Ctrl Pts',(79.6803322742601,7.28625638218252,57.0292314663774));
#173479=CARTESIAN_POINT('Ctrl Pts',(79.5410759231692,7.41747193530605,57.0560274184527));
#173480=CARTESIAN_POINT('Ctrl Pts',(79.4570638547685,7.49394657412402,57.0722183209985));
#173481=CARTESIAN_POINT('Ctrl Pts',(79.0872997516207,7.81906044935153,57.1435280569425));
#173482=CARTESIAN_POINT('Ctrl Pts',(78.7889709618237,8.05235200373957,57.2011712390321));
#173483=CARTESIAN_POINT('Ctrl Pts',(78.1174129528399,8.517604868232,57.3302768838052));
#173484=CARTESIAN_POINT('Ctrl Pts',(77.7405971542483,8.74279654721798,57.4023171101932));
#173485=CARTESIAN_POINT('Ctrl Pts',(77.2559807990117,8.98974113405135,57.4940844809444));
#173486=CARTESIAN_POINT('Ctrl Pts',(77.1610063170831,9.03620483700701,57.512030631217));
#173487=CARTESIAN_POINT('Ctrl Pts',(77.0182703926689,9.10317545515927,57.5389429559715));
#173488=CARTESIAN_POINT('Ctrl Pts',(76.9710594998861,9.1248668231769,57.5478349740397));
#173489=CARTESIAN_POINT('Ctrl Pts',(76.8860420719781,9.16310689984286,57.5638308016666));
#173490=CARTESIAN_POINT('Ctrl Pts',(76.8482983669322,9.17979569101789,57.5709262592174));
#173491=CARTESIAN_POINT('Ctrl Pts',(76.7676386295085,9.2148482130727,57.5860769369247));
#173492=CARTESIAN_POINT('Ctrl Pts',(76.7246948348139,9.23314390965153,57.5941357238436));
#173493=CARTESIAN_POINT('Ctrl Pts',(76.60789671928,9.28191352929628,57.6160337185872));
#173494=CARTESIAN_POINT('Ctrl Pts',(76.5338007459809,9.31178522144678,57.6299038641073));
#173495=CARTESIAN_POINT('Ctrl Pts',(76.1076484158523,9.47750842145583,57.7095554523373));
#173496=CARTESIAN_POINT('Ctrl Pts',(75.7484278885031,9.59361138243197,57.7762128644523));
#173497=CARTESIAN_POINT('Ctrl Pts',(74.8034124781921,9.83925991498714,57.9508388607145));
#173498=CARTESIAN_POINT('Ctrl Pts',(74.2108875082253,9.93585627851298,58.0595775716456));
#173499=CARTESIAN_POINT('Ctrl Pts',(73.5345862939291,9.9825167094355,58.1848171674148));
#173500=CARTESIAN_POINT('Ctrl Pts',(73.4555248144918,9.98699671540131,58.1994767589549));
#173501=CARTESIAN_POINT('Ctrl Pts',(73.288548965615,9.99440248209955,58.2304880626753));
#173502=CARTESIAN_POINT('Ctrl Pts',(73.2006327068963,9.99710044370478,58.2468457342875));
#173503=CARTESIAN_POINT('Ctrl Pts',(73.0799243445904,9.99915650863733,58.2693555841932));
#173504=CARTESIAN_POINT('Ctrl Pts',(73.0471476756212,9.99954803125916,58.2754729715675));
#173505=CARTESIAN_POINT('Ctrl Pts',(72.9923354438664,9.99992389894518,58.2857123252784));
#173506=CARTESIAN_POINT('Ctrl Pts',(72.970300205909,9.99999963373074,58.2898311889631));
#173507=CARTESIAN_POINT('Ctrl Pts',(72.9316375680396,10.0000002740669,58.2970626910476));
#173508=CARTESIAN_POINT('Ctrl Pts',(72.9150100544956,9.99995763056317,58.3001742181077));
#173509=CARTESIAN_POINT('Ctrl Pts',(72.8809597342367,9.99978240993586,58.3065490651667));
#173510=CARTESIAN_POINT('Ctrl Pts',(72.8635468579032,9.99964571039881,58.3098106669871));
#173511=CARTESIAN_POINT('Ctrl Pts',(72.8461248809557,9.99946181761384,58.3130755089793));
#173512=CARTESIAN_POINT('',(75.0041293598347,9.77968000307984,57.9325610948633));
#173513=CARTESIAN_POINT('Origin',(72.9482953420705,-4.33680868994202E-16,
58.2950601000533));
#173514=CARTESIAN_POINT('Ctrl Pts',(75.0041293598347,9.77968000307985,57.9325610948633));
#173515=CARTESIAN_POINT('Ctrl Pts',(75.4467731959013,9.68351044596169,57.8484084812634));
#173516=CARTESIAN_POINT('Ctrl Pts',(75.8823845795871,9.55632191769558,57.7657085087382));
#173517=CARTESIAN_POINT('Ctrl Pts',(76.4137973744841,9.35987501664702,57.6653655792823));
#173518=CARTESIAN_POINT('Ctrl Pts',(76.5190230165497,9.31888043583612,57.6455221604581));
#173519=CARTESIAN_POINT('Ctrl Pts',(76.6728943200235,9.25582894320786,57.6165442198741));
#173520=CARTESIAN_POINT('Ctrl Pts',(76.7220899015498,9.23519660415285,57.6072853543921));
#173521=CARTESIAN_POINT('Ctrl Pts',(76.8091783031061,9.19782827926034,57.5909053484051));
#173522=CARTESIAN_POINT('Ctrl Pts',(76.8471362271565,9.18125383967444,57.5837696068368));
#173523=CARTESIAN_POINT('Ctrl Pts',(76.9268996140984,9.14581800647895,57.5687822374121));
#173524=CARTESIAN_POINT('Ctrl Pts',(76.9686808112055,9.12690222134181,57.5609359660551));
#173525=CARTESIAN_POINT('Ctrl Pts',(77.0794756270088,9.07579704194072,57.5401405485904));
#173526=CARTESIAN_POINT('Ctrl Pts',(77.1482563307976,9.04308963391436,57.5272425661963));
#173527=CARTESIAN_POINT('Ctrl Pts',(77.4705124676917,8.88519716572557,57.4668634272212));
#173528=CARTESIAN_POINT('Ctrl Pts',(77.7190181804325,8.74977280691174,57.4204584101275));
#173529=CARTESIAN_POINT('Ctrl Pts',(78.030189700602,8.56227075632774,57.3624489883775));
#173530=CARTESIAN_POINT('Ctrl Pts',(78.0984063294809,8.52001558487187,57.3497377317351));
#173531=CARTESIAN_POINT('Ctrl Pts',(78.5379996776848,8.24019661230819,57.2678455490562));
#173532=CARTESIAN_POINT('Ctrl Pts',(78.8939109332315,7.97842237061735,57.2016625143765));
#173533=CARTESIAN_POINT('Ctrl Pts',(79.3476775541994,7.5950744599062,57.1165645447774));
#173534=CARTESIAN_POINT('Ctrl Pts',(79.4617500686661,7.49408041115362,57.0951020493699));
#173535=CARTESIAN_POINT('Ctrl Pts',(79.6434067570898,7.32557470952058,57.0607515561276));
#173536=CARTESIAN_POINT('Ctrl Pts',(79.7124128243414,7.25967526053967,57.0476603624098));
#173537=CARTESIAN_POINT('Ctrl Pts',(79.8058152013125,7.1678479967598,57.0298693125774));
#173538=CARTESIAN_POINT('Ctrl Pts',(79.831033463482,7.14278536173196,57.0250584543731));
#173539=CARTESIAN_POINT('Ctrl Pts',(79.8731595354281,7.10046388306709,57.0170088902476));
#173540=CARTESIAN_POINT('Ctrl Pts',(79.8901396147404,7.08327920502248,57.0137606339998));
#173541=CARTESIAN_POINT('Ctrl Pts',(79.9247720949334,7.04797082913142,57.0071276940998));
#173542=CARTESIAN_POINT('Ctrl Pts',(79.9424182806319,7.02984123948933,57.0037438572943));
#173543=CARTESIAN_POINT('Ctrl Pts',(79.9884130416565,6.98222137726603,56.9949133561584));
#173544=CARTESIAN_POINT('Ctrl Pts',(80.0166497030171,6.9526209096185,56.9894816561048));
#173545=CARTESIAN_POINT('Ctrl Pts',(80.1346281038101,6.82739516097374,56.9667451047949));
#173546=CARTESIAN_POINT('Ctrl Pts',(80.2226658552105,6.73013999979803,56.9496759291628));
#173547=CARTESIAN_POINT('Ctrl Pts',(80.6517489159532,6.23676348029673,56.8660676926006));
#173548=CARTESIAN_POINT('Ctrl Pts',(80.9633740470488,5.81539628222818,56.8040398013639));
#173549=CARTESIAN_POINT('Ctrl Pts',(81.4453105520073,5.04364709862668,56.7073943844033));
#173550=CARTESIAN_POINT('Ctrl Pts',(81.6308100979954,4.70447436208174,56.6699331639591));
#173551=CARTESIAN_POINT('Ctrl Pts',(81.8308315451034,4.28277923689722,56.6294054265953));
#173552=CARTESIAN_POINT('Ctrl Pts',(81.8643070574446,4.20997536880926,56.6226166543153));
#173553=CARTESIAN_POINT('Ctrl Pts',(81.9160634039712,4.09378520405455,56.6121113516085));
#173554=CARTESIAN_POINT('Ctrl Pts',(81.9349106545668,4.05066516732619,56.6082837483891));
#173555=CARTESIAN_POINT('Ctrl Pts',(81.9699159626637,3.96902650888971,56.6011707618622));
#173556=CARTESIAN_POINT('Ctrl Pts',(81.9861375089232,3.93053730728745,56.5978729252474));
#173557=CARTESIAN_POINT('Ctrl Pts',(82.0223224139472,3.84317003762379,56.5905126847755));
#173558=CARTESIAN_POINT('Ctrl Pts',(82.0421431112546,3.79423190014176,56.5864782685232));
#173559=CARTESIAN_POINT('Ctrl Pts',(82.1013519343705,3.64468451638565,56.5744176790237));
#173560=CARTESIAN_POINT('Ctrl Pts',(82.1395177407302,3.54358074476346,56.5666310876267));
#173561=CARTESIAN_POINT('Ctrl Pts',(82.4352121519685,2.72058092398231,56.5061836780537));
#173562=CARTESIAN_POINT('Ctrl Pts',(82.6119385957249,1.97126808711763,56.4695337509488));
#173563=CARTESIAN_POINT('Ctrl Pts',(82.7281380081178,0.991098423549219,
56.441227783338));
#173564=CARTESIAN_POINT('Ctrl Pts',(82.7468707753557,0.772672857103674,
56.4361240812196));
#173565=CARTESIAN_POINT('Ctrl Pts',(82.7649817165545,0.43152827789089,56.4298729603844));
#173566=CARTESIAN_POINT('Ctrl Pts',(82.7692517277016,0.309152529424284,
56.4279738879533));
#173567=CARTESIAN_POINT('Ctrl Pts',(82.7719144434371,0.149660739939274,
56.4259216450456));
#173568=CARTESIAN_POINT('Ctrl Pts',(82.772329179715,0.112592879492385,56.4254744054767));
#173569=CARTESIAN_POINT('Ctrl Pts',(82.772672621413,0.0521326317942333,
56.4247925418771));
#173570=CARTESIAN_POINT('Ctrl Pts',(82.7727242018314,0.0287415005287805,
56.4245403622984));
#173571=CARTESIAN_POINT('Ctrl Pts',(82.7726661340173,-0.0169416276703035,
56.4240702888416));
#173572=CARTESIAN_POINT('Ctrl Pts',(82.7725639466525,-0.0392334248043524,
56.4238513272883));
#173573=CARTESIAN_POINT('Ctrl Pts',(82.7721695074228,-0.0891861820863875,
56.4233842456027));
#173574=CARTESIAN_POINT('Ctrl Pts',(82.7718373999325,-0.116846746766408,
56.4231418120011));
#173575=CARTESIAN_POINT('Ctrl Pts',(82.7702682912575,-0.214211127703349,
56.4223462242944));
#173576=CARTESIAN_POINT('Ctrl Pts',(82.7684232141908,-0.283903871205759,
56.4218809962315));
#173577=CARTESIAN_POINT('Ctrl Pts',(82.7514678215683,-0.744270613431884,
56.4195180785911));
#173578=CARTESIAN_POINT('Ctrl Pts',(82.7144252780961,-1.13382056373104,
56.4209119721584));
#173579=CARTESIAN_POINT('Ctrl Pts',(82.6052931881912,-1.8435017078387,56.4305945125638));
#173580=CARTESIAN_POINT('Ctrl Pts',(82.5399806426814,-2.16415622368731,
56.4377128133442));
#173581=CARTESIAN_POINT('Ctrl Pts',(82.3652512676739,-2.850712493114,56.4593591472192));
#173582=CARTESIAN_POINT('Ctrl Pts',(82.2504409526624,-3.21468349051168,
56.4749121566158));
#173583=CARTESIAN_POINT('Ctrl Pts',(82.0868436703953,-3.64682070573528,
56.4985531461655));
#173584=CARTESIAN_POINT('Ctrl Pts',(82.0572953560391,-3.72213598365673,
56.5028691375047));
#173585=CARTESIAN_POINT('Ctrl Pts',(82.0090577248409,-3.84088573544864,
56.5099858420662));
#173586=CARTESIAN_POINT('Ctrl Pts',(81.9909582898006,-3.88456282520516,
56.5126709482585));
#173587=CARTESIAN_POINT('Ctrl Pts',(81.9562808526226,-3.96661619706265,
56.5178428066775));
#173588=CARTESIAN_POINT('Ctrl Pts',(81.9397694297435,-4.00502032509871,
56.5203165159637));
#173589=CARTESIAN_POINT('Ctrl Pts',(81.9019320038613,-4.09154593844688,
56.5260099543371));
#173590=CARTESIAN_POINT('Ctrl Pts',(81.8804682009263,-4.13960401150748,
56.5292567362268));
#173591=CARTESIAN_POINT('Ctrl Pts',(81.8141787371259,-4.28497097243821,
56.5393345924802));
#173592=CARTESIAN_POINT('Ctrl Pts',(81.7681873359722,-4.38172372332873,
56.5463942828094));
#173593=CARTESIAN_POINT('Ctrl Pts',(81.5058189814662,-4.9117697516955,56.5870146276126));
#173594=CARTESIAN_POINT('Ctrl Pts',(81.2602263253606,-5.32942619913495,
56.6263204953934));
#173595=CARTESIAN_POINT('Ctrl Pts',(80.8728807565106,-5.89100418600472,
56.6891085646355));
#173596=CARTESIAN_POINT('Ctrl Pts',(80.7552135735168,-6.0511825699636,56.7082615762688));
#173597=CARTESIAN_POINT('Ctrl Pts',(80.4486136846681,-6.44346996401407,
56.7582033175902));
#173598=CARTESIAN_POINT('Ctrl Pts',(80.2539329007789,-6.67071082421701,
56.789947642877));
#173599=CARTESIAN_POINT('Ctrl Pts',(80.0155401018831,-6.92480966505708,
56.8285554582269));
#173600=CARTESIAN_POINT('Ctrl Pts',(79.981409274778,-6.96064813086315,56.8340769419965));
#173601=CARTESIAN_POINT('Ctrl Pts',(79.9281007141816,-7.01579153353887,
56.8426896371303));
#173602=CARTESIAN_POINT('Ctrl Pts',(79.9091073806543,-7.03527746600376,
56.8457560801649));
#173603=CARTESIAN_POINT('Ctrl Pts',(79.8735424461723,-7.07146550267104,
56.8514935310629));
#173604=CARTESIAN_POINT('Ctrl Pts',(79.8569910549472,-7.08818735527259,
56.854161837644));
#173605=CARTESIAN_POINT('Ctrl Pts',(79.8186029725964,-7.12669558203949,
56.8603464727588));
#173606=CARTESIAN_POINT('Ctrl Pts',(79.7967242794013,-7.14843877457842,
56.8638683496786));
#173607=CARTESIAN_POINT('Ctrl Pts',(79.7250615635052,-7.21899582591115,
56.8753954531214));
#173608=CARTESIAN_POINT('Ctrl Pts',(79.6748683310947,-7.26738210044562,
56.8834556529879));
#173609=CARTESIAN_POINT('Ctrl Pts',(79.3643522650139,-7.56046252068008,
56.9332577743923));
#173610=CARTESIAN_POINT('Ctrl Pts',(79.0916111501441,-7.79132120682228,
56.9767486482454));
#173611=CARTESIAN_POINT('Ctrl Pts',(78.5712273142436,-8.18558759206743,
57.0599872196992));
#173612=CARTESIAN_POINT('Ctrl Pts',(78.3274762239563,-8.35359141757045,
57.0990690184376));
#173613=CARTESIAN_POINT('Ctrl Pts',(77.7870864065363,-8.69130472030276,
57.1862307245456));
#173614=CARTESIAN_POINT('Ctrl Pts',(77.4884667747596,-8.85701839758791,
57.234711640782));
#173615=CARTESIAN_POINT('Ctrl Pts',(77.1124017501038,-9.04083342081322,
57.2962812532537));
#173616=CARTESIAN_POINT('Ctrl Pts',(77.0423483203296,-9.07405335039982,
57.307771059466));
#173617=CARTESIAN_POINT('Ctrl Pts',(76.929888902214,-9.12576107533153,57.3262494043446));
#173618=CARTESIAN_POINT('Ctrl Pts',(76.8877255700245,-9.14478760842171,
57.3331846997422));
#173619=CARTESIAN_POINT('Ctrl Pts',(76.8074789874316,-9.18031904352521,
57.3463981763294));
#173620=CARTESIAN_POINT('Ctrl Pts',(76.7694216413366,-9.19688205912606,
57.3526706594674));
#173621=CARTESIAN_POINT('Ctrl Pts',(76.6824509286958,-9.23407823800715,
57.3670183021908));
#173622=CARTESIAN_POINT('Ctrl Pts',(76.633474839612,-9.25455595583889,57.3751075500505));
#173623=CARTESIAN_POINT('Ctrl Pts',(76.4816189053081,-9.31660574127028,
57.4002184511718));
#173624=CARTESIAN_POINT('Ctrl Pts',(76.378214730224,-9.35682265566409,57.4173587225579));
#173625=CARTESIAN_POINT('Ctrl Pts',(75.739476932803,-9.59283472494313,57.5234747703491));
#173626=CARTESIAN_POINT('Ctrl Pts',(75.1891093755968,-9.74313201815768,
57.616012094509));
#173627=CARTESIAN_POINT('Ctrl Pts',(74.1900029408918,-9.92393171210476,
57.7842862093356));
#173628=CARTESIAN_POINT('Ctrl Pts',(73.7461400514239,-9.97308825592136,
57.8591144494693));
#173629=CARTESIAN_POINT('Ctrl Pts',(73.2170467071406,-9.99507402277027,
57.9474173561294));
#173630=CARTESIAN_POINT('Ctrl Pts',(73.13364670806,-9.99746554065069,57.9613093890031));
#173631=CARTESIAN_POINT('Ctrl Pts',(73.0183569662301,-9.99928798570218,
57.98046728672));
#173632=CARTESIAN_POINT('Ctrl Pts',(72.9864894719869,-9.99963516940403,
57.9857579020262));
#173633=CARTESIAN_POINT('Ctrl Pts',(72.9325316234741,-9.99995797073097,
57.9947070962686));
#173634=CARTESIAN_POINT('Ctrl Pts',(72.9104423816072,-10.0000149225272,
57.9983682015829));
#173635=CARTESIAN_POINT('Ctrl Pts',(72.8650142675287,-9.99997740846153,
58.0058921311289));
#173636=CARTESIAN_POINT('Ctrl Pts',(72.8416755847843,-9.99987420205068,
58.0097546436185));
#173637=CARTESIAN_POINT('Ctrl Pts',(72.7805815077889,-9.99938432564018,
58.0198583561287));
#173638=CARTESIAN_POINT('Ctrl Pts',(72.7428268299027,-9.9988619377727,58.0260949572416));
#173639=CARTESIAN_POINT('Ctrl Pts',(72.5856660738486,-9.99577296064053,
58.0520280822776));
#173640=CARTESIAN_POINT('Ctrl Pts',(72.4662981431576,-9.99122903863457,
58.0716581122195));
#173641=CARTESIAN_POINT('Ctrl Pts',(71.8382485224242,-9.95574377442191,
58.1746775120596));
#173642=CARTESIAN_POINT('Ctrl Pts',(71.332275642921,-9.88711017454876,58.2568035286751));
#173643=CARTESIAN_POINT('Ctrl Pts',(70.4149954224508,-9.68853418958247,
58.4059584866381));
#173644=CARTESIAN_POINT('Ctrl Pts',(70.002446261913,-9.57034611044422,58.473140665632));
#173645=CARTESIAN_POINT('Ctrl Pts',(69.475798030153,-9.38119460952537,58.5593936039634));
#173646=CARTESIAN_POINT('Ctrl Pts',(69.3536395505551,-9.3345336323122,58.5794337231402));
#173647=CARTESIAN_POINT('Ctrl Pts',(69.1799689677899,-9.26417482849022,
58.6079747962927));
#173648=CARTESIAN_POINT('Ctrl Pts',(69.1276840931917,-9.24246267624203,
58.6165739109851));
#173649=CARTESIAN_POINT('Ctrl Pts',(69.0369436745227,-9.20385471888833,
58.6315091405707));
#173650=CARTESIAN_POINT('Ctrl Pts',(68.9984045297915,-9.18716346753873,
58.6378560425308));
#173651=CARTESIAN_POINT('Ctrl Pts',(68.9191198423403,-9.15221778039782,
58.6509206101879));
#173652=CARTESIAN_POINT('Ctrl Pts',(68.8783890760657,-9.13393149665779,
58.6576363084923));
#173653=CARTESIAN_POINT('Ctrl Pts',(68.7740672659082,-9.08623583337875,
58.6748471125024));
#173654=CARTESIAN_POINT('Ctrl Pts',(68.7106608202108,-9.05642001868879,
58.6853175976995));
#173655=CARTESIAN_POINT('Ctrl Pts',(68.4529010933933,-8.93181945359217,
58.7279200086083));
#173656=CARTESIAN_POINT('Ctrl Pts',(68.2613403139167,-8.83127078516811,
58.7596712853618));
#173657=CARTESIAN_POINT('Ctrl Pts',(67.5867832372689,-8.44825033328149,
58.8716923656468));
#173658=CARTESIAN_POINT('Ctrl Pts',(67.1244353361462,-8.13076970883627,
58.9489368434906));
#173659=CARTESIAN_POINT('Ctrl Pts',(66.5515050109661,-7.66113969389995,
59.0437393520847));
#173660=CARTESIAN_POINT('Ctrl Pts',(66.4151940803343,-7.54304802082542,
59.066211621884));
#173661=CARTESIAN_POINT('Ctrl Pts',(66.2024587130554,-7.34836727730175,
59.1010578819761));
#173662=CARTESIAN_POINT('Ctrl Pts',(66.1239772493992,-7.27416411882655,
59.1138613557963));
#173663=CARTESIAN_POINT('Ctrl Pts',(66.020283563421,-7.17288189485434,59.1306897887546));
#173664=CARTESIAN_POINT('Ctrl Pts',(65.9940129064589,-7.14693565865169,
59.1349454501724));
#173665=CARTESIAN_POINT('Ctrl Pts',(65.9505646042505,-7.10354506535806,
59.1419698335437));
#173666=CARTESIAN_POINT('Ctrl Pts',(65.933307466961,-7.08618363545235,59.1447561301731));
#173667=CARTESIAN_POINT('Ctrl Pts',(65.9006600671254,-7.05309656307589,
59.1500199472768));
#173668=CARTESIAN_POINT('Ctrl Pts',(65.8852578349303,-7.03738342126679,
59.1525001552024));
#173669=CARTESIAN_POINT('Ctrl Pts',(65.8443266233363,-6.99534909116079,
59.1590831842411));
#173670=CARTESIAN_POINT('Ctrl Pts',(65.8188888331638,-6.96893643795431,
59.1631659323899));
#173671=CARTESIAN_POINT('Ctrl Pts',(65.7260282901543,-6.8714488235828,59.1780405856725));
#173672=CARTESIAN_POINT('Ctrl Pts',(65.6594915527174,-6.79950845535027,
59.1886411877593));
#173673=CARTESIAN_POINT('Ctrl Pts',(65.2682083459048,-6.36376760191899,
59.2506854862593));
#173674=CARTESIAN_POINT('Ctrl Pts',(64.9690019957253,-5.97718409652332,
59.2969223037193));
#173675=CARTESIAN_POINT('Ctrl Pts',(64.4820929619994,-5.24292591026478,
59.3713729644349));
#173676=CARTESIAN_POINT('Ctrl Pts',(64.2844585657862,-4.90321920214682,
59.40127276137));
#173677=CARTESIAN_POINT('Ctrl Pts',(64.0504444438035,-4.4405409171905,59.4365137785057));
#173678=CARTESIAN_POINT('Ctrl Pts',(63.9958559312707,-4.32739695139035,
59.4447187310132));
#173679=CARTESIAN_POINT('Ctrl Pts',(63.9200046964509,-4.16235183274881,
59.4560996843544));
#173680=CARTESIAN_POINT('Ctrl Pts',(63.8970407421879,-4.11126453786561,
59.4595423884426));
#173681=CARTESIAN_POINT('Ctrl Pts',(63.8575157325095,-4.02133402450607,
59.4654628737801));
#173682=CARTESIAN_POINT('Ctrl Pts',(63.8407710571365,-3.98257497481352,
59.4679694160702));
#173683=CARTESIAN_POINT('Ctrl Pts',(63.806478922087,-3.90180678617291,59.473099166708));
#173684=CARTESIAN_POINT('Ctrl Pts',(63.7889714103401,-3.85978134686698,
59.4757161218222));
#173685=CARTESIAN_POINT('Ctrl Pts',(63.7442102713071,-3.7502492135287,59.4824014704031));
#173686=CARTESIAN_POINT('Ctrl Pts',(63.7174010286647,-3.68255964634962,
59.4864002347442));
#173687=CARTESIAN_POINT('Ctrl Pts',(63.6075193260636,-3.39609343517798,
59.5027648311992));
#173688=CARTESIAN_POINT('Ctrl Pts',(63.5313270261378,-3.17469714629436,
59.5140514019717));
#173689=CARTESIAN_POINT('Ctrl Pts',(63.2973269190406,-2.40921389201419,
59.5483745945473));
#173690=CARTESIAN_POINT('Ctrl Pts',(63.1775481661048,-1.85438684178791,
59.5653567652896));
#173691=CARTESIAN_POINT('Ctrl Pts',(63.0598574046051,-0.946967874140944,
59.5789299855943));
#173692=CARTESIAN_POINT('Ctrl Pts',(63.0328413169354,-0.599497723594773,
59.5808302493471));
#173693=CARTESIAN_POINT('Ctrl Pts',(63.0223514195684,-0.202514087150256,
59.5788164213045));
#173694=CARTESIAN_POINT('Ctrl Pts',(63.0214117882815,-0.153682582570271,
59.5784965442126));
#173695=CARTESIAN_POINT('Ctrl Pts',(63.020509351098,-0.0788965070287953,
59.5778943145523));
#173696=CARTESIAN_POINT('Ctrl Pts',(63.0202951359107,-0.052945302010251,
59.5776646261293));
#173697=CARTESIAN_POINT('Ctrl Pts',(63.0201398336951,-0.0179958244278507,
59.577327158151));
#173698=CARTESIAN_POINT('Ctrl Pts',(63.020111739358,-0.00899790371852897,
59.5772377635995));
#173699=CARTESIAN_POINT('Ctrl Pts',(63.0200955324887,6.3021835685309E-11,
59.5771458498765));
#173700=CARTESIAN_POINT('Origin',(71.1115577432812,0.,47.8784035486295));
#173701=CARTESIAN_POINT('',(64.0306785352666,-5.86505158422741,49.6545847421392));
#173702=CARTESIAN_POINT('Origin',(71.2017879831895,0.,48.390124667801));
#173703=CARTESIAN_POINT('Ctrl Pts',(61.9506556875219,-4.3047803149361,49.4937177486876));
#173704=CARTESIAN_POINT('Ctrl Pts',(62.2558206002957,-4.61623330510467,
49.5206334656356));
#173705=CARTESIAN_POINT('Ctrl Pts',(62.5832897840105,-4.90076464302932,
49.547843602726));
#173706=CARTESIAN_POINT('Ctrl Pts',(63.2824918720409,-5.42189876047775,
49.6025356820337));
#173707=CARTESIAN_POINT('Ctrl Pts',(63.6484713972954,-5.65428821703993,
49.6296108874038));
#173708=CARTESIAN_POINT('Ctrl Pts',(64.0306785258525,-5.86505159962108,
49.6545847362842));
#173709=CARTESIAN_POINT('',(80.8588354304983,2.85105345906058E-13,46.3896787948389));
#173710=CARTESIAN_POINT('Ctrl Pts',(64.6378450224609,-7.86451166255203,
49.0198937666656));
#173711=CARTESIAN_POINT('Ctrl Pts',(65.5842187461411,-8.63596418606187,
48.8664417213224));
#173712=CARTESIAN_POINT('Ctrl Pts',(66.665244343586,-9.22997942887594,48.6898268456387));
#173713=CARTESIAN_POINT('Ctrl Pts',(68.7747317454522,-9.93701681694214,
48.3390049827969));
#173714=CARTESIAN_POINT('Ctrl Pts',(69.7756131305846,-10.1127840631434,
48.1705755632247));
#173715=CARTESIAN_POINT('Ctrl Pts',(72.216831965991,-10.1565930546866,47.7638481135821));
#173716=CARTESIAN_POINT('Ctrl Pts',(73.5290184110035,-9.86044398257961,
47.5496328656722));
#173717=CARTESIAN_POINT('Ctrl Pts',(75.8074028357543,-8.93620081766558,
47.1739853063171));
#173718=CARTESIAN_POINT('Ctrl Pts',(76.875925036593,-8.24881812823009,46.9959483360242));
#173719=CARTESIAN_POINT('Ctrl Pts',(78.8289563773398,-6.37831825034712,
46.6778185170246));
#173720=CARTESIAN_POINT('Ctrl Pts',(79.5456376526136,-5.24822323308914,
46.5682067541693));
#173721=CARTESIAN_POINT('Ctrl Pts',(80.2581416878816,-3.61460952657338,
46.4612355483114));
#173722=CARTESIAN_POINT('Ctrl Pts',(80.4496406732615,-3.04167150164063,
46.4332669072356));
#173723=CARTESIAN_POINT('Ctrl Pts',(80.736121211927,-1.83560492013537,46.3940854916214));
#173724=CARTESIAN_POINT('Ctrl Pts',(80.8744849978637,-0.999929053673554,
46.3765472486026));
#173725=CARTESIAN_POINT('Ctrl Pts',(80.8588354304983,5.39845945723982E-13,
46.3896787948389));
#173726=CARTESIAN_POINT('',(81.2058372116564,-1.25526296912604E-15,46.0985097275438));
#173727=CARTESIAN_POINT('Ctrl Pts',(80.8588354304983,5.47409340079241E-13,
46.3896787948389));
#173728=CARTESIAN_POINT('Ctrl Pts',(80.8552340384864,0.230110930372039,
46.3927007215552));
#173729=CARTESIAN_POINT('Ctrl Pts',(80.8433646224346,0.468917934731292,
46.3974082864174));
#173730=CARTESIAN_POINT('Ctrl Pts',(80.7059853381663,2.01312934365047,46.4391509714778));
#173731=CARTESIAN_POINT('Ctrl Pts',(80.3339343657837,3.27999513199469,46.5206449108692));
#173732=CARTESIAN_POINT('Ctrl Pts',(79.4591112270451,4.96117031922987,46.6937471773202));
#173733=CARTESIAN_POINT('Ctrl Pts',(79.1359999079507,5.46514833664704,46.7562038675566));
#173734=CARTESIAN_POINT('Ctrl Pts',(77.9119991335175,7.03455036712757,46.9907537556784));
#173735=CARTESIAN_POINT('Ctrl Pts',(76.9694568196666,7.75538512274565,47.1711076777577));
#173736=CARTESIAN_POINT('Ctrl Pts',(75.2419357532795,8.79481324655818,47.499283653396));
#173737=CARTESIAN_POINT('Ctrl Pts',(74.2128668963147,9.19433759694196,47.6920275536023));
#173738=CARTESIAN_POINT('Ctrl Pts',(72.605135482623,9.51488062321757,47.9910034564073));
#173739=CARTESIAN_POINT('Ctrl Pts',(72.0575858302653,9.57463114299576,48.0926072795593));
#173740=CARTESIAN_POINT('Ctrl Pts',(70.1521659122945,9.60900492598336,48.4482545044341));
#173741=CARTESIAN_POINT('Ctrl Pts',(68.9147695441831,9.32689482673615,48.6834345344816));
#173742=CARTESIAN_POINT('Ctrl Pts',(66.8402588659947,8.48044663053028,49.0744129611521));
#173743=CARTESIAN_POINT('Ctrl Pts',(65.8928670853075,7.88377482069447,49.2515523539232));
#173744=CARTESIAN_POINT('Ctrl Pts',(64.1751301883544,6.30870724482377,49.5779460890239));
#173745=CARTESIAN_POINT('Ctrl Pts',(63.6087131950866,5.46229732862544,49.6908447836293));
#173746=CARTESIAN_POINT('Ctrl Pts',(62.8054838250294,4.0282503011191,49.8519237176284));
#173747=CARTESIAN_POINT('Ctrl Pts',(62.4739050278201,3.16727015018886,49.9201710396792));
#173748=CARTESIAN_POINT('Ctrl Pts',(62.2702697970345,2.27382383776023,49.9649923034));
#173749=CARTESIAN_POINT('Origin',(72.3389200802052,-4.33680868994202E-16,
54.8391212561108));
#173750=CARTESIAN_POINT('',(80.8412511893021,-3.85114170205159,53.0468024688033));
#173751=CARTESIAN_POINT('',(62.6457011510073,-8.83286634079036E-15,56.4456612375439));
#173752=CARTESIAN_POINT('Ctrl Pts',(62.6457011510073,1.4432899320127E-14,
56.4456612375439));
#173753=CARTESIAN_POINT('Ctrl Pts',(62.6558818028268,1.2588196834612,56.4371186563363));
#173754=CARTESIAN_POINT('Ctrl Pts',(62.9068166598699,2.3426378835086,56.3841671741036));
#173755=CARTESIAN_POINT('Ctrl Pts',(63.3895004888157,3.72170130583507,56.2902490190701));
#173756=CARTESIAN_POINT('Ctrl Pts',(63.6188721136369,4.23445645416726,56.246865015372));
#173757=CARTESIAN_POINT('Ctrl Pts',(64.3236027030591,5.50911067298779,56.1159109714176));
#173758=CARTESIAN_POINT('Ctrl Pts',(65.0460461515127,6.57626816176057,55.9846336701387));
#173759=CARTESIAN_POINT('Ctrl Pts',(67.1241688952235,8.25959511912813,55.600727527555));
#173760=CARTESIAN_POINT('Ctrl Pts',(68.1153344812789,8.80727618002418,55.4182675813396));
#173761=CARTESIAN_POINT('Ctrl Pts',(70.1652119838017,9.51224353360967,55.046367693855));
#173762=CARTESIAN_POINT('Ctrl Pts',(71.3752373091251,9.74662388873713,54.8298371513194));
#173763=CARTESIAN_POINT('Ctrl Pts',(73.9983723123867,9.59906696956911,54.3510038345899));
#173764=CARTESIAN_POINT('Ctrl Pts',(75.2412925532651,9.26681056744937,54.1219257269736));
#173765=CARTESIAN_POINT('Ctrl Pts',(77.4110681835218,8.19401660720014,53.7267754853011));
#173766=CARTESIAN_POINT('Ctrl Pts',(78.3513233293596,7.49763695817288,53.5574829999965));
#173767=CARTESIAN_POINT('Ctrl Pts',(79.9997511629273,5.71009860563118,53.2525982152993));
#173768=CARTESIAN_POINT('Ctrl Pts',(80.6675890443261,4.60317191979347,53.1250053406627));
#173769=CARTESIAN_POINT('Ctrl Pts',(81.4593335541564,2.42846581422788,52.9736249621716));
#173770=CARTESIAN_POINT('Ctrl Pts',(81.6594257029317,1.39833823602532,52.935032235611));
#173771=CARTESIAN_POINT('Ctrl Pts',(81.7086205819825,-0.363183533732222,
52.9176503833502));
#173772=CARTESIAN_POINT('Ctrl Pts',(81.645129190087,-1.08304839861894,52.9237907714508));
#173773=CARTESIAN_POINT('Ctrl Pts',(81.3602107718099,-2.49761284659637,
52.9640327929444));
#173774=CARTESIAN_POINT('Ctrl Pts',(81.1375058307725,-3.19089770223702,
52.9985048418238));
#173775=CARTESIAN_POINT('Ctrl Pts',(80.8412511898528,-3.85114170233543,
53.0468024683008));
#173776=CARTESIAN_POINT('',(77.6076111848316,-7.81540780901842,53.6169804474894));
#173777=CARTESIAN_POINT('Origin',(72.288792169145,-4.33680868994202E-16,
54.55483174546));
#173778=CARTESIAN_POINT('Origin',(1.36168634987441,-56.100840902432,65.8484117826429));
#173779=CARTESIAN_POINT('Ctrl Pts',(76.6496952865774,-8.9910764663851,54.0790152794584));
#173780=CARTESIAN_POINT('Ctrl Pts',(75.4612431654612,-9.5637074614093,54.2810582811977));
#173781=CARTESIAN_POINT('Ctrl Pts',(74.166995732845,-9.89613305269025,54.5052439135236));
#173782=CARTESIAN_POINT('Ctrl Pts',(71.3800140752479,-10.0235187484533,
54.9838678620627));
#173783=CARTESIAN_POINT('Ctrl Pts',(70.0865581450753,-9.73932742333592,
55.2011833834671));
#173784=CARTESIAN_POINT('Ctrl Pts',(67.866731806019,-8.91204338453401,55.5785455713441));
#173785=CARTESIAN_POINT('Ctrl Pts',(66.7699239004441,-8.24310830719802,
55.7676027583461));
#173786=CARTESIAN_POINT('Ctrl Pts',(64.7456933822644,-6.38037642119864,
56.1118241547508));
#173787=CARTESIAN_POINT('Ctrl Pts',(64.0299445336693,-5.2602300440886,56.2276516472125));
#173788=CARTESIAN_POINT('Ctrl Pts',(63.0420874263768,-3.11680606634751,
56.3884754344893));
#173789=CARTESIAN_POINT('Ctrl Pts',(62.7309508857847,-1.88072460747348,
56.4393114111633));
#173790=CARTESIAN_POINT('Ctrl Pts',(62.6487768516383,-0.412225399740427,
56.4472167150806));
#173791=CARTESIAN_POINT('Ctrl Pts',(62.6440527780866,-0.203818411142372,
56.4470443866571));
#173792=CARTESIAN_POINT('Ctrl Pts',(62.6457011510073,1.80064296806393E-14,
56.4456612375439));
#173793=CARTESIAN_POINT('',(62.4908425500831,-1.65832766814155E-15,56.5756030327798));
#173794=CARTESIAN_POINT('Origin',(73.035119430904,-4.33680868994202E-16,
58.7874639765594));
#173795=CARTESIAN_POINT('',(65.3160352562258,5.15420400344998E-16,59.6408334769718));
#173796=CARTESIAN_POINT('',(80.5805554279152,-1.3827821383334E-15,56.9492867231348));
#173797=CARTESIAN_POINT('Origin',(72.9482953420705,-4.33680868994202E-16,
58.2950601000533));
#173798=CARTESIAN_POINT('',(80.3548127969482,-1.3827821383334E-15,55.6690366442189));
#173799=CARTESIAN_POINT('',(80.6673795167487,-1.3827821383334E-15,57.4416905996409));
#173800=CARTESIAN_POINT('Origin',(72.7225527111036,-4.33680868994202E-16,
57.0148100211374));
#173801=CARTESIAN_POINT('Origin',(72.9482953420705,-4.33680868994202E-16,
58.2950601000533));
#173802=CARTESIAN_POINT('Origin',(73.035119430904,-8.67361737988404E-16,
58.7874639765594));
#173803=CARTESIAN_POINT('',(79.0803910612662,-1.66338215743418E-15,55.6398949280495));
#173804=CARTESIAN_POINT('Origin',(72.6791406666868,-8.67361737988404E-16,
56.7686080828844));
#173805=CARTESIAN_POINT('',(78.3423863061819,-1.66338215743418E-15,51.4544619777476));
#173806=CARTESIAN_POINT('',(79.4363698254834,-1.66338215743418E-15,57.6587508217245));
#173807=CARTESIAN_POINT('Origin',(71.9411359116025,-8.67361737988404E-16,
52.5831751325825));
#173808=CARTESIAN_POINT('Origin',(72.6791406666868,-8.67361737988404E-16,
56.7686080828844));
#173809=CARTESIAN_POINT('',(79.370005043936,-1.69399832741288E-15,55.8426848218858));
#173810=CARTESIAN_POINT('Origin',(72.7225527111036,-8.67361737988404E-16,
57.0148100211374));
#173811=CARTESIAN_POINT('Origin',(79.3265929995192,-1.69399832741287E-15,
55.5964828836328));
#173812=CARTESIAN_POINT('Origin',(72.9482953420705,-4.33680868994202E-16,
58.2950601000533));
#173813=CARTESIAN_POINT('',(64.9104554685532,-1.44401447829076E-15,60.2200614423113));
#173814=CARTESIAN_POINT('Origin',(64.8236313797197,-1.44401447829077E-15,
59.7276575658052));
#173815=CARTESIAN_POINT('Origin',(73.035119430904,-4.33680868994202E-16,
58.7874639765594));
#173816=CARTESIAN_POINT('Origin',(74.4590344877726,0.,66.8628875512595));
#173817=CARTESIAN_POINT('',(69.479116529072,-3.1224989991992,53.0172955767497));
#173818=CARTESIAN_POINT('',(69.479116529072,3.1224989991992,53.0172955767497));
#173819=CARTESIAN_POINT('Origin',(71.9411359116025,0.,52.5831751325825));
#173820=CARTESIAN_POINT('',(69.0102664493713,-3.1224989991992,50.3583146436167));
#173821=CARTESIAN_POINT('',(71.997015105242,-3.1224989991992,67.2970079954268));
#173822=CARTESIAN_POINT('',(69.0102664493713,3.1224989991992,50.3583146436167));
#173823=CARTESIAN_POINT('Origin',(71.4722858319019,0.,49.9241941994495));
#173824=CARTESIAN_POINT('',(71.997015105242,3.1224989991992,67.2970079954268));
#173825=CARTESIAN_POINT('Origin',(73.035119430904,-4.33680868994202E-16,
58.7874639765594));
#173826=CARTESIAN_POINT('Origin',(73.035119430904,-4.33680868994202E-16,
58.7874639765594));
#173827=CARTESIAN_POINT('Ctrl Pts',(64.0263520775732,-2.56296981511825,
60.3759527238769));
#173828=CARTESIAN_POINT('Ctrl Pts',(63.7875845097259,-1.77172877889257,
60.4006974385262));
#173829=CARTESIAN_POINT('Ctrl Pts',(63.6565142256614,-0.956392695659807,
60.4105594712462));
#173830=CARTESIAN_POINT('Ctrl Pts',(63.6035905069927,0.30360001951426,60.3883547596279));
#173831=CARTESIAN_POINT('Ctrl Pts',(63.611715312006,0.743305782075929,60.3733985025284));
#173832=CARTESIAN_POINT('Ctrl Pts',(63.7164166135911,1.97589461027358,60.3151289341474));
#173833=CARTESIAN_POINT('Ctrl Pts',(63.879562647937,2.75611408109453,60.2597360604376));
#173834=CARTESIAN_POINT('Ctrl Pts',(64.5648131938851,4.72056632679071,60.0820156254564));
#173835=CARTESIAN_POINT('Ctrl Pts',(65.227248808725,5.8102138204816,59.9468224778353));
#173836=CARTESIAN_POINT('Ctrl Pts',(66.7215046807206,7.47366464069322,59.6286908078873));
#173837=CARTESIAN_POINT('Ctrl Pts',(67.4441302929274,8.0844582883649,59.4676839220779));
#173838=CARTESIAN_POINT('Ctrl Pts',(68.6416845804107,8.81513527266344,59.2149470199522));
#173839=CARTESIAN_POINT('Ctrl Pts',(69.043883161962,9.0215869125654,59.1317880463288));
#173840=CARTESIAN_POINT('Ctrl Pts',(70.9344218775917,9.82102618121542,58.7492604909112));
#173841=CARTESIAN_POINT('Ctrl Pts',(72.2569812764208,9.93197375381987,58.4985556012195));
#173842=CARTESIAN_POINT('Ctrl Pts',(73.7464228758253,9.9476694037475,58.1960089508397));
#173843=CARTESIAN_POINT('Ctrl Pts',(74.3790867245964,9.89542960221607,58.063113491427));
#173844=CARTESIAN_POINT('Ctrl Pts',(75.0041293597107,9.77968000098264,57.9325610961289));
#173845=CARTESIAN_POINT('Ctrl Pts',(72.8461347155083,9.99946198871296,58.3130737055659));
#173846=CARTESIAN_POINT('Ctrl Pts',(71.9149068124353,9.98320644558344,58.4838062328919));
#173847=CARTESIAN_POINT('Ctrl Pts',(70.9897556457315,9.82983607379267,58.6559080466542));
#173848=CARTESIAN_POINT('Ctrl Pts',(69.5021320403036,9.3582570208983,58.930684869102));
#173849=CARTESIAN_POINT('Ctrl Pts',(68.9219285900236,9.11090652668606,59.0373716283145));
#173850=CARTESIAN_POINT('Ctrl Pts',(67.5783941095989,8.37896837345306,59.2833197292783));
#173851=CARTESIAN_POINT('Ctrl Pts',(66.8474154851385,7.84011641204557,59.4160341187888));
#173852=CARTESIAN_POINT('Ctrl Pts',(65.2642516723813,6.28883638723455,59.7091484603951));
#173853=CARTESIAN_POINT('Ctrl Pts',(64.5212429759071,5.18470424453446,59.8532670983327));
#173854=CARTESIAN_POINT('Ctrl Pts',(63.5478969272612,2.87521845013382,60.0418329593114));
#173855=CARTESIAN_POINT('Ctrl Pts',(63.2799418969696,1.6982627346725,60.0936703250998));
#173856=CARTESIAN_POINT('Ctrl Pts',(63.1657385233228,-0.917901988626705,
60.1290073346147));
#173857=CARTESIAN_POINT('Ctrl Pts',(63.4167115584965,-2.22103464168441,
60.0982490330575));
#173858=CARTESIAN_POINT('Ctrl Pts',(64.2574469136842,-4.53354012896003,
59.9683289205253));
#173859=CARTESIAN_POINT('Ctrl Pts',(64.9136511838193,-5.6373681902584,59.8580788638135));
#173860=CARTESIAN_POINT('Ctrl Pts',(66.6986338989128,-7.63000409523024,
59.5591622625367));
#173861=CARTESIAN_POINT('Ctrl Pts',(67.7775303758803,-8.37226083492883,
59.3819682455633));
#173862=CARTESIAN_POINT('Ctrl Pts',(69.9524651194837,-9.39905901463539,
59.0158642552059));
#173863=CARTESIAN_POINT('Ctrl Pts',(71.1596155168285,-9.70968120699252,
58.8080610233883));
#173864=CARTESIAN_POINT('Ctrl Pts',(73.3729201406308,-9.83583275513113,
58.43066506375));
#173865=CARTESIAN_POINT('Ctrl Pts',(74.3575262345018,-9.73497309686251,
58.2662251899724));
#173866=CARTESIAN_POINT('Ctrl Pts',(76.3782480250941,-9.20815341290068,
57.9276702428763));
#173867=CARTESIAN_POINT('Ctrl Pts',(77.3972451749448,-8.74454053614141,
57.7553593824384));
#173868=CARTESIAN_POINT('Ctrl Pts',(78.6753907266003,-7.87164291992839,
57.5382919268542));
#173869=CARTESIAN_POINT('Ctrl Pts',(79.0201448012645,-7.60006937811386,
57.4797430645897));
#173870=CARTESIAN_POINT('Ctrl Pts',(80.3839454547407,-6.36466254602424,
57.2501127656707));
#173871=CARTESIAN_POINT('Ctrl Pts',(81.1129231951604,-5.29014523519362,
57.1344711030446));
#173872=CARTESIAN_POINT('Ctrl Pts',(81.992728202448,-3.42226759385829,56.994493242659));
#173873=CARTESIAN_POINT('Ctrl Pts',(82.2662184197964,-2.54642331504456,
56.9511812568696));
#173874=CARTESIAN_POINT('Ctrl Pts',(82.4839371806097,-1.23056618564693,
56.9195544439548));
#173875=CARTESIAN_POINT('Ctrl Pts',(82.5259926495773,-0.810139400801797,
56.9142786692208));
#173876=CARTESIAN_POINT('Ctrl Pts',(82.5450936724779,-0.258026219139575,
56.9142906530356));
#173877=CARTESIAN_POINT('Ctrl Pts',(82.5469438787143,-0.128531025228586,
56.9147998423219));
#173878=CARTESIAN_POINT('Ctrl Pts',(82.5462364601441,-3.03547362939804E-8,
56.915810141241));
#173879=CARTESIAN_POINT('Origin',(69.9094522328998,0.,41.0609244223396));
#173880=CARTESIAN_POINT('',(60.0036718763913,-9.6034686896093E-16,42.5716136120261));
#173881=CARTESIAN_POINT('Ctrl Pts',(60.0036718763913,-9.71445146547012E-15,
42.5716136120261));
#173882=CARTESIAN_POINT('Ctrl Pts',(60.015100851557,1.12076762514684,42.5552913438929));
#173883=CARTESIAN_POINT('Ctrl Pts',(60.2126873206611,2.13839800656458,42.5043854450878));
#173884=CARTESIAN_POINT('Ctrl Pts',(60.9006318822312,4.25527362975578,42.352347691539));
#173885=CARTESIAN_POINT('Ctrl Pts',(61.5373356061649,5.40491193212032,42.2258291698478));
#173886=CARTESIAN_POINT('Ctrl Pts',(63.2842977147422,7.47099370248614,41.8858881841359));
#173887=CARTESIAN_POINT('Ctrl Pts',(64.3217540848946,8.2258424335728,41.683036578767));
#173888=CARTESIAN_POINT('Ctrl Pts',(66.451028591047,9.32975004786528,41.2743904466553));
#173889=CARTESIAN_POINT('Ctrl Pts',(67.6946653135831,9.68938228252847,41.0411463826451));
#173890=CARTESIAN_POINT('Ctrl Pts',(70.249425026084,9.89392953488958,40.5602284082465));
#173891=CARTESIAN_POINT('Ctrl Pts',(71.3809810751992,9.72068069599538,40.3427593588294));
#173892=CARTESIAN_POINT('Ctrl Pts',(73.2715781015043,9.17865716757742,39.9806019499236));
#173893=CARTESIAN_POINT('Ctrl Pts',(74.1892182222798,8.75151497853075,39.8057754039733));
#173894=CARTESIAN_POINT('Ctrl Pts',(75.4581963738792,7.89714843430856,39.5638811008101));
#173895=CARTESIAN_POINT('Ctrl Pts',(75.868825936961,7.5689631723131,39.4854636028735));
#173896=CARTESIAN_POINT('Ctrl Pts',(77.2483266748846,6.26457595469469,39.2185396485213));
#173897=CARTESIAN_POINT('Ctrl Pts',(77.9577795744693,5.18258137974227,39.0727146413577));
#173898=CARTESIAN_POINT('Ctrl Pts',(78.8596251672318,3.1507044373941,38.8836436555022));
#173899=CARTESIAN_POINT('Ctrl Pts',(79.131437675942,2.12458558215186,38.8239526068959));
#173900=CARTESIAN_POINT('Ctrl Pts',(79.3692586925281,-0.323481828215834,
38.7530699483904));
#173901=CARTESIAN_POINT('Ctrl Pts',(79.1854889076528,-1.5955261956348,38.7654352018601));
#173902=CARTESIAN_POINT('Ctrl Pts',(78.5652621680601,-3.63454258061496,
38.8438640005469));
#173903=CARTESIAN_POINT('Ctrl Pts',(78.1275440032739,-4.54476502256378,
38.9083134454724));
#173904=CARTESIAN_POINT('Ctrl Pts',(77.2671455806108,-5.79308784648288,
39.0418902563234));
#173905=CARTESIAN_POINT('Ctrl Pts',(76.9402683789618,-6.19380668058799,
39.0934590420892));
#173906=CARTESIAN_POINT('Ctrl Pts',(75.7122858853336,-7.467828066414,39.2868961783433));
#173907=CARTESIAN_POINT('Ctrl Pts',(74.6693898303905,-8.18345984132722,
39.4501703743754));
#173908=CARTESIAN_POINT('Ctrl Pts',(72.5648273975363,-9.08634426397409,
39.7900363806716));
#173909=CARTESIAN_POINT('Ctrl Pts',(71.539508412694,-9.3357772537295,39.9591202037972));
#173910=CARTESIAN_POINT('Ctrl Pts',(69.2592631600181,-9.48947083365311,
40.3326286562384));
#173911=CARTESIAN_POINT('Ctrl Pts',(68.1626906187745,-9.30992149226666,
40.5078344866331));
#173912=CARTESIAN_POINT('Ctrl Pts',(66.3499023071681,-8.76459892370793,
40.7990369030172));
#173913=CARTESIAN_POINT('Ctrl Pts',(65.4869193623454,-8.3529885143117,40.9385799356877));
#173914=CARTESIAN_POINT('Ctrl Pts',(64.7021225437138,-7.81768501306327,
41.065233192728));
#173915=CARTESIAN_POINT('Ctrl Pts',(76.8678595013252,-7.42547303891627,
39.8339694781584));
#173916=CARTESIAN_POINT('Ctrl Pts',(76.2996665754096,-7.93011918472383,
39.9050608108253));
#173917=CARTESIAN_POINT('Ctrl Pts',(75.6825187982154,-8.37119663038465,
39.9887641400102));
#173918=CARTESIAN_POINT('Ctrl Pts',(74.4558505579195,-9.04934668012714,
40.1542389939804));
#173919=CARTESIAN_POINT('Ctrl Pts',(73.8654202486675,-9.30370903464973,
40.2335728392658));
#173920=CARTESIAN_POINT('Ctrl Pts',(72.2903388606086,-9.80223571367267,
40.441283110937));
#173921=CARTESIAN_POINT('Ctrl Pts',(71.2931850079593,-9.95167476081707,
40.5682944419678));
#173922=CARTESIAN_POINT('Ctrl Pts',(69.4560555737328,-9.95340529705847,
40.8124145716253));
#173923=CARTESIAN_POINT('Ctrl Pts',(68.0374687632394,-9.86536563346914,
41.0176380044774));
#173924=CARTESIAN_POINT('Ctrl Pts',(65.5125902514186,-8.79704444319692,
41.3538217666584));
#173925=CARTESIAN_POINT('Ctrl Pts',(64.6573596433338,-8.25918115529596,
41.4580511199009));
#173926=CARTESIAN_POINT('Ctrl Pts',(63.4723018145351,-7.22572972472362,
41.5943541895369));
#173927=CARTESIAN_POINT('Ctrl Pts',(63.0784912802987,-6.81814121716002,
41.6388112706362));
#173928=CARTESIAN_POINT('Ctrl Pts',(61.9669303031546,-5.46050870597522,
41.7656919416805));
#173929=CARTESIAN_POINT('Ctrl Pts',(61.3871579820319,-4.41116939664101,
41.8264853738403));
#173930=CARTESIAN_POINT('Ctrl Pts',(60.7520023897809,-2.43621381970203,
41.8462181459636));
#173931=CARTESIAN_POINT('Ctrl Pts',(60.6035823151644,-1.57716493704874,
41.8289274144168));
#173932=CARTESIAN_POINT('Ctrl Pts',(60.5714935134192,-0.70586883869046,
41.7935745403973));
#173933=CARTESIAN_POINT('Ctrl Pts',(72.9974833261206,-9.75859007406184,
40.5164212233382));
#173934=CARTESIAN_POINT('Ctrl Pts',(72.1680866689036,-10.0182427508679,
40.6526096763793));
#173935=CARTESIAN_POINT('Ctrl Pts',(71.3084745515891,-10.1699514565876,
40.7953672456757));
#173936=CARTESIAN_POINT('Ctrl Pts',(69.096234136181,-10.2640179840406,41.1594237519536));
#173937=CARTESIAN_POINT('Ctrl Pts',(67.8768440048148,-10.0398244678189,
41.3550739449956));
#173938=CARTESIAN_POINT('Ctrl Pts',(65.5868797574183,-9.26087437006304,
41.725821401744));
#173939=CARTESIAN_POINT('Ctrl Pts',(64.429406738187,-8.59349167447454,41.9157601187445));
#173940=CARTESIAN_POINT('Ctrl Pts',(62.3355503431521,-6.75255369228092,
42.2527084519859));
#173941=CARTESIAN_POINT('Ctrl Pts',(61.5631077787736,-5.64482332823591,
42.3683202081607));
#173942=CARTESIAN_POINT('Ctrl Pts',(60.4566040978486,-3.37627727188828,
42.5298683525699));
#173943=CARTESIAN_POINT('Ctrl Pts',(60.1092783965342,-2.07466361355572,
42.5774466901993));
#173944=CARTESIAN_POINT('Ctrl Pts',(60.0075858713322,-0.493629709332019,
42.5770362265899));
#173945=CARTESIAN_POINT('Ctrl Pts',(60.0011799984526,-0.244362777846393,
42.575172382544));
#173946=CARTESIAN_POINT('Ctrl Pts',(60.0036718763913,-6.10622663543836E-15,
42.5716136120261));
#173947=CARTESIAN_POINT('',(60.6263323388303,-1.1327982893212E-15,41.6823623120182));
#173948=CARTESIAN_POINT('',(59.8151727645246,-1.25526296912604E-15,42.8408182434253));
#173949=CARTESIAN_POINT('Origin',(69.7358040552328,0.,40.0761166693274));
#173950=CARTESIAN_POINT('Origin',(73.0915550886457,-4.33680868994202E-16,
59.1075264962884));
#173951=CARTESIAN_POINT('Ctrl Pts',(81.6610766756267,4.47259269587928E-12,
52.9993788854899));
#173952=CARTESIAN_POINT('Ctrl Pts',(81.6610722764663,-0.00232025445502517,
52.9993539366116));
#173953=CARTESIAN_POINT('Ctrl Pts',(81.661067045244,-0.00464051070797554,
52.9993291640552));
#173954=CARTESIAN_POINT('Ctrl Pts',(81.6609993686616,-0.0305384148304018,
52.9990546279118));
#173955=CARTESIAN_POINT('Ctrl Pts',(81.6608518350455,-0.054115947562142,
52.9988228830155));
#173956=CARTESIAN_POINT('Ctrl Pts',(81.6602425001029,-0.115647279179397,
52.9982651715894));
#173957=CARTESIAN_POINT('Ctrl Pts',(81.6596439234659,-0.153599559557272,
52.9979679311037));
#173958=CARTESIAN_POINT('Ctrl Pts',(81.6559699978132,-0.323336835080533,
52.9968448740763));
#173959=CARTESIAN_POINT('Ctrl Pts',(81.6504306382807,-0.455057219995967,
52.9965296115069));
#173960=CARTESIAN_POINT('Ctrl Pts',(81.6266559635856,-0.835254836627224,
52.9971545979555));
#173961=CARTESIAN_POINT('Ctrl Pts',(81.6015184647897,-1.08318716183554,
52.9994595362967));
#173962=CARTESIAN_POINT('Ctrl Pts',(81.474195624691,-1.98833237428493,53.0142996630001));
#173963=CARTESIAN_POINT('Ctrl Pts',(81.3137681540632,-2.63524327442574,
53.0373067696788));
#173964=CARTESIAN_POINT('Ctrl Pts',(81.0527830174814,-3.3569861251441,53.0756325690094));
#173965=CARTESIAN_POINT('Ctrl Pts',(81.0161192583185,-3.45347191784948,
53.0810339964031));
#173966=CARTESIAN_POINT('Ctrl Pts',(80.9584501697706,-3.5981461001753,53.089552188204));
#173967=CARTESIAN_POINT('Ctrl Pts',(80.9385925672861,-3.64679406876821,
53.092488995169));
#173968=CARTESIAN_POINT('Ctrl Pts',(80.9022225162372,-3.73383870110997,
53.0978741346783));
#173969=CARTESIAN_POINT('Ctrl Pts',(80.8858567197031,-3.77229655864622,
53.1002995016838));
#173970=CARTESIAN_POINT('Ctrl Pts',(80.8504034898739,-3.85411521597498,
53.1055580685769));
#173971=CARTESIAN_POINT('Ctrl Pts',(80.8312451048555,-3.89744331436159,
53.1084023826643));
#173972=CARTESIAN_POINT('Ctrl Pts',(80.7782437501906,-4.01494090251588,
53.1162783170956));
#173973=CARTESIAN_POINT('Ctrl Pts',(80.7437752410286,-4.08881713239427,
53.1214079609473));
#173974=CARTESIAN_POINT('Ctrl Pts',(80.5644807627053,-4.46060791753182,
53.1481310887594));
#173975=CARTESIAN_POINT('Ctrl Pts',(80.4052406243085,-4.75115004446838,
53.1719827824595));
#173976=CARTESIAN_POINT('Ctrl Pts',(80.0553836328029,-5.31746468070993,
53.224836143526));
#173977=CARTESIAN_POINT('Ctrl Pts',(79.8646680539399,-5.59262914290383,
53.2538583446598));
#173978=CARTESIAN_POINT('Ctrl Pts',(79.487921471852,-6.07933967601403,53.3120132898615));
#173979=CARTESIAN_POINT('Ctrl Pts',(79.3061523332329,-6.29380594126246,
53.3403692069814));
#173980=CARTESIAN_POINT('Ctrl Pts',(79.0749264208731,-6.54332446046129,
53.3770383702038));
#173981=CARTESIAN_POINT('Ctrl Pts',(79.0341547104778,-6.58650217127409,
53.3835253887303));
#173982=CARTESIAN_POINT('Ctrl Pts',(78.97272632313,-6.65034533360716,53.3933336964837));
#173983=CARTESIAN_POINT('Ctrl Pts',(78.9523697631261,-6.67130755192734,
53.3965896191447));
#173984=CARTESIAN_POINT('Ctrl Pts',(78.9155399574673,-6.70888447947886,
53.4024908438246));
#173985=CARTESIAN_POINT('Ctrl Pts',(78.8991009973588,-6.7255333291227,53.4051286087279));
#173986=CARTESIAN_POINT('Ctrl Pts',(78.8621076697072,-6.76272290145134,
53.4110728755343));
#173987=CARTESIAN_POINT('Ctrl Pts',(78.8415209041491,-6.78322958915602,
53.4143865479715));
#173988=CARTESIAN_POINT('Ctrl Pts',(78.7791598347458,-6.84477967856057,
53.4244404681999));
#173989=CARTESIAN_POINT('Ctrl Pts',(78.7371042565384,-6.88552595802291,
53.4312424413944));
#173990=CARTESIAN_POINT('Ctrl Pts',(78.6379734609746,-6.97980400347526,
53.447320443257));
#173991=CARTESIAN_POINT('Ctrl Pts',(78.5806122158642,-7.03301822335197,
53.4566578090453));
#173992=CARTESIAN_POINT('Ctrl Pts',(78.2327508384596,-7.34778625380926,
53.5134520550835));
#173993=CARTESIAN_POINT('Ctrl Pts',(77.9272003779144,-7.59155407372705,
53.564017729834));
#173994=CARTESIAN_POINT('Ctrl Pts',(77.6076111848315,-7.81540780901845,
53.6169804474894));
#173995=CARTESIAN_POINT('Ctrl Pts',(80.841251189302,-3.85114170205161,53.0468024688033));
#173996=CARTESIAN_POINT('Ctrl Pts',(80.8507779136793,-3.82942848242393,
53.0453809010695));
#173997=CARTESIAN_POINT('Ctrl Pts',(80.8602207064578,-3.80768840471765,
53.0439756042331));
#173998=CARTESIAN_POINT('Ctrl Pts',(80.8792048973429,-3.76353516228782,
53.0411580292377));
#173999=CARTESIAN_POINT('Ctrl Pts',(80.8887378829764,-3.74112938354105,
53.0397472097096));
#174000=CARTESIAN_POINT('Ctrl Pts',(80.9163307695015,-3.67558706517093,
53.0356755751662));
#174001=CARTESIAN_POINT('Ctrl Pts',(80.9341623540418,-3.63235242951933,
53.0330595355005));
#174002=CARTESIAN_POINT('Ctrl Pts',(80.982223849608,-3.51336899811502,53.0260511192625));
#174003=CARTESIAN_POINT('Ctrl Pts',(81.0118098928388,-3.43735710624604,
53.0217849107517));
#174004=CARTESIAN_POINT('Ctrl Pts',(81.183168553697,-2.98000080361263,52.9973720652675));
#174005=CARTESIAN_POINT('Ctrl Pts',(81.301710550912,-2.5901662948204,52.9817814278254));
#174006=CARTESIAN_POINT('Ctrl Pts',(81.4650039959974,-1.89866215450415,
52.9626858339964));
#174007=CARTESIAN_POINT('Ctrl Pts',(81.5207698692727,-1.6002609329892,52.9571167954222));
#174008=CARTESIAN_POINT('Ctrl Pts',(81.5807520080895,-1.16684122199171,
52.9525768273773));
#174009=CARTESIAN_POINT('Ctrl Pts',(81.5963630564538,-1.03360813536364,
52.9516575893418));
#174010=CARTESIAN_POINT('Ctrl Pts',(81.6236379970694,-0.749572634412603,
52.9506649274304));
#174011=CARTESIAN_POINT('Ctrl Pts',(81.6345423798266,-0.598733092378248,
52.9507142757853));
#174012=CARTESIAN_POINT('Ctrl Pts',(81.6464653136749,-0.353392227770225,
52.95167538014));
#174013=CARTESIAN_POINT('Ctrl Pts',(81.6496579259418,-0.259021630920684,
52.9522561509393));
#174014=CARTESIAN_POINT('Ctrl Pts',(81.6520988061173,-0.130967865973636,
52.9533185372138));
#174015=CARTESIAN_POINT('Ctrl Pts',(81.6525632048301,-0.0973118027878368,
52.9536234500613));
#174016=CARTESIAN_POINT('Ctrl Pts',(81.6530315026046,-0.0424365229063424,
52.954161815321));
#174017=CARTESIAN_POINT('Ctrl Pts',(81.6531421625657,-0.0212183265239835,
52.9543800258197));
#174018=CARTESIAN_POINT('Ctrl Pts',(81.653182392128,-1.2050098533051E-12,
52.9546081790047));
#174019=CARTESIAN_POINT('Origin',(69.6316151486327,0.,39.48523201752));
#174020=CARTESIAN_POINT('Ctrl Pts',(61.9717635125435,8.13085086909029E-10,
49.8885587101925));
#174021=CARTESIAN_POINT('Ctrl Pts',(61.9719008215855,-0.0386086908632389,
49.8893374284854));
#174022=CARTESIAN_POINT('Ctrl Pts',(61.9722723485771,-0.07721697300564,
49.890067325024));
#174023=CARTESIAN_POINT('Ctrl Pts',(61.9740902680162,-0.193059381531131,
49.8921128159878));
#174024=CARTESIAN_POINT('Ctrl Pts',(61.9762401391437,-0.270281536593981,
49.8932835767828));
#174025=CARTESIAN_POINT('Ctrl Pts',(61.9903399164194,-0.622718691519423,
49.8977695916096));
#174026=CARTESIAN_POINT('Ctrl Pts',(62.0132749459347,-0.897383461623408,
49.8988800511485));
#174027=CARTESIAN_POINT('Ctrl Pts',(62.1314503069768,-1.82461418207681,
49.8952281601475));
#174028=CARTESIAN_POINT('Ctrl Pts',(62.2825927448918,-2.46800064525378,
49.88026429198));
#174029=CARTESIAN_POINT('Ctrl Pts',(62.5446291335746,-3.22012079152954,
49.8496607753499));
#174030=CARTESIAN_POINT('Ctrl Pts',(62.5927555060374,-3.34910781432234,
49.8439163670925));
#174031=CARTESIAN_POINT('Ctrl Pts',(62.6799351968114,-3.56801770024668,
49.8333222087998));
#174032=CARTESIAN_POINT('Ctrl Pts',(62.7176037771392,-3.65847766312796,
49.8286919141738));
#174033=CARTESIAN_POINT('Ctrl Pts',(62.7984789875565,-3.84447399668024,
49.8186477774749));
#174034=CARTESIAN_POINT('Ctrl Pts',(62.8418829557966,-3.93990795901347,
49.813202487331));
#174035=CARTESIAN_POINT('Ctrl Pts',(62.9337938583576,-4.13336329246223,
49.8015641096309));
#174036=CARTESIAN_POINT('Ctrl Pts',(62.9824332342972,-4.23130270792171,
49.7953497651111));
#174037=CARTESIAN_POINT('Ctrl Pts',(63.3148528957183,-4.87238148852751,
49.7525174065633));
#174038=CARTESIAN_POINT('Ctrl Pts',(63.6491750771382,-5.38710153959971,
49.7078918497935));
#174039=CARTESIAN_POINT('Ctrl Pts',(64.0306847538311,-5.86505936749701,
49.6545838761671));
#174040=CARTESIAN_POINT('Ctrl Pts',(78.7320872163416,0.,37.9066414382813));
#174041=CARTESIAN_POINT('Ctrl Pts',(78.740769625225,2.41806680288088,37.9558818259319));
#174042=CARTESIAN_POINT('Ctrl Pts',(76.7871543254317,7.2349491628497,38.4018995743988));
#174043=CARTESIAN_POINT('Ctrl Pts',(69.6881675238581,10.2370276571518,39.8059564749922));
#174044=CARTESIAN_POINT('Ctrl Pts',(62.5891807222845,7.23494916284969,41.2100133755855));
#174045=CARTESIAN_POINT('Ctrl Pts',(59.6587577725946,1.77635683940025E-15,
41.8790399982859));
#174046=CARTESIAN_POINT('Ctrl Pts',(62.6412751755846,-7.2349491628497,41.5054557014892));
#174047=CARTESIAN_POINT('Ctrl Pts',(69.7923564304583,-10.2370276571518,
40.3968411267995));
#174048=CARTESIAN_POINT('Ctrl Pts',(76.9434376853319,-7.2349491628497,39.2882265521098));
#174049=CARTESIAN_POINT('Ctrl Pts',(79.9259550883219,-1.77635683940025E-15,
38.9146422553131));
#174050=CARTESIAN_POINT('Ctrl Pts',(76.995532138632,7.23494916284969,39.5836688780135));
#174051=CARTESIAN_POINT('Ctrl Pts',(69.8965453370584,10.2370276571518,40.9877257786068));
#174052=CARTESIAN_POINT('Ctrl Pts',(62.7975585354848,7.23494916284971,42.3917826792002));
#174053=CARTESIAN_POINT('Ctrl Pts',(59.8671355857949,3.5527136788005E-15,
43.0608093019006));
#174054=CARTESIAN_POINT('Ctrl Pts',(62.8496529887849,-7.23494916284971,
42.6872250051038));
#174055=CARTESIAN_POINT('Ctrl Pts',(70.0007342436585,-10.2370276571518,
41.5786104304142));
#174056=CARTESIAN_POINT('Ctrl Pts',(77.1518154985322,-7.23494916284971,
40.4699958557245));
#174057=CARTESIAN_POINT('Ctrl Pts',(80.1343329015222,-4.44089209850063E-15,
40.0964115589277));
#174058=CARTESIAN_POINT('Ctrl Pts',(77.2039099518322,7.2349491628497,40.7654381816281));
#174059=CARTESIAN_POINT('Ctrl Pts',(70.1049231502587,10.2370276571518,42.1694950822215));
#174060=CARTESIAN_POINT('Ctrl Pts',(63.0059363486851,7.23494916284972,43.5735519828148));
#174061=CARTESIAN_POINT('Ctrl Pts',(60.0755133989952,6.21724893790088E-15,
44.2425786055152));
#174062=CARTESIAN_POINT('Ctrl Pts',(63.0580308019852,-7.23494916284971,
43.8689943087185));
#174063=CARTESIAN_POINT('Ctrl Pts',(70.2091120568588,-10.2370276571518,
42.7603797340288));
#174064=CARTESIAN_POINT('Ctrl Pts',(77.3601933117325,-7.23494916284971,
41.6517651593391));
#174065=CARTESIAN_POINT('Ctrl Pts',(80.3427107147225,-7.99360577730113E-15,
41.2781808625424));
#174066=CARTESIAN_POINT('Ctrl Pts',(77.4122877650325,7.2349491628497,41.9472074852428));
#174067=CARTESIAN_POINT('Ctrl Pts',(70.3133009634589,10.2370276571518,43.3512643858361));
#174068=CARTESIAN_POINT('Ctrl Pts',(63.2143141618854,7.23494916284972,44.7553212864295));
#174069=CARTESIAN_POINT('Ctrl Pts',(60.2838912121955,9.76996261670138E-15,
45.4243479091299));
#174070=CARTESIAN_POINT('Ctrl Pts',(63.2664086151855,-7.23494916284971,
45.0507636123332));
#174071=CARTESIAN_POINT('Ctrl Pts',(70.4174898700591,-10.2370276571518,
43.9421490376435));
#174072=CARTESIAN_POINT('Ctrl Pts',(77.5685711249327,-7.23494916284971,
42.8335344629538));
#174073=CARTESIAN_POINT('Ctrl Pts',(80.5510885279228,-1.15463194561016E-14,
42.459950166157));
#174074=CARTESIAN_POINT('Ctrl Pts',(77.6206655782328,7.2349491628497,43.1289767888574));
#174075=CARTESIAN_POINT('Ctrl Pts',(70.5216787766592,10.2370276571518,44.5330336894508));
#174076=CARTESIAN_POINT('Ctrl Pts',(63.4226919750857,7.23494916284972,45.9370905900442));
#174077=CARTESIAN_POINT('Ctrl Pts',(60.4922690253957,1.15463194561016E-14,
46.6061172127446));
#174078=CARTESIAN_POINT('Ctrl Pts',(63.4747864283858,-7.2349491628497,46.2325329159478));
#174079=CARTESIAN_POINT('Ctrl Pts',(70.6258676832593,-10.2370276571518,
45.1239183412581));
#174080=CARTESIAN_POINT('Ctrl Pts',(77.776948938133,-7.23494916284971,44.0153037665684));
#174081=CARTESIAN_POINT('Ctrl Pts',(80.759466341123,0.,43.6417194697717));
#174082=CARTESIAN_POINT('Ctrl Pts',(77.8290433914331,7.23494916284965,44.3107460924721));
#174083=CARTESIAN_POINT('Ctrl Pts',(70.7300565898595,10.2370276571518,45.7148029930655));
#174084=CARTESIAN_POINT('Ctrl Pts',(63.631069788286,7.23494916284971,47.1188598936588));
#174085=CARTESIAN_POINT('Ctrl Pts',(60.700646838596,7.90478793533111E-14,
47.7878865163592));
#174086=CARTESIAN_POINT('Ctrl Pts',(63.683164241586,-7.23494916284972,47.4143022195625));
#174087=CARTESIAN_POINT('Ctrl Pts',(70.8342454964596,-10.2370276571518,
46.3056876448728));
#174088=CARTESIAN_POINT('Ctrl Pts',(77.9853267513333,-7.23494916284967,
45.1970730701831));
#174089=CARTESIAN_POINT('Ctrl Pts',(80.9678441543233,-1.59872115546023E-14,
44.8234887733864));
#174090=CARTESIAN_POINT('Ctrl Pts',(78.0374212046334,7.23494916284965,45.4925153960867));
#174091=CARTESIAN_POINT('Ctrl Pts',(70.9384344030598,10.2370276571518,46.8965722966801));
#174092=CARTESIAN_POINT('Ctrl Pts',(63.8394476014863,7.23494916284974,48.3006291972735));
#174093=CARTESIAN_POINT('Ctrl Pts',(60.9090246517963,-4.61852778244065E-14,
48.9696558199739));
#174094=CARTESIAN_POINT('Ctrl Pts',(63.8915420547863,-7.23494916284968,
48.5960715231771));
#174095=CARTESIAN_POINT('Ctrl Pts',(71.0426233096599,-10.2370276571518,
47.4874569484874));
#174096=CARTESIAN_POINT('Ctrl Pts',(78.1937045645336,-7.23494916284967,
46.3788423737977));
#174097=CARTESIAN_POINT('Ctrl Pts',(81.1762219675236,-2.04281036531029E-14,
46.005258077001));
#174098=CARTESIAN_POINT('Ctrl Pts',(78.2457990178337,7.23494916284965,46.6742846997014));
#174099=CARTESIAN_POINT('Ctrl Pts',(71.1468122162601,10.2370276571518,48.0783416002948));
#174100=CARTESIAN_POINT('Ctrl Pts',(64.0478254146866,7.23494916284971,49.4823985008881));
#174101=CARTESIAN_POINT('Ctrl Pts',(61.1174024649966,8.34887714518118E-14,
50.1514251235885));
#174102=CARTESIAN_POINT('Ctrl Pts',(64.0999198679866,-7.23494916284971,
49.7778408267918));
#174103=CARTESIAN_POINT('Ctrl Pts',(71.2510011228602,-10.2370276571518,
48.6692262521021));
#174104=CARTESIAN_POINT('Ctrl Pts',(77.6476023720424,-7.55168562811132,
47.6775768608315));
#174105=CARTESIAN_POINT('Ctrl Pts',(79.691478707762,-3.87217647526957,47.4026589808119));
#174106=CARTESIAN_POINT('Ctrl Pts',(80.1038958562351,-2.27117162724,47.3646400428343));
#174107=CARTESIAN_POINT('Ctrl Pts',(79.8990610925212,0.,38.2745868880941));
#174108=CARTESIAN_POINT('Ctrl Pts',(79.9077435014046,2.70221125641844,38.3238272757448));
#174109=CARTESIAN_POINT('Ctrl Pts',(77.7225204280915,8.08512033008161,38.810683723625));
#174110=CARTESIAN_POINT('Ctrl Pts',(69.7862784696405,11.4399698695112,40.3623712981132));
#174111=CARTESIAN_POINT('Ctrl Pts',(61.8500365111895,8.0851203300816,41.9140588726013));
#174112=CARTESIAN_POINT('Ctrl Pts',(58.5722019012198,1.77635683940025E-15,
42.6443435444217));
#174113=CARTESIAN_POINT('Ctrl Pts',(61.9021309644895,-8.08512033008161,
42.209501198505));
#174114=CARTESIAN_POINT('Ctrl Pts',(69.8904673762406,-11.4399698695112,
40.9532559499205));
#174115=CARTESIAN_POINT('Ctrl Pts',(77.8788037879917,-8.08512033008161,
39.697010701336));
#174116=CARTESIAN_POINT('Ctrl Pts',(81.2087328512614,-1.77635683940025E-15,
39.2621683554193));
#174117=CARTESIAN_POINT('Ctrl Pts',(77.9308982412917,8.0851203300816,39.9924530272397));
#174118=CARTESIAN_POINT('Ctrl Pts',(69.9946562828407,11.4399698695112,41.5441406017278));
#174119=CARTESIAN_POINT('Ctrl Pts',(62.0584143243898,8.08512033008162,43.095828176216));
#174120=CARTESIAN_POINT('Ctrl Pts',(58.7805797144201,3.5527136788005E-15,
43.8261128480364));
#174121=CARTESIAN_POINT('Ctrl Pts',(62.1105087776898,-8.08512033008161,
43.3912705021196));
#174122=CARTESIAN_POINT('Ctrl Pts',(70.0988451894409,-11.4399698695112,
42.1350252535352));
#174123=CARTESIAN_POINT('Ctrl Pts',(78.0871816011919,-8.08512033008162,
40.8787800049507));
#174124=CARTESIAN_POINT('Ctrl Pts',(81.4171106644617,-4.44089209850063E-15,
40.4439376590339));
#174125=CARTESIAN_POINT('Ctrl Pts',(78.139276054492,8.08512033008161,41.1742223308544));
#174126=CARTESIAN_POINT('Ctrl Pts',(70.203034096041,11.4399698695112,42.7259099053425));
#174127=CARTESIAN_POINT('Ctrl Pts',(62.2667921375901,8.08512033008162,44.2775974798306));
#174128=CARTESIAN_POINT('Ctrl Pts',(58.9889575276203,6.21724893790088E-15,
45.007882151651));
#174129=CARTESIAN_POINT('Ctrl Pts',(62.3188865908901,-8.08512033008161,
44.5730398057343));
#174130=CARTESIAN_POINT('Ctrl Pts',(70.3072230026411,-11.4399698695112,
43.3167945571498));
#174131=CARTESIAN_POINT('Ctrl Pts',(78.2955594143922,-8.08512033008162,
42.0605493085653));
#174132=CARTESIAN_POINT('Ctrl Pts',(81.625488477662,-7.99360577730113E-15,
41.6257069626486));
#174133=CARTESIAN_POINT('Ctrl Pts',(78.3476538676923,8.08512033008161,42.355991634469));
#174134=CARTESIAN_POINT('Ctrl Pts',(70.4114119092413,11.4399698695112,43.9076792089571));
#174135=CARTESIAN_POINT('Ctrl Pts',(62.4751699507903,8.08512033008163,45.4593667834453));
#174136=CARTESIAN_POINT('Ctrl Pts',(59.1973353408206,9.76996261670138E-15,
46.1896514552657));
#174137=CARTESIAN_POINT('Ctrl Pts',(62.5272644040904,-8.08512033008161,
45.7548091093489));
#174138=CARTESIAN_POINT('Ctrl Pts',(70.5156008158414,-11.4399698695112,
44.4985638607645));
#174139=CARTESIAN_POINT('Ctrl Pts',(78.5039372275925,-8.08512033008162,
43.24231861218));
#174140=CARTESIAN_POINT('Ctrl Pts',(81.8338662908623,-1.15463194561016E-14,
42.8074762662632));
#174141=CARTESIAN_POINT('Ctrl Pts',(78.5560316808926,8.08512033008161,43.5377609380837));
#174142=CARTESIAN_POINT('Ctrl Pts',(70.6197897224416,11.4399698695112,45.0894485125718));
#174143=CARTESIAN_POINT('Ctrl Pts',(62.6835477639906,8.08512033008163,46.6411360870599));
#174144=CARTESIAN_POINT('Ctrl Pts',(59.4057131540209,1.15463194561016E-14,
47.3714207588804));
#174145=CARTESIAN_POINT('Ctrl Pts',(62.7356422172907,-8.08512033008161,
46.9365784129636));
#174146=CARTESIAN_POINT('Ctrl Pts',(70.7239786290417,-11.4399698695112,
45.6803331643791));
#174147=CARTESIAN_POINT('Ctrl Pts',(78.7123150407928,-8.08512033008162,
44.4240879157947));
#174148=CARTESIAN_POINT('Ctrl Pts',(82.0422441040625,0.,43.9892455698779));
#174149=CARTESIAN_POINT('Ctrl Pts',(78.7644094940929,8.08512033008155,44.7195302416983));
#174150=CARTESIAN_POINT('Ctrl Pts',(70.8281675356419,11.4399698695112,46.2712178161865));
#174151=CARTESIAN_POINT('Ctrl Pts',(62.8919255771909,8.08512033008161,47.8229053906746));
#174152=CARTESIAN_POINT('Ctrl Pts',(59.6140909672212,7.90478793533111E-14,
48.553190062495));
#174153=CARTESIAN_POINT('Ctrl Pts',(62.944020030491,-8.08512033008163,48.1183477165782));
#174154=CARTESIAN_POINT('Ctrl Pts',(70.932356442242,-11.4399698695112,46.8621024679938));
#174155=CARTESIAN_POINT('Ctrl Pts',(78.9206928539931,-8.08512033008157,
45.6058572194093));
#174156=CARTESIAN_POINT('Ctrl Pts',(82.2506219172628,-1.59872115546023E-14,
45.1710148734926));
#174157=CARTESIAN_POINT('Ctrl Pts',(78.9727873072932,8.08512033008155,45.901299545313));
#174158=CARTESIAN_POINT('Ctrl Pts',(71.0365453488421,11.4399698695112,47.4529871198011));
#174159=CARTESIAN_POINT('Ctrl Pts',(63.1003033903912,8.08512033008165,49.0046746942892));
#174160=CARTESIAN_POINT('Ctrl Pts',(59.8224687804215,-4.61852778244065E-14,
49.7349593661097));
#174161=CARTESIAN_POINT('Ctrl Pts',(63.1523978436912,-8.08512033008159,
49.3001170201929));
#174162=CARTESIAN_POINT('Ctrl Pts',(71.1407342554422,-11.4399698695112,
48.0438717716084));
#174163=CARTESIAN_POINT('Ctrl Pts',(79.1290706671934,-8.08512033008157,
46.787626523024));
#174164=CARTESIAN_POINT('Ctrl Pts',(82.4589997304631,-2.04281036531029E-14,
46.3527841771072));
#174165=CARTESIAN_POINT('Ctrl Pts',(79.1811651204935,8.08512033008155,47.0830688489276));
#174166=CARTESIAN_POINT('Ctrl Pts',(71.2449231620424,11.4399698695112,48.6347564234158));
#174167=CARTESIAN_POINT('Ctrl Pts',(63.3086812035915,8.08512033008162,50.1864439979039));
#174168=CARTESIAN_POINT('Ctrl Pts',(60.0308465936217,8.34887714518118E-14,
50.9167286697243));
#174169=CARTESIAN_POINT('Ctrl Pts',(63.3607756568915,-8.08512033008162,
50.4818863238076));
#174170=CARTESIAN_POINT('Ctrl Pts',(71.3491120686425,-11.4399698695112,
49.2256410752231));
#174171=CARTESIAN_POINT('Ctrl Pts',(78.4946332631429,-8.43907615989096,
48.1019368912023));
#174172=CARTESIAN_POINT('Ctrl Pts',(80.7769657380788,-4.32719180704438,
47.7849727601233));
#174173=CARTESIAN_POINT('Ctrl Pts',(81.2371482556239,-2.53805458520595,
47.7385314988347));
#174174=CARTESIAN_POINT('Ctrl Pts',(79.6939233571059,0.,37.1111929787152));
#174175=CARTESIAN_POINT('Ctrl Pts',(79.7026057659892,2.70221125641844,37.1604333663658));
#174176=CARTESIAN_POINT('Ctrl Pts',(77.5173826926761,8.08512033008161,37.6472898142461));
#174177=CARTESIAN_POINT('Ctrl Pts',(69.5811407342251,11.4399698695112,39.1989773887342));
#174178=CARTESIAN_POINT('Ctrl Pts',(61.6448987757741,8.0851203300816,40.7506649632223));
#174179=CARTESIAN_POINT('Ctrl Pts',(58.3670641658044,1.77635683940025E-15,
41.4809496350428));
#174180=CARTESIAN_POINT('Ctrl Pts',(61.6969932290742,-8.08512033008161,
41.046107289126));
#174181=CARTESIAN_POINT('Ctrl Pts',(69.6853296408252,-11.4399698695112,
39.7898620405415));
#174182=CARTESIAN_POINT('Ctrl Pts',(77.6736660525763,-8.08512033008161,
38.5336167919571));
#174183=CARTESIAN_POINT('Ctrl Pts',(81.0035951158461,-1.77635683940025E-15,
38.0987744460403));
#174184=CARTESIAN_POINT('Ctrl Pts',(77.7257605058764,8.0851203300816,38.8290591178608));
#174185=CARTESIAN_POINT('Ctrl Pts',(69.7895185474254,11.4399698695112,40.3807466923489));
#174186=CARTESIAN_POINT('Ctrl Pts',(61.8532765889744,8.08512033008162,41.932434266837));
#174187=CARTESIAN_POINT('Ctrl Pts',(58.5754419790047,3.5527136788005E-15,
42.6627189386574));
#174188=CARTESIAN_POINT('Ctrl Pts',(61.9053710422745,-8.08512033008161,
42.2278765927407));
#174189=CARTESIAN_POINT('Ctrl Pts',(69.8937074540255,-11.4399698695112,
40.9716313441562));
#174190=CARTESIAN_POINT('Ctrl Pts',(77.8820438657766,-8.08512033008162,
39.7153860955717));
#174191=CARTESIAN_POINT('Ctrl Pts',(81.2119729290464,-4.44089209850063E-15,
39.280543749655));
#174192=CARTESIAN_POINT('Ctrl Pts',(77.9341383190766,8.08512033008161,40.0108284214754));
#174193=CARTESIAN_POINT('Ctrl Pts',(69.9978963606257,11.4399698695112,41.5625159959635));
#174194=CARTESIAN_POINT('Ctrl Pts',(62.0616544021747,8.08512033008162,43.1142035704517));
#174195=CARTESIAN_POINT('Ctrl Pts',(58.783819792205,6.21724893790088E-15,
43.8444882422721));
#174196=CARTESIAN_POINT('Ctrl Pts',(62.1137488554748,-8.08512033008161,
43.4096458963553));
#174197=CARTESIAN_POINT('Ctrl Pts',(70.1020852672257,-11.4399698695112,
42.1534006477709));
#174198=CARTESIAN_POINT('Ctrl Pts',(78.0904216789768,-8.08512033008162,
40.8971553991864));
#174199=CARTESIAN_POINT('Ctrl Pts',(81.4203507422466,-7.99360577730113E-15,
40.4623130532696));
#174200=CARTESIAN_POINT('Ctrl Pts',(78.1425161322769,8.08512033008161,41.1925977250901));
#174201=CARTESIAN_POINT('Ctrl Pts',(70.2062741738259,11.4399698695112,42.7442852995782));
#174202=CARTESIAN_POINT('Ctrl Pts',(62.270032215375,8.08512033008163,44.2959728740663));
#174203=CARTESIAN_POINT('Ctrl Pts',(58.9921976054052,9.76996261670138E-15,
45.0262575458867));
#174204=CARTESIAN_POINT('Ctrl Pts',(62.322126668675,-8.08512033008161,44.59141519997));
#174205=CARTESIAN_POINT('Ctrl Pts',(70.310463080426,-11.4399698695112,43.3351699513855));
#174206=CARTESIAN_POINT('Ctrl Pts',(78.2987994921771,-8.08512033008162,
42.0789247028011));
#174207=CARTESIAN_POINT('Ctrl Pts',(81.6287285554469,-1.15463194561016E-14,
41.6440823568843));
#174208=CARTESIAN_POINT('Ctrl Pts',(78.3508939454772,8.08512033008161,42.3743670287047));
#174209=CARTESIAN_POINT('Ctrl Pts',(70.4146519870262,11.4399698695112,43.9260546031928));
#174210=CARTESIAN_POINT('Ctrl Pts',(62.4784100285753,8.08512033008163,45.477742177681));
#174211=CARTESIAN_POINT('Ctrl Pts',(59.2005754186055,1.15463194561016E-14,
46.2080268495014));
#174212=CARTESIAN_POINT('Ctrl Pts',(62.5305044818753,-8.08512033008161,
45.7731845035846));
#174213=CARTESIAN_POINT('Ctrl Pts',(70.5188408936263,-11.4399698695112,
44.5169392550002));
#174214=CARTESIAN_POINT('Ctrl Pts',(78.5071773053774,-8.08512033008162,
43.2606940064157));
#174215=CARTESIAN_POINT('Ctrl Pts',(81.8371063686472,0.,42.8258516604989));
#174216=CARTESIAN_POINT('Ctrl Pts',(78.5592717586776,8.08512033008155,43.5561363323194));
#174217=CARTESIAN_POINT('Ctrl Pts',(70.6230298002265,11.4399698695112,45.1078239068075));
#174218=CARTESIAN_POINT('Ctrl Pts',(62.6867878417755,8.08512033008161,46.6595114812956));
#174219=CARTESIAN_POINT('Ctrl Pts',(59.4089532318058,7.90478793533111E-14,
47.3897961531161));
#174220=CARTESIAN_POINT('Ctrl Pts',(62.7388822950756,-8.08512033008163,
46.9549538071993));
#174221=CARTESIAN_POINT('Ctrl Pts',(70.7272187068266,-11.4399698695112,
45.6987085586148));
#174222=CARTESIAN_POINT('Ctrl Pts',(78.7155551185777,-8.08512033008157,
44.4424633100304));
#174223=CARTESIAN_POINT('Ctrl Pts',(82.0454841818474,-1.59872115546023E-14,
44.0076209641136));
#174224=CARTESIAN_POINT('Ctrl Pts',(78.7676495718778,8.08512033008155,44.737905635934));
#174225=CARTESIAN_POINT('Ctrl Pts',(70.8314076134267,11.4399698695112,46.2895932104222));
#174226=CARTESIAN_POINT('Ctrl Pts',(62.8951656549758,8.08512033008165,47.8412807849103));
#174227=CARTESIAN_POINT('Ctrl Pts',(59.6173310450061,-4.61852778244065E-14,
48.5715654567307));
#174228=CARTESIAN_POINT('Ctrl Pts',(62.9472601082759,-8.08512033008159,
48.1367231108139));
#174229=CARTESIAN_POINT('Ctrl Pts',(70.9355965200269,-11.4399698695112,
46.8804778622295));
#174230=CARTESIAN_POINT('Ctrl Pts',(78.923932931778,-8.08512033008157,45.624232613645));
#174231=CARTESIAN_POINT('Ctrl Pts',(82.2538619950477,-2.04281036531029E-14,
45.1893902677283));
#174232=CARTESIAN_POINT('Ctrl Pts',(78.9760273850781,8.08512033008155,45.9196749395487));
#174233=CARTESIAN_POINT('Ctrl Pts',(71.039785426627,11.4399698695112,47.4713625140368));
#174234=CARTESIAN_POINT('Ctrl Pts',(63.1035434681761,8.08512033008162,49.0230500885249));
#174235=CARTESIAN_POINT('Ctrl Pts',(59.8257088582064,8.34887714518118E-14,
49.7533347603454));
#174236=CARTESIAN_POINT('Ctrl Pts',(63.1556379214762,-8.08512033008162,
49.3184924144286));
#174237=CARTESIAN_POINT('Ctrl Pts',(71.1439743332271,-11.4399698695112,
48.0622471658441));
#174238=CARTESIAN_POINT('Ctrl Pts',(78.2894955277276,-8.43907615989096,
46.9385429818233));
#174239=CARTESIAN_POINT('Ctrl Pts',(80.5718280026635,-4.32719180704438,
46.6215788507443));
#174240=CARTESIAN_POINT('Ctrl Pts',(81.0320105202085,-2.53805458520595,
46.5751375894558));
#174241=CARTESIAN_POINT('Ctrl Pts',(78.7231713724909,0.,37.8560771751443));
#174242=CARTESIAN_POINT('Ctrl Pts',(78.7318537813743,2.41806680288088,37.9053175627949));
#174243=CARTESIAN_POINT('Ctrl Pts',(76.778238481581,7.2349491628497,38.3513353112619));
#174244=CARTESIAN_POINT('Ctrl Pts',(69.6792516800074,10.2370276571518,39.7553922118552));
#174245=CARTESIAN_POINT('Ctrl Pts',(62.5802648784339,7.23494916284969,41.1594491124486));
#174246=CARTESIAN_POINT('Ctrl Pts',(59.6498419287439,1.77635683940025E-15,
41.828475735149));
#174247=CARTESIAN_POINT('Ctrl Pts',(62.6323593317339,-7.2349491628497,41.4548914383522));
#174248=CARTESIAN_POINT('Ctrl Pts',(69.7834405866076,-10.2370276571518,
40.3462768636625));
#174249=CARTESIAN_POINT('Ctrl Pts',(76.9345218414812,-7.2349491628497,39.2376622889728));
#174250=CARTESIAN_POINT('Ctrl Pts',(79.9170392444712,-1.77635683940025E-15,
38.8640779921761));
#174251=CARTESIAN_POINT('Ctrl Pts',(76.9866162947813,7.23494916284969,39.5331046148765));
#174252=CARTESIAN_POINT('Ctrl Pts',(69.8876294932077,10.2370276571518,40.9371615154699));
#174253=CARTESIAN_POINT('Ctrl Pts',(62.7886426916342,7.23494916284971,42.3412184160632));
#174254=CARTESIAN_POINT('Ctrl Pts',(59.8582197419442,3.5527136788005E-15,
43.0102450387636));
#174255=CARTESIAN_POINT('Ctrl Pts',(62.8407371449342,-7.23494916284971,
42.6366607419669));
#174256=CARTESIAN_POINT('Ctrl Pts',(69.9918183998079,-10.2370276571518,
41.5280461672772));
#174257=CARTESIAN_POINT('Ctrl Pts',(77.1428996546815,-7.23494916284971,
40.4194315925875));
#174258=CARTESIAN_POINT('Ctrl Pts',(80.1254170576715,-4.44089209850063E-15,
40.0458472957908));
#174259=CARTESIAN_POINT('Ctrl Pts',(77.1949941079816,7.2349491628497,40.7148739184912));
#174260=CARTESIAN_POINT('Ctrl Pts',(70.096007306408,10.2370276571518,42.1189308190845));
#174261=CARTESIAN_POINT('Ctrl Pts',(62.9970205048345,7.23494916284972,43.5229877196779));
#174262=CARTESIAN_POINT('Ctrl Pts',(60.0665975551445,6.21724893790088E-15,
44.1920143423783));
#174263=CARTESIAN_POINT('Ctrl Pts',(63.0491149581345,-7.23494916284971,
43.8184300455816));
#174264=CARTESIAN_POINT('Ctrl Pts',(70.2001962130081,-10.2370276571518,
42.7098154708919));
#174265=CARTESIAN_POINT('Ctrl Pts',(77.3512774678818,-7.23494916284971,
41.6012008962022));
#174266=CARTESIAN_POINT('Ctrl Pts',(80.3337948708718,-7.99360577730113E-15,
41.2276165994054));
#174267=CARTESIAN_POINT('Ctrl Pts',(77.4033719211819,7.2349491628497,41.8966432221058));
#174268=CARTESIAN_POINT('Ctrl Pts',(70.3043851196083,10.2370276571518,43.3007001226992));
#174269=CARTESIAN_POINT('Ctrl Pts',(63.2053983180347,7.23494916284972,44.7047570232925));
#174270=CARTESIAN_POINT('Ctrl Pts',(60.2749753683448,9.76996261670138E-15,
45.3737836459929));
#174271=CARTESIAN_POINT('Ctrl Pts',(63.2574927713348,-7.23494916284971,
45.0001993491962));
#174272=CARTESIAN_POINT('Ctrl Pts',(70.4085740262084,-10.2370276571518,
43.8915847745065));
#174273=CARTESIAN_POINT('Ctrl Pts',(77.5596552810821,-7.23494916284971,
42.7829701998168));
#174274=CARTESIAN_POINT('Ctrl Pts',(80.5421726840721,-1.15463194561016E-14,
42.4093859030201));
#174275=CARTESIAN_POINT('Ctrl Pts',(77.6117497343821,7.2349491628497,43.0784125257205));
#174276=CARTESIAN_POINT('Ctrl Pts',(70.5127629328085,10.2370276571518,44.4824694263138));
#174277=CARTESIAN_POINT('Ctrl Pts',(63.413776131235,7.23494916284972,45.8865263269072));
#174278=CARTESIAN_POINT('Ctrl Pts',(60.483353181545,1.15463194561016E-14,
46.5555529496076));
#174279=CARTESIAN_POINT('Ctrl Pts',(63.4658705845351,-7.2349491628497,46.1819686528109));
#174280=CARTESIAN_POINT('Ctrl Pts',(70.6169518394087,-10.2370276571518,
45.0733540781212));
#174281=CARTESIAN_POINT('Ctrl Pts',(77.7680330942823,-7.23494916284971,
43.9647395034315));
#174282=CARTESIAN_POINT('Ctrl Pts',(80.7505504972723,0.,43.5911552066347));
#174283=CARTESIAN_POINT('Ctrl Pts',(77.8201275475825,7.23494916284965,44.2601818293351));
#174284=CARTESIAN_POINT('Ctrl Pts',(70.7211407460088,10.2370276571518,45.6642387299285));
#174285=CARTESIAN_POINT('Ctrl Pts',(63.6221539444353,7.23494916284971,47.0682956305219));
#174286=CARTESIAN_POINT('Ctrl Pts',(60.6917309947453,7.90478793533111E-14,
47.7373222532223));
#174287=CARTESIAN_POINT('Ctrl Pts',(63.6742483977354,-7.23494916284972,
47.3637379564255));
#174288=CARTESIAN_POINT('Ctrl Pts',(70.8253296526089,-10.2370276571518,
46.2551233817358));
#174289=CARTESIAN_POINT('Ctrl Pts',(77.9764109074827,-7.23494916284967,
45.1465088070461));
#174290=CARTESIAN_POINT('Ctrl Pts',(80.9589283104726,-1.59872115546023E-14,
44.7729245102494));
#174291=CARTESIAN_POINT('Ctrl Pts',(78.0285053607827,7.23494916284965,45.4419511329498));
#174292=CARTESIAN_POINT('Ctrl Pts',(70.9295185592091,10.2370276571518,46.8460080335432));
#174293=CARTESIAN_POINT('Ctrl Pts',(63.8305317576356,7.23494916284974,48.2500649341365));
#174294=CARTESIAN_POINT('Ctrl Pts',(60.9001088079456,-4.61852778244065E-14,
48.9190915568369));
#174295=CARTESIAN_POINT('Ctrl Pts',(63.8826262109356,-7.23494916284968,
48.5455072600402));
#174296=CARTESIAN_POINT('Ctrl Pts',(71.0337074658092,-10.2370276571518,
47.4368926853505));
#174297=CARTESIAN_POINT('Ctrl Pts',(78.1847887206829,-7.23494916284967,
46.3282781106608));
#174298=CARTESIAN_POINT('Ctrl Pts',(81.1673061236729,-2.04281036531029E-14,
45.9546938138641));
#174299=CARTESIAN_POINT('Ctrl Pts',(78.236883173983,7.23494916284965,46.6237204365644));
#174300=CARTESIAN_POINT('Ctrl Pts',(71.1378963724094,10.2370276571518,48.0277773371578));
#174301=CARTESIAN_POINT('Ctrl Pts',(64.0389095708359,7.23494916284971,49.4318342377512));
#174302=CARTESIAN_POINT('Ctrl Pts',(61.1084866211459,8.34887714518118E-14,
50.1008608604516));
#174303=CARTESIAN_POINT('Ctrl Pts',(64.0910040241359,-7.23494916284971,
49.7272765636548));
#174304=CARTESIAN_POINT('Ctrl Pts',(71.2420852790095,-10.2370276571518,
48.6186619889651));
#174305=CARTESIAN_POINT('Ctrl Pts',(77.6386865281917,-7.55168562811132,
47.6270125976946));
#174306=CARTESIAN_POINT('Ctrl Pts',(79.6825628639114,-3.87217647526957,
47.352094717675));
#174307=CARTESIAN_POINT('Ctrl Pts',(80.0949800123844,-2.27117162724,47.3140757796973));
#174308=CARTESIAN_POINT('Ctrl Pts',(82.4182377853508,-4.33680868994202E-16,
57.4564977112756));
#174309=CARTESIAN_POINT('Ctrl Pts',(82.4135348138723,-2.47968200709192,
57.4298258346316));
#174310=CARTESIAN_POINT('Ctrl Pts',(80.3829258470673,-7.41930423095383,
57.7328747079373));
#174311=CARTESIAN_POINT('Ctrl Pts',(73.0622286040322,-10.4978792386127,
58.9412077372665));
#174312=CARTESIAN_POINT('Ctrl Pts',(65.7415313609972,-7.41930423095383,
60.1495407665957));
#174313=CARTESIAN_POINT('Ctrl Pts',(62.6956179107897,-2.21003770839445E-15,
60.6041140765543));
#174314=CARTESIAN_POINT('Ctrl Pts',(65.7133135321263,7.41930423095382,59.9895095067313));
#174315=CARTESIAN_POINT('Ctrl Pts',(73.0057929462905,10.4978792386127,58.6211452175376));
#174316=CARTESIAN_POINT('Ctrl Pts',(80.2982723604547,7.41930423095383,57.2527809283438));
#174317=CARTESIAN_POINT('Ctrl Pts',(83.3159679817913,1.78676518025611E-15,
56.6381763585208));
#174318=CARTESIAN_POINT('Ctrl Pts',(80.2700545315838,-7.41930423095382,
57.0927496684794));
#174319=CARTESIAN_POINT('Ctrl Pts',(72.9493572885488,-10.4978792386127,
58.3010826978086));
#174320=CARTESIAN_POINT('Ctrl Pts',(65.6286600455137,-7.41930423095384,
59.5094157271378));
#174321=CARTESIAN_POINT('Ctrl Pts',(62.5827465953062,-3.54230533794464E-15,
59.9639890370964));
#174322=CARTESIAN_POINT('Ctrl Pts',(65.6004422166428,7.41930423095383,59.3493844672733));
#174323=CARTESIAN_POINT('Ctrl Pts',(72.892921630807,10.4978792386127,57.9810201780796));
#174324=CARTESIAN_POINT('Ctrl Pts',(80.1854010449712,7.41930423095384,56.6126558888859));
#174325=CARTESIAN_POINT('Ctrl Pts',(83.2030966663078,5.33947885905661E-15,
55.9980513190628));
#174326=CARTESIAN_POINT('Ctrl Pts',(80.1571832161003,-7.41930423095383,
56.4526246290214));
#174327=CARTESIAN_POINT('Ctrl Pts',(72.8364859730653,-10.4978792386127,
57.6609576583506));
#174328=CARTESIAN_POINT('Ctrl Pts',(65.5157887300302,-7.41930423095384,
58.8692906876799));
#174329=CARTESIAN_POINT('Ctrl Pts',(62.4698752798227,-7.5391082265952E-15,
59.3238639976385));
#174330=CARTESIAN_POINT('Ctrl Pts',(65.4875709011593,7.41930423095383,58.7092594278154));
#174331=CARTESIAN_POINT('Ctrl Pts',(72.7800503153235,10.4978792386127,57.3408951386217));
#174332=CARTESIAN_POINT('Ctrl Pts',(80.0725297294877,7.41930423095384,55.972530849428));
#174333=CARTESIAN_POINT('Ctrl Pts',(83.0902253508243,7.11583569845686E-15,
55.3579262796049));
#174334=CARTESIAN_POINT('Ctrl Pts',(80.0443119006168,-7.41930423095383,
55.8124995895635));
#174335=CARTESIAN_POINT('Ctrl Pts',(72.7236146575817,-10.4978792386127,
57.0208326188927));
#174336=CARTESIAN_POINT('Ctrl Pts',(65.4029174145467,-7.41930423095385,
58.2291656482219));
#174337=CARTESIAN_POINT('Ctrl Pts',(62.3570039643392,-9.31546506599545E-15,
58.6837389581805));
#174338=CARTESIAN_POINT('Ctrl Pts',(65.3746995856758,7.41930423095384,58.0691343883574));
#174339=CARTESIAN_POINT('Ctrl Pts',(72.66717899984,10.4978792386127,56.7007700991637));
#174340=CARTESIAN_POINT('Ctrl Pts',(79.9596584140042,7.41930423095385,55.33240580997));
#174341=CARTESIAN_POINT('Ctrl Pts',(82.9773540353409,9.33628174770718E-15,
54.717801240147));
#174342=CARTESIAN_POINT('Ctrl Pts',(79.9314405851334,-7.41930423095383,
55.1723745501055));
#174343=CARTESIAN_POINT('Ctrl Pts',(72.6107433420983,-10.4978792386127,
56.3807075794348));
#174344=CARTESIAN_POINT('Ctrl Pts',(65.2900460990632,-7.41930423095385,
57.589040608764));
#174345=CARTESIAN_POINT('Ctrl Pts',(62.2441326488557,-1.24240895349459E-14,
58.0436139187226));
#174346=CARTESIAN_POINT('Ctrl Pts',(65.2618282701924,7.41930423095383,57.4290093488995));
#174347=CARTESIAN_POINT('Ctrl Pts',(72.5543076843565,10.4978792386127,56.0606450597058));
#174348=CARTESIAN_POINT('Ctrl Pts',(79.8467870985207,7.41930423095385,54.6922807705121));
#174349=CARTESIAN_POINT('Ctrl Pts',(82.8644827198574,1.04083408558608E-17,
54.077676200689));
#174350=CARTESIAN_POINT('Ctrl Pts',(79.8185692696499,-7.41930423095378,
54.5322495106476));
#174351=CARTESIAN_POINT('Ctrl Pts',(72.4978720266148,-10.4978792386127,
55.7405825399768));
#174352=CARTESIAN_POINT('Ctrl Pts',(65.1771747835797,-7.41930423095383,
56.9489155693061));
#174353=CARTESIAN_POINT('Ctrl Pts',(62.1312613333722,-7.81492925927552E-14,
57.4034888792646));
#174354=CARTESIAN_POINT('Ctrl Pts',(65.1489569547089,7.41930423095385,56.7888843094416));
#174355=CARTESIAN_POINT('Ctrl Pts',(72.441436368873,10.4978792386127,55.4205200202479));
#174356=CARTESIAN_POINT('Ctrl Pts',(79.7339157830373,7.4193042309538,54.0521557310541));
#174357=CARTESIAN_POINT('Ctrl Pts',(82.7516114043739,1.5109441475758E-14,
53.4375511612311));
#174358=CARTESIAN_POINT('Ctrl Pts',(79.7056979541665,-7.41930423095378,
53.8921244711896));
#174359=CARTESIAN_POINT('Ctrl Pts',(72.3850007111313,-10.4978792386127,
55.1004575005189));
#174360=CARTESIAN_POINT('Ctrl Pts',(65.0643034680963,-7.41930423095387,
56.3087905298481));
#174361=CARTESIAN_POINT('Ctrl Pts',(62.0183900178887,4.44193293258621E-14,
56.7633638398067));
#174362=CARTESIAN_POINT('Ctrl Pts',(65.0360856392254,7.41930423095381,56.1487592699836));
#174363=CARTESIAN_POINT('Ctrl Pts',(72.3285650533895,10.4978792386127,54.7803949807899));
#174364=CARTESIAN_POINT('Ctrl Pts',(79.6210444675538,7.4193042309538,53.4120306915962));
#174365=CARTESIAN_POINT('Ctrl Pts',(82.6387400888904,1.77739767348584E-14,
52.7974261217731));
#174366=CARTESIAN_POINT('Ctrl Pts',(79.592826638683,-7.41930423095377,53.2519994317317));
#174367=CARTESIAN_POINT('Ctrl Pts',(72.2721293956478,-10.4978792386127,
54.460332461061));
#174368=CARTESIAN_POINT('Ctrl Pts',(64.9514321526128,-7.41930423095384,
55.6686654903902));
#174369=CARTESIAN_POINT('Ctrl Pts',(61.9055187024052,-8.21460954814057E-14,
56.1232388003488));
#174370=CARTESIAN_POINT('Ctrl Pts',(64.9232143237419,7.41930423095385,55.5086342305257));
#174371=CARTESIAN_POINT('Ctrl Pts',(72.215693737906,10.4978792386127,54.140269941332));
#174372=CARTESIAN_POINT('Ctrl Pts',(79.5081731520703,7.41930423095381,52.7719056521383));
#174373=CARTESIAN_POINT('Ctrl Pts',(82.5258687734069,2.04385119939587E-14,
52.1573010823152));
#174374=CARTESIAN_POINT('Ctrl Pts',(79.4799553231995,-7.41930423095377,
52.6118743922738));
#174375=CARTESIAN_POINT('Ctrl Pts',(72.1592580801643,-10.4978792386127,
53.820207421603));
#174376=CARTESIAN_POINT('Ctrl Pts',(64.8385608371293,-7.41930423095387,
55.0285404509322));
#174377=CARTESIAN_POINT('Ctrl Pts',(61.7926473869218,3.95343480175114E-14,
55.4831137608908));
#174378=CARTESIAN_POINT('Ctrl Pts',(64.8103430082584,7.41930423095381,54.8685091910678));
#174379=CARTESIAN_POINT('Ctrl Pts',(72.1028224224225,10.4978792386127,53.5001449018741));
#174380=CARTESIAN_POINT('Ctrl Pts',(79.3953018365868,7.4193042309538,52.1317806126803));
#174381=CARTESIAN_POINT('Ctrl Pts',(82.4129974579234,2.39912256727592E-14,
51.5171760428573));
#174382=CARTESIAN_POINT('Ctrl Pts',(79.4795767970927,-7.14529177399519,
51.9549608851035));
#174383=CARTESIAN_POINT('Ctrl Pts',(75.0186143089714,-9.23540832385942,
52.6895937030669));
#174384=CARTESIAN_POINT('Ctrl Pts',(72.8565297133897,-9.43430675859939,
53.0463734606267));
#174385=CARTESIAN_POINT('Ctrl Pts',(82.9022195620938,-4.33680868994202E-16,
57.0503887809141));
#174386=CARTESIAN_POINT('Ctrl Pts',(82.8975165906153,-2.62292530172754,
57.02371690427));
#174387=CARTESIAN_POINT('Ctrl Pts',(80.7501491929166,-7.84789369480698,
57.3473534391675));
#174388=CARTESIAN_POINT('Ctrl Pts',(73.0073737230196,-11.1043081293031,
58.630110247862));
#174389=CARTESIAN_POINT('Ctrl Pts',(65.2645982531226,-7.84789369480698,
59.9128670565566));
#174390=CARTESIAN_POINT('Ctrl Pts',(62.0435471565745,-2.21003770839445E-15,
60.3983218589028));
#174391=CARTESIAN_POINT('Ctrl Pts',(65.2363804242517,7.84789369480698,59.7528357966921));
#174392=CARTESIAN_POINT('Ctrl Pts',(72.9509380652778,11.1043081293031,58.3100477281331));
#174393=CARTESIAN_POINT('Ctrl Pts',(80.665495706304,7.84789369480698,56.867259659574));
#174394=CARTESIAN_POINT('Ctrl Pts',(83.8583289739812,1.78676518025611E-15,
56.2217735973633));
#174395=CARTESIAN_POINT('Ctrl Pts',(80.6372778774331,-7.84789369480698,
56.7072283997095));
#174396=CARTESIAN_POINT('Ctrl Pts',(72.8945024075361,-11.1043081293031,
57.9899852084041));
#174397=CARTESIAN_POINT('Ctrl Pts',(65.1517269376391,-7.847893694807,59.2727420170987));
#174398=CARTESIAN_POINT('Ctrl Pts',(61.930675841091,-3.54230533794464E-15,
59.7581968194449));
#174399=CARTESIAN_POINT('Ctrl Pts',(65.1235091087682,7.84789369480699,59.1127107572342));
#174400=CARTESIAN_POINT('Ctrl Pts',(72.8380667497943,11.1043081293031,57.6699226886751));
#174401=CARTESIAN_POINT('Ctrl Pts',(80.5526243908205,7.847893694807,56.2271346201161));
#174402=CARTESIAN_POINT('Ctrl Pts',(83.7454576584977,5.33947885905661E-15,
55.5816485579054));
#174403=CARTESIAN_POINT('Ctrl Pts',(80.5244065619496,-7.84789369480699,
56.0671033602516));
#174404=CARTESIAN_POINT('Ctrl Pts',(72.7816310920526,-11.1043081293031,
57.3498601689462));
#174405=CARTESIAN_POINT('Ctrl Pts',(65.0388556221556,-7.847893694807,58.6326169776407));
#174406=CARTESIAN_POINT('Ctrl Pts',(61.8178045256075,-7.5391082265952E-15,
59.1180717799869));
#174407=CARTESIAN_POINT('Ctrl Pts',(65.0106377932847,7.84789369480699,58.4725857177762));
#174408=CARTESIAN_POINT('Ctrl Pts',(72.7251954343108,11.1043081293031,57.0297976492172));
#174409=CARTESIAN_POINT('Ctrl Pts',(80.439753075337,7.84789369480699,55.5870095806582));
#174410=CARTESIAN_POINT('Ctrl Pts',(83.6325863430142,7.11583569845686E-15,
54.9415235184475));
#174411=CARTESIAN_POINT('Ctrl Pts',(80.4115352464661,-7.84789369480698,
55.4269783207937));
#174412=CARTESIAN_POINT('Ctrl Pts',(72.6687597765691,-11.1043081293031,
56.7097351294882));
#174413=CARTESIAN_POINT('Ctrl Pts',(64.9259843066721,-7.847893694807,57.9924919381828));
#174414=CARTESIAN_POINT('Ctrl Pts',(61.704933210124,-9.31546506599545E-15,
58.477946740529));
#174415=CARTESIAN_POINT('Ctrl Pts',(64.8977664778012,7.84789369480699,57.8324606783183));
#174416=CARTESIAN_POINT('Ctrl Pts',(72.6123241188273,11.1043081293031,56.3896726097593));
#174417=CARTESIAN_POINT('Ctrl Pts',(80.3268817598535,7.847893694807,54.9468845412002));
#174418=CARTESIAN_POINT('Ctrl Pts',(83.5197150275307,9.33628174770718E-15,
54.3013984789895));
#174419=CARTESIAN_POINT('Ctrl Pts',(80.2986639309826,-7.84789369480698,
54.7868532813357));
#174420=CARTESIAN_POINT('Ctrl Pts',(72.5558884610856,-11.1043081293031,
56.0696100900303));
#174421=CARTESIAN_POINT('Ctrl Pts',(64.8131129911886,-7.847893694807,57.3523668987248));
#174422=CARTESIAN_POINT('Ctrl Pts',(61.5920618946405,-1.24240895349459E-14,
57.8378217010711));
#174423=CARTESIAN_POINT('Ctrl Pts',(64.7848951623178,7.84789369480698,57.1923356388604));
#174424=CARTESIAN_POINT('Ctrl Pts',(72.4994528033438,11.1043081293031,55.7495475703013));
#174425=CARTESIAN_POINT('Ctrl Pts',(80.21401044437,7.847893694807,54.3067595017423));
#174426=CARTESIAN_POINT('Ctrl Pts',(83.4068437120472,1.04083408558608E-17,
53.6612734395316));
#174427=CARTESIAN_POINT('Ctrl Pts',(80.1857926154992,-7.84789369480693,
54.1467282418778));
#174428=CARTESIAN_POINT('Ctrl Pts',(72.4430171456021,-11.1043081293031,
55.4294850505724));
#174429=CARTESIAN_POINT('Ctrl Pts',(64.7002416757051,-7.84789369480699,
56.7122418592669));
#174430=CARTESIAN_POINT('Ctrl Pts',(61.479190579157,-7.81492925927552E-14,
57.1976966616131));
#174431=CARTESIAN_POINT('Ctrl Pts',(64.6720238468343,7.847893694807,56.5522105994024));
#174432=CARTESIAN_POINT('Ctrl Pts',(72.3865814878603,11.1043081293031,55.1094225308434));
#174433=CARTESIAN_POINT('Ctrl Pts',(80.1011391288866,7.84789369480695,53.6666344622843));
#174434=CARTESIAN_POINT('Ctrl Pts',(83.2939723965637,1.5109441475758E-14,
53.0211484000736));
#174435=CARTESIAN_POINT('Ctrl Pts',(80.0729213000157,-7.84789369480693,
53.5066032024198));
#174436=CARTESIAN_POINT('Ctrl Pts',(72.3301458301186,-11.1043081293031,
54.7893600111144));
#174437=CARTESIAN_POINT('Ctrl Pts',(64.5873703602217,-7.84789369480702,
56.072116819809));
#174438=CARTESIAN_POINT('Ctrl Pts',(61.3663192636735,4.44193293258621E-14,
56.5575716221552));
#174439=CARTESIAN_POINT('Ctrl Pts',(64.5591525313508,7.84789369480696,55.9120855599445));
#174440=CARTESIAN_POINT('Ctrl Pts',(72.2737101723769,11.1043081293031,54.4692974913855));
#174441=CARTESIAN_POINT('Ctrl Pts',(79.9882678134031,7.84789369480695,53.0265094228264));
#174442=CARTESIAN_POINT('Ctrl Pts',(83.1811010810802,1.77739767348584E-14,
52.3810233606157));
#174443=CARTESIAN_POINT('Ctrl Pts',(79.9600499845322,-7.84789369480693,
52.8664781629619));
#174444=CARTESIAN_POINT('Ctrl Pts',(72.2172745146351,-11.1043081293031,
54.1492349716565));
#174445=CARTESIAN_POINT('Ctrl Pts',(64.4744990447382,-7.84789369480699,
55.431991780351));
#174446=CARTESIAN_POINT('Ctrl Pts',(61.2534479481901,-8.21460954814057E-14,
55.9174465826972));
#174447=CARTESIAN_POINT('Ctrl Pts',(64.4462812158673,7.847893694807,55.2719605204866));
#174448=CARTESIAN_POINT('Ctrl Pts',(72.1608388568933,11.1043081293031,53.8291724519275));
#174449=CARTESIAN_POINT('Ctrl Pts',(79.8753964979196,7.84789369480696,52.3863843833685));
#174450=CARTESIAN_POINT('Ctrl Pts',(83.0682297655968,2.04385119939587E-14,
51.7408983211578));
#174451=CARTESIAN_POINT('Ctrl Pts',(79.8471786690487,-7.84789369480692,
52.226353123504));
#174452=CARTESIAN_POINT('Ctrl Pts',(72.1044031991516,-11.1043081293031,
53.5091099321985));
#174453=CARTESIAN_POINT('Ctrl Pts',(64.3616277292547,-7.84789369480703,
54.7918667408931));
#174454=CARTESIAN_POINT('Ctrl Pts',(61.1405766327066,3.95343480175114E-14,
55.2773215432393));
#174455=CARTESIAN_POINT('Ctrl Pts',(64.3334099003838,7.84789369480696,54.6318354810286));
#174456=CARTESIAN_POINT('Ctrl Pts',(72.0479675414099,11.1043081293031,53.1890474124696));
#174457=CARTESIAN_POINT('Ctrl Pts',(79.7625251824361,7.84789369480696,51.7462593439105));
#174458=CARTESIAN_POINT('Ctrl Pts',(82.9553584501133,2.39912256727592E-14,
51.1007732816998));
#174459=CARTESIAN_POINT('Ctrl Pts',(79.8532683905412,-7.55805241504216,
51.568299089764));
#174460=CARTESIAN_POINT('Ctrl Pts',(75.1351236247948,-9.76890830967669,
52.3482800822328));
#174461=CARTESIAN_POINT('Ctrl Pts',(72.8483838954811,-9.97929647052207,
52.7270399031534));
#174462=CARTESIAN_POINT('Ctrl Pts',(83.0141466356044,-4.33680868994202E-16,
57.6851587580378));
#174463=CARTESIAN_POINT('Ctrl Pts',(83.0094436641259,-2.62292530172754,
57.6584868813937));
#174464=CARTESIAN_POINT('Ctrl Pts',(80.8620762664272,-7.84789369480698,
57.9821234162912));
#174465=CARTESIAN_POINT('Ctrl Pts',(73.1193007965301,-11.1043081293031,
59.2648802249857));
#174466=CARTESIAN_POINT('Ctrl Pts',(65.3765253266331,-7.84789369480698,
60.5476370336803));
#174467=CARTESIAN_POINT('Ctrl Pts',(62.155474230085,-2.21003770839445E-15,
61.0330918360265));
#174468=CARTESIAN_POINT('Ctrl Pts',(65.3483074977623,7.84789369480698,60.3876057738158));
#174469=CARTESIAN_POINT('Ctrl Pts',(73.0628651387884,11.1043081293031,58.9448177052568));
#174470=CARTESIAN_POINT('Ctrl Pts',(80.7774227798145,7.84789369480698,57.5020296366977));
#174471=CARTESIAN_POINT('Ctrl Pts',(83.9702560474918,1.78676518025611E-15,
56.856543574487));
#174472=CARTESIAN_POINT('Ctrl Pts',(80.7492049509437,-7.84789369480698,
57.3419983768332));
#174473=CARTESIAN_POINT('Ctrl Pts',(73.0064294810467,-11.1043081293031,
58.6247551855278));
#174474=CARTESIAN_POINT('Ctrl Pts',(65.2636540111497,-7.847893694807,59.9075119942224));
#174475=CARTESIAN_POINT('Ctrl Pts',(62.0426029146016,-3.54230533794464E-15,
60.3929667965686));
#174476=CARTESIAN_POINT('Ctrl Pts',(65.2354361822788,7.84789369480699,59.7474807343579));
#174477=CARTESIAN_POINT('Ctrl Pts',(72.9499938233049,11.1043081293031,58.3046926657988));
#174478=CARTESIAN_POINT('Ctrl Pts',(80.664551464331,7.847893694807,56.8619045972398));
#174479=CARTESIAN_POINT('Ctrl Pts',(83.8573847320083,5.33947885905661E-15,
56.2164185350291));
#174480=CARTESIAN_POINT('Ctrl Pts',(80.6363336354602,-7.84789369480699,
56.7018733373753));
#174481=CARTESIAN_POINT('Ctrl Pts',(72.8935581655632,-11.1043081293031,
57.9846301460699));
#174482=CARTESIAN_POINT('Ctrl Pts',(65.1507826956662,-7.847893694807,59.2673869547644));
#174483=CARTESIAN_POINT('Ctrl Pts',(61.9297315991181,-7.5391082265952E-15,
59.7528417571106));
#174484=CARTESIAN_POINT('Ctrl Pts',(65.1225648667953,7.84789369480699,59.1073556948999));
#174485=CARTESIAN_POINT('Ctrl Pts',(72.8371225078214,11.1043081293031,57.6645676263409));
#174486=CARTESIAN_POINT('Ctrl Pts',(80.5516801488476,7.84789369480699,56.2217795577819));
#174487=CARTESIAN_POINT('Ctrl Pts',(83.7445134165248,7.11583569845686E-15,
55.5762934955712));
#174488=CARTESIAN_POINT('Ctrl Pts',(80.5234623199767,-7.84789369480698,
56.0617482979174));
#174489=CARTESIAN_POINT('Ctrl Pts',(72.7806868500797,-11.1043081293031,
57.3445051066119));
#174490=CARTESIAN_POINT('Ctrl Pts',(65.0379113801827,-7.847893694807,58.6272619153065));
#174491=CARTESIAN_POINT('Ctrl Pts',(61.8168602836346,-9.31546506599545E-15,
59.1127167176527));
#174492=CARTESIAN_POINT('Ctrl Pts',(65.0096935513118,7.84789369480699,58.467230655442));
#174493=CARTESIAN_POINT('Ctrl Pts',(72.7242511923379,11.1043081293031,57.024442586883));
#174494=CARTESIAN_POINT('Ctrl Pts',(80.4388088333641,7.847893694807,55.5816545183239));
#174495=CARTESIAN_POINT('Ctrl Pts',(83.6316421010413,9.33628174770718E-15,
54.9361684561132));
#174496=CARTESIAN_POINT('Ctrl Pts',(80.4105910044932,-7.84789369480698,
55.4216232584594));
#174497=CARTESIAN_POINT('Ctrl Pts',(72.6678155345962,-11.1043081293031,
56.704380067154));
#174498=CARTESIAN_POINT('Ctrl Pts',(64.9250400646992,-7.847893694807,57.9871368758485));
#174499=CARTESIAN_POINT('Ctrl Pts',(61.7039889681511,-1.24240895349459E-14,
58.4725916781948));
#174500=CARTESIAN_POINT('Ctrl Pts',(64.8968222358283,7.84789369480698,57.8271056159841));
#174501=CARTESIAN_POINT('Ctrl Pts',(72.6113798768544,11.1043081293031,56.384317547425));
#174502=CARTESIAN_POINT('Ctrl Pts',(80.3259375178806,7.847893694807,54.941529478866));
#174503=CARTESIAN_POINT('Ctrl Pts',(83.5187707855578,1.04083408558608E-17,
54.2960434166553));
#174504=CARTESIAN_POINT('Ctrl Pts',(80.2977196890098,-7.84789369480693,
54.7814982190015));
#174505=CARTESIAN_POINT('Ctrl Pts',(72.5549442191127,-11.1043081293031,
56.0642550276961));
#174506=CARTESIAN_POINT('Ctrl Pts',(64.8121687492157,-7.84789369480699,
57.3470118363906));
#174507=CARTESIAN_POINT('Ctrl Pts',(61.5911176526676,-7.81492925927552E-14,
57.8324666387368));
#174508=CARTESIAN_POINT('Ctrl Pts',(64.7839509203449,7.847893694807,57.1869805765261));
#174509=CARTESIAN_POINT('Ctrl Pts',(72.4985085613709,11.1043081293031,55.7441925079671));
#174510=CARTESIAN_POINT('Ctrl Pts',(80.2130662023972,7.84789369480695,54.301404439408));
#174511=CARTESIAN_POINT('Ctrl Pts',(83.4058994700743,1.5109441475758E-14,
53.6559183771974));
#174512=CARTESIAN_POINT('Ctrl Pts',(80.1848483735263,-7.84789369480693,
54.1413731795435));
#174513=CARTESIAN_POINT('Ctrl Pts',(72.4420729036292,-11.1043081293031,
55.4241299882381));
#174514=CARTESIAN_POINT('Ctrl Pts',(64.6992974337323,-7.84789369480702,
56.7068867969327));
#174515=CARTESIAN_POINT('Ctrl Pts',(61.4782463371841,4.44193293258621E-14,
57.1923415992789));
#174516=CARTESIAN_POINT('Ctrl Pts',(64.6710796048613,7.84789369480696,56.5468555370682));
#174517=CARTESIAN_POINT('Ctrl Pts',(72.3856372458874,11.1043081293031,55.1040674685092));
#174518=CARTESIAN_POINT('Ctrl Pts',(80.1001948869137,7.84789369480695,53.6612793999501));
#174519=CARTESIAN_POINT('Ctrl Pts',(83.2930281545908,1.77739767348584E-14,
53.0157933377394));
#174520=CARTESIAN_POINT('Ctrl Pts',(80.0719770580428,-7.84789369480693,
53.5012481400856));
#174521=CARTESIAN_POINT('Ctrl Pts',(72.3292015881457,-11.1043081293031,
54.7840049487802));
#174522=CARTESIAN_POINT('Ctrl Pts',(64.5864261182488,-7.84789369480699,
56.0667617574747));
#174523=CARTESIAN_POINT('Ctrl Pts',(61.3653750217006,-8.21460954814057E-14,
56.5522165598209));
#174524=CARTESIAN_POINT('Ctrl Pts',(64.5582082893779,7.847893694807,55.9067304976102));
#174525=CARTESIAN_POINT('Ctrl Pts',(72.2727659304039,11.1043081293031,54.4639424290512));
#174526=CARTESIAN_POINT('Ctrl Pts',(79.9873235714302,7.84789369480696,53.0211543604921));
#174527=CARTESIAN_POINT('Ctrl Pts',(83.1801568391073,2.04385119939587E-14,
52.3756682982815));
#174528=CARTESIAN_POINT('Ctrl Pts',(79.9591057425593,-7.84789369480692,
52.8611231006277));
#174529=CARTESIAN_POINT('Ctrl Pts',(72.2163302726622,-11.1043081293031,
54.1438799093222));
#174530=CARTESIAN_POINT('Ctrl Pts',(64.4735548027653,-7.84789369480703,
55.4266367180168));
#174531=CARTESIAN_POINT('Ctrl Pts',(61.2525037062171,3.95343480175114E-14,
55.912091520363));
#174532=CARTESIAN_POINT('Ctrl Pts',(64.4453369738944,7.84789369480696,55.2666054581523));
#174533=CARTESIAN_POINT('Ctrl Pts',(72.1598946149204,11.1043081293031,53.8238173895933));
#174534=CARTESIAN_POINT('Ctrl Pts',(79.8744522559467,7.84789369480696,52.3810293210342));
#174535=CARTESIAN_POINT('Ctrl Pts',(83.0672855236239,2.39912256727592E-14,
51.7355432588235));
#174536=CARTESIAN_POINT('Ctrl Pts',(79.9651954640518,-7.55805241504216,
52.2030690668877));
#174537=CARTESIAN_POINT('Ctrl Pts',(75.2470506983054,-9.76890830967669,
52.9830500593565));
#174538=CARTESIAN_POINT('Ctrl Pts',(72.9603109689917,-9.97929647052207,
53.3618098802771));
#174539=CARTESIAN_POINT('Ctrl Pts',(82.420455096836,-4.33680868994202E-16,
57.4690727095904));
#174540=CARTESIAN_POINT('Ctrl Pts',(82.4157521253576,-2.47968200709192,
57.4424008329463));
#174541=CARTESIAN_POINT('Ctrl Pts',(80.3851431585526,-7.41930423095383,
57.745449706252));
#174542=CARTESIAN_POINT('Ctrl Pts',(73.0644459155175,-10.4978792386127,
58.9537827355813));
#174543=CARTESIAN_POINT('Ctrl Pts',(65.7437486724824,-7.41930423095383,
60.1621157649105));
#174544=CARTESIAN_POINT('Ctrl Pts',(62.6978352222749,-2.21003770839445E-15,
60.6166890748691));
#174545=CARTESIAN_POINT('Ctrl Pts',(65.7155308436115,7.41930423095382,60.002084505046));
#174546=CARTESIAN_POINT('Ctrl Pts',(73.0080102577757,10.4978792386127,58.6337202158523));
#174547=CARTESIAN_POINT('Ctrl Pts',(80.30048967194,7.41930423095383,57.2653559266586));
#174548=CARTESIAN_POINT('Ctrl Pts',(83.3181852932766,1.78676518025611E-15,
56.6507513568355));
#174549=CARTESIAN_POINT('Ctrl Pts',(80.2722718430691,-7.41930423095382,
57.1053246667941));
#174550=CARTESIAN_POINT('Ctrl Pts',(72.951574600034,-10.4978792386127,58.3136576961233));
#174551=CARTESIAN_POINT('Ctrl Pts',(65.6308773569989,-7.41930423095384,
59.5219907254526));
#174552=CARTESIAN_POINT('Ctrl Pts',(62.5849639067914,-3.54230533794464E-15,
59.9765640354111));
#174553=CARTESIAN_POINT('Ctrl Pts',(65.6026595281281,7.41930423095383,59.3619594655881));
#174554=CARTESIAN_POINT('Ctrl Pts',(72.8951389422923,10.4978792386127,57.9935951763944));
#174555=CARTESIAN_POINT('Ctrl Pts',(80.1876183564565,7.41930423095384,56.6252308872007));
#174556=CARTESIAN_POINT('Ctrl Pts',(83.2053139777931,5.33947885905661E-15,
56.0106263173776));
#174557=CARTESIAN_POINT('Ctrl Pts',(80.1594005275856,-7.41930423095383,
56.4651996273362));
#174558=CARTESIAN_POINT('Ctrl Pts',(72.8387032845505,-10.4978792386127,
57.6735326566654));
#174559=CARTESIAN_POINT('Ctrl Pts',(65.5180060415154,-7.41930423095384,
58.8818656859946));
#174560=CARTESIAN_POINT('Ctrl Pts',(62.4720925913079,-7.5391082265952E-15,
59.3364389959532));
#174561=CARTESIAN_POINT('Ctrl Pts',(65.4897882126446,7.41930423095383,58.7218344261301));
#174562=CARTESIAN_POINT('Ctrl Pts',(72.7822676268087,10.4978792386127,57.3534701369364));
#174563=CARTESIAN_POINT('Ctrl Pts',(80.074747040973,7.41930423095384,55.9851058477427));
#174564=CARTESIAN_POINT('Ctrl Pts',(83.0924426623096,7.11583569845686E-15,
55.3705012779196));
#174565=CARTESIAN_POINT('Ctrl Pts',(80.0465292121021,-7.41930423095383,
55.8250745878782));
#174566=CARTESIAN_POINT('Ctrl Pts',(72.725831969067,-10.4978792386127,57.0334076172075));
#174567=CARTESIAN_POINT('Ctrl Pts',(65.405134726032,-7.41930423095385,58.2417406465367));
#174568=CARTESIAN_POINT('Ctrl Pts',(62.3592212758244,-9.31546506599545E-15,
58.6963139564953));
#174569=CARTESIAN_POINT('Ctrl Pts',(65.3769168971611,7.41930423095384,58.0817093866722));
#174570=CARTESIAN_POINT('Ctrl Pts',(72.6693963113252,10.4978792386127,56.7133450974785));
#174571=CARTESIAN_POINT('Ctrl Pts',(79.9618757254895,7.41930423095385,55.3449808082848));
#174572=CARTESIAN_POINT('Ctrl Pts',(82.9795713468261,9.33628174770718E-15,
54.7303762384617));
#174573=CARTESIAN_POINT('Ctrl Pts',(79.9336578966186,-7.41930423095383,
55.1849495484203));
#174574=CARTESIAN_POINT('Ctrl Pts',(72.6129606535835,-10.4978792386127,
56.3932825777495));
#174575=CARTESIAN_POINT('Ctrl Pts',(65.2922634105485,-7.41930423095385,
57.6016156070787));
#174576=CARTESIAN_POINT('Ctrl Pts',(62.246349960341,-1.24240895349459E-14,
58.0561889170373));
#174577=CARTESIAN_POINT('Ctrl Pts',(65.2640455816776,7.41930423095383,57.4415843472143));
#174578=CARTESIAN_POINT('Ctrl Pts',(72.5565249958418,10.4978792386127,56.0732200580206));
#174579=CARTESIAN_POINT('Ctrl Pts',(79.849004410006,7.41930423095385,54.7048557688268));
#174580=CARTESIAN_POINT('Ctrl Pts',(82.8667000313426,1.04083408558608E-17,
54.0902511990038));
#174581=CARTESIAN_POINT('Ctrl Pts',(79.8207865811352,-7.41930423095378,
54.5448245089623));
#174582=CARTESIAN_POINT('Ctrl Pts',(72.5000893381,-10.4978792386127,55.7531575382916));
#174583=CARTESIAN_POINT('Ctrl Pts',(65.179392095065,-7.41930423095383,56.9614905676208));
#174584=CARTESIAN_POINT('Ctrl Pts',(62.1334786448575,-7.81492925927552E-14,
57.4160638775794));
#174585=CARTESIAN_POINT('Ctrl Pts',(65.1511742661941,7.41930423095385,56.8014593077563));
#174586=CARTESIAN_POINT('Ctrl Pts',(72.4436536803583,10.4978792386127,55.4330950185626));
#174587=CARTESIAN_POINT('Ctrl Pts',(79.7361330945226,7.4193042309538,54.0647307293689));
#174588=CARTESIAN_POINT('Ctrl Pts',(82.7538287158591,1.5109441475758E-14,
53.4501261595458));
#174589=CARTESIAN_POINT('Ctrl Pts',(79.7079152656517,-7.41930423095378,
53.9046994695044));
#174590=CARTESIAN_POINT('Ctrl Pts',(72.3872180226165,-10.4978792386127,
55.1130324988336));
#174591=CARTESIAN_POINT('Ctrl Pts',(65.0665207795815,-7.41930423095387,
56.3213655281629));
#174592=CARTESIAN_POINT('Ctrl Pts',(62.020607329374,4.44193293258621E-14,
56.7759388381215));
#174593=CARTESIAN_POINT('Ctrl Pts',(65.0383029507106,7.41930423095381,56.1613342682984));
#174594=CARTESIAN_POINT('Ctrl Pts',(72.3307823648748,10.4978792386127,54.7929699791047));
#174595=CARTESIAN_POINT('Ctrl Pts',(79.6232617790391,7.4193042309538,53.424605689911));
#174596=CARTESIAN_POINT('Ctrl Pts',(82.6409574003756,1.77739767348584E-14,
52.8100011200879));
#174597=CARTESIAN_POINT('Ctrl Pts',(79.5950439501682,-7.41930423095377,
53.2645744300465));
#174598=CARTESIAN_POINT('Ctrl Pts',(72.2743467071331,-10.4978792386127,
54.4729074593757));
#174599=CARTESIAN_POINT('Ctrl Pts',(64.953649464098,-7.41930423095384,55.6812404887049));
#174600=CARTESIAN_POINT('Ctrl Pts',(61.9077360138905,-8.21460954814057E-14,
56.1358137986635));
#174601=CARTESIAN_POINT('Ctrl Pts',(64.9254316352271,7.41930423095385,55.5212092288404));
#174602=CARTESIAN_POINT('Ctrl Pts',(72.2179110493913,10.4978792386127,54.1528449396467));
#174603=CARTESIAN_POINT('Ctrl Pts',(79.5103904635556,7.41930423095381,52.784480650453));
#174604=CARTESIAN_POINT('Ctrl Pts',(82.5280860848922,2.04385119939587E-14,
52.1698760806299));
#174605=CARTESIAN_POINT('Ctrl Pts',(79.4821726346847,-7.41930423095377,
52.6244493905885));
#174606=CARTESIAN_POINT('Ctrl Pts',(72.1614753916496,-10.4978792386127,
53.8327824199178));
#174607=CARTESIAN_POINT('Ctrl Pts',(64.8407781486145,-7.41930423095387,
55.041115449247));
#174608=CARTESIAN_POINT('Ctrl Pts',(61.794864698407,3.95343480175114E-14,
55.4956887592056));
#174609=CARTESIAN_POINT('Ctrl Pts',(64.8125603197436,7.41930423095381,54.8810841893825));
#174610=CARTESIAN_POINT('Ctrl Pts',(72.1050397339078,10.4978792386127,53.5127199001888));
#174611=CARTESIAN_POINT('Ctrl Pts',(79.3975191480721,7.4193042309538,52.1443556109951));
#174612=CARTESIAN_POINT('Ctrl Pts',(82.4152147694087,2.39912256727592E-14,
51.529751041172));
#174613=CARTESIAN_POINT('Ctrl Pts',(79.481794108578,-7.14529177399519,51.9675358834182));
#174614=CARTESIAN_POINT('Ctrl Pts',(75.0208316204567,-9.23540832385942,
52.7021687013817));
#174615=CARTESIAN_POINT('Ctrl Pts',(72.858747024875,-9.43430675859939,53.0589484589415));
#174616=CARTESIAN_POINT('Origin',(71.9970151052421,-5.75,67.2970079954268));
#174617=CARTESIAN_POINT('',(69.479116529072,-5.75,53.0172955767497));
#174618=CARTESIAN_POINT('',(69.479116529072,-1.27999799280051E-15,53.0172955767497));
#174619=CARTESIAN_POINT('',(69.0102664493713,-5.75,50.3583146436167));
#174620=CARTESIAN_POINT('',(71.9970151052421,-5.75,67.2970079954268));
#174621=CARTESIAN_POINT('',(69.0102664493713,4.54725483176297E-16,50.3583146436167));
#174622=CARTESIAN_POINT('Origin',(76.9210538703031,-5.75,66.4287671070923));
#174623=CARTESIAN_POINT('',(74.403155294133,-5.75,52.1490546884152));
#174624=CARTESIAN_POINT('',(71.9411359116025,-5.75,52.5831751325825));
#174625=CARTESIAN_POINT('',(73.9343052144324,-5.75,49.4900737552822));
#174626=CARTESIAN_POINT('',(76.9210538703031,-5.75,66.4287671070923));
#174627=CARTESIAN_POINT('',(71.4722858319019,-5.75,49.9241941994495));
#174628=CARTESIAN_POINT('Origin',(76.9210538703031,-3.1224989991992,66.4287671070923));
#174629=CARTESIAN_POINT('',(74.403155294133,-3.1224989991992,52.1490546884152));
#174630=CARTESIAN_POINT('',(74.403155294133,3.70547026447916E-16,52.1490546884152));
#174631=CARTESIAN_POINT('',(73.9343052144324,-3.1224989991992,49.4900737552822));
#174632=CARTESIAN_POINT('',(76.9210538703031,-3.1224989991992,66.4287671070923));
#174633=CARTESIAN_POINT('',(73.9343052144324,2.10527050242472E-15,49.4900737552822));
#174634=CARTESIAN_POINT('Origin',(74.4590344877726,0.,66.8628875512595));
#174635=CARTESIAN_POINT('',(74.403155294133,3.1224989991992,52.1490546884152));
#174636=CARTESIAN_POINT('Origin',(71.9411359116025,0.,52.5831751325825));
#174637=CARTESIAN_POINT('',(73.9343052144324,3.1224989991992,49.4900737552822));
#174638=CARTESIAN_POINT('',(76.9210538703031,3.1224989991992,66.4287671070923));
#174639=CARTESIAN_POINT('Origin',(71.4722858319019,0.,49.9241941994495));
#174640=CARTESIAN_POINT('Origin',(76.9210538703031,5.75,66.4287671070923));
#174641=CARTESIAN_POINT('',(74.403155294133,5.75,52.1490546884152));
#174642=CARTESIAN_POINT('',(74.403155294133,3.70547026447918E-16,52.1490546884152));
#174643=CARTESIAN_POINT('',(73.9343052144324,5.75,49.4900737552822));
#174644=CARTESIAN_POINT('',(76.9210538703031,5.75,66.4287671070923));
#174645=CARTESIAN_POINT('',(73.9343052144324,2.10527050242472E-15,49.4900737552822));
#174646=CARTESIAN_POINT('Origin',(71.997015105242,5.75,67.2970079954268));
#174647=CARTESIAN_POINT('',(69.479116529072,5.75,53.0172955767497));
#174648=CARTESIAN_POINT('',(71.9411359116025,5.75,52.5831751325825));
#174649=CARTESIAN_POINT('',(69.0102664493713,5.75,50.3583146436167));
#174650=CARTESIAN_POINT('',(71.997015105242,5.75,67.2970079954268));
#174651=CARTESIAN_POINT('',(71.4722858319019,5.75,49.9241941994495));
#174652=CARTESIAN_POINT('Origin',(71.997015105242,3.1224989991992,67.2970079954268));
#174653=CARTESIAN_POINT('',(69.479116529072,-1.27999799280051E-15,53.0172955767497));
#174654=CARTESIAN_POINT('',(69.0102664493713,4.54725483176297E-16,50.3583146436167));
#174655=CARTESIAN_POINT('Origin',(71.9411359116025,-8.67361737988404E-16,
52.5831751325825));
#174656=CARTESIAN_POINT('Origin',(72.7225527111036,-4.33680868994202E-16,
57.0148100211374));
#174657=CARTESIAN_POINT('Origin',(71.4722858319019,8.67361737988404E-16,
49.9241941994495));
#174658=CARTESIAN_POINT('',(68.0608117040921,6.,50.5257291321711));
#174659=CARTESIAN_POINT('',(64.6493375762823,1.47451495458029E-14,51.1272640648928));
#174660=CARTESIAN_POINT('',(68.0608117040921,6.,50.5257291321711));
#174661=CARTESIAN_POINT('',(74.8837599597117,6.,49.3226592667278));
#174662=CARTESIAN_POINT('',(74.8837599597117,6.,49.3226592667278));
#174663=CARTESIAN_POINT('',(78.2952340875215,0.,48.7211243340062));
#174664=CARTESIAN_POINT('',(78.2952340875215,0.,48.7211243340062));
#174665=CARTESIAN_POINT('',(74.8837599597116,-6.,49.3226592667279));
#174666=CARTESIAN_POINT('',(74.8837599597116,-6.,49.3226592667279));
#174667=CARTESIAN_POINT('',(68.0608117040921,-6.,50.5257291321711));
#174668=CARTESIAN_POINT('',(68.0608117040921,-6.,50.5257291321711));
#174669=CARTESIAN_POINT('',(64.6493375762823,1.59872115546023E-14,51.1272640648928));
#174670=CARTESIAN_POINT('Origin',(74.8837599597116,-6.,49.3226592667279));
#174671=CARTESIAN_POINT('',(78.2952340875215,0.,48.7211243340062));
#174672=CARTESIAN_POINT('',(74.8837599597116,-6.,49.3226592667279));
#174673=CARTESIAN_POINT('Origin',(68.0608117040921,-6.,50.5257291321711));
#174674=CARTESIAN_POINT('',(68.0608117040921,-6.,50.5257291321711));
#174675=CARTESIAN_POINT('Origin',(64.6493375762823,1.59872115546023E-14,
51.1272640648928));
#174676=CARTESIAN_POINT('',(64.6493375762823,1.47451495458029E-14,51.1272640648928));
#174677=CARTESIAN_POINT('Origin',(68.0608117040921,6.,50.5257291321711));
#174678=CARTESIAN_POINT('',(68.0608117040921,6.,50.5257291321711));
#174679=CARTESIAN_POINT('Origin',(74.8837599597117,6.,49.3226592667278));
#174680=CARTESIAN_POINT('',(74.8837599597117,6.,49.3226592667278));
#174681=CARTESIAN_POINT('Origin',(78.2952340875215,0.,48.7211243340062));
#174682=CARTESIAN_POINT('Origin',(73.035119430904,-4.33680868994202E-16,
58.7874639765594));
#174683=CARTESIAN_POINT('Origin',(71.5591099207353,0.,50.4165980759556));
#174684=CARTESIAN_POINT('Origin',(71.9064062760691,0.,52.38621358198));
#174685=CARTESIAN_POINT('Origin',(69.7358040552328,0.,40.0761166693274));
#174686=CARTESIAN_POINT('',(0.,0.,0.));
#174687=CARTESIAN_POINT('Origin',(-20.5675364832709,-75.,72.98888938658));
#174688=CARTESIAN_POINT('',(-20.5675364832709,-75.,82.48888938658));
#174689=CARTESIAN_POINT('Origin',(-20.5675364832709,-75.,72.98888938658));
#174690=CARTESIAN_POINT('',(-20.5675364832709,-75.,82.98888938658));
#174691=CARTESIAN_POINT('Origin',(-20.5675364832709,-75.,82.73888938658));
#174692=CARTESIAN_POINT('Origin',(-20.5675364832709,-75.,72.98888938658));
#174693=CARTESIAN_POINT('Origin',(-20.5675364832709,-75.,72.98888938658));
#174694=CARTESIAN_POINT('',(-20.5675364832709,-75.,83.98888938658));
#174695=CARTESIAN_POINT('Origin',(-20.5675364832709,-75.,72.98888938658));
#174696=CARTESIAN_POINT('',(-20.5675364832709,-75.,84.48888938658));
#174697=CARTESIAN_POINT('Origin',(-20.5675364832709,-75.,84.23888938658));
#174698=CARTESIAN_POINT('Origin',(-20.5675364832709,-75.,72.98888938658));
#174699=CARTESIAN_POINT('Origin',(-25.5675364832709,-75.,72.98888938658));
#174700=CARTESIAN_POINT('',(-20.5675364832709,-75.,85.08888938658));
#174701=CARTESIAN_POINT('Origin',(-20.5675364832709,-75.,72.98888938658));
#174702=CARTESIAN_POINT('',(-22.5675364832709,-75.,85.08888938658));
#174703=CARTESIAN_POINT('',(-25.5675364832709,-75.,85.08888938658));
#174704=CARTESIAN_POINT('',(-22.5675364832709,-79.7069721126241,84.1358357635471));
#174705=CARTESIAN_POINT('Origin',(-22.5675364832709,-75.,72.98888938658));
#174706=CARTESIAN_POINT('',(-21.7675364832709,-79.7069721126241,84.1358357635471));
#174707=CARTESIAN_POINT('',(-22.1675364832709,-79.7069721126241,84.1358357635471));
#174708=CARTESIAN_POINT('',(-21.7675364832709,-82.3000526807644,82.6387199995009));
#174709=CARTESIAN_POINT('Origin',(-21.7675364832709,-75.,72.98888938658));
#174710=CARTESIAN_POINT('',(-22.5675364832709,-82.3000526807644,82.6387199995009));
#174711=CARTESIAN_POINT('',(-22.1675364832709,-82.3000526807644,82.6387199995009));
#174712=CARTESIAN_POINT('',(-22.5675364832709,-82.3000526807644,63.3390587736591));
#174713=CARTESIAN_POINT('Origin',(-22.5675364832709,-75.,72.98888938658));
#174714=CARTESIAN_POINT('',(-21.7675364832709,-82.3000526807644,63.3390587736591));
#174715=CARTESIAN_POINT('',(-22.1675364832709,-82.3000526807644,63.3390587736591));
#174716=CARTESIAN_POINT('',(-21.7675364832709,-79.7069721126241,61.8419430096129));
#174717=CARTESIAN_POINT('Origin',(-21.7675364832709,-75.,72.98888938658));
#174718=CARTESIAN_POINT('',(-22.5675364832709,-79.7069721126241,61.8419430096129));
#174719=CARTESIAN_POINT('',(-22.1675364832709,-79.7069721126241,61.8419430096129));
#174720=CARTESIAN_POINT('',(-22.5675364832709,-62.9929752066116,71.4917736225339));
#174721=CARTESIAN_POINT('Origin',(-22.5675364832709,-75.,72.98888938658));
#174722=CARTESIAN_POINT('',(-21.7675364832709,-62.9929752066116,71.4917736225339));
#174723=CARTESIAN_POINT('',(-22.1675364832709,-62.9929752066116,71.4917736225339));
#174724=CARTESIAN_POINT('',(-21.7675364832709,-62.9929752066116,74.4860051506262));
#174725=CARTESIAN_POINT('Origin',(-21.7675364832709,-75.,72.98888938658));
#174726=CARTESIAN_POINT('',(-22.5675364832709,-62.9929752066116,74.4860051506262));
#174727=CARTESIAN_POINT('',(-22.1675364832709,-62.9929752066116,74.4860051506262));
#174728=CARTESIAN_POINT('Origin',(-22.5675364832709,-75.,72.98888938658));
#174729=CARTESIAN_POINT('Origin',(-22.5675364832709,-75.,72.98888938658));
#174730=CARTESIAN_POINT('',(-22.5675364832709,-75.,84.48888938658));
#174731=CARTESIAN_POINT('Origin',(-22.5675364832709,-75.,72.98888938658));
#174732=CARTESIAN_POINT('',(-22.5675364832709,-75.,83.98888938658));
#174733=CARTESIAN_POINT('Origin',(-22.5675364832709,-75.,84.23888938658));
#174734=CARTESIAN_POINT('Origin',(-22.5675364832709,-75.,72.98888938658));
#174735=CARTESIAN_POINT('Origin',(-22.5675364832709,-75.,72.98888938658));
#174736=CARTESIAN_POINT('',(-22.5675364832709,-75.,82.98888938658));
#174737=CARTESIAN_POINT('Origin',(-22.5675364832709,-75.,72.98888938658));
#174738=CARTESIAN_POINT('',(-22.5675364832709,-75.,82.48888938658));
#174739=CARTESIAN_POINT('Origin',(-22.5675364832709,-75.,82.73888938658));
#174740=CARTESIAN_POINT('Origin',(-22.5675364832709,-75.,72.98888938658));
#174741=CARTESIAN_POINT('Origin',(-25.5675364832709,-75.,72.98888938658));
#174742=CARTESIAN_POINT('',(-22.5675364832709,-75.,80.48888938658));
#174743=CARTESIAN_POINT('Origin',(-22.5675364832709,-75.,72.98888938658));
#174744=CARTESIAN_POINT('',(-20.5675364832709,-75.,80.48888938658));
#174745=CARTESIAN_POINT('',(-25.5675364832709,-75.,80.48888938658));
#174746=CARTESIAN_POINT('Origin',(-20.5675364832709,-75.,72.98888938658));
#174747=CARTESIAN_POINT('Origin',(-21.7675364832709,-62.9,72.98888938658));
#174748=CARTESIAN_POINT('Origin',(-21.7675364832709,-62.9,72.98888938658));
#174749=CARTESIAN_POINT('Origin',(-22.5675364832709,-62.9,72.98888938658));
#174750=CARTESIAN_POINT('Origin',(-21.7675364832709,-81.05,83.4677967723717));
#174751=CARTESIAN_POINT('Origin',(-21.7675364832709,-81.05,83.4677967723717));
#174752=CARTESIAN_POINT('Origin',(-22.5675364832709,-81.05,83.4677967723717));
#174753=CARTESIAN_POINT('Origin',(-21.7675364832709,-81.05,83.4677967723717));
#174754=CARTESIAN_POINT('Origin',(-21.7675364832709,-81.05,62.5099820007883));
#174755=CARTESIAN_POINT('Origin',(-21.7675364832709,-81.05,62.5099820007883));
#174756=CARTESIAN_POINT('Origin',(-21.7675364832709,-81.05,62.5099820007883));
#174757=CARTESIAN_POINT('Origin',(-22.5675364832709,-81.05,62.5099820007883));
#174758=CARTESIAN_POINT('Origin',(-21.7675364832709,-62.9,72.98888938658));
#174759=CARTESIAN_POINT('Origin',(-20.5675364832709,-82.5,72.98888938658));
#174760=CARTESIAN_POINT('Origin',(-22.5675364832709,-84.5,72.98888938658));
#174761=CARTESIAN_POINT('Origin',(-22.5675364832709,-86.,72.98888938658));
#174762=CARTESIAN_POINT('Origin',(-22.5675364832709,-87.1,72.98888938658));
#174763=CARTESIAN_POINT('Origin',(-20.5675364832709,-86.5,72.98888938658));
#174764=CARTESIAN_POINT('Origin',(-20.5675364832709,-85.,72.98888938658));
#174765=CARTESIAN_POINT('',(0.,0.,0.));
#174766=CARTESIAN_POINT('Origin',(-23.90845228375,74.9968912574536,72.9873550812444));
#174767=CARTESIAN_POINT('',(-23.2177969711981,74.9968912574536,59.9387052680259));
#174768=CARTESIAN_POINT('',(-23.5174110875174,74.9968912574536,59.9387052680259));
#174769=CARTESIAN_POINT('',(-23.90845228375,74.9968912574536,59.9387052680259));
#174770=CARTESIAN_POINT('',(-24.4189072313413,74.9968582940746,86.0360048944213));
#174771=CARTESIAN_POINT('Ctrl Pts',(-23.5174110875174,74.9968912574536,
59.9387052680259));
#174772=CARTESIAN_POINT('Ctrl Pts',(-23.5306316897371,74.3947093830811,
59.9387052680259));
#174773=CARTESIAN_POINT('Ctrl Pts',(-23.5438009327752,73.793028183032,59.9803906448424));
#174774=CARTESIAN_POINT('Ctrl Pts',(-23.5751921994059,72.3608197445332,
60.1799448633758));
#174775=CARTESIAN_POINT('Ctrl Pts',(-23.5935749184201,71.5387148881984,
60.3770562255265));
#174776=CARTESIAN_POINT('Ctrl Pts',(-23.6306843757188,69.9428310814621,
60.9276138359542));
#174777=CARTESIAN_POINT('Ctrl Pts',(-23.6489357223363,69.1728925676118,
61.2800101514938));
#174778=CARTESIAN_POINT('Ctrl Pts',(-23.6862170214012,67.6961427337877,
62.1378741299171));
#174779=CARTESIAN_POINT('Ctrl Pts',(-23.7053154597809,66.9947011771143,
62.6443806601604));
#174780=CARTESIAN_POINT('Ctrl Pts',(-23.7372605442535,65.8985267731378,
63.6146285486161));
#174781=CARTESIAN_POINT('Ctrl Pts',(-23.7502862986929,65.4766725502222,
64.0434367410376));
#174782=CARTESIAN_POINT('Ctrl Pts',(-23.7777995451244,64.6603512478079,
64.9966630206717));
#174783=CARTESIAN_POINT('Ctrl Pts',(-23.7922833732239,64.2728028609773,
65.5248392427358));
#174784=CARTESIAN_POINT('Ctrl Pts',(-23.8229194172938,63.5337098738831,
66.7093534474452));
#174785=CARTESIAN_POINT('Ctrl Pts',(-23.8389795075283,63.1953279007174,
67.3712230547026));
#174786=CARTESIAN_POINT('Ctrl Pts',(-23.8698174699092,62.6654826054796,
68.6699413541111));
#174787=CARTESIAN_POINT('Ctrl Pts',(-23.8844820424246,62.4627426292908,
69.2996974587134));
#174788=CARTESIAN_POINT('Ctrl Pts',(-23.9176950045324,62.109553889035,70.7712848286564));
#174789=CARTESIAN_POINT('Ctrl Pts',(-23.9362135892086,61.9923040633228,
71.6179945676372));
#174790=CARTESIAN_POINT('Ctrl Pts',(-23.964236598216,61.942036872041,72.8849992863093));
#174791=CARTESIAN_POINT('Ctrl Pts',(-23.973449779398,61.9453912131552,73.3004782105993));
#174792=CARTESIAN_POINT('Ctrl Pts',(-24.0009465645323,62.0148930288987,
74.5447443855187));
#174793=CARTESIAN_POINT('Ctrl Pts',(-24.0189709350315,62.1403795210907,
75.3680792306046));
#174794=CARTESIAN_POINT('Ctrl Pts',(-24.0563699443479,62.5538671926331,
77.0100297541816));
#174795=CARTESIAN_POINT('Ctrl Pts',(-24.0754984434071,62.8467982285305,
77.8232629944303));
#174796=CARTESIAN_POINT('Ctrl Pts',(-24.1128050945005,63.5787378125085,
79.3589157490377));
#174797=CARTESIAN_POINT('Ctrl Pts',(-24.131294169336,64.0118682653229,80.0796236908367));
#174798=CARTESIAN_POINT('Ctrl Pts',(-24.1688946314926,65.0198641919139,
81.4405602344044));
#174799=CARTESIAN_POINT('Ctrl Pts',(-24.1875288663165,65.5948118402807,
82.0757351216293));
#174800=CARTESIAN_POINT('Ctrl Pts',(-24.2218130943148,66.745942130525,83.1204114609486));
#174801=CARTESIAN_POINT('Ctrl Pts',(-24.23740864815,67.3011544652776,83.5482557034675));
#174802=CARTESIAN_POINT('Ctrl Pts',(-24.2700005819463,68.5362341373696,
84.3506630736698));
#174803=CARTESIAN_POINT('Ctrl Pts',(-24.2868300007145,69.2206272059027,
84.7133789293529));
#174804=CARTESIAN_POINT('Ctrl Pts',(-24.3227853064787,70.7187769706881,
85.3442055799435));
#174805=CARTESIAN_POINT('Ctrl Pts',(-24.3417755229759,71.5350002648146,
85.5972454112807));
#174806=CARTESIAN_POINT('Ctrl Pts',(-24.3701818801963,72.8017543034024,
85.8575872429789));
#174807=CARTESIAN_POINT('Ctrl Pts',(-24.3798493266896,73.237675649591,85.9243818645359));
#174808=CARTESIAN_POINT('Ctrl Pts',(-24.3993200275243,74.1149668455025,
86.0136375501037));
#174809=CARTESIAN_POINT('Ctrl Pts',(-24.4091108195205,74.5557662227505,
86.0360037801385));
#174810=CARTESIAN_POINT('Ctrl Pts',(-24.4189072313413,74.9968582940747,
86.0360048944213));
#174811=CARTESIAN_POINT('',(-25.2173493892328,79.4629869826027,60.7268819234023));
#174812=CARTESIAN_POINT('Ctrl Pts',(-25.2179534601443,79.4630374617318,
60.7268167557867));
#174813=CARTESIAN_POINT('Ctrl Pts',(-25.1949255782283,80.4489154598281,
61.0859425267927));
#174814=CARTESIAN_POINT('Ctrl Pts',(-25.1723485468283,81.3878867153683,
61.562672966569));
#174815=CARTESIAN_POINT('Ctrl Pts',(-25.1418319224898,82.5496720747983,
62.3410093153827));
#174816=CARTESIAN_POINT('Ctrl Pts',(-25.1341597941251,82.8318350663601,
62.5469129762632));
#174817=CARTESIAN_POINT('Ctrl Pts',(-25.1058958914059,83.8409298929905,
63.3472530552093));
#174818=CARTESIAN_POINT('Ctrl Pts',(-25.0856284897418,84.511359906732,64.0082978439567));
#174819=CARTESIAN_POINT('Ctrl Pts',(-25.0463381621833,85.6523246677436,
65.4059328422703));
#174820=CARTESIAN_POINT('Ctrl Pts',(-25.027232400678,86.1315603731781,66.1291213643972));
#174821=CARTESIAN_POINT('Ctrl Pts',(-24.9900396375443,86.9286890065907,
67.6387170859581));
#174822=CARTESIAN_POINT('Ctrl Pts',(-24.9718326777449,87.2487759197293,
68.4193091338106));
#174823=CARTESIAN_POINT('Ctrl Pts',(-24.9272869194746,87.8326974023058,
70.3586157341816));
#174824=CARTESIAN_POINT('Ctrl Pts',(-24.9018234838558,88.0181608402933,
71.5331436490753));
#174825=CARTESIAN_POINT('Ctrl Pts',(-24.8571030316205,88.0603938351231,
73.5672948670293));
#174826=CARTESIAN_POINT('Ctrl Pts',(-24.8383743123942,87.9947871936716,
74.4177895566877));
#174827=CARTESIAN_POINT('Ctrl Pts',(-24.8106986129751,87.7741381142733,
75.6676798065923));
#174828=CARTESIAN_POINT('Ctrl Pts',(-24.8016093736651,87.6816712847804,
76.0758065751895));
#174829=CARTESIAN_POINT('Ctrl Pts',(-24.7773198416252,87.385647964188,77.1418062935282));
#174830=CARTESIAN_POINT('Ctrl Pts',(-24.7620753388422,87.1493723837374,
77.7892260852975));
#174831=CARTESIAN_POINT('Ctrl Pts',(-24.7308380021253,86.5571700848344,
79.0839389629231));
#174832=CARTESIAN_POINT('Ctrl Pts',(-24.7149083735725,86.195172121125,79.7258182827827));
#174833=CARTESIAN_POINT('Ctrl Pts',(-24.6873016319441,85.4903137590593,
80.7605121739211));
#174834=CARTESIAN_POINT('Ctrl Pts',(-24.6758558722288,85.1745290711364,
81.1696271952864));
#174835=CARTESIAN_POINT('Ctrl Pts',(-24.6475001697504,84.3290860728388,
82.1400231901871));
#174836=CARTESIAN_POINT('Ctrl Pts',(-24.6307810261104,83.772354714319,82.6751014390908));
#174837=CARTESIAN_POINT('Ctrl Pts',(-24.599585770867,82.6689003170912,83.5620240742505));
#174838=CARTESIAN_POINT('Ctrl Pts',(-24.5852411678047,82.1368548866381,
83.9282997510593));
#174839=CARTESIAN_POINT('Ctrl Pts',(-24.5583913263161,81.085177231511,84.5428023818064));
#174840=CARTESIAN_POINT('Ctrl Pts',(-24.5458806664955,80.5719400938607,
84.7989772586651));
#174841=CARTESIAN_POINT('Ctrl Pts',(-24.5143902223458,79.249545675383,85.3535788429129));
#174842=CARTESIAN_POINT('Ctrl Pts',(-24.4951894160072,78.4245499633485,
85.6071693181083));
#174843=CARTESIAN_POINT('Ctrl Pts',(-24.4570936740858,76.7300922849556,
85.9494606259938));
#174844=CARTESIAN_POINT('Ctrl Pts',(-24.4381782821791,75.8645543327958,
86.036007086387));
#174845=CARTESIAN_POINT('Ctrl Pts',(-24.4189072313414,74.9968582940746,
86.0360048944213));
#174846=CARTESIAN_POINT('',(-24.9173192207092,79.4630659019012,60.7267130748814));
#174847=CARTESIAN_POINT('',(-24.9176605481234,79.4630324820554,60.7268149418411));
#174848=CARTESIAN_POINT('Ctrl Pts',(-24.9171176851385,79.4630266224176,
60.7268128073552));
#174849=CARTESIAN_POINT('Ctrl Pts',(-24.907479882823,79.8753728640667,60.8770177568019));
#174850=CARTESIAN_POINT('Ctrl Pts',(-24.8978319043974,80.2798785853172,
61.0479289126257));
#174851=CARTESIAN_POINT('Ctrl Pts',(-24.8785453377169,81.0645998434556,
61.4271900252295));
#174852=CARTESIAN_POINT('Ctrl Pts',(-24.8689206935574,81.4445900685363,
61.6347482191992));
#174853=CARTESIAN_POINT('Ctrl Pts',(-24.840349563971,82.5416901570323,62.3068854017982));
#174854=CARTESIAN_POINT('Ctrl Pts',(-24.821762902311,83.2242721675299,62.8233682841019));
#174855=CARTESIAN_POINT('Ctrl Pts',(-24.7882924710906,84.3372637008269,
63.8515965314164));
#174856=CARTESIAN_POINT('Ctrl Pts',(-24.7735463269596,84.7882160198035,
64.3366558744028));
#174857=CARTESIAN_POINT('Ctrl Pts',(-24.7428192805704,85.6549656223796,
65.4239947985609));
#174858=CARTESIAN_POINT('Ctrl Pts',(-24.7269426546624,86.0608893983088,
66.0312845368707));
#174859=CARTESIAN_POINT('Ctrl Pts',(-24.6987033488005,86.6799171820225,
67.1498996693163));
#174860=CARTESIAN_POINT('Ctrl Pts',(-24.6864856504174,86.9152660426622,
67.646819458865));
#174861=CARTESIAN_POINT('Ctrl Pts',(-24.6551612930385,87.4390675705398,
68.96131540558));
#174862=CARTESIAN_POINT('Ctrl Pts',(-24.6363747440106,87.6787068724131,
69.7954432923412));
#174863=CARTESIAN_POINT('Ctrl Pts',(-24.6080786233649,87.9084778632656,
71.0558328275135));
#174864=CARTESIAN_POINT('Ctrl Pts',(-24.598861742352,87.9634238082213,71.4678552598435));
#174865=CARTESIAN_POINT('Ctrl Pts',(-24.5727907796244,88.063181685535,72.6410378365364));
#174866=CARTESIAN_POINT('Ctrl Pts',(-24.5562271243097,88.0611130529392,
73.4044777942705));
#174867=CARTESIAN_POINT('Ctrl Pts',(-24.5235275316636,87.9269505313888,
74.8870509312707));
#174868=CARTESIAN_POINT('Ctrl Pts',(-24.507401032424,87.8011257772416,75.6040034445301));
#174869=CARTESIAN_POINT('Ctrl Pts',(-24.4751432975777,87.4285472490523,
77.0204440402907));
#174870=CARTESIAN_POINT('Ctrl Pts',(-24.4591568287965,87.1806075424267,
77.7169362046151));
#174871=CARTESIAN_POINT('Ctrl Pts',(-24.4306825968416,86.6442142364001,
78.8965270434755));
#174872=CARTESIAN_POINT('Ctrl Pts',(-24.4183384755492,86.3809768706051,
79.3889984866159));
#174873=CARTESIAN_POINT('Ctrl Pts',(-24.3898062791471,85.6984170606593,
80.489923224599));
#174874=CARTESIAN_POINT('Ctrl Pts',(-24.3738573236368,85.2573577437238,
81.0826630754251));
#174875=CARTESIAN_POINT('Ctrl Pts',(-24.3484360912179,84.4881558658776,
81.9518531013098));
#174876=CARTESIAN_POINT('Ctrl Pts',(-24.3391233173508,84.1924687290483,
82.2549158317457));
#174877=CARTESIAN_POINT('Ctrl Pts',(-24.3107674447563,83.2503363923736,
83.1309876363149));
#174878=CARTESIAN_POINT('Ctrl Pts',(-24.2920534731176,82.561299893995,83.6547055024374));
#174879=CARTESIAN_POINT('Ctrl Pts',(-24.2569824435957,81.1923267956187,
84.4954455722956));
#174880=CARTESIAN_POINT('Ctrl Pts',(-24.2405874762494,80.5269788055029,
84.8295547203288));
#174881=CARTESIAN_POINT('Ctrl Pts',(-24.2054384202444,79.0371977989294,
85.4245808899677));
#174882=CARTESIAN_POINT('Ctrl Pts',(-24.1869132397422,78.2079210009582,
85.6640247659888));
#174883=CARTESIAN_POINT('Ctrl Pts',(-24.159348477152,76.9706829437812,85.8919677005822));
#174884=CARTESIAN_POINT('Ctrl Pts',(-24.1506142201114,76.57716252112,85.9460441609189));
#174885=CARTESIAN_POINT('Ctrl Pts',(-24.122990590964,75.323465862265,86.0603600583802));
#174886=CARTESIAN_POINT('Ctrl Pts',(-24.1044674113239,74.4594960530369,
86.0533918699913));
#174887=CARTESIAN_POINT('Ctrl Pts',(-24.0764752968672,73.1853327358667,
85.9164537916965));
#174888=CARTESIAN_POINT('Ctrl Pts',(-24.0672638926978,72.7705275994402,
85.8515162077124));
#174889=CARTESIAN_POINT('Ctrl Pts',(-24.0391353816953,71.5153348118852,
85.5924780012352));
#174890=CARTESIAN_POINT('Ctrl Pts',(-24.0205803158517,70.6904341543003,
85.3350183743386));
#174891=CARTESIAN_POINT('Ctrl Pts',(-23.9853250595168,69.2015481645728,
84.7028176556543));
#174892=CARTESIAN_POINT('Ctrl Pts',(-23.9686655586623,68.5330870501817,
84.3476938805495));
#174893=CARTESIAN_POINT('Ctrl Pts',(-23.9431413809485,67.549959050079,83.7103959685794));
#174894=CARTESIAN_POINT('Ctrl Pts',(-23.9341463648957,67.2118231353462,
83.4674848765376));
#174895=CARTESIAN_POINT('Ctrl Pts',(-23.9084332537329,66.2843549821508,
82.7315139018156));
#174896=CARTESIAN_POINT('Ctrl Pts',(-23.8915970203927,65.7261456823091,
82.2020274357745));
#174897=CARTESIAN_POINT('Ctrl Pts',(-23.8558673745728,64.6471229765557,
80.9806261645898));
#174898=CARTESIAN_POINT('Ctrl Pts',(-23.8373498958916,64.1418959989384,
80.2797596515301));
#174899=CARTESIAN_POINT('Ctrl Pts',(-23.7998503057796,63.2811086834496,
78.7956795514478));
#174900=CARTESIAN_POINT('Ctrl Pts',(-23.7810378773673,62.9262616653751,
78.0168781016788));
#174901=CARTESIAN_POINT('Ctrl Pts',(-23.7441929747498,62.3776760125511,
76.412461113905));
#174902=CARTESIAN_POINT('Ctrl Pts',(-23.7258692836287,62.1830391019126,
75.5914155731213));
#174903=CARTESIAN_POINT('Ctrl Pts',(-23.6883757749156,61.9518865214893,
73.9030935608427));
#174904=CARTESIAN_POINT('Ctrl Pts',(-23.6696975256392,61.9198874434843,
73.0393246060036));
#174905=CARTESIAN_POINT('Ctrl Pts',(-23.6339180304091,62.0214110492959,
71.4041912157041));
#174906=CARTESIAN_POINT('Ctrl Pts',(-23.6167598849786,62.1385016709135,
70.6354831377901));
#174907=CARTESIAN_POINT('Ctrl Pts',(-23.5853517843891,62.4792638045982,
69.2448625450023));
#174908=CARTESIAN_POINT('Ctrl Pts',(-23.5711600566694,62.6831158930766,
68.6206416349461));
#174909=CARTESIAN_POINT('Ctrl Pts',(-23.5404775668991,63.2166128083746,
67.3264351919183));
#174910=CARTESIAN_POINT('Ctrl Pts',(-23.5239715408375,63.5585307626862,
66.6639952735067));
#174911=CARTESIAN_POINT('Ctrl Pts',(-23.4985238885039,64.17653413673,65.6825672886288));
#174912=CARTESIAN_POINT('Ctrl Pts',(-23.4894745094915,64.4147139712013,
65.3415995372487));
#174913=CARTESIAN_POINT('Ctrl Pts',(-23.4589239558264,65.2683875666543,
64.2360065988036));
#174914=CARTESIAN_POINT('Ctrl Pts',(-23.43713499007,65.9536909696,63.5295327002692));
#174915=CARTESIAN_POINT('Ctrl Pts',(-23.4003935425218,67.246631807523,62.4668871104082));
#174916=CARTESIAN_POINT('Ctrl Pts',(-23.3853234262154,67.815748405656,62.070489364388));
#174917=CARTESIAN_POINT('Ctrl Pts',(-23.3513960249935,69.1434681142476,
61.2946542503527));
#174918=CARTESIAN_POINT('Ctrl Pts',(-23.3326256794217,69.9130319325745,
60.9401066017162));
#174919=CARTESIAN_POINT('Ctrl Pts',(-23.2955716873773,71.5096272106183,
60.3849607232919));
#174920=CARTESIAN_POINT('Ctrl Pts',(-23.2769908251956,72.3328673269368,
60.1856238439957));
#174921=CARTESIAN_POINT('Ctrl Pts',(-23.2446586345435,73.7752227019225,
59.9816281184901));
#174922=CARTESIAN_POINT('Ctrl Pts',(-23.2312093739932,74.3858353153039,
59.9387052680259));
#174923=CARTESIAN_POINT('Ctrl Pts',(-23.2177969711981,74.9968912574536,
59.9387052680259));
#174924=CARTESIAN_POINT('Origin',(-23.90845228375,74.9968912574536,72.9873550812444));
#174925=CARTESIAN_POINT('',(-21.4178560137093,74.9968912615648,59.9387052680259));
#174926=CARTESIAN_POINT('',(-21.7173525905574,74.9968912574536,59.9387052680259));
#174927=CARTESIAN_POINT('',(-23.90845228375,74.9968912574536,59.9387052680259));
#174928=CARTESIAN_POINT('Ctrl Pts',(-21.7173525905574,74.9968912574536,
59.9387052680259));
#174929=CARTESIAN_POINT('Ctrl Pts',(-21.7302063156957,74.4099001677546,
59.9387052680259));
#174930=CARTESIAN_POINT('Ctrl Pts',(-21.7431527425349,73.8232749118547,
59.9783138155532));
#174931=CARTESIAN_POINT('Ctrl Pts',(-21.7708092415273,72.5655155837762,
60.1491152972995));
#174932=CARTESIAN_POINT('Ctrl Pts',(-21.7855248966112,71.8982337599918,
60.2936435535157));
#174933=CARTESIAN_POINT('Ctrl Pts',(-21.8191003663665,70.4283593294628,
60.7348728947392));
#174934=CARTESIAN_POINT('Ctrl Pts',(-21.8378973148665,69.6374204991757,
61.0596192085729));
#174935=CARTESIAN_POINT('Ctrl Pts',(-21.8747288597517,68.1409049880788,
61.8531785853791));
#174936=CARTESIAN_POINT('Ctrl Pts',(-21.8930604919257,67.4377836432537,
62.3180383883955));
#174937=CARTESIAN_POINT('Ctrl Pts',(-21.9305692928866,66.1141772728772,
63.3900487508716));
#174938=CARTESIAN_POINT('Ctrl Pts',(-21.9492545327781,65.4995031373312,
63.997887959706));
#174939=CARTESIAN_POINT('Ctrl Pts',(-21.9848582071682,64.4606572539026,
65.2516214026179));
#174940=CARTESIAN_POINT('Ctrl Pts',(-22.0018106593114,64.0248831296256,
65.883213286058));
#174941=CARTESIAN_POINT('Ctrl Pts',(-22.0330147115562,63.3236714450916,
67.119415143412));
#174942=CARTESIAN_POINT('Ctrl Pts',(-22.0472138050556,63.0437252157077,
67.713020593513));
#174943=CARTESIAN_POINT('Ctrl Pts',(-22.0779145829976,62.5438034372538,
69.0198477713323));
#174944=CARTESIAN_POINT('Ctrl Pts',(-22.0944308896737,62.3379321954157,
69.7360073497001));
#174945=CARTESIAN_POINT('Ctrl Pts',(-22.129335439035,62.030797955824,71.2954150665285));
#174946=CARTESIAN_POINT('Ctrl Pts',(-22.1476938852872,61.9484251444568,
72.1389601782033));
#174947=CARTESIAN_POINT('Ctrl Pts',(-22.1755511193479,61.9481517353011,
73.3995577115146));
#174948=CARTESIAN_POINT('Ctrl Pts',(-22.1847606537286,61.9678629056999,
73.8143580866054));
#174949=CARTESIAN_POINT('Ctrl Pts',(-22.2166947481541,62.1053025258008,
75.2539209439819));
#174950=CARTESIAN_POINT('Ctrl Pts',(-22.239043878839,62.3246091103632,76.2651053904178));
#174951=CARTESIAN_POINT('Ctrl Pts',(-22.2711436235005,62.7965937029218,
77.6342938685587));
#174952=CARTESIAN_POINT('Ctrl Pts',(-22.2804156024698,62.9513880347713,
78.0219507666679));
#174953=CARTESIAN_POINT('Ctrl Pts',(-22.3067245585184,63.4466509246774,
79.1079827179994));
#174954=CARTESIAN_POINT('Ctrl Pts',(-22.3236323917217,63.831229993946,79.784277032089));
#174955=CARTESIAN_POINT('Ctrl Pts',(-22.3598918509028,64.7648882940439,
81.1308600635285));
#174956=CARTESIAN_POINT('Ctrl Pts',(-22.3790270103378,65.3251442237077,
81.7889387092825));
#174957=CARTESIAN_POINT('Ctrl Pts',(-22.4072423632755,66.2508914561918,
82.6803250777755));
#174958=CARTESIAN_POINT('Ctrl Pts',(-22.4165352981841,66.5696746640338,
82.958724063532));
#174959=CARTESIAN_POINT('Ctrl Pts',(-22.4449458637187,67.5774712698267,
83.7559451056425));
#174960=CARTESIAN_POINT('Ctrl Pts',(-22.4641503387602,68.3048636704198,
84.2224384205132));
#174961=CARTESIAN_POINT('Ctrl Pts',(-22.501285303839,69.810995887443,84.9898517968133));
#174962=CARTESIAN_POINT('Ctrl Pts',(-22.5195102657382,70.5832021864251,
85.2947829556675));
#174963=CARTESIAN_POINT('Ctrl Pts',(-22.5473234879989,71.7857662883215,
85.6418050277371));
#174964=CARTESIAN_POINT('Ctrl Pts',(-22.5567166580511,72.1979223482805,
85.739304069248));
#174965=CARTESIAN_POINT('Ctrl Pts',(-22.5755244853457,73.0384172083656,
85.8954110279683));
#174966=CARTESIAN_POINT('Ctrl Pts',(-22.5849742453824,73.4663957365637,
85.9531220346386));
#174967=CARTESIAN_POINT('Ctrl Pts',(-22.6134362956185,74.7541220080876,
86.0621095313202));
#174968=CARTESIAN_POINT('Ctrl Pts',(-22.6326452386617,75.6168779584812,
86.0496578720941));
#174969=CARTESIAN_POINT('Ctrl Pts',(-22.6709677204125,77.3455119283745,
85.8529668449526));
#174970=CARTESIAN_POINT('Ctrl Pts',(-22.6901390972948,78.2066494312835,
85.6655821751704));
#174971=CARTESIAN_POINT('Ctrl Pts',(-22.7188784283504,79.4392868969434,
85.2636194263096));
#174972=CARTESIAN_POINT('Ctrl Pts',(-22.7281584536231,79.8297491229408,
85.1152168230004));
#174973=CARTESIAN_POINT('Ctrl Pts',(-22.7529088994009,80.8584175963002,
84.6666711263083));
#174974=CARTESIAN_POINT('Ctrl Pts',(-22.7682334187029,81.4805314596249,
84.3331176818899));
#174975=CARTESIAN_POINT('Ctrl Pts',(-22.8027983993634,82.798230900913,83.4826918577857));
#174976=CARTESIAN_POINT('Ctrl Pts',(-22.8219893591569,83.4755286998752,
82.9435445720348));
#174977=CARTESIAN_POINT('Ctrl Pts',(-22.8500422418408,84.3943652677719,
82.0498945200944));
#174978=CARTESIAN_POINT('Ctrl Pts',(-22.8591742850748,84.6799558464963,
81.7440895610898));
#174979=CARTESIAN_POINT('Ctrl Pts',(-22.8848888190843,85.4369641606758,
80.8510945590963));
#174980=CARTESIAN_POINT('Ctrl Pts',(-22.9016020345431,85.8729940299941,
80.2360725574547));
#174981=CARTESIAN_POINT('Ctrl Pts',(-22.9328203510394,86.592180103431,79.0093760664373));
#174982=CARTESIAN_POINT('Ctrl Pts',(-22.9473374998402,86.8858300687438,
78.4066353215133));
#174983=CARTESIAN_POINT('Ctrl Pts',(-22.9810286478547,87.4499899421313,
76.9793754199744));
#174984=CARTESIAN_POINT('Ctrl Pts',(-23.0001903855084,87.687230217045,76.1450754570486));
#174985=CARTESIAN_POINT('Ctrl Pts',(-23.0281619377263,87.9139481390874,
74.8824264543852));
#174986=CARTESIAN_POINT('Ctrl Pts',(-23.0372443937547,87.9679773265212,
74.4680913785842));
#174987=CARTESIAN_POINT('Ctrl Pts',(-23.0630282534535,88.0641325863715,
73.2933767558786));
#174988=CARTESIAN_POINT('Ctrl Pts',(-23.0798660430062,88.0597426142557,
72.5308961097817));
#174989=CARTESIAN_POINT('Ctrl Pts',(-23.110718626206,87.9284862467173,71.1264365952234));
#174990=CARTESIAN_POINT('Ctrl Pts',(-23.1247527535594,87.8198404230815,
70.4851270400342));
#174991=CARTESIAN_POINT('Ctrl Pts',(-23.1548832091132,87.488965590155,69.147273968047));
#174992=CARTESIAN_POINT('Ctrl Pts',(-23.1709822825055,87.2551013670816,
68.4558621510493));
#174993=CARTESIAN_POINT('Ctrl Pts',(-23.2030228570246,86.6699535964167,
67.1090751142984));
#174994=CARTESIAN_POINT('Ctrl Pts',(-23.2189810029665,86.3179822987398,
66.4568526780595));
#174995=CARTESIAN_POINT('Ctrl Pts',(-23.2540992817533,85.4388073950574,
65.1145176809523));
#174996=CARTESIAN_POINT('Ctrl Pts',(-23.273094347954,84.8942159179656,64.4399488194559));
#174997=CARTESIAN_POINT('Ctrl Pts',(-23.3010605059325,83.9890549409349,
63.5222526741222));
#174998=CARTESIAN_POINT('Ctrl Pts',(-23.3102640153634,83.6766534830802,
63.2349759785988));
#174999=CARTESIAN_POINT('Ctrl Pts',(-23.3349547795299,82.8080045551004,
62.511045374306));
#175000=CARTESIAN_POINT('Ctrl Pts',(-23.3505379759931,82.2293415547844,
62.1035037303804));
#175001=CARTESIAN_POINT('Ctrl Pts',(-23.3857950726989,80.8338711771206,
61.2813490305736));
#175002=CARTESIAN_POINT('Ctrl Pts',(-23.4054853657382,80.0007276929279,
60.9017215669824));
#175003=CARTESIAN_POINT('Ctrl Pts',(-23.4346634324885,78.7391752955122,
60.4798934857545));
#175004=CARTESIAN_POINT('Ctrl Pts',(-23.4438349553282,78.3374278451823,
60.3666537439739));
#175005=CARTESIAN_POINT('Ctrl Pts',(-23.4704941584884,77.1454165599863,
60.0915798224803));
#175006=CARTESIAN_POINT('Ctrl Pts',(-23.4878574344418,76.3447741654688,
59.9834942206835));
#175007=CARTESIAN_POINT('Ctrl Pts',(-23.5094742272526,75.3585248802206,
59.9424627256623));
#175008=CARTESIAN_POINT('Ctrl Pts',(-23.5134418416706,75.1776854349154,
59.9387052680259));
#175009=CARTESIAN_POINT('Ctrl Pts',(-23.5174110875174,74.9968912574536,
59.9387052680259));
#175010=CARTESIAN_POINT('Ctrl Pts',(-23.2177969711981,74.9968912574536,
59.9387052680259));
#175011=CARTESIAN_POINT('Ctrl Pts',(-23.2122766055301,75.2483937134876,
59.9387052680259));
#175012=CARTESIAN_POINT('Ctrl Pts',(-23.206749248666,75.4999709804517,59.9459765228389));
#175013=CARTESIAN_POINT('Ctrl Pts',(-23.1868382383162,76.4020104636423,
59.9982159163286));
#175014=CARTESIAN_POINT('Ctrl Pts',(-23.1723428150149,77.0489752417336,
60.084601801932));
#175015=CARTESIAN_POINT('Ctrl Pts',(-23.1387122513219,78.5330764331777,
60.3972523725853));
#175016=CARTESIAN_POINT('Ctrl Pts',(-23.1199095752067,79.3595669630887,
60.6592427751684));
#175017=CARTESIAN_POINT('Ctrl Pts',(-23.0821115498925,80.928707858494,61.3343719010139));
#175018=CARTESIAN_POINT('Ctrl Pts',(-23.0633339395976,81.6692455056542,
61.7419933123616));
#175019=CARTESIAN_POINT('Ctrl Pts',(-23.026231243293,83.0632383898893,62.6957779977219));
#175020=CARTESIAN_POINT('Ctrl Pts',(-23.0076119265723,83.7131413994759,
63.2400738492398));
#175021=CARTESIAN_POINT('Ctrl Pts',(-22.9696043379337,84.9119525223814,
64.4605110212791));
#175022=CARTESIAN_POINT('Ctrl Pts',(-22.9507158743888,85.4552559591635,
65.1363601419598));
#175023=CARTESIAN_POINT('Ctrl Pts',(-22.9155042556653,86.3281026320126,
66.4751749515315));
#175024=CARTESIAN_POINT('Ctrl Pts',(-22.8991783125384,86.6760500700446,
67.1220261592005));
#175025=CARTESIAN_POINT('Ctrl Pts',(-22.8668564914752,87.2581364432114,
68.4639344324216));
#175026=CARTESIAN_POINT('Ctrl Pts',(-22.8509925336531,87.4918125648176,
69.1563744887733));
#175027=CARTESIAN_POINT('Ctrl Pts',(-22.8206340138724,87.8212172413,70.4928648072465));
#175028=CARTESIAN_POINT('Ctrl Pts',(-22.806238240693,87.9291085757939,71.1316691579198));
#175029=CARTESIAN_POINT('Ctrl Pts',(-22.7750988398522,88.0602372016251,
72.5378822152587));
#175030=CARTESIAN_POINT('Ctrl Pts',(-22.7584828653642,88.0641145347429,
73.3047098546431));
#175031=CARTESIAN_POINT('Ctrl Pts',(-22.7324138496429,87.9662301188309,
74.4832024422141));
#175032=CARTESIAN_POINT('Ctrl Pts',(-22.7231744470205,87.9117785726254,
74.8970656786553));
#175033=CARTESIAN_POINT('Ctrl Pts',(-22.6948123438722,87.6837443283447,
76.1590496732804));
#175034=CARTESIAN_POINT('Ctrl Pts',(-22.6760669416386,87.4455877607315,
76.9930815762467));
#175035=CARTESIAN_POINT('Ctrl Pts',(-22.6424278831996,86.8811365666569,
78.4164937016521));
#175036=CARTESIAN_POINT('Ctrl Pts',(-22.6276612363186,86.5885910904656,
79.0158974838695));
#175037=CARTESIAN_POINT('Ctrl Pts',(-22.5964391064742,85.8693918341243,
80.241760875551));
#175038=CARTESIAN_POINT('Ctrl Pts',(-22.580104399766,85.4313757342021,80.8587724139661));
#175039=CARTESIAN_POINT('Ctrl Pts',(-22.5543476911904,84.6719346593615,
81.7529372499967));
#175040=CARTESIAN_POINT('Ctrl Pts',(-22.5451298498866,84.3862669712625,
82.0582711510441));
#175041=CARTESIAN_POINT('Ctrl Pts',(-22.5168945854871,83.4668746349344,
82.9509064102007));
#175042=CARTESIAN_POINT('Ctrl Pts',(-22.4982518930569,82.7891212725679,
83.4894561594511));
#175043=CARTESIAN_POINT('Ctrl Pts',(-22.4640609704995,81.4753840607504,
84.3357126021793));
#175044=CARTESIAN_POINT('Ctrl Pts',(-22.4486091828021,80.8581356614063,
84.6664773458807));
#175045=CARTESIAN_POINT('Ctrl Pts',(-22.4164653455312,79.5109525283242,
85.254573077216));
#175046=CARTESIAN_POINT('Ctrl Pts',(-22.3998470581778,78.7785961749314,
85.4997529814177));
#175047=CARTESIAN_POINT('Ctrl Pts',(-22.371927537044,77.5385094339891,85.7960100070408));
#175048=CARTESIAN_POINT('Ctrl Pts',(-22.3608216463112,77.0417476535548,
85.8846425891359));
#175049=CARTESIAN_POINT('Ctrl Pts',(-22.3309115730071,75.686064074394,86.0462136198581));
#175050=CARTESIAN_POINT('Ctrl Pts',(-22.3124113574507,74.8230307679019,
86.06323056571));
#175051=CARTESIAN_POINT('Ctrl Pts',(-22.2844976295114,73.5511422499418,
85.9622972377186));
#175052=CARTESIAN_POINT('Ctrl Pts',(-22.2753810369904,73.1394503764237,
85.9097862283033));
#175053=CARTESIAN_POINT('Ctrl Pts',(-22.2479090344006,71.9058450340341,
85.6922628264543));
#175054=CARTESIAN_POINT('Ctrl Pts',(-22.2299005836022,71.0966584396281,
85.4676368267309));
#175055=CARTESIAN_POINT('Ctrl Pts',(-22.1963292659058,69.6602856382711,
84.9154445903109));
#175056=CARTESIAN_POINT('Ctrl Pts',(-22.1808755930549,69.0272956180662,
84.6115799670374));
#175057=CARTESIAN_POINT('Ctrl Pts',(-22.1498527206671,67.7979802517079,
83.8944401723291));
#175058=CARTESIAN_POINT('Ctrl Pts',(-22.1343011644881,67.2054601110404,
83.4793725230097));
#175059=CARTESIAN_POINT('Ctrl Pts',(-22.099644458544,65.9862354625609,82.4647897794127));
#175060=CARTESIAN_POINT('Ctrl Pts',(-22.0806461069253,65.3786610366711,
81.8475661646679));
#175061=CARTESIAN_POINT('Ctrl Pts',(-22.0436459429237,64.3087605378871,
80.5198641077891));
#175062=CARTESIAN_POINT('Ctrl Pts',(-22.0253349894935,63.8455304541845,
79.815383715023));
#175063=CARTESIAN_POINT('Ctrl Pts',(-21.9883357764173,63.0602967221302,
78.3254831707363));
#175064=CARTESIAN_POINT('Ctrl Pts',(-21.9701218644042,62.740445122404,77.543387573231));
#175065=CARTESIAN_POINT('Ctrl Pts',(-21.9329171687018,62.2502690489961,
75.9090249825322));
#175066=CARTESIAN_POINT('Ctrl Pts',(-21.9138313883391,62.0849382226692,
75.0595520014559));
#175067=CARTESIAN_POINT('Ctrl Pts',(-21.8831639335681,61.9542807843014,
73.659696518979));
#175068=CARTESIAN_POINT('Ctrl Pts',(-21.8714103011927,61.9376040534942,
73.1167750496578));
#175069=CARTESIAN_POINT('Ctrl Pts',(-21.8447841194471,61.9761462799511,
71.899530429945));
#175070=CARTESIAN_POINT('Ctrl Pts',(-21.829870331753,62.0498643471665,71.2273407251253));
#175071=CARTESIAN_POINT('Ctrl Pts',(-21.7960876134562,62.3355164686168,
69.716065712891));
#175072=CARTESIAN_POINT('Ctrl Pts',(-21.7774683443526,62.5794646088965,
68.8862256271957));
#175073=CARTESIAN_POINT('Ctrl Pts',(-21.7395220919643,63.2273532065084,
67.2874750558743));
#175074=CARTESIAN_POINT('Ctrl Pts',(-21.7205019632403,63.6295849146174,
66.5224489724313));
#175075=CARTESIAN_POINT('Ctrl Pts',(-21.6924089429919,64.3379396258668,
65.4485197264231));
#175076=CARTESIAN_POINT('Ctrl Pts',(-21.6831340767359,64.5886944224072,
65.1059385879003));
#175077=CARTESIAN_POINT('Ctrl Pts',(-21.659278120494,65.270927375683,64.2633473401903));
#175078=CARTESIAN_POINT('Ctrl Pts',(-21.6446174555065,65.7244658960641,
63.7827468956438));
#175079=CARTESIAN_POINT('Ctrl Pts',(-21.6118775989816,66.8263515960952,
62.7795688081261));
#175080=CARTESIAN_POINT('Ctrl Pts',(-21.5938354133167,67.4922483153368,
62.280490089044));
#175081=CARTESIAN_POINT('Ctrl Pts',(-21.5663060261506,68.5552678323796,
61.631962757131));
#175082=CARTESIAN_POINT('Ctrl Pts',(-21.5570934981404,68.9196079363756,
61.4328722197951));
#175083=CARTESIAN_POINT('Ctrl Pts',(-21.5238327972696,70.2730997642258,
60.7750240509474));
#175084=CARTESIAN_POINT('Ctrl Pts',(-21.5001959074978,71.309231096036,60.4232634933932));
#175085=CARTESIAN_POINT('Ctrl Pts',(-21.4667040833065,72.7881122727344,
60.1201607677847));
#175086=CARTESIAN_POINT('Ctrl Pts',(-21.4573831533975,73.2030744272741,
60.0557806310605));
#175087=CARTESIAN_POINT('Ctrl Pts',(-21.4380251932069,74.0776710893075,
59.9630036391895));
#175088=CARTESIAN_POINT('Ctrl Pts',(-21.4279728616493,74.5371369704319,
59.9387052677362));
#175089=CARTESIAN_POINT('Ctrl Pts',(-21.4178560137093,74.996891265676,59.9387052680259));
#175090=CARTESIAN_POINT('Origin',(-23.90845228375,74.9968912574536,72.9873550812444));
#175091=CARTESIAN_POINT('',(-19.6178714446467,74.9968993681034,59.9387052680284));
#175092=CARTESIAN_POINT('',(-19.9173382169355,74.9968858117148,59.938705268027));
#175093=CARTESIAN_POINT('',(-23.90845228375,74.9968912574536,59.9387052680259));
#175094=CARTESIAN_POINT('',(-19.4177763141321,83.3874087122245,62.9938945755098));
#175095=CARTESIAN_POINT('Ctrl Pts',(-19.6178714446467,74.9968993681034,
59.9387052680284));
#175096=CARTESIAN_POINT('Ctrl Pts',(-19.6014685026439,75.7392562382868,
59.9387057294552));
#175097=CARTESIAN_POINT('Ctrl Pts',(-19.5849037811272,76.4802620090225,
60.0020567382725));
#175098=CARTESIAN_POINT('Ctrl Pts',(-19.5521553242652,77.9468225819595,
60.2546657056363));
#175099=CARTESIAN_POINT('Ctrl Pts',(-19.5358475432088,78.6695897925503,
60.4440397486719));
#175100=CARTESIAN_POINT('Ctrl Pts',(-19.5024014277747,80.0908261196311,
60.949875575312));
#175101=CARTESIAN_POINT('Ctrl Pts',(-19.4854578253639,80.7856360811503,
61.2681603085282));
#175102=CARTESIAN_POINT('Ctrl Pts',(-19.4513770173665,82.1343953610875,
62.0353827008737));
#175103=CARTESIAN_POINT('Ctrl Pts',(-19.4340082401173,82.7833490499622,
62.4868441028634));
#175104=CARTESIAN_POINT('Ctrl Pts',(-19.4164777809729,83.3875372457796,
62.9941412915471));
#175105=CARTESIAN_POINT('',(-19.7174312187882,83.3870026620653,62.9934580993663));
#175106=CARTESIAN_POINT('Ctrl Pts',(-19.4175483972726,83.3873255397984,
62.9939635397476));
#175107=CARTESIAN_POINT('Ctrl Pts',(-19.5175444259387,83.3883618596074,
62.9948336320698));
#175108=CARTESIAN_POINT('Ctrl Pts',(-19.6175404546048,83.3883617890154,
62.9948335017092));
#175109=CARTESIAN_POINT('Ctrl Pts',(-19.7175364832709,83.3869807545433,
62.993674068783));
#175110=CARTESIAN_POINT('Ctrl Pts',(-19.9173382169355,74.9968858117148,
59.9387052680271));
#175111=CARTESIAN_POINT('Ctrl Pts',(-19.9007967949276,75.7554436370929,
59.9387049514496));
#175112=CARTESIAN_POINT('Ctrl Pts',(-19.8844783676533,76.5125565364492,
60.0048502818403));
#175113=CARTESIAN_POINT('Ctrl Pts',(-19.8511771565402,78.0094031487965,
60.2684072581934));
#175114=CARTESIAN_POINT('Ctrl Pts',(-19.8344745302453,78.7461983267385,
60.4657909926964));
#175115=CARTESIAN_POINT('Ctrl Pts',(-19.8097614398516,79.8151448713332,
60.8550310149607));
#175116=CARTESIAN_POINT('Ctrl Pts',(-19.8016215987501,80.1629869715839,
60.9990145028378));
#175117=CARTESIAN_POINT('Ctrl Pts',(-19.7685609555398,81.5415893673538,
61.640821849789));
#175118=CARTESIAN_POINT('Ctrl Pts',(-19.7433909837073,82.5110269727701,
62.258205377191));
#175119=CARTESIAN_POINT('Ctrl Pts',(-19.7185673678502,83.3874552850052,
62.9940724750352));
#175120=CARTESIAN_POINT('Origin',(-30.2175364832709,75.,72.98888938658));
#175121=CARTESIAN_POINT('',(-21.9012048916249,75.,85.23888938658));
#175122=CARTESIAN_POINT('',(-21.2338306962369,75.0000000451294,85.23888938658));
#175123=CARTESIAN_POINT('',(-30.2175364832709,75.,85.23888938658));
#175124=CARTESIAN_POINT('',(-20.333830095635,74.9999987451807,60.7388893865801));
#175125=CARTESIAN_POINT('Ctrl Pts',(-21.2338306951809,75.0000000451541,
85.23888938658));
#175126=CARTESIAN_POINT('Ctrl Pts',(-21.2308191510264,74.871361328295,85.2388893870541));
#175127=CARTESIAN_POINT('Ctrl Pts',(-21.2278115085571,74.7427004254411,
85.2368631119487));
#175128=CARTESIAN_POINT('Ctrl Pts',(-21.2058934519332,73.8042229972792,
85.20728181132));
#175129=CARTESIAN_POINT('Ctrl Pts',(-21.1871523997013,72.9989089654438,
85.1014707422029));
#175130=CARTESIAN_POINT('Ctrl Pts',(-21.1495260451104,71.4409117896302,
84.7370461654598));
#175131=CARTESIAN_POINT('Ctrl Pts',(-21.1311094437916,70.6910556826918,
84.4832054784111));
#175132=CARTESIAN_POINT('Ctrl Pts',(-21.0942053201137,69.2442539047876,
83.831808053776));
#175133=CARTESIAN_POINT('Ctrl Pts',(-21.075441657003,68.5512901173082,83.4345407518324));
#175134=CARTESIAN_POINT('Ctrl Pts',(-21.0377929593798,67.2413083429758,
82.5031960890114));
#175135=CARTESIAN_POINT('Ctrl Pts',(-21.0191271760664,66.629013431728,81.9691962546522));
#175136=CARTESIAN_POINT('Ctrl Pts',(-20.9858849275086,65.6589217849771,
80.9370958377329));
#175137=CARTESIAN_POINT('Ctrl Pts',(-20.971616746096,65.2772244909203,80.4653436863645));
#175138=CARTESIAN_POINT('Ctrl Pts',(-20.9385451921586,64.4703503834183,
79.3012370082582));
#175139=CARTESIAN_POINT('Ctrl Pts',(-20.9198101437826,64.0759242141126,
78.5910156278606));
#175140=CARTESIAN_POINT('Ctrl Pts',(-20.8822214137268,63.4419820235771,
77.1235982340241));
#175141=CARTESIAN_POINT('Ctrl Pts',(-20.8638337880297,63.1999769384464,
76.3716486083549));
#175142=CARTESIAN_POINT('Ctrl Pts',(-20.8269888930974,62.8620798677787,
74.8238825473228));
#175143=CARTESIAN_POINT('Ctrl Pts',(-20.8082536887632,62.7685033600815,
74.031380699892));
#175144=CARTESIAN_POINT('Ctrl Pts',(-20.7706138558305,62.7361723723302,
72.4252421628072));
#175145=CARTESIAN_POINT('Ctrl Pts',(-20.751950591255,62.8002954436033,71.6154360354312));
#175146=CARTESIAN_POINT('Ctrl Pts',(-20.7199080581257,63.0423491357255,
70.2712374331459));
#175147=CARTESIAN_POINT('Ctrl Pts',(-20.7068214756622,63.1778605296797,
69.7318865262472));
#175148=CARTESIAN_POINT('Ctrl Pts',(-20.6748772346359,63.6000066794672,
68.4325907237052));
#175149=CARTESIAN_POINT('Ctrl Pts',(-20.6561810950743,63.9264273894639,
67.6883523095461));
#175150=CARTESIAN_POINT('Ctrl Pts',(-20.627897104647,64.5165457174671,66.639564847221));
#175151=CARTESIAN_POINT('Ctrl Pts',(-20.618657075158,64.7254772554321,66.3067550654007));
#175152=CARTESIAN_POINT('Ctrl Pts',(-20.5904775305639,65.4134561475278,
65.3196280949693));
#175153=CARTESIAN_POINT('Ctrl Pts',(-20.5718102858009,65.9417256516032,
64.7023305719617));
#175154=CARTESIAN_POINT('Ctrl Pts',(-20.5379444375143,66.9837287179269,
63.7044026020081));
#175155=CARTESIAN_POINT('Ctrl Pts',(-20.5230629812357,67.4735626595182,
63.3030726194347));
#175156=CARTESIAN_POINT('Ctrl Pts',(-20.494111971847,68.4912688554889,62.5932566893908));
#175157=CARTESIAN_POINT('Ctrl Pts',(-20.4800537774037,69.015598449212,62.2828304602826));
#175158=CARTESIAN_POINT('Ctrl Pts',(-20.4549535739366,69.974637421168,61.8075866858196));
#175159=CARTESIAN_POINT('Ctrl Pts',(-20.4440701016085,70.3997239685461,
61.6260877697878));
#175160=CARTESIAN_POINT('Ctrl Pts',(-20.4166548860844,71.4996832993576,
61.2283065868462));
#175161=CARTESIAN_POINT('Ctrl Pts',(-20.4002998196522,72.1849361025285,
61.0457350114487));
#175162=CARTESIAN_POINT('Ctrl Pts',(-20.3671858554372,73.5813927560392,
60.8006112868465));
#175163=CARTESIAN_POINT('Ctrl Pts',(-20.3504179150539,74.2900185738204,
60.7388894593063));
#175164=CARTESIAN_POINT('Ctrl Pts',(-20.333830095635,74.9999987451808,60.7388893865801));
#175165=CARTESIAN_POINT('',(-20.1338946865143,82.8747201161109,63.6053345409726));
#175166=CARTESIAN_POINT('Ctrl Pts',(-20.333830095635,74.9999987451808,60.7388893865801));
#175167=CARTESIAN_POINT('Ctrl Pts',(-20.3171609122067,75.7134614016029,
60.7388893134971));
#175168=CARTESIAN_POINT('Ctrl Pts',(-20.3006993175161,76.4255596663345,
60.8012190536067));
#175169=CARTESIAN_POINT('Ctrl Pts',(-20.2672143173303,77.8301246910242,
61.0489997289239));
#175170=CARTESIAN_POINT('Ctrl Pts',(-20.250461415262,78.5199352933805,61.2338634607188));
#175171=CARTESIAN_POINT('Ctrl Pts',(-20.2255958036809,79.5230727248523,
61.5989754564678));
#175172=CARTESIAN_POINT('Ctrl Pts',(-20.2173661387531,79.8509732204579,
61.7347175085119));
#175173=CARTESIAN_POINT('Ctrl Pts',(-20.1841011379601,81.1444854104172,
62.3372463704192));
#175174=CARTESIAN_POINT('Ctrl Pts',(-20.1588428593053,82.0528151074486,
62.9156573754959));
#175175=CARTESIAN_POINT('Ctrl Pts',(-20.1339068674138,82.8741969746378,
63.6048858697113));
#175176=CARTESIAN_POINT('',(-19.4263813260168,87.1238126841961,74.7426470661147));
#175177=CARTESIAN_POINT('Ctrl Pts',(-20.1339146423347,82.8747673376467,
63.605364495691));
#175178=CARTESIAN_POINT('Ctrl Pts',(-20.0750070626096,83.6655473294934,
64.2689966087262));
#175179=CARTESIAN_POINT('Ctrl Pts',(-20.0153558799609,84.3692856442602,
65.0299429613645));
#175180=CARTESIAN_POINT('Ctrl Pts',(-19.8973223675187,85.576628975846,66.7207259848247));
#175181=CARTESIAN_POINT('Ctrl Pts',(-19.8395215672343,86.0726477946759,
67.6455451969489));
#175182=CARTESIAN_POINT('Ctrl Pts',(-19.7215871660935,86.8132860967313,
69.5867095690446));
#175183=CARTESIAN_POINT('Ctrl Pts',(-19.6618458561677,87.0579171526477,
70.5940527189557));
#175184=CARTESIAN_POINT('Ctrl Pts',(-19.5435268983665,87.290081387854,72.6588170657527));
#175185=CARTESIAN_POINT('Ctrl Pts',(-19.485538173564,87.273451718315,73.7081850984936));
#175186=CARTESIAN_POINT('Ctrl Pts',(-19.4263813260168,87.1238126841961,
74.7426470661147));
#175187=CARTESIAN_POINT('',(-19.1263815299174,87.1238125173955,74.7426482192146));
#175188=CARTESIAN_POINT('',(-19.4263814899908,87.1238253799095,74.7426467836703));
#175189=CARTESIAN_POINT('',(-19.0011490535824,82.874758698514,63.6053538167644));
#175190=CARTESIAN_POINT('Ctrl Pts',(-19.1263815299174,87.1238125173955,
74.7426482192146));
#175191=CARTESIAN_POINT('Ctrl Pts',(-19.1161087162537,87.2734479483372,
73.7082118549104));
#175192=CARTESIAN_POINT('Ctrl Pts',(-19.1067682656167,87.2900817700419,
72.6588612733507));
#175193=CARTESIAN_POINT('Ctrl Pts',(-19.085604853827,87.0579293876326,70.5941212219599));
#175194=CARTESIAN_POINT('Ctrl Pts',(-19.0740038291453,86.8133083884435,
69.5867931485784));
#175195=CARTESIAN_POINT('Ctrl Pts',(-19.0533079901649,86.0726883888103,
67.645626130394));
#175196=CARTESIAN_POINT('Ctrl Pts',(-19.0441709589811,85.5766676037541,
66.720788062231));
#175197=CARTESIAN_POINT('Ctrl Pts',(-19.02327760971,84.3693228475831,65.0299871776317));
#175198=CARTESIAN_POINT('Ctrl Pts',(-19.0117355006677,83.66558539603,64.2690330647643));
#175199=CARTESIAN_POINT('Ctrl Pts',(-19.0011200059672,82.8747987388434,
63.6053908480439));
#175200=CARTESIAN_POINT('',(-19.2012431461282,75.0000012408645,60.7388893865801));
#175201=CARTESIAN_POINT('Ctrl Pts',(-19.0011647644417,82.8742002889142,
63.6048886507497));
#175202=CARTESIAN_POINT('Ctrl Pts',(-19.0263800941151,82.052819403866,62.9156604862996));
#175203=CARTESIAN_POINT('Ctrl Pts',(-19.0510542001329,81.1444903313531,
62.3372490326857));
#175204=CARTESIAN_POINT('Ctrl Pts',(-19.0845340441755,79.8509765741827,
61.7347189482849));
#175205=CARTESIAN_POINT('Ctrl Pts',(-19.0928876791463,79.5230760771588,
61.5989767903968));
#175206=CARTESIAN_POINT('Ctrl Pts',(-19.1179505022709,78.5199407196386,
61.2338652070603));
#175207=CARTESIAN_POINT('Ctrl Pts',(-19.1344708541158,77.8301319180988,
61.0490012011107));
#175208=CARTESIAN_POINT('Ctrl Pts',(-19.1676976678863,76.4255613881577,
60.8012191599193));
#175209=CARTESIAN_POINT('Ctrl Pts',(-19.1845437886602,75.7134618805566,
60.7388894588501));
#175210=CARTESIAN_POINT('Ctrl Pts',(-19.2012431461282,75.0000012408646,
60.7388893865801));
#175211=CARTESIAN_POINT('',(-20.1012419532334,74.9999999736999,85.23888938658));
#175212=CARTESIAN_POINT('Ctrl Pts',(-19.2012431461282,75.0000012408646,
60.7388893865801));
#175213=CARTESIAN_POINT('Ctrl Pts',(-19.2134414436994,74.4788431540949,
60.7388893337893));
#175214=CARTESIAN_POINT('Ctrl Pts',(-19.2255316436779,73.9582261001053,
60.7721462266043));
#175215=CARTESIAN_POINT('Ctrl Pts',(-19.2496023259986,72.9325536678046,
60.9037227977139));
#175216=CARTESIAN_POINT('Ctrl Pts',(-19.2616559602448,72.4284066056991,
61.000875007271));
#175217=CARTESIAN_POINT('Ctrl Pts',(-19.2971923316806,70.964770891133,61.3795292005648));
#175218=CARTESIAN_POINT('Ctrl Pts',(-19.3201799357145,70.0319253130648,
61.747067855105));
#175219=CARTESIAN_POINT('Ctrl Pts',(-19.3593847583475,68.5631416228094,
62.5446770846949));
#175220=CARTESIAN_POINT('Ctrl Pts',(-19.3752189169677,67.9996079481036,
62.9137102767736));
#175221=CARTESIAN_POINT('Ctrl Pts',(-19.4094187241687,66.8432021863185,
63.8150608881449));
#175222=CARTESIAN_POINT('Ctrl Pts',(-19.4278042339043,66.2660911726339,
64.3626902025144));
#175223=CARTESIAN_POINT('Ctrl Pts',(-19.4649076716685,65.2322706283307,
65.5545942849738));
#175224=CARTESIAN_POINT('Ctrl Pts',(-19.48317667112,64.7765667923802,66.1948699295475));
#175225=CARTESIAN_POINT('Ctrl Pts',(-19.5187769340716,64.0126196723153,
67.5210652427873));
#175226=CARTESIAN_POINT('Ctrl Pts',(-19.5363488515712,63.6999414443376,
68.200539244494));
#175227=CARTESIAN_POINT('Ctrl Pts',(-19.5728306395091,63.1810136242172,
69.667751902816));
#175228=CARTESIAN_POINT('Ctrl Pts',(-19.5914858748346,62.9873504500301,
70.4561749871619));
#175229=CARTESIAN_POINT('Ctrl Pts',(-19.6196435768446,62.817633464455,71.6452040910368));
#175230=CARTESIAN_POINT('Ctrl Pts',(-19.6288601738607,62.7809380375738,
72.0349137298658));
#175231=CARTESIAN_POINT('Ctrl Pts',(-19.6544834290468,62.7307562290817,
73.1252885164172));
#175232=CARTESIAN_POINT('Ctrl Pts',(-19.6707160276316,62.7586102506711,
73.8263408637774));
#175233=CARTESIAN_POINT('Ctrl Pts',(-19.7059100506015,62.9475964263193,
75.3253565069979));
#175234=CARTESIAN_POINT('Ctrl Pts',(-19.725057923176,63.1285523053371,76.1175051964773));
#175235=CARTESIAN_POINT('Ctrl Pts',(-19.7559496259563,63.5493004420543,
77.3713704283252));
#175236=CARTESIAN_POINT('Ctrl Pts',(-19.7678070748152,63.7424600523,77.8460957691832));
#175237=CARTESIAN_POINT('Ctrl Pts',(-19.7986461064567,64.3165236659883,
79.0372199075292));
#175238=CARTESIAN_POINT('Ctrl Pts',(-19.8177871208792,64.7398369689772,
79.7304043474254));
#175239=CARTESIAN_POINT('Ctrl Pts',(-19.8478203966771,65.516099512857,80.7571314685154));
#175240=CARTESIAN_POINT('Ctrl Pts',(-19.8588668534339,65.8256947439059,
81.1204375505771));
#175241=CARTESIAN_POINT('Ctrl Pts',(-19.8888962515482,66.7161925145208,
82.0496449273593));
#175242=CARTESIAN_POINT('Ctrl Pts',(-19.9080316552855,67.333342169459,82.5774824699059));
#175243=CARTESIAN_POINT('Ctrl Pts',(-19.9378463954545,68.3820843582458,
83.3080331022866));
#175244=CARTESIAN_POINT('Ctrl Pts',(-19.9486871406438,68.7811211268677,
83.5533145481652));
#175245=CARTESIAN_POINT('Ctrl Pts',(-19.9785111556418,69.9064760633333,
84.1591494050551));
#175246=CARTESIAN_POINT('Ctrl Pts',(-19.9976447410377,70.6560739141292,
84.4714415311945));
#175247=CARTESIAN_POINT('Ctrl Pts',(-20.0273999530786,71.8763787356722,
84.8430979285698));
#175248=CARTESIAN_POINT('Ctrl Pts',(-20.0381847070728,72.3291363992183,
84.9532429649795));
#175249=CARTESIAN_POINT('Ctrl Pts',(-20.0663734302189,73.5172146050537,
85.1714571165322));
#175250=CARTESIAN_POINT('Ctrl Pts',(-20.0839074383617,74.2579106759087,
85.2388893849859));
#175251=CARTESIAN_POINT('Ctrl Pts',(-20.1012419538474,74.9999999736855,
85.23888938658));
#175252=CARTESIAN_POINT('',(-18.5675364832709,75.,85.23888938658));
#175253=CARTESIAN_POINT('',(-30.2175364832709,75.,85.23888938658));
#175254=CARTESIAN_POINT('Origin',(-18.5675364832709,75.,72.98888938658));
#175255=CARTESIAN_POINT('Ctrl Pts',(-20.1012419538474,74.9999999736855,
85.23888938658));
#175256=CARTESIAN_POINT('Ctrl Pts',(-20.1028223166909,75.0676551875689,
85.2388893867253));
#175257=CARTESIAN_POINT('Ctrl Pts',(-20.1044017500603,75.1353219645402,
85.2383289101491));
#175258=CARTESIAN_POINT('Ctrl Pts',(-20.1153971737163,75.6066547974153,
85.2305174346676));
#175259=CARTESIAN_POINT('Ctrl Pts',(-20.1247609958429,76.009738492333,85.2038767090203));
#175260=CARTESIAN_POINT('Ctrl Pts',(-20.1530480306987,77.2159205135722,
85.0640365427909));
#175261=CARTESIAN_POINT('Ctrl Pts',(-20.1721961606555,78.0098209912336,
84.8910092458878));
#175262=CARTESIAN_POINT('Ctrl Pts',(-20.2097492344187,79.5392277376216,
84.3947517872493));
#175263=CARTESIAN_POINT('Ctrl Pts',(-20.2281692206887,80.2718241419228,
84.0751941446952));
#175264=CARTESIAN_POINT('Ctrl Pts',(-20.265532914787,81.6596032469581,83.300974092744));
#175265=CARTESIAN_POINT('Ctrl Pts',(-20.2840271704208,82.3120316605387,
82.8490926166641));
#175266=CARTESIAN_POINT('Ctrl Pts',(-20.3202501892902,83.50066929936,81.8425624201366));
#175267=CARTESIAN_POINT('Ctrl Pts',(-20.3382423866161,84.0373753924667,
81.2939928603718));
#175268=CARTESIAN_POINT('Ctrl Pts',(-20.3717530294913,84.9365885538429,
80.1837622258671));
#175269=CARTESIAN_POINT('Ctrl Pts',(-20.3871132904699,85.3113286396946,
79.635579466878));
#175270=CARTESIAN_POINT('Ctrl Pts',(-20.4117890395023,85.8362236370969,
78.7156457704034));
#175271=CARTESIAN_POINT('Ctrl Pts',(-20.421094180155,86.0157658109008,78.3621921294577));
#175272=CARTESIAN_POINT('Ctrl Pts',(-20.448804125734,86.4978596859949,77.2869681387593));
#175273=CARTESIAN_POINT('Ctrl Pts',(-20.467019065534,86.7487697008896,76.5442620191068));
#175274=CARTESIAN_POINT('Ctrl Pts',(-20.5040710007189,87.1120325898912,
74.9934560479705));
#175275=CARTESIAN_POINT('Ctrl Pts',(-20.5231799791372,87.2181120052346,
74.1877862472172));
#175276=CARTESIAN_POINT('Ctrl Pts',(-20.5557315826169,87.262242220435,72.7976337715917));
#175277=CARTESIAN_POINT('Ctrl Pts',(-20.5691687789934,87.2394256899517,
72.2171244313196));
#175278=CARTESIAN_POINT('Ctrl Pts',(-20.601583588832,87.0863470034626,70.8349469069845));
#175279=CARTESIAN_POINT('Ctrl Pts',(-20.6207303159624,86.9174291951864,
70.0403079980347));
#175280=CARTESIAN_POINT('Ctrl Pts',(-20.6582415576073,86.4293524196668,
68.5092825435072));
#175281=CARTESIAN_POINT('Ctrl Pts',(-20.6766611147279,86.1139751779511,
67.7757783466081));
#175282=CARTESIAN_POINT('Ctrl Pts',(-20.7139441602189,85.3489439344115,
66.3870454821064));
#175283=CARTESIAN_POINT('Ctrl Pts',(-20.7323540862565,84.9023774132677,
65.7343795777472));
#175284=CARTESIAN_POINT('Ctrl Pts',(-20.7684423465106,83.9067986201705,
64.544176703437));
#175285=CARTESIAN_POINT('Ctrl Pts',(-20.7863796880053,83.3638662589221,
64.0061298905882));
#175286=CARTESIAN_POINT('Ctrl Pts',(-20.819482597375,82.2728299293608,63.1101366643164));
#175287=CARTESIAN_POINT('Ctrl Pts',(-20.8345200996702,81.7392693547576,
62.7387157770536));
#175288=CARTESIAN_POINT('Ctrl Pts',(-20.8685278016309,80.4789467263994,
62.002508333814));
#175289=CARTESIAN_POINT('Ctrl Pts',(-20.8876760720512,79.7402454016475,
61.6641599491032));
#175290=CARTESIAN_POINT('Ctrl Pts',(-20.9252196337597,78.2194380305459,
61.1426538905575));
#175291=CARTESIAN_POINT('Ctrl Pts',(-20.9436417815588,77.4418691498786,
60.9582888637351));
#175292=CARTESIAN_POINT('Ctrl Pts',(-20.9809858540324,75.86814439489,60.7441145447466));
#175293=CARTESIAN_POINT('Ctrl Pts',(-20.9994564621255,75.0758712250009,
60.7136119037197));
#175294=CARTESIAN_POINT('Ctrl Pts',(-21.035655851417,73.5219913558667,60.8043087243461));
#175295=CARTESIAN_POINT('Ctrl Pts',(-21.0536474532168,72.7636378407663,
60.9204515119222));
#175296=CARTESIAN_POINT('Ctrl Pts',(-21.0870392604064,71.3825806657978,
61.2666833019794));
#175297=CARTESIAN_POINT('Ctrl Pts',(-21.1022910619968,70.7579984613976,
61.4779701746728));
#175298=CARTESIAN_POINT('Ctrl Pts',(-21.1365117190325,69.4090390905218,
62.059086120334));
#175299=CARTESIAN_POINT('Ctrl Pts',(-21.1556599928895,68.6983143827961,
62.4528465332682));
#175300=CARTESIAN_POINT('Ctrl Pts',(-21.1932065886658,67.3759844771906,
63.3674268622471));
#175301=CARTESIAN_POINT('Ctrl Pts',(-21.2116283123113,66.7661046410529,
63.8838842631046));
#175302=CARTESIAN_POINT('Ctrl Pts',(-21.248978490679,65.659598076138,65.0236246952985));
#175303=CARTESIAN_POINT('Ctrl Pts',(-21.267456116477,65.1647440817905,65.6433942431097));
#175304=CARTESIAN_POINT('Ctrl Pts',(-21.3036624201977,64.3154992015791,
66.9481885705126));
#175305=CARTESIAN_POINT('Ctrl Pts',(-21.3216541228067,63.9589435030155,
67.6275753624872));
#175306=CARTESIAN_POINT('Ctrl Pts',(-21.355080561869,63.417577167365,68.9459806329616));
#175307=CARTESIAN_POINT('Ctrl Pts',(-21.3703640420479,63.2167111228776,
69.5754258751196));
#175308=CARTESIAN_POINT('Ctrl Pts',(-21.4046161709535,62.8841636337735,
71.0074871142765));
#175309=CARTESIAN_POINT('Ctrl Pts',(-21.4237644421783,62.7796352669119,
71.8132496104919));
#175310=CARTESIAN_POINT('Ctrl Pts',(-21.4613114637403,62.7316661781799,
73.4203395033265));
#175311=CARTESIAN_POINT('Ctrl Pts',(-21.4797331112469,62.7857374480785,
74.2176902529325));
#175312=CARTESIAN_POINT('Ctrl Pts',(-21.5170841560245,63.0470665200251,
75.784597454807));
#175313=CARTESIAN_POINT('Ctrl Pts',(-21.5355627995451,63.2525521160856,
76.5506415933651));
#175314=CARTESIAN_POINT('Ctrl Pts',(-21.5728111592244,63.8150992117279,
78.050231102644));
#175315=CARTESIAN_POINT('Ctrl Pts',(-21.5918703440964,64.1743111610024,
78.7788496574188));
#175316=CARTESIAN_POINT('Ctrl Pts',(-21.6254652707981,64.9324581646813,
79.9957208106493));
#175317=CARTESIAN_POINT('Ctrl Pts',(-21.6399043307748,65.3019956610183,
80.4988691966758));
#175318=CARTESIAN_POINT('Ctrl Pts',(-21.6733168717337,66.2363698955215,
81.5864563713893));
#175319=CARTESIAN_POINT('Ctrl Pts',(-21.6924649125501,66.8242294875584,
82.1472814426361));
#175320=CARTESIAN_POINT('Ctrl Pts',(-21.7205547811873,67.7726337654651,
82.8874649023955));
#175321=CARTESIAN_POINT('Ctrl Pts',(-21.7296687303816,68.0935491655393,
83.1139847958481));
#175322=CARTESIAN_POINT('Ctrl Pts',(-21.7576697230568,69.1087909334589,
83.759839284864));
#175323=CARTESIAN_POINT('Ctrl Pts',(-21.7768004439335,69.8343025437369,
84.126001677358));
#175324=CARTESIAN_POINT('Ctrl Pts',(-21.8143017642663,71.3303827853448,
84.7032000564873));
#175325=CARTESIAN_POINT('Ctrl Pts',(-21.8325820446841,72.0960836069837,
84.9161033760842));
#175326=CARTESIAN_POINT('Ctrl Pts',(-21.860391207462,73.2618002069962,85.12123634458));
#175327=CARTESIAN_POINT('Ctrl Pts',(-21.8695882980235,73.6496522610376,
85.1705043446784));
#175328=CARTESIAN_POINT('Ctrl Pts',(-21.8862630534666,74.3590334071425,
85.2263152718581));
#175329=CARTESIAN_POINT('Ctrl Pts',(-21.8937447193925,74.6795488660732,
85.23888938658));
#175330=CARTESIAN_POINT('Ctrl Pts',(-21.9012048916249,75.,85.23888938658));
#175331=CARTESIAN_POINT('Origin',(-30.2175364832709,75.,72.98888938658));
#175332=CARTESIAN_POINT('',(-23.7011390782975,75.,85.23888938658));
#175333=CARTESIAN_POINT('',(-23.0338668482845,75.,85.23888938658));
#175334=CARTESIAN_POINT('',(-30.2175364832709,75.,85.23888938658));
#175335=CARTESIAN_POINT('Ctrl Pts',(-23.0338668482845,75.,85.23888938658));
#175336=CARTESIAN_POINT('Ctrl Pts',(-23.0263120013374,74.6783909709593,
85.23888938658));
#175337=CARTESIAN_POINT('Ctrl Pts',(-23.0187763345677,74.3567175223817,
85.2262242055521));
#175338=CARTESIAN_POINT('Ctrl Pts',(-23.0021463072687,73.646290598585,85.1701281976121));
#175339=CARTESIAN_POINT('Ctrl Pts',(-22.9930805082051,73.2585458076826,
85.1207666313114));
#175340=CARTESIAN_POINT('Ctrl Pts',(-22.9655328564508,72.0931519560926,
84.9153772668127));
#175341=CARTESIAN_POINT('Ctrl Pts',(-22.9468179854882,71.3276772120241,
84.702339729707));
#175342=CARTESIAN_POINT('Ctrl Pts',(-22.909325835243,69.8318905314435,84.1248828191962));
#175343=CARTESIAN_POINT('Ctrl Pts',(-22.8906302771522,69.1064587569298,
83.7585632583867));
#175344=CARTESIAN_POINT('Ctrl Pts',(-22.8623485231606,68.0913006755297,
83.1124533420822));
#175345=CARTESIAN_POINT('Ctrl Pts',(-22.8531101847616,67.7703796652923,
82.885821448698));
#175346=CARTESIAN_POINT('Ctrl Pts',(-22.8249319472578,66.8220873124818,
82.1453693358333));
#175347=CARTESIAN_POINT('Ctrl Pts',(-22.8062649784837,66.2343545239643,
81.5844021538354));
#175348=CARTESIAN_POINT('Ctrl Pts',(-22.772514657242,65.2975885592793,80.4935127700809));
#175349=CARTESIAN_POINT('Ctrl Pts',(-22.7577467471229,64.9260065200069,
79.986804823199));
#175350=CARTESIAN_POINT('Ctrl Pts',(-22.7241964292437,64.1672401178712,
78.7656014122186));
#175351=CARTESIAN_POINT('Ctrl Pts',(-22.705439963898,63.808944887396,78.0365987554647));
#175352=CARTESIAN_POINT('Ctrl Pts',(-22.6677622618039,63.2480161277709,
76.5357888114333));
#175353=CARTESIAN_POINT('Ctrl Pts',(-22.6493118745897,63.0433526965446,
75.7688555730252));
#175354=CARTESIAN_POINT('Ctrl Pts',(-22.6123430726462,62.784051079789,74.2008677874072));
#175355=CARTESIAN_POINT('Ctrl Pts',(-22.5935539315486,62.7310754699687,
73.4033577197027));
#175356=CARTESIAN_POINT('Ctrl Pts',(-22.5559060724289,62.781283068323,71.7962247618505));
#175357=CARTESIAN_POINT('Ctrl Pts',(-22.5372356107837,62.8869387764042,
70.990580215964));
#175358=CARTESIAN_POINT('Ctrl Pts',(-22.5087256307091,63.1632579992058,
69.8081608861876));
#175359=CARTESIAN_POINT('Ctrl Pts',(-22.4992183387842,63.2745084341583,
69.4198078208809));
#175360=CARTESIAN_POINT('Ctrl Pts',(-22.4707616900542,63.6660156724947,
68.2708918550354));
#175361=CARTESIAN_POINT('Ctrl Pts',(-22.4521007963699,64.0027134346281,
67.5319316564175));
#175362=CARTESIAN_POINT('Ctrl Pts',(-22.4221282699137,64.6454425721158,
66.4264747920951));
#175363=CARTESIAN_POINT('Ctrl Pts',(-22.4110817102931,64.9040650358912,
66.0351678654252));
#175364=CARTESIAN_POINT('Ctrl Pts',(-22.3811040731956,65.6691619197105,
65.0105288885819));
#175365=CARTESIAN_POINT('Ctrl Pts',(-22.3624431202076,66.2170498682182,
64.4110947555521));
#175366=CARTESIAN_POINT('Ctrl Pts',(-22.3322146846502,67.1769138921836,
63.5500541139756));
#175367=CARTESIAN_POINT('Ctrl Pts',(-22.3209160929939,67.5522257861086,
63.2511818551385));
#175368=CARTESIAN_POINT('Ctrl Pts',(-22.2906934185333,68.6064343357118,
62.508367425302));
#175369=CARTESIAN_POINT('Ctrl Pts',(-22.2720314700177,69.3134571007556,
62.1085285853074));
#175370=CARTESIAN_POINT('Ctrl Pts',(-22.2407773987685,70.532645300244,61.5705672310305));
#175371=CARTESIAN_POINT('Ctrl Pts',(-22.2284680414892,71.0235294802595,
61.3904833254764));
#175372=CARTESIAN_POINT('Ctrl Pts',(-22.197269485049,72.3017101128349,61.0122943939119));
#175373=CARTESIAN_POINT('Ctrl Pts',(-22.1785935328695,73.0999239393653,
60.8600268606802));
#175374=CARTESIAN_POINT('Ctrl Pts',(-22.1504170890603,74.2948041261042,
60.7530176446002));
#175375=CARTESIAN_POINT('Ctrl Pts',(-22.1412575001515,74.6837354561053,
60.7367942227941));
#175376=CARTESIAN_POINT('Ctrl Pts',(-22.1131454851736,75.8828449525262,
60.7439182963387));
#175377=CARTESIAN_POINT('Ctrl Pts',(-22.0944845789022,76.6904385687269,
60.8290724566312));
#175378=CARTESIAN_POINT('Ctrl Pts',(-22.0644079776263,77.9468822684201,
61.0892202410691));
#175379=CARTESIAN_POINT('Ctrl Pts',(-22.0532589317533,78.4041274143085,
61.2118711536342));
#175380=CARTESIAN_POINT('Ctrl Pts',(-22.0231815612751,79.6221848193041,
61.6154867007138));
#175381=CARTESIAN_POINT('Ctrl Pts',(-22.0045203442948,80.3640608371865,
61.945985284902));
#175382=CARTESIAN_POINT('Ctrl Pts',(-21.9738909404253,81.4988620635565,
62.5930511504154));
#175383=CARTESIAN_POINT('Ctrl Pts',(-21.9621972881698,81.9145368779402,
62.8647675968961));
#175384=CARTESIAN_POINT('Ctrl Pts',(-21.9315920193264,82.9627916328812,
63.6447323820389));
#175385=CARTESIAN_POINT('Ctrl Pts',(-21.9129263876182,83.5633824444697,
64.1918557313839));
#175386=CARTESIAN_POINT('Ctrl Pts',(-21.8797508772358,84.5090247055591,
65.2426144734212));
#175387=CARTESIAN_POINT('Ctrl Pts',(-21.8655483736077,84.8788580692846,
65.7201554167352));
#175388=CARTESIAN_POINT('Ctrl Pts',(-21.8325390794003,85.6596290684338,
66.898600115335));
#175389=CARTESIAN_POINT('Ctrl Pts',(-21.8138060932651,86.0391010609107,
67.6169660992002));
#175390=CARTESIAN_POINT('Ctrl Pts',(-21.7762304371996,86.6419396418536,
69.0968546758051));
#175391=CARTESIAN_POINT('Ctrl Pts',(-21.7578527532016,86.8680156369997,
69.8531430322923));
#175392=CARTESIAN_POINT('Ctrl Pts',(-21.7210286054322,87.1734415483734,
71.4067543125131));
#175393=CARTESIAN_POINT('Ctrl Pts',(-21.7023040011737,87.2504951157242,
72.2007313623139));
#175394=CARTESIAN_POINT('Ctrl Pts',(-21.6646685076583,87.2494910342737,
73.8068600343059));
#175395=CARTESIAN_POINT('Ctrl Pts',(-21.646005872562,87.1685851536727,74.6151245877216));
#175396=CARTESIAN_POINT('Ctrl Pts',(-21.6143142329042,86.9016250375725,
75.9395158528669));
#175397=CARTESIAN_POINT('Ctrl Pts',(-21.6015735042928,86.7598021247821,
76.4619185572941));
#175398=CARTESIAN_POINT('Ctrl Pts',(-21.5699607729825,86.3202589225274,
77.7398285391198));
#175399=CARTESIAN_POINT('Ctrl Pts',(-21.5512745108845,85.98114122429,78.4783539511488));
#175400=CARTESIAN_POINT('Ctrl Pts',(-21.5230340597457,85.3739164593992,
79.5155579927865));
#175401=CARTESIAN_POINT('Ctrl Pts',(-21.5138267781192,85.1602057794428,
79.8435057235982));
#175402=CARTESIAN_POINT('Ctrl Pts',(-21.4856735614721,84.4567546946394,
80.8176150508236));
#175403=CARTESIAN_POINT('Ctrl Pts',(-21.4670104272666,83.9183223689934,
81.4258722644299));
#175404=CARTESIAN_POINT('Ctrl Pts',(-21.4350379002795,82.9184112585684,
82.3519309510348));
#175405=CARTESIAN_POINT('Ctrl Pts',(-21.4220203126617,82.488095121459,82.6995133893867));
#175406=CARTESIAN_POINT('Ctrl Pts',(-21.3901421683619,81.3721585820072,
83.4824731299147));
#175407=CARTESIAN_POINT('Ctrl Pts',(-21.3714481011795,80.6639444453159,
83.8810625691443));
#175408=CARTESIAN_POINT('Ctrl Pts',(-21.3431722529523,79.5621920905754,
84.364429515229));
#175409=CARTESIAN_POINT('Ctrl Pts',(-21.3339383729774,79.1954466615754,
84.5047366456281));
#175410=CARTESIAN_POINT('Ctrl Pts',(-21.3057636184893,78.0526067978761,
84.8801022401905));
#175411=CARTESIAN_POINT('Ctrl Pts',(-21.2870973434153,77.2594137432834,
85.0559685801673));
#175412=CARTESIAN_POINT('Ctrl Pts',(-21.2566621730713,75.9718283819674,
85.2099586950105));
#175413=CARTESIAN_POINT('Ctrl Pts',(-21.2452100806794,75.4860727952401,
85.2388893847883));
#175414=CARTESIAN_POINT('Ctrl Pts',(-21.2338306951809,75.0000000451541,
85.23888938658));
#175415=CARTESIAN_POINT('Ctrl Pts',(-21.9012048916249,75.,85.23888938658));
#175416=CARTESIAN_POINT('Ctrl Pts',(-21.912586321363,75.4888884534696,85.23888938658));
#175417=CARTESIAN_POINT('Ctrl Pts',(-21.9239205229409,75.9776271232784,
85.2096225450995));
#175418=CARTESIAN_POINT('Ctrl Pts',(-21.9478961821272,76.9924718404084,
85.0874979530066));
#175419=CARTESIAN_POINT('Ctrl Pts',(-21.9604488578908,77.5166460610561,
84.9894213843955));
#175420=CARTESIAN_POINT('Ctrl Pts',(-21.9918811638311,78.8181833158265,
84.6568425582864));
#175421=CARTESIAN_POINT('Ctrl Pts',(-22.0105626377578,79.5817381472458,
84.3786799766011));
#175422=CARTESIAN_POINT('Ctrl Pts',(-22.0387765318448,80.6638973212022,
83.8578868167239));
#175423=CARTESIAN_POINT('Ctrl Pts',(-22.047963967763,81.007304699502,83.6719193403085));
#175424=CARTESIAN_POINT('Ctrl Pts',(-22.0761003861245,82.0344804774716,
83.0504535172506));
#175425=CARTESIAN_POINT('Ctrl Pts',(-22.0947621134101,82.6843931620147,
82.5632869565897));
#175426=CARTESIAN_POINT('Ctrl Pts',(-22.1258540645354,83.6613163762424,
81.6670157259261));
#175427=CARTESIAN_POINT('Ctrl Pts',(-22.1380036120981,84.0188201814993,
81.2948608886773));
#175428=CARTESIAN_POINT('Ctrl Pts',(-22.1690484562985,84.8753753289718,
80.2824828351675));
#175429=CARTESIAN_POINT('Ctrl Pts',(-22.187721216155,85.3362271984165,79.6132346325209));
#175430=CARTESIAN_POINT('Ctrl Pts',(-22.2237942094955,86.0779072546758,
78.2679920585282));
#175431=CARTESIAN_POINT('Ctrl Pts',(-22.2408382490607,86.3710832047136,
77.6027196336544));
#175432=CARTESIAN_POINT('Ctrl Pts',(-22.2668498050486,86.729151558269,76.544560108793));
#175433=CARTESIAN_POINT('Ctrl Pts',(-22.2759272013247,86.836795687971,76.1678919732641));
#175434=CARTESIAN_POINT('Ctrl Pts',(-22.3033834381558,87.105287081249,75.023402150957));
#175435=CARTESIAN_POINT('Ctrl Pts',(-22.3218965085367,87.2106624127075,
74.2446545384812));
#175436=CARTESIAN_POINT('Ctrl Pts',(-22.3577323383323,87.269894669926,72.7095136457393));
#175437=CARTESIAN_POINT('Ctrl Pts',(-22.3751417675776,87.2295980158523,
71.9567578392927));
#175438=CARTESIAN_POINT('Ctrl Pts',(-22.4113116058556,87.0065321938148,
70.4347788507262));
#175439=CARTESIAN_POINT('Ctrl Pts',(-22.429662439971,86.8179661250924,69.6698563217369));
#175440=CARTESIAN_POINT('Ctrl Pts',(-22.4664299287135,86.2939170618744,
68.1782892826909));
#175441=CARTESIAN_POINT('Ctrl Pts',(-22.4851244804542,85.9580308520165,
67.4557177032548));
#175442=CARTESIAN_POINT('Ctrl Pts',(-22.5227458722235,85.1432600648163,
66.0727335883611));
#175443=CARTESIAN_POINT('Ctrl Pts',(-22.5414073161341,84.6637588863931,
65.4171855764211));
#175444=CARTESIAN_POINT('Ctrl Pts',(-22.5722643028744,83.7855937627976,
64.4371902879453));
#175445=CARTESIAN_POINT('Ctrl Pts',(-22.5841822499176,83.4251278384314,
64.0818451042407));
#175446=CARTESIAN_POINT('Ctrl Pts',(-22.6150040070451,82.4324300019875,
63.2175829726687));
#175447=CARTESIAN_POINT('Ctrl Pts',(-22.6336727732604,81.7698128061756,
62.7473524548337));
#175448=CARTESIAN_POINT('Ctrl Pts',(-22.6681615035931,80.4934350204194,
62.0199139796853));
#175449=CARTESIAN_POINT('Ctrl Pts',(-22.683654689078,79.8958711362499,61.74048052583));
#175450=CARTESIAN_POINT('Ctrl Pts',(-22.7168617911713,78.5614370104438,
61.243051738332));
#175451=CARTESIAN_POINT('Ctrl Pts',(-22.7346003127391,77.8206366530425,
61.0434910778566));
#175452=CARTESIAN_POINT('Ctrl Pts',(-22.7712051161519,76.2863466356868,
60.7809578982311));
#175453=CARTESIAN_POINT('Ctrl Pts',(-22.7896421665589,75.4955214493371,
60.723379044344));
#175454=CARTESIAN_POINT('Ctrl Pts',(-22.8265862691434,73.9076783255466,
60.7616688154799));
#175455=CARTESIAN_POINT('Ctrl Pts',(-22.8453667500809,73.1144494904388,
60.8586469249961));
#175456=CARTESIAN_POINT('Ctrl Pts',(-22.883016901072,71.5451717287155,61.208244562513));
#175457=CARTESIAN_POINT('Ctrl Pts',(-22.9016852345603,70.7734956343306,
61.462567723342));
#175458=CARTESIAN_POINT('Ctrl Pts',(-22.9359987009992,69.4373570739347,
62.0552916966354));
#175459=CARTESIAN_POINT('Ctrl Pts',(-22.9513198607114,68.8641024388829,
62.3663980635183));
#175460=CARTESIAN_POINT('Ctrl Pts',(-22.9843524361103,67.6769570109697,
63.1389623386834));
#175461=CARTESIAN_POINT('Ctrl Pts',(-23.0020747944056,67.0761284594397,
63.6155080452088));
#175462=CARTESIAN_POINT('Ctrl Pts',(-23.0386402328967,65.9535390102774,
64.6914355274705));
#175463=CARTESIAN_POINT('Ctrl Pts',(-23.057055786477,65.4375575413906,65.2917536735474));
#175464=CARTESIAN_POINT('Ctrl Pts',(-23.0939578118267,64.5242824656047,
66.5891391158697));
#175465=CARTESIAN_POINT('Ctrl Pts',(-23.1127205262052,64.1302740978057,
67.2839342198859));
#175466=CARTESIAN_POINT('Ctrl Pts',(-23.150369023893,63.4772774808831,68.7525951946088));
#175467=CARTESIAN_POINT('Ctrl Pts',(-23.1690346957872,63.222317781978,69.5239905982264));
#175468=CARTESIAN_POINT('Ctrl Pts',(-23.202227942829,62.9135806669705,70.9042560445563));
#175469=CARTESIAN_POINT('Ctrl Pts',(-23.216447902048,62.8255154532279,71.5025654295138));
#175470=CARTESIAN_POINT('Ctrl Pts',(-23.2494737518504,62.7234541939232,
72.9132411431064));
#175471=CARTESIAN_POINT('Ctrl Pts',(-23.2682072921613,62.7453318376152,
73.7253705764239));
#175472=CARTESIAN_POINT('Ctrl Pts',(-23.3057864814918,62.9462990163618,
75.3107912865271));
#175473=CARTESIAN_POINT('Ctrl Pts',(-23.3241668488167,63.1204905522849,
76.0808464733005));
#175474=CARTESIAN_POINT('Ctrl Pts',(-23.3609966120288,63.616888236998,77.5846186867617));
#175475=CARTESIAN_POINT('Ctrl Pts',(-23.3797241105354,63.9394396058289,
78.3142962358958));
#175476=CARTESIAN_POINT('Ctrl Pts',(-23.4173608291487,64.7286015836965,
79.7132850820113));
#175477=CARTESIAN_POINT('Ctrl Pts',(-23.4360236235025,65.1957736412047,
80.3778180926077));
#175478=CARTESIAN_POINT('Ctrl Pts',(-23.4678074493266,66.0808862600834,
81.4036674680061));
#175479=CARTESIAN_POINT('Ctrl Pts',(-23.4806390461079,66.4637486534798,
81.7918147908507));
#175480=CARTESIAN_POINT('Ctrl Pts',(-23.5123389224929,67.4776347598111,
82.6911425165524));
#175481=CARTESIAN_POINT('Ctrl Pts',(-23.5310276517792,68.1360094350865,
83.167559580311));
#175482=CARTESIAN_POINT('Ctrl Pts',(-23.5592802040287,69.1750490493099,
83.7724796465241));
#175483=CARTESIAN_POINT('Ctrl Pts',(-23.5684965578351,69.5227521303402,
83.9531781953693));
#175484=CARTESIAN_POINT('Ctrl Pts',(-23.5966572561651,70.6146745287655,
84.4557174583123));
#175485=CARTESIAN_POINT('Ctrl Pts',(-23.6153212874812,71.3826421586133,
84.7206389130407));
#175486=CARTESIAN_POINT('Ctrl Pts',(-23.647754008211,72.7275538437635,85.0398455494248));
#175487=CARTESIAN_POINT('Ctrl Pts',(-23.6612250736101,73.2925523801279,
85.1327842323363));
#175488=CARTESIAN_POINT('Ctrl Pts',(-23.6834766321493,74.240518326684,85.2212331412086));
#175489=CARTESIAN_POINT('Ctrl Pts',(-23.6923070761891,74.6202726623436,
85.23888938658));
#175490=CARTESIAN_POINT('Ctrl Pts',(-23.7011390782975,75.,85.23888938658));
#175491=CARTESIAN_POINT('Origin',(-30.2175364832709,75.,72.98888938658));
#175492=CARTESIAN_POINT('',(-25.5022222452499,75.,85.23888938658));
#175493=CARTESIAN_POINT('',(-24.833932583624,74.9999999810258,85.23888938658));
#175494=CARTESIAN_POINT('',(-30.2175364832709,75.,85.23888938658));
#175495=CARTESIAN_POINT('Ctrl Pts',(-24.83393258407,74.9999999810153,85.23888938658));
#175496=CARTESIAN_POINT('Ctrl Pts',(-24.8330121802999,74.960857355121,85.2388893865193));
#175497=CARTESIAN_POINT('Ctrl Pts',(-24.8320915953716,74.9217106155544,
85.2387017768826));
#175498=CARTESIAN_POINT('Ctrl Pts',(-24.8127288074479,74.0983640523228,
85.2308081150725));
#175499=CARTESIAN_POINT('Ctrl Pts',(-24.7944554783897,73.3166959232225,
85.1480018195794));
#175500=CARTESIAN_POINT('Ctrl Pts',(-24.7588414083011,71.8165776073276,
84.8415734427302));
#175501=CARTESIAN_POINT('Ctrl Pts',(-24.7412594202536,71.1000320551724,
84.6254928687546));
#175502=CARTESIAN_POINT('Ctrl Pts',(-24.70501977218,69.6668392301149,84.0459427716953));
#175503=CARTESIAN_POINT('Ctrl Pts',(-24.6866087150995,68.9571207409134,
83.6746107660014));
#175504=CARTESIAN_POINT('Ctrl Pts',(-24.6587121174065,67.9612855727158,
83.0224389804367));
#175505=CARTESIAN_POINT('Ctrl Pts',(-24.6494928561014,67.6443946644282,
82.792495280465));
#175506=CARTESIAN_POINT('Ctrl Pts',(-24.6236449432613,66.7853464856481,
82.1040135503076));
#175507=CARTESIAN_POINT('Ctrl Pts',(-24.607195609566,66.2712438558182,81.6129741337991));
#175508=CARTESIAN_POINT('Ctrl Pts',(-24.5717868012854,65.2671534027392,
80.4716175012459));
#175509=CARTESIAN_POINT('Ctrl Pts',(-24.5526390934194,64.7934848457995,
79.8113939098884));
#175510=CARTESIAN_POINT('Ctrl Pts',(-24.5245074450009,64.1917606340085,
78.7681225330309));
#175511=CARTESIAN_POINT('Ctrl Pts',(-24.5153625937877,64.011575983453,78.4177117221588));
#175512=CARTESIAN_POINT('Ctrl Pts',(-24.4873393741456,63.5130408309317,
77.321262500087));
#175513=CARTESIAN_POINT('Ctrl Pts',(-24.4682185600995,63.2515827525554,
76.5518058783384));
#175514=CARTESIAN_POINT('Ctrl Pts',(-24.4359839844773,62.9396546659635,
75.2097537695167));
#175515=CARTESIAN_POINT('Ctrl Pts',(-24.4228498483481,62.8497751980916,
74.6490715313364));
#175516=CARTESIAN_POINT('Ctrl Pts',(-24.3907371325704,62.7266073101506,
73.2770561846433));
#175517=CARTESIAN_POINT('Ctrl Pts',(-24.3715910967796,62.7344196684428,
72.4647268153079));
#175518=CARTESIAN_POINT('Ctrl Pts',(-24.3412584919897,62.8754832630862,
71.1728903525902));
#175519=CARTESIAN_POINT('Ctrl Pts',(-24.3299297831827,62.9576560108063,
70.6902574351304));
#175520=CARTESIAN_POINT('Ctrl Pts',(-24.3093242695386,63.157743835355,69.8299664364236));
#175521=CARTESIAN_POINT('Ctrl Pts',(-24.3000501342154,63.2654969868885,
69.4506324720218));
#175522=CARTESIAN_POINT('Ctrl Pts',(-24.2697702028235,63.6767577691774,
68.2301547070909));
#175523=CARTESIAN_POINT('Ctrl Pts',(-24.2490918108296,64.0540125958005,
67.4169304399856));
#175524=CARTESIAN_POINT('Ctrl Pts',(-24.2093264662316,64.9353771546991,
65.9588136368118));
#175525=CARTESIAN_POINT('Ctrl Pts',(-24.1901958334356,65.4221086084808,
65.3088765046616));
#175526=CARTESIAN_POINT('Ctrl Pts',(-24.1605297197393,66.2815503642943,
64.3712018079504));
#175527=CARTESIAN_POINT('Ctrl Pts',(-24.1498287435204,66.6127000649262,
64.0485816731829));
#175528=CARTESIAN_POINT('Ctrl Pts',(-24.1201442699103,67.5724993407992,
63.2138761227789));
#175529=CARTESIAN_POINT('Ctrl Pts',(-24.1010120245648,68.2349415319324,
62.7442499488733));
#175530=CARTESIAN_POINT('Ctrl Pts',(-24.0727021089201,69.289701565734,62.1437073689938));
#175531=CARTESIAN_POINT('Ctrl Pts',(-24.0633386197286,69.6501906439882,
61.9614227308088));
#175532=CARTESIAN_POINT('Ctrl Pts',(-24.0350509998723,70.7595284257385,
61.467697073355));
#175533=CARTESIAN_POINT('Ctrl Pts',(-24.0159028058597,71.5309199688538,
61.2124318421222));
#175534=CARTESIAN_POINT('Ctrl Pts',(-23.9783515037176,73.0999023173503,
60.8609100051232));
#175535=CARTESIAN_POINT('Ctrl Pts',(-23.9599309020457,73.8931184972221,
60.7629715970578));
#175536=CARTESIAN_POINT('Ctrl Pts',(-23.9225709853616,75.4815689532512,
60.722787721409));
#175537=CARTESIAN_POINT('Ctrl Pts',(-23.904081555327,76.2730173676356,60.779524382697));
#175538=CARTESIAN_POINT('Ctrl Pts',(-23.8678634362634,77.8083196437933,
61.0405773617241));
#175539=CARTESIAN_POINT('Ctrl Pts',(-23.8498714208046,78.5495039887092,
61.2394283831196));
#175540=CARTESIAN_POINT('Ctrl Pts',(-23.8163855339271,79.8877636465009,
61.7367574745244));
#175541=CARTESIAN_POINT('Ctrl Pts',(-23.8010478112739,80.4885605653581,
62.0172710457133));
#175542=CARTESIAN_POINT('Ctrl Pts',(-23.7667417987372,81.7680023894197,
62.7461556850651));
#175543=CARTESIAN_POINT('Ctrl Pts',(-23.7475935338195,82.4307052325513,
63.2162711595252));
#175544=CARTESIAN_POINT('Ctrl Pts',(-23.7168433096365,83.4239619206798,
64.08071189901));
#175545=CARTESIAN_POINT('Ctrl Pts',(-23.7051198335117,83.7848512030601,
64.4363956576645));
#175546=CARTESIAN_POINT('Ctrl Pts',(-23.6744145331563,84.6634205510409,
65.4167535831173));
#175547=CARTESIAN_POINT('Ctrl Pts',(-23.6552742920802,85.1429519640128,
66.0722815645031));
#175548=CARTESIAN_POINT('Ctrl Pts',(-23.6272695660277,85.7522480813967,
67.1063898850051));
#175549=CARTESIAN_POINT('Ctrl Pts',(-23.6182185523546,85.9340885984846,
67.4517108876169));
#175550=CARTESIAN_POINT('Ctrl Pts',(-23.590263874454,86.4421807057408,68.539603470355));
#175551=CARTESIAN_POINT('Ctrl Pts',(-23.5711206896711,86.7114636581776,
69.3063279237869));
#175552=CARTESIAN_POINT('Ctrl Pts',(-23.5397769471509,87.0284096400574,
70.6095314041081));
#175553=CARTESIAN_POINT('Ctrl Pts',(-23.5274907470146,87.1201638457728,
71.1326538507386));
#175554=CARTESIAN_POINT('Ctrl Pts',(-23.4962238131374,87.2656105445745,
72.4655747094982));
#175555=CARTESIAN_POINT('Ctrl Pts',(-23.4770806724929,87.2733688763959,
73.277812894189));
#175556=CARTESIAN_POINT('Ctrl Pts',(-23.4490546123071,87.1659225412469,
74.4739710096168));
#175557=CARTESIAN_POINT('Ctrl Pts',(-23.4399878465529,87.1123736033312,
74.8611993165106));
#175558=CARTESIAN_POINT('Ctrl Pts',(-23.4145770368626,86.911318144442,75.9340947150916));
#175559=CARTESIAN_POINT('Ctrl Pts',(-23.3980458367828,86.7233398203084,
76.6106336928983));
#175560=CARTESIAN_POINT('Ctrl Pts',(-23.367041637428,86.2611951901439,77.8505006464516));
#175561=CARTESIAN_POINT('Ctrl Pts',(-23.3526269177924,85.9997219403267,
78.416218202404));
#175562=CARTESIAN_POINT('Ctrl Pts',(-23.3192385975873,85.3013701666968,
79.6672979462397));
#175563=CARTESIAN_POINT('Ctrl Pts',(-23.300090573773,84.8370828892794,80.3340351514571));
#175564=CARTESIAN_POINT('Ctrl Pts',(-23.2695021498846,83.9856822909245,
81.3297294986452));
#175565=CARTESIAN_POINT('Ctrl Pts',(-23.2579317490028,83.6380738197449,
81.6892215484255));
#175566=CARTESIAN_POINT('Ctrl Pts',(-23.2273792588619,82.6717641973288,
82.5734047131662));
#175567=CARTESIAN_POINT('Ctrl Pts',(-23.2082399709085,82.0212544609202,
83.0596831454881));
#175568=CARTESIAN_POINT('Ctrl Pts',(-23.1802414685338,80.9936912667864,
83.6795469027744));
#175569=CARTESIAN_POINT('Ctrl Pts',(-23.1711950484374,80.650441193471,83.8648724434101));
#175570=CARTESIAN_POINT('Ctrl Pts',(-23.1432437850686,79.5680658267244,
84.3841695874317));
#175571=CARTESIAN_POINT('Ctrl Pts',(-23.1241000139813,78.8041887715563,
84.6614118051235));
#175572=CARTESIAN_POINT('Ctrl Pts',(-23.092794553374,77.5058799785268,84.9915092788248));
#175573=CARTESIAN_POINT('Ctrl Pts',(-23.0805447012976,76.9853079426462,
85.0885121181525));
#175574=CARTESIAN_POINT('Ctrl Pts',(-23.0568225823766,75.9752893647638,
85.2097625158968));
#175575=CARTESIAN_POINT('Ctrl Pts',(-23.0453237417114,75.4877187316448,
85.23888938658));
#175576=CARTESIAN_POINT('Ctrl Pts',(-23.0338668482845,75.,85.23888938658));
#175577=CARTESIAN_POINT('',(-24.5014289287959,79.1898481021894,61.4773919099605));
#175578=CARTESIAN_POINT('Ctrl Pts',(-23.7011390782975,75.,85.23888938658));
#175579=CARTESIAN_POINT('Ctrl Pts',(-23.711138974241,75.4299403257455,85.23888938658));
#175580=CARTESIAN_POINT('Ctrl Pts',(-23.7211834578993,75.8598450501858,
85.2162549034665));
#175581=CARTESIAN_POINT('Ctrl Pts',(-23.7405701053338,76.67993557658,85.1295527181096));
#175582=CARTESIAN_POINT('Ctrl Pts',(-23.7498409659175,77.0697177426204,
85.069210539615));
#175583=CARTESIAN_POINT('Ctrl Pts',(-23.7780432552013,78.2500489799088,
84.8276708580129));
#175584=CARTESIAN_POINT('Ctrl Pts',(-23.7967172116631,79.0260974340909,
84.5867384923059));
#175585=CARTESIAN_POINT('Ctrl Pts',(-23.8246735716932,80.122456630624,84.1229455851328));
#175586=CARTESIAN_POINT('Ctrl Pts',(-23.8336166228644,80.4652004592394,
83.9587733355535));
#175587=CARTESIAN_POINT('Ctrl Pts',(-23.8609478396887,81.4917762273504,
83.4069786330634));
#175588=CARTESIAN_POINT('Ctrl Pts',(-23.8790634001258,82.1464024477594,
82.9693036849566));
#175589=CARTESIAN_POINT('Ctrl Pts',(-23.9138127481122,83.2956582429748,
82.0295234357861));
#175590=CARTESIAN_POINT('Ctrl Pts',(-23.9302990833014,83.7978674253144,
81.5415816859414));
#175591=CARTESIAN_POINT('Ctrl Pts',(-23.9655267975286,84.7864708438371,
80.4013076184334));
#175592=CARTESIAN_POINT('Ctrl Pts',(-23.9842685146157,85.2551783471532,
79.7379833250757));
#175593=CARTESIAN_POINT('Ctrl Pts',(-24.0218991260129,86.0447596067269,
78.3461182380094));
#175594=CARTESIAN_POINT('Ctrl Pts',(-24.0403190708493,86.3671820510835,
77.622871999162));
#175595=CARTESIAN_POINT('Ctrl Pts',(-24.0772298684548,86.8704400366199,
76.1178293978822));
#175596=CARTESIAN_POINT('Ctrl Pts',(-24.0959965207465,87.0488096300684,
75.339164270484));
#175597=CARTESIAN_POINT('Ctrl Pts',(-24.1336458027265,87.2534837979751,
73.7448529145002));
#175598=CARTESIAN_POINT('Ctrl Pts',(-24.1523119534404,87.2766522964618,
72.9327309876617));
#175599=CARTESIAN_POINT('Ctrl Pts',(-24.1857152921631,87.1762002643047,
71.513031033439));
#175600=CARTESIAN_POINT('Ctrl Pts',(-24.2001420143546,87.0871443185291,
70.9058728992067));
#175601=CARTESIAN_POINT('Ctrl Pts',(-24.2333633595733,86.7756987037478,
69.5172928243099));
#175602=CARTESIAN_POINT('Ctrl Pts',(-24.252103018098,86.5203555977892,68.7461937853734));
#175603=CARTESIAN_POINT('Ctrl Pts',(-24.2897205685122,85.8696587461812,
67.2848420936276));
#175604=CARTESIAN_POINT('Ctrl Pts',(-24.3081302371888,85.4796044106335,
66.59643013653));
#175605=CARTESIAN_POINT('Ctrl Pts',(-24.3555502304331,84.3081294375343,
64.9277245171954));
#175606=CARTESIAN_POINT('Ctrl Pts',(-24.3849309971721,83.4379723911377,
64.020931329993));
#175607=CARTESIAN_POINT('Ctrl Pts',(-24.4429386257001,81.4573944055484,
62.5049048593974));
#175608=CARTESIAN_POINT('Ctrl Pts',(-24.4722171551946,80.3594150263118,
61.9033791425484));
#175609=CARTESIAN_POINT('Ctrl Pts',(-24.5011646348533,79.1897461138953,
61.4776545483405));
#175610=CARTESIAN_POINT('Ctrl Pts',(-24.5020520203782,79.1897645405808,
61.477661255121));
#175611=CARTESIAN_POINT('Ctrl Pts',(-24.5125418046939,78.7623268423097,
61.322085908071));
#175612=CARTESIAN_POINT('Ctrl Pts',(-24.5228906675777,78.3265556311944,
61.1904388306657));
#175613=CARTESIAN_POINT('Ctrl Pts',(-24.5424644562946,77.4947744517867,
60.9889151848011));
#175614=CARTESIAN_POINT('Ctrl Pts',(-24.5516792289608,77.1006806111332,
60.9136907674308));
#175615=CARTESIAN_POINT('Ctrl Pts',(-24.5778835211609,76.0002940361128,
60.7591588247104));
#175616=CARTESIAN_POINT('Ctrl Pts',(-24.5951014639648,75.2897265319481,
60.7217394633869));
#175617=CARTESIAN_POINT('Ctrl Pts',(-24.6329131207955,73.6976368691199,
60.7763670271403));
#175618=CARTESIAN_POINT('Ctrl Pts',(-24.6531206325569,72.8212005650578,
60.9019251752237));
#175619=CARTESIAN_POINT('Ctrl Pts',(-24.6861647868287,71.4173086727461,
61.2608277090111));
#175620=CARTESIAN_POINT('Ctrl Pts',(-24.6991435803042,70.8791242303854,
61.4389330517108));
#175621=CARTESIAN_POINT('Ctrl Pts',(-24.7290959930944,69.7115537195404,
61.9173650258494));
#175622=CARTESIAN_POINT('Ctrl Pts',(-24.7459006918793,69.0915542528856,
62.2354434946132));
#175623=CARTESIAN_POINT('Ctrl Pts',(-24.7807577979218,67.8410241662928,
63.0179642747568));
#175624=CARTESIAN_POINT('Ctrl Pts',(-24.7986082540868,67.2211292125195,
63.4936555520269));
#175625=CARTESIAN_POINT('Ctrl Pts',(-24.8299852249833,66.2150337533001,
64.4307781454737));
#175626=CARTESIAN_POINT('Ctrl Pts',(-24.8436259496644,65.8095810325872,
64.8677380032304));
#175627=CARTESIAN_POINT('Ctrl Pts',(-24.8655811323225,65.2321081959332,
65.5889718544895));
#175628=CARTESIAN_POINT('Ctrl Pts',(-24.8734682389785,65.0371225598899,
65.8536555248908));
#175629=CARTESIAN_POINT('Ctrl Pts',(-24.8988885544839,64.4425285237137,
66.7327620601062));
#175630=CARTESIAN_POINT('Ctrl Pts',(-24.916225865812,64.0873129039124,67.3752791692422));
#175631=CARTESIAN_POINT('Ctrl Pts',(-24.9445693940492,63.5922400120015,
68.4978200978249));
#175632=CARTESIAN_POINT('Ctrl Pts',(-24.9557990219495,63.4203753776834,
68.9616091579511));
#175633=CARTESIAN_POINT('Ctrl Pts',(-24.991191551118,62.9707920372626,70.4444184105539));
#175634=CARTESIAN_POINT('Ctrl Pts',(-25.0165149476227,62.7963775809172,
71.4896608629926));
#175635=CARTESIAN_POINT('Ctrl Pts',(-25.0605993053149,62.7291359905145,
73.3408964512946));
#175636=CARTESIAN_POINT('Ctrl Pts',(-25.0790518804435,62.7780339324203,
74.1384901465993));
#175637=CARTESIAN_POINT('Ctrl Pts',(-25.1145026886564,63.0234223963534,
75.6710346121499));
#175638=CARTESIAN_POINT('Ctrl Pts',(-25.1316616917218,63.2114049355636,
76.4037603153742));
#175639=CARTESIAN_POINT('Ctrl Pts',(-25.1656894913147,63.6926489417875,
77.7492126837831));
#175640=CARTESIAN_POINT('Ctrl Pts',(-25.1819489843272,63.9716683124179,
78.3640898425759));
#175641=CARTESIAN_POINT('Ctrl Pts',(-25.216118304735,64.6766406413764,79.6288984702076));
#175642=CARTESIAN_POINT('Ctrl Pts',(-25.2338084321378,65.1166502414938,
80.2676859027829));
#175643=CARTESIAN_POINT('Ctrl Pts',(-25.2642361424389,65.9735515230226,
81.2894217431666));
#175644=CARTESIAN_POINT('Ctrl Pts',(-25.2770595146836,66.3620685198686,
81.6930119904588));
#175645=CARTESIAN_POINT('Ctrl Pts',(-25.3068814134131,67.2935598837059,
82.5366283717952));
#175646=CARTESIAN_POINT('Ctrl Pts',(-25.323733229335,67.8493112143265,82.9596567953659));
#175647=CARTESIAN_POINT('Ctrl Pts',(-25.3586951911263,69.0981345086375,
83.7518620114951));
#175648=CARTESIAN_POINT('Ctrl Pts',(-25.376601320342,69.7968141874185,84.1064641152546));
#175649=CARTESIAN_POINT('Ctrl Pts',(-25.4075151318772,71.0581039950824,
84.6014918961754));
#175650=CARTESIAN_POINT('Ctrl Pts',(-25.4206199201852,71.6057279659652,
84.7732010160532));
#175651=CARTESIAN_POINT('Ctrl Pts',(-25.4508552603207,72.8462113482914,
85.0684748773236));
#175652=CARTESIAN_POINT('Ctrl Pts',(-25.4678284623517,73.5417624027446,
85.1720231422624));
#175653=CARTESIAN_POINT('Ctrl Pts',(-25.4904073576037,74.49471956676,85.2310757780062));
#175654=CARTESIAN_POINT('Ctrl Pts',(-25.4963391614053,74.7473913001414,
85.23888938658));
#175655=CARTESIAN_POINT('Ctrl Pts',(-25.5022222452499,75.,85.23888938658));
#175656=CARTESIAN_POINT('Origin',(-30.2175364832709,75.,72.98888938658));
#175657=CARTESIAN_POINT('',(-27.3010916068384,75.,85.23888938658));
#175658=CARTESIAN_POINT('',(-26.6339799854461,75.,85.23888938658));
#175659=CARTESIAN_POINT('',(-30.2175364832709,75.,85.23888938658));
#175660=CARTESIAN_POINT('',(-25.633313136734,79.1896865699813,61.4777794235982));
#175661=CARTESIAN_POINT('Ctrl Pts',(-26.6339799854461,75.,85.23888938658));
#175662=CARTESIAN_POINT('Ctrl Pts',(-26.6191344607835,74.3618886790399,
85.23888938658));
#175663=CARTESIAN_POINT('Ctrl Pts',(-26.6038014873088,73.7246076393242,
85.1890298360207));
#175664=CARTESIAN_POINT('Ctrl Pts',(-26.5510773887447,71.5348844170923,
84.8441233871728));
#175665=CARTESIAN_POINT('Ctrl Pts',(-26.5162064908492,70.037852256756,84.2995345304749));
#175666=CARTESIAN_POINT('Ctrl Pts',(-26.4650951800277,68.1955326183883,
83.1912671047002));
#175667=CARTESIAN_POINT('Ctrl Pts',(-26.4514103901535,67.7269049983729,
82.8626618812816));
#175668=CARTESIAN_POINT('Ctrl Pts',(-26.4174837867177,66.6092017933043,
81.9560294094145));
#175669=CARTESIAN_POINT('Ctrl Pts',(-26.397717102787,65.9954229202779,81.3394994261153));
#175670=CARTESIAN_POINT('Ctrl Pts',(-26.3402521640497,64.4294838156008,
79.3912524211144));
#175671=CARTESIAN_POINT('Ctrl Pts',(-26.3007334648626,63.6714882588937,
77.927602021171));
#175672=CARTESIAN_POINT('Ctrl Pts',(-26.2463389568543,63.0199241914413,
75.6502720141751));
#175673=CARTESIAN_POINT('Ctrl Pts',(-26.2295436540705,62.8815895363798,
74.9252011742734));
#175674=CARTESIAN_POINT('Ctrl Pts',(-26.192645675109,62.7288491446227,73.3776538367586));
#175675=CARTESIAN_POINT('Ctrl Pts',(-26.1730357227808,62.7302834796635,
72.5571854721671));
#175676=CARTESIAN_POINT('Ctrl Pts',(-26.1356161377997,62.893448701657,70.9611979077159));
#175677=CARTESIAN_POINT('Ctrl Pts',(-26.1178365708504,63.0484246652574,
70.1888978503789));
#175678=CARTESIAN_POINT('Ctrl Pts',(-26.0845253655014,63.465989093539,68.8107300743042));
#175679=CARTESIAN_POINT('Ctrl Pts',(-26.0688767706139,63.705513665866,68.2008865543368));
#175680=CARTESIAN_POINT('Ctrl Pts',(-26.0144120069597,64.7089497653021,
66.146257029447));
#175681=CARTESIAN_POINT('Ctrl Pts',(-25.978333870295,65.7113512534435,64.8373035441054));
#175682=CARTESIAN_POINT('Ctrl Pts',(-25.9261162324526,67.3661157897606,
63.3917373803513));
#175683=CARTESIAN_POINT('Ctrl Pts',(-25.9125953614106,67.816675035508,63.0500079896439));
#175684=CARTESIAN_POINT('Ctrl Pts',(-25.8784056904707,69.0294522571061,
62.2558563967337));
#175685=CARTESIAN_POINT('Ctrl Pts',(-25.8582495341768,69.8200434030659,
61.8527550487459));
#175686=CARTESIAN_POINT('Ctrl Pts',(-25.8097366834901,71.7916545355979,
61.1032577446227));
#175687=CARTESIAN_POINT('Ctrl Pts',(-25.7800416015991,72.9949463612515,
60.8422260893582));
#175688=CARTESIAN_POINT('Ctrl Pts',(-25.7334192166397,74.9862994855731,
60.7146562681797));
#175689=CARTESIAN_POINT('Ctrl Pts',(-25.7159396589751,75.7586830737479,
60.738118782859));
#175690=CARTESIAN_POINT('Ctrl Pts',(-25.6770209075191,77.4336945508136,
60.9480964001632));
#175691=CARTESIAN_POINT('Ctrl Pts',(-25.654923438463,78.3279707607524,61.1639952156199));
#175692=CARTESIAN_POINT('Ctrl Pts',(-25.6332414813969,79.189732077303,61.4776494394493));
#175693=CARTESIAN_POINT('Ctrl Pts',(-25.6339066113238,79.1897464476885,
61.4776546698313));
#175694=CARTESIAN_POINT('Ctrl Pts',(-25.6244228599011,79.5687070061174,
61.6155850215755));
#175695=CARTESIAN_POINT('Ctrl Pts',(-25.6149598570696,79.9406262882323,
61.7721452284987));
#175696=CARTESIAN_POINT('Ctrl Pts',(-25.5961845640087,80.6653410871441,
62.1202659299911));
#175697=CARTESIAN_POINT('Ctrl Pts',(-25.5868826993398,81.0178063006061,
62.3113862569872));
#175698=CARTESIAN_POINT('Ctrl Pts',(-25.5592839406543,82.0314738714595,
62.9271967218725));
#175699=CARTESIAN_POINT('Ctrl Pts',(-25.5407561921154,82.6619102834156,
63.3985604625245));
#175700=CARTESIAN_POINT('Ctrl Pts',(-25.5102264420635,83.6270429003146,
64.2764651963806));
#175701=CARTESIAN_POINT('Ctrl Pts',(-25.4981809809063,83.9886043293266,
64.6499927535362));
#175702=CARTESIAN_POINT('Ctrl Pts',(-25.470364243981,84.7633543361056,65.5595136167616));
#175703=CARTESIAN_POINT('Ctrl Pts',(-25.4544354609332,85.158065708514,66.1090341992136));
#175704=CARTESIAN_POINT('Ctrl Pts',(-25.4196190296736,85.9220036523635,
67.3828026001748));
#175705=CARTESIAN_POINT('Ctrl Pts',(-25.4009646689382,86.2686440486874,
68.1169254575523));
#175706=CARTESIAN_POINT('Ctrl Pts',(-25.3728060380299,86.6715156917527,
69.2484003154342));
#175707=CARTESIAN_POINT('Ctrl Pts',(-25.3635897704838,86.7850070930907,
69.623009846663));
#175708=CARTESIAN_POINT('Ctrl Pts',(-25.3380015362742,87.0507602419729,
70.6801890597495));
#175709=CARTESIAN_POINT('Ctrl Pts',(-25.321802762279,87.1628268943266,71.3713103111357));
#175710=CARTESIAN_POINT('Ctrl Pts',(-25.2866422182078,87.2762726975011,
72.8764725514986));
#175711=CARTESIAN_POINT('Ctrl Pts',(-25.2674943079216,87.2568201649851,
73.6887930209408));
#175712=CARTESIAN_POINT('Ctrl Pts',(-25.2393672130477,87.1089389726804,
74.8839006810161));
#175713=CARTESIAN_POINT('Ctrl Pts',(-25.2302257318265,87.041791937479,75.2720271696218));
#175714=CARTESIAN_POINT('Ctrl Pts',(-25.2022049284722,86.7795554791705,
76.4474677567833));
#175715=CARTESIAN_POINT('Ctrl Pts',(-25.1830828927367,86.5249307987711,
77.2192151133254));
#175716=CARTESIAN_POINT('Ctrl Pts',(-25.1508847843385,85.9663959330241,
78.477115675564));
#175717=CARTESIAN_POINT('Ctrl Pts',(-25.137785447126,85.7013110055866,78.9775795287955));
#175718=CARTESIAN_POINT('Ctrl Pts',(-25.1057074235496,84.974651219608,80.1460910728034));
#175719=CARTESIAN_POINT('Ctrl Pts',(-25.0865614772975,84.4794755639195,
80.7900908997777));
#175720=CARTESIAN_POINT('Ctrl Pts',(-25.0562364262827,83.5894869590496,
81.7365845430329));
#175721=CARTESIAN_POINT('Ctrl Pts',(-25.044914848025,83.2336084026925,82.072344040375));
#175722=CARTESIAN_POINT('Ctrl Pts',(-25.0146107691436,82.2371558735807,
82.9056635592529));
#175723=CARTESIAN_POINT('Ctrl Pts',(-24.995473199644,81.5656622672234,83.3624575174222));
#175724=CARTESIAN_POINT('Ctrl Pts',(-24.9655815292263,80.4401412988308,
83.9747594835686));
#175725=CARTESIAN_POINT('Ctrl Pts',(-24.9546683989537,80.0136298427335,
84.1758458051449));
#175726=CARTESIAN_POINT('Ctrl Pts',(-24.9247721148819,78.8251849668783,
84.6545088452004));
#175727=CARTESIAN_POINT('Ctrl Pts',(-24.9056378692957,78.0456005704614,
84.8818720659351));
#175728=CARTESIAN_POINT('Ctrl Pts',(-24.8691385022778,76.5074657479838,
85.1691835366419));
#175729=CARTESIAN_POINT('Ctrl Pts',(-24.8516738491272,75.7544946100201,
85.2388893877493));
#175730=CARTESIAN_POINT('Ctrl Pts',(-24.83393258407,74.9999999810153,85.23888938658));
#175731=CARTESIAN_POINT('Ctrl Pts',(-25.5022222452499,75.,85.23888938658));
#175732=CARTESIAN_POINT('Ctrl Pts',(-25.5145582143817,75.5296836159723,
85.23888938658));
#175733=CARTESIAN_POINT('Ctrl Pts',(-25.5266607095738,76.0590905354262,
85.204536325136));
#175734=CARTESIAN_POINT('Ctrl Pts',(-25.5528563869749,77.1976076353555,
85.0559901518693));
#175735=CARTESIAN_POINT('Ctrl Pts',(-25.5670074610243,77.8034077134567,
84.9297935650865));
#175736=CARTESIAN_POINT('Ctrl Pts',(-25.5979716716373,79.0545874499822,
84.5686637966591));
#175737=CARTESIAN_POINT('Ctrl Pts',(-25.6144957909623,79.6950543068848,
84.3241147354621));
#175738=CARTESIAN_POINT('Ctrl Pts',(-25.6428038802106,80.7750953811887,
83.8043959163946));
#175739=CARTESIAN_POINT('Ctrl Pts',(-25.6547341790472,81.2239504874583,
83.5524757249011));
#175740=CARTESIAN_POINT('Ctrl Pts',(-25.6788361783004,82.1061277943838,
82.9815554703247));
#175741=CARTESIAN_POINT('Ctrl Pts',(-25.6909699054758,82.5369640183544,
82.6607349247864));
#175742=CARTESIAN_POINT('Ctrl Pts',(-25.7112200888136,83.2054426742654,
82.0910848494002));
#175743=CARTESIAN_POINT('Ctrl Pts',(-25.7192361417016,83.4561204881654,
81.8586849080742));
#175744=CARTESIAN_POINT('Ctrl Pts',(-25.743511910138,84.1745022555095,81.1345132843351));
#175745=CARTESIAN_POINT('Ctrl Pts',(-25.7598819243811,84.6114232063115,
80.6140607396345));
#175746=CARTESIAN_POINT('Ctrl Pts',(-25.7874700754102,85.2860334182378,
79.6597521881797));
#175747=CARTESIAN_POINT('Ctrl Pts',(-25.7988506171131,85.5447652769501,
79.2427542847843));
#175748=CARTESIAN_POINT('Ctrl Pts',(-25.8226608907992,86.0378577557304,
78.3300066105182));
#175749=CARTESIAN_POINT('Ctrl Pts',(-25.8350291901725,86.2653630445236,
77.831763274363));
#175750=CARTESIAN_POINT('Ctrl Pts',(-25.8614698333218,86.6709539871991,
76.7586901004144));
#175751=CARTESIAN_POINT('Ctrl Pts',(-25.8757928860907,86.8415752119532,
76.1825750362739));
#175752=CARTESIAN_POINT('Ctrl Pts',(-25.9088926368427,87.135626729741,74.8327338465253));
#175753=CARTESIAN_POINT('Ctrl Pts',(-25.9274277270387,87.2285181775744,
74.0549915971521));
#175754=CARTESIAN_POINT('Ctrl Pts',(-25.956943262443,87.2582207561284,72.7778440792218));
#175755=CARTESIAN_POINT('Ctrl Pts',(-25.9682148471961,87.2396262566493,
72.2817356219742));
#175756=CARTESIAN_POINT('Ctrl Pts',(-25.9890232955504,87.1503377314522,
71.375217119128));
#175757=CARTESIAN_POINT('Ctrl Pts',(-25.9985499355979,87.0887182070633,
70.9646517574472));
#175758=CARTESIAN_POINT('Ctrl Pts',(-26.0248858082225,86.8671575003706,
69.8703439722172));
#175759=CARTESIAN_POINT('Ctrl Pts',(-26.0418770296343,86.6691107154739,
69.1959198412059));
#175760=CARTESIAN_POINT('Ctrl Pts',(-26.076389872062,86.1410827207986,67.8405101810176));
#175761=CARTESIAN_POINT('Ctrl Pts',(-26.0937667670734,85.803624014196,67.1655518865847));
#175762=CARTESIAN_POINT('Ctrl Pts',(-26.1276076056421,85.0216574270792,
65.9064830067026));
#175763=CARTESIAN_POINT('Ctrl Pts',(-26.1442010004447,84.5824647065737,
65.3226992987825));
#175764=CARTESIAN_POINT('Ctrl Pts',(-26.1776635838977,83.6406458278622,
64.2791520242437));
#175765=CARTESIAN_POINT('Ctrl Pts',(-26.1939882784656,83.1464861244611,
63.8152825186859));
#175766=CARTESIAN_POINT('Ctrl Pts',(-26.2282475967468,82.0096615039802,
62.9127989002998));
#175767=CARTESIAN_POINT('Ctrl Pts',(-26.2459640520519,81.3584153361494,
62.4896741456299));
#175768=CARTESIAN_POINT('Ctrl Pts',(-26.2763555392959,80.1778305594957,
61.8730059192247));
#175769=CARTESIAN_POINT('Ctrl Pts',(-26.2891146528552,79.6670833495305,
61.6490865264613));
#175770=CARTESIAN_POINT('Ctrl Pts',(-26.3189224438612,78.4845004647766,
61.2241039602073));
#175771=CARTESIAN_POINT('Ctrl Pts',(-26.3358360679419,77.8070767349799,
61.0443402680199));
#175772=CARTESIAN_POINT('Ctrl Pts',(-26.3693694917381,76.4101983602222,
60.7991277925184));
#175773=CARTESIAN_POINT('Ctrl Pts',(-26.3858965208382,75.6928151195828,
60.7374009453157));
#175774=CARTESIAN_POINT('Ctrl Pts',(-26.4177107095338,74.2988393329807,
60.7403409390513));
#175775=CARTESIAN_POINT('Ctrl Pts',(-26.433098685999,73.6248026975056,60.7976055921089));
#175776=CARTESIAN_POINT('Ctrl Pts',(-26.4739869598978,71.928762114844,61.084204811009));
#175777=CARTESIAN_POINT('Ctrl Pts',(-26.4991577052325,70.9250630761789,
61.3893637125483));
#175778=CARTESIAN_POINT('Ctrl Pts',(-26.5394496017554,69.3356561106817,
62.1047196212309));
#175779=CARTESIAN_POINT('Ctrl Pts',(-26.5551668293537,68.7246641508355,
62.4451664658636));
#175780=CARTESIAN_POINT('Ctrl Pts',(-26.5845868601615,67.6673044851022,
63.1589522258663));
#175781=CARTESIAN_POINT('Ctrl Pts',(-26.5983651700094,67.212064180179,63.5155523955322));
#175782=CARTESIAN_POINT('Ctrl Pts',(-26.6309031984934,66.2047929183061,
64.4264131486841));
#175783=CARTESIAN_POINT('Ctrl Pts',(-26.6494385005048,65.677238477793,65.0040401879711));
#175784=CARTESIAN_POINT('Ctrl Pts',(-26.6835152225745,64.7917739601575,
66.1819107053303));
#175785=CARTESIAN_POINT('Ctrl Pts',(-26.699124989789,64.4230831402206,66.7702353200393));
#175786=CARTESIAN_POINT('Ctrl Pts',(-26.7282222628511,63.8455535873771,
67.8932581754709));
#175787=CARTESIAN_POINT('Ctrl Pts',(-26.7417877914915,63.6206550203681,
68.417498873445));
#175788=CARTESIAN_POINT('Ctrl Pts',(-26.7739871746114,63.1781401653773,
69.6865315707564));
#175789=CARTESIAN_POINT('Ctrl Pts',(-26.7924057247524,62.9930944229818,
70.4401275384381));
#175790=CARTESIAN_POINT('Ctrl Pts',(-26.8259662057046,62.7822023604105,
71.873823859587));
#175791=CARTESIAN_POINT('Ctrl Pts',(-26.841194940152,62.7393317975643,72.5484801014744));
#175792=CARTESIAN_POINT('Ctrl Pts',(-26.8738752755997,62.7665423153993,
73.9706719580667));
#175793=CARTESIAN_POINT('Ctrl Pts',(-26.891785792233,62.849235171412,74.7152278980948));
#175794=CARTESIAN_POINT('Ctrl Pts',(-26.9271500513814,63.1458292715302,
76.1628947758508));
#175795=CARTESIAN_POINT('Ctrl Pts',(-26.9443595783814,63.3560502168863,
76.8636968340701));
#175796=CARTESIAN_POINT('Ctrl Pts',(-26.977276902664,63.8869178748331,78.1897925355681));
#175797=CARTESIAN_POINT('Ctrl Pts',(-26.9929723131151,64.2013438969176,
78.8146081545245));
#175798=CARTESIAN_POINT('Ctrl Pts',(-27.0222081515521,64.8625384705814,
79.8890166205348));
#175799=CARTESIAN_POINT('Ctrl Pts',(-27.035719320342,65.190544498994,80.3478593849382));
#175800=CARTESIAN_POINT('Ctrl Pts',(-27.0673457801649,66.0304724343931,
81.3664133494237));
#175801=CARTESIAN_POINT('Ctrl Pts',(-27.0852704564228,66.5650812259686,
81.904466025504));
#175802=CARTESIAN_POINT('Ctrl Pts',(-27.1191463267901,67.6905232501511,
82.8447335551604));
#175803=CARTESIAN_POINT('Ctrl Pts',(-27.1351057959906,68.2736290477985,
83.2515418518609));
#175804=CARTESIAN_POINT('Ctrl Pts',(-27.1628269622865,69.3133414011717,
83.8500371397582));
#175805=CARTESIAN_POINT('Ctrl Pts',(-27.1744849767242,69.7523000306373,
84.0687919840298));
#175806=CARTESIAN_POINT('Ctrl Pts',(-27.1971313539743,70.6224088729331,
84.439076728993));
#175807=CARTESIAN_POINT('Ctrl Pts',(-27.2080552166184,71.0512797416377,
84.5939618347456));
#175808=CARTESIAN_POINT('Ctrl Pts',(-27.2374137065437,72.2396282620299,
84.949606447519));
#175809=CARTESIAN_POINT('Ctrl Pts',(-27.2554184518982,73.0113618164258,
85.1018468685512));
#175810=CARTESIAN_POINT('Ctrl Pts',(-27.2825281172747,74.1937952563766,
85.2189866014275));
#175811=CARTESIAN_POINT('Ctrl Pts',(-27.2917126768954,74.5968360592202,
85.23888938658));
#175812=CARTESIAN_POINT('Ctrl Pts',(-27.3010916068384,75.,85.23888938658));
#175813=CARTESIAN_POINT('Origin',(-30.2175364832709,75.,72.98888938658));
#175814=CARTESIAN_POINT('',(-28.5675339373409,75.,85.23888938658));
#175815=CARTESIAN_POINT('',(-28.4332364523223,75.,85.23888938658));
#175816=CARTESIAN_POINT('',(-30.2175364832709,75.,85.23888938658));
#175817=CARTESIAN_POINT('',(-28.5670923992066,80.5057115855401,83.931352177925));
#175818=CARTESIAN_POINT('Origin',(-28.5675339373409,75.,72.98888938658));
#175819=CARTESIAN_POINT('Ctrl Pts',(-28.566799738496,80.5059347416729,83.9317949705846));
#175820=CARTESIAN_POINT('Ctrl Pts',(-28.5535796072272,79.9942929045818,
84.1892281124963));
#175821=CARTESIAN_POINT('Ctrl Pts',(-28.5405678264509,79.4652288872978,
84.4104600130184));
#175822=CARTESIAN_POINT('Ctrl Pts',(-28.5147317043305,78.4072126454951,
84.7680835514775));
#175823=CARTESIAN_POINT('Ctrl Pts',(-28.501791026997,77.880764281267,84.9077689340001));
#175824=CARTESIAN_POINT('Ctrl Pts',(-28.4700174024026,76.5730609737536,
85.1630194521663));
#175825=CARTESIAN_POINT('Ctrl Pts',(-28.4514197202864,75.7871460836583,
85.23888938658));
#175826=CARTESIAN_POINT('Ctrl Pts',(-28.4332364523223,75.,85.23888938658));
#175827=CARTESIAN_POINT('Origin',(-30.2175364832709,75.,72.98888938658));
#175828=CARTESIAN_POINT('',(-18.5675364832709,75.,83.48888938658));
#175829=CARTESIAN_POINT('Origin',(-18.5675364832709,75.,72.98888938658));
#175830=CARTESIAN_POINT('',(-16.5675364832709,75.,83.48888938658));
#175831=CARTESIAN_POINT('',(-30.2175364832709,75.,83.48888938658));
#175832=CARTESIAN_POINT('Origin',(-16.5675364832709,75.,72.98888938658));
#175833=CARTESIAN_POINT('Origin',(-30.2175364832709,75.,72.98888938658));
#175834=CARTESIAN_POINT('Ctrl Pts',(-28.4332364523223,75.,85.23888938658));
#175835=CARTESIAN_POINT('Ctrl Pts',(-28.4272749498642,74.7419290458744,
85.23888938658));
#175836=CARTESIAN_POINT('Ctrl Pts',(-28.4213453076129,74.4837260430028,
85.2307342343628));
#175837=CARTESIAN_POINT('Ctrl Pts',(-28.4026862400576,73.6716846387427,
85.1793089434919));
#175838=CARTESIAN_POINT('Ctrl Pts',(-28.3900005580085,73.120626176869,85.1065915600061));
#175839=CARTESIAN_POINT('Ctrl Pts',(-28.3491296798301,71.4220415560737,
84.7637580573169));
#175840=CARTESIAN_POINT('Ctrl Pts',(-28.3208970451119,70.3072774227404,
84.3655230158273));
#175841=CARTESIAN_POINT('Ctrl Pts',(-28.2744393311864,68.5252546847671,
83.4217141014942));
#175842=CARTESIAN_POINT('Ctrl Pts',(-28.2554501173914,67.8262563139882,
82.9540067640435));
#175843=CARTESIAN_POINT('Ctrl Pts',(-28.2169592060924,66.5772317562602,
81.9182646195507));
#175844=CARTESIAN_POINT('Ctrl Pts',(-28.1981684500683,66.0233171933883,
81.3612222826943));
#175845=CARTESIAN_POINT('Ctrl Pts',(-28.1616294382387,65.0322733817012,
80.1523014088068));
#175846=CARTESIAN_POINT('Ctrl Pts',(-28.1439543433449,64.596781755144,79.5037254941978));
#175847=CARTESIAN_POINT('Ctrl Pts',(-28.0882170818909,63.4469586964431,
77.3785390349933));
#175848=CARTESIAN_POINT('Ctrl Pts',(-28.048685544448,62.9644379248214,75.7972773555105));
#175849=CARTESIAN_POINT('Ctrl Pts',(-27.9981982467316,62.7525313524604,
73.6060037079195));
#175850=CARTESIAN_POINT('Ctrl Pts',(-27.9852995728824,62.7371041860924,
73.040908888065));
#175851=CARTESIAN_POINT('Ctrl Pts',(-27.9587146833293,62.784210732244,71.9151150510992));
#175852=CARTESIAN_POINT('Ctrl Pts',(-27.9452213158272,62.846343595883,71.3557522001653));
#175853=CARTESIAN_POINT('Ctrl Pts',(-27.9050939417333,63.1482049915785,
69.6915179279531));
#175854=CARTESIAN_POINT('Ctrl Pts',(-27.8795411038892,63.5024125963837,
68.6135998065467));
#175855=CARTESIAN_POINT('Ctrl Pts',(-27.8157427363851,64.7162759867173,
66.1358619334095));
#175856=CARTESIAN_POINT('Ctrl Pts',(-27.7764672099206,65.7182862431928,
64.8299194672785));
#175857=CARTESIAN_POINT('Ctrl Pts',(-27.7276820821298,67.3215909710765,
63.4310423100382));
#175858=CARTESIAN_POINT('Ctrl Pts',(-27.7162937230547,67.7163678791779,
63.1268860850115));
#175859=CARTESIAN_POINT('Ctrl Pts',(-27.6857189745135,68.7920210069889,
62.3980554773914));
#175860=CARTESIAN_POINT('Ctrl Pts',(-27.6664002681072,69.4979985547185,
62.0147029178625));
#175861=CARTESIAN_POINT('Ctrl Pts',(-27.6273286350037,71.0296360170234,
61.3682125275706));
#175862=CARTESIAN_POINT('Ctrl Pts',(-27.6077835078715,71.8560126351464,
61.117947601639));
#175863=CARTESIAN_POINT('Ctrl Pts',(-27.5502213685077,74.3098029942126,
60.6492701197802));
#175864=CARTESIAN_POINT('Ctrl Pts',(-27.5106451187069,75.9631888004553,
60.6675726774185));
#175865=CARTESIAN_POINT('Ctrl Pts',(-27.4593017697344,78.1518737205639,
61.1360586865382));
#175866=CARTESIAN_POINT('Ctrl Pts',(-27.4455805910085,78.7296572604109,
61.3049875462863));
#175867=CARTESIAN_POINT('Ctrl Pts',(-27.4042205380485,80.3696740473794,
61.9185992689906));
#175868=CARTESIAN_POINT('Ctrl Pts',(-27.3766829939307,81.3845739332598,
62.471187798176));
#175869=CARTESIAN_POINT('Ctrl Pts',(-27.3306180247843,82.9888676637545,
63.6635883551543));
#175870=CARTESIAN_POINT('Ctrl Pts',(-27.3114076338512,83.6157423471456,
64.2394760263181));
#175871=CARTESIAN_POINT('Ctrl Pts',(-27.266683614692,84.8642990763544,65.6518763485752));
#175872=CARTESIAN_POINT('Ctrl Pts',(-27.2419529267703,85.4493246742462,
66.5121738831067));
#175873=CARTESIAN_POINT('Ctrl Pts',(-27.1972850869743,86.326590303122,68.2371433892149));
#175874=CARTESIAN_POINT('Ctrl Pts',(-27.1769847565351,86.644672984736,69.0809060502006));
#175875=CARTESIAN_POINT('Ctrl Pts',(-27.1369967096554,87.0623364724272,
70.7129777021961));
#175876=CARTESIAN_POINT('Ctrl Pts',(-27.1181738246318,87.1834450510193,
71.4910816820856));
#175877=CARTESIAN_POINT('Ctrl Pts',(-27.0815337674519,87.2748157577772,
73.0571920400213));
#175878=CARTESIAN_POINT('Ctrl Pts',(-27.0637927592734,87.2453557865096,
73.8415443202955));
#175879=CARTESIAN_POINT('Ctrl Pts',(-27.0285245469332,87.042273413979,75.3553303872363));
#175880=CARTESIAN_POINT('Ctrl Pts',(-27.0106861812576,86.8763023485678,
76.0823979323705));
#175881=CARTESIAN_POINT('Ctrl Pts',(-26.9560904443585,86.1639986647825,
78.2647375315542));
#175882=CARTESIAN_POINT('Ctrl Pts',(-26.9218022723246,85.406793785591,79.6347969653061));
#175883=CARTESIAN_POINT('Ctrl Pts',(-26.8715478842244,84.0529225937617,
81.2608741454549));
#175884=CARTESIAN_POINT('Ctrl Pts',(-26.8580254905575,83.6621824953892,
81.6691969570759));
#175885=CARTESIAN_POINT('Ctrl Pts',(-26.8233349394846,82.5753679147139,
82.6581833308507));
#175886=CARTESIAN_POINT('Ctrl Pts',(-26.8027190063652,81.8406239914801,
83.1912081901866));
#175887=CARTESIAN_POINT('Ctrl Pts',(-26.7536317685662,79.9848987459978,
84.2461241957079));
#175888=CARTESIAN_POINT('Ctrl Pts',(-26.7238224526101,78.8304820323874,
84.6893982949392));
#175889=CARTESIAN_POINT('Ctrl Pts',(-26.6768151453692,76.8645997039973,
85.1214536856491));
#175890=CARTESIAN_POINT('Ctrl Pts',(-26.6590742008417,76.0853352897924,
85.2158222530688));
#175891=CARTESIAN_POINT('Ctrl Pts',(-26.6386599167246,75.2016038738315,
85.237645433459));
#175892=CARTESIAN_POINT('Ctrl Pts',(-26.636324880805,75.100791606156,85.23888938658));
#175893=CARTESIAN_POINT('Ctrl Pts',(-26.6339799854461,75.,85.23888938658));
#175894=CARTESIAN_POINT('',(-28.2015531594526,75.00001897909,60.7388893865947));
#175895=CARTESIAN_POINT('Ctrl Pts',(-27.3010916068384,75.,85.23888938658));
#175896=CARTESIAN_POINT('Ctrl Pts',(-27.3058229610351,75.2033826262405,
85.23888938658));
#175897=CARTESIAN_POINT('Ctrl Pts',(-27.3106144561045,75.4067963411875,
85.2338243834481));
#175898=CARTESIAN_POINT('Ctrl Pts',(-27.3284325344786,76.1564688718875,
85.196444072552));
#175899=CARTESIAN_POINT('Ctrl Pts',(-27.3416267514371,76.700445405241,85.1326243949349));
#175900=CARTESIAN_POINT('Ctrl Pts',(-27.3663300689989,77.7204171731748,
84.9430629030699));
#175901=CARTESIAN_POINT('Ctrl Pts',(-27.3778533444614,78.196691782318,84.8246024386126));
#175902=CARTESIAN_POINT('Ctrl Pts',(-27.4049117962594,79.311901247527,84.4749770165384));
#175903=CARTESIAN_POINT('Ctrl Pts',(-27.4202137963442,79.9412372568343,
84.2186209013142));
#175904=CARTESIAN_POINT('Ctrl Pts',(-27.443661321696,80.8507374759572,83.7568092182322));
#175905=CARTESIAN_POINT('Ctrl Pts',(-27.4516255212873,81.1487583792507,
83.589455131192));
#175906=CARTESIAN_POINT('Ctrl Pts',(-27.4724655619897,81.895838660614,83.1278143911429));
#175907=CARTESIAN_POINT('Ctrl Pts',(-27.4854035766097,82.3332578802525,
82.8160823844634));
#175908=CARTESIAN_POINT('Ctrl Pts',(-27.5104419511676,83.1471463816151,
82.1513667409141));
#175909=CARTESIAN_POINT('Ctrl Pts',(-27.522530685445,83.5245858552855,81.8012914623614));
#175910=CARTESIAN_POINT('Ctrl Pts',(-27.5502688602431,84.3504208840545,
80.9324734068029));
#175911=CARTESIAN_POINT('Ctrl Pts',(-27.5656966933563,84.779532225077,80.3977786503999));
#175912=CARTESIAN_POINT('Ctrl Pts',(-27.5957947175092,85.5100585257217,
79.3126688038495));
#175913=CARTESIAN_POINT('Ctrl Pts',(-27.6106600120252,85.8183477470029,
78.7694458291332));
#175914=CARTESIAN_POINT('Ctrl Pts',(-27.6444082217492,86.4181348212994,
77.4949663337692));
#175915=CARTESIAN_POINT('Ctrl Pts',(-27.6630233100806,86.6833278989251,
76.7543128852062));
#175916=CARTESIAN_POINT('Ctrl Pts',(-27.6975205814915,87.0495871238234,
75.3066059726427));
#175917=CARTESIAN_POINT('Ctrl Pts',(-27.7134539259211,87.1634343043775,
74.6060515393013));
#175918=CARTESIAN_POINT('Ctrl Pts',(-27.7412590167738,87.2529116368176,
73.4058194687855));
#175919=CARTESIAN_POINT('Ctrl Pts',(-27.7530393663587,87.2597501207847,
72.9102718279261));
#175920=CARTESIAN_POINT('Ctrl Pts',(-27.7757995881677,87.2152814417707,
71.9609702666392));
#175921=CARTESIAN_POINT('Ctrl Pts',(-27.7867125648806,87.1686515422412,
71.5077945096812));
#175922=CARTESIAN_POINT('Ctrl Pts',(-27.8156815443413,86.9757301515703,
70.2989864261983));
#175923=CARTESIAN_POINT('Ctrl Pts',(-27.8333353719806,86.7833350659435,
69.5527983956408));
#175924=CARTESIAN_POINT('Ctrl Pts',(-27.8651210764537,86.3103238864562,
68.2424471102556));
#175925=CARTESIAN_POINT('Ctrl Pts',(-27.8793700232485,86.053820750885,67.6723877258993));
#175926=CARTESIAN_POINT('Ctrl Pts',(-27.9073692610972,85.4892886817221,
66.6370909515588));
#175927=CARTESIAN_POINT('Ctrl Pts',(-27.9207554178926,85.1907845063452,
66.168446960112));
#175928=CARTESIAN_POINT('Ctrl Pts',(-27.9452553340675,84.5800992988148,
65.3397551300243));
#175929=CARTESIAN_POINT('Ctrl Pts',(-27.9564014000352,84.2767144470895,
64.9745189473525));
#175930=CARTESIAN_POINT('Ctrl Pts',(-27.9830279008244,83.4919537648032,
64.134210935316));
#175931=CARTESIAN_POINT('Ctrl Pts',(-27.9982668164661,82.9909700275654,
63.6795928526122));
#175932=CARTESIAN_POINT('Ctrl Pts',(-28.0308464320267,81.8658252908171,
62.8166522069551));
#175933=CARTESIAN_POINT('Ctrl Pts',(-28.0486347182099,81.2367073262537,
62.4192443947449));
#175934=CARTESIAN_POINT('Ctrl Pts',(-28.0843777710471,79.9069104355396,
61.7395093727613));
#175935=CARTESIAN_POINT('Ctrl Pts',(-28.1020658386639,79.2082978167326,
61.4599441731932));
#175936=CARTESIAN_POINT('Ctrl Pts',(-28.1325884212831,77.9375545894379,
61.0824377087962));
#175937=CARTESIAN_POINT('Ctrl Pts',(-28.1455798759461,77.3757856424469,
60.9577440834114));
#175938=CARTESIAN_POINT('Ctrl Pts',(-28.1643434019884,76.5683511157738,
60.8372983827645));
#175939=CARTESIAN_POINT('Ctrl Pts',(-28.1699401585733,76.3283548966331,
60.8087267273936));
#175940=CARTESIAN_POINT('Ctrl Pts',(-28.1841624485064,75.7260116475704,
60.7550329302604));
#175941=CARTESIAN_POINT('Ctrl Pts',(-28.1928541804325,75.3631092856355,
60.7388899491354));
#175942=CARTESIAN_POINT('Ctrl Pts',(-28.2015531594526,75.0000189790899,
60.7388893865947));
#175943=CARTESIAN_POINT('',(-28.5675342178229,63.2672737070204,69.46672519));
#175944=CARTESIAN_POINT('Ctrl Pts',(-28.2015531594526,75.0000189790899,
60.7388893865947));
#175945=CARTESIAN_POINT('Ctrl Pts',(-28.2115085777166,74.5844856319101,
60.7388887428033));
#175946=CARTESIAN_POINT('Ctrl Pts',(-28.2214581486582,74.1692192048778,
60.7600311204056));
#175947=CARTESIAN_POINT('Ctrl Pts',(-28.2563764973938,72.7014270353383,
60.9098820884185));
#175948=CARTESIAN_POINT('Ctrl Pts',(-28.2802056089586,71.6654569059614,
61.153913573752));
#175949=CARTESIAN_POINT('Ctrl Pts',(-28.3161178277994,70.2052579637771,
61.7051026614066));
#175950=CARTESIAN_POINT('Ctrl Pts',(-28.3279543485361,69.7479402986497,
61.9105662236379));
#175951=CARTESIAN_POINT('Ctrl Pts',(-28.3551888069236,68.7402228127518,
62.439770798747));
#175952=CARTESIAN_POINT('Ctrl Pts',(-28.3704805414799,68.1999305771706,
62.7796884624181));
#175953=CARTESIAN_POINT('Ctrl Pts',(-28.4005460677347,67.172577142645,63.5439176697712));
#175954=CARTESIAN_POINT('Ctrl Pts',(-28.4152665757593,66.6876325732374,
63.9677699594751));
#175955=CARTESIAN_POINT('Ctrl Pts',(-28.4443880543649,65.7956167561956,
64.880690622336));
#175956=CARTESIAN_POINT('Ctrl Pts',(-28.458867085717,65.3888279971904,65.3672798388102));
#175957=CARTESIAN_POINT('Ctrl Pts',(-28.498775366339,64.4150539396884,66.7347398350393));
#175958=CARTESIAN_POINT('Ctrl Pts',(-28.5239637024401,63.9201129993077,
67.6605065258106));
#175959=CARTESIAN_POINT('Ctrl Pts',(-28.5548780727218,63.445093108566,68.9106765416759));
#175960=CARTESIAN_POINT('Ctrl Pts',(-28.5615651320877,63.351205608257,69.1871419701496));
#175961=CARTESIAN_POINT('Ctrl Pts',(-28.568231723297,63.2672824189022,69.4666971484707));
#175962=CARTESIAN_POINT('Origin',(-28.5675339373409,75.,72.98888938658));
#175963=CARTESIAN_POINT('Origin',(-23.90845228375,74.9968912574536,72.9873550812444));
#175964=CARTESIAN_POINT('Ctrl Pts',(-19.9173382169355,74.9968858117149,
59.938705268027));
#175965=CARTESIAN_POINT('Ctrl Pts',(-19.9330420568071,74.2767378935156,
59.9387055685744));
#175966=CARTESIAN_POINT('Ctrl Pts',(-19.9489225765158,73.5578381134046,
59.9983214666742));
#175967=CARTESIAN_POINT('Ctrl Pts',(-19.9801875397725,72.1459011840029,
60.2341150131016));
#175968=CARTESIAN_POINT('Ctrl Pts',(-19.9955184081017,71.4550251746423,
60.4084653748063));
#175969=CARTESIAN_POINT('Ctrl Pts',(-20.0214018597075,70.33484625965,60.7908125262915));
#175970=CARTESIAN_POINT('Ctrl Pts',(-20.0317932982671,69.8964947186888,
60.9675269909449));
#175971=CARTESIAN_POINT('Ctrl Pts',(-20.0556893445538,68.9115536151873,
61.428192831652));
#175972=CARTESIAN_POINT('Ctrl Pts',(-20.0690233674465,68.373536871566,61.7278371577208));
#175973=CARTESIAN_POINT('Ctrl Pts',(-20.1014548923896,67.1267436688524,
62.5426181791745));
#175974=CARTESIAN_POINT('Ctrl Pts',(-20.1207321421361,66.4447485068989,
63.0932866102794));
#175975=CARTESIAN_POINT('Ctrl Pts',(-20.1544590052907,65.3517709601478,
64.1738449216507));
#175976=CARTESIAN_POINT('Ctrl Pts',(-20.1687858392181,64.9167365633608,
64.6749072142671));
#175977=CARTESIAN_POINT('Ctrl Pts',(-20.2000827148801,64.0643659267137,
65.8224904223784));
#175978=CARTESIAN_POINT('Ctrl Pts',(-20.2170830906625,63.6622529469042,
66.4772578952479));
#175979=CARTESIAN_POINT('Ctrl Pts',(-20.2482227120542,63.0283175309696,
67.7483152702444));
#175980=CARTESIAN_POINT('Ctrl Pts',(-20.2623973174422,62.7810003086865,
68.3541805370158));
#175981=CARTESIAN_POINT('Ctrl Pts',(-20.2918856392969,62.3683715854022,
69.631439903851));
#175982=CARTESIAN_POINT('Ctrl Pts',(-20.3071798697992,62.208859614119,70.3025983686922));
#175983=CARTESIAN_POINT('Ctrl Pts',(-20.3367714609488,62.0020807315052,
71.6329195219529));
#175984=CARTESIAN_POINT('Ctrl Pts',(-20.3510559154005,61.9503445633049,
72.2893442443117));
#175985=CARTESIAN_POINT('Ctrl Pts',(-20.3785808855754,61.9464631009909,
73.5402113093633));
#175986=CARTESIAN_POINT('Ctrl Pts',(-20.3917485995825,61.9850951817803,
74.1329921751189));
#175987=CARTESIAN_POINT('Ctrl Pts',(-20.4239469084602,62.1786459992294,
75.5768132285351));
#175988=CARTESIAN_POINT('Ctrl Pts',(-20.442671274263,62.3780103413679,76.4190528982472));
#175989=CARTESIAN_POINT('Ctrl Pts',(-20.4731627485336,62.8273500526258,
77.724088988084));
#175990=CARTESIAN_POINT('Ctrl Pts',(-20.484656147901,63.0244933321518,78.2023399842857));
#175991=CARTESIAN_POINT('Ctrl Pts',(-20.5152005459052,63.6255454851649,
79.4453787026285));
#175992=CARTESIAN_POINT('Ctrl Pts',(-20.533963916611,64.0779194525373,80.1838562999077));
#175993=CARTESIAN_POINT('Ctrl Pts',(-20.5641170501726,64.9012866303631,
81.2695486505498));
#175994=CARTESIAN_POINT('Ctrl Pts',(-20.5752195748772,65.2251642673089,
81.6493013698919));
#175995=CARTESIAN_POINT('Ctrl Pts',(-20.5955234230254,65.8592165383069,
82.3117935273445));
#175996=CARTESIAN_POINT('Ctrl Pts',(-20.6046911779992,66.1628183603434,
82.5999201880847));
#175997=CARTESIAN_POINT('Ctrl Pts',(-20.6346185984662,67.1951964060269,
83.48938727183));
#175998=CARTESIAN_POINT('Ctrl Pts',(-20.655580595683,67.9754682664369,84.0263189844671));
#175999=CARTESIAN_POINT('Ctrl Pts',(-20.6920836689512,69.4263633798384,
84.808174845495));
#176000=CARTESIAN_POINT('Ctrl Pts',(-20.7074175988213,70.0719036021621,
85.0913650963437));
#176001=CARTESIAN_POINT('Ctrl Pts',(-20.7364113500887,71.3135071457599,
85.5201836585844));
#176002=CARTESIAN_POINT('Ctrl Pts',(-20.7499833159838,71.9031382356305,
85.6786039963794));
#176003=CARTESIAN_POINT('Ctrl Pts',(-20.7827001188224,73.3514320986593,
85.9607593187245));
#176004=CARTESIAN_POINT('Ctrl Pts',(-20.8015164287551,74.2155559906024,
86.0413303144843));
#176005=CARTESIAN_POINT('Ctrl Pts',(-20.8393343037172,75.9252661660537,
86.0302742768058));
#176006=CARTESIAN_POINT('Ctrl Pts',(-20.8581058582092,76.7667479860193,
85.9429421494968));
#176007=CARTESIAN_POINT('Ctrl Pts',(-20.8951238339364,78.4201817940811,
85.6071520765293));
#176008=CARTESIAN_POINT('Ctrl Pts',(-20.9136668209986,79.228273233321,85.3596464630248));
#176009=CARTESIAN_POINT('Ctrl Pts',(-20.9503565042217,80.7556820110671,
84.7245334042394));
#176010=CARTESIAN_POINT('Ctrl Pts',(-20.9680553081979,81.4738907755999,
84.3440054328353));
#176011=CARTESIAN_POINT('Ctrl Pts',(-21.0027004007613,82.7930115983596,
83.4790247872099));
#176012=CARTESIAN_POINT('Ctrl Pts',(-21.019713441587,83.3956378002191,83.0031263137548));
#176013=CARTESIAN_POINT('Ctrl Pts',(-21.0528120499888,84.4871179982778,
81.9730233894142));
#176014=CARTESIAN_POINT('Ctrl Pts',(-21.0687362238809,84.9777240174162,
81.4247491183197));
#176015=CARTESIAN_POINT('Ctrl Pts',(-21.0993279547773,85.814806856134,80.313435524131));
#176016=CARTESIAN_POINT('Ctrl Pts',(-21.1139020257325,86.1698360147959,
79.7596555846068));
#176017=CARTESIAN_POINT('Ctrl Pts',(-21.145109445782,86.8437470022363,78.5101369405165));
#176018=CARTESIAN_POINT('Ctrl Pts',(-21.1616176529458,87.1462750542629,
77.8083081998923));
#176019=CARTESIAN_POINT('Ctrl Pts',(-21.187548413683,87.5167704632658,76.6878974934662));
#176020=CARTESIAN_POINT('Ctrl Pts',(-21.1967602241767,87.6287006191586,
76.2856547671196));
#176021=CARTESIAN_POINT('Ctrl Pts',(-21.2250037279068,87.9125711093249,
75.03641198948));
#176022=CARTESIAN_POINT('Ctrl Pts',(-21.2436593958821,88.0198633178678,
74.1771537817256));
#176023=CARTESIAN_POINT('Ctrl Pts',(-21.2776117572916,88.0586334289964,
72.6270566305324));
#176024=CARTESIAN_POINT('Ctrl Pts',(-21.2927971039351,88.0215759479958,
71.9402125395721));
#176025=CARTESIAN_POINT('Ctrl Pts',(-21.3169667097406,87.875329475273,70.8455022641578));
#176026=CARTESIAN_POINT('Ctrl Pts',(-21.3260206594937,87.8001790700835,
70.4344102966169));
#176027=CARTESIAN_POINT('Ctrl Pts',(-21.3543309053144,87.5050793294366,
69.1673020077081));
#176028=CARTESIAN_POINT('Ctrl Pts',(-21.3737642612831,87.2178691754204,
68.329538119423));
#176029=CARTESIAN_POINT('Ctrl Pts',(-21.4119659520071,86.4879995764537,
66.7453317928356));
#176030=CARTESIAN_POINT('Ctrl Pts',(-21.4304732288375,86.0512599347866,
66.0009854150646));
#176031=CARTESIAN_POINT('Ctrl Pts',(-21.45877073841,85.2903319415476,64.9562540583632));
#176032=CARTESIAN_POINT('Ctrl Pts',(-21.4682633490694,85.0191071670509,
64.6202353673414));
#176033=CARTESIAN_POINT('Ctrl Pts',(-21.4870039107528,84.449790917879,63.982399851356));
#176034=CARTESIAN_POINT('Ctrl Pts',(-21.4961934348158,84.1526419610169,
63.6804350576366));
#176035=CARTESIAN_POINT('Ctrl Pts',(-21.5233547247884,83.2321115197238,
62.8318145792477));
#176036=CARTESIAN_POINT('Ctrl Pts',(-21.5414238145453,82.5707706179085,
62.329484825224));
#176037=CARTESIAN_POINT('Ctrl Pts',(-21.5785210670392,81.1333979409496,
61.4394720739356));
#176038=CARTESIAN_POINT('Ctrl Pts',(-21.597076175883,80.3573456562022,61.0594111100691));
#176039=CARTESIAN_POINT('Ctrl Pts',(-21.6250796896882,79.1531224230812,
60.6110914879113));
#176040=CARTESIAN_POINT('Ctrl Pts',(-21.6343447696767,78.7497996221477,
60.4828824650073));
#176041=CARTESIAN_POINT('Ctrl Pts',(-21.6625492020202,77.5076450230888,
60.153547569202));
#176042=CARTESIAN_POINT('Ctrl Pts',(-21.6811736407976,76.6544741846669,
60.0157351749384));
#176043=CARTESIAN_POINT('Ctrl Pts',(-21.7057297020164,75.528449936209,59.9468231966896));
#176044=CARTESIAN_POINT('Ctrl Pts',(-21.7115334678031,75.2626331470515,
59.9387052680259));
#176045=CARTESIAN_POINT('Ctrl Pts',(-21.7173525905574,74.9968912574536,
59.9387052680259));
#176046=CARTESIAN_POINT('Ctrl Pts',(-21.4178560137093,74.996891265676,59.9387052680259));
#176047=CARTESIAN_POINT('Ctrl Pts',(-21.41681366863,75.0442600341101,59.9387052680558));
#176048=CARTESIAN_POINT('Ctrl Pts',(-21.4157707615431,75.0916318668529,
59.9389632028205));
#176049=CARTESIAN_POINT('Ctrl Pts',(-21.3957577137173,76.0001586580206,
59.9488585939689));
#176050=CARTESIAN_POINT('Ctrl Pts',(-21.3765309548117,76.858270577439,60.0434684027457));
#176051=CARTESIAN_POINT('Ctrl Pts',(-21.3458801869731,78.2198977052432,
60.3318795149761));
#176052=CARTESIAN_POINT('Ctrl Pts',(-21.3342766158643,78.7318223000384,
60.4733979380445));
#176053=CARTESIAN_POINT('Ctrl Pts',(-21.3069126076966,79.905205400192,60.8762128117258));
#176054=CARTESIAN_POINT('Ctrl Pts',(-21.291086993832,80.5567698007339,61.1611528710284));
#176055=CARTESIAN_POINT('Ctrl Pts',(-21.2587222061821,81.844710534345,61.854465152685));
#176056=CARTESIAN_POINT('Ctrl Pts',(-21.2423307058054,82.4753959811991,
62.2679410595901));
#176057=CARTESIAN_POINT('Ctrl Pts',(-21.2066278909854,83.7443724506534,
63.266651874344));
#176058=CARTESIAN_POINT('Ctrl Pts',(-21.1874199767991,84.3673335228922,
63.8656602232681));
#176059=CARTESIAN_POINT('Ctrl Pts',(-21.1592772520458,85.1987432622261,
64.8408609746335));
#176060=CARTESIAN_POINT('Ctrl Pts',(-21.1500818761777,85.4552887949796,
65.1729407676574));
#176061=CARTESIAN_POINT('Ctrl Pts',(-21.1218145432478,86.1889436702785,
66.2235998285199));
#176062=CARTESIAN_POINT('Ctrl Pts',(-21.1025835347235,86.6112356261139,
66.9775770080341));
#176063=CARTESIAN_POINT('Ctrl Pts',(-21.0670621257983,87.2581623840701,
68.4597967379077));
#176064=CARTESIAN_POINT('Ctrl Pts',(-21.0505482640139,87.4995922590061,
69.176840533366));
#176065=CARTESIAN_POINT('Ctrl Pts',(-21.0245961035509,87.7758976962381,
70.3156719535861));
#176066=CARTESIAN_POINT('Ctrl Pts',(-21.0153375906866,87.8546928580724,
70.7250919862511));
#176067=CARTESIAN_POINT('Ctrl Pts',(-20.9879143247382,88.0307955637858,
71.9548059008335));
#176068=CARTESIAN_POINT('Ctrl Pts',(-20.9700045145971,88.0700073241251,
72.7812983205284));
#176069=CARTESIAN_POINT('Ctrl Pts',(-20.9327282218023,87.9899244881527,
74.4687021843473));
#176070=CARTESIAN_POINT('Ctrl Pts',(-20.9136153739934,87.8634149024849,
75.3252771702288));
#176071=CARTESIAN_POINT('Ctrl Pts',(-20.88548594242,87.5502408558111,76.5733917951643));
#176072=CARTESIAN_POINT('Ctrl Pts',(-20.8762371854095,87.4273830566958,
76.9784850315698));
#176073=CARTESIAN_POINT('Ctrl Pts',(-20.8507301847959,87.0372377676382,
78.0706669550707));
#176074=CARTESIAN_POINT('Ctrl Pts',(-20.8343758561155,86.7311001454912,
78.7422095494678));
#176075=CARTESIAN_POINT('Ctrl Pts',(-20.8065255442574,86.1070840304626,
79.8516360577577));
#176076=CARTESIAN_POINT('Ctrl Pts',(-20.7948767455376,85.8156806869038,
80.3023077829987));
#176077=CARTESIAN_POINT('Ctrl Pts',(-20.7666792793523,85.0516918165158,
81.337916593493));
#176078=CARTESIAN_POINT('Ctrl Pts',(-20.7500468352409,84.5546952456442,
81.9024698525982));
#176079=CARTESIAN_POINT('Ctrl Pts',(-20.7186048796733,83.5163516485031,
82.8947221405498));
#176080=CARTESIAN_POINT('Ctrl Pts',(-20.7037805924562,82.9842316261899,
83.3285119549456));
#176081=CARTESIAN_POINT('Ctrl Pts',(-20.6727459699732,81.8191585735813,
84.1344894493512));
#176082=CARTESIAN_POINT('Ctrl Pts',(-20.6565728896771,81.1839074716829,
84.4992085356232));
#176083=CARTESIAN_POINT('Ctrl Pts',(-20.6294708145913,80.0579524538981,
85.0254065546555));
#176084=CARTESIAN_POINT('Ctrl Pts',(-20.6183950189988,79.5821048388523,
85.2145723093971));
#176085=CARTESIAN_POINT('Ctrl Pts',(-20.5883413164331,78.2743649906955,
85.6473368864876));
#176086=CARTESIAN_POINT('Ctrl Pts',(-20.569210958263,77.4273096571947,85.8368703335035));
#176087=CARTESIAN_POINT('Ctrl Pts',(-20.5377080645285,75.9903290890004,
86.0111278513581));
#176088=CARTESIAN_POINT('Ctrl Pts',(-20.5251349688791,75.4088756721479,
86.0424631067098));
#176089=CARTESIAN_POINT('Ctrl Pts',(-20.4968563732491,74.1138237924929,
86.0256277651038));
#176090=CARTESIAN_POINT('Ctrl Pts',(-20.4811152915302,73.4023336282443,
85.9578503823963));
#176091=CARTESIAN_POINT('Ctrl Pts',(-20.4474752967114,71.8825012624425,
85.6860734269489));
#176092=CARTESIAN_POINT('Ctrl Pts',(-20.4295842421063,71.0808580967995,
85.4621922381434));
#176093=CARTESIAN_POINT('Ctrl Pts',(-20.4022763370671,69.9175317344837,
85.0140181389652));
#176094=CARTESIAN_POINT('Ctrl Pts',(-20.3931231801359,69.5365017488138,
84.8458821231825));
#176095=CARTESIAN_POINT('Ctrl Pts',(-20.3651767119189,68.3937867628417,
84.2748676877471));
#176096=CARTESIAN_POINT('Ctrl Pts',(-20.3466886326991,67.6634124563664,
83.8145901929087));
#176097=CARTESIAN_POINT('Ctrl Pts',(-20.3089705059557,66.3023363505552,
82.755536642036));
#176098=CARTESIAN_POINT('Ctrl Pts',(-20.2900276098555,65.675242593848,82.1590250083103));
#176099=CARTESIAN_POINT('Ctrl Pts',(-20.2620774778898,64.8342974085004,
81.1830559580949));
#176100=CARTESIAN_POINT('Ctrl Pts',(-20.252852986785,64.5728121536784,80.8477876691409));
#176101=CARTESIAN_POINT('Ctrl Pts',(-20.2287246937958,63.9370110683983,
79.9449272410045));
#176102=CARTESIAN_POINT('Ctrl Pts',(-20.2137340927338,63.589842662658,79.3597959535171));
#176103=CARTESIAN_POINT('Ctrl Pts',(-20.180104674203,62.908689691543,77.9760753281143));
#176104=CARTESIAN_POINT('Ctrl Pts',(-20.1614842839252,62.6053081244397,
77.1659456196048));
#176105=CARTESIAN_POINT('Ctrl Pts',(-20.1334055932045,62.2775686771867,
75.9299624077936));
#176106=CARTESIAN_POINT('Ctrl Pts',(-20.1242425797183,62.1902767982458,
75.5232436360709));
#176107=CARTESIAN_POINT('Ctrl Pts',(-20.0981978934479,61.9965793065736,
74.3501104304278));
#176108=CARTESIAN_POINT('Ctrl Pts',(-20.0815282551429,61.9386765950035,
73.5774782424547));
#176109=CARTESIAN_POINT('Ctrl Pts',(-20.050001059248,61.9588586865063,72.139145920468));
#176110=CARTESIAN_POINT('Ctrl Pts',(-20.0352810139129,62.0190389983518,
71.4756993029304));
#176111=CARTESIAN_POINT('Ctrl Pts',(-20.0016074559056,62.2747903613662,
69.9575120421242));
#176112=CARTESIAN_POINT('Ctrl Pts',(-19.9826750811475,62.5063387440246,
69.1120612509894));
#176113=CARTESIAN_POINT('Ctrl Pts',(-19.9542428259785,62.9701294617421,
67.9082770841441));
#176114=CARTESIAN_POINT('Ctrl Pts',(-19.9450489658567,63.1380126501298,
67.5277735283805));
#176115=CARTESIAN_POINT('Ctrl Pts',(-19.9193164912298,63.6613477631329,
66.4801808585826));
#176116=CARTESIAN_POINT('Ctrl Pts',(-19.9029642840316,64.0569679482172,
65.8350167335816));
#176117=CARTESIAN_POINT('Ctrl Pts',(-19.8718434284005,64.8982605894784,
64.6976236507171));
#176118=CARTESIAN_POINT('Ctrl Pts',(-19.8571985066566,65.32996246771,64.1980163306893));
#176119=CARTESIAN_POINT('Ctrl Pts',(-19.8245579560657,66.3838078226897,
63.1504171632873));
#176120=CARTESIAN_POINT('Ctrl Pts',(-19.8066007523067,67.0240990345888,
62.6246747936668));
#176121=CARTESIAN_POINT('Ctrl Pts',(-19.7744569492311,68.2306011504375,
61.8124398093872));
#176122=CARTESIAN_POINT('Ctrl Pts',(-19.7605100521488,68.7760217270058,
61.4998749157207));
#176123=CARTESIAN_POINT('Ctrl Pts',(-19.7361577734367,69.7761724614817,
61.0189111200789));
#176124=CARTESIAN_POINT('Ctrl Pts',(-19.7256297548061,70.2217660199513,
60.8342593997852));
#176125=CARTESIAN_POINT('Ctrl Pts',(-19.6989346662376,71.3661028564162,
60.4327279679045));
#176126=CARTESIAN_POINT('Ctrl Pts',(-19.6826650619117,72.0747597355435,
60.2491281214674));
#176127=CARTESIAN_POINT('Ctrl Pts',(-19.6502356237299,73.5223875407533,
60.0012997842663));
#176128=CARTESIAN_POINT('Ctrl Pts',(-19.634176490088,74.2589730558603,59.9387048093555));
#176129=CARTESIAN_POINT('Ctrl Pts',(-19.6178714446467,74.9968993681035,
59.9387052680284));
#176130=CARTESIAN_POINT('Origin',(-29.0675369414309,75.,72.98888938658));
#176131=CARTESIAN_POINT('',(-29.3659074908669,61.9518604038339,72.9107242579373));
#176132=CARTESIAN_POINT('',(-29.0715747727696,75.,60.2348484464093));
#176133=CARTESIAN_POINT('Ctrl Pts',(-29.3659074908668,61.951860403834,72.9107242579373));
#176134=CARTESIAN_POINT('Ctrl Pts',(-29.3546070927146,61.9679108610104,
72.1178290340207));
#176135=CARTESIAN_POINT('Ctrl Pts',(-29.3435513987406,62.0560537850465,
71.3272167571516));
#176136=CARTESIAN_POINT('Ctrl Pts',(-29.3198744527501,62.3845025016822,
69.7320276469564));
#176137=CARTESIAN_POINT('Ctrl Pts',(-29.3073471940742,62.631814685764,68.9317585168648));
#176138=CARTESIAN_POINT('Ctrl Pts',(-29.271600961411,63.5738929101862,66.6770808866654));
#176139=CARTESIAN_POINT('Ctrl Pts',(-29.2493251735019,64.4653657292663,
65.3168568073909));
#176140=CARTESIAN_POINT('Ctrl Pts',(-29.2008834203262,66.7259955316958,
62.9788091341843));
#176141=CARTESIAN_POINT('Ctrl Pts',(-29.1779340274077,68.0820978808835,
62.0244452185557));
#176142=CARTESIAN_POINT('Ctrl Pts',(-29.1412176792257,70.3529225888009,
61.0067126405035));
#176143=CARTESIAN_POINT('Ctrl Pts',(-29.1283139882168,71.161267589059,60.7373079796422));
#176144=CARTESIAN_POINT('Ctrl Pts',(-29.1035475953523,72.7936407465736,
60.3677278885743));
#176145=CARTESIAN_POINT('Ctrl Pts',(-29.0916996520816,73.614095259019,60.2633970793433));
#176146=CARTESIAN_POINT('Ctrl Pts',(-29.077037613407,74.6255543768367,60.2335039391159));
#176147=CARTESIAN_POINT('Ctrl Pts',(-29.0743156629422,74.8128642429899,
60.2321075556721));
#176148=CARTESIAN_POINT('Ctrl Pts',(-29.0715747727696,75.,60.2348484464093));
#176149=CARTESIAN_POINT('',(-29.5675339851921,75.,59.7388891318012));
#176150=CARTESIAN_POINT('',(-29.0675369414309,75.,60.23888627858));
#176151=CARTESIAN_POINT('Origin',(-29.5675339847409,75.,72.98888938658));
#176152=CARTESIAN_POINT('Ctrl Pts',(-29.0715747727696,75.,60.2348484464093));
#176153=CARTESIAN_POINT('Ctrl Pts',(-29.0624830013438,75.6207456049797,
60.2439402197083));
#176154=CARTESIAN_POINT('Ctrl Pts',(-29.0530879239043,76.2395732334621,
60.2986134781171));
#176155=CARTESIAN_POINT('Ctrl Pts',(-29.0196088358868,78.4291737250614,
60.654585606508));
#176156=CARTESIAN_POINT('Ctrl Pts',(-28.997054407396,79.9505617589687,61.2063873465342));
#176157=CARTESIAN_POINT('Ctrl Pts',(-28.9605640939282,82.031973030273,62.4497133388104));
#176158=CARTESIAN_POINT('Ctrl Pts',(-28.9479315721182,82.6958287686398,
62.9401165234336));
#176159=CARTESIAN_POINT('Ctrl Pts',(-28.9236753448959,83.9002169768209,
64.0256989171434));
#176160=CARTESIAN_POINT('Ctrl Pts',(-28.9120635621438,84.4420480810486,
64.6158534954276));
#176161=CARTESIAN_POINT('Ctrl Pts',(-28.8757570605852,85.9290861966703,
66.5825031306264));
#176162=CARTESIAN_POINT('Ctrl Pts',(-28.849912430552,86.6557590389786,68.0941753323764));
#176163=CARTESIAN_POINT('Ctrl Pts',(-28.8133913070783,87.2699061763046,
70.4880258729443));
#176164=CARTESIAN_POINT('Ctrl Pts',(-28.8014073382066,87.3946594029363,
71.2917639572309));
#176165=CARTESIAN_POINT('Ctrl Pts',(-28.7766246431267,87.4843571247555,
72.9010220159898));
#176166=CARTESIAN_POINT('Ctrl Pts',(-28.7642803679124,87.4519621690978,
73.7016986292209));
#176167=CARTESIAN_POINT('Ctrl Pts',(-28.7402659878291,87.2354224393507,
75.2800816266037));
#176168=CARTESIAN_POINT('Ctrl Pts',(-28.7286237203282,87.052444662765,76.0555728901073));
#176169=CARTESIAN_POINT('Ctrl Pts',(-28.6920185593489,86.2697007508172,
78.3547530241982));
#176170=CARTESIAN_POINT('Ctrl Pts',(-28.6664353682694,85.4407395791364,
79.7818999882862));
#176171=CARTESIAN_POINT('Ctrl Pts',(-28.6175016536567,83.2796947023339,
82.2305946258017));
#176172=CARTESIAN_POINT('Ctrl Pts',(-28.5917552851528,81.9706263726822,
83.2219482748408));
#176173=CARTESIAN_POINT('Ctrl Pts',(-28.5670511147326,80.5057179591556,
83.9313635516325));
#176174=CARTESIAN_POINT('',(-29.3655838523951,68.398637325302,84.2438270474906));
#176175=CARTESIAN_POINT('Ctrl Pts',(-29.3655838526627,68.3986373254374,
84.2438270472598));
#176176=CARTESIAN_POINT('Ctrl Pts',(-29.3515369276677,68.1394510957219,
84.0755215996163));
#176177=CARTESIAN_POINT('Ctrl Pts',(-29.3375494753959,67.8866810149154,
83.8983413632411));
#176178=CARTESIAN_POINT('Ctrl Pts',(-29.3235615282545,67.6409397655344,
83.7127408512439));
#176179=CARTESIAN_POINT('Ctrl Pts',(-29.3096896422788,67.3972374869589,
83.5286803087323));
#176180=CARTESIAN_POINT('Ctrl Pts',(-29.2958172696114,67.1604481100554,
83.3363387224561));
#176181=CARTESIAN_POINT('Ctrl Pts',(-29.2818859230026,66.9311451205241,
83.136204656219));
#176182=CARTESIAN_POINT('Ctrl Pts',(-29.2769072652868,66.8491989074151,
83.0646825671448));
#176183=CARTESIAN_POINT('Ctrl Pts',(-29.2719210757759,66.7682085691129,
82.9921656866276));
#176184=CARTESIAN_POINT('Ctrl Pts',(-29.2669246850387,66.6881994399432,
82.9186776996054));
#176185=CARTESIAN_POINT('Ctrl Pts',(-29.253192592924,66.4683021601713,82.7167031423293));
#176186=CARTESIAN_POINT('Ctrl Pts',(-29.2393423955425,66.2558213412074,
82.5073393284892));
#176187=CARTESIAN_POINT('Ctrl Pts',(-29.2254372276085,66.0511772646013,
82.2911763378466));
#176188=CARTESIAN_POINT('Ctrl Pts',(-29.2113899558857,65.8444418289547,
82.0728042706834));
#176189=CARTESIAN_POINT('Ctrl Pts',(-29.1972865843269,65.6457041683321,
81.8474936242022));
#176190=CARTESIAN_POINT('Ctrl Pts',(-29.1831922031098,65.4553465105166,
81.6158677489117));
#176191=CARTESIAN_POINT('Ctrl Pts',(-29.1776338924618,65.3802763829204,
81.5245229392928));
#176192=CARTESIAN_POINT('Ctrl Pts',(-29.1720769800155,65.3065089777228,
81.4321961088971));
#176193=CARTESIAN_POINT('Ctrl Pts',(-29.1665254579116,65.2340655732272,
81.3389259770428));
#176194=CARTESIAN_POINT('Ctrl Pts',(-29.1526002959194,65.0523521396864,
81.1049718162177));
#176195=CARTESIAN_POINT('Ctrl Pts',(-29.1387540387589,64.8789555202937,
80.8651301507343));
#176196=CARTESIAN_POINT('Ctrl Pts',(-29.1249636357171,64.7142624726138,
80.620000836512));
#176197=CARTESIAN_POINT('Ctrl Pts',(-29.1112138923694,64.550055006748,80.3755942627985));
#176198=CARTESIAN_POINT('Ctrl Pts',(-29.0975196742648,64.3945000183605,
80.1259313935898));
#176199=CARTESIAN_POINT('Ctrl Pts',(-29.0838581339783,64.2479378038455,
79.8716355509124));
#176200=CARTESIAN_POINT('Ctrl Pts',(-29.0702192763373,64.1016189307598,
79.6177619228831));
#176201=CARTESIAN_POINT('Ctrl Pts',(-29.0566129880926,63.9642631393004,
79.3592709194713));
#176202=CARTESIAN_POINT('Ctrl Pts',(-29.0430165354331,63.8361638164801,
79.0968081432358));
#176203=CARTESIAN_POINT('Ctrl Pts',(-29.0294524529147,63.7083694697629,
78.8349702327134));
#176204=CARTESIAN_POINT('Ctrl Pts',(-29.0158981592045,63.5897876890377,
78.5691796794683));
#176205=CARTESIAN_POINT('Ctrl Pts',(-29.0023310824776,63.4806627565782,
78.3000992657792));
#176206=CARTESIAN_POINT('Ctrl Pts',(-28.9909220184838,63.3888955054007,
78.0738194472864));
#176207=CARTESIAN_POINT('Ctrl Pts',(-28.9795039146484,63.3038151339953,
77.8452135701696));
#176208=CARTESIAN_POINT('Ctrl Pts',(-28.968063347715,63.2255401942507,77.6146858321683));
#176209=CARTESIAN_POINT('Ctrl Pts',(-28.9545124222423,63.1328264431715,
77.3416343116226));
#176210=CARTESIAN_POINT('Ctrl Pts',(-28.9408729669519,63.0496843738629,
77.0657889256946));
#176211=CARTESIAN_POINT('Ctrl Pts',(-28.927181688329,62.9762246025752,76.7878423327904));
#176212=CARTESIAN_POINT('Ctrl Pts',(-28.9133962221623,62.9022594734155,
76.5079836389326));
#176213=CARTESIAN_POINT('Ctrl Pts',(-28.8995582171853,62.8381102929787,
76.2259950093747));
#176214=CARTESIAN_POINT('Ctrl Pts',(-28.8857051426603,62.7838370734446,
75.9425807157959));
#176215=CARTESIAN_POINT('Ctrl Pts',(-28.8717987806007,62.7293550853761,
75.6580762346949));
#176216=CARTESIAN_POINT('Ctrl Pts',(-28.8578772328365,62.6848251069248,
75.3721353741));
#176217=CARTESIAN_POINT('Ctrl Pts',(-28.8439784026856,62.6502555083076,
75.0854635881187));
#176218=CARTESIAN_POINT('Ctrl Pts',(-28.8299871301315,62.6154559840967,
74.7968851216078));
#176219=CARTESIAN_POINT('Ctrl Pts',(-28.8160188783894,62.5907496985111,
74.507566246316));
#176220=CARTESIAN_POINT('Ctrl Pts',(-28.8021123121141,62.5760933692594,
74.2182154033664));
#176221=CARTESIAN_POINT('Ctrl Pts',(-28.7906519385058,62.5640151174734,
73.9797619491884));
#176222=CARTESIAN_POINT('Ctrl Pts',(-28.779233457813,62.5587611821413,73.7412866412681));
#176223=CARTESIAN_POINT('Ctrl Pts',(-28.7678785097109,62.5602818434642,
73.5031784169355));
#176224=CARTESIAN_POINT('Ctrl Pts',(-28.7538051587481,62.5621665548957,
73.2080664905723));
#176225=CARTESIAN_POINT('Ctrl Pts',(-28.7397945616724,62.574495885705,72.9135590415678));
#176226=CARTESIAN_POINT('Ctrl Pts',(-28.7257924240596,62.5972144711822,
72.6203915837616));
#176227=CARTESIAN_POINT('Ctrl Pts',(-28.7118903162118,62.6197707575284,
72.3293184827403));
#176228=CARTESIAN_POINT('Ctrl Pts',(-28.6979965473916,62.6525684315748,
72.039566545924));
#176229=CARTESIAN_POINT('Ctrl Pts',(-28.6840579785024,62.6955019826906,
71.7518582558115));
#176230=CARTESIAN_POINT('Ctrl Pts',(-28.6791171162738,62.7107208163266,
71.6498731069214));
#176231=CARTESIAN_POINT('Ctrl Pts',(-28.6741706248306,62.7272127669116,
71.5481447522842));
#176232=CARTESIAN_POINT('Ctrl Pts',(-28.6692161373386,62.744971557244,71.446705358476));
#176233=CARTESIAN_POINT('Ctrl Pts',(-28.6547265382075,62.7969078581004,
71.1500417469971));
#176234=CARTESIAN_POINT('Ctrl Pts',(-28.6401112616264,62.8597417243038,
70.8558425314139));
#176235=CARTESIAN_POINT('Ctrl Pts',(-28.6253112490716,62.9332865719164,
70.5648824322531));
#176236=CARTESIAN_POINT('Ctrl Pts',(-28.6106590834907,63.0060967321,70.2768289232089));
#176237=CARTESIAN_POINT('Ctrl Pts',(-28.5958258543968,63.0894049728235,
69.9919503385894));
#176238=CARTESIAN_POINT('Ctrl Pts',(-28.5807542555663,63.1829792308997,
69.7109948177064));
#176239=CARTESIAN_POINT('Ctrl Pts',(-28.5763682341958,63.2102104954961,
69.6292332917668));
#176240=CARTESIAN_POINT('Ctrl Pts',(-28.5719620257246,63.2383108366438,
69.5478039687374));
#176241=CARTESIAN_POINT('Ctrl Pts',(-28.5675342178229,63.2672737070204,
69.46672519));
#176242=CARTESIAN_POINT('',(-29.3666998404582,61.9513562005121,72.9886184577035));
#176243=CARTESIAN_POINT('Ctrl Pts',(-29.3655838529308,68.398637325302,84.2438270474913));
#176244=CARTESIAN_POINT('Ctrl Pts',(-29.3663355387957,67.4434486808997,
83.6844513479272));
#176245=CARTESIAN_POINT('Ctrl Pts',(-29.3681108351944,66.5594392044141,
83.0049447002618));
#176246=CARTESIAN_POINT('Ctrl Pts',(-29.3658391655718,64.9568327293927,
81.398488742438));
#176247=CARTESIAN_POINT('Ctrl Pts',(-29.3646108212369,64.2514758328537,
80.473804649592));
#176248=CARTESIAN_POINT('Ctrl Pts',(-29.3665216258898,63.1238041156622,
78.508904879264));
#176249=CARTESIAN_POINT('Ctrl Pts',(-29.3680011405059,62.6942531079225,
77.4766733383823));
#176250=CARTESIAN_POINT('Ctrl Pts',(-29.3656365873995,62.1043691345675,
75.2854002296065));
#176251=CARTESIAN_POINT('Ctrl Pts',(-29.3647732455976,61.9527377954335,
74.1368535505302));
#176252=CARTESIAN_POINT('Ctrl Pts',(-29.3658340844142,61.9516996901141,
72.9886310426174));
#176253=CARTESIAN_POINT('Ctrl Pts',(-29.3673261860752,61.9511076972435,
72.988609352938));
#176254=CARTESIAN_POINT('Ctrl Pts',(-29.3668532876725,61.9512817219048,
72.9626462799096));
#176255=CARTESIAN_POINT('Ctrl Pts',(-29.3663803892696,61.9515326191958,
72.9366844270784));
#176256=CARTESIAN_POINT('Ctrl Pts',(-29.3659074908668,61.951860403834,72.9107242579373));
#176257=CARTESIAN_POINT('Origin',(-28.5675364832709,75.,72.98888938658));
#176258=CARTESIAN_POINT('',(-27.5675364826718,89.5000000000001,66.2250147575798));
#176259=CARTESIAN_POINT('',(-27.56753648264,89.5,79.7527640156553));
#176260=CARTESIAN_POINT('Ctrl Pts',(-27.5675364817657,89.5,66.2250147580311));
#176261=CARTESIAN_POINT('Ctrl Pts',(-30.4269114864224,89.5,72.9888893867033));
#176262=CARTESIAN_POINT('Ctrl Pts',(-27.5675364816388,89.5,79.7527640154292));
#176263=CARTESIAN_POINT('',(-27.5675364826398,88.1076872567925,63.8134583462434));
#176264=CARTESIAN_POINT('Origin',(-27.5675364832709,75.,72.98888938658));
#176265=CARTESIAN_POINT('',(-27.5675364826717,76.3923127432732,57.0495837172059));
#176266=CARTESIAN_POINT('Ctrl Pts',(-27.5675364817724,76.3923127436787,
57.0495837174391));
#176267=CARTESIAN_POINT('Ctrl Pts',(-30.4269114864031,82.2500000000807,
60.4315210317516));
#176268=CARTESIAN_POINT('Ctrl Pts',(-27.567536481677,88.1076872565176,63.8134583460843));
#176269=CARTESIAN_POINT('',(-27.5675364826717,73.6076872567269,57.0495837172059));
#176270=CARTESIAN_POINT('Origin',(-27.5675364832709,75.,72.98888938658));
#176271=CARTESIAN_POINT('',(-27.5675364826398,61.8923127432075,63.8134583462433));
#176272=CARTESIAN_POINT('Ctrl Pts',(-27.567536481677,61.8923127434824,63.8134583460842));
#176273=CARTESIAN_POINT('Ctrl Pts',(-30.426911486403,67.7499999999193,60.4315210317516));
#176274=CARTESIAN_POINT('Ctrl Pts',(-27.5675364817723,73.6076872563213,
57.0495837174391));
#176275=CARTESIAN_POINT('',(-27.5675364826718,60.5,66.2250147575798));
#176276=CARTESIAN_POINT('Origin',(-27.5675364832709,75.,72.98888938658));
#176277=CARTESIAN_POINT('',(-27.5675364826718,60.5,79.7527640155803));
#176278=CARTESIAN_POINT('Ctrl Pts',(-27.5675364817658,60.5,66.2250147580311));
#176279=CARTESIAN_POINT('Ctrl Pts',(-30.4269114864094,60.5,72.9888893866725));
#176280=CARTESIAN_POINT('Ctrl Pts',(-27.5675364816705,60.5,79.7527640153542));
#176281=CARTESIAN_POINT('',(-27.5675364826398,61.8923127432075,82.1643204269167));
#176282=CARTESIAN_POINT('Origin',(-27.5675364832709,75.,72.98888938658));
#176283=CARTESIAN_POINT('',(-27.5675364826717,73.6076872567269,88.9281950559541));
#176284=CARTESIAN_POINT('Ctrl Pts',(-27.5675364817723,73.6076872563214,
88.9281950557209));
#176285=CARTESIAN_POINT('Ctrl Pts',(-30.4269114864031,67.7499999999193,
85.5462577414084));
#176286=CARTESIAN_POINT('Ctrl Pts',(-27.567536481677,61.8923127434824,82.1643204270758));
#176287=CARTESIAN_POINT('',(-27.5675364816388,75.,88.9888893864172));
#176288=CARTESIAN_POINT('Origin',(-27.5675364832709,75.,72.98888938658));
#176289=CARTESIAN_POINT('',(-29.5675364841684,75.,86.9888893874774));
#176290=CARTESIAN_POINT('',(-28.5675364832709,75.,87.98888938658));
#176291=CARTESIAN_POINT('Origin',(-29.5675364832709,75.,72.98888938658));
#176292=CARTESIAN_POINT('',(-27.5675364826399,76.3923127432082,88.9281950559916));
#176293=CARTESIAN_POINT('Origin',(-27.5675364832709,75.,72.98888938658));
#176294=CARTESIAN_POINT('',(-27.5675364826716,88.1076872567275,82.1643204269542));
#176295=CARTESIAN_POINT('Ctrl Pts',(-27.5675364817722,88.1076872563225,
82.1643204271884));
#176296=CARTESIAN_POINT('Ctrl Pts',(-30.426911486403,82.2499999999205,85.5462577415009));
#176297=CARTESIAN_POINT('Ctrl Pts',(-27.5675364816771,76.3923127434836,
88.9281950558335));
#176298=CARTESIAN_POINT('Origin',(-27.5675364832709,75.,72.98888938658));
#176299=CARTESIAN_POINT('Origin',(-17.5675364832709,75.,72.98888938658));
#176300=CARTESIAN_POINT('',(-18.5675364839018,89.5,66.2250147575047));
#176301=CARTESIAN_POINT('',(-18.56753648387,89.5,79.7527640155803));
#176302=CARTESIAN_POINT('Ctrl Pts',(-18.5675364848006,89.5,79.7527640151869));
#176303=CARTESIAN_POINT('Ctrl Pts',(-15.7081614801611,89.5,72.9888893866029));
#176304=CARTESIAN_POINT('Ctrl Pts',(-18.567536484777,89.5,66.2250147580289));
#176305=CARTESIAN_POINT('',(-18.5675364838598,88.1076872567062,82.1643204269666));
#176306=CARTESIAN_POINT('Origin',(-18.5675364832709,75.,72.98888938658));
#176307=CARTESIAN_POINT('',(-18.567536483878,76.3923127432567,88.9281950559637));
#176308=CARTESIAN_POINT('Ctrl Pts',(-18.5675364847385,88.1076872562589,
82.1643204272251));
#176309=CARTESIAN_POINT('Ctrl Pts',(-15.7081614801807,82.2499999999541,
85.5462577414815));
#176310=CARTESIAN_POINT('Ctrl Pts',(-18.5675364847937,76.3923127436291,
88.9281950557496));
#176311=CARTESIAN_POINT('',(-18.567536483878,73.6076872567433,88.9281950559637));
#176312=CARTESIAN_POINT('Origin',(-18.5675364832709,75.,72.98888938658));
#176313=CARTESIAN_POINT('',(-18.5675364838598,61.8923127432938,82.1643204269665));
#176314=CARTESIAN_POINT('Ctrl Pts',(-18.5675364847937,73.607687256371,88.9281950557496));
#176315=CARTESIAN_POINT('Ctrl Pts',(-15.7081614801806,67.750000000046,85.5462577414815));
#176316=CARTESIAN_POINT('Ctrl Pts',(-18.5675364847385,61.8923127437411,
82.1643204272251));
#176317=CARTESIAN_POINT('',(-18.56753648387,60.5,79.7527640155802));
#176318=CARTESIAN_POINT('Origin',(-18.5675364832709,75.,72.98888938658));
#176319=CARTESIAN_POINT('',(-18.5675364839017,60.5,66.2250147575048));
#176320=CARTESIAN_POINT('Ctrl Pts',(-18.5675364848005,60.5,79.7527640151869));
#176321=CARTESIAN_POINT('Ctrl Pts',(-15.7081614801611,60.5,72.9888893866029));
#176322=CARTESIAN_POINT('Ctrl Pts',(-18.5675364847769,60.5,66.225014758029));
#176323=CARTESIAN_POINT('',(-18.5675364838598,61.8923127432938,63.8134583461934));
#176324=CARTESIAN_POINT('Origin',(-18.5675364832709,75.,72.98888938658));
#176325=CARTESIAN_POINT('',(-18.5675364838782,73.6076872567434,57.0495837171963));
#176326=CARTESIAN_POINT('Ctrl Pts',(-18.5675364847385,61.8923127437411,
63.8134583459349));
#176327=CARTESIAN_POINT('Ctrl Pts',(-15.7081614801806,67.750000000046,60.4315210316784));
#176328=CARTESIAN_POINT('Ctrl Pts',(-18.5675364847938,73.6076872563712,
57.0495837174103));
#176329=CARTESIAN_POINT('',(-18.5675364848006,75.,56.9888893868452));
#176330=CARTESIAN_POINT('Origin',(-18.5675364832709,75.,72.98888938658));
#176331=CARTESIAN_POINT('',(-16.5675364823734,75.,58.9888893856825));
#176332=CARTESIAN_POINT('',(-17.5675364832709,75.,57.98888938658));
#176333=CARTESIAN_POINT('Origin',(-16.5675364832709,75.,72.98888938658));
#176334=CARTESIAN_POINT('',(-18.5675364838598,76.3923127432944,57.0495837172181));
#176335=CARTESIAN_POINT('Origin',(-18.5675364832709,75.,72.98888938658));
#176336=CARTESIAN_POINT('',(-18.5675364838783,88.107687256744,63.8134583462153));
#176337=CARTESIAN_POINT('Ctrl Pts',(-18.5675364847385,76.3923127437421,
57.0495837174757));
#176338=CARTESIAN_POINT('Ctrl Pts',(-15.7081614801806,82.2500000000471,
60.4315210317322));
#176339=CARTESIAN_POINT('Ctrl Pts',(-18.5675364847939,88.1076872563724,
63.8134583460004));
#176340=CARTESIAN_POINT('Origin',(-18.5675364832709,75.,72.98888938658));
#176341=CARTESIAN_POINT('Origin',(-31.5405364832709,75.,72.98888938658));
#176342=CARTESIAN_POINT('',(-27.5675364832709,76.39231274307,57.04958371709));
#176343=CARTESIAN_POINT('',(-27.5675364832709,73.60768725693,57.04958371709));
#176344=CARTESIAN_POINT('Origin',(-16.5675364832709,75.,89.73204719308));
#176345=CARTESIAN_POINT('',(-27.5675364832709,76.39231274307,88.92819505607));
#176346=CARTESIAN_POINT('',(-27.5675364832709,88.10768725693,82.164320426837));
#176347=CARTESIAN_POINT('Origin',(-16.5675364832709,75.,56.24573158008));
#176348=CARTESIAN_POINT('',(-27.5675364832709,61.89231274307,63.813458346323));
#176349=CARTESIAN_POINT('Origin',(-16.5675364832709,89.5,64.61731048333));
#176350=CARTESIAN_POINT('',(-27.5675364832709,88.10768725693,63.813458346323));
#176351=CARTESIAN_POINT('Origin',(-31.5405364832709,75.,72.98888938658));
#176352=CARTESIAN_POINT('',(-27.5675364832709,60.5,66.225014757346));
#176353=CARTESIAN_POINT('Origin',(-31.5405364832709,75.,72.98888938658));
#176354=CARTESIAN_POINT('',(-27.5675364832709,89.5,66.225014757346));
#176355=CARTESIAN_POINT('Origin',(-16.5675364832709,89.5,81.36046828983));
#176356=CARTESIAN_POINT('',(-27.5675364832709,89.5,79.752764015814));
#176357=CARTESIAN_POINT('Origin',(-16.5675364832709,60.5,81.36046828983));
#176358=CARTESIAN_POINT('',(-27.5675364832709,61.89231274307,82.164320426837));
#176359=CARTESIAN_POINT('',(-27.5675364832709,73.60768725693,88.92819505607));
#176360=CARTESIAN_POINT('Origin',(-31.5405364832709,75.,72.98888938658));
#176361=CARTESIAN_POINT('Origin',(-31.5405364832709,75.,72.98888938658));
#176362=CARTESIAN_POINT('',(-27.5675364832709,60.5,79.752764015814));
#176363=CARTESIAN_POINT('Origin',(-31.5405364832709,75.,72.98888938658));
#176364=CARTESIAN_POINT('Origin',(-16.5675364832709,60.5,64.61731048333));
#176365=CARTESIAN_POINT('Origin',(-29.5675364832709,75.,72.98888938658));
#176366=CARTESIAN_POINT('Ctrl Pts',(-29.4235335827009,62.44414915689,76.731819067654));
#176367=CARTESIAN_POINT('Ctrl Pts',(-29.3785752787509,61.85675590838,74.761378091484));
#176368=CARTESIAN_POINT('Ctrl Pts',(-29.2886586708509,61.6274868926,70.540717962258));
#176369=CARTESIAN_POINT('Ctrl Pts',(-29.1537837590009,64.19287556944,64.740945094149));
#176370=CARTESIAN_POINT('Ctrl Pts',(-29.0189088471409,69.10991196088,60.73624495104));
#176371=CARTESIAN_POINT('Ctrl Pts',(-28.8840339352909,75.308544783193,59.3974994093));
#176372=CARTESIAN_POINT('Ctrl Pts',(-28.7491590234309,81.440049640839,61.01614190121));
#176373=CARTESIAN_POINT('Ctrl Pts',(-28.6142841115809,86.17025756511,65.239934789744));
#176374=CARTESIAN_POINT('Ctrl Pts',(-28.4794091997309,88.46992237593,71.14982987547));
#176375=CARTESIAN_POINT('Ctrl Pts',(-28.3445342878709,87.8386577141,77.459886586808));
#176376=CARTESIAN_POINT('Ctrl Pts',(-28.2096593760209,84.413821081764,82.797096210383));
#176377=CARTESIAN_POINT('Ctrl Pts',(-28.0747844641709,78.940624888933,86.00013159165));
#176378=CARTESIAN_POINT('Ctrl Pts',(-27.9399095523109,72.609985526153,86.37204219574));
#176379=CARTESIAN_POINT('Ctrl Pts',(-27.8050346404609,66.799390990941,83.83190373521));
#176380=CARTESIAN_POINT('Ctrl Pts',(-27.6701597286009,62.77317238826,78.932426619492));
#176381=CARTESIAN_POINT('Ctrl Pts',(-27.5352848167509,61.40739728363,72.7396913102611));
#176382=CARTESIAN_POINT('Ctrl Pts',(-27.4004099049009,62.99924558451,66.601179175152));
#176383=CARTESIAN_POINT('Ctrl Pts',(-27.2655349930409,67.202345967366,61.8525731252));
#176384=CARTESIAN_POINT('Ctrl Pts',(-27.1306600811909,73.102143042981,59.52712548816));
#176385=CARTESIAN_POINT('Ctrl Pts',(-26.9957851693409,79.414896067747,60.13083195176));
#176386=CARTESIAN_POINT('Ctrl Pts',(-26.8609102574809,84.767008940321,63.532331627755));
#176387=CARTESIAN_POINT('Ctrl Pts',(-26.7260353456309,87.99391188448,68.991489954176));
#176388=CARTESIAN_POINT('Ctrl Pts',(-26.5911604337809,88.39346095746,75.320445064586));
#176389=CARTESIAN_POINT('Ctrl Pts',(-26.4562855219229,85.87871800947,81.142075432836));
#176390=CARTESIAN_POINT('Ctrl Pts',(-26.3214106100699,80.996867631233,85.18964866916));
#176391=CARTESIAN_POINT('Ctrl Pts',(-26.1865356982159,74.8101548300925,
86.58245060783));
#176392=CARTESIAN_POINT('Ctrl Pts',(-26.0516607863629,68.66475068801,85.01742067074));
#176393=CARTESIAN_POINT('Ctrl Pts',(-25.9167858745089,63.89783716987,80.835094323236));
#176394=CARTESIAN_POINT('Ctrl Pts',(-25.7819109626559,61.54665231168,74.945508333151));
#176395=CARTESIAN_POINT('Ctrl Pts',(-25.6470360508029,62.12278386605,68.630175581195));
#176396=CARTESIAN_POINT('Ctrl Pts',(-25.5121611389499,65.500901269506,63.263275982751));
#176397=CARTESIAN_POINT('Ctrl Pts',(-25.3772862270959,70.945844710137,60.01251283554));
#176398=CARTESIAN_POINT('Ctrl Pts',(-25.2424113152429,77.273267122096,59.58553507798));
#176399=CARTESIAN_POINT('Ctrl Pts',(-25.1524947073409,81.160959972294,61.24456506882));
#176400=CARTESIAN_POINT('Ctrl Pts',(-25.1075364033899,82.811656888157,62.4704803028));
#176401=CARTESIAN_POINT('Ctrl Pts',(-29.5803515522709,62.73283940876,76.645759801271));
#176402=CARTESIAN_POINT('Ctrl Pts',(-29.5353932483209,62.15895179256,74.720624165918));
#176403=CARTESIAN_POINT('Ctrl Pts',(-29.4454766404109,61.93495424192,70.597007514748));
#176404=CARTESIAN_POINT('Ctrl Pts',(-29.3106017285609,64.44135824997,64.930585855648));
#176405=CARTESIAN_POINT('Ctrl Pts',(-29.1757268167109,69.245339740392,61.01796373317));
#176406=CARTESIAN_POINT('Ctrl Pts',(-29.0408519048509,75.301450570921,59.70999928245));
#176407=CARTESIAN_POINT('Ctrl Pts',(-28.9059769930009,81.291976875715,61.29142515603));
#176408=CARTESIAN_POINT('Ctrl Pts',(-28.7711020811409,85.91342555028,65.418102536579));
#176409=CARTESIAN_POINT('Ctrl Pts',(-28.6362271692909,88.16021534517,71.192114429511));
#176410=CARTESIAN_POINT('Ctrl Pts',(-28.5013522574409,87.5434650286,77.357087236615));
#176411=CARTESIAN_POINT('Ctrl Pts',(-28.3664773455809,84.197373911983,82.571581131104));
#176412=CARTESIAN_POINT('Ctrl Pts',(-28.2316024337309,78.850020117821,85.70097075929));
#176413=CARTESIAN_POINT('Ctrl Pts',(-28.0967275218809,72.664937905644,86.06433021321));
#176414=CARTESIAN_POINT('Ctrl Pts',(-27.9618526100209,66.987943396495,83.58259585616));
#176415=CARTESIAN_POINT('Ctrl Pts',(-27.8269776981709,63.05429757737,78.795769910022));
#176416=CARTESIAN_POINT('Ctrl Pts',(-27.6921027863109,61.71992504067,72.7454209940753));
#176417=CARTESIAN_POINT('Ctrl Pts',(-27.5572278744609,63.27517278834,66.748048526563));
#176418=CARTESIAN_POINT('Ctrl Pts',(-27.4223529626109,67.381633435404,62.108624745));
#176419=CARTESIAN_POINT('Ctrl Pts',(-27.2874780507509,73.145779496604,59.83664493523));
#176420=CARTESIAN_POINT('Ctrl Pts',(-27.1526031389009,79.31338662218,60.42647068511));
#176421=CARTESIAN_POINT('Ctrl Pts',(-27.0177282270509,84.542441102891,63.749761420078));
#176422=CARTESIAN_POINT('Ctrl Pts',(-26.8828533151909,87.69514951931,69.083400113308));
#176423=CARTESIAN_POINT('Ctrl Pts',(-26.7479784033409,88.08551196495,75.266836798267));
#176424=CARTESIAN_POINT('Ctrl Pts',(-26.6131034914909,85.62858921442,80.954613399192));
#176425=CARTESIAN_POINT('Ctrl Pts',(-26.4782285796339,80.858984723211,84.90912285579));
#176426=CARTESIAN_POINT('Ctrl Pts',(-26.3433536677799,74.8145198429094,
86.26990081237));
#176427=CARTESIAN_POINT('Ctrl Pts',(-26.2084787559269,68.810413832813,84.74085480758));
#176428=CARTESIAN_POINT('Ctrl Pts',(-26.0736038440729,64.15310351731,80.654690549114));
#176429=CARTESIAN_POINT('Ctrl Pts',(-25.9387289322199,61.85597824913,74.900520795182));
#176430=CARTESIAN_POINT('Ctrl Pts',(-25.8038540203669,62.41886310557,68.730393256763));
#176431=CARTESIAN_POINT('Ctrl Pts',(-25.6689791085129,65.719309184614,63.486892033801));
#176432=CARTESIAN_POINT('Ctrl Pts',(-25.5341041966599,71.039059827646,60.31087201977));
#176433=CARTESIAN_POINT('Ctrl Pts',(-25.3992292848069,77.220999054703,59.89371154324));
#176434=CARTESIAN_POINT('Ctrl Pts',(-25.3093126769049,81.019304173067,61.51459630666));
#176435=CARTESIAN_POINT('Ctrl Pts',(-25.2643543729539,82.632047459634,62.71232469914));
#176436=CARTESIAN_POINT('Ctrl Pts',(-29.7371695218309,63.02152966063,76.559700534901));
#176437=CARTESIAN_POINT('Ctrl Pts',(-29.6922112178809,62.46114767674,74.679870240367));
#176438=CARTESIAN_POINT('Ctrl Pts',(-29.6022946099809,62.24242159123,70.653297067253));
#176439=CARTESIAN_POINT('Ctrl Pts',(-29.4674196981209,64.68984093049,65.120226617163));
#176440=CARTESIAN_POINT('Ctrl Pts',(-29.3325447862709,69.380767519885,61.29968251531));
#176441=CARTESIAN_POINT('Ctrl Pts',(-29.1976698744209,75.2943563586239,
60.02249915561));
#176442=CARTESIAN_POINT('Ctrl Pts',(-29.0627949625609,81.143904110566,61.56670841083));
#176443=CARTESIAN_POINT('Ctrl Pts',(-28.9279200507109,85.65659353544,65.596270283389));
#176444=CARTESIAN_POINT('Ctrl Pts',(-28.7930451388509,87.8505083144,71.23439898352));
#176445=CARTESIAN_POINT('Ctrl Pts',(-28.6581702270009,87.24827234311,77.254287886388));
#176446=CARTESIAN_POINT('Ctrl Pts',(-28.5232953151509,83.98092674223,82.346066051798));
#176447=CARTESIAN_POINT('Ctrl Pts',(-28.3884204032909,78.759415346747,85.40180992691));
#176448=CARTESIAN_POINT('Ctrl Pts',(-28.2535454914409,72.719890285177,85.75661823069));
#176449=CARTESIAN_POINT('Ctrl Pts',(-28.1186705795909,67.176495802086,83.33328797713));
#176450=CARTESIAN_POINT('Ctrl Pts',(-27.9837956677309,63.33542276651,78.659113200594));
#176451=CARTESIAN_POINT('Ctrl Pts',(-27.8489207558809,62.03245279771,72.7511506779378));
#176452=CARTESIAN_POINT('Ctrl Pts',(-27.7140458440209,63.55109999215,66.894917878018));
#176453=CARTESIAN_POINT('Ctrl Pts',(-27.5791709321709,67.560920903401,62.36467636483));
#176454=CARTESIAN_POINT('Ctrl Pts',(-27.4442960203209,73.189415950175,60.1461643823));
#176455=CARTESIAN_POINT('Ctrl Pts',(-27.3094211084609,79.211877176565,60.72210941845));
#176456=CARTESIAN_POINT('Ctrl Pts',(-27.1745461966109,84.317873265426,63.967191212364));
#176457=CARTESIAN_POINT('Ctrl Pts',(-27.0396712847609,87.39638715412,69.175310272392));
#176458=CARTESIAN_POINT('Ctrl Pts',(-26.9047963729009,87.77756297245,75.213228531899));
#176459=CARTESIAN_POINT('Ctrl Pts',(-26.7699214610509,85.3784604194,80.767151365512));
#176460=CARTESIAN_POINT('Ctrl Pts',(-26.6350465492009,80.72110181523,84.62859704241));
#176461=CARTESIAN_POINT('Ctrl Pts',(-26.5001716373439,74.8188848557683,
85.95735101692));
#176462=CARTESIAN_POINT('Ctrl Pts',(-26.3652967254909,68.956076977649,84.46428894445));
#176463=CARTESIAN_POINT('Ctrl Pts',(-26.2304218136369,64.40836986477,80.47428677502));
#176464=CARTESIAN_POINT('Ctrl Pts',(-26.0955469017839,62.16530418659,74.855533257242));
#176465=CARTESIAN_POINT('Ctrl Pts',(-25.9606719899309,62.71494234507,68.830610932353));
#176466=CARTESIAN_POINT('Ctrl Pts',(-25.8257970780769,65.937717099708,63.710508084863));
#176467=CARTESIAN_POINT('Ctrl Pts',(-25.6909221662239,71.132274945143,60.609231204));
#176468=CARTESIAN_POINT('Ctrl Pts',(-25.5560472543709,77.168730987308,60.20188800851));
#176469=CARTESIAN_POINT('Ctrl Pts',(-25.4661306464689,80.877648373842,61.7846275445));
#176470=CARTESIAN_POINT('Ctrl Pts',(-25.4211723425179,82.452438031115,62.95416909548));
#176471=CARTESIAN_POINT('Ctrl Pts',(-29.8939874914009,63.3102199125,76.473641268518));
#176472=CARTESIAN_POINT('Ctrl Pts',(-29.8490291874409,62.76334356092,74.639116314802));
#176473=CARTESIAN_POINT('Ctrl Pts',(-29.7591125795409,62.54988894054,70.709586619743));
#176474=CARTESIAN_POINT('Ctrl Pts',(-29.6242376676909,64.93832361102,65.309867378662));
#176475=CARTESIAN_POINT('Ctrl Pts',(-29.4893627558309,69.516195299397,61.58140129744));
#176476=CARTESIAN_POINT('Ctrl Pts',(-29.3544878439809,75.2872621463521,
60.33499902876));
#176477=CARTESIAN_POINT('Ctrl Pts',(-29.2196129321309,80.995831345442,61.84199166565));
#176478=CARTESIAN_POINT('Ctrl Pts',(-29.0847380202709,85.39976152061,65.774438030224));
#176479=CARTESIAN_POINT('Ctrl Pts',(-28.9498631084209,87.54080128363,71.276683537561));
#176480=CARTESIAN_POINT('Ctrl Pts',(-28.8149881965709,86.95307965761,77.151488536196));
#176481=CARTESIAN_POINT('Ctrl Pts',(-28.6801132847109,83.764479572449,82.120550972519));
#176482=CARTESIAN_POINT('Ctrl Pts',(-28.5452383728609,78.668810575635,85.10264909454));
#176483=CARTESIAN_POINT('Ctrl Pts',(-28.4103634610009,72.774842664668,85.44890624816));
#176484=CARTESIAN_POINT('Ctrl Pts',(-28.2754885491509,67.365048207639,83.08398009808));
#176485=CARTESIAN_POINT('Ctrl Pts',(-28.1406136373009,63.61654795562,78.522456491124));
#176486=CARTESIAN_POINT('Ctrl Pts',(-28.0057387254409,62.34498055475,72.7568803617516));
#176487=CARTESIAN_POINT('Ctrl Pts',(-27.8708638135909,63.82702719598,67.041787229428));
#176488=CARTESIAN_POINT('Ctrl Pts',(-27.7359889017409,67.740208371439,62.62072798463));
#176489=CARTESIAN_POINT('Ctrl Pts',(-27.6011139898809,73.233052403798,60.45568382937));
#176490=CARTESIAN_POINT('Ctrl Pts',(-27.4662390780309,79.110367730999,61.0177481518));
#176491=CARTESIAN_POINT('Ctrl Pts',(-27.3313641661709,84.093305427996,64.184621004688));
#176492=CARTESIAN_POINT('Ctrl Pts',(-27.1964892543209,87.09762478895,69.267220431524));
#176493=CARTESIAN_POINT('Ctrl Pts',(-27.0616143424709,87.46961397994,75.159620265581));
#176494=CARTESIAN_POINT('Ctrl Pts',(-26.9267394306109,85.12833162435,80.579689331869));
#176495=CARTESIAN_POINT('Ctrl Pts',(-26.7918645187609,80.583218907207,84.34807122905));
#176496=CARTESIAN_POINT('Ctrl Pts',(-26.6569896069109,74.8232498685848,
85.64480122147));
#176497=CARTESIAN_POINT('Ctrl Pts',(-26.5221146950539,69.101740122451,84.18772308129));
#176498=CARTESIAN_POINT('Ctrl Pts',(-26.3872397832009,64.6636362122,80.293883000897));
#176499=CARTESIAN_POINT('Ctrl Pts',(-26.2523648713479,62.47463012405,74.810545719273));
#176500=CARTESIAN_POINT('Ctrl Pts',(-26.1174899594939,63.01102158459,68.93082860792));
#176501=CARTESIAN_POINT('Ctrl Pts',(-25.9826150476409,66.156125014816,63.934124135913));
#176502=CARTESIAN_POINT('Ctrl Pts',(-25.8477401357879,71.225490062652,60.90759038823));
#176503=CARTESIAN_POINT('Ctrl Pts',(-25.7128652239349,77.116462919915,60.51006447377));
#176504=CARTESIAN_POINT('Ctrl Pts',(-25.6229486160329,80.735992574615,62.05465878235));
#176505=CARTESIAN_POINT('Ctrl Pts',(-25.5779903120819,82.272828602591,63.196013491817));
#176506=CARTESIAN_POINT('Ctrl Pts',(-29.3659074908668,61.9518604038339,
72.9107242579373));
#176507=CARTESIAN_POINT('Ctrl Pts',(-29.3564982338579,61.9539954571989,
72.4863077052749));
#176508=CARTESIAN_POINT('Ctrl Pts',(-29.3471083830932,61.9767196234027,
72.0619896297967));
#176509=CARTESIAN_POINT('Ctrl Pts',(-29.3281064148669,62.0654264883602,
71.201562242445));
#176510=CARTESIAN_POINT('Ctrl Pts',(-29.3185886994199,62.1328230949399,
70.7675430471975));
#176511=CARTESIAN_POINT('Ctrl Pts',(-29.289671755828,62.4039391099025,69.4669196437128));
#176512=CARTESIAN_POINT('Ctrl Pts',(-29.2702173421716,62.6747728688316,
68.6164798036698));
#176513=CARTESIAN_POINT('Ctrl Pts',(-29.2253010143749,63.4868923496922,
66.7420249311327));
#176514=CARTESIAN_POINT('Ctrl Pts',(-29.1996910938571,64.0862024991567,
65.740124142594));
#176515=CARTESIAN_POINT('Ctrl Pts',(-29.1554746275351,65.3421021879449,
64.1717374147651));
#176516=CARTESIAN_POINT('Ctrl Pts',(-29.1369985242667,65.9388441111051,
63.5616726039035));
#176517=CARTESIAN_POINT('Ctrl Pts',(-29.0982964755062,67.2973649983439,
62.4171369941487));
#176518=CARTESIAN_POINT('Ctrl Pts',(-29.0780486891563,68.0695483513939,
61.8944315984558));
#176519=CARTESIAN_POINT('Ctrl Pts',(-29.0439062068915,69.4272642755156,
61.1728740841599));
#176520=CARTESIAN_POINT('Ctrl Pts',(-29.030205421648,69.9843041918136,60.9255555918941));
#176521=CARTESIAN_POINT('Ctrl Pts',(-29.005076972165,71.0608373329505,60.5371020287685));
#176522=CARTESIAN_POINT('Ctrl Pts',(-28.9935432859152,71.5729114864887,
60.3872947629798));
#176523=CARTESIAN_POINT('Ctrl Pts',(-28.9678778363645,72.7305854823305,
60.1235672511679));
#176524=CARTESIAN_POINT('Ctrl Pts',(-28.9537518307,73.3799877554864,60.0257510402805));
#176525=CARTESIAN_POINT('Ctrl Pts',(-28.9272333959977,74.5867108664625,
59.935094182849));
#176526=CARTESIAN_POINT('Ctrl Pts',(-28.9148514570428,75.1431274515827,
59.9285573507583));
#176527=CARTESIAN_POINT('Ctrl Pts',(-28.894245021341,76.0531290116093,59.9765702061662));
#176528=CARTESIAN_POINT('Ctrl Pts',(-28.8862433423036,76.4068465772595,
60.009980381597));
#176529=CARTESIAN_POINT('Ctrl Pts',(-28.8628405996903,77.4569079514817,
60.1535672105847));
#176530=CARTESIAN_POINT('Ctrl Pts',(-28.847775368609,78.1460495216983,60.3060100929327));
#176531=CARTESIAN_POINT('Ctrl Pts',(-28.8184409165635,79.45395328342,60.7071765218225));
#176532=CARTESIAN_POINT('Ctrl Pts',(-28.8041641772532,80.0746521341312,
60.9501490391669));
#176533=CARTESIAN_POINT('Ctrl Pts',(-28.7788127382842,81.1069822190985,
61.4473862647356));
#176534=CARTESIAN_POINT('Ctrl Pts',(-28.7678363057078,81.5291068465773,
61.6800814496751));
#176535=CARTESIAN_POINT('Ctrl Pts',(-28.7507665891748,82.1645694268526,
62.0782275091685));
#176536=CARTESIAN_POINT('Ctrl Pts',(-28.7446895648506,82.3876760344657,
62.2279149754432));
#176537=CARTESIAN_POINT('Ctrl Pts',(-28.7305581875881,82.9046652249705,
62.5990232838268));
#176538=CARTESIAN_POINT('Ctrl Pts',(-28.7225807105516,83.1937714381268,
62.8259749995625));
#176539=CARTESIAN_POINT('Ctrl Pts',(-28.7013577352784,83.9441115759072,
63.4680045318863));
#176540=CARTESIAN_POINT('Ctrl Pts',(-28.6882685949821,84.3866748563063,
63.9049517853678));
#176541=CARTESIAN_POINT('Ctrl Pts',(-28.6666857942288,85.0510748040619,
64.6603255432425));
#176542=CARTESIAN_POINT('Ctrl Pts',(-28.6583249479937,85.2931207574033,
64.961113426));
#176543=CARTESIAN_POINT('Ctrl Pts',(-28.6410882186472,85.7535049093648,
65.5877304124733));
#176544=CARTESIAN_POINT('Ctrl Pts',(-28.63214885462,85.9714103310952,65.9138967139593));
#176545=CARTESIAN_POINT('Ctrl Pts',(-28.6167537591334,86.3191113527359,
66.4890147020966));
#176546=CARTESIAN_POINT('Ctrl Pts',(-28.6103288702727,86.4563168757537,
66.7334789894221));
#176547=CARTESIAN_POINT('Ctrl Pts',(-28.5984854509473,86.6980408423123,
67.1993015118161));
#176548=CARTESIAN_POINT('Ctrl Pts',(-28.5930704354805,86.8042213244609,
67.419152406551));
#176549=CARTESIAN_POINT('Ctrl Pts',(-28.5762221012571,87.1197468350586,
68.1228960845822));
#176550=CARTESIAN_POINT('Ctrl Pts',(-28.5650682168193,87.3058434984508,
68.6170223101508));
#176551=CARTESIAN_POINT('Ctrl Pts',(-28.5457936377573,87.5752215663412,
69.4876053155158));
#176552=CARTESIAN_POINT('Ctrl Pts',(-28.5376684111527,87.6727047519809,
69.8596919164948));
#176553=CARTESIAN_POINT('Ctrl Pts',(-28.5232331813806,87.8144021310478,
70.5161458065337));
#176554=CARTESIAN_POINT('Ctrl Pts',(-28.5169818665082,87.8658550860038,
70.7989828665514));
#176555=CARTESIAN_POINT('Ctrl Pts',(-28.4996699092958,87.9802350822815,
71.5701860550689));
#176556=CARTESIAN_POINT('Ctrl Pts',(-28.4882983323491,88.0251587755903,
72.0612388390642));
#176557=CARTESIAN_POINT('Ctrl Pts',(-28.4713222982358,88.0506123982403,
72.8005799439378));
#176558=CARTESIAN_POINT('Ctrl Pts',(-28.4656642202474,88.0520553470386,
73.0481475982963));
#176559=CARTESIAN_POINT('Ctrl Pts',(-28.4551716412926,88.0412888590141,
73.5141885267032));
#176560=CARTESIAN_POINT('Ctrl Pts',(-28.4503395549486,88.030653834725,73.7321861328932));
#176561=CARTESIAN_POINT('Ctrl Pts',(-28.4334128661627,87.9730180649228,
74.5067584769098));
#176562=CARTESIAN_POINT('Ctrl Pts',(-28.4217087262867,87.8953464065803,
75.060685681791));
#176563=CARTESIAN_POINT('Ctrl Pts',(-28.4001843683505,87.6892138892675,
76.0622437309167));
#176564=CARTESIAN_POINT('Ctrl Pts',(-28.3903751682219,87.5714840520253,
76.5121166723893));
#176565=CARTESIAN_POINT('Ctrl Pts',(-28.3753343901809,87.3620113754935,
77.1690380808749));
#176566=CARTESIAN_POINT('Ctrl Pts',(-28.3703382894102,87.2881121570046,
77.3818215717414));
#176567=CARTESIAN_POINT('Ctrl Pts',(-28.3539567018314,87.032071207605,78.0622424495177));
#176568=CARTESIAN_POINT('Ctrl Pts',(-28.3423086815491,86.8284778504005,
78.5218363055945));
#176569=CARTESIAN_POINT('Ctrl Pts',(-28.3257320467384,86.4970967377994,
79.1662564668239));
#176570=CARTESIAN_POINT('Ctrl Pts',(-28.3206683464067,86.3900996146686,
79.3617753846728));
#176571=CARTESIAN_POINT('Ctrl Pts',(-28.3110781464308,86.1746926264359,
79.7321581480111));
#176572=CARTESIAN_POINT('Ctrl Pts',(-28.3065585731675,86.0672566883146,
79.9070521614495));
#176573=CARTESIAN_POINT('Ctrl Pts',(-28.2903497051778,85.6606113672015,
80.5346701629311));
#176574=CARTESIAN_POINT('Ctrl Pts',(-28.2790534865079,85.3369588787352,
80.9710469484754));
#176575=CARTESIAN_POINT('Ctrl Pts',(-28.2617405571487,84.8055873283224,
81.6018369594899));
#176576=CARTESIAN_POINT('Ctrl Pts',(-28.2557863558243,84.6165958335401,
81.812028313147));
#176577=CARTESIAN_POINT('Ctrl Pts',(-28.2449075350388,84.2652088931614,
82.1784473410338));
#176578=CARTESIAN_POINT('Ctrl Pts',(-28.2400168935055,84.1051963462792,
82.3369738074407));
#176579=CARTESIAN_POINT('Ctrl Pts',(-28.2223958786166,83.5256814169202,
82.8824447742505));
#176580=CARTESIAN_POINT('Ctrl Pts',(-28.2092075896598,83.0847143411874,
83.2466708502592));
#176581=CARTESIAN_POINT('Ctrl Pts',(-28.1898112962602,82.3986096141907,
83.7415470218061));
#176582=CARTESIAN_POINT('Ctrl Pts',(-28.1835238643657,82.1702444803154,
83.8955205290103));
#176583=CARTESIAN_POINT('Ctrl Pts',(-28.172426025588,81.7524222984042,84.1581830692444));
#176584=CARTESIAN_POINT('Ctrl Pts',(-28.1675783568522,81.5646239048304,
84.2696982543368));
#176585=CARTESIAN_POINT('Ctrl Pts',(-28.1499587002885,80.8584550908841,
84.6648230738459));
#176586=CARTESIAN_POINT('Ctrl Pts',(-28.1377313665428,80.3231327240567,
84.9174692347079));
#176587=CARTESIAN_POINT('Ctrl Pts',(-28.120177029338,79.5443191346533,85.2226728645883));
#176588=CARTESIAN_POINT('Ctrl Pts',(-28.1149880891762,79.3128811832984,
85.305941847855));
#176589=CARTESIAN_POINT('Ctrl Pts',(-28.105027972566,78.8718287703843,85.450826165863));
#176590=CARTESIAN_POINT('Ctrl Pts',(-28.1002660041616,78.662662659087,85.5138227930762));
#176591=CARTESIAN_POINT('Ctrl Pts',(-28.084358923876,77.970561149516,85.7036742889627));
#176592=CARTESIAN_POINT('Ctrl Pts',(-28.0729223317712,77.4815190943867,
85.8084453208436));
#176593=CARTESIAN_POINT('Ctrl Pts',(-28.0508832707176,76.5299993537951,
85.9561309732578));
#176594=CARTESIAN_POINT('Ctrl Pts',(-28.0402809737513,76.0680803210234,
86.0029343227759));
#176595=CARTESIAN_POINT('Ctrl Pts',(-28.0252281641927,75.3909220703083,
86.0347769539215));
#176596=CARTESIAN_POINT('Ctrl Pts',(-28.0205423784486,75.1767369359267,
86.0394917040199));
#176597=CARTESIAN_POINT('Ctrl Pts',(-28.0070172332282,74.5475319527212,
86.0374732746602));
#176598=CARTESIAN_POINT('Ctrl Pts',(-27.9983748948165,74.133017053517,86.016020173507));
#176599=CARTESIAN_POINT('Ctrl Pts',(-27.9842063416753,73.459831027145,85.9489422438951));
#176600=CARTESIAN_POINT('Ctrl Pts',(-27.9787046285731,73.1999971494259,
85.9151310851981));
#176601=CARTESIAN_POINT('Ctrl Pts',(-27.9680786331366,72.7089387105117,
85.8362548591247));
#176602=CARTESIAN_POINT('Ctrl Pts',(-27.962959731273,72.4774716752162,85.7926708696398));
#176603=CARTESIAN_POINT('Ctrl Pts',(-27.9459079922839,71.7226864299946,
85.6295219740991));
#176604=CARTESIAN_POINT('Ctrl Pts',(-27.933669204793,71.204894921339,85.4840841649155));
#176605=CARTESIAN_POINT('Ctrl Pts',(-27.9131107191997,70.3528257095262,
85.1874098975274));
#176606=CARTESIAN_POINT('Ctrl Pts',(-27.9047868359488,70.0126814631457,
85.0528224317421));
#176607=CARTESIAN_POINT('Ctrl Pts',(-27.8904074149884,69.426970927856,84.7919520033186));
#176608=CARTESIAN_POINT('Ctrl Pts',(-27.8842971544598,69.178704676175,84.6717539983116));
#176609=CARTESIAN_POINT('Ctrl Pts',(-27.8698641651585,68.5902566395028,
84.3630061943237));
#176610=CARTESIAN_POINT('Ctrl Pts',(-27.8617102002911,68.254769317834,84.1669030613641));
#176611=CARTESIAN_POINT('Ctrl Pts',(-27.8453550084675,67.6000791285052,
83.7438474717693));
#176612=CARTESIAN_POINT('Ctrl Pts',(-27.837132829163,67.2807834941334,83.5164356122228));
#176613=CARTESIAN_POINT('Ctrl Pts',(-27.8216158902758,66.7164728185939,
83.0752714533215));
#176614=CARTESIAN_POINT('Ctrl Pts',(-27.8144342768204,66.4680829739782,
82.8658224671431));
#176615=CARTESIAN_POINT('Ctrl Pts',(-27.7925141076388,65.7427195640055,
82.2069105184709));
#176616=CARTESIAN_POINT('Ctrl Pts',(-27.7775244449321,65.2904168095573,
81.7301117030604));
#176617=CARTESIAN_POINT('Ctrl Pts',(-27.7543237430188,64.6387834351827,
80.9306647299601));
#176618=CARTESIAN_POINT('Ctrl Pts',(-27.7459456038654,64.4137660149623,
80.628877251408));
#176619=CARTESIAN_POINT('Ctrl Pts',(-27.7285710578544,63.9655724982218,
79.969189009831));
#176620=CARTESIAN_POINT('Ctrl Pts',(-27.7197240144243,63.7467831046844,
79.6100593961934));
#176621=CARTESIAN_POINT('Ctrl Pts',(-27.7023250909221,63.3523070043413,
78.8856638740414));
#176622=CARTESIAN_POINT('Ctrl Pts',(-27.6936986564019,63.1753358727586,
78.5210595402815));
#176623=CARTESIAN_POINT('Ctrl Pts',(-27.6675797083518,62.7034813042502,
77.4225764407909));
#176624=CARTESIAN_POINT('Ctrl Pts',(-27.649675103024,62.4568896885277,76.6677537942532));
#176625=CARTESIAN_POINT('Ctrl Pts',(-27.622778973032,62.1890845922095,75.5014481464094));
#176626=CARTESIAN_POINT('Ctrl Pts',(-27.6136892790897,62.1165761733617,
75.1015430110143));
#176627=CARTESIAN_POINT('Ctrl Pts',(-27.5967623749457,62.015285521393,74.3407693058522));
#176628=CARTESIAN_POINT('Ctrl Pts',(-27.588911682362,61.9825824542457,73.9804215063247));
#176629=CARTESIAN_POINT('Ctrl Pts',(-27.5726952476484,61.9462255563491,
73.2211702198871));
#176630=CARTESIAN_POINT('Ctrl Pts',(-27.5643023785364,61.9456694868364,
72.8232192864476));
#176631=CARTESIAN_POINT('Ctrl Pts',(-27.5329917923185,62.0097849875933,
71.3750406569346));
#176632=CARTESIAN_POINT('Ctrl Pts',(-27.5093033935215,62.1833553964862,
70.3293263596869));
#176633=CARTESIAN_POINT('Ctrl Pts',(-27.4749412181969,62.6153512025303,
68.8498644114641));
#176634=CARTESIAN_POINT('Ctrl Pts',(-27.4640850915678,62.7787328643152,
68.3879182399081));
#176635=CARTESIAN_POINT('Ctrl Pts',(-27.4356932887815,63.2809772079994,
67.1895048707421));
#176636=CARTESIAN_POINT('Ctrl Pts',(-27.4185930823565,63.6633232223783,
66.4766538853576));
#176637=CARTESIAN_POINT('Ctrl Pts',(-27.3825509135325,64.5707608461097,
65.1036229345754));
#176638=CARTESIAN_POINT('Ctrl Pts',(-27.363866715291,65.102041958874,64.4464312496956));
#176639=CARTESIAN_POINT('Ctrl Pts',(-27.3275858984294,66.2484712427984,
63.2771098842673));
#176640=CARTESIAN_POINT('Ctrl Pts',(-27.3099850543916,66.8589056351111,
62.7579304603558));
#176641=CARTESIAN_POINT('Ctrl Pts',(-27.2561001277643,68.8874815752587,
61.3386319068995));
#176642=CARTESIAN_POINT('Ctrl Pts',(-27.2193312238702,70.4484153494107,
60.6471229272152));
#176643=CARTESIAN_POINT('Ctrl Pts',(-27.163845282467,72.8976775687344,60.0821227070811));
#176644=CARTESIAN_POINT('Ctrl Pts',(-27.1454072056421,73.7258624050007,
59.9740771483805));
#176645=CARTESIAN_POINT('Ctrl Pts',(-27.0942944771862,76.0636964224413,
59.8985369954317));
#176646=CARTESIAN_POINT('Ctrl Pts',(-27.0619671031244,77.5720983174881,
60.1092423462382));
#176647=CARTESIAN_POINT('Ctrl Pts',(-27.020462786728,79.3446424713931,60.678195355492));
#176648=CARTESIAN_POINT('Ctrl Pts',(-27.0122985285325,79.6845914787547,
60.8032117456719));
#176649=CARTESIAN_POINT('Ctrl Pts',(-26.9871305006992,80.7306118381862,
61.239437844667));
#176650=CARTESIAN_POINT('Ctrl Pts',(-26.9704806532513,81.4149891932611,
61.6001714360441));
#176651=CARTESIAN_POINT('Ctrl Pts',(-26.9358799470581,82.7624597916229,
62.4688447909563));
#176652=CARTESIAN_POINT('Ctrl Pts',(-26.9179148479559,83.419644908176,62.9864356224054));
#176653=CARTESIAN_POINT('Ctrl Pts',(-26.8896489617799,84.3392982919,63.8646050038314));
#176654=CARTESIAN_POINT('Ctrl Pts',(-26.8796608922059,84.6415223812075,
64.1837672662168));
#176655=CARTESIAN_POINT('Ctrl Pts',(-26.8613952628632,85.1671283270705,
64.7991669455865));
#176656=CARTESIAN_POINT('Ctrl Pts',(-26.8532042088827,85.3946645605935,
65.0903585287338));
#176657=CARTESIAN_POINT('Ctrl Pts',(-26.8358997393618,85.8552599102491,
65.734769397251));
#176658=CARTESIAN_POINT('Ctrl Pts',(-26.8268048243646,86.0843151965931,
66.090858545665));
#176659=CARTESIAN_POINT('Ctrl Pts',(-26.8007583416444,86.6917107047555,
67.1434425426908));
#176660=CARTESIAN_POINT('Ctrl Pts',(-26.783872294885,87.0257464058268,67.8657205014914));
#176661=CARTESIAN_POINT('Ctrl Pts',(-26.7574958584136,87.4270111134863,
68.9894125338539));
#176662=CARTESIAN_POINT('Ctrl Pts',(-26.7484197851956,87.5445328786064,
69.3730634014937));
#176663=CARTESIAN_POINT('Ctrl Pts',(-26.7296221147459,87.7491128006321,
70.1712710306875));
#176664=CARTESIAN_POINT('Ctrl Pts',(-26.7199881481467,87.8340296633232,
70.5860658319642));
#176665=CARTESIAN_POINT('Ctrl Pts',(-26.7009018641838,87.9650356085774,
71.4411355472774));
#176666=CARTESIAN_POINT('Ctrl Pts',(-26.6914264830145,88.0093605486581,
71.8799832571119));
#176667=CARTESIAN_POINT('Ctrl Pts',(-26.6644730962213,88.0727815060036,
73.1416759569455));
#176668=CARTESIAN_POINT('Ctrl Pts',(-26.6471711075735,88.0366256560804,
73.9674584092148));
#176669=CARTESIAN_POINT('Ctrl Pts',(-26.6221879431741,87.8817029207814,
75.0896077926789));
#176670=CARTESIAN_POINT('Ctrl Pts',(-26.6152061766537,87.8284521936595,
75.3952408936558));
#176671=CARTESIAN_POINT('Ctrl Pts',(-26.5981209286503,87.6737666541221,
76.1278569934313));
#176672=CARTESIAN_POINT('Ctrl Pts',(-26.5879730360397,87.5615069598982,
76.5525448167818));
#176673=CARTESIAN_POINT('Ctrl Pts',(-26.5727315783776,87.3551027342262,
77.1974324033812));
#176674=CARTESIAN_POINT('Ctrl Pts',(-26.5674697523318,87.2762257092991,
77.4219902446079));
#176675=CARTESIAN_POINT('Ctrl Pts',(-26.551714967308,87.0178572943662,78.0971664379141));
#176676=CARTESIAN_POINT('Ctrl Pts',(-26.5414479421155,86.8189623764084,
78.5403282845433));
#176677=CARTESIAN_POINT('Ctrl Pts',(-26.5193723997868,86.3391411211965,
79.4682464492547));
#176678=CARTESIAN_POINT('Ctrl Pts',(-26.5075648013405,86.0502750435632,
79.948961822146));
#176679=CARTESIAN_POINT('Ctrl Pts',(-26.4901011932104,85.5956111489685,
80.6069925442744));
#176680=CARTESIAN_POINT('Ctrl Pts',(-26.4847749661921,85.4536682915792,
80.8008845086256));
#176681=CARTESIAN_POINT('Ctrl Pts',(-26.4733338461345,85.1429547905315,
81.2017922635603));
#176682=CARTESIAN_POINT('Ctrl Pts',(-26.4672136573702,84.9729538104197,
81.4078623196491));
#176683=CARTESIAN_POINT('Ctrl Pts',(-26.4503871463832,84.4896779366806,
81.9583567950162));
#176684=CARTESIAN_POINT('Ctrl Pts',(-26.4396561649543,84.1638512724422,
82.2917404998743));
#176685=CARTESIAN_POINT('Ctrl Pts',(-26.4240726942374,83.6463503031868,
82.7663707883053));
#176686=CARTESIAN_POINT('Ctrl Pts',(-26.4189237189563,83.4674861103605,
82.9214875466556));
#176687=CARTESIAN_POINT('Ctrl Pts',(-26.4073473207837,83.0507913278121,
83.2632709622442));
#176688=CARTESIAN_POINT('Ctrl Pts',(-26.4009613103596,82.8103684385238,
83.4467584999488));
#176689=CARTESIAN_POINT('Ctrl Pts',(-26.3827457350335,82.1046571584463,
83.9476350985173));
#176690=CARTESIAN_POINT('Ctrl Pts',(-26.3709709794553,81.6243515321666,
84.243935498527));
#176691=CARTESIAN_POINT('Ctrl Pts',(-26.3539767729892,80.9332015918654,
84.6115655225933));
#176692=CARTESIAN_POINT('Ctrl Pts',(-26.3491329449994,80.7366421684322,
84.7099033048351));
#176693=CARTESIAN_POINT('Ctrl Pts',(-26.338946675524,80.3253459523221,84.9029724294442));
#176694=CARTESIAN_POINT('Ctrl Pts',(-26.3336041944195,80.110275842259,84.9970073624504));
#176695=CARTESIAN_POINT('Ctrl Pts',(-26.3142319607583,79.3264514548815,
85.3149591532496));
#176696=CARTESIAN_POINT('Ctrl Pts',(-26.3000246950262,78.744007635783,85.5051243373986));
#176697=CARTESIAN_POINT('Ctrl Pts',(-26.2816122076784,77.9367555483608,
85.7060944034288));
#176698=CARTESIAN_POINT('Ctrl Pts',(-26.2768286949653,77.7214757596124,
85.7537910392488));
#176699=CARTESIAN_POINT('Ctrl Pts',(-26.2660720302795,77.2285041652266,
85.8498414943771));
#176700=CARTESIAN_POINT('Ctrl Pts',(-26.2601348364542,76.9500237034786,
85.8946831368301));
#176701=CARTESIAN_POINT('Ctrl Pts',(-26.2429700601151,76.138463532457,85.9985253292113));
#176702=CARTESIAN_POINT('Ctrl Pts',(-26.2317986248592,75.6023259005181,
86.0338074442609));
#176703=CARTESIAN_POINT('Ctrl Pts',(-26.2155065051407,74.8506832506398,
86.0374429040957));
#176704=CARTESIAN_POINT('Ctrl Pts',(-26.2107555598615,74.6352579008578,
86.0332104581162));
#176705=CARTESIAN_POINT('Ctrl Pts',(-26.2003641428551,74.1714666081721,
86.012729816208));
#176706=CARTESIAN_POINT('Ctrl Pts',(-26.1947078232235,73.9231713470529,
85.9947174873763));
#176707=CARTESIAN_POINT('Ctrl Pts',(-26.1741183630528,73.0272419081808,
85.9040947848472));
#176708=CARTESIAN_POINT('Ctrl Pts',(-26.1589940667163,72.3837514385232,
85.7902964704825));
#176709=CARTESIAN_POINT('Ctrl Pts',(-26.1398650436156,71.5455017237514,
85.5752119984921));
#176710=CARTESIAN_POINT('Ctrl Pts',(-26.1352370951203,71.3402287048517,
85.5170114831311));
#176711=CARTESIAN_POINT('Ctrl Pts',(-26.1249826355312,70.8823191795475,
85.3747761601401));
#176712=CARTESIAN_POINT('Ctrl Pts',(-26.1193885736418,70.6306924143436,
85.2879748852595));
#176713=CARTESIAN_POINT('Ctrl Pts',(-26.1032504285204,69.9103993676397,
85.0145340562684));
#176714=CARTESIAN_POINT('Ctrl Pts',(-26.0927587683217,69.4492339301159,
84.8081158674202));
#176715=CARTESIAN_POINT('Ctrl Pts',(-26.0768767947257,68.7979686602581,
84.4705736902692));
#176716=CARTESIAN_POINT('Ctrl Pts',(-26.0718192632528,68.5972638812067,
84.3598225197354));
#176717=CARTESIAN_POINT('Ctrl Pts',(-26.0604385782711,68.1581486434782,
84.10237796679));
#176718=CARTESIAN_POINT('Ctrl Pts',(-26.0540845086778,67.921209111272,83.9531453635371));
#176719=CARTESIAN_POINT('Ctrl Pts',(-26.0326176020567,67.1415381307353,
83.4266271577465));
#176720=CARTESIAN_POINT('Ctrl Pts',(-26.0173623862014,66.6216448893775,
83.015447269992));
#176721=CARTESIAN_POINT('Ctrl Pts',(-25.9978851098422,65.973547218442,82.4162631829118));
#176722=CARTESIAN_POINT('Ctrl Pts',(-25.9930886383386,65.8150472624552,
82.2619092271083));
#176723=CARTESIAN_POINT('Ctrl Pts',(-25.9825821331696,65.4714486242781,
81.9094715854228));
#176724=CARTESIAN_POINT('Ctrl Pts',(-25.9769067577913,65.2887395400715,
81.7098203747785));
#176725=CARTESIAN_POINT('Ctrl Pts',(-25.9616090100639,64.8125894617919,
81.15577405542));
#176726=CARTESIAN_POINT('Ctrl Pts',(-25.9520003131318,64.5312628947353,
80.7909775931263));
#176727=CARTESIAN_POINT('Ctrl Pts',(-25.9358139057098,64.1077298156168,
80.1779590637891));
#176728=CARTESIAN_POINT('Ctrl Pts',(-25.9294925541469,63.9532998099031,
79.938159223049));
#176729=CARTESIAN_POINT('Ctrl Pts',(-25.9143714584637,63.6068872801481,
79.3599371596408));
#176730=CARTESIAN_POINT('Ctrl Pts',(-25.9055075558728,63.4217170354802,
79.0173944753116));
#176731=CARTESIAN_POINT('Ctrl Pts',(-25.8852161328144,63.0330730830113,
78.2152563338669));
#176732=CARTESIAN_POINT('Ctrl Pts',(-25.8737953749455,62.8399720566537,
77.7505994263655));
#176733=CARTESIAN_POINT('Ctrl Pts',(-25.8573466709818,62.594885478589,77.0476217222832));
#176734=CARTESIAN_POINT('Ctrl Pts',(-25.8520771467528,62.5216288080039,
76.8167769541858));
#176735=CARTESIAN_POINT('Ctrl Pts',(-25.8392202706116,62.356130905073,76.238552697275));
#176736=CARTESIAN_POINT('Ctrl Pts',(-25.8317252506728,62.2718865056701,
75.8894256090391));
#176737=CARTESIAN_POINT('Ctrl Pts',(-25.8169810487476,62.1356880662047,
75.2015691474896));
#176738=CARTESIAN_POINT('Ctrl Pts',(-25.8097163405197,62.0824302136498,
74.8631149413459));
#176739=CARTESIAN_POINT('Ctrl Pts',(-25.7937780429484,61.9969305702283,
74.1360762109128));
#176740=CARTESIAN_POINT('Ctrl Pts',(-25.7850983229709,61.9686106220109,
73.7470119385911));
#176741=CARTESIAN_POINT('Ctrl Pts',(-25.7614694609691,61.9387668588439,
72.6965261009687));
#176742=CARTESIAN_POINT('Ctrl Pts',(-25.746365168282,61.9696615368098,72.0340609509725));
#176743=CARTESIAN_POINT('Ctrl Pts',(-25.7241830758666,62.0912090174244,
71.0485307984549));
#176744=CARTESIAN_POINT('Ctrl Pts',(-25.7168555428034,62.1444179674266,
70.7208169164824));
#176745=CARTESIAN_POINT('Ctrl Pts',(-25.704296129729,62.2596456587527,70.1518497829427));
#176746=CARTESIAN_POINT('Ctrl Pts',(-25.6990213326695,62.3160591499028,
69.9099172028483));
#176747=CARTESIAN_POINT('Ctrl Pts',(-25.6886754232146,62.4409224071355,
69.4365971656001));
#176748=CARTESIAN_POINT('Ctrl Pts',(-25.6835980324187,62.509009553304,69.2050318081367));
#176749=CARTESIAN_POINT('Ctrl Pts',(-25.6710176818858,62.6915976545898,
68.6422538530757));
#176750=CARTESIAN_POINT('Ctrl Pts',(-25.6634230092666,62.813162807868,68.3133358375227));
#176751=CARTESIAN_POINT('Ctrl Pts',(-25.6469308771572,63.1010327267764,
67.6207602958996));
#176752=CARTESIAN_POINT('Ctrl Pts',(-25.6380085508726,63.2712409369225,
67.2586855968152));
#176753=CARTESIAN_POINT('Ctrl Pts',(-25.6094806088747,63.8639870406997,
66.1334341852122));
#176754=CARTESIAN_POINT('Ctrl Pts',(-25.5897204907838,64.34705706191,65.4019308983917));
#176755=CARTESIAN_POINT('Ctrl Pts',(-25.5633040231181,65.114039605429,64.4631759975833));
#176756=CARTESIAN_POINT('Ctrl Pts',(-25.5560721227099,65.3388955919402,
64.2093238118185));
#176757=CARTESIAN_POINT('Ctrl Pts',(-25.5376324116602,65.938520962717,63.5839944296733));
#176758=CARTESIAN_POINT('Ctrl Pts',(-25.5262670521131,66.3264140418631,
63.226077368409));
#176759=CARTESIAN_POINT('Ctrl Pts',(-25.5015769521811,67.196543220476,62.5149302089825));
#176760=CARTESIAN_POINT('Ctrl Pts',(-25.4882596254439,67.6845399522126,
62.1686021886949));
#176761=CARTESIAN_POINT('Ctrl Pts',(-25.4563912935859,68.9029738909808,
61.4226452836094));
#176762=CARTESIAN_POINT('Ctrl Pts',(-25.4378456278295,69.653482210693,61.0554991545458));
#176763=CARTESIAN_POINT('Ctrl Pts',(-25.4108569344788,70.8205996163349,
60.6192454789367));
#176764=CARTESIAN_POINT('Ctrl Pts',(-25.402011059299,71.2151668380905,60.4933124186287));
#176765=CARTESIAN_POINT('Ctrl Pts',(-25.3752278174413,72.4071241617779,
60.1745015968442));
#176766=CARTESIAN_POINT('Ctrl Pts',(-25.3571272368688,73.2199161670816,
60.037475388827));
#176767=CARTESIAN_POINT('Ctrl Pts',(-25.3188691789373,74.9443395382244,
59.9095450364837));
#176768=CARTESIAN_POINT('Ctrl Pts',(-25.2986976872818,75.8576415839786,
59.9358960975145));
#176769=CARTESIAN_POINT('Ctrl Pts',(-25.2583479843491,77.6829440804511,
60.1832535935612));
#176770=CARTESIAN_POINT('Ctrl Pts',(-25.2381057548755,78.5905580872887,
60.409751827594));
#176771=CARTESIAN_POINT('Ctrl Pts',(-25.2177843835793,79.4626792952277,
60.7277886365121));
#176772=CARTESIAN_POINT('',(-25.21690938235,79.4632381180988,60.7262027183532));
#176773=CARTESIAN_POINT('Ctrl Pts',(-29.4261514861327,72.242088232536,85.74414017529));
#176774=CARTESIAN_POINT('Ctrl Pts',(-29.3779431821827,70.095650878086,85.28004229623));
#176775=CARTESIAN_POINT('Ctrl Pts',(-29.2815265742827,66.04485241176,83.24564128978));
#176776=CARTESIAN_POINT('Ctrl Pts',(-29.1369016624246,62.20076662219,77.634595795182));
#176777=CARTESIAN_POINT('Ctrl Pts',(-28.9922767505727,61.55056525346,70.864604569967));
#176778=CARTESIAN_POINT('Ctrl Pts',(-28.8476518387227,64.25574478693,64.624573520997));
#176779=CARTESIAN_POINT('Ctrl Pts',(-28.7030269268629,69.641577033905,60.47138590026));
#176780=CARTESIAN_POINT('Ctrl Pts',(-28.5584020150127,76.364284952381,59.44121987509));
#176781=CARTESIAN_POINT('Ctrl Pts',(-28.4137771031546,82.746616870673,61.79109721394));
#176782=CARTESIAN_POINT('Ctrl Pts',(-28.2691521913028,87.19622473785,66.934740200613));
#176783=CARTESIAN_POINT('Ctrl Pts',(-28.1245272794527,88.60296550284,73.5888484027236));
#176784=CARTESIAN_POINT('Ctrl Pts',(-27.9799023675929,86.61586754518,80.093271282679));
#176785=CARTESIAN_POINT('Ctrl Pts',(-27.8352774557427,81.730697090025,84.82520375033));
#176786=CARTESIAN_POINT('Ctrl Pts',(-27.6906525438927,75.1662677935533,
86.60406386368));
#176787=CARTESIAN_POINT('Ctrl Pts',(-27.5460276320329,68.560355920967,84.98603926299));
#176788=CARTESIAN_POINT('Ctrl Pts',(-27.4014027201827,63.56108732498,80.374815045269));
#176789=CARTESIAN_POINT('Ctrl Pts',(-27.2567778083246,61.41574231844,73.9208573383313));
#176790=CARTESIAN_POINT('Ctrl Pts',(-27.1121528964728,62.65956851573,67.234380562697));
#176791=CARTESIAN_POINT('Ctrl Pts',(-26.9675279846227,66.982240536617,61.98361091626));
#176792=CARTESIAN_POINT('Ctrl Pts',(-26.8229030727646,73.305283879178,59.47857635201));
#176793=CARTESIAN_POINT('Ctrl Pts',(-26.6782781609127,80.05114628266,60.34426435248));
#176794=CARTESIAN_POINT('Ctrl Pts',(-26.5336532490595,85.53678527666,64.36469220339));
#176795=CARTESIAN_POINT('Ctrl Pts',(-26.3890283372062,88.39357475485,70.536793074933));
#176796=CARTESIAN_POINT('Ctrl Pts',(-26.2444034253522,87.90876699715,77.320673726326));
#176797=CARTESIAN_POINT('Ctrl Pts',(-26.0997785134991,84.203317946944,83.02380642958));
#176798=CARTESIAN_POINT('Ctrl Pts',(-25.9551536016452,78.201709510007,86.22330197028));
#176799=CARTESIAN_POINT('Ctrl Pts',(-25.8105286897922,71.40129854677,86.12091018816));
#176800=CARTESIAN_POINT('Ctrl Pts',(-25.665903777939,65.49873617875,82.742176443924));
#176801=CARTESIAN_POINT('Ctrl Pts',(-25.5212788660852,61.96667080937,76.930072003796));
#176802=CARTESIAN_POINT('Ctrl Pts',(-25.3766539542322,61.68631520576,70.134664941592));
#176803=CARTESIAN_POINT('Ctrl Pts',(-25.2320290423791,64.72765802224,64.051391343194));
#176804=CARTESIAN_POINT('Ctrl Pts',(-25.0874041305261,70.331750046873,60.1978610671));
#176805=CARTESIAN_POINT('Ctrl Pts',(-24.942779218673,77.100997250995,59.53595519057));
#176806=CARTESIAN_POINT('Ctrl Pts',(-24.846362610771,81.263224902643,61.33139849116));
#176807=CARTESIAN_POINT('Ctrl Pts',(-24.79815430682,82.998435097713,62.6773649606));
#176808=CARTESIAN_POINT('Ctrl Pts',(-29.5486931499337,72.242088232536,85.74414017529));
#176809=CARTESIAN_POINT('Ctrl Pts',(-29.5004848459837,70.095650878086,85.28004229623));
#176810=CARTESIAN_POINT('Ctrl Pts',(-29.4040682380836,66.04485241176,83.24564128978));
#176811=CARTESIAN_POINT('Ctrl Pts',(-29.2594433262332,62.20076662219,77.634595795182));
#176812=CARTESIAN_POINT('Ctrl Pts',(-29.1148184143737,61.55056525346,70.864604569967));
#176813=CARTESIAN_POINT('Ctrl Pts',(-28.9701935025236,64.25574478693,64.624573520997));
#176814=CARTESIAN_POINT('Ctrl Pts',(-28.8255685906649,69.641577033905,60.47138590026));
#176815=CARTESIAN_POINT('Ctrl Pts',(-28.6809436788136,76.364284952381,59.44121987509));
#176816=CARTESIAN_POINT('Ctrl Pts',(-28.5363187669632,82.746616870673,61.79109721394));
#176817=CARTESIAN_POINT('Ctrl Pts',(-28.3916938551037,87.19622473785,66.934740200613));
#176818=CARTESIAN_POINT('Ctrl Pts',(-28.2470689432536,88.60296550284,73.5888484027236));
#176819=CARTESIAN_POINT('Ctrl Pts',(-28.1024440313949,86.61586754518,80.093271282679));
#176820=CARTESIAN_POINT('Ctrl Pts',(-27.9578191195436,81.730697090025,84.82520375033));
#176821=CARTESIAN_POINT('Ctrl Pts',(-27.8131942076936,75.1662677935533,
86.60406386368));
#176822=CARTESIAN_POINT('Ctrl Pts',(-27.6685692958349,68.560355920967,84.98603926299));
#176823=CARTESIAN_POINT('Ctrl Pts',(-27.5239443839836,63.56108732498,80.374815045269));
#176824=CARTESIAN_POINT('Ctrl Pts',(-27.3793194721332,61.41574231844,73.9208573383313));
#176825=CARTESIAN_POINT('Ctrl Pts',(-27.2346945602737,62.65956851573,67.234380562697));
#176826=CARTESIAN_POINT('Ctrl Pts',(-27.0900696484237,66.982240536617,61.98361091626));
#176827=CARTESIAN_POINT('Ctrl Pts',(-26.9454447365732,73.305283879178,59.47857635201));
#176828=CARTESIAN_POINT('Ctrl Pts',(-26.8008198247137,80.05114628266,60.34426435248));
#176829=CARTESIAN_POINT('Ctrl Pts',(-26.6561949128635,85.53678527666,64.36469220339));
#176830=CARTESIAN_POINT('Ctrl Pts',(-26.5115700010092,88.39357475485,70.536793074933));
#176831=CARTESIAN_POINT('Ctrl Pts',(-26.3669450891548,87.90876699715,77.320673726326));
#176832=CARTESIAN_POINT('Ctrl Pts',(-26.2223201773017,84.203317946944,83.02380642958));
#176833=CARTESIAN_POINT('Ctrl Pts',(-26.0776952654478,78.201709510007,86.22330197028));
#176834=CARTESIAN_POINT('Ctrl Pts',(-25.9330703535948,71.40129854677,86.12091018816));
#176835=CARTESIAN_POINT('Ctrl Pts',(-25.7884454417409,65.49873617875,82.742176443924));
#176836=CARTESIAN_POINT('Ctrl Pts',(-25.6438205298878,61.96667080937,76.930072003796));
#176837=CARTESIAN_POINT('Ctrl Pts',(-25.4991956180348,61.68631520576,70.134664941592));
#176838=CARTESIAN_POINT('Ctrl Pts',(-25.3545707061817,64.72765802224,64.051391343194));
#176839=CARTESIAN_POINT('Ctrl Pts',(-25.2099457943287,70.331750046873,60.1978610671));
#176840=CARTESIAN_POINT('Ctrl Pts',(-25.0653208824749,77.100997250995,59.53595519057));
#176841=CARTESIAN_POINT('Ctrl Pts',(-24.9689042745729,81.263224902643,61.33139849116));
#176842=CARTESIAN_POINT('Ctrl Pts',(-24.9206959706219,82.998435097713,62.6773649606));
#176843=CARTESIAN_POINT('Ctrl Pts',(-29.6712348137352,72.242088232536,85.74414017529));
#176844=CARTESIAN_POINT('Ctrl Pts',(-29.6230265097852,70.095650878086,85.28004229623));
#176845=CARTESIAN_POINT('Ctrl Pts',(-29.5266099018845,66.04485241176,83.24564128978));
#176846=CARTESIAN_POINT('Ctrl Pts',(-29.3819849900345,62.20076662219,77.634595795182));
#176847=CARTESIAN_POINT('Ctrl Pts',(-29.2373600781752,61.55056525346,70.864604569967));
#176848=CARTESIAN_POINT('Ctrl Pts',(-29.0927351663245,64.25574478693,64.624573520997));
#176849=CARTESIAN_POINT('Ctrl Pts',(-28.9481102544736,69.641577033905,60.47138590026));
#176850=CARTESIAN_POINT('Ctrl Pts',(-28.8034853426145,76.364284952381,59.44121987509));
#176851=CARTESIAN_POINT('Ctrl Pts',(-28.6588604307645,82.746616870673,61.79109721394));
#176852=CARTESIAN_POINT('Ctrl Pts',(-28.5142355189052,87.19622473785,66.934740200613));
#176853=CARTESIAN_POINT('Ctrl Pts',(-28.3696106070545,88.60296550284,73.5888484027236));
#176854=CARTESIAN_POINT('Ctrl Pts',(-28.2249856952036,86.61586754518,80.093271282679));
#176855=CARTESIAN_POINT('Ctrl Pts',(-28.0803607833445,81.730697090025,84.82520375033));
#176856=CARTESIAN_POINT('Ctrl Pts',(-27.9357358714945,75.1662677935533,
86.60406386368));
#176857=CARTESIAN_POINT('Ctrl Pts',(-27.7911109596436,68.560355920967,84.98603926299));
#176858=CARTESIAN_POINT('Ctrl Pts',(-27.6464860477845,63.56108732498,80.374815045269));
#176859=CARTESIAN_POINT('Ctrl Pts',(-27.5018611359345,61.41574231844,73.9208573383313));
#176860=CARTESIAN_POINT('Ctrl Pts',(-27.3572362240752,62.65956851573,67.234380562697));
#176861=CARTESIAN_POINT('Ctrl Pts',(-27.2126113122245,66.982240536617,61.98361091626));
#176862=CARTESIAN_POINT('Ctrl Pts',(-27.0679864003745,73.305283879178,59.47857635201));
#176863=CARTESIAN_POINT('Ctrl Pts',(-26.9233614885152,80.05114628266,60.34426435248));
#176864=CARTESIAN_POINT('Ctrl Pts',(-26.7787365766645,85.53678527666,64.36469220339));
#176865=CARTESIAN_POINT('Ctrl Pts',(-26.6341116648141,88.39357475485,70.536793074933));
#176866=CARTESIAN_POINT('Ctrl Pts',(-26.4894867529572,87.90876699715,77.320673726326));
#176867=CARTESIAN_POINT('Ctrl Pts',(-26.3448618411036,84.203317946944,83.02380642958));
#176868=CARTESIAN_POINT('Ctrl Pts',(-26.2002369292505,78.201709510007,86.22330197028));
#176869=CARTESIAN_POINT('Ctrl Pts',(-26.0556120173974,71.40129854677,86.12091018816));
#176870=CARTESIAN_POINT('Ctrl Pts',(-25.9109871055435,65.49873617875,82.742176443924));
#176871=CARTESIAN_POINT('Ctrl Pts',(-25.7663621936905,61.96667080937,76.930072003796));
#176872=CARTESIAN_POINT('Ctrl Pts',(-25.6217372818374,61.68631520576,70.134664941592));
#176873=CARTESIAN_POINT('Ctrl Pts',(-25.4771123699836,64.72765802224,64.051391343194));
#176874=CARTESIAN_POINT('Ctrl Pts',(-25.3324874581306,70.331750046873,60.1978610671));
#176875=CARTESIAN_POINT('Ctrl Pts',(-25.1878625462775,77.100997250995,59.53595519057));
#176876=CARTESIAN_POINT('Ctrl Pts',(-25.0914459383755,81.263224902643,61.33139849116));
#176877=CARTESIAN_POINT('Ctrl Pts',(-25.0432376344245,82.998435097713,62.6773649606));
#176878=CARTESIAN_POINT('Ctrl Pts',(-29.793776477544,72.242088232536,85.74414017529));
#176879=CARTESIAN_POINT('Ctrl Pts',(-29.745568173594,70.095650878086,85.28004229623));
#176880=CARTESIAN_POINT('Ctrl Pts',(-29.6491515656854,66.04485241176,83.24564128978));
#176881=CARTESIAN_POINT('Ctrl Pts',(-29.5045266538354,62.20076662219,77.634595795182));
#176882=CARTESIAN_POINT('Ctrl Pts',(-29.359901741984,61.55056525346,70.864604569967));
#176883=CARTESIAN_POINT('Ctrl Pts',(-29.2152768301254,64.25574478693,64.624573520997));
#176884=CARTESIAN_POINT('Ctrl Pts',(-29.0706519182754,69.641577033905,60.47138590026));
#176885=CARTESIAN_POINT('Ctrl Pts',(-28.9260270064154,76.364284952381,59.44121987509));
#176886=CARTESIAN_POINT('Ctrl Pts',(-28.7814020945654,82.746616870673,61.79109721394));
#176887=CARTESIAN_POINT('Ctrl Pts',(-28.636777182714,87.19622473785,66.934740200613));
#176888=CARTESIAN_POINT('Ctrl Pts',(-28.4921522708554,88.60296550284,73.5888484027236));
#176889=CARTESIAN_POINT('Ctrl Pts',(-28.3475273590054,86.61586754518,80.093271282679));
#176890=CARTESIAN_POINT('Ctrl Pts',(-28.2029024471454,81.730697090025,84.82520375033));
#176891=CARTESIAN_POINT('Ctrl Pts',(-28.0582775352954,75.1662677935533,
86.60406386368));
#176892=CARTESIAN_POINT('Ctrl Pts',(-27.9136526234454,68.560355920967,84.98603926299));
#176893=CARTESIAN_POINT('Ctrl Pts',(-27.7690277115854,63.56108732498,80.374815045269));
#176894=CARTESIAN_POINT('Ctrl Pts',(-27.6244027997354,61.41574231844,73.9208573383313));
#176895=CARTESIAN_POINT('Ctrl Pts',(-27.479777887884,62.65956851573,67.234380562697));
#176896=CARTESIAN_POINT('Ctrl Pts',(-27.3351529760254,66.982240536617,61.98361091626));
#176897=CARTESIAN_POINT('Ctrl Pts',(-27.1905280641754,73.305283879178,59.47857635201));
#176898=CARTESIAN_POINT('Ctrl Pts',(-27.045903152324,80.05114628266,60.34426435248));
#176899=CARTESIAN_POINT('Ctrl Pts',(-26.9012782404654,85.53678527666,64.36469220339));
#176900=CARTESIAN_POINT('Ctrl Pts',(-26.7566533286154,88.39357475485,70.536793074933));
#176901=CARTESIAN_POINT('Ctrl Pts',(-26.6120284167559,87.90876699715,77.320673726326));
#176902=CARTESIAN_POINT('Ctrl Pts',(-26.4674035049062,84.203317946944,83.02380642958));
#176903=CARTESIAN_POINT('Ctrl Pts',(-26.3227785930532,78.201709510007,86.22330197028));
#176904=CARTESIAN_POINT('Ctrl Pts',(-26.1781536811993,71.40129854677,86.12091018816));
#176905=CARTESIAN_POINT('Ctrl Pts',(-26.0335287693461,65.49873617875,82.742176443924));
#176906=CARTESIAN_POINT('Ctrl Pts',(-25.8889038574932,61.96667080937,76.930072003796));
#176907=CARTESIAN_POINT('Ctrl Pts',(-25.7442789456393,61.68631520576,70.134664941592));
#176908=CARTESIAN_POINT('Ctrl Pts',(-25.5996540337862,64.72765802224,64.051391343194));
#176909=CARTESIAN_POINT('Ctrl Pts',(-25.4550291219332,70.331750046873,60.1978610671));
#176910=CARTESIAN_POINT('Ctrl Pts',(-25.3104042100802,77.100997250995,59.53595519057));
#176911=CARTESIAN_POINT('Ctrl Pts',(-25.2139876021782,81.263224902643,61.33139849116));
#176912=CARTESIAN_POINT('Ctrl Pts',(-25.1657792982272,82.998435097713,62.6773649606));
#176913=CARTESIAN_POINT('Ctrl Pts',(-29.3655838523953,68.3986373253016,
84.2438270474911));
#176914=CARTESIAN_POINT('Ctrl Pts',(-29.3303036656744,67.0118618461396,
83.4317063126597));
#176915=CARTESIAN_POINT('Ctrl Pts',(-29.295627364516,65.7984777383591,82.3803230252724));
#176916=CARTESIAN_POINT('Ctrl Pts',(-29.2347381075076,64.0710938904411,
80.2099621171983));
#176917=CARTESIAN_POINT('Ctrl Pts',(-29.1967714573929,63.0876642002268,
78.7374991847509));
#176918=CARTESIAN_POINT('Ctrl Pts',(-29.1127653603425,62.0094805862012,
75.0668637575475));
#176919=CARTESIAN_POINT('Ctrl Pts',(-29.075894631943,61.849552996255,73.362907125417));
#176920=CARTESIAN_POINT('Ctrl Pts',(-28.9922442448893,62.2248483961828,
69.5720079624171));
#176921=CARTESIAN_POINT('Ctrl Pts',(-28.9538064145163,62.9148739729229,
67.918150971998));
#176922=CARTESIAN_POINT('Ctrl Pts',(-28.8854503569787,64.3835342434137,
65.1722907800826));
#176923=CARTESIAN_POINT('Ctrl Pts',(-28.8482263560423,65.5292543314931,
63.8773740095138));
#176924=CARTESIAN_POINT('Ctrl Pts',(-28.7869286879839,67.6922978786627,
62.1109491954587));
#176925=CARTESIAN_POINT('Ctrl Pts',(-28.749043597868,69.1574097871512,61.1249202595484));
#176926=CARTESIAN_POINT('Ctrl Pts',(-28.6656746731545,72.791210878067,60.0229950603654));
#176927=CARTESIAN_POINT('Ctrl Pts',(-28.6291541528474,74.4762656818076,
59.8442380189926));
#176928=CARTESIAN_POINT('Ctrl Pts',(-28.5552353989382,77.8296245530595,
60.1356096181981));
#176929=CARTESIAN_POINT('Ctrl Pts',(-28.5179385729896,79.4914698953371,
60.6227695423812));
#176930=CARTESIAN_POINT('Ctrl Pts',(-28.432590730343,82.9459183275816,62.4060056730255));
#176931=CARTESIAN_POINT('Ctrl Pts',(-28.3942903930222,84.2103440468305,
63.6694196806762));
#176932=CARTESIAN_POINT('Ctrl Pts',(-28.3368489710222,85.8953250158704,
65.6718124865958));
#176933=CARTESIAN_POINT('Ctrl Pts',(-28.2993959861414,86.8343667803122,
67.138410339181));
#176934=CARTESIAN_POINT('Ctrl Pts',(-28.2228502956742,87.8868735919899,
70.4626573346849));
#176935=CARTESIAN_POINT('Ctrl Pts',(-28.1861287854085,88.1538522357153,
72.1469332660725));
#176936=CARTESIAN_POINT('Ctrl Pts',(-28.1085461465717,87.8816167397,75.6693497096587));
#176937=CARTESIAN_POINT('Ctrl Pts',(-28.071489187918,87.4204639031838,77.326781740075));
#176938=CARTESIAN_POINT('Ctrl Pts',(-27.9868394695532,85.6965669402866,
80.7751238150649));
#176939=CARTESIAN_POINT('Ctrl Pts',(-27.9484187558418,84.4514930162676,
82.0646263543981));
#176940=CARTESIAN_POINT('Ctrl Pts',(-27.8840027503118,82.2328210086097,
83.9854448061145));
#176941=CARTESIAN_POINT('Ctrl Pts',(-27.8469128057308,80.7355565107899,
84.8353927582127));
#176942=CARTESIAN_POINT('Ctrl Pts',(-27.7827496034337,77.9600462808923,
85.7525454179823));
#176943=CARTESIAN_POINT('Ctrl Pts',(-27.7448787069659,76.2410030146933,
86.1552553504064));
#176944=CARTESIAN_POINT('Ctrl Pts',(-27.6613031356659,72.4438039999917,
85.8925693173151));
#176945=CARTESIAN_POINT('Ctrl Pts',(-27.6245645194847,70.7959511083946,
85.4545391189869));
#176946=CARTESIAN_POINT('Ctrl Pts',(-27.545723918875,67.5664106015694,83.8861011614419));
#176947=CARTESIAN_POINT('Ctrl Pts',(-27.5081701457295,66.2304310118682,
82.7623462776217));
#176948=CARTESIAN_POINT('Ctrl Pts',(-27.431506954629,63.9090167105023,80.1533697833607));
#176949=CARTESIAN_POINT('Ctrl Pts',(-27.3938450433659,63.1284302719079,
78.5852444941449));
#176950=CARTESIAN_POINT('Ctrl Pts',(-27.336564037718,62.2772781947343,76.1182439307806));
#176951=CARTESIAN_POINT('Ctrl Pts',(-27.2985997691107,61.8445740460357,
74.4007921117391));
#176952=CARTESIAN_POINT('Ctrl Pts',(-27.2144471677441,62.0716673767697,
70.5744157048113));
#176953=CARTESIAN_POINT('Ctrl Pts',(-27.1780151180435,62.4847242407732,
68.935483672655));
#176954=CARTESIAN_POINT('Ctrl Pts',(-27.1051166195486,63.8981388774045,
65.9319091457067));
#176955=CARTESIAN_POINT('Ctrl Pts',(-27.0686837698037,64.8969736487736,
64.5683559877304));
#176956=CARTESIAN_POINT('Ctrl Pts',(-26.9839443790261,67.7196119249671,
61.9357859485755));
#176957=CARTESIAN_POINT('Ctrl Pts',(-26.9459015379113,69.327603593445,61.1819992045566));
#176958=CARTESIAN_POINT('Ctrl Pts',(-26.8876102860954,71.813569601353,60.2477452459042));
#176959=CARTESIAN_POINT('Ctrl Pts',(-26.8502010969373,73.5127405961876,
59.8797505089315));
#176960=CARTESIAN_POINT('Ctrl Pts',(-26.776102883949,76.8860764812136,59.9992914624847));
#176961=CARTESIAN_POINT('Ctrl Pts',(-26.7384047115212,78.6141185724286,
60.295511445562));
#176962=CARTESIAN_POINT('Ctrl Pts',(-26.6585341496444,81.9242227082905,
61.8029934063736));
#176963=CARTESIAN_POINT('Ctrl Pts',(-26.6217434954712,83.3143614652629,
62.7946497723639));
#176964=CARTESIAN_POINT('Ctrl Pts',(-26.5367444780904,85.9809277806067,
65.6007532047945));
#176965=CARTESIAN_POINT('Ctrl Pts',(-26.4986415165783,86.7489790972207,
67.2052974950796));
#176966=CARTESIAN_POINT('Ctrl Pts',(-26.4362248200088,87.7833246297908,
69.8540188908578));
#176967=CARTESIAN_POINT('Ctrl Pts',(-26.399137480781,88.0825874756072,71.5493285777499));
#176968=CARTESIAN_POINT('Ctrl Pts',(-26.3345682468581,88.0180046780585,
74.4902614964474));
#176969=CARTESIAN_POINT('Ctrl Pts',(-26.2962027710616,87.8165600689918,
76.2685907288012));
#176970=CARTESIAN_POINT('Ctrl Pts',(-26.2116136533861,86.2603114685271,
79.7928374527051));
#176971=CARTESIAN_POINT('Ctrl Pts',(-26.1745142485159,85.2763652365629,
81.2065457467116));
#176972=CARTESIAN_POINT('Ctrl Pts',(-26.0976814723828,82.7596788106203,
83.6370669645292));
#176973=CARTESIAN_POINT('Ctrl Pts',(-26.061001678293,81.3005380198983,84.514815841502));
#176974=CARTESIAN_POINT('Ctrl Pts',(-25.9817789563582,77.9559060942714,
85.8700472606715));
#176975=CARTESIAN_POINT('Ctrl Pts',(-25.9440135851621,76.2063164733864,
86.0461011698092));
#176976=CARTESIAN_POINT('Ctrl Pts',(-25.8883468613302,73.6702296561183,
86.026800080011));
#176977=CARTESIAN_POINT('Ctrl Pts',(-25.8501294132486,71.8965454052951,
85.8493490383461));
#176978=CARTESIAN_POINT('Ctrl Pts',(-25.7675740621284,68.4365062298204,
84.3765890039499));
#176979=CARTESIAN_POINT('Ctrl Pts',(-25.7302992652139,66.9790706515215,
83.441711317101));
#176980=CARTESIAN_POINT('Ctrl Pts',(-25.6539646250139,64.5392499423534,
80.9658198961808));
#176981=CARTESIAN_POINT('Ctrl Pts',(-25.6173876023456,63.6010130518938,
79.5514735758964));
#176982=CARTESIAN_POINT('Ctrl Pts',(-25.5339424579599,62.1333165939061,
76.0457160962318));
#176983=CARTESIAN_POINT('Ctrl Pts',(-25.4960524688697,61.9605630472732,
74.2878474727087));
#176984=CARTESIAN_POINT('Ctrl Pts',(-25.4316021534887,61.9411497240743,
71.3516283557702));
#176985=CARTESIAN_POINT('Ctrl Pts',(-25.394425179123,62.2657958791927,69.6567021743647));
#176986=CARTESIAN_POINT('Ctrl Pts',(-25.3304167651469,63.3694437429962,
66.957686320141));
#176987=CARTESIAN_POINT('Ctrl Pts',(-25.2918432869613,64.1915570536306,
65.356393445582));
#176988=CARTESIAN_POINT('Ctrl Pts',(-25.2071469265163,66.9068391352455,
62.6169175361422));
#176989=CARTESIAN_POINT('Ctrl Pts',(-25.1702264504549,68.3236635254637,
61.6526283543061));
#176990=CARTESIAN_POINT('Ctrl Pts',(-25.0872961958142,71.7948914737712,
60.1648056900118));
#176991=CARTESIAN_POINT('Ctrl Pts',(-25.0495042431519,73.5443650049303,
59.9662747528024));
#176992=CARTESIAN_POINT('Ctrl Pts',(-24.9874702782534,76.3698133569276,
59.9123510791511));
#176993=CARTESIAN_POINT('Ctrl Pts',(-24.9527649126985,77.9545502963124,
60.1778193699471));
#176994=CARTESIAN_POINT('Ctrl Pts',(-24.9175248385795,79.4626737065055,
60.7277865984719));
#176995=CARTESIAN_POINT('Ctrl Pts',(-24.5840827087049,74.5742912897478,
60.79818693484));
#176996=CARTESIAN_POINT('Ctrl Pts',(-24.5542910420379,75.8420333362322,
60.75391640706));
#176997=CARTESIAN_POINT('Ctrl Pts',(-24.4947077087039,78.39120740833,61.06410883866));
#176998=CARTESIAN_POINT('Ctrl Pts',(-24.4053327087039,81.887755584948,62.68064695513));
#176999=CARTESIAN_POINT('Ctrl Pts',(-24.3159577087039,84.719288560893,65.292377040265));
#177000=CARTESIAN_POINT('Ctrl Pts',(-24.2265827087039,86.61250404011,68.647152239787));
#177001=CARTESIAN_POINT('Ctrl Pts',(-24.1372077087039,87.38460819383,72.4210925622802));
#177002=CARTESIAN_POINT('Ctrl Pts',(-24.0478327087039,86.9610641626,76.249849747832));
#177003=CARTESIAN_POINT('Ctrl Pts',(-23.9584577087039,85.38276101444,79.7637835434));
#177004=CARTESIAN_POINT('Ctrl Pts',(-23.8690827087039,82.802073437376,82.623647685499));
#177005=CARTESIAN_POINT('Ctrl Pts',(-23.7797077087039,79.468149063245,84.55334187238));
#177006=CARTESIAN_POINT('Ctrl Pts',(-23.6903327087039,75.702855490151,85.36656733984));
#177007=CARTESIAN_POINT('Ctrl Pts',(-23.6009577087039,71.869706029794,84.98481273641));
#177008=CARTESIAN_POINT('Ctrl Pts',(-23.5115827087039,68.338765023158,83.44493385557));
#177009=CARTESIAN_POINT('Ctrl Pts',(-23.4222077087039,65.450920651772,80.895595461536));
#177010=CARTESIAN_POINT('Ctrl Pts',(-23.3328327087039,63.48497452013,77.582918723914));
#177011=CARTESIAN_POINT('Ctrl Pts',(-23.2434577087039,62.63072526867,73.8267199037071));
#177012=CARTESIAN_POINT('Ctrl Pts',(-23.1540827087039,62.97064481461,69.989634282714));
#177013=CARTESIAN_POINT('Ctrl Pts',(-23.0647077087039,64.47191625279,66.442106209615));
#177014=CARTESIAN_POINT('Ctrl Pts',(-22.9753327087039,66.98960210332,63.5266252341));
#177015=CARTESIAN_POINT('Ctrl Pts',(-22.8859577087039,70.280637032969,61.52466108548));
#177016=CARTESIAN_POINT('Ctrl Pts',(-22.7965827087039,74.0272941491374,
60.62948969719));
#177017=CARTESIAN_POINT('Ctrl Pts',(-22.7072077087039,77.867859356231,60.92753373859));
#177018=CARTESIAN_POINT('Ctrl Pts',(-22.6178327087039,81.431552375351,62.39001909784));
#177019=CARTESIAN_POINT('Ctrl Pts',(-22.5284577087039,84.374323041932,64.875752825426));
#177020=CARTESIAN_POINT('Ctrl Pts',(-22.4390827087039,86.41206699382,68.144754346856));
#177021=CARTESIAN_POINT('Ctrl Pts',(-22.3497077087039,87.34805400249,71.881423944257));
#177022=CARTESIAN_POINT('Ctrl Pts',(-22.2603327087039,87.09192092988,75.725011748597));
#177023=CARTESIAN_POINT('Ctrl Pts',(-22.1709577087039,85.6683956707,79.304445669906));
#177024=CARTESIAN_POINT('Ctrl Pts',(-22.0815827087039,83.214909843509,82.274155867271));
#177025=CARTESIAN_POINT('Ctrl Pts',(-21.9922077087039,79.968330708787,84.34743715126));
#177026=CARTESIAN_POINT('Ctrl Pts',(-21.9028327087039,76.242093256469,85.32412840723));
#177027=CARTESIAN_POINT('Ctrl Pts',(-21.8134577087039,72.395940203395,85.10993678068));
#177028=CARTESIAN_POINT('Ctrl Pts',(-21.7240827087039,68.801191296739,83.72554100684));
#177029=CARTESIAN_POINT('Ctrl Pts',(-21.6347077087039,65.804894934405,81.304595020325));
#177030=CARTESIAN_POINT('Ctrl Pts',(-21.5453327087049,63.69632301805,78.080824582763));
#177031=CARTESIAN_POINT('Ctrl Pts',(-21.4559577087049,62.67904373127,74.365462660522));
#177032=CARTESIAN_POINT('Ctrl Pts',(-21.3665827087049,62.8512684251,70.517202012466));
#177033=CARTESIAN_POINT('Ctrl Pts',(-21.2772077087049,64.19636998435,66.907565859634));
#177034=CARTESIAN_POINT('Ctrl Pts',(-21.1878327087049,66.584488061824,63.885039861635));
#177035=CARTESIAN_POINT('Ctrl Pts',(-21.0984577087049,69.785066205781,61.74142821188));
#177036=CARTESIAN_POINT('Ctrl Pts',(-21.0090827087049,73.489110507031,60.68368194036));
#177037=CARTESIAN_POINT('Ctrl Pts',(-20.9197077087049,77.339020845536,60.81391920844));
#177038=CARTESIAN_POINT('Ctrl Pts',(-20.8303327087049,80.963114733938,62.11956649947));
#177039=CARTESIAN_POINT('Ctrl Pts',(-20.7409577087049,84.011510717237,64.474572505729));
#177040=CARTESIAN_POINT('Ctrl Pts',(-20.6515827087049,86.18990703204,67.651577519286));
#177041=CARTESIAN_POINT('Ctrl Pts',(-20.5622077087049,87.28799442708,71.343863455311));
#177042=CARTESIAN_POINT('Ctrl Pts',(-20.4728327087049,87.19976008168,75.194965383434));
#177043=CARTESIAN_POINT('Ctrl Pts',(-20.3834577087049,85.93372241786,78.833085776478));
#177044=CARTESIAN_POINT('Ctrl Pts',(-20.2940827087049,83.612108704975,81.90698901644));
#177045=CARTESIAN_POINT('Ctrl Pts',(-20.2047077087049,80.459054853646,84.11991078892));
#177046=CARTESIAN_POINT('Ctrl Pts',(-20.1153327087049,76.77896662795,85.25820864606));
#177047=CARTESIAN_POINT('Ctrl Pts',(-20.0259577087049,72.92713135283,85.21198772236));
#177048=CARTESIAN_POINT('Ctrl Pts',(-19.9365827087049,69.275417355079,83.98571033155));
#177049=CARTESIAN_POINT('Ctrl Pts',(-19.8472077087049,66.176372622231,81.697765160933));
#177050=CARTESIAN_POINT('Ctrl Pts',(-19.7578327087049,63.9291887075,78.569037653464));
#177051=CARTESIAN_POINT('Ctrl Pts',(-19.6684577087049,62.75081583481,74.90158503273));
#177052=CARTESIAN_POINT('Ctrl Pts',(-19.5790827087049,62.75501783514,71.049474737007));
#177053=CARTESIAN_POINT('Ctrl Pts',(-19.4897077087049,63.94138904505,67.384601665003));
#177054=CARTESIAN_POINT('Ctrl Pts',(-19.4003327087049,66.195393405158,64.260784146057));
#177055=CARTESIAN_POINT('Ctrl Pts',(-19.3109577087049,69.299422377156,61.97960566264));
#177056=CARTESIAN_POINT('Ctrl Pts',(-19.2215827087049,72.953802645656,60.7612973129));
#177057=CARTESIAN_POINT('Ctrl Pts',(-19.1322077087049,76.805730932023,60.72348241298));
#177058=CARTESIAN_POINT('Ctrl Pts',(-19.0428327087049,80.48332202154,61.86979685924));
#177059=CARTESIAN_POINT('Ctrl Pts',(-18.9534577087039,83.631559184886,64.089627347503));
#177060=CARTESIAN_POINT('Ctrl Pts',(-18.8938743753709,85.17478074676,66.1421806368));
#177061=CARTESIAN_POINT('Ctrl Pts',(-18.8640827087039,85.7703123683,67.262212718386));
#177062=CARTESIAN_POINT('Ctrl Pts',(-24.7409006782679,74.5637780077301,
60.49712592814));
#177063=CARTESIAN_POINT('Ctrl Pts',(-24.7111090116019,75.8628281513697,
60.45176209751));
#177064=CARTESIAN_POINT('Ctrl Pts',(-24.6515256782679,78.47495650485,60.76961502662));
#177065=CARTESIAN_POINT('Ctrl Pts',(-24.5621506782679,82.057855268582,62.42607509136));
#177066=CARTESIAN_POINT('Ctrl Pts',(-24.4727756782679,84.95931564794,65.102304338201));
#177067=CARTESIAN_POINT('Ctrl Pts',(-24.3834006782679,86.89928588639,68.539928906151));
#177068=CARTESIAN_POINT('Ctrl Pts',(-24.2940256782679,87.6904578875,72.4070702789702));
#177069=CARTESIAN_POINT('Ctrl Pts',(-24.2046506782679,87.25645403306,76.330382269486));
#177070=CARTESIAN_POINT('Ctrl Pts',(-24.1152756782679,85.63917318558,79.931096006583));
#177071=CARTESIAN_POINT('Ctrl Pts',(-24.0259006782679,82.994753071114,82.861587217225));
#177072=CARTESIAN_POINT('Ctrl Pts',(-23.9365256782679,79.578494259545,84.83893703977));
#177073=CARTESIAN_POINT('Ctrl Pts',(-23.8471506782679,75.7202131758358,
85.67224588461));
#177074=CARTESIAN_POINT('Ctrl Pts',(-23.7577756782679,71.792400439106,85.28106348769));
#177075=CARTESIAN_POINT('Ctrl Pts',(-23.6684006782679,68.174259481666,83.70315583141));
#177076=CARTESIAN_POINT('Ctrl Pts',(-23.5790256782679,65.215097043329,81.090859097905));
#177077=CARTESIAN_POINT('Ctrl Pts',(-23.4896506782679,63.20059999972,77.696372653464));
#177078=CARTESIAN_POINT('Ctrl Pts',(-23.4002756782679,62.32525424947,73.8474109262253));
#177079=CARTESIAN_POINT('Ctrl Pts',(-23.3109006782679,62.67356843231,69.915564821625));
#177080=CARTESIAN_POINT('Ctrl Pts',(-23.2215256782679,64.21191519837,66.280427164319));
#177081=CARTESIAN_POINT('Ctrl Pts',(-23.1321506782679,66.791777698665,63.292945609594));
#177082=CARTESIAN_POINT('Ctrl Pts',(-23.0427756782679,70.164087870074,61.24154104977));
#177083=CARTESIAN_POINT('Ctrl Pts',(-22.9534006782679,74.0032722518053,
60.32426255155));
#177084=CARTESIAN_POINT('Ctrl Pts',(-22.8640256782679,77.938683874199,60.62966707439));
#177085=CARTESIAN_POINT('Ctrl Pts',(-22.7746506782679,81.590385686263,62.12826990236));
#177086=CARTESIAN_POINT('Ctrl Pts',(-22.6852756782679,84.605830876964,64.675391191609));
#177087=CARTESIAN_POINT('Ctrl Pts',(-22.5959006782679,86.69389885636,68.0251238188));
#177088=CARTESIAN_POINT('Ctrl Pts',(-22.5065256782679,87.65300095559,71.854074030477));
#177089=CARTESIAN_POINT('Ctrl Pts',(-22.4171506782679,87.39054243283,75.792582896034));
#177090=CARTESIAN_POINT('Ctrl Pts',(-22.3277756782679,85.93186186169,79.460414346857));
#177091=CARTESIAN_POINT('Ctrl Pts',(-22.2384006782679,83.417784865457,82.503464365711));
#177092=CARTESIAN_POINT('Ctrl Pts',(-22.1490256782679,80.091028367167,84.62794730547));
#177093=CARTESIAN_POINT('Ctrl Pts',(-22.0596506782679,76.272767932331,85.62875888215));
#177094=CARTESIAN_POINT('Ctrl Pts',(-21.9702756782679,72.331630466779,85.4092775894));
#177095=CARTESIAN_POINT('Ctrl Pts',(-21.8809006782679,68.648105812461,83.99069284351));
#177096=CARTESIAN_POINT('Ctrl Pts',(-21.7915256782679,65.577813057976,81.509959290305));
#177097=CARTESIAN_POINT('Ctrl Pts',(-21.7021506782679,63.41716795007,78.206574771673));
#177098=CARTESIAN_POINT('Ctrl Pts',(-21.6127756782679,62.37476598252,74.399458448487));
#177099=CARTESIAN_POINT('Ctrl Pts',(-21.5234006782689,62.55124392917,70.456161338886));
#177100=CARTESIAN_POINT('Ctrl Pts',(-21.4340256782689,63.92956405242,66.757381783671));
#177101=CARTESIAN_POINT('Ctrl Pts',(-21.3446506782689,66.376658980107,63.660211627688));
#177102=CARTESIAN_POINT('Ctrl Pts',(-21.2552756782689,69.656278449357,61.4636614468));
#177103=CARTESIAN_POINT('Ctrl Pts',(-21.1659006782689,73.451797652123,60.37979312378));
#177104=CARTESIAN_POINT('Ctrl Pts',(-21.0765256782689,77.396785192848,60.51324672522));
#177105=CARTESIAN_POINT('Ctrl Pts',(-20.9871506782689,81.110379531183,61.85113821951));
#177106=CARTESIAN_POINT('Ctrl Pts',(-20.8977756782689,84.234058556389,64.264303341857));
#177107=CARTESIAN_POINT('Ctrl Pts',(-20.8084006782689,86.46625244275,67.519767519802));
#177108=CARTESIAN_POINT('Ctrl Pts',(-20.7190256782689,87.59145815176,71.303237973316));
#177109=CARTESIAN_POINT('Ctrl Pts',(-20.6296506782689,87.50104477518,75.2494465311));
#177110=CARTESIAN_POINT('Ctrl Pts',(-20.5402756782689,86.20374110555,78.977413771966));
#177111=CARTESIAN_POINT('Ctrl Pts',(-20.4509006782689,83.824792931074,82.127229979831));
#177112=CARTESIAN_POINT('Ctrl Pts',(-20.3615256782689,80.593871412118,84.39480196293));
#177113=CARTESIAN_POINT('Ctrl Pts',(-20.2721506782689,76.822899903006,85.5612111697));
#177114=CARTESIAN_POINT('Ctrl Pts',(-20.1827756782689,72.875939887522,85.51384877627));
#177115=CARTESIAN_POINT('Ctrl Pts',(-20.0934006782689,69.134043334935,84.25728729746));
#177116=CARTESIAN_POINT('Ctrl Pts',(-20.0040256782689,65.958464741074,81.912839141965));
#177117=CARTESIAN_POINT('Ctrl Pts',(-19.9146506782689,63.65578447949,78.706844729098));
#177118=CARTESIAN_POINT('Ctrl Pts',(-19.8252756782689,62.4483105665,74.948820873245));
#177119=CARTESIAN_POINT('Ctrl Pts',(-19.7359006782689,62.45261633923,71.001579045262));
#177120=CARTESIAN_POINT('Ctrl Pts',(-19.6465256782689,63.668286116,67.246198442551));
#177121=CARTESIAN_POINT('Ctrl Pts',(-19.5571506782689,65.977955260347,64.045235275048));
#177122=CARTESIAN_POINT('Ctrl Pts',(-19.4677756782689,69.158641183889,61.70772091653));
#177123=CARTESIAN_POINT('Ctrl Pts',(-19.3784006782689,72.903269853321,60.45932528185));
#177124=CARTESIAN_POINT('Ctrl Pts',(-19.2890256782679,76.850325177053,60.42057650697));
#177125=CARTESIAN_POINT('Ctrl Pts',(-19.1996506782679,80.618737880831,61.59520028015));
#177126=CARTESIAN_POINT('Ctrl Pts',(-19.1102756782679,83.844723759108,63.869851596353));
#177127=CARTESIAN_POINT('Ctrl Pts',(-19.0506923449349,85.42605664712,65.973094643852));
#177128=CARTESIAN_POINT('Ctrl Pts',(-19.0209006782679,86.0362954892,67.120786984341));
#177129=CARTESIAN_POINT('Ctrl Pts',(-24.8977186478319,74.5532647257124,
60.19606492144));
#177130=CARTESIAN_POINT('Ctrl Pts',(-24.8679269811659,75.8836229665074,
60.14960778797));
#177131=CARTESIAN_POINT('Ctrl Pts',(-24.8083436478319,78.558705601371,60.47512121458));
#177132=CARTESIAN_POINT('Ctrl Pts',(-24.7189686478319,82.227954952215,62.1715032276));
#177133=CARTESIAN_POINT('Ctrl Pts',(-24.6295936478319,85.19934273499,64.912231636138));
#177134=CARTESIAN_POINT('Ctrl Pts',(-24.5402186478319,87.18606773268,68.432705572515));
#177135=CARTESIAN_POINT('Ctrl Pts',(-24.4508436478319,87.99630758116,72.393047995661));
#177136=CARTESIAN_POINT('Ctrl Pts',(-24.3614686478319,87.55184390352,76.41091479114));
#177137=CARTESIAN_POINT('Ctrl Pts',(-24.2720936478319,85.89558535672,80.098408469768));
#177138=CARTESIAN_POINT('Ctrl Pts',(-24.1827186478319,83.187432704849,83.09952674895));
#177139=CARTESIAN_POINT('Ctrl Pts',(-24.0933436478319,79.688839455842,85.12453220716));
#177140=CARTESIAN_POINT('Ctrl Pts',(-24.0039686478319,75.7375708615167,
85.97792442938));
#177141=CARTESIAN_POINT('Ctrl Pts',(-23.9145936478319,71.715094848414,85.57731423897));
#177142=CARTESIAN_POINT('Ctrl Pts',(-23.8252186478319,68.00975394017,83.96137780724));
#177143=CARTESIAN_POINT('Ctrl Pts',(-23.7358436478319,64.97927343488,81.286122734268));
#177144=CARTESIAN_POINT('Ctrl Pts',(-23.6464686478319,62.91622547931,77.809826583006));
#177145=CARTESIAN_POINT('Ctrl Pts',(-23.5570936478319,62.01978323026,73.8681019487347));
#177146=CARTESIAN_POINT('Ctrl Pts',(-23.4677186478319,62.37649205001,69.841495360525));
#177147=CARTESIAN_POINT('Ctrl Pts',(-23.3783436478319,63.95191414396,66.118748119013));
#177148=CARTESIAN_POINT('Ctrl Pts',(-23.2889686478319,66.593953294018,63.059265985079));
#177149=CARTESIAN_POINT('Ctrl Pts',(-23.1995936478319,70.047538707191,60.95842101407));
#177150=CARTESIAN_POINT('Ctrl Pts',(-23.1102186478319,73.979250354488,60.01903540591));
#177151=CARTESIAN_POINT('Ctrl Pts',(-23.0208436478319,78.009508392183,60.33180041019));
#177152=CARTESIAN_POINT('Ctrl Pts',(-22.9314686478319,81.749218997189,61.8665207069));
#177153=CARTESIAN_POINT('Ctrl Pts',(-22.8420936478319,84.837338712008,64.475029557805));
#177154=CARTESIAN_POINT('Ctrl Pts',(-22.7527186478319,86.97573071891,67.905493290763));
#177155=CARTESIAN_POINT('Ctrl Pts',(-22.6633436478319,87.95794790869,71.826724116717));
#177156=CARTESIAN_POINT('Ctrl Pts',(-22.5739686478319,87.68916393577,75.860154043494));
#177157=CARTESIAN_POINT('Ctrl Pts',(-22.4845936478319,86.19532805268,79.616383023829));
#177158=CARTESIAN_POINT('Ctrl Pts',(-22.3952186478319,83.620659887387,82.732772864167));
#177159=CARTESIAN_POINT('Ctrl Pts',(-22.3058436478319,80.213726025524,84.90845745969));
#177160=CARTESIAN_POINT('Ctrl Pts',(-22.2164686478319,76.303442608167,85.93338935707));
#177161=CARTESIAN_POINT('Ctrl Pts',(-22.1270936478319,72.267320730135,85.70861839811));
#177162=CARTESIAN_POINT('Ctrl Pts',(-22.0377186478319,68.495020328158,84.25584468017));
#177163=CARTESIAN_POINT('Ctrl Pts',(-21.9483436478319,65.350731181526,81.715323560263));
#177164=CARTESIAN_POINT('Ctrl Pts',(-21.8589686478319,63.13801288209,78.332324960555));
#177165=CARTESIAN_POINT('Ctrl Pts',(-21.7695936478319,62.07048823376,74.43345423642));
#177166=CARTESIAN_POINT('Ctrl Pts',(-21.6802186478319,62.25121943325,70.395120665275));
#177167=CARTESIAN_POINT('Ctrl Pts',(-21.5908436478319,63.6627581205,66.607197707679));
#177168=CARTESIAN_POINT('Ctrl Pts',(-21.5014686478319,66.168829898414,63.435383393718));
#177169=CARTESIAN_POINT('Ctrl Pts',(-21.4120936478329,69.527490692963,61.18589468171));
#177170=CARTESIAN_POINT('Ctrl Pts',(-21.3227186478329,73.414484797248,60.07590430719));
#177171=CARTESIAN_POINT('Ctrl Pts',(-21.2333436478329,77.454549540195,60.212574242));
#177172=CARTESIAN_POINT('Ctrl Pts',(-21.1439686478329,81.257644328458,61.58270993957));
#177173=CARTESIAN_POINT('Ctrl Pts',(-21.0545936478329,84.456606395566,64.054034178009));
#177174=CARTESIAN_POINT('Ctrl Pts',(-20.9652186478329,86.74259785348,67.387957520349));
#177175=CARTESIAN_POINT('Ctrl Pts',(-20.8758436478329,87.89492187645,71.262612491355));
#177176=CARTESIAN_POINT('Ctrl Pts',(-20.7864686478329,87.80232946867,75.3039276788));
#177177=CARTESIAN_POINT('Ctrl Pts',(-20.6970936478329,86.47375979323,79.121741767484));
#177178=CARTESIAN_POINT('Ctrl Pts',(-20.6077186478329,84.03747715715,82.347470943245));
#177179=CARTESIAN_POINT('Ctrl Pts',(-20.5183436478329,80.728687970562,84.66969313695));
#177180=CARTESIAN_POINT('Ctrl Pts',(-20.4289686478329,76.866833178031,85.86421369334));
#177181=CARTESIAN_POINT('Ctrl Pts',(-20.3395936478329,72.824748422185,85.81570983017));
#177182=CARTESIAN_POINT('Ctrl Pts',(-20.2502186478329,68.992669314766,84.52886426336));
#177183=CARTESIAN_POINT('Ctrl Pts',(-20.1608436478329,65.740556859899,82.127913122978));
#177184=CARTESIAN_POINT('Ctrl Pts',(-20.0714686478329,63.38238025148,78.844651804709));
#177185=CARTESIAN_POINT('Ctrl Pts',(-19.9820936478329,62.14580529819,74.996056713737));
#177186=CARTESIAN_POINT('Ctrl Pts',(-19.8927186478329,62.15021484332,70.953683353497));
#177187=CARTESIAN_POINT('Ctrl Pts',(-19.8033436478329,63.39518318695,67.107795220083));
#177188=CARTESIAN_POINT('Ctrl Pts',(-19.7139686478329,65.760517115547,63.829686404028));
#177189=CARTESIAN_POINT('Ctrl Pts',(-19.6245936478329,69.017859990633,61.43583617042));
#177190=CARTESIAN_POINT('Ctrl Pts',(-19.5352186478319,72.852737060995,60.15735325081));
#177191=CARTESIAN_POINT('Ctrl Pts',(-19.4458436478319,76.894919422089,60.11767060096));
#177192=CARTESIAN_POINT('Ctrl Pts',(-19.3564686478319,80.754153740124,61.32060370107));
#177193=CARTESIAN_POINT('Ctrl Pts',(-19.2670936478319,84.05788833333,63.650075845204));
#177194=CARTESIAN_POINT('Ctrl Pts',(-19.2075103144989,85.67733254748,65.804008650901));
#177195=CARTESIAN_POINT('Ctrl Pts',(-19.1777186478319,86.3022786101,66.979361250291));
#177196=CARTESIAN_POINT('Ctrl Pts',(-25.0545366173959,74.5427514436947,
59.89500391474));
#177197=CARTESIAN_POINT('Ctrl Pts',(-25.0247449507299,75.9044177816449,
59.84745347843));
#177198=CARTESIAN_POINT('Ctrl Pts',(-24.9651616173959,78.642454697891,60.18062740255));
#177199=CARTESIAN_POINT('Ctrl Pts',(-24.8757866173959,82.398054635848,61.91693136384));
#177200=CARTESIAN_POINT('Ctrl Pts',(-24.7864116173959,85.43936982203,64.722158934074));
#177201=CARTESIAN_POINT('Ctrl Pts',(-24.6970366173959,87.47284957896,68.325482238879));
#177202=CARTESIAN_POINT('Ctrl Pts',(-24.6076616173959,88.30215727482,72.379025712351));
#177203=CARTESIAN_POINT('Ctrl Pts',(-24.5182866173959,87.84723377397,76.491447312794));
#177204=CARTESIAN_POINT('Ctrl Pts',(-24.4289116173959,86.15199752785,80.265720932952));
#177205=CARTESIAN_POINT('Ctrl Pts',(-24.3395366173959,83.380112338587,83.33746628068));
#177206=CARTESIAN_POINT('Ctrl Pts',(-24.2501616173959,79.799184652141,85.41012737455));
#177207=CARTESIAN_POINT('Ctrl Pts',(-24.1607866173959,75.7549285472015,
86.28360297416));
#177208=CARTESIAN_POINT('Ctrl Pts',(-24.0714116173959,71.637789257726,85.87356499026));
#177209=CARTESIAN_POINT('Ctrl Pts',(-23.9820366173959,67.845248398678,84.21959978308));
#177210=CARTESIAN_POINT('Ctrl Pts',(-23.8926616173959,64.74344982644,81.481386370637));
#177211=CARTESIAN_POINT('Ctrl Pts',(-23.8032866173959,62.6318509589,77.923280512555));
#177212=CARTESIAN_POINT('Ctrl Pts',(-23.7139116173959,61.71431221106,73.8887929712528));
#177213=CARTESIAN_POINT('Ctrl Pts',(-23.6245366173959,62.07941566771,69.767425899435));
#177214=CARTESIAN_POINT('Ctrl Pts',(-23.5351616173959,63.69191308954,65.957069073716));
#177215=CARTESIAN_POINT('Ctrl Pts',(-23.4457866173959,66.396128889362,62.82558636057));
#177216=CARTESIAN_POINT('Ctrl Pts',(-23.3564116173959,69.930989544296,60.67530097837));
#177217=CARTESIAN_POINT('Ctrl Pts',(-23.2670366173959,73.955228457156,59.71380826027));
#177218=CARTESIAN_POINT('Ctrl Pts',(-23.1776616173959,78.080332910152,60.03393374599));
#177219=CARTESIAN_POINT('Ctrl Pts',(-23.0882866173959,81.908052308101,61.60477151142));
#177220=CARTESIAN_POINT('Ctrl Pts',(-22.9989116173959,85.06884654704,64.274667923988));
#177221=CARTESIAN_POINT('Ctrl Pts',(-22.9095366173959,87.25756258145,67.785862762707));
#177222=CARTESIAN_POINT('Ctrl Pts',(-22.8201616173959,88.26289486179,71.799374202937));
#177223=CARTESIAN_POINT('Ctrl Pts',(-22.7307866173959,87.98778543871,75.927725190932));
#177224=CARTESIAN_POINT('Ctrl Pts',(-22.6414116173959,86.45879424367,79.77235170078));
#177225=CARTESIAN_POINT('Ctrl Pts',(-22.5520366173959,83.823534909334,82.962081362607));
#177226=CARTESIAN_POINT('Ctrl Pts',(-22.4626616173959,80.336423683903,85.1889676139));
#177227=CARTESIAN_POINT('Ctrl Pts',(-22.3732866173959,76.334117284029,86.23801983199));
#177228=CARTESIAN_POINT('Ctrl Pts',(-22.2839116173959,72.203010993519,86.00795920683));
#177229=CARTESIAN_POINT('Ctrl Pts',(-22.1945366173959,68.34193484388,84.52099651684));
#177230=CARTESIAN_POINT('Ctrl Pts',(-22.1051616173959,65.123649305097,81.920687830243));
#177231=CARTESIAN_POINT('Ctrl Pts',(-22.0157866173959,62.85885781411,78.458075149464));
#177232=CARTESIAN_POINT('Ctrl Pts',(-21.9264116173959,61.766210485,74.467450024384));
#177233=CARTESIAN_POINT('Ctrl Pts',(-21.8370366173959,61.95119493732,70.334079991696));
#177234=CARTESIAN_POINT('Ctrl Pts',(-21.7476616173959,63.39595218857,66.457013631716));
#177235=CARTESIAN_POINT('Ctrl Pts',(-21.6582866173959,65.961000816697,63.210555159771));
#177236=CARTESIAN_POINT('Ctrl Pts',(-21.5689116173959,69.398702936539,60.90812791663));
#177237=CARTESIAN_POINT('Ctrl Pts',(-21.4795366173959,73.377171942341,59.7720154906));
#177238=CARTESIAN_POINT('Ctrl Pts',(-21.3901616173959,77.512313887507,59.91190175878));
#177239=CARTESIAN_POINT('Ctrl Pts',(-21.3007866173969,81.404909125703,61.31428165962));
#177240=CARTESIAN_POINT('Ctrl Pts',(-21.2114116173969,84.679154234719,63.843765014137));
#177241=CARTESIAN_POINT('Ctrl Pts',(-21.1220366173969,87.0189432642,67.256147520865));
#177242=CARTESIAN_POINT('Ctrl Pts',(-21.0326616173969,88.19838560114,71.22198700936));
#177243=CARTESIAN_POINT('Ctrl Pts',(-20.9432866173969,88.10361416217,75.358408826466));
#177244=CARTESIAN_POINT('Ctrl Pts',(-20.8539116173969,86.74377848093,79.266069762973));
#177245=CARTESIAN_POINT('Ctrl Pts',(-20.7645366173969,84.25016138325,82.567711906636));
#177246=CARTESIAN_POINT('Ctrl Pts',(-20.6751616173969,80.863504529035,84.94458431096));
#177247=CARTESIAN_POINT('Ctrl Pts',(-20.5857866173969,76.910766453087,86.16721621697));
#177248=CARTESIAN_POINT('Ctrl Pts',(-20.4964116173969,72.773556956877,86.11757088408));
#177249=CARTESIAN_POINT('Ctrl Pts',(-20.4070366173969,68.851295294622,84.80044122928));
#177250=CARTESIAN_POINT('Ctrl Pts',(-20.3176616173969,65.522648978742,82.34298710401));
#177251=CARTESIAN_POINT('Ctrl Pts',(-20.2282866173969,63.10897602347,78.982458880342));
#177252=CARTESIAN_POINT('Ctrl Pts',(-20.1389116173969,61.84330002988,75.043292554251));
#177253=CARTESIAN_POINT('Ctrl Pts',(-20.0495366173969,61.84781334742,70.905787661752));
#177254=CARTESIAN_POINT('Ctrl Pts',(-19.9601616173959,63.12208025789,66.969391997631));
#177255=CARTESIAN_POINT('Ctrl Pts',(-19.8707866173959,65.543078970735,63.614137533019));
#177256=CARTESIAN_POINT('Ctrl Pts',(-19.7814116173959,68.877078797366,61.16395142431));
#177257=CARTESIAN_POINT('Ctrl Pts',(-19.6920366173959,72.80220426866,59.85538121976));
#177258=CARTESIAN_POINT('Ctrl Pts',(-19.6026616173959,76.939513667119,59.81476469495));
#177259=CARTESIAN_POINT('Ctrl Pts',(-19.5132866173959,80.889569599415,61.04600712199));
#177260=CARTESIAN_POINT('Ctrl Pts',(-19.4239116173959,84.271052907552,63.430300094054));
#177261=CARTESIAN_POINT('Ctrl Pts',(-19.3643282840629,85.92860844783,65.634922657953));
#177262=CARTESIAN_POINT('Ctrl Pts',(-19.3345366173959,86.568261731,66.837935516246));
#177263=CARTESIAN_POINT('Ctrl Pts',(-19.0011309998534,82.8754003805133,
63.605888350301));
#177264=CARTESIAN_POINT('Ctrl Pts',(-19.0704950494351,82.9610760105436,
63.5038382511702));
#177265=CARTESIAN_POINT('Ctrl Pts',(-19.1398591055042,83.0467520694653,
63.4017884960521));
#177266=CARTESIAN_POINT('Ctrl Pts',(-19.2784798309862,83.2179723873018,
63.1978476809956));
#177267=CARTESIAN_POINT('Ctrl Pts',(-19.3477365217846,83.3035166713306,
63.0959565885018));
#177268=CARTESIAN_POINT('Ctrl Pts',(-19.4169932345698,83.3890614012314,
62.9940658153935));
#177269=CARTESIAN_POINT('',(-24.5011471556111,79.1897367105132,61.4776867539786));
#177270=CARTESIAN_POINT('Ctrl Pts',(-18.9799062324529,82.659284818849,63.474668109995));
#177271=CARTESIAN_POINT('Ctrl Pts',(-18.9294356932999,84.248501099275,64.932060456454));
#177272=CARTESIAN_POINT('Ctrl Pts',(-18.8284946149979,86.5752695444,68.654743887637));
#177273=CARTESIAN_POINT('Ctrl Pts',(-18.7275535366989,86.69361007784,72.8921974616309));
#177274=CARTESIAN_POINT('Ctrl Pts',(-18.6770829975479,86.22929765373,74.847875926051));
#177275=CARTESIAN_POINT('Ctrl Pts',(-19.1367242020169,82.848190368771,63.240013146138));
#177276=CARTESIAN_POINT('Ctrl Pts',(-19.0862536628639,84.478747085231,64.730686006568));
#177277=CARTESIAN_POINT('Ctrl Pts',(-18.9853125845619,86.87012683464,68.542252716656));
#177278=CARTESIAN_POINT('Ctrl Pts',(-18.8843715062629,86.99947754428,72.8890389661518));
#177279=CARTESIAN_POINT('Ctrl Pts',(-18.8339009671119,86.52649715737,74.897076676965));
#177280=CARTESIAN_POINT('Ctrl Pts',(-19.2935421715809,83.037095918694,63.005358182281));
#177281=CARTESIAN_POINT('Ctrl Pts',(-19.2430716324269,84.708993071182,64.529311556686));
#177282=CARTESIAN_POINT('Ctrl Pts',(-19.1421305541259,87.16498412488,68.429761545683));
#177283=CARTESIAN_POINT('Ctrl Pts',(-19.0411894758269,87.3053450107,72.8858804706761));
#177284=CARTESIAN_POINT('Ctrl Pts',(-18.9907189366759,86.823696661,74.94627742788));
#177285=CARTESIAN_POINT('Ctrl Pts',(-19.4503601411449,83.226001468616,62.77070321842));
#177286=CARTESIAN_POINT('Ctrl Pts',(-19.3998896019909,84.939239057138,64.327937106799));
#177287=CARTESIAN_POINT('Ctrl Pts',(-19.2989485236899,87.45984141513,68.317270374702));
#177288=CARTESIAN_POINT('Ctrl Pts',(-19.1980074453909,87.61121247713,72.8827219751971));
#177289=CARTESIAN_POINT('Ctrl Pts',(-19.1475369062399,87.12089616464,74.995478178794));
#177290=CARTESIAN_POINT('Ctrl Pts',(-19.4175174361238,83.388929634868,62.9926155500965));
#177291=CARTESIAN_POINT('Ctrl Pts',(-19.4032204672393,83.8621876848378,
63.4414112721832));
#177292=CARTESIAN_POINT('Ctrl Pts',(-19.3888608262415,84.3009905168755,
63.9263196278537));
#177293=CARTESIAN_POINT('Ctrl Pts',(-19.3744395805123,84.7010622422469,
64.4413732028743));
#177294=CARTESIAN_POINT('Ctrl Pts',(-19.3705423958794,84.8091772698555,
64.5805608233731));
#177295=CARTESIAN_POINT('Ctrl Pts',(-19.3666407123037,84.9144636261772,
64.72194968504));
#177296=CARTESIAN_POINT('Ctrl Pts',(-19.3627345508503,85.0168365456723,
64.8654214859088));
#177297=CARTESIAN_POINT('Ctrl Pts',(-19.3583084311856,85.1328365619313,
65.0279911509682));
#177298=CARTESIAN_POINT('Ctrl Pts',(-19.3538768656123,85.2450706686846,
65.1931996793289));
#177299=CARTESIAN_POINT('Ctrl Pts',(-19.3494392777582,85.3534235182666,
65.3608767801899));
#177300=CARTESIAN_POINT('Ctrl Pts',(-19.3423986111134,85.5253358992735,
65.626912881322));
#177301=CARTESIAN_POINT('Ctrl Pts',(-19.3353359681688,85.6874616819676,
65.8991738812724));
#177302=CARTESIAN_POINT('Ctrl Pts',(-19.3282589746455,85.8393581862296,
66.1769664936222));
#177303=CARTESIAN_POINT('Ctrl Pts',(-19.3213083493066,85.9885423967203,
66.449798786603));
#177304=CARTESIAN_POINT('Ctrl Pts',(-19.3143438813069,86.1278596552626,
66.7279675738523));
#177305=CARTESIAN_POINT('Ctrl Pts',(-19.3073727951192,86.2568501668907,
67.0108436589344));
#177306=CARTESIAN_POINT('Ctrl Pts',(-19.29832459757,86.424274812026,67.3780057669402));
#177307=CARTESIAN_POINT('Ctrl Pts',(-19.2892464024017,86.5745484311984,
67.7536630701635));
#177308=CARTESIAN_POINT('Ctrl Pts',(-19.2801213644855,86.7062645729879,
68.1360633882202));
#177309=CARTESIAN_POINT('Ctrl Pts',(-19.2782027681902,86.7339587156302,
68.2164654468505));
#177310=CARTESIAN_POINT('Ctrl Pts',(-19.2762821010851,86.760832549227,68.2971654300741));
#177311=CARTESIAN_POINT('Ctrl Pts',(-19.2743592065957,86.7868731270772,
68.3781467925786));
#177312=CARTESIAN_POINT('Ctrl Pts',(-19.2735558745621,86.7977521589094,
68.4119785618106));
#177313=CARTESIAN_POINT('Ctrl Pts',(-19.272751612069,86.8084848102752,68.445859771803));
#177314=CARTESIAN_POINT('Ctrl Pts',(-19.2719468277685,86.819070927241,68.4797889760641));
#177315=CARTESIAN_POINT('Ctrl Pts',(-19.2713566720992,86.8268338233854,
68.5046695710729));
#177316=CARTESIAN_POINT('Ctrl Pts',(-19.270766235899,86.8345179219805,68.5295759752025));
#177317=CARTESIAN_POINT('Ctrl Pts',(-19.2701755446975,86.8421231642585,
68.5545076247401));
#177318=CARTESIAN_POINT('Ctrl Pts',(-19.2583305133496,86.9946298089418,
69.0544578010013));
#177319=CARTESIAN_POINT('Ctrl Pts',(-19.2464062952224,87.1153540390979,
69.564319294164));
#177320=CARTESIAN_POINT('Ctrl Pts',(-19.2344955395952,87.2038929865606,
70.0794616457638));
#177321=CARTESIAN_POINT('Ctrl Pts',(-19.2255648541586,87.2702794958154,
70.4657154185047));
#177322=CARTESIAN_POINT('Ctrl Pts',(-19.2166306713089,87.3186150091839,
70.8551919742187));
#177323=CARTESIAN_POINT('Ctrl Pts',(-19.2076647208652,87.3486597642837,
71.2459541183869));
#177324=CARTESIAN_POINT('Ctrl Pts',(-19.2044523919758,87.3594242264995,
71.3859567352262));
#177325=CARTESIAN_POINT('Ctrl Pts',(-19.2012374970565,87.3678345149059,
71.5260384699884));
#177326=CARTESIAN_POINT('Ctrl Pts',(-19.1980166927661,87.3738885371928,
71.666139079149));
#177327=CARTESIAN_POINT('Ctrl Pts',(-19.193379589662,87.3826047220359,71.8678467617762));
#177328=CARTESIAN_POINT('Ctrl Pts',(-19.1887351237912,87.3864339891829,
72.0695940567423));
#177329=CARTESIAN_POINT('Ctrl Pts',(-19.184087360571,87.3854106257393,72.2711996352709));
#177330=CARTESIAN_POINT('Ctrl Pts',(-19.1794322607388,87.3843856468905,
72.4731234533085));
#177331=CARTESIAN_POINT('Ctrl Pts',(-19.1747738531391,87.3784927198538,
72.6749058999744));
#177332=CARTESIAN_POINT('Ctrl Pts',(-19.1701162224715,87.3677144817021,
72.8763672965244));
#177333=CARTESIAN_POINT('Ctrl Pts',(-19.1691220913346,87.3654139596315,
72.9193674958705));
#177334=CARTESIAN_POINT('Ctrl Pts',(-19.1681279955927,87.362890688285,72.962353053272));
#177335=CARTESIAN_POINT('Ctrl Pts',(-19.1671339749643,87.3601441923391,
73.0053221826803));
#177336=CARTESIAN_POINT('Ctrl Pts',(-19.164564094539,87.3530435689029,73.1164119542731));
#177337=CARTESIAN_POINT('Ctrl Pts',(-19.1619911494633,87.344447828162,73.2274437727421));
#177338=CARTESIAN_POINT('Ctrl Pts',(-19.1594114054907,87.3343429044137,
73.3383711450185));
#177339=CARTESIAN_POINT('Ctrl Pts',(-19.1547191646531,87.315963275902,73.5401345570934));
#177340=CARTESIAN_POINT('Ctrl Pts',(-19.1500219576322,87.2926435057615,
73.7415587553322));
#177341=CARTESIAN_POINT('Ctrl Pts',(-19.1453140801817,87.2642981382976,
73.9423640347745));
#177342=CARTESIAN_POINT('Ctrl Pts',(-19.1406652548541,87.2363083140989,
74.1406505617326));
#177343=CARTESIAN_POINT('Ctrl Pts',(-19.1360060251019,87.2034181226359,
74.3383335922857));
#177344=CARTESIAN_POINT('Ctrl Pts',(-19.1313308986475,87.1655957877574,
74.5351501296208));
#177345=CARTESIAN_POINT('Ctrl Pts',(-19.129685292205,87.1522826338667,74.6044279480896));
#177346=CARTESIAN_POINT('Ctrl Pts',(-19.1280377161887,87.1383588610024,
74.6735984676939));
#177347=CARTESIAN_POINT('Ctrl Pts',(-19.1263879310737,87.1238246165211,
74.7426504105179));
#177348=CARTESIAN_POINT('Ctrl Pts',(-19.7210834129279,83.3320088770948,
62.9389668654546));
#177349=CARTESIAN_POINT('Ctrl Pts',(-19.0031848503602,83.3320088770948,
62.9389668654546));
#177350=CARTESIAN_POINT('Ctrl Pts',(-19.7210834129279,84.1021422518589,
63.6603901351978));
#177351=CARTESIAN_POINT('Ctrl Pts',(-19.0031848503602,84.1021422518589,
63.6603901351978));
#177352=CARTESIAN_POINT('Ctrl Pts',(-19.7210834129279,84.7817891561514,
64.4762669802466));
#177353=CARTESIAN_POINT('Ctrl Pts',(-19.0031848503602,84.7817891561514,
64.4762669802466));
#177354=CARTESIAN_POINT('Ctrl Pts',(-19.7210834129279,85.9590960090797,
66.2981609192099));
#177355=CARTESIAN_POINT('Ctrl Pts',(-19.0031848503602,85.9590960090797,
66.2981609192099));
#177356=CARTESIAN_POINT('Ctrl Pts',(-19.7210834129279,86.4453006331497,
67.315919751713));
#177357=CARTESIAN_POINT('Ctrl Pts',(-19.0031848503602,86.4453006331497,
67.315919751713));
#177358=CARTESIAN_POINT('Ctrl Pts',(-19.7210834129279,87.1284456210047,
69.4403738334441));
#177359=CARTESIAN_POINT('Ctrl Pts',(-19.0031848503602,87.1284456210047,
69.4403738334441));
#177360=CARTESIAN_POINT('Ctrl Pts',(-19.7210834129279,87.3257156024833,
70.5513335535036));
#177361=CARTESIAN_POINT('Ctrl Pts',(-19.0031848503602,87.3257156024833,
70.5513335535036));
#177362=CARTESIAN_POINT('Ctrl Pts',(-19.7210834129279,87.3979750045476,
72.2235418419717));
#177363=CARTESIAN_POINT('Ctrl Pts',(-19.0031848503602,87.3979750045476,
72.2235418419717));
#177364=CARTESIAN_POINT('Ctrl Pts',(-19.7210834129279,87.3848332607061,
72.7841104016103));
#177365=CARTESIAN_POINT('Ctrl Pts',(-19.0031848503602,87.3848332607061,
72.7841104016103));
#177366=CARTESIAN_POINT('Ctrl Pts',(-19.7210834129279,87.2890617556199,
73.8354475183249));
#177367=CARTESIAN_POINT('Ctrl Pts',(-19.0031848503602,87.2890617556199,
73.8354475183249));
#177368=CARTESIAN_POINT('Ctrl Pts',(-19.7210834129279,87.2139739637454,
74.3287972481997));
#177369=CARTESIAN_POINT('Ctrl Pts',(-19.0031848503602,87.2139739637454,
74.3287972481997));
#177370=CARTESIAN_POINT('Ctrl Pts',(-19.7210834129279,87.1076595086348,
74.8182427933889));
#177371=CARTESIAN_POINT('Ctrl Pts',(-19.0031848503602,87.1076595086348,
74.8182427933889));
#177372=CARTESIAN_POINT('Ctrl Pts',(-19.7175219896828,83.3888301557713,
62.9925212140073));
#177373=CARTESIAN_POINT('Ctrl Pts',(-19.7032357686156,83.8619600719994,
63.4411857890303));
#177374=CARTESIAN_POINT('Ctrl Pts',(-19.6888822186524,84.3006547083239,
63.9259433661352));
#177375=CARTESIAN_POINT('Ctrl Pts',(-19.674461721319,84.7006418514101,64.4408320198575));
#177376=CARTESIAN_POINT('Ctrl Pts',(-19.6707792859391,84.8027830448213,
64.5723145999207));
#177377=CARTESIAN_POINT('Ctrl Pts',(-19.6670924849655,84.9023999937689,
64.7057617926793));
#177378=CARTESIAN_POINT('Ctrl Pts',(-19.6634013247513,84.9994212391248,
64.8410738773966));
#177379=CARTESIAN_POINT('Ctrl Pts',(-19.6587526282975,85.1216110908412,
65.0114877234196));
#177380=CARTESIAN_POINT('Ctrl Pts',(-19.6540986130407,85.2396562484237,
65.1848208107002));
#177381=CARTESIAN_POINT('Ctrl Pts',(-19.6494392777599,85.3534235182665,
65.3608767801898));
#177382=CARTESIAN_POINT('Ctrl Pts',(-19.6424230631589,85.5247388522517,
65.6259889451812));
#177383=CARTESIAN_POINT('Ctrl Pts',(-19.6354021244995,85.68633772351,65.8972863128462));
#177384=CARTESIAN_POINT('Ctrl Pts',(-19.6283648699484,85.8377823502123,
66.1740854297724));
#177385=CARTESIAN_POINT('Ctrl Pts',(-19.621843385339,85.9781273945805,66.43059756356));
#177386=CARTESIAN_POINT('Ctrl Pts',(-19.6153078888228,86.1097519757193,
66.6918353088855));
#177387=CARTESIAN_POINT('Ctrl Pts',(-19.6087491550728,86.2322746523157,
66.9572772307433));
#177388=CARTESIAN_POINT('Ctrl Pts',(-19.5999665130593,86.3963418104133,
67.3127240995923));
#177389=CARTESIAN_POINT('Ctrl Pts',(-19.5911412883923,86.5441725466508,
67.6759164140595));
#177390=CARTESIAN_POINT('Ctrl Pts',(-19.5822984309476,86.6745701714822,
68.0451907180569));
#177391=CARTESIAN_POINT('Ctrl Pts',(-19.579653377885,86.7135743778791,68.1556471101027));
#177392=CARTESIAN_POINT('Ctrl Pts',(-19.5770067471956,86.7510191125115,
68.26664746382));
#177393=CARTESIAN_POINT('Ctrl Pts',(-19.5743592065984,86.7868731270772,
68.3781467925785));
#177394=CARTESIAN_POINT('Ctrl Pts',(-19.5735592697391,86.7977061801516,
68.4118355764103));
#177395=CARTESIAN_POINT('Ctrl Pts',(-19.5727597867005,86.8083930780443,
68.4455702452619));
#177396=CARTESIAN_POINT('Ctrl Pts',(-19.571960356956,86.8189337354123,68.4793492961659));
#177397=CARTESIAN_POINT('Ctrl Pts',(-19.5719568884247,86.8189794687629,
68.4794958552583));
#177398=CARTESIAN_POINT('Ctrl Pts',(-19.5719534198934,86.8190251993725,
68.4796424152244));
#177399=CARTESIAN_POINT('Ctrl Pts',(-19.5719499513622,86.819070927241,68.4797889760641));
#177400=CARTESIAN_POINT('Ctrl Pts',(-19.5599906187491,86.9767384694338,
68.9851238653064));
#177401=CARTESIAN_POINT('Ctrl Pts',(-19.5480134164975,87.1018196188291,
69.5008432106858));
#177402=CARTESIAN_POINT('Ctrl Pts',(-19.5359444704607,87.193903283335,70.0221345398778));
#177403=CARTESIAN_POINT('Ctrl Pts',(-19.5269013179855,87.2629007431023,
70.4127334338933));
#177404=CARTESIAN_POINT('Ctrl Pts',(-19.5178062838736,87.3134180275645,
70.8067205289831));
#177405=CARTESIAN_POINT('Ctrl Pts',(-19.5086971906096,87.3452097472485,
71.2020880584462));
#177406=CARTESIAN_POINT('Ctrl Pts',(-19.5051350676615,87.3576419412074,
71.3566970528696));
#177407=CARTESIAN_POINT('Ctrl Pts',(-19.5015738726351,87.3672022426337,
71.511406589515));
#177408=CARTESIAN_POINT('Ctrl Pts',(-19.4980166927664,87.3738885371928,
71.666139079149));
#177409=CARTESIAN_POINT('Ctrl Pts',(-19.4934105162435,87.3825465905272,
71.8665014975215));
#177410=CARTESIAN_POINT('Ctrl Pts',(-19.4888065269328,87.386382737324,72.0669026460856));
#177411=CARTESIAN_POINT('Ctrl Pts',(-19.4841972065756,87.3854304240733,
72.2671719933372));
#177412=CARTESIAN_POINT('Ctrl Pts',(-19.4795811934391,87.3844767280543,
72.4677321336821));
#177413=CARTESIAN_POINT('Ctrl Pts',(-19.4749598337635,87.3787206699474,
72.6681608773103));
#177414=CARTESIAN_POINT('Ctrl Pts',(-19.4703255764928,87.3681440282755,
72.8682892798773));
#177415=CARTESIAN_POINT('Ctrl Pts',(-19.4694361642207,87.3661141463868,
72.9066981654557));
#177416=CARTESIAN_POINT('Ctrl Pts',(-19.4685462768817,87.3639065508694,
72.9450959748942));
#177417=CARTESIAN_POINT('Ctrl Pts',(-19.4676558610962,87.3615208940382,
72.9834814859482));
#177418=CARTESIAN_POINT('Ctrl Pts',(-19.4649097591887,87.35416336862,73.1018649724439));
#177419=CARTESIAN_POINT('Ctrl Pts',(-19.4621600849288,87.3451095527422,
73.2201796537156));
#177420=CARTESIAN_POINT('Ctrl Pts',(-19.4594114054906,87.3343429044137,
73.3383711450185));
#177421=CARTESIAN_POINT('Ctrl Pts',(-19.4546834481501,87.3158233734374,
73.5416703443159));
#177422=CARTESIAN_POINT('Ctrl Pts',(-19.4499407562388,87.2922895922582,
73.7446106609143));
#177423=CARTESIAN_POINT('Ctrl Pts',(-19.4451892350924,87.2636549340332,
73.9469144504035));
#177424=CARTESIAN_POINT('Ctrl Pts',(-19.4404973026353,87.2353793822287,
74.1466811539214));
#177425=CARTESIAN_POINT('Ctrl Pts',(-19.4357967610088,87.2021300366619,
74.3458271887575));
#177426=CARTESIAN_POINT('Ctrl Pts',(-19.4310932961472,87.1638740066269,
74.5440915419293));
#177427=CARTESIAN_POINT('Ctrl Pts',(-19.4295207442365,87.1510835223988,
74.6103790547719));
#177428=CARTESIAN_POINT('Ctrl Pts',(-19.4279478655589,87.1377338036843,
74.6765680641747));
#177429=CARTESIAN_POINT('Ctrl Pts',(-19.4263748726166,87.1238249181727,
74.7426489773759));
#177430=CARTESIAN_POINT('Ctrl Pts',(-19.6963598728939,83.226001468616,62.77070321842));
#177431=CARTESIAN_POINT('Ctrl Pts',(-19.6458893337409,84.939239057138,64.327937106799));
#177432=CARTESIAN_POINT('Ctrl Pts',(-19.5449482554399,87.45984141513,68.317270374702));
#177433=CARTESIAN_POINT('Ctrl Pts',(-19.4440071771409,87.61121247713,72.8827219751971));
#177434=CARTESIAN_POINT('Ctrl Pts',(-19.3935366379889,87.12089616464,74.995478178794));
#177435=CARTESIAN_POINT('Ctrl Pts',(-19.8531778424579,83.037095918694,63.005358182281));
#177436=CARTESIAN_POINT('Ctrl Pts',(-19.8027073033049,84.708993071182,64.529311556686));
#177437=CARTESIAN_POINT('Ctrl Pts',(-19.7017662250039,87.16498412488,68.429761545683));
#177438=CARTESIAN_POINT('Ctrl Pts',(-19.6008251467039,87.3053450107,72.8858804706761));
#177439=CARTESIAN_POINT('Ctrl Pts',(-19.5503546075529,86.823696661,74.94627742788));
#177440=CARTESIAN_POINT('Ctrl Pts',(-20.0099958120219,82.848190368771,63.240013146138));
#177441=CARTESIAN_POINT('Ctrl Pts',(-19.9595252728689,84.478747085231,64.730686006568));
#177442=CARTESIAN_POINT('Ctrl Pts',(-19.8585841945679,86.87012683464,68.542252716656));
#177443=CARTESIAN_POINT('Ctrl Pts',(-19.7576431162679,86.99947754428,72.8890389661519));
#177444=CARTESIAN_POINT('Ctrl Pts',(-19.7071725771169,86.52649715737,74.897076676965));
#177445=CARTESIAN_POINT('Ctrl Pts',(-20.1668137815859,82.659284818849,63.474668109995));
#177446=CARTESIAN_POINT('Ctrl Pts',(-20.1163432424329,84.248501099275,64.932060456454));
#177447=CARTESIAN_POINT('Ctrl Pts',(-20.0154021641319,86.5752695444,68.654743887637));
#177448=CARTESIAN_POINT('Ctrl Pts',(-19.9144610858319,86.69361007784,72.8921974616309));
#177449=CARTESIAN_POINT('Ctrl Pts',(-19.8639905466809,86.22929765373,74.847875926051));
#177450=CARTESIAN_POINT('Ctrl Pts',(-19.7180890220136,83.3888904642227,
62.9941398919268));
#177451=CARTESIAN_POINT('Ctrl Pts',(-19.7872818648352,83.3034260995692,
63.0959359304728));
#177452=CARTESIAN_POINT('Ctrl Pts',(-19.8564746782248,83.2179621899393,
63.1977322762277));
#177453=CARTESIAN_POINT('Ctrl Pts',(-19.9950718297746,83.0467739441428,
63.4016368653651));
#177454=CARTESIAN_POINT('Ctrl Pts',(-20.0644762132755,82.9610495545407,
63.5037451776019));
#177455=CARTESIAN_POINT('Ctrl Pts',(-20.1338805884022,82.8753255974315,
63.6058538308433));
#177456=CARTESIAN_POINT('Ctrl Pts',(-25.3005363491459,74.5427514436947,
59.89500391474));
#177457=CARTESIAN_POINT('Ctrl Pts',(-25.2707446824789,75.9044177816449,
59.84745347843));
#177458=CARTESIAN_POINT('Ctrl Pts',(-25.2111613491459,78.642454697891,60.18062740255));
#177459=CARTESIAN_POINT('Ctrl Pts',(-25.1217863491459,82.398054635848,61.91693136384));
#177460=CARTESIAN_POINT('Ctrl Pts',(-25.0324113491459,85.43936982203,64.722158934074));
#177461=CARTESIAN_POINT('Ctrl Pts',(-24.9430363491459,87.47284957896,68.325482238879));
#177462=CARTESIAN_POINT('Ctrl Pts',(-24.8536613491459,88.30215727482,72.3790257123511));
#177463=CARTESIAN_POINT('Ctrl Pts',(-24.7642863491459,87.84723377397,76.491447312794));
#177464=CARTESIAN_POINT('Ctrl Pts',(-24.6749113491459,86.15199752785,80.265720932952));
#177465=CARTESIAN_POINT('Ctrl Pts',(-24.5855363491449,83.380112338587,83.33746628068));
#177466=CARTESIAN_POINT('Ctrl Pts',(-24.4961613491449,79.799184652141,85.41012737455));
#177467=CARTESIAN_POINT('Ctrl Pts',(-24.4067863491449,75.7549285472016,
86.28360297416));
#177468=CARTESIAN_POINT('Ctrl Pts',(-24.3174113491449,71.637789257726,85.87356499026));
#177469=CARTESIAN_POINT('Ctrl Pts',(-24.2280363491449,67.845248398678,84.21959978308));
#177470=CARTESIAN_POINT('Ctrl Pts',(-24.1386613491449,64.74344982644,81.481386370637));
#177471=CARTESIAN_POINT('Ctrl Pts',(-24.0492863491449,62.6318509589,77.923280512555));
#177472=CARTESIAN_POINT('Ctrl Pts',(-23.9599113491449,61.71431221106,73.8887929712529));
#177473=CARTESIAN_POINT('Ctrl Pts',(-23.8705363491449,62.07941566771,69.767425899435));
#177474=CARTESIAN_POINT('Ctrl Pts',(-23.7811613491449,63.69191308954,65.957069073716));
#177475=CARTESIAN_POINT('Ctrl Pts',(-23.6917863491449,66.396128889362,62.82558636057));
#177476=CARTESIAN_POINT('Ctrl Pts',(-23.6024113491449,69.930989544296,60.67530097837));
#177477=CARTESIAN_POINT('Ctrl Pts',(-23.5130363491449,73.955228457156,59.71380826027));
#177478=CARTESIAN_POINT('Ctrl Pts',(-23.4236613491449,78.080332910152,60.03393374599));
#177479=CARTESIAN_POINT('Ctrl Pts',(-23.3342863491449,81.908052308101,61.60477151142));
#177480=CARTESIAN_POINT('Ctrl Pts',(-23.2449113491459,85.06884654704,64.274667923988));
#177481=CARTESIAN_POINT('Ctrl Pts',(-23.1555363491459,87.25756258145,67.785862762707));
#177482=CARTESIAN_POINT('Ctrl Pts',(-23.0661613491459,88.26289486179,71.799374202937));
#177483=CARTESIAN_POINT('Ctrl Pts',(-22.9767863491459,87.98778543871,75.927725190932));
#177484=CARTESIAN_POINT('Ctrl Pts',(-22.8874113491459,86.45879424367,79.77235170078));
#177485=CARTESIAN_POINT('Ctrl Pts',(-22.7980363491459,83.823534909334,82.962081362607));
#177486=CARTESIAN_POINT('Ctrl Pts',(-22.7086613491459,80.336423683903,85.1889676139));
#177487=CARTESIAN_POINT('Ctrl Pts',(-22.6192863491459,76.334117284029,86.23801983199));
#177488=CARTESIAN_POINT('Ctrl Pts',(-22.5299113491459,72.203010993519,86.00795920683));
#177489=CARTESIAN_POINT('Ctrl Pts',(-22.4405363491459,68.34193484388,84.52099651684));
#177490=CARTESIAN_POINT('Ctrl Pts',(-22.3511613491459,65.123649305097,81.920687830243));
#177491=CARTESIAN_POINT('Ctrl Pts',(-22.2617863491459,62.85885781411,78.458075149464));
#177492=CARTESIAN_POINT('Ctrl Pts',(-22.1724113491459,61.766210485,74.467450024384));
#177493=CARTESIAN_POINT('Ctrl Pts',(-22.0830363491459,61.95119493732,70.334079991696));
#177494=CARTESIAN_POINT('Ctrl Pts',(-21.9936613491459,63.39595218857,66.457013631716));
#177495=CARTESIAN_POINT('Ctrl Pts',(-21.9042863491459,65.961000816697,63.210555159771));
#177496=CARTESIAN_POINT('Ctrl Pts',(-21.8149113491459,69.398702936539,60.90812791663));
#177497=CARTESIAN_POINT('Ctrl Pts',(-21.7255363491459,73.377171942341,59.7720154906));
#177498=CARTESIAN_POINT('Ctrl Pts',(-21.6361613491459,77.512313887507,59.91190175878));
#177499=CARTESIAN_POINT('Ctrl Pts',(-21.5467863491459,81.404909125703,61.31428165962));
#177500=CARTESIAN_POINT('Ctrl Pts',(-21.4574113491459,84.679154234719,63.843765014137));
#177501=CARTESIAN_POINT('Ctrl Pts',(-21.3680363491459,87.0189432642,67.256147520865));
#177502=CARTESIAN_POINT('Ctrl Pts',(-21.2786613491459,88.19838560114,71.22198700936));
#177503=CARTESIAN_POINT('Ctrl Pts',(-21.1892863491459,88.10361416217,75.358408826466));
#177504=CARTESIAN_POINT('Ctrl Pts',(-21.0999113491459,86.74377848093,79.266069762973));
#177505=CARTESIAN_POINT('Ctrl Pts',(-21.0105363491459,84.25016138325,82.567711906636));
#177506=CARTESIAN_POINT('Ctrl Pts',(-20.9211613491459,80.863504529035,84.94458431096));
#177507=CARTESIAN_POINT('Ctrl Pts',(-20.8317863491459,76.910766453087,86.16721621697));
#177508=CARTESIAN_POINT('Ctrl Pts',(-20.7424113491459,72.773556956877,86.11757088408));
#177509=CARTESIAN_POINT('Ctrl Pts',(-20.6530363491459,68.851295294622,84.80044122928));
#177510=CARTESIAN_POINT('Ctrl Pts',(-20.5636613491459,65.522648978742,82.34298710401));
#177511=CARTESIAN_POINT('Ctrl Pts',(-20.4742863491459,63.10897602347,78.982458880342));
#177512=CARTESIAN_POINT('Ctrl Pts',(-20.3849113491459,61.84330002988,75.043292554251));
#177513=CARTESIAN_POINT('Ctrl Pts',(-20.2955363491459,61.84781334742,70.905787661752));
#177514=CARTESIAN_POINT('Ctrl Pts',(-20.2061613491459,63.12208025789,66.969391997631));
#177515=CARTESIAN_POINT('Ctrl Pts',(-20.1167863491459,65.543078970735,63.614137533019));
#177516=CARTESIAN_POINT('Ctrl Pts',(-20.0274113491459,68.877078797366,61.16395142431));
#177517=CARTESIAN_POINT('Ctrl Pts',(-19.9380363491459,72.80220426866,59.85538121976));
#177518=CARTESIAN_POINT('Ctrl Pts',(-19.8486613491459,76.939513667119,59.81476469495));
#177519=CARTESIAN_POINT('Ctrl Pts',(-19.7592863491459,80.889569599415,61.04600712199));
#177520=CARTESIAN_POINT('Ctrl Pts',(-19.6699113491459,84.271052907551,63.430300094054));
#177521=CARTESIAN_POINT('Ctrl Pts',(-19.6103280158119,85.92860844783,65.634922657953));
#177522=CARTESIAN_POINT('Ctrl Pts',(-19.5805363491459,86.568261731,66.837935516246));
#177523=CARTESIAN_POINT('Ctrl Pts',(-25.4573543187099,74.5532647257124,
60.19606492144));
#177524=CARTESIAN_POINT('Ctrl Pts',(-25.4275626520429,75.8836229665074,
60.14960778797));
#177525=CARTESIAN_POINT('Ctrl Pts',(-25.3679793187099,78.558705601371,60.47512121458));
#177526=CARTESIAN_POINT('Ctrl Pts',(-25.2786043187099,82.227954952215,62.1715032276));
#177527=CARTESIAN_POINT('Ctrl Pts',(-25.1892293187099,85.19934273499,64.912231636138));
#177528=CARTESIAN_POINT('Ctrl Pts',(-25.0998543187099,87.18606773268,68.432705572515));
#177529=CARTESIAN_POINT('Ctrl Pts',(-25.0104793187089,87.99630758116,72.393047995661));
#177530=CARTESIAN_POINT('Ctrl Pts',(-24.9211043187089,87.55184390352,76.41091479114));
#177531=CARTESIAN_POINT('Ctrl Pts',(-24.8317293187089,85.89558535672,80.098408469768));
#177532=CARTESIAN_POINT('Ctrl Pts',(-24.7423543187089,83.187432704849,83.09952674895));
#177533=CARTESIAN_POINT('Ctrl Pts',(-24.6529793187089,79.688839455842,85.12453220716));
#177534=CARTESIAN_POINT('Ctrl Pts',(-24.5636043187089,75.7375708615168,
85.97792442938));
#177535=CARTESIAN_POINT('Ctrl Pts',(-24.4742293187089,71.715094848414,85.57731423897));
#177536=CARTESIAN_POINT('Ctrl Pts',(-24.3848543187089,68.00975394017,83.96137780724));
#177537=CARTESIAN_POINT('Ctrl Pts',(-24.2954793187089,64.97927343488,81.286122734268));
#177538=CARTESIAN_POINT('Ctrl Pts',(-24.2061043187089,62.91622547931,77.809826583006));
#177539=CARTESIAN_POINT('Ctrl Pts',(-24.1167293187089,62.01978323026,73.8681019487348));
#177540=CARTESIAN_POINT('Ctrl Pts',(-24.0273543187089,62.37649205001,69.841495360525));
#177541=CARTESIAN_POINT('Ctrl Pts',(-23.9379793187089,63.95191414396,66.118748119013));
#177542=CARTESIAN_POINT('Ctrl Pts',(-23.8486043187089,66.593953294018,63.059265985079));
#177543=CARTESIAN_POINT('Ctrl Pts',(-23.7592293187089,70.047538707191,60.95842101407));
#177544=CARTESIAN_POINT('Ctrl Pts',(-23.6698543187089,73.979250354488,60.01903540591));
#177545=CARTESIAN_POINT('Ctrl Pts',(-23.5804793187089,78.009508392183,60.33180041019));
#177546=CARTESIAN_POINT('Ctrl Pts',(-23.4911043187089,81.749218997189,61.8665207069));
#177547=CARTESIAN_POINT('Ctrl Pts',(-23.4017293187089,84.837338712008,64.475029557805));
#177548=CARTESIAN_POINT('Ctrl Pts',(-23.3123543187089,86.97573071891,67.905493290763));
#177549=CARTESIAN_POINT('Ctrl Pts',(-23.2229793187089,87.95794790869,71.826724116717));
#177550=CARTESIAN_POINT('Ctrl Pts',(-23.1336043187099,87.68916393577,75.860154043494));
#177551=CARTESIAN_POINT('Ctrl Pts',(-23.0442293187099,86.19532805268,79.616383023829));
#177552=CARTESIAN_POINT('Ctrl Pts',(-22.9548543187099,83.620659887386,82.732772864167));
#177553=CARTESIAN_POINT('Ctrl Pts',(-22.8654793187099,80.213726025524,84.90845745969));
#177554=CARTESIAN_POINT('Ctrl Pts',(-22.7761043187099,76.303442608167,85.93338935707));
#177555=CARTESIAN_POINT('Ctrl Pts',(-22.6867293187099,72.267320730135,85.70861839811));
#177556=CARTESIAN_POINT('Ctrl Pts',(-22.5973543187099,68.495020328158,84.25584468017));
#177557=CARTESIAN_POINT('Ctrl Pts',(-22.5079793187099,65.350731181526,81.715323560263));
#177558=CARTESIAN_POINT('Ctrl Pts',(-22.4186043187099,63.13801288209,78.332324960555));
#177559=CARTESIAN_POINT('Ctrl Pts',(-22.3292293187099,62.07048823376,74.43345423642));
#177560=CARTESIAN_POINT('Ctrl Pts',(-22.2398543187099,62.25121943325,70.395120665275));
#177561=CARTESIAN_POINT('Ctrl Pts',(-22.1504793187099,63.6627581205,66.607197707679));
#177562=CARTESIAN_POINT('Ctrl Pts',(-22.0611043187099,66.168829898414,63.435383393718));
#177563=CARTESIAN_POINT('Ctrl Pts',(-21.9717293187099,69.527490692963,61.18589468171));
#177564=CARTESIAN_POINT('Ctrl Pts',(-21.8823543187099,73.414484797248,60.07590430719));
#177565=CARTESIAN_POINT('Ctrl Pts',(-21.7929793187099,77.454549540195,60.212574242));
#177566=CARTESIAN_POINT('Ctrl Pts',(-21.7036043187099,81.257644328458,61.58270993957));
#177567=CARTESIAN_POINT('Ctrl Pts',(-21.6142293187099,84.456606395566,64.054034178009));
#177568=CARTESIAN_POINT('Ctrl Pts',(-21.5248543187099,86.74259785348,67.387957520349));
#177569=CARTESIAN_POINT('Ctrl Pts',(-21.4354793187099,87.89492187645,71.262612491355));
#177570=CARTESIAN_POINT('Ctrl Pts',(-21.3461043187099,87.80232946867,75.3039276788));
#177571=CARTESIAN_POINT('Ctrl Pts',(-21.2567293187099,86.47375979323,79.121741767484));
#177572=CARTESIAN_POINT('Ctrl Pts',(-21.1673543187099,84.03747715715,82.347470943245));
#177573=CARTESIAN_POINT('Ctrl Pts',(-21.0779793187099,80.728687970562,84.66969313695));
#177574=CARTESIAN_POINT('Ctrl Pts',(-20.9886043187099,76.866833178031,85.86421369334));
#177575=CARTESIAN_POINT('Ctrl Pts',(-20.8992293187099,72.824748422185,85.81570983017));
#177576=CARTESIAN_POINT('Ctrl Pts',(-20.8098543187099,68.992669314766,84.52886426336));
#177577=CARTESIAN_POINT('Ctrl Pts',(-20.7204793187099,65.740556859899,82.127913122978));
#177578=CARTESIAN_POINT('Ctrl Pts',(-20.6311043187099,63.38238025148,78.844651804709));
#177579=CARTESIAN_POINT('Ctrl Pts',(-20.5417293187099,62.14580529819,74.996056713737));
#177580=CARTESIAN_POINT('Ctrl Pts',(-20.4523543187099,62.15021484332,70.953683353497));
#177581=CARTESIAN_POINT('Ctrl Pts',(-20.3629793187099,63.39518318695,67.107795220083));
#177582=CARTESIAN_POINT('Ctrl Pts',(-20.2736043187099,65.760517115547,63.829686404028));
#177583=CARTESIAN_POINT('Ctrl Pts',(-20.1842293187099,69.017859990633,61.43583617042));
#177584=CARTESIAN_POINT('Ctrl Pts',(-20.0948543187099,72.852737060995,60.15735325081));
#177585=CARTESIAN_POINT('Ctrl Pts',(-20.0054793187099,76.894919422089,60.11767060096));
#177586=CARTESIAN_POINT('Ctrl Pts',(-19.9161043187099,80.754153740124,61.32060370107));
#177587=CARTESIAN_POINT('Ctrl Pts',(-19.8267293187099,84.057888333329,63.650075845203));
#177588=CARTESIAN_POINT('Ctrl Pts',(-19.7671459853759,85.67733254748,65.804008650901));
#177589=CARTESIAN_POINT('Ctrl Pts',(-19.7373543187099,86.3022786101,66.979361250291));
#177590=CARTESIAN_POINT('Ctrl Pts',(-25.6141722882739,74.5637780077301,
60.49712592814));
#177591=CARTESIAN_POINT('Ctrl Pts',(-25.5843806216069,75.8628281513697,
60.45176209751));
#177592=CARTESIAN_POINT('Ctrl Pts',(-25.5247972882739,78.47495650485,60.76961502662));
#177593=CARTESIAN_POINT('Ctrl Pts',(-25.4354222882739,82.057855268582,62.42607509136));
#177594=CARTESIAN_POINT('Ctrl Pts',(-25.3460472882739,84.95931564794,65.102304338201));
#177595=CARTESIAN_POINT('Ctrl Pts',(-25.2566722882729,86.89928588639,68.539928906151));
#177596=CARTESIAN_POINT('Ctrl Pts',(-25.1672972882729,87.6904578875,72.4070702789702));
#177597=CARTESIAN_POINT('Ctrl Pts',(-25.0779222882729,87.25645403306,76.330382269486));
#177598=CARTESIAN_POINT('Ctrl Pts',(-24.9885472882729,85.63917318558,79.931096006583));
#177599=CARTESIAN_POINT('Ctrl Pts',(-24.8991722882729,82.994753071114,82.861587217225));
#177600=CARTESIAN_POINT('Ctrl Pts',(-24.8097972882729,79.578494259545,84.83893703977));
#177601=CARTESIAN_POINT('Ctrl Pts',(-24.7204222882729,75.7202131758358,
85.67224588461));
#177602=CARTESIAN_POINT('Ctrl Pts',(-24.6310472882729,71.792400439106,85.28106348769));
#177603=CARTESIAN_POINT('Ctrl Pts',(-24.5416722882729,68.174259481666,83.70315583141));
#177604=CARTESIAN_POINT('Ctrl Pts',(-24.4522972882729,65.215097043329,81.090859097905));
#177605=CARTESIAN_POINT('Ctrl Pts',(-24.3629222882729,63.20059999972,77.696372653464));
#177606=CARTESIAN_POINT('Ctrl Pts',(-24.2735472882729,62.32525424947,73.8474109262254));
#177607=CARTESIAN_POINT('Ctrl Pts',(-24.1841722882729,62.67356843231,69.915564821625));
#177608=CARTESIAN_POINT('Ctrl Pts',(-24.0947972882729,64.21191519837,66.280427164319));
#177609=CARTESIAN_POINT('Ctrl Pts',(-24.0054222882729,66.791777698664,63.292945609594));
#177610=CARTESIAN_POINT('Ctrl Pts',(-23.9160472882729,70.164087870074,61.24154104977));
#177611=CARTESIAN_POINT('Ctrl Pts',(-23.8266722882729,74.0032722518052,
60.32426255155));
#177612=CARTESIAN_POINT('Ctrl Pts',(-23.7372972882729,77.938683874199,60.62966707439));
#177613=CARTESIAN_POINT('Ctrl Pts',(-23.6479222882729,81.590385686263,62.12826990236));
#177614=CARTESIAN_POINT('Ctrl Pts',(-23.5585472882729,84.605830876964,64.675391191609));
#177615=CARTESIAN_POINT('Ctrl Pts',(-23.4691722882729,86.69389885636,68.0251238188));
#177616=CARTESIAN_POINT('Ctrl Pts',(-23.3797972882729,87.65300095559,71.854074030477));
#177617=CARTESIAN_POINT('Ctrl Pts',(-23.2904222882729,87.39054243283,75.792582896034));
#177618=CARTESIAN_POINT('Ctrl Pts',(-23.2010472882729,85.93186186169,79.460414346857));
#177619=CARTESIAN_POINT('Ctrl Pts',(-23.1116722882729,83.417784865457,82.503464365711));
#177620=CARTESIAN_POINT('Ctrl Pts',(-23.0222972882739,80.091028367167,84.62794730547));
#177621=CARTESIAN_POINT('Ctrl Pts',(-22.9329222882739,76.272767932331,85.62875888215));
#177622=CARTESIAN_POINT('Ctrl Pts',(-22.8435472882739,72.331630466779,85.4092775894));
#177623=CARTESIAN_POINT('Ctrl Pts',(-22.7541722882739,68.648105812461,83.99069284351));
#177624=CARTESIAN_POINT('Ctrl Pts',(-22.6647972882739,65.577813057976,81.509959290305));
#177625=CARTESIAN_POINT('Ctrl Pts',(-22.5754222882739,63.41716795007,78.206574771673));
#177626=CARTESIAN_POINT('Ctrl Pts',(-22.4860472882739,62.37476598252,74.399458448487));
#177627=CARTESIAN_POINT('Ctrl Pts',(-22.3966722882739,62.55124392917,70.456161338886));
#177628=CARTESIAN_POINT('Ctrl Pts',(-22.3072972882739,63.92956405242,66.757381783671));
#177629=CARTESIAN_POINT('Ctrl Pts',(-22.2179222882739,66.376658980107,63.660211627688));
#177630=CARTESIAN_POINT('Ctrl Pts',(-22.1285472882739,69.656278449357,61.4636614468));
#177631=CARTESIAN_POINT('Ctrl Pts',(-22.0391722882739,73.451797652123,60.37979312378));
#177632=CARTESIAN_POINT('Ctrl Pts',(-21.9497972882739,77.396785192848,60.51324672522));
#177633=CARTESIAN_POINT('Ctrl Pts',(-21.8604222882739,81.110379531183,61.85113821951));
#177634=CARTESIAN_POINT('Ctrl Pts',(-21.7710472882739,84.234058556389,64.264303341857));
#177635=CARTESIAN_POINT('Ctrl Pts',(-21.6816722882739,86.46625244275,67.519767519802));
#177636=CARTESIAN_POINT('Ctrl Pts',(-21.5922972882739,87.59145815176,71.303237973316));
#177637=CARTESIAN_POINT('Ctrl Pts',(-21.5029222882739,87.50104477518,75.2494465311));
#177638=CARTESIAN_POINT('Ctrl Pts',(-21.4135472882739,86.20374110555,78.977413771966));
#177639=CARTESIAN_POINT('Ctrl Pts',(-21.3241722882739,83.824792931074,82.127229979831));
#177640=CARTESIAN_POINT('Ctrl Pts',(-21.2347972882739,80.593871412118,84.39480196293));
#177641=CARTESIAN_POINT('Ctrl Pts',(-21.1454222882739,76.822899903006,85.5612111697));
#177642=CARTESIAN_POINT('Ctrl Pts',(-21.0560472882739,72.875939887522,85.51384877627));
#177643=CARTESIAN_POINT('Ctrl Pts',(-20.9666722882739,69.134043334935,84.25728729746));
#177644=CARTESIAN_POINT('Ctrl Pts',(-20.8772972882739,65.958464741074,81.912839141965));
#177645=CARTESIAN_POINT('Ctrl Pts',(-20.7879222882739,63.65578447949,78.706844729098));
#177646=CARTESIAN_POINT('Ctrl Pts',(-20.6985472882739,62.4483105665,74.948820873245));
#177647=CARTESIAN_POINT('Ctrl Pts',(-20.6091722882739,62.45261633923,71.001579045262));
#177648=CARTESIAN_POINT('Ctrl Pts',(-20.5197972882739,63.668286116,67.246198442551));
#177649=CARTESIAN_POINT('Ctrl Pts',(-20.4304222882739,65.977955260347,64.045235275048));
#177650=CARTESIAN_POINT('Ctrl Pts',(-20.3410472882739,69.158641183889,61.70772091653));
#177651=CARTESIAN_POINT('Ctrl Pts',(-20.2516722882739,72.903269853321,60.45932528185));
#177652=CARTESIAN_POINT('Ctrl Pts',(-20.1622972882739,76.850325177053,60.42057650697));
#177653=CARTESIAN_POINT('Ctrl Pts',(-20.0729222882739,80.618737880831,61.59520028015));
#177654=CARTESIAN_POINT('Ctrl Pts',(-19.9835472882739,83.844723759108,63.869851596353));
#177655=CARTESIAN_POINT('Ctrl Pts',(-19.9239639549399,85.42605664712,65.973094643852));
#177656=CARTESIAN_POINT('Ctrl Pts',(-19.8941722882739,86.0362954892,67.120786984341));
#177657=CARTESIAN_POINT('Ctrl Pts',(-25.7709902578379,74.5742912897478,
60.79818693484));
#177658=CARTESIAN_POINT('Ctrl Pts',(-25.7411985911709,75.8420333362322,
60.75391640706));
#177659=CARTESIAN_POINT('Ctrl Pts',(-25.6816152578379,78.39120740833,61.06410883866));
#177660=CARTESIAN_POINT('Ctrl Pts',(-25.5922402578369,81.887755584948,62.68064695513));
#177661=CARTESIAN_POINT('Ctrl Pts',(-25.5028652578369,84.719288560893,65.292377040265));
#177662=CARTESIAN_POINT('Ctrl Pts',(-25.4134902578369,86.61250404011,68.647152239787));
#177663=CARTESIAN_POINT('Ctrl Pts',(-25.3241152578369,87.38460819383,72.4210925622802));
#177664=CARTESIAN_POINT('Ctrl Pts',(-25.2347402578369,86.9610641626,76.249849747832));
#177665=CARTESIAN_POINT('Ctrl Pts',(-25.1453652578369,85.38276101444,79.7637835434));
#177666=CARTESIAN_POINT('Ctrl Pts',(-25.0559902578369,82.802073437376,82.623647685499));
#177667=CARTESIAN_POINT('Ctrl Pts',(-24.9666152578369,79.468149063245,84.55334187238));
#177668=CARTESIAN_POINT('Ctrl Pts',(-24.8772402578369,75.702855490151,85.36656733984));
#177669=CARTESIAN_POINT('Ctrl Pts',(-24.7878652578369,71.869706029794,84.98481273641));
#177670=CARTESIAN_POINT('Ctrl Pts',(-24.6984902578369,68.338765023158,83.44493385557));
#177671=CARTESIAN_POINT('Ctrl Pts',(-24.6091152578369,65.450920651772,80.895595461536));
#177672=CARTESIAN_POINT('Ctrl Pts',(-24.5197402578369,63.48497452013,77.582918723914));
#177673=CARTESIAN_POINT('Ctrl Pts',(-24.4303652578369,62.63072526867,73.8267199037072));
#177674=CARTESIAN_POINT('Ctrl Pts',(-24.3409902578369,62.97064481461,69.989634282714));
#177675=CARTESIAN_POINT('Ctrl Pts',(-24.2516152578369,64.47191625279,66.442106209615));
#177676=CARTESIAN_POINT('Ctrl Pts',(-24.1622402578369,66.98960210332,63.526625234101));
#177677=CARTESIAN_POINT('Ctrl Pts',(-24.0728652578369,70.280637032969,61.52466108548));
#177678=CARTESIAN_POINT('Ctrl Pts',(-23.9834902578369,74.0272941491374,
60.62948969719));
#177679=CARTESIAN_POINT('Ctrl Pts',(-23.8941152578369,77.867859356231,60.92753373859));
#177680=CARTESIAN_POINT('Ctrl Pts',(-23.8047402578369,81.431552375351,62.39001909784));
#177681=CARTESIAN_POINT('Ctrl Pts',(-23.7153652578369,84.374323041932,64.875752825426));
#177682=CARTESIAN_POINT('Ctrl Pts',(-23.6259902578369,86.41206699382,68.144754346856));
#177683=CARTESIAN_POINT('Ctrl Pts',(-23.5366152578369,87.34805400249,71.881423944257));
#177684=CARTESIAN_POINT('Ctrl Pts',(-23.4472402578369,87.09192092988,75.725011748597));
#177685=CARTESIAN_POINT('Ctrl Pts',(-23.3578652578369,85.6683956707,79.304445669906));
#177686=CARTESIAN_POINT('Ctrl Pts',(-23.2684902578369,83.214909843509,82.274155867272));
#177687=CARTESIAN_POINT('Ctrl Pts',(-23.1791152578369,79.968330708787,84.34743715126));
#177688=CARTESIAN_POINT('Ctrl Pts',(-23.0897402578369,76.242093256469,85.32412840723));
#177689=CARTESIAN_POINT('Ctrl Pts',(-23.0003652578379,72.395940203395,85.10993678068));
#177690=CARTESIAN_POINT('Ctrl Pts',(-22.9109902578379,68.801191296739,83.72554100684));
#177691=CARTESIAN_POINT('Ctrl Pts',(-22.8216152578379,65.804894934405,81.304595020325));
#177692=CARTESIAN_POINT('Ctrl Pts',(-22.7322402578379,63.69632301805,78.080824582763));
#177693=CARTESIAN_POINT('Ctrl Pts',(-22.6428652578379,62.67904373127,74.365462660522));
#177694=CARTESIAN_POINT('Ctrl Pts',(-22.5534902578379,62.8512684251,70.517202012466));
#177695=CARTESIAN_POINT('Ctrl Pts',(-22.4641152578379,64.19636998435,66.907565859634));
#177696=CARTESIAN_POINT('Ctrl Pts',(-22.3747402578379,66.584488061824,63.885039861635));
#177697=CARTESIAN_POINT('Ctrl Pts',(-22.2853652578379,69.785066205781,61.74142821188));
#177698=CARTESIAN_POINT('Ctrl Pts',(-22.1959902578379,73.489110507031,60.68368194036));
#177699=CARTESIAN_POINT('Ctrl Pts',(-22.1066152578379,77.339020845536,60.81391920844));
#177700=CARTESIAN_POINT('Ctrl Pts',(-22.0172402578379,80.963114733938,62.11956649947));
#177701=CARTESIAN_POINT('Ctrl Pts',(-21.9278652578379,84.011510717237,64.474572505729));
#177702=CARTESIAN_POINT('Ctrl Pts',(-21.8384902578379,86.18990703204,67.651577519286));
#177703=CARTESIAN_POINT('Ctrl Pts',(-21.7491152578379,87.28799442708,71.343863455311));
#177704=CARTESIAN_POINT('Ctrl Pts',(-21.6597402578379,87.19976008168,75.194965383434));
#177705=CARTESIAN_POINT('Ctrl Pts',(-21.5703652578379,85.93372241786,78.833085776477));
#177706=CARTESIAN_POINT('Ctrl Pts',(-21.4809902578379,83.612108704975,81.90698901644));
#177707=CARTESIAN_POINT('Ctrl Pts',(-21.3916152578379,80.459054853646,84.11991078892));
#177708=CARTESIAN_POINT('Ctrl Pts',(-21.3022402578379,76.77896662795,85.25820864606));
#177709=CARTESIAN_POINT('Ctrl Pts',(-21.2128652578379,72.92713135283,85.21198772236));
#177710=CARTESIAN_POINT('Ctrl Pts',(-21.1234902578379,69.27541735508,83.98571033155));
#177711=CARTESIAN_POINT('Ctrl Pts',(-21.0341152578379,66.176372622231,81.697765160933));
#177712=CARTESIAN_POINT('Ctrl Pts',(-20.9447402578379,63.9291887075,78.569037653464));
#177713=CARTESIAN_POINT('Ctrl Pts',(-20.8553652578379,62.75081583481,74.90158503273));
#177714=CARTESIAN_POINT('Ctrl Pts',(-20.7659902578379,62.75501783514,71.049474737007));
#177715=CARTESIAN_POINT('Ctrl Pts',(-20.6766152578379,63.94138904505,67.384601665003));
#177716=CARTESIAN_POINT('Ctrl Pts',(-20.5872402578379,66.195393405158,64.260784146057));
#177717=CARTESIAN_POINT('Ctrl Pts',(-20.4978652578379,69.299422377156,61.97960566264));
#177718=CARTESIAN_POINT('Ctrl Pts',(-20.4084902578379,72.953802645656,60.7612973129));
#177719=CARTESIAN_POINT('Ctrl Pts',(-20.3191152578379,76.805730932023,60.72348241298));
#177720=CARTESIAN_POINT('Ctrl Pts',(-20.2297402578379,80.48332202154,61.86979685924));
#177721=CARTESIAN_POINT('Ctrl Pts',(-20.1403652578379,83.631559184886,64.089627347503));
#177722=CARTESIAN_POINT('Ctrl Pts',(-20.0807819245039,85.17478074676,66.1421806368));
#177723=CARTESIAN_POINT('Ctrl Pts',(-20.0509902578369,85.7703123683,67.262212718386));
#177724=CARTESIAN_POINT('Ctrl Pts',(-29.0130799422609,72.422116845822,84.91151378796));
#177725=CARTESIAN_POINT('Ctrl Pts',(-28.9648716383109,70.415792799191,84.47771089461));
#177726=CARTESIAN_POINT('Ctrl Pts',(-28.8684550304109,66.629418901909,82.576109782766));
#177727=CARTESIAN_POINT('Ctrl Pts',(-28.7238301185509,63.03626406749,77.331337332641));
#177728=CARTESIAN_POINT('Ctrl Pts',(-28.5792052067009,62.42850598941,71.003271823318));
#177729=CARTESIAN_POINT('Ctrl Pts',(-28.4345802948509,64.95709911941,65.170572201634));
#177730=CARTESIAN_POINT('Ctrl Pts',(-28.2899553829909,69.991359600301,61.28849282187));
#177731=CARTESIAN_POINT('Ctrl Pts',(-28.1453304711409,76.275228322274,60.32557309628));
#177732=CARTESIAN_POINT('Ctrl Pts',(-28.0007055592909,82.240939818442,62.52205714543));
#177733=CARTESIAN_POINT('Ctrl Pts',(-27.8560806474309,86.40008997649,67.329937790089));
#177734=CARTESIAN_POINT('Ctrl Pts',(-27.7114557355809,87.71500271706,73.5496847895006));
#177735=CARTESIAN_POINT('Ctrl Pts',(-27.5668308237209,85.85761684592,79.629517497618));
#177736=CARTESIAN_POINT('Ctrl Pts',(-27.4222059118709,81.291336383219,84.05256291155));
#177737=CARTESIAN_POINT('Ctrl Pts',(-27.2775810000209,75.1554143062945,
85.71530411088));
#177738=CARTESIAN_POINT('Ctrl Pts',(-27.1329560881609,68.980717517489,84.20289954075));
#177739=CARTESIAN_POINT('Ctrl Pts',(-26.9883311763109,64.30778691511,79.892682886532));
#177740=CARTESIAN_POINT('Ctrl Pts',(-26.8437062644609,62.30248391102,73.860021128897));
#177741=CARTESIAN_POINT('Ctrl Pts',(-26.6990813526009,63.46511668212,67.610018484104));
#177742=CARTESIAN_POINT('Ctrl Pts',(-26.5544564407489,67.505617003827,62.70200410244));
#177743=CARTESIAN_POINT('Ctrl Pts',(-26.4098315288959,73.41591011336,60.36049104895));
#177744=CARTESIAN_POINT('Ctrl Pts',(-26.2652066170419,79.721421861612,61.1696694061));
#177745=CARTESIAN_POINT('Ctrl Pts',(-26.1205817051879,84.848973989789,64.927655195095));
#177746=CARTESIAN_POINT('Ctrl Pts',(-25.9759567933349,87.5192803998,70.696858927558));
#177747=CARTESIAN_POINT('Ctrl Pts',(-25.8313318814809,87.06611950964,77.037907200944));
#177748=CARTESIAN_POINT('Ctrl Pts',(-25.6867069696279,83.602551603711,82.368755669438));
#177749=CARTESIAN_POINT('Ctrl Pts',(-25.5420820577749,77.992711046048,85.35939726776));
#177750=CARTESIAN_POINT('Ctrl Pts',(-25.3974571459209,71.636211512424,85.26368932913));
#177751=CARTESIAN_POINT('Ctrl Pts',(-25.2528322340679,66.118951578813,82.105509685936));
#177752=CARTESIAN_POINT('Ctrl Pts',(-25.1082073222149,62.81744936158,76.672802844726));
#177753=CARTESIAN_POINT('Ctrl Pts',(-24.9635824103609,62.55539457204,70.320980571748));
#177754=CARTESIAN_POINT('Ctrl Pts',(-24.8189574985079,65.398207204844,64.634805721403));
#177755=CARTESIAN_POINT('Ctrl Pts',(-24.6743325866549,70.636480087695,61.03282290959));
#177756=CARTESIAN_POINT('Ctrl Pts',(-24.5297076748019,76.963850143509,60.4141243606));
#177757=CARTESIAN_POINT('Ctrl Pts',(-24.4332910668999,80.854379446751,62.092366244));
#177758=CARTESIAN_POINT('Ctrl Pts',(-24.3850827629489,82.476320069947,63.350471861665));
#177759=CARTESIAN_POINT('Ctrl Pts',(-29.1698979118309,72.358453566317,85.2059543519));
#177760=CARTESIAN_POINT('Ctrl Pts',(-29.1216896078809,70.302581436659,84.76143828298));
#177761=CARTESIAN_POINT('Ctrl Pts',(-29.0252729999709,66.42269943008,82.812875320713));
#177762=CARTESIAN_POINT('Ctrl Pts',(-28.8806480881209,62.74080821513,77.438578220143));
#177763=CARTESIAN_POINT('Ctrl Pts',(-28.7360231762609,62.11804097252,70.954235106618));
#177764=CARTESIAN_POINT('Ctrl Pts',(-28.5913982644109,64.70908011794,64.977491413082));
#177765=CARTESIAN_POINT('Ctrl Pts',(-28.4467733525609,69.867666455716,60.99954038599));
#177766=CARTESIAN_POINT('Ctrl Pts',(-28.3021484407009,76.306721300137,60.01284044075));
#177767=CARTESIAN_POINT('Ctrl Pts',(-28.1575235288509,82.419761723069,62.26356875528));
#177768=CARTESIAN_POINT('Ctrl Pts',(-28.0128986170009,86.68162605518,67.190184591183));
#177769=CARTESIAN_POINT('Ctrl Pts',(-27.8682737051409,88.02901181812,73.5635341660382));
#177770=CARTESIAN_POINT('Ctrl Pts',(-27.7236487932909,86.12575603404,79.793514132931));
#177771=CARTESIAN_POINT('Ctrl Pts',(-27.5790238814309,81.446706926677,84.32579086559));
#177772=CARTESIAN_POINT('Ctrl Pts',(-27.4343989695809,75.1592524105996,
86.02959504233));
#177773=CARTESIAN_POINT('Ctrl Pts',(-27.2897740577309,68.832065604203,84.47984020103));
#177774=CARTESIAN_POINT('Ctrl Pts',(-27.1451491458709,64.04373253039,80.063178641754));
#177775=CARTESIAN_POINT('Ctrl Pts',(-27.0005242340209,61.98890665889,73.8815345568893));
#177776=CARTESIAN_POINT('Ctrl Pts',(-26.8558993221709,63.18025175349,67.477182144676));
#177777=CARTESIAN_POINT('Ctrl Pts',(-26.7112744103109,67.320536078556,62.44795967377));
#177778=CARTESIAN_POINT('Ctrl Pts',(-26.5666494984599,73.376789505017,60.04862072552));
#177779=CARTESIAN_POINT('Ctrl Pts',(-26.4220245866059,79.838021870863,60.87778251281));
#177780=CARTESIAN_POINT('Ctrl Pts',(-26.2773996747519,85.092203782,64.728575339723));
#177781=CARTESIAN_POINT('Ctrl Pts',(-26.1327747628989,87.82845595185,70.640255052583));
#177782=CARTESIAN_POINT('Ctrl Pts',(-25.9881498510449,87.36410382194,77.137901551893));
#177783=CARTESIAN_POINT('Ctrl Pts',(-25.8435249391919,83.814999808094,82.600400400082));
#177784=CARTESIAN_POINT('Ctrl Pts',(-25.6989000273379,78.066618895403,85.66489874077));
#177785=CARTESIAN_POINT('Ctrl Pts',(-25.5542751154849,71.553139552267,85.56682720345));
#177786=CARTESIAN_POINT('Ctrl Pts',(-25.4096502036319,65.899625630305,82.330653306324));
#177787=CARTESIAN_POINT('Ctrl Pts',(-25.2650252917779,62.51658967167,76.763780595904));
#177788=CARTESIAN_POINT('Ctrl Pts',(-25.1204003799249,62.24806318954,70.25509402282));
#177789=CARTESIAN_POINT('Ctrl Pts',(-24.9757754680719,65.161081787626,64.428493669391));
#177790=CARTESIAN_POINT('Ctrl Pts',(-24.8311505562189,70.528718807919,60.73755646174));
#177791=CARTESIAN_POINT('Ctrl Pts',(-24.6865256443659,77.01234929305,60.10357856287));
#177792=CARTESIAN_POINT('Ctrl Pts',(-24.5901090364639,80.998958922529,61.82326622784));
#177793=CARTESIAN_POINT('Ctrl Pts',(-24.5419007325129,82.66095491405,63.112441961868));
#177794=CARTESIAN_POINT('Ctrl Pts',(-29.3267158813909,72.294790286804,85.50039491585));
#177795=CARTESIAN_POINT('Ctrl Pts',(-29.2785075774409,70.189370074118,85.04516567134));
#177796=CARTESIAN_POINT('Ctrl Pts',(-29.1820909695409,66.215979958243,83.04964085865));
#177797=CARTESIAN_POINT('Ctrl Pts',(-29.0374660576809,62.44535236276,77.545819107633));
#177798=CARTESIAN_POINT('Ctrl Pts',(-28.8928411458309,61.80757595563,70.905198389902));
#177799=CARTESIAN_POINT('Ctrl Pts',(-28.7482162339709,64.46106111648,64.784410624515));
#177800=CARTESIAN_POINT('Ctrl Pts',(-28.6035913221209,69.743973311151,60.7105879501));
#177801=CARTESIAN_POINT('Ctrl Pts',(-28.4589664102709,76.338214278025,59.70010778522));
#177802=CARTESIAN_POINT('Ctrl Pts',(-28.3143414984109,82.59858362772,62.00508036515));
#177803=CARTESIAN_POINT('Ctrl Pts',(-28.1697165865609,86.96316213389,67.050431392305));
#177804=CARTESIAN_POINT('Ctrl Pts',(-28.0250916747109,88.34302091918,73.5773835426106));
#177805=CARTESIAN_POINT('Ctrl Pts',(-27.8804667628509,86.39389522214,79.957510768277));
#177806=CARTESIAN_POINT('Ctrl Pts',(-27.7358418510009,81.6020774701,84.59901881965));
#177807=CARTESIAN_POINT('Ctrl Pts',(-27.5912169391409,75.163090514862,86.34388597378));
#177808=CARTESIAN_POINT('Ctrl Pts',(-27.4465920272909,68.683413690878,84.75678086128));
#177809=CARTESIAN_POINT('Ctrl Pts',(-27.3019671154409,63.77967814565,80.233674396936));
#177810=CARTESIAN_POINT('Ctrl Pts',(-27.1573422035809,61.67532940676,73.903047984833));
#177811=CARTESIAN_POINT('Ctrl Pts',(-27.0127172917309,62.89538682488,67.344345805202));
#177812=CARTESIAN_POINT('Ctrl Pts',(-26.8680923798809,67.135455153326,62.19391524507));
#177813=CARTESIAN_POINT('Ctrl Pts',(-26.7234674680209,73.337668896726,59.73675040207));
#177814=CARTESIAN_POINT('Ctrl Pts',(-26.5788425561709,79.954621880163,60.58589561953));
#177815=CARTESIAN_POINT('Ctrl Pts',(-26.4342176443159,85.33543357425,64.52949548439));
#177816=CARTESIAN_POINT('Ctrl Pts',(-26.2895927324629,88.1376315039,70.583651177657));
#177817=CARTESIAN_POINT('Ctrl Pts',(-26.1449678206089,87.66208813423,77.237895902889));
#177818=CARTESIAN_POINT('Ctrl Pts',(-26.0003429087559,84.027448012443,82.832045130756));
#177819=CARTESIAN_POINT('Ctrl Pts',(-25.8557179969019,78.140526744715,85.9704002138));
#177820=CARTESIAN_POINT('Ctrl Pts',(-25.7110930850489,71.470067592072,85.86996507777));
#177821=CARTESIAN_POINT('Ctrl Pts',(-25.5664681731959,65.680299681772,82.555796926686));
#177822=CARTESIAN_POINT('Ctrl Pts',(-25.4218432613419,62.21572998176,76.854758347052));
#177823=CARTESIAN_POINT('Ctrl Pts',(-25.2772183494889,61.94073180705,70.189207473868));
#177824=CARTESIAN_POINT('Ctrl Pts',(-25.1325934376359,64.92395637042,64.222181617367));
#177825=CARTESIAN_POINT('Ctrl Pts',(-24.9879685257829,70.420957528155,60.44229001389));
#177826=CARTESIAN_POINT('Ctrl Pts',(-24.8433436139299,77.060848442593,59.79303276515));
#177827=CARTESIAN_POINT('Ctrl Pts',(-24.7469270060279,81.143538398306,61.55416621167));
#177828=CARTESIAN_POINT('Ctrl Pts',(-24.6987187020769,82.845589758148,62.87441206207));
#177829=CARTESIAN_POINT('Ctrl Pts',(-29.4835338509509,72.2311270073,85.79483547979));
#177830=CARTESIAN_POINT('Ctrl Pts',(-29.4353255470009,70.076158711586,85.32889305971));
#177831=CARTESIAN_POINT('Ctrl Pts',(-29.3389089391009,66.009260486414,83.2864063966));
#177832=CARTESIAN_POINT('Ctrl Pts',(-29.1942840272509,62.14989651041,77.653059995135));
#177833=CARTESIAN_POINT('Ctrl Pts',(-29.0496591153909,61.49711093875,70.856161673202));
#177834=CARTESIAN_POINT('Ctrl Pts',(-28.9050342035409,64.21304211501,64.591329835963));
#177835=CARTESIAN_POINT('Ctrl Pts',(-28.7604092916909,69.620280166566,60.42163551422));
#177836=CARTESIAN_POINT('Ctrl Pts',(-28.6157843798309,76.369707255888,59.38737512969));
#177837=CARTESIAN_POINT('Ctrl Pts',(-28.4711594679809,82.777405532348,61.74659197501));
#177838=CARTESIAN_POINT('Ctrl Pts',(-28.3265345561209,87.24469821258,66.9106781934));
#177839=CARTESIAN_POINT('Ctrl Pts',(-28.1819096442709,88.65703002025,73.5912329191485));
#177840=CARTESIAN_POINT('Ctrl Pts',(-28.0372847324209,86.66203441026,80.12150740359));
#177841=CARTESIAN_POINT('Ctrl Pts',(-27.8926598205609,81.757448013558,84.87224677369));
#177842=CARTESIAN_POINT('Ctrl Pts',(-27.7480349087109,75.1669286191668,
86.65817690523));
#177843=CARTESIAN_POINT('Ctrl Pts',(-27.6034099968509,68.534761777592,85.03372152155));
#177844=CARTESIAN_POINT('Ctrl Pts',(-27.4587850850009,63.51562376093,80.404170152158));
#177845=CARTESIAN_POINT('Ctrl Pts',(-27.3141601731509,61.36175215463,73.924561412825));
#177846=CARTESIAN_POINT('Ctrl Pts',(-27.1695352612909,62.61052189625,67.211509465773));
#177847=CARTESIAN_POINT('Ctrl Pts',(-27.0249103494409,66.950374228055,61.9398708164));
#177848=CARTESIAN_POINT('Ctrl Pts',(-26.8802854375909,73.298548288383,59.42488007864));
#177849=CARTESIAN_POINT('Ctrl Pts',(-26.7356605257309,80.071221889414,60.29400872623));
#177850=CARTESIAN_POINT('Ctrl Pts',(-26.5910356138809,85.57866336647,64.330415629018));
#177851=CARTESIAN_POINT('Ctrl Pts',(-26.4464107020269,88.44680705594,70.527047302681));
#177852=CARTESIAN_POINT('Ctrl Pts',(-26.3017857901729,87.96007244653,77.337890253839));
#177853=CARTESIAN_POINT('Ctrl Pts',(-26.1571608783199,84.239896216826,83.0636898614));
#177854=CARTESIAN_POINT('Ctrl Pts',(-26.0125359664659,78.21443459407,86.27590168681));
#177855=CARTESIAN_POINT('Ctrl Pts',(-25.8679110546129,71.386995631916,86.17310295209));
#177856=CARTESIAN_POINT('Ctrl Pts',(-25.7232861427599,65.460973733264,82.780940547073));
#177857=CARTESIAN_POINT('Ctrl Pts',(-25.5786612309059,61.91487029185,76.94573609823));
#177858=CARTESIAN_POINT('Ctrl Pts',(-25.4340363190529,61.63340042455,70.12332092494));
#177859=CARTESIAN_POINT('Ctrl Pts',(-25.2894114071999,64.6868309532,64.015869565355));
#177860=CARTESIAN_POINT('Ctrl Pts',(-25.1447864953469,70.313196248379,60.14702356604));
#177861=CARTESIAN_POINT('Ctrl Pts',(-25.0001615834929,77.109347592134,59.48248696742));
#177862=CARTESIAN_POINT('Ctrl Pts',(-24.9037449755909,81.288117874084,61.28506619551));
#177863=CARTESIAN_POINT('Ctrl Pts',(-24.8555366716399,83.03022460225,62.63638216227));
#177864=CARTESIAN_POINT('Origin',(-18.5675364832709,75.,72.98888938658));
#177865=CARTESIAN_POINT('Origin',(-16.5675364832709,75.,72.98888938658));
#177866=CARTESIAN_POINT('',(0.,0.,0.));
#177867=CARTESIAN_POINT('Origin',(-20.5675364832709,75.,72.98888938658));
#177868=CARTESIAN_POINT('',(-20.5675364832709,75.,82.48888938658));
#177869=CARTESIAN_POINT('Origin',(-20.5675364832709,75.,72.98888938658));
#177870=CARTESIAN_POINT('',(-20.5675364832709,75.,82.98888938658));
#177871=CARTESIAN_POINT('Origin',(-20.5675364832709,75.,82.73888938658));
#177872=CARTESIAN_POINT('Origin',(-20.5675364832709,75.,72.98888938658));
#177873=CARTESIAN_POINT('Origin',(-20.5675364832709,75.,72.98888938658));
#177874=CARTESIAN_POINT('',(-20.5675364832709,75.,83.98888938658));
#177875=CARTESIAN_POINT('Origin',(-20.5675364832709,75.,72.98888938658));
#177876=CARTESIAN_POINT('',(-20.5675364832709,75.,84.48888938658));
#177877=CARTESIAN_POINT('Origin',(-20.5675364832709,75.,84.23888938658));
#177878=CARTESIAN_POINT('Origin',(-20.5675364832709,75.,72.98888938658));
#177879=CARTESIAN_POINT('Origin',(-25.5675364832709,75.,72.98888938658));
#177880=CARTESIAN_POINT('',(-20.5675364832709,75.,85.08888938658));
#177881=CARTESIAN_POINT('Origin',(-20.5675364832709,75.,72.98888938658));
#177882=CARTESIAN_POINT('',(-22.5675364832709,75.,85.08888938658));
#177883=CARTESIAN_POINT('',(-25.5675364832709,75.,85.08888938658));
#177884=CARTESIAN_POINT('',(-22.5675364832709,70.2930278873758,84.1358357635471));
#177885=CARTESIAN_POINT('Origin',(-22.5675364832709,75.,72.98888938658));
#177886=CARTESIAN_POINT('',(-21.7675364832709,70.2930278873758,84.1358357635471));
#177887=CARTESIAN_POINT('',(-22.1675364832709,70.2930278873758,84.1358357635471));
#177888=CARTESIAN_POINT('',(-21.7675364832709,67.6999473192355,82.6387199995009));
#177889=CARTESIAN_POINT('Origin',(-21.7675364832709,75.,72.98888938658));
#177890=CARTESIAN_POINT('',(-22.5675364832709,67.6999473192355,82.6387199995009));
#177891=CARTESIAN_POINT('',(-22.1675364832709,67.6999473192355,82.6387199995009));
#177892=CARTESIAN_POINT('',(-22.5675364832709,67.6999473192356,63.3390587736591));
#177893=CARTESIAN_POINT('Origin',(-22.5675364832709,75.,72.98888938658));
#177894=CARTESIAN_POINT('',(-21.7675364832709,67.6999473192356,63.3390587736591));
#177895=CARTESIAN_POINT('',(-22.1675364832709,67.6999473192356,63.3390587736591));
#177896=CARTESIAN_POINT('',(-21.7675364832709,70.2930278873759,61.8419430096129));
#177897=CARTESIAN_POINT('Origin',(-21.7675364832709,75.,72.98888938658));
#177898=CARTESIAN_POINT('',(-22.5675364832709,70.2930278873759,61.8419430096129));
#177899=CARTESIAN_POINT('',(-22.1675364832709,70.2930278873759,61.8419430096129));
#177900=CARTESIAN_POINT('',(-22.5675364832709,87.0070247933884,71.4917736225339));
#177901=CARTESIAN_POINT('Origin',(-22.5675364832709,75.,72.98888938658));
#177902=CARTESIAN_POINT('',(-21.7675364832709,87.0070247933884,71.4917736225339));
#177903=CARTESIAN_POINT('',(-22.1675364832709,87.0070247933884,71.4917736225339));
#177904=CARTESIAN_POINT('',(-21.7675364832709,87.0070247933884,74.4860051506262));
#177905=CARTESIAN_POINT('Origin',(-21.7675364832709,75.,72.98888938658));
#177906=CARTESIAN_POINT('',(-22.5675364832709,87.0070247933884,74.4860051506262));
#177907=CARTESIAN_POINT('',(-22.1675364832709,87.0070247933884,74.4860051506262));
#177908=CARTESIAN_POINT('Origin',(-22.5675364832709,75.,72.98888938658));
#177909=CARTESIAN_POINT('Origin',(-22.5675364832709,75.,72.98888938658));
#177910=CARTESIAN_POINT('',(-22.5675364832709,75.,84.48888938658));
#177911=CARTESIAN_POINT('Origin',(-22.5675364832709,75.,72.98888938658));
#177912=CARTESIAN_POINT('',(-22.5675364832709,75.,83.98888938658));
#177913=CARTESIAN_POINT('Origin',(-22.5675364832709,75.,84.23888938658));
#177914=CARTESIAN_POINT('Origin',(-22.5675364832709,75.,72.98888938658));
#177915=CARTESIAN_POINT('Origin',(-22.5675364832709,75.,72.98888938658));
#177916=CARTESIAN_POINT('',(-22.5675364832709,75.,82.98888938658));
#177917=CARTESIAN_POINT('Origin',(-22.5675364832709,75.,72.98888938658));
#177918=CARTESIAN_POINT('',(-22.5675364832709,75.,82.48888938658));
#177919=CARTESIAN_POINT('Origin',(-22.5675364832709,75.,82.73888938658));
#177920=CARTESIAN_POINT('Origin',(-22.5675364832709,75.,72.98888938658));
#177921=CARTESIAN_POINT('Origin',(-25.5675364832709,75.,72.98888938658));
#177922=CARTESIAN_POINT('',(-22.5675364832709,75.,80.48888938658));
#177923=CARTESIAN_POINT('Origin',(-22.5675364832709,75.,72.98888938658));
#177924=CARTESIAN_POINT('',(-20.5675364832709,75.,80.48888938658));
#177925=CARTESIAN_POINT('',(-25.5675364832709,75.,80.48888938658));
#177926=CARTESIAN_POINT('Origin',(-20.5675364832709,75.,72.98888938658));
#177927=CARTESIAN_POINT('Origin',(-21.7675364832709,87.1,72.98888938658));
#177928=CARTESIAN_POINT('Origin',(-21.7675364832709,87.1,72.98888938658));
#177929=CARTESIAN_POINT('Origin',(-22.5675364832709,87.1,72.98888938658));
#177930=CARTESIAN_POINT('Origin',(-21.7675364832709,68.95,83.4677967723717));
#177931=CARTESIAN_POINT('Origin',(-21.7675364832709,68.95,83.4677967723717));
#177932=CARTESIAN_POINT('Origin',(-22.5675364832709,68.95,83.4677967723717));
#177933=CARTESIAN_POINT('Origin',(-21.7675364832709,68.95,83.4677967723717));
#177934=CARTESIAN_POINT('Origin',(-21.7675364832709,68.95,62.5099820007883));
#177935=CARTESIAN_POINT('Origin',(-21.7675364832709,68.95,62.5099820007883));
#177936=CARTESIAN_POINT('Origin',(-21.7675364832709,68.95,62.5099820007883));
#177937=CARTESIAN_POINT('Origin',(-22.5675364832709,68.95,62.5099820007883));
#177938=CARTESIAN_POINT('Origin',(-21.7675364832709,87.1,72.98888938658));
#177939=CARTESIAN_POINT('Origin',(-20.5675364832709,67.5,72.98888938658));
#177940=CARTESIAN_POINT('Origin',(-22.5675364832709,65.5,72.98888938658));
#177941=CARTESIAN_POINT('Origin',(-22.5675364832709,64.,72.98888938658));
#177942=CARTESIAN_POINT('Origin',(-22.5675364832709,62.9,72.98888938658));
#177943=CARTESIAN_POINT('Origin',(-20.5675364832709,63.5,72.98888938658));
#177944=CARTESIAN_POINT('Origin',(-20.5675364832709,65.,72.98888938658));
#177945=CARTESIAN_POINT('',(0.,0.,0.));
#177946=CARTESIAN_POINT('Origin',(-30.5675364832709,75.,72.98888938658));
#177947=CARTESIAN_POINT('',(-29.5675364832709,50.5080487007827,62.8698826100749));
#177948=CARTESIAN_POINT('Origin',(-29.5675364832709,75.,72.98888938658));
#177949=CARTESIAN_POINT('',(-30.5675364832709,49.5838236997517,62.4880331226987));
#177950=CARTESIAN_POINT('Origin',(-30.5675364832709,50.508048292488,62.8698824413853));
#177951=CARTESIAN_POINT('Origin',(-30.5675364832709,75.,72.98888938658));
#177952=CARTESIAN_POINT('Origin',(-50.5675364832709,75.,72.98888938658));
#177953=CARTESIAN_POINT('',(-50.5675364832709,49.5838236997517,62.4880331226987));
#177954=CARTESIAN_POINT('',(-50.5675364832709,49.5838236997517,62.4880331226987));
#177955=CARTESIAN_POINT('Origin',(-50.5675364832709,75.,72.98888938658));
#177956=CARTESIAN_POINT('Origin',(-50.5675364832709,75.,72.98888938658));
#177957=CARTESIAN_POINT('',(-30.6675364832709,72.1690856026562,85.0614170289144));
#177958=CARTESIAN_POINT('',(-30.6675364832709,68.4842284934922,83.5389946787084));
#177959=CARTESIAN_POINT('Origin',(-30.6675364832709,75.,72.98888938658));
#177960=CARTESIAN_POINT('',(-31.1675364832709,72.1690856026562,85.0614170289144));
#177961=CARTESIAN_POINT('',(-31.1675364832709,72.1690856026562,85.0614170289144));
#177962=CARTESIAN_POINT('',(-31.1675364832709,68.4842284934922,83.5389946787084));
#177963=CARTESIAN_POINT('Origin',(-31.1675364832709,75.,72.98888938658));
#177964=CARTESIAN_POINT('',(-31.1675364832709,68.4842284934922,83.5389946787084));
#177965=CARTESIAN_POINT('Origin',(-50.5675364832709,70.2650684482863,84.4492743365102));
#177966=CARTESIAN_POINT('Origin',(-30.6675364832709,70.2650684482863,84.4492743365102));
#177967=CARTESIAN_POINT('Origin',(-31.1675364832709,70.2650684482863,84.4492743365102));
#177968=CARTESIAN_POINT('Origin',(-30.5675364832709,75.,72.98888938658));
#177969=CARTESIAN_POINT('',(-30.5675364832709,50.0459359961198,62.678957782042));
#177970=CARTESIAN_POINT('Origin',(-30.5675364832709,75.,72.98888938658));
#177971=CARTESIAN_POINT('',(-30.0675364832709,50.508048292488,62.8698824413853));
#177972=CARTESIAN_POINT('Origin',(-30.5675364832709,50.508048292488,62.8698824413853));
#177973=CARTESIAN_POINT('Origin',(-30.0675364832709,75.,72.98888938658));
#177974=CARTESIAN_POINT('Origin',(-50.5675364832709,75.,72.98888938658));
#177975=CARTESIAN_POINT('',(-50.5675364832709,50.0459359961198,62.678957782042));
#177976=CARTESIAN_POINT('Origin',(-50.5675364832709,75.,72.98888938658));
#177977=CARTESIAN_POINT('',(-50.5675364832709,50.0459359961198,62.678957782042));
#177978=CARTESIAN_POINT('Origin',(-30.6175364832709,75.,72.98888938658));
#177979=CARTESIAN_POINT('',(-30.0675364832709,60.269085605794,66.9027176170056));
#177980=CARTESIAN_POINT('Origin',(-30.0675364832709,75.,72.98888938658));
#177981=CARTESIAN_POINT('',(-31.1675364832709,61.4243663467144,67.3800292653639));
#177982=CARTESIAN_POINT('',(-30.6175364832709,60.8467259762541,67.1413734411847));
#177983=CARTESIAN_POINT('Origin',(-31.1675364832709,75.,72.98888938658));
#177984=CARTESIAN_POINT('Origin',(-30.0675364832709,75.,72.98888938658));
#177985=CARTESIAN_POINT('Origin',(-31.1675364832709,75.,72.98888938658));
#177986=CARTESIAN_POINT('Origin',(-30.6675364832709,75.,72.98888938658));
#177987=CARTESIAN_POINT('',(-30.6675364832709,61.5987434053236,67.4520742656245));
#177988=CARTESIAN_POINT('Origin',(-30.6675364832709,75.,72.98888938658));
#177989=CARTESIAN_POINT('Origin',(-30.1175364832709,75.,72.98888938658));
#177990=CARTESIAN_POINT('',(-29.5675364832709,60.4434626644033,66.9747626172662));
#177991=CARTESIAN_POINT('',(-30.1175364832709,61.0211030348634,67.2134184414453));
#177992=CARTESIAN_POINT('Origin',(-29.5675364832709,75.,72.98888938658));
#177993=CARTESIAN_POINT('Origin',(-29.5675364832709,75.,72.98888938658));
#177994=CARTESIAN_POINT('Origin',(-50.5675364832709,75.,72.98888938658));
#177995=CARTESIAN_POINT('',(0.,0.,0.));
#177996=CARTESIAN_POINT('Origin',(-23.90845228375,-75.0031087425464,72.9873550812444));
#177997=CARTESIAN_POINT('',(-23.2177969711981,-75.0031087425464,59.9387052680259));
#177998=CARTESIAN_POINT('',(-23.5174110875174,-75.0031087425464,59.9387052680259));
#177999=CARTESIAN_POINT('',(-23.90845228375,-75.0031087425464,59.9387052680259));
#178000=CARTESIAN_POINT('',(-24.4189072313413,-75.0031417059253,86.0360048944213));
#178001=CARTESIAN_POINT('Ctrl Pts',(-23.5174110875174,-75.0031087425464,
59.9387052680259));
#178002=CARTESIAN_POINT('Ctrl Pts',(-23.5258740395449,-75.3885856088758,
59.9387052680259));
#178003=CARTESIAN_POINT('Ctrl Pts',(-23.5343495220848,-75.7740190949249,
59.9557866063909));
#178004=CARTESIAN_POINT('Ctrl Pts',(-23.5617944162149,-77.0283277708885,
60.067265150459));
#178005=CARTESIAN_POINT('Ctrl Pts',(-23.5806373594291,-77.8884227880291,
60.2317600988326));
#178006=CARTESIAN_POINT('Ctrl Pts',(-23.6089443886813,-79.1242668073003,
60.5996061157332));
#178007=CARTESIAN_POINT('Ctrl Pts',(-23.6181074284407,-79.5170208469362,
60.7372585206103));
#178008=CARTESIAN_POINT('Ctrl Pts',(-23.6431780322771,-80.5789266596909,
61.1674516227681));
#178009=CARTESIAN_POINT('Ctrl Pts',(-23.6589117584693,-81.2311459690073,
61.497732867221));
#178010=CARTESIAN_POINT('Ctrl Pts',(-23.68934766305,-82.414672015085,62.2275925132549));
#178011=CARTESIAN_POINT('Ctrl Pts',(-23.7039535895129,-82.9498688086055,
62.616590314994));
#178012=CARTESIAN_POINT('Ctrl Pts',(-23.7347491794576,-84.0220013905403,
63.5277639727065));
#178013=CARTESIAN_POINT('Ctrl Pts',(-23.7508786121394,-84.5481913996176,
64.0589906959572));
#178014=CARTESIAN_POINT('Ctrl Pts',(-23.7819901432446,-85.4556145331789,
65.1475589814397));
#178015=CARTESIAN_POINT('Ctrl Pts',(-23.7968526295174,-85.8447759766575,
65.6951994335084));
#178016=CARTESIAN_POINT('Ctrl Pts',(-23.8226701199644,-86.452147742019,
66.706757312822));
#178017=CARTESIAN_POINT('Ctrl Pts',(-23.8337287308387,-86.6884310827492,
67.1581488692751));
#178018=CARTESIAN_POINT('Ctrl Pts',(-23.8637678447263,-87.2523286094977,
68.4083152461614));
#178019=CARTESIAN_POINT('Ctrl Pts',(-23.882921492897,-87.5281114458154,
69.22766109732));
#178020=CARTESIAN_POINT('Ctrl Pts',(-23.9138265338306,-87.8435897107306,
70.6021111891274));
#178021=CARTESIAN_POINT('Ctrl Pts',(-23.9257488716751,-87.9323958052821,
71.1432084592251));
#178022=CARTESIAN_POINT('Ctrl Pts',(-23.9524410857355,-88.0533393736483,
72.352000542165));
#178023=CARTESIAN_POINT('Ctrl Pts',(-23.9672449577233,-88.068755849995,
73.0198351480965));
#178024=CARTESIAN_POINT('Ctrl Pts',(-24.0010417074449,-87.9867815343067,
74.5488835393699));
#178025=CARTESIAN_POINT('Ctrl Pts',(-24.0197803191019,-87.8548981206235,
75.4051312796587));
#178026=CARTESIAN_POINT('Ctrl Pts',(-24.057933133333,-87.4242752312913,
77.0770172011696));
#178027=CARTESIAN_POINT('Ctrl Pts',(-24.0770391433777,-87.1269764979674,
77.8886355774496));
#178028=CARTESIAN_POINT('Ctrl Pts',(-24.1052341797259,-86.5675808489017,
79.0461925561804));
#178029=CARTESIAN_POINT('Ctrl Pts',(-24.1145281505967,-86.3649112316087,
79.4182158163765));
#178030=CARTESIAN_POINT('Ctrl Pts',(-24.1388756575297,-85.7912380572986,
80.3592018984337));
#178031=CARTESIAN_POINT('Ctrl Pts',(-24.1540139134244,-85.3932895243157,
80.9102335930352));
#178032=CARTESIAN_POINT('Ctrl Pts',(-24.1885571156498,-84.3793035702454,
82.1057102021331));
#178033=CARTESIAN_POINT('Ctrl Pts',(-24.2079565921027,-83.7365453105005,
82.723089235518));
#178034=CARTESIAN_POINT('Ctrl Pts',(-24.2355717066776,-82.7562314143682,
83.4888987406805));
#178035=CARTESIAN_POINT('Ctrl Pts',(-24.2434729123377,-82.4676211814838,
83.6959677129961));
#178036=CARTESIAN_POINT('Ctrl Pts',(-24.2704762780277,-81.4487495403035,
84.365751152243));
#178037=CARTESIAN_POINT('Ctrl Pts',(-24.2892701843075,-80.6811917885786,
84.7675739845685));
#178038=CARTESIAN_POINT('Ctrl Pts',(-24.326542154466,-79.1204700528668,
85.3963986786834));
#178039=CARTESIAN_POINT('Ctrl Pts',(-24.3447363405948,-78.3342799627899,
85.6301527642972));
#178040=CARTESIAN_POINT('Ctrl Pts',(-24.3813496645858,-76.6986863541472,
85.9531842222863));
#178041=CARTESIAN_POINT('Ctrl Pts',(-24.4000561482487,-75.8519283269992,
86.0360027502243));
#178042=CARTESIAN_POINT('Ctrl Pts',(-24.4189072313414,-75.0031417059253,
86.0360048944213));
#178043=CARTESIAN_POINT('',(-25.2173493892328,-70.5370130173974,60.7268819234023));
#178044=CARTESIAN_POINT('Ctrl Pts',(-25.2179534601443,-70.5369625382682,
60.7268167557867));
#178045=CARTESIAN_POINT('Ctrl Pts',(-25.1949255782263,-69.5510845400866,
61.0859425268238));
#178046=CARTESIAN_POINT('Ctrl Pts',(-25.1723485468244,-68.6121132844695,
61.5626729666513));
#178047=CARTESIAN_POINT('Ctrl Pts',(-25.1418319224832,-67.4503279249558,
62.3410093155562));
#178048=CARTESIAN_POINT('Ctrl Pts',(-25.1341597941179,-67.168164933375,
62.546912976461));
#178049=CARTESIAN_POINT('Ctrl Pts',(-25.1058958914003,-66.1590701068227,
63.3472530553906));
#178050=CARTESIAN_POINT('Ctrl Pts',(-25.0856284897384,-65.4886400931649,
64.0082978440766));
#178051=CARTESIAN_POINT('Ctrl Pts',(-25.0463381621821,-64.3476753322238,
65.4059328423162));
#178052=CARTESIAN_POINT('Ctrl Pts',(-25.0272324006768,-63.8684396267926,
66.1291213644448));
#178053=CARTESIAN_POINT('Ctrl Pts',(-24.9900396375432,-63.0713109933876,
67.638717086007));
#178054=CARTESIAN_POINT('Ctrl Pts',(-24.9718326777438,-62.7512240802528,
68.4193091338589));
#178055=CARTESIAN_POINT('Ctrl Pts',(-24.9272869194739,-62.167302597689,
70.3586157342146));
#178056=CARTESIAN_POINT('Ctrl Pts',(-24.9018234838554,-61.9818391597063,
71.5331436490922));
#178057=CARTESIAN_POINT('Ctrl Pts',(-24.8571030316205,-61.939606164877,
73.5672948670295));
#178058=CARTESIAN_POINT('Ctrl Pts',(-24.8383743123942,-62.0052128063284,
74.4177895566878));
#178059=CARTESIAN_POINT('Ctrl Pts',(-24.8106986129752,-62.2258618857267,
75.6676798065923));
#178060=CARTESIAN_POINT('Ctrl Pts',(-24.8016093736651,-62.3183287152197,
76.0758065751899));
#178061=CARTESIAN_POINT('Ctrl Pts',(-24.7773198416253,-62.6143520358101,
77.1418062935212));
#178062=CARTESIAN_POINT('Ctrl Pts',(-24.7620753388425,-62.8506276162574,
77.7892260852831));
#178063=CARTESIAN_POINT('Ctrl Pts',(-24.730838002126,-63.4428299151513,
79.083938962895));
#178064=CARTESIAN_POINT('Ctrl Pts',(-24.7149083735733,-63.8048278788549,
79.7258182827486));
#178065=CARTESIAN_POINT('Ctrl Pts',(-24.687301631946,-64.509686240891,80.7605121738516));
#178066=CARTESIAN_POINT('Ctrl Pts',(-24.6758558722316,-64.8254709287872,
81.169627195189));
#178067=CARTESIAN_POINT('Ctrl Pts',(-24.6475001697529,-65.6709139270774,
82.1400231901055));
#178068=CARTESIAN_POINT('Ctrl Pts',(-24.6307810261119,-66.2276452856273,
82.6751014390459));
#178069=CARTESIAN_POINT('Ctrl Pts',(-24.5995857708681,-67.3310996828718,
83.5620240742223));
#178070=CARTESIAN_POINT('Ctrl Pts',(-24.5852411678063,-67.8631451133042,
83.9282997510201));
#178071=CARTESIAN_POINT('Ctrl Pts',(-24.5583913263179,-68.9148227684136,
84.5428023817671));
#178072=CARTESIAN_POINT('Ctrl Pts',(-24.5458806664972,-69.42805990607,84.7989772586328));
#178073=CARTESIAN_POINT('Ctrl Pts',(-24.514390222347,-70.7504543245645,
85.3535788428957));
#178074=CARTESIAN_POINT('Ctrl Pts',(-24.4951894160082,-71.5754500366103,
85.607169318098));
#178075=CARTESIAN_POINT('Ctrl Pts',(-24.4570936740862,-73.2699077150253,
85.9494606259919));
#178076=CARTESIAN_POINT('Ctrl Pts',(-24.4381782821793,-74.1354456671949,
86.036007086387));
#178077=CARTESIAN_POINT('Ctrl Pts',(-24.4189072313414,-75.0031417059253,
86.0360048944213));
#178078=CARTESIAN_POINT('',(-24.9173192207092,-70.5369340980989,60.7267130748814));
#178079=CARTESIAN_POINT('',(-24.9176605481234,-70.5369675179446,60.7268149418411));
#178080=CARTESIAN_POINT('Ctrl Pts',(-24.9171176851385,-70.5369733775824,
60.7268128073552));
#178081=CARTESIAN_POINT('Ctrl Pts',(-24.907354037465,-70.1192429353976,
60.8789790540991));
#178082=CARTESIAN_POINT('Ctrl Pts',(-24.8975797564189,-69.7095626266936,
61.0523944958426));
#178083=CARTESIAN_POINT('Ctrl Pts',(-24.8780421092287,-68.915232029882,
61.4375907871025));
#178084=CARTESIAN_POINT('Ctrl Pts',(-24.8682932702408,-68.5308118305049,
61.64854254573));
#178085=CARTESIAN_POINT('Ctrl Pts',(-24.839312347075,-67.4195428302757,
62.3333119862464));
#178086=CARTESIAN_POINT('Ctrl Pts',(-24.8204486087593,-66.7285259145455,
62.8606386207108));
#178087=CARTESIAN_POINT('Ctrl Pts',(-24.7870712095047,-65.6249880349399,
63.8916559887359));
#178088=CARTESIAN_POINT('Ctrl Pts',(-24.7727296370073,-65.1881453816324,
64.3648623656643));
#178089=CARTESIAN_POINT('Ctrl Pts',(-24.742250830614,-64.3297071453802,
65.4449268297063));
#178090=CARTESIAN_POINT('Ctrl Pts',(-24.7262134284685,-63.9210741808339,
66.0592788242168));
#178091=CARTESIAN_POINT('Ctrl Pts',(-24.6980302381648,-63.3069294808542,
67.1772593829506));
#178092=CARTESIAN_POINT('Ctrl Pts',(-24.6860398778007,-63.076924372585,
67.6653304883622));
#178093=CARTESIAN_POINT('Ctrl Pts',(-24.6549461700741,-62.5579145370382,
68.9706612988227));
#178094=CARTESIAN_POINT('Ctrl Pts',(-24.6361603086848,-62.318910108264,
69.8049355406911));
#178095=CARTESIAN_POINT('Ctrl Pts',(-24.5983722391606,-62.0133377431336,
71.4882412958202));
#178096=CARTESIAN_POINT('Ctrl Pts',(-24.5796277914179,-61.9435284678936,
72.3324777567359));
#178097=CARTESIAN_POINT('Ctrl Pts',(-24.5427656769566,-61.9680684749626,
74.0162199068147));
#178098=CARTESIAN_POINT('Ctrl Pts',(-24.5243480055858,-62.0611344834041,
74.8517940532979));
#178099=CARTESIAN_POINT('Ctrl Pts',(-24.4878677169977,-62.4004662751921,
76.46542723281));
#178100=CARTESIAN_POINT('Ctrl Pts',(-24.4702471435588,-62.640654323058,
77.2409779439216));
#178101=CARTESIAN_POINT('Ctrl Pts',(-24.433796255826,-63.2784289509455,
78.7776809955811));
#178102=CARTESIAN_POINT('Ctrl Pts',(-24.4148532855467,-63.6822389597166,
79.5321159405294));
#178103=CARTESIAN_POINT('Ctrl Pts',(-24.3870337108765,-64.3884638652798,
80.5880248805467));
#178104=CARTESIAN_POINT('Ctrl Pts',(-24.3779772084299,-64.6365595877853,
80.9230672036952));
#178105=CARTESIAN_POINT('Ctrl Pts',(-24.3526031268852,-65.3720877557516,
81.8228797791645));
#178106=CARTESIAN_POINT('Ctrl Pts',(-24.3361839511979,-65.8925173725387,
82.3585972053378));
#178107=CARTESIAN_POINT('Ctrl Pts',(-24.3007805274961,-67.1080018457081,
83.4123021007472));
#178108=CARTESIAN_POINT('Ctrl Pts',(-24.2821791710908,-67.8146617871703,
83.9115696836482));
#178109=CARTESIAN_POINT('Ctrl Pts',(-24.2540944650781,-68.9301293119283,
84.5442570908524));
#178110=CARTESIAN_POINT('Ctrl Pts',(-24.2448678542072,-69.3045934236883,
84.7334176271645));
#178111=CARTESIAN_POINT('Ctrl Pts',(-24.216668816178,-70.4754509318188,
85.2556863772761));
#178112=CARTESIAN_POINT('Ctrl Pts',(-24.1980647980835,-71.2963084756696,
85.5281394442645));
#178113=CARTESIAN_POINT('Ctrl Pts',(-24.163396596036,-72.8455498637824,
85.8768137532399));
#178114=CARTESIAN_POINT('Ctrl Pts',(-24.1473926977216,-73.5651139084155,
85.9767881417826));
#178115=CARTESIAN_POINT('Ctrl Pts',(-24.1158008336593,-75.010197341672,
86.0559642583735));
#178116=CARTESIAN_POINT('Ctrl Pts',(-24.1002471628222,-75.733187632082,
86.0355574927849));
#178117=CARTESIAN_POINT('Ctrl Pts',(-24.0657733724578,-77.301063771048,
85.8605317011928));
#178118=CARTESIAN_POINT('Ctrl Pts',(-24.0469468205147,-78.1399678374923,
85.6822121490468));
#178119=CARTESIAN_POINT('Ctrl Pts',(-24.010189394764,-79.7547398415525,
85.1690140982003));
#178120=CARTESIAN_POINT('Ctrl Pts',(-23.9919616414302,-80.527762820596,
84.8384734047039));
#178121=CARTESIAN_POINT('Ctrl Pts',(-23.9546341481889,-82.0200678806927,
84.0224231758214));
#178122=CARTESIAN_POINT('Ctrl Pts',(-23.9360244917028,-82.7335970089921,
83.5348665781671));
#178123=CARTESIAN_POINT('Ctrl Pts',(-23.8989792941308,-84.0370277063888,
82.4404483463286));
#178124=CARTESIAN_POINT('Ctrl Pts',(-23.8804521106617,-84.6265974673046,
81.8395370520967));
#178125=CARTESIAN_POINT('Ctrl Pts',(-23.8471181138764,-85.5882146151588,
80.6489263907446));
#178126=CARTESIAN_POINT('Ctrl Pts',(-23.8322209852127,-85.9787829923853,
80.0781038763657));
#178127=CARTESIAN_POINT('Ctrl Pts',(-23.798456560602,-86.7469237694405,
78.7387393171392));
#178128=CARTESIAN_POINT('Ctrl Pts',(-23.7796666603123,-87.0978561620125,
77.9585423880256));
#178129=CARTESIAN_POINT('Ctrl Pts',(-23.742885269507,-87.6378737949811,
76.3540605202281));
#178130=CARTESIAN_POINT('Ctrl Pts',(-23.7245943383307,-87.8282524332701,
75.5344466062342));
#178131=CARTESIAN_POINT('Ctrl Pts',(-23.6888150613604,-88.0419621207994,
73.922431733533));
#178132=CARTESIAN_POINT('Ctrl Pts',(-23.671751351237,-88.074616373477,73.1348591085154));
#178133=CARTESIAN_POINT('Ctrl Pts',(-23.6366919564938,-87.9960084407066,
71.529557093911));
#178134=CARTESIAN_POINT('Ctrl Pts',(-23.6185648586246,-87.878651766991,
70.7155723503837));
#178135=CARTESIAN_POINT('Ctrl Pts',(-23.5861034257923,-87.5307434037802,
69.2780105212558));
#178136=CARTESIAN_POINT('Ctrl Pts',(-23.5718543535404,-87.3276283875879,
68.6506414981074));
#178137=CARTESIAN_POINT('Ctrl Pts',(-23.5481237056837,-86.9171444844969,
67.6485192350802));
#178138=CARTESIAN_POINT('Ctrl Pts',(-23.5387724395496,-86.7371913800963,
67.2638317826352));
#178139=CARTESIAN_POINT('Ctrl Pts',(-23.5103596573091,-86.1358175788794,
66.1263420779984));
#178140=CARTESIAN_POINT('Ctrl Pts',(-23.4916029113219,-85.6582590297536,
65.4058986222406));
#178141=CARTESIAN_POINT('Ctrl Pts',(-23.4537955479461,-84.5678435881823,
64.0695602513784));
#178142=CARTESIAN_POINT('Ctrl Pts',(-23.4346204906349,-83.9576249067465,
63.4569902583999));
#178143=CARTESIAN_POINT('Ctrl Pts',(-23.4005635230591,-82.7595073227506,
62.4716583259945));
#178144=CARTESIAN_POINT('Ctrl Pts',(-23.3855753038685,-82.1937684308081,
62.0769924688238));
#178145=CARTESIAN_POINT('Ctrl Pts',(-23.3517305051871,-80.8700308021691,
61.3014086187056));
#178146=CARTESIAN_POINT('Ctrl Pts',(-23.3329524032564,-80.100710066655,
60.9459022531436));
#178147=CARTESIAN_POINT('Ctrl Pts',(-23.2958780198951,-78.5039024588121,
60.3886648378157));
#178148=CARTESIAN_POINT('Ctrl Pts',(-23.2772858870629,-77.6801776269435,
60.1882985938689));
#178149=CARTESIAN_POINT('Ctrl Pts',(-23.244844685141,-76.2331614615956,
59.98222025733));
#178150=CARTESIAN_POINT('Ctrl Pts',(-23.2313015712184,-75.6183651000271,
59.9387052680259));
#178151=CARTESIAN_POINT('Ctrl Pts',(-23.2177969711981,-75.0031087425464,
59.9387052680259));
#178152=CARTESIAN_POINT('Origin',(-23.90845228375,-75.0031087425464,72.9873550812444));
#178153=CARTESIAN_POINT('',(-21.4178560137238,-75.0031087387644,59.9387052680259));
#178154=CARTESIAN_POINT('',(-21.7173525905574,-75.0031087425464,59.9387052680259));
#178155=CARTESIAN_POINT('',(-23.90845228375,-75.0031087425464,59.9387052680259));
#178156=CARTESIAN_POINT('Ctrl Pts',(-21.7173525905574,-75.0031087425464,
59.9387052680259));
#178157=CARTESIAN_POINT('Ctrl Pts',(-21.7279055222494,-75.4850294936703,
59.9387052680259));
#178158=CARTESIAN_POINT('Ctrl Pts',(-21.7385230017382,-75.9668862553294,
59.9654031749341));
#178159=CARTESIAN_POINT('Ctrl Pts',(-21.7679240675029,-77.3024452901014,
60.1140452558455));
#178160=CARTESIAN_POINT('Ctrl Pts',(-21.7864421216113,-78.1469014580676,
60.2938282072216));
#178161=CARTESIAN_POINT('Ctrl Pts',(-21.8159352477052,-79.4291237185252,
60.702712051699));
#178162=CARTESIAN_POINT('Ctrl Pts',(-21.8266151492676,-79.882222448103,
60.8755298104572));
#178163=CARTESIAN_POINT('Ctrl Pts',(-21.8519577830707,-80.9380865230419,
61.3471373671513));
#178164=CARTESIAN_POINT('Ctrl Pts',(-21.8664533772828,-81.5294397994638,
61.6680956779007));
#178165=CARTESIAN_POINT('Ctrl Pts',(-21.9000034898083,-82.8187825234477,
62.5026496888453));
#178166=CARTESIAN_POINT('Ctrl Pts',(-21.9191269729969,-83.4957006312058,
63.043025618808));
#178167=CARTESIAN_POINT('Ctrl Pts',(-21.9473475391778,-84.4216993305954,
63.9462324866392));
#178168=CARTESIAN_POINT('Ctrl Pts',(-21.9566752112369,-84.7141784534085,
64.2611375895916));
#178169=CARTESIAN_POINT('Ctrl Pts',(-21.9833264542847,-85.4990775401469,
65.1946537624708));
#178170=CARTESIAN_POINT('Ctrl Pts',(-22.0008084882079,-85.951579087771,
65.8443486378435));
#178171=CARTESIAN_POINT('Ctrl Pts',(-22.0325838201198,-86.6674665002242,
67.101668350843));
#178172=CARTESIAN_POINT('Ctrl Pts',(-22.0468106480542,-86.9488626352141,
67.6960871336582));
#178173=CARTESIAN_POINT('Ctrl Pts',(-22.0777047614038,-87.4537260096757,
69.0106622728197));
#178174=CARTESIAN_POINT('Ctrl Pts',(-22.0943914982232,-87.6620372687037,
69.7341288886568));
#178175=CARTESIAN_POINT('Ctrl Pts',(-22.1294675642277,-87.9700062664921,
71.3014524052135));
#178176=CARTESIAN_POINT('Ctrl Pts',(-22.147833465954,-88.0520039394007,
72.145310832488));
#178177=CARTESIAN_POINT('Ctrl Pts',(-22.1756984054644,-88.0516373226961,
73.4062056611231));
#178178=CARTESIAN_POINT('Ctrl Pts',(-22.1849086029447,-88.0317133004347,
73.8210197869936));
#178179=CARTESIAN_POINT('Ctrl Pts',(-22.2165499231349,-87.8947925396264,
75.2474115217725));
#178180=CARTESIAN_POINT('Ctrl Pts',(-22.2386139872856,-87.6793050389978,
76.2457925937928));
#178181=CARTESIAN_POINT('Ctrl Pts',(-22.2704084912974,-87.2151472936438,
77.6033153361541));
#178182=CARTESIAN_POINT('Ctrl Pts',(-22.2796727141446,-87.0614873053053,
77.9910019193931));
#178183=CARTESIAN_POINT('Ctrl Pts',(-22.3051887888618,-86.5841101656086,
79.0450571324956));
#178184=CARTESIAN_POINT('Ctrl Pts',(-22.3213071119102,-86.2218425641866,
79.692231264384));
#178185=CARTESIAN_POINT('Ctrl Pts',(-22.3529083373018,-85.4201163206346,
80.8758455797193));
#178186=CARTESIAN_POINT('Ctrl Pts',(-22.3682834493315,-84.9889684320517,
81.4149845564498));
#178187=CARTESIAN_POINT('Ctrl Pts',(-22.3950863482788,-84.1558584102784,
82.3025736978643));
#178188=CARTESIAN_POINT('Ctrl Pts',(-22.4066316775564,-83.7714168305926,
82.6653145011311));
#178189=CARTESIAN_POINT('Ctrl Pts',(-22.4338912775281,-82.8225075887755,
83.4575825212767));
#178190=CARTESIAN_POINT('Ctrl Pts',(-22.4496709708313,-82.2429225410224,
83.8664060700109));
#178191=CARTESIAN_POINT('Ctrl Pts',(-22.4826037731214,-80.9612295771777,
84.6224938354518));
#178192=CARTESIAN_POINT('Ctrl Pts',(-22.4995831787795,-80.2552331908446,
84.9577706620152));
#178193=CARTESIAN_POINT('Ctrl Pts',(-22.5325450616795,-78.8574394922688,
85.4739714605351));
#178194=CARTESIAN_POINT('Ctrl Pts',(-22.5483954088286,-78.1723752269056,
85.665178554888));
#178195=CARTESIAN_POINT('Ctrl Pts',(-22.5760360101624,-76.9397628278786,
85.903003010317));
#178196=CARTESIAN_POINT('Ctrl Pts',(-22.587959276298,-76.3984101366401,
85.9726438876509));
#178197=CARTESIAN_POINT('Ctrl Pts',(-22.6190042307515,-74.9942563843571,
86.0644345013557));
#178198=CARTESIAN_POINT('Ctrl Pts',(-22.6382386174052,-74.1307621203506,
86.0353089734078));
#178199=CARTESIAN_POINT('Ctrl Pts',(-22.6727313652882,-72.5749278003073,
85.8276092401245));
#178200=CARTESIAN_POINT('Ctrl Pts',(-22.688208923268,-71.8821713248205,
85.6770335192465));
#178201=CARTESIAN_POINT('Ctrl Pts',(-22.7130842691032,-70.8071619049747,
85.3499706788249));
#178202=CARTESIAN_POINT('Ctrl Pts',(-22.7223276789988,-70.4152854548392,
85.2099616521215));
#178203=CARTESIAN_POINT('Ctrl Pts',(-22.7506180336334,-69.2331495062128,
84.7227331440658));
#178204=CARTESIAN_POINT('Ctrl Pts',(-22.7693292570255,-68.4700986548075,
84.3156960176756));
#178205=CARTESIAN_POINT('Ctrl Pts',(-22.8052308235053,-67.1177286366594,
83.4119184043845));
#178206=CARTESIAN_POINT('Ctrl Pts',(-22.8222017284822,-66.5211288698208,
82.9325431138843));
#178207=CARTESIAN_POINT('Ctrl Pts',(-22.8480288852443,-65.6699239372478,
82.1159758633101));
#178208=CARTESIAN_POINT('Ctrl Pts',(-22.8571021742464,-65.3838726097524,
81.8140391787974));
#178209=CARTESIAN_POINT('Ctrl Pts',(-22.8833462494765,-64.6039940379515,
80.9078298739082));
#178210=CARTESIAN_POINT('Ctrl Pts',(-22.9006651616273,-64.1492881082466,
80.2722764235936));
#178211=CARTESIAN_POINT('Ctrl Pts',(-22.9322238148094,-63.420985671439,
79.0333195354624));
#178212=CARTESIAN_POINT('Ctrl Pts',(-22.9464765218011,-63.1311932840505,
78.4423425760535));
#178213=CARTESIAN_POINT('Ctrl Pts',(-22.9770326934869,-62.6142163608826,
77.1494521765591));
#178214=CARTESIAN_POINT('Ctrl Pts',(-22.9933345129949,-62.3994438891434,
76.4450044857766));
#178215=CARTESIAN_POINT('Ctrl Pts',(-23.0260362176216,-62.0858017418872,
74.9840266933657));
#178216=CARTESIAN_POINT('Ctrl Pts',(-23.0424688984152,-61.9915363368737,
74.2293314714673));
#178217=CARTESIAN_POINT('Ctrl Pts',(-23.0769262950679,-61.9334218436445,
72.6616294686187));
#178218=CARTESIAN_POINT('Ctrl Pts',(-23.0947623215829,-61.9788001263085,
71.8514825686357));
#178219=CARTESIAN_POINT('Ctrl Pts',(-23.1306635972023,-62.2237507322968,
70.2192800241415));
#178220=CARTESIAN_POINT('Ctrl Pts',(-23.1490078637108,-62.4286147657149,
69.4017833384164));
#178221=CARTESIAN_POINT('Ctrl Pts',(-23.186048784348,-62.9937640693951,
67.8148486279439));
#178222=CARTESIAN_POINT('Ctrl Pts',(-23.2042716490927,-63.3532618081069,
67.0493206846451));
#178223=CARTESIAN_POINT('Ctrl Pts',(-23.2415311394046,-64.2262368425864,
65.5795356979476));
#178224=CARTESIAN_POINT('Ctrl Pts',(-23.2606445669586,-64.7413162631444,
64.8810382503422));
#178225=CARTESIAN_POINT('Ctrl Pts',(-23.2916628434666,-65.6972847449895,
63.8231523380311));
#178226=CARTESIAN_POINT('Ctrl Pts',(-23.3037627027081,-66.0991769513896,
63.4322008835633));
#178227=CARTESIAN_POINT('Ctrl Pts',(-23.3315230797198,-67.0667774133513,
62.605159897377));
#178228=CARTESIAN_POINT('Ctrl Pts',(-23.3472354467346,-67.6456480225656,
62.1872116077931));
#178229=CARTESIAN_POINT('Ctrl Pts',(-23.3770439007649,-68.815519792736,
61.480456318847));
#178230=CARTESIAN_POINT('Ctrl Pts',(-23.3911310382946,-69.3999296712872,
61.184839910032));
#178231=CARTESIAN_POINT('Ctrl Pts',(-23.4206027246984,-70.648251547133,
60.6670916472714));
#178232=CARTESIAN_POINT('Ctrl Pts',(-23.4359727849947,-71.3128536017084,
60.4519777741411));
#178233=CARTESIAN_POINT('Ctrl Pts',(-23.4668095013143,-72.6881582521576,
60.1257463559955));
#178234=CARTESIAN_POINT('Ctrl Pts',(-23.4822248385575,-73.3972883002128,
60.0181098992289));
#178235=CARTESIAN_POINT('Ctrl Pts',(-23.5043649020229,-74.40848676433,59.9488656461147));
#178236=CARTESIAN_POINT('Ctrl Pts',(-23.5108840566336,-74.7058106598718,
59.9387052680259));
#178237=CARTESIAN_POINT('Ctrl Pts',(-23.5174110875174,-75.0031087425464,
59.9387052680259));
#178238=CARTESIAN_POINT('Ctrl Pts',(-23.2177969711981,-75.0031087425464,
59.9387052680259));
#178239=CARTESIAN_POINT('Ctrl Pts',(-23.2123696959067,-74.7558473929478,
59.9387052680259));
#178240=CARTESIAN_POINT('Ctrl Pts',(-23.2069356605294,-74.5085120342089,
59.9457333592563));
#178241=CARTESIAN_POINT('Ctrl Pts',(-23.1870440719356,-73.6072176795643,
59.997047349715));
#178242=CARTESIAN_POINT('Ctrl Pts',(-23.1724726631029,-72.9567675916252,
60.0835149849251));
#178243=CARTESIAN_POINT('Ctrl Pts',(-23.1387649040543,-71.4692304011195,
60.3966045566484));
#178244=CARTESIAN_POINT('Ctrl Pts',(-23.1199621028945,-70.6426901946818,
60.6584441188451));
#178245=CARTESIAN_POINT('Ctrl Pts',(-23.0821642900146,-69.0734071685228,
61.3332941733369));
#178246=CARTESIAN_POINT('Ctrl Pts',(-23.0633856665419,-68.3327795084699,
61.7407906439637));
#178247=CARTESIAN_POINT('Ctrl Pts',(-23.0262799044402,-66.9385082822665,
62.6944000048576));
#178248=CARTESIAN_POINT('Ctrl Pts',(-23.0076587848129,-66.2884283456319,
63.2386606339165));
#178249=CARTESIAN_POINT('Ctrl Pts',(-22.9696489429302,-65.089360746866,
64.4589854659968));
#178250=CARTESIAN_POINT('Ctrl Pts',(-22.950760136218,-64.5459609327155,
65.1347407662965));
#178251=CARTESIAN_POINT('Ctrl Pts',(-22.9155386888329,-63.6726496477427,
66.4738119744188));
#178252=CARTESIAN_POINT('Ctrl Pts',(-22.8992021686245,-63.3244079052054,
67.1210541591254));
#178253=CARTESIAN_POINT('Ctrl Pts',(-22.8668711397119,-62.7420991952012,
68.4633079657042));
#178254=CARTESIAN_POINT('Ctrl Pts',(-22.8510088435519,-62.5084099403389,
69.1556632672244));
#178255=CARTESIAN_POINT('Ctrl Pts',(-22.8206476946401,-62.1788908517869,
70.4922565068026));
#178256=CARTESIAN_POINT('Ctrl Pts',(-22.8062474186823,-62.070940327118,
71.1312576104667));
#178257=CARTESIAN_POINT('Ctrl Pts',(-22.7751127380341,-61.9398092071712,
72.5372511441418));
#178258=CARTESIAN_POINT('Ctrl Pts',(-22.758505876112,-61.9358845560748,
73.303654728887));
#178259=CARTESIAN_POINT('Ctrl Pts',(-22.7324455406655,-62.0336043832685,
74.4817778955585));
#178260=CARTESIAN_POINT('Ctrl Pts',(-22.7232053297365,-62.0880162647817,
74.8956863581744));
#178261=CARTESIAN_POINT('Ctrl Pts',(-22.6948421594479,-62.3159267091236,
76.1577337341884));
#178262=CARTESIAN_POINT('Ctrl Pts',(-22.6760964756324,-62.553997005025,
76.9917910798007));
#178263=CARTESIAN_POINT('Ctrl Pts',(-22.6424505830227,-63.118420781376,
78.415564530002));
#178264=CARTESIAN_POINT('Ctrl Pts',(-22.6276767664198,-63.4110696739612,
79.0152810730968));
#178265=CARTESIAN_POINT('Ctrl Pts',(-22.5964536780277,-64.130251562773,
80.2411962973343));
#178266=CARTESIAN_POINT('Ctrl Pts',(-22.5801252206438,-64.5680610345939,
80.8579979938936));
#178267=CARTESIAN_POINT('Ctrl Pts',(-22.5543744219634,-65.3272491916067,
81.7520377711469));
#178268=CARTESIAN_POINT('Ctrl Pts',(-22.5451559795505,-65.6129093885819,
82.057419901823));
#178269=CARTESIAN_POINT('Ctrl Pts',(-22.516919888215,-66.5322453940485,
82.9501584093053));
#178270=CARTESIAN_POINT('Ctrl Pts',(-22.4982769191142,-67.2099523810732,
83.4887688967499));
#178271=CARTESIAN_POINT('Ctrl Pts',(-22.4640738082773,-68.5240941504044,
84.3354497482744));
#178272=CARTESIAN_POINT('Ctrl Pts',(-22.4486093883778,-69.1418384806561,
84.6664984142158));
#178273=CARTESIAN_POINT('Ctrl Pts',(-22.4165167298404,-70.4869128356522,
85.2536056933848));
#178274=CARTESIAN_POINT('Ctrl Pts',(-22.3999604916125,-71.2164354828224,
85.4980721619425));
#178275=CARTESIAN_POINT('Ctrl Pts',(-22.3720627248218,-72.4554404905535,
85.7948858721622));
#178276=CARTESIAN_POINT('Ctrl Pts',(-22.360913397835,-72.9541153397416,
85.8840633147286));
#178277=CARTESIAN_POINT('Ctrl Pts',(-22.3309591565491,-74.3117424637426,
86.0460983856683));
#178278=CARTESIAN_POINT('Ctrl Pts',(-22.3124587905585,-75.1747837319727,
86.0632601490741));
#178279=CARTESIAN_POINT('Ctrl Pts',(-22.2845439381383,-76.4467593173734,
85.9625327976298));
#178280=CARTESIAN_POINT('Ctrl Pts',(-22.2754261188661,-76.8585189587835,
85.910079867448));
#178281=CARTESIAN_POINT('Ctrl Pts',(-22.2479497859112,-78.0923377446237,
85.6927129397798));
#178282=CARTESIAN_POINT('Ctrl Pts',(-22.2299384351025,-78.9016750433963,
85.4681657864787));
#178283=CARTESIAN_POINT('Ctrl Pts',(-22.1963630139692,-80.3383096775272,
84.9160778634896));
#178284=CARTESIAN_POINT('Ctrl Pts',(-22.1809075997859,-80.9714103559225,
84.6122494653766));
#178285=CARTESIAN_POINT('Ctrl Pts',(-22.1498865798407,-82.2007044815308,
83.8952952213165));
#178286=CARTESIAN_POINT('Ctrl Pts',(-22.1343394179012,-82.7931166020135,
83.4804158618099));
#178287=CARTESIAN_POINT('Ctrl Pts',(-22.0996873551722,-84.0123479757959,
82.4661369479483));
#178288=CARTESIAN_POINT('Ctrl Pts',(-22.080688351565,-84.6200189723064,
81.8489994871049));
#178289=CARTESIAN_POINT('Ctrl Pts',(-22.043690851755,-85.6900364840045,
80.5215557984812));
#178290=CARTESIAN_POINT('Ctrl Pts',(-22.0253834532474,-86.1533078349851,
79.817264122057));
#178291=CARTESIAN_POINT('Ctrl Pts',(-21.9883886554898,-86.9387141208914,
78.3276836433768));
#178292=CARTESIAN_POINT('Ctrl Pts',(-21.9701755051764,-87.2586859117162,
77.5457118574822));
#178293=CARTESIAN_POINT('Ctrl Pts',(-21.9329730465891,-87.7491604203139,
75.9115124136033));
#178294=CARTESIAN_POINT('Ctrl Pts',(-21.9138874461547,-87.9146567082245,
75.0620736225233));
#178295=CARTESIAN_POINT('Ctrl Pts',(-21.8832775743841,-88.045338634546,
73.6649069858103));
#178296=CARTESIAN_POINT('Ctrl Pts',(-21.8715817793504,-88.0622044875514,
73.12467336566));
#178297=CARTESIAN_POINT('Ctrl Pts',(-21.8449720591184,-88.0246676027813,
71.9080495797004));
#178298=CARTESIAN_POINT('Ctrl Pts',(-21.8300144490856,-87.9511175274875,
71.2337992547658));
#178299=CARTESIAN_POINT('Ctrl Pts',(-21.7936672920935,-87.6443580933324,
69.607775881084));
#178300=CARTESIAN_POINT('Ctrl Pts',(-21.7725828052433,-87.3557864236126,
68.6706321687396));
#178301=CARTESIAN_POINT('Ctrl Pts',(-21.741871450258,-86.7992517857775,
67.393518066754));
#178302=CARTESIAN_POINT('Ctrl Pts',(-21.7326758901293,-86.6151054813704,
67.0206528993441));
#178303=CARTESIAN_POINT('Ctrl Pts',(-21.7066756118522,-86.0413009332282,
65.9863438652782));
#178304=CARTESIAN_POINT('Ctrl Pts',(-21.690065426756,-85.6106812483756,
65.3496032144281));
#178305=CARTESIAN_POINT('Ctrl Pts',(-21.6585775345741,-84.7080001966367,
64.2396374698938));
#178306=CARTESIAN_POINT('Ctrl Pts',(-21.6438352746905,-84.2507237753405,
63.757561024057));
#178307=CARTESIAN_POINT('Ctrl Pts',(-21.6098769346781,-83.1041922799144,
62.7199745475537));
#178308=CARTESIAN_POINT('Ctrl Pts',(-21.59067854922,-82.3911786697216,62.1955487260731));
#178309=CARTESIAN_POINT('Ctrl Pts',(-21.5619309785478,-81.2723054333921,
61.5358252856643));
#178310=CARTESIAN_POINT('Ctrl Pts',(-21.5526917073905,-80.9040126423071,
61.3417681468817));
#178311=CARTESIAN_POINT('Ctrl Pts',(-21.5284782116718,-79.9091842943437,
60.8769115349169));
#178312=CARTESIAN_POINT('Ctrl Pts',(-21.5136425067296,-79.2696016194965,
60.6370732223613));
#178313=CARTESIAN_POINT('Ctrl Pts',(-21.4795996204699,-77.7857795419246,
60.2097487304598));
#178314=CARTESIAN_POINT('Ctrl Pts',(-21.4603866287851,-76.9357391930337,
60.0538549661469));
#178315=CARTESIAN_POINT('Ctrl Pts',(-21.4335870203312,-75.7194752094565,
59.9534586080836));
#178316=CARTESIAN_POINT('Ctrl Pts',(-21.425739200257,-75.3613555812664,
59.9387052678182));
#178317=CARTESIAN_POINT('Ctrl Pts',(-21.4178560137238,-75.0031087349823,
59.9387052680259));
#178318=CARTESIAN_POINT('Origin',(-23.90845228375,-75.0031087425464,72.9873550812444));
#178319=CARTESIAN_POINT('',(-19.6178714446467,-75.0031006318966,59.9387052680284));
#178320=CARTESIAN_POINT('',(-19.9173382169355,-75.0031141882852,59.9387052680271));
#178321=CARTESIAN_POINT('',(-23.90845228375,-75.0031087425464,59.9387052680259));
#178322=CARTESIAN_POINT('',(-19.417776314132,-66.6125912877755,62.9938945755099));
#178323=CARTESIAN_POINT('Ctrl Pts',(-19.6178714446467,-75.0031006318966,
59.9387052680284));
#178324=CARTESIAN_POINT('Ctrl Pts',(-19.6014685026439,-74.2607437617124,
59.9387057294552));
#178325=CARTESIAN_POINT('Ctrl Pts',(-19.5849037811272,-73.5197379909757,
60.0020567382727));
#178326=CARTESIAN_POINT('Ctrl Pts',(-19.5521553242651,-72.053177418037,
60.2546657056371));
#178327=CARTESIAN_POINT('Ctrl Pts',(-19.5358475432087,-71.3304102074453,
60.4440397486732));
#178328=CARTESIAN_POINT('Ctrl Pts',(-19.5024014277746,-69.9091738803646,
60.9498755753139));
#178329=CARTESIAN_POINT('Ctrl Pts',(-19.4854578253639,-69.2143639188463,
61.26816030853));
#178330=CARTESIAN_POINT('Ctrl Pts',(-19.4513770173664,-67.8656046389107,
62.0353827008749));
#178331=CARTESIAN_POINT('Ctrl Pts',(-19.4340082401172,-67.2166509500368,
62.4868441028642));
#178332=CARTESIAN_POINT('Ctrl Pts',(-19.4164777809729,-66.6124627542204,
62.9941412915471));
#178333=CARTESIAN_POINT('',(-19.7174312187883,-66.6129973379348,62.9934580993662));
#178334=CARTESIAN_POINT('Ctrl Pts',(-19.4175483972726,-66.6126744602016,
62.9939635397476));
#178335=CARTESIAN_POINT('Ctrl Pts',(-19.5175444259387,-66.6116381403926,
62.9948336320698));
#178336=CARTESIAN_POINT('Ctrl Pts',(-19.6175404546048,-66.6116382109846,
62.9948335017092));
#178337=CARTESIAN_POINT('Ctrl Pts',(-19.7175364832709,-66.6130192454567,
62.993674068783));
#178338=CARTESIAN_POINT('Ctrl Pts',(-19.9173382169355,-75.0031141882852,
59.9387052680271));
#178339=CARTESIAN_POINT('Ctrl Pts',(-19.9007967949276,-74.2445563629071,
59.9387049514496));
#178340=CARTESIAN_POINT('Ctrl Pts',(-19.8844783676533,-73.4874434635508,
60.0048502818403));
#178341=CARTESIAN_POINT('Ctrl Pts',(-19.8511771565402,-71.9905968512035,
60.2684072581934));
#178342=CARTESIAN_POINT('Ctrl Pts',(-19.8344745302453,-71.2538016732615,
60.4657909926964));
#178343=CARTESIAN_POINT('Ctrl Pts',(-19.8097614398516,-70.1848551286669,
60.8550310149607));
#178344=CARTESIAN_POINT('Ctrl Pts',(-19.8016215987501,-69.8370130284161,
60.9990145028378));
#178345=CARTESIAN_POINT('Ctrl Pts',(-19.7685609555398,-68.4584106326462,
61.640821849789));
#178346=CARTESIAN_POINT('Ctrl Pts',(-19.7433909837073,-67.4889730272299,
62.258205377191));
#178347=CARTESIAN_POINT('Ctrl Pts',(-19.7185673678502,-66.6125447149948,
62.9940724750352));
#178348=CARTESIAN_POINT('Origin',(-30.2175364832709,-75.,72.98888938658));
#178349=CARTESIAN_POINT('',(-21.9012048916249,-75.,85.23888938658));
#178350=CARTESIAN_POINT('',(-21.2338306941238,-75.,85.23888938658));
#178351=CARTESIAN_POINT('',(-30.2175364832709,-75.,85.23888938658));
#178352=CARTESIAN_POINT('',(-20.333830095635,-75.0000012548192,60.7388893865801));
#178353=CARTESIAN_POINT('Ctrl Pts',(-21.2338306941238,-75.,85.23888938658));
#178354=CARTESIAN_POINT('Ctrl Pts',(-21.2306064320489,-75.1377250058455,
85.23888938658));
#178355=CARTESIAN_POINT('Ctrl Pts',(-21.2273866755216,-75.2754746736316,
85.2365667529554));
#178356=CARTESIAN_POINT('Ctrl Pts',(-21.2078116035036,-76.1137341068034,
85.2082763223829));
#178357=CARTESIAN_POINT('Ctrl Pts',(-21.1916182257208,-76.810955591155,
85.1245500444249));
#178358=CARTESIAN_POINT('Ctrl Pts',(-21.1659705196501,-77.879673500507,
84.9020176777777));
#178359=CARTESIAN_POINT('Ctrl Pts',(-21.1567744412272,-78.2581393887295,
84.8041199660589));
#178360=CARTESIAN_POINT('Ctrl Pts',(-21.1286306389688,-79.4051451785294,
84.4481109454274));
#178361=CARTESIAN_POINT('Ctrl Pts',(-21.1099683881167,-80.1532725878486,
84.1317275942547));
#178362=CARTESIAN_POINT('Ctrl Pts',(-21.0785119861276,-81.3307116932154,
83.4896691172602));
#178363=CARTESIAN_POINT('Ctrl Pts',(-21.0660031776475,-81.7797483939057,
83.205508177142));
#178364=CARTESIAN_POINT('Ctrl Pts',(-21.0346129911703,-82.8643483604228,
82.4160666426164));
#178365=CARTESIAN_POINT('Ctrl Pts',(-21.0159325702271,-83.4707913209333,
81.8751337942049));
#178366=CARTESIAN_POINT('Ctrl Pts',(-20.9877251688978,-84.2833073570522,
80.9910685407017));
#178367=CARTESIAN_POINT('Ctrl Pts',(-20.978542572352,-84.5334034172025,
80.6914140839258));
#178368=CARTESIAN_POINT('Ctrl Pts',(-20.9504103312409,-85.2576446298438,
79.7342338652322));
#178369=CARTESIAN_POINT('Ctrl Pts',(-20.9317488399315,-85.6812092600103,
79.0412205812099));
#178370=CARTESIAN_POINT('Ctrl Pts',(-20.9008496550773,-86.2537312242886,
77.8544357222563));
#178371=CARTESIAN_POINT('Ctrl Pts',(-20.8888901159346,-86.4456055879746,
77.384127955797));
#178372=CARTESIAN_POINT('Ctrl Pts',(-20.8580282641812,-86.8667578848845,
76.1352399480246));
#178373=CARTESIAN_POINT('Ctrl Pts',(-20.8393588367127,-87.0488915854874,
75.3433905021401));
#178374=CARTESIAN_POINT('Ctrl Pts',(-20.8108520335845,-87.2025781778472,
74.1389171989822));
#178375=CARTESIAN_POINT('Ctrl Pts',(-20.8013448125835,-87.233848160121,
73.7361764964692));
#178376=CARTESIAN_POINT('Ctrl Pts',(-20.7728875543568,-87.2679058104121,
72.5229272900381));
#178377=CARTESIAN_POINT('Ctrl Pts',(-20.7542266297324,-87.2102682856516,
71.712966244044));
#178378=CARTESIAN_POINT('Ctrl Pts',(-20.7140962005733,-86.9203307398547,
70.0253900318385));
#178379=CARTESIAN_POINT('Ctrl Pts',(-20.6929048898017,-86.6697671416374,
69.1557229615675));
#178380=CARTESIAN_POINT('Ctrl Pts',(-20.6627410197266,-86.1756530420926,
67.9566977656067));
#178381=CARTESIAN_POINT('Ctrl Pts',(-20.653577681573,-86.0077871259066,
67.5993814610305));
#178382=CARTESIAN_POINT('Ctrl Pts',(-20.6321211873006,-85.5792460322651,
66.7910845979833));
#178383=CARTESIAN_POINT('Ctrl Pts',(-20.6198593184561,-85.306478951447,
66.3473741622852));
#178384=CARTESIAN_POINT('Ctrl Pts',(-20.5887064250236,-84.5387213002112,
65.2602169756139));
#178385=CARTESIAN_POINT('Ctrl Pts',(-20.570031460076,-84.0065472535975,
64.6461268255294));
#178386=CARTESIAN_POINT('Ctrl Pts',(-20.5418670051956,-83.1353033545976,
63.822082051671));
#178387=CARTESIAN_POINT('Ctrl Pts',(-20.5327174220962,-82.8404264015553,
63.5686329215459));
#178388=CARTESIAN_POINT('Ctrl Pts',(-20.5078304802431,-82.0034257913031,
62.9157914966793));
#178389=CARTESIAN_POINT('Ctrl Pts',(-20.4922564045862,-81.4396531612366,
62.5463734080976));
#178390=CARTESIAN_POINT('Ctrl Pts',(-20.4532579389303,-79.9700443453893,
61.7478730057183));
#178391=CARTESIAN_POINT('Ctrl Pts',(-20.4296832227902,-79.0365557338568,
61.3799267732218));
#178392=CARTESIAN_POINT('Ctrl Pts',(-20.3944895648947,-77.5721200205929,
61.0009833763027));
#178393=CARTESIAN_POINT('Ctrl Pts',(-20.3825725228186,-77.0678749125199,
60.9037917831714));
#178394=CARTESIAN_POINT('Ctrl Pts',(-20.358270691628,-76.0419975995413,
60.7721607017485));
#178395=CARTESIAN_POINT('Ctrl Pts',(-20.346008912442,-75.5212703996809,
60.7388894399758));
#178396=CARTESIAN_POINT('Ctrl Pts',(-20.333830095635,-75.0000012548192,
60.7388893865801));
#178397=CARTESIAN_POINT('',(-20.1338946865143,-67.1252798838891,63.6053345409727));
#178398=CARTESIAN_POINT('Ctrl Pts',(-20.333830095635,-75.0000012548192,
60.7388893865801));
#178399=CARTESIAN_POINT('Ctrl Pts',(-20.3171609122067,-74.2865385983972,
60.7388893134971));
#178400=CARTESIAN_POINT('Ctrl Pts',(-20.3006993175161,-73.5744403336657,
60.8012190536066));
#178401=CARTESIAN_POINT('Ctrl Pts',(-20.2672143173303,-72.1698753089757,
61.0489997289239));
#178402=CARTESIAN_POINT('Ctrl Pts',(-20.250461415262,-71.4800647066194,
61.2338634607188));
#178403=CARTESIAN_POINT('Ctrl Pts',(-20.2255958036809,-70.4769272751478,
61.5989754564678));
#178404=CARTESIAN_POINT('Ctrl Pts',(-20.2173661387531,-70.1490267795421,
61.7347175085119));
#178405=CARTESIAN_POINT('Ctrl Pts',(-20.1841011379601,-68.8555145895829,
62.3372463704191));
#178406=CARTESIAN_POINT('Ctrl Pts',(-20.1588428593053,-67.9471848925514,
62.9156573754958));
#178407=CARTESIAN_POINT('Ctrl Pts',(-20.1339068674138,-67.1258030253621,
63.6048858697113));
#178408=CARTESIAN_POINT('',(-19.4263813260168,-62.8761873158039,74.7426470661147));
#178409=CARTESIAN_POINT('Ctrl Pts',(-20.1339146423347,-67.1252326623533,
63.605364495691));
#178410=CARTESIAN_POINT('Ctrl Pts',(-20.0750070626096,-66.3344526705064,
64.2689966087264));
#178411=CARTESIAN_POINT('Ctrl Pts',(-20.0153558799609,-65.6307143557395,
65.0299429613649));
#178412=CARTESIAN_POINT('Ctrl Pts',(-19.8973223675187,-64.4233710241535,
66.7207259848254));
#178413=CARTESIAN_POINT('Ctrl Pts',(-19.8395215672342,-63.9273522053236,
67.6455451969498));
#178414=CARTESIAN_POINT('Ctrl Pts',(-19.7215871660935,-63.1867139032684,
69.5867095690456));
#178415=CARTESIAN_POINT('Ctrl Pts',(-19.6618458561676,-62.9420828473522,
70.5940527189565));
#178416=CARTESIAN_POINT('Ctrl Pts',(-19.5435268983665,-62.709918612146,
72.6588170657532));
#178417=CARTESIAN_POINT('Ctrl Pts',(-19.485538173564,-62.726548281685,73.7081850984939));
#178418=CARTESIAN_POINT('Ctrl Pts',(-19.4263813260168,-62.8761873158039,
74.7426470661147));
#178419=CARTESIAN_POINT('',(-19.1263815299174,-62.8761874826045,74.7426482192146));
#178420=CARTESIAN_POINT('',(-19.4263814899908,-62.8761746200905,74.7426467836703));
#178421=CARTESIAN_POINT('',(-19.0011490535824,-67.1252413014861,63.6053538167643));
#178422=CARTESIAN_POINT('Ctrl Pts',(-19.1263815299174,-62.8761874826045,
74.7426482192146));
#178423=CARTESIAN_POINT('Ctrl Pts',(-19.1161087162537,-62.7265520516628,
73.7082118549102));
#178424=CARTESIAN_POINT('Ctrl Pts',(-19.1067682656167,-62.7099182299581,
72.6588612733502));
#178425=CARTESIAN_POINT('Ctrl Pts',(-19.0856048538269,-62.9420706123676,
70.5941212219589));
#178426=CARTESIAN_POINT('Ctrl Pts',(-19.0740038291453,-63.1866916115569,
69.5867931485772));
#178427=CARTESIAN_POINT('Ctrl Pts',(-19.0533079901649,-63.9273116111903,
67.6456261303927));
#178428=CARTESIAN_POINT('Ctrl Pts',(-19.0441709589811,-64.4233323962465,
66.72078806223));
#178429=CARTESIAN_POINT('Ctrl Pts',(-19.02327760971,-65.6306771524171,65.0299871776315));
#178430=CARTESIAN_POINT('Ctrl Pts',(-19.0117355006677,-66.3344146039702,
64.2690330647641));
#178431=CARTESIAN_POINT('Ctrl Pts',(-19.0011200059672,-67.1252012611567,
63.6053908480438));
#178432=CARTESIAN_POINT('',(-19.2012431461282,-74.9999987591354,60.7388893865801));
#178433=CARTESIAN_POINT('Ctrl Pts',(-19.0011647644417,-67.1257997110858,
63.6048886507497));
#178434=CARTESIAN_POINT('Ctrl Pts',(-19.0263800941151,-67.9471805961339,
62.9156604862996));
#178435=CARTESIAN_POINT('Ctrl Pts',(-19.0510542001329,-68.8555096686468,
62.3372490326858));
#178436=CARTESIAN_POINT('Ctrl Pts',(-19.0845340441755,-70.1490234258174,
61.7347189482848));
#178437=CARTESIAN_POINT('Ctrl Pts',(-19.0928876791463,-70.4769239228417,
61.5989767903966));
#178438=CARTESIAN_POINT('Ctrl Pts',(-19.1179505022708,-71.4800592803612,
61.2338652070604));
#178439=CARTESIAN_POINT('Ctrl Pts',(-19.1344708541158,-72.1698680819012,
61.0490012011107));
#178440=CARTESIAN_POINT('Ctrl Pts',(-19.1676976678863,-73.5744386118425,
60.8012191599193));
#178441=CARTESIAN_POINT('Ctrl Pts',(-19.1845437886602,-74.2865381194436,
60.7388894588501));
#178442=CARTESIAN_POINT('Ctrl Pts',(-19.2012431461282,-74.9999987591354,
60.7388893865801));
#178443=CARTESIAN_POINT('',(-20.1012419544621,-75.,85.23888938658));
#178444=CARTESIAN_POINT('Ctrl Pts',(-19.2012431461282,-74.9999987591355,
60.7388893865801));
#178445=CARTESIAN_POINT('Ctrl Pts',(-19.2178347971233,-75.7088577649548,
60.7388893147761));
#178446=CARTESIAN_POINT('Ctrl Pts',(-19.2341852858951,-76.4163686749837,
60.8004162178675));
#178447=CARTESIAN_POINT('Ctrl Pts',(-19.2673328934291,-77.8106116762636,
61.0447571830811));
#178448=CARTESIAN_POINT('Ctrl Pts',(-19.2839937885109,-78.494782026441,
61.2267323451918));
#178449=CARTESIAN_POINT('Ctrl Pts',(-19.311244664781,-79.593309853432,61.6232931047021));
#178450=CARTESIAN_POINT('Ctrl Pts',(-19.3219325275506,-80.0179864860926,
61.8042979707288));
#178451=CARTESIAN_POINT('Ctrl Pts',(-19.3468572306141,-80.9759380243795,
62.2781617174915));
#178452=CARTESIAN_POINT('Ctrl Pts',(-19.3611960243164,-81.4996448467354,
62.5876329293234));
#178453=CARTESIAN_POINT('Ctrl Pts',(-19.3944166011216,-82.6628971902388,
63.3973133031375));
#178454=CARTESIAN_POINT('Ctrl Pts',(-19.413069929433,-83.280053766562,63.9247273598141));
#178455=CARTESIAN_POINT('Ctrl Pts',(-19.4412301671133,-84.1114166774393,
64.7914748368682));
#178456=CARTESIAN_POINT('Ctrl Pts',(-19.4504457623239,-84.3685202090294,
65.0865891827013));
#178457=CARTESIAN_POINT('Ctrl Pts',(-19.4759727466578,-85.0428155437503,
65.9398294921322));
#178458=CARTESIAN_POINT('Ctrl Pts',(-19.4921123752355,-85.4271994391204,
66.5219811776687));
#178459=CARTESIAN_POINT('Ctrl Pts',(-19.5272142319967,-86.1474679780081,
67.8455964083996));
#178460=CARTESIAN_POINT('Ctrl Pts',(-19.5463621687656,-86.4632789847727,
68.5942634992112));
#178461=CARTESIAN_POINT('Ctrl Pts',(-19.5772397965211,-86.8539719299969,
69.8572093570509));
#178462=CARTESIAN_POINT('Ctrl Pts',(-19.5890839114878,-86.974372130228,
70.3547896391956));
#178463=CARTESIAN_POINT('Ctrl Pts',(-19.6199096330926,-87.2042289723775,
71.6563126341651));
#178464=CARTESIAN_POINT('Ctrl Pts',(-19.6390505730574,-87.2656335795455,
72.4662047349187));
#178465=CARTESIAN_POINT('Ctrl Pts',(-19.6670600734787,-87.2374782401112,
73.6662943300324));
#178466=CARTESIAN_POINT('Ctrl Pts',(-19.6761146115089,-87.2096937876043,
74.0557205722193));
#178467=CARTESIAN_POINT('Ctrl Pts',(-19.7040719067252,-87.0671351656653,
75.2480705121353));
#178468=CARTESIAN_POINT('Ctrl Pts',(-19.7232146149536,-86.8912379171253,
76.0414467850986));
#178469=CARTESIAN_POINT('Ctrl Pts',(-19.7545879924084,-86.4723266558067,
77.3168214272262));
#178470=CARTESIAN_POINT('Ctrl Pts',(-19.7669023350968,-86.2736644264822,
77.8106903141346));
#178471=CARTESIAN_POINT('Ctrl Pts',(-19.7981973510168,-85.6928905608521,
79.0205688640787));
#178472=CARTESIAN_POINT('Ctrl Pts',(-19.8173406139994,-85.270624768396,
79.7144624313536));
#178473=CARTESIAN_POINT('Ctrl Pts',(-19.847486772466,-84.4931449152546,
80.7461161919661));
#178474=CARTESIAN_POINT('Ctrl Pts',(-19.8586396021926,-84.180915928759,
81.1132447328241));
#178475=CARTESIAN_POINT('Ctrl Pts',(-19.8887752040406,-83.2876110380681,
82.0461677596425));
#178476=CARTESIAN_POINT('Ctrl Pts',(-19.9079114798814,-82.6706680835386,
82.5742762522738));
#178477=CARTESIAN_POINT('Ctrl Pts',(-19.9377563186642,-81.6212087066361,
83.3059761542012));
#178478=CARTESIAN_POINT('Ctrl Pts',(-19.9486253805139,-81.2211899597887,
83.5520081760404));
#178479=CARTESIAN_POINT('Ctrl Pts',(-19.9784776666449,-80.0948208550819,
84.1585583275757));
#178480=CARTESIAN_POINT('Ctrl Pts',(-19.9976115130056,-79.3452541474879,
84.470939410336));
#178481=CARTESIAN_POINT('Ctrl Pts',(-20.0350217201929,-77.8110753435025,
84.9383825170732));
#178482=CARTESIAN_POINT('Ctrl Pts',(-20.0534076839674,-77.0311025355401,
85.0953814068152));
#178483=CARTESIAN_POINT('Ctrl Pts',(-20.0818291252186,-75.828729464966,
85.2178636174536));
#178484=CARTESIAN_POINT('Ctrl Pts',(-20.0915624256451,-75.4143798971417,
85.23888938658));
#178485=CARTESIAN_POINT('Ctrl Pts',(-20.1012419544621,-75.,85.23888938658));
#178486=CARTESIAN_POINT('',(-18.5675364832709,-75.,85.23888938658));
#178487=CARTESIAN_POINT('',(-30.2175364832709,-75.,85.23888938658));
#178488=CARTESIAN_POINT('Origin',(-18.5675364832709,-75.,72.98888938658));
#178489=CARTESIAN_POINT('Ctrl Pts',(-20.1012419544621,-75.,85.23888938658));
#178490=CARTESIAN_POINT('Ctrl Pts',(-20.1098579992633,-74.6311477731973,
85.23888938658));
#178491=CARTESIAN_POINT('Ctrl Pts',(-20.1184331195332,-74.2622715547378,
85.2222299412455));
#178492=CARTESIAN_POINT('Ctrl Pts',(-20.145877416015,-73.087224156511,85.115753719202));
#178493=CARTESIAN_POINT('Ctrl Pts',(-20.1649782572491,-72.2891976155929,
84.9626562940479));
#178494=CARTESIAN_POINT('Ctrl Pts',(-20.1977202056339,-70.9484151427787,
84.5644244052684));
#178495=CARTESIAN_POINT('Ctrl Pts',(-20.2113398668839,-70.3974549724233,
84.35660373583));
#178496=CARTESIAN_POINT('Ctrl Pts',(-20.2439365013652,-69.1278236305742,
83.7702075449523));
#178497=CARTESIAN_POINT('Ctrl Pts',(-20.2630835717669,-68.4276235773446,
83.3582260703368));
#178498=CARTESIAN_POINT('Ctrl Pts',(-20.2911519949849,-67.4567749344234,
82.6489038929779));
#178499=CARTESIAN_POINT('Ctrl Pts',(-20.3002500764559,-67.1515755586627,
82.4026218359583));
#178500=CARTESIAN_POINT('Ctrl Pts',(-20.3282394912505,-66.2529667088787,
81.6033603048994));
#178501=CARTESIAN_POINT('Ctrl Pts',(-20.3473742153681,-65.7022016462761,
81.0057866056215));
#178502=CARTESIAN_POINT('Ctrl Pts',(-20.3791352989799,-64.8850433499647,
79.9207080826668));
#178503=CARTESIAN_POINT('Ctrl Pts',(-20.3918182081102,-64.5852802091917,
79.4616066950045));
#178504=CARTESIAN_POINT('Ctrl Pts',(-20.4234809337223,-63.9206734423513,
78.2773350508884));
#178505=CARTESIAN_POINT('Ctrl Pts',(-20.4426256228864,-63.5951959624939,
77.5330701653992));
#178506=CARTESIAN_POINT('Ctrl Pts',(-20.4728580291676,-63.196193285558,
76.3006741841303));
#178507=CARTESIAN_POINT('Ctrl Pts',(-20.4840921895732,-63.0743287590611,
75.8307437016975));
#178508=CARTESIAN_POINT('Ctrl Pts',(-20.5143089920941,-62.8241808655607,
74.5599525780504));
#178509=CARTESIAN_POINT('Ctrl Pts',(-20.5334459048401,-62.7469506126223,
73.7515122717918));
#178510=CARTESIAN_POINT('Ctrl Pts',(-20.5708752753044,-62.7531722258421,
72.1470863459014));
#178511=CARTESIAN_POINT('Ctrl Pts',(-20.5892688834294,-62.8335003297472,
71.3549662903585));
#178512=CARTESIAN_POINT('Ctrl Pts',(-20.6336253435835,-63.2049955670995,
69.5056949374356));
#178513=CARTESIAN_POINT('Ctrl Pts',(-20.6587656706778,-63.5622215670142,
68.4687124396808));
#178514=CARTESIAN_POINT('Ctrl Pts',(-20.6935541827797,-64.2275848730086,
67.143332573469));
#178515=CARTESIAN_POINT('Ctrl Pts',(-20.7027671383237,-64.4196940867455,
66.802404984226));
#178516=CARTESIAN_POINT('Ctrl Pts',(-20.7301847934922,-65.0413334271389,
65.8131232904221));
#178517=CARTESIAN_POINT('Ctrl Pts',(-20.7481357032069,-65.5165846133254,
65.1958484834529));
#178518=CARTESIAN_POINT('Ctrl Pts',(-20.7846359035095,-66.5828894218892,
64.0540723966837));
#178519=CARTESIAN_POINT('Ctrl Pts',(-20.8031673576678,-67.1725813883994,
63.5331911230243));
#178520=CARTESIAN_POINT('Ctrl Pts',(-20.8399662375233,-68.4498940416262,
62.6068244322778));
#178521=CARTESIAN_POINT('Ctrl Pts',(-20.8583400584759,-69.1354236449765,
62.2047389495531));
#178522=CARTESIAN_POINT('Ctrl Pts',(-20.8953953203869,-70.5654543317576,
61.5429209378203));
#178523=CARTESIAN_POINT('Ctrl Pts',(-20.9136304218762,-71.3058177537415,
61.2829758193711));
#178524=CARTESIAN_POINT('Ctrl Pts',(-20.9491254009607,-72.7872992193625,
60.9174960981567));
#178525=CARTESIAN_POINT('Ctrl Pts',(-20.9666212717685,-73.5233888346176,
60.8055321609235));
#178526=CARTESIAN_POINT('Ctrl Pts',(-21.0030209867884,-75.0734559861661,
60.7123688138211));
#178527=CARTESIAN_POINT('Ctrl Pts',(-21.0216751093077,-75.8846719839338,
60.7440657022435));
#178528=CARTESIAN_POINT('Ctrl Pts',(-21.0498342314644,-77.0742678618884,
60.9094464154216));
#178529=CARTESIAN_POINT('Ctrl Pts',(-21.0590502488745,-77.4589289532811,
60.9818415273505));
#178530=CARTESIAN_POINT('Ctrl Pts',(-21.0846189366024,-78.5185179938907,
61.2343232499738));
#178531=CARTESIAN_POINT('Ctrl Pts',(-21.1007988461708,-79.1824981283792,
61.4538772995856));
#178532=CARTESIAN_POINT('Ctrl Pts',(-21.1359406362732,-80.569214644824,
62.0479865168428));
#178533=CARTESIAN_POINT('Ctrl Pts',(-21.155088545207,-81.280755162341,62.440353055518));
#178534=CARTESIAN_POINT('Ctrl Pts',(-21.1859723044965,-82.3697246124248,
63.1903442669647));
#178535=CARTESIAN_POINT('Ctrl Pts',(-21.197822228415,-82.7725401964285,
63.5066984326108));
#178536=CARTESIAN_POINT('Ctrl Pts',(-21.2189561588785,-83.4487388621008,
64.1098752124259));
#178537=CARTESIAN_POINT('Ctrl Pts',(-21.2282354324976,-83.7302342046026,
64.3865008010614));
#178538=CARTESIAN_POINT('Ctrl Pts',(-21.2586709516802,-84.6086355588132,
65.3373099039359));
#178539=CARTESIAN_POINT('Ctrl Pts',(-21.2794961590458,-85.1446657587784,
66.0636963168416));
#178540=CARTESIAN_POINT('Ctrl Pts',(-21.3194054798936,-86.002709791375,
67.542881664105));
#178541=CARTESIAN_POINT('Ctrl Pts',(-21.3385368832819,-86.3386537709364,
68.2821328961576));
#178542=CARTESIAN_POINT('Ctrl Pts',(-21.366845478053,-86.7290037998938,
69.4313695560812));
#178543=CARTESIAN_POINT('Ctrl Pts',(-21.3762087030407,-86.8398654341242,
69.8198100631227));
#178544=CARTESIAN_POINT('Ctrl Pts',(-21.40449699031,-87.1150137129048,71.0024597484276));
#178545=CARTESIAN_POINT('Ctrl Pts',(-21.4236452306662,-87.2198772616073,
71.8081875427081));
#178546=CARTESIAN_POINT('Ctrl Pts',(-21.4611946394842,-87.2685122063475,
73.4152996624451));
#178547=CARTESIAN_POINT('Ctrl Pts',(-21.4796157718967,-87.2147651333003,
74.2127061848986));
#178548=CARTESIAN_POINT('Ctrl Pts',(-21.5169717251508,-86.9540341921901,
75.7799416387219));
#178549=CARTESIAN_POINT('Ctrl Pts',(-21.5354562493324,-86.7487911403512,
76.5462509272946));
#178550=CARTESIAN_POINT('Ctrl Pts',(-21.5727085414766,-86.1867213661318,
78.0462026760087));
#178551=CARTESIAN_POINT('Ctrl Pts',(-21.591765904968,-85.8277814604079,
78.7749324589671));
#178552=CARTESIAN_POINT('Ctrl Pts',(-21.6253895591423,-85.0694528617131,
79.9930811898409));
#178553=CARTESIAN_POINT('Ctrl Pts',(-21.6398565408902,-84.6993106228171,
80.4972818176621));
#178554=CARTESIAN_POINT('Ctrl Pts',(-21.6732968651578,-83.7642286605803,
81.5858463747827));
#178555=CARTESIAN_POINT('Ctrl Pts',(-21.6924449246834,-83.1764068116068,
82.1467135255278));
#178556=CARTESIAN_POINT('Ctrl Pts',(-21.7205354724368,-82.2280368066412,
82.8869760443013));
#178557=CARTESIAN_POINT('Ctrl Pts',(-21.7296499241723,-81.9071202675885,
83.1135289069823));
#178558=CARTESIAN_POINT('Ctrl Pts',(-21.7576512820501,-80.8919033173423,
83.759459534353));
#178559=CARTESIAN_POINT('Ctrl Pts',(-21.776781865191,-80.1664152904246,
84.1256686992288));
#178560=CARTESIAN_POINT('Ctrl Pts',(-21.8142821899548,-78.6704209245698,
84.7029447245979));
#178561=CARTESIAN_POINT('Ctrl Pts',(-21.832561147153,-77.9047858153812,
84.9158881957529));
#178562=CARTESIAN_POINT('Ctrl Pts',(-21.8603682992152,-76.7391633025329,
85.1210973853699));
#178563=CARTESIAN_POINT('Ctrl Pts',(-21.8695647919879,-76.3513423178009,
85.1703931784277));
#178564=CARTESIAN_POINT('Ctrl Pts',(-21.8862470655318,-75.6416511975222,
85.2262883894837));
#178565=CARTESIAN_POINT('Ctrl Pts',(-21.8937367490427,-75.3207934997004,
85.23888938658));
#178566=CARTESIAN_POINT('Ctrl Pts',(-21.9012048916249,-75.,85.23888938658));
#178567=CARTESIAN_POINT('Origin',(-30.2175364832709,-75.,72.98888938658));
#178568=CARTESIAN_POINT('',(-23.7011390782975,-75.,85.23888938658));
#178569=CARTESIAN_POINT('',(-23.0338668482845,-75.,85.23888938658));
#178570=CARTESIAN_POINT('',(-30.2175364832709,-75.,85.23888938658));
#178571=CARTESIAN_POINT('Ctrl Pts',(-23.0338668482845,-75.,85.23888938658));
#178572=CARTESIAN_POINT('Ctrl Pts',(-23.0262998213682,-75.3221275290304,
85.23888938658));
#178573=CARTESIAN_POINT('Ctrl Pts',(-23.0187520574098,-75.6443192851186,
85.2261833347588));
#178574=CARTESIAN_POINT('Ctrl Pts',(-23.0021110631907,-76.3552153782709,
85.1699594113113));
#178575=CARTESIAN_POINT('Ctrl Pts',(-22.9930462891128,-76.7429128769076,
85.1205558194789));
#178576=CARTESIAN_POINT('Ctrl Pts',(-22.9655012593938,-77.9081622466141,
84.9150515089088));
#178577=CARTESIAN_POINT('Ctrl Pts',(-22.9467881084611,-78.6735358073442,
84.7019538959952));
#178578=CARTESIAN_POINT('Ctrl Pts',(-22.9092981855756,-80.1691910224016,
84.1243808155406));
#178579=CARTESIAN_POINT('Ctrl Pts',(-22.8906024098433,-80.8945872066577,
83.7579908032428));
#178580=CARTESIAN_POINT('Ctrl Pts',(-22.8623198133254,-81.909707671069,
83.1117662916684));
#178581=CARTESIAN_POINT('Ctrl Pts',(-22.8530808382852,-82.2306302407263,
82.8850848256554));
#178582=CARTESIAN_POINT('Ctrl Pts',(-22.824902106691,-83.178870787705,82.1445137654766));
#178583=CARTESIAN_POINT('Ctrl Pts',(-22.8062350344313,-83.7665466798045,
81.5834832571938));
#178584=CARTESIAN_POINT('Ctrl Pts',(-22.7724413254797,-84.704392308442,
80.4911044305202));
#178585=CARTESIAN_POINT('Ctrl Pts',(-22.7576307643293,-85.0768946777483,
79.9827909842042));
#178586=CARTESIAN_POINT('Ctrl Pts',(-22.7258675315935,-85.7946398020826,
78.8261839460199));
#178587=CARTESIAN_POINT('Ctrl Pts',(-22.7089460654834,-86.1240687535363,
78.1709110718784));
#178588=CARTESIAN_POINT('Ctrl Pts',(-22.6824840211798,-86.5377102969475,
77.1239567949714));
#178589=CARTESIAN_POINT('Ctrl Pts',(-22.6732223531819,-86.6646548218113,
76.7509859093388));
#178590=CARTESIAN_POINT('Ctrl Pts',(-22.6450265951199,-86.9973091154328,
75.5935185211075));
#178591=CARTESIAN_POINT('Ctrl Pts',(-22.6263550089459,-87.1433282171846,
74.7941866258295));
#178592=CARTESIAN_POINT('Ctrl Pts',(-22.5907447062317,-87.2668104205586,
73.2826552319992));
#178593=CARTESIAN_POINT('Ctrl Pts',(-22.5741527572156,-87.2633568713064,
72.575340754826));
#178594=CARTESIAN_POINT('Ctrl Pts',(-22.5485936965896,-87.1633383413165,
71.4826400741407));
#178595=CARTESIAN_POINT('Ctrl Pts',(-22.5395218894431,-87.1090271249557,
71.0949390303734));
#178596=CARTESIAN_POINT('Ctrl Pts',(-22.5114905391636,-86.8856144647397,
69.9146944208019));
#178597=CARTESIAN_POINT('Ctrl Pts',(-22.4923599986056,-86.6564182770519,
69.1357839382328));
#178598=CARTESIAN_POINT('Ctrl Pts',(-22.4558442370873,-86.0680835663841,
67.6850317512595));
#178599=CARTESIAN_POINT('Ctrl Pts',(-22.438354726871,-85.7199633126631,
67.0126227254432));
#178600=CARTESIAN_POINT('Ctrl Pts',(-22.4020820150213,-84.8873137300267,
65.7140760295469));
#178601=CARTESIAN_POINT('Ctrl Pts',(-22.3837133357845,-84.3996427845281,
65.0940426269605));
#178602=CARTESIAN_POINT('Ctrl Pts',(-22.3469081045789,-83.3062230582697,
63.9499714314866));
#178603=CARTESIAN_POINT('Ctrl Pts',(-22.3281933730792,-82.7018506065069,
63.4297644457954));
#178604=CARTESIAN_POINT('Ctrl Pts',(-22.2905622558381,-81.3887496671941,
62.5054296299141));
#178605=CARTESIAN_POINT('Ctrl Pts',(-22.2719000999076,-80.6815276224345,
62.1059075553095));
#178606=CARTESIAN_POINT('Ctrl Pts',(-22.2405052754543,-79.456667547083,
61.5661199666943));
#178607=CARTESIAN_POINT('Ctrl Pts',(-22.2280571681325,-78.9600030982355,
61.3845830934975));
#178608=CARTESIAN_POINT('Ctrl Pts',(-22.1967252800081,-77.6754119885708,
61.0071614945103));
#178609=CARTESIAN_POINT('Ctrl Pts',(-22.1780462749118,-76.8768863022691,
60.8564152130231));
#178610=CARTESIAN_POINT('Ctrl Pts',(-22.1498480449613,-75.6810554373594,
60.7516270575066));
#178611=CARTESIAN_POINT('Ctrl Pts',(-22.1406722760618,-75.291363291028,
60.7361536121109));
#178612=CARTESIAN_POINT('Ctrl Pts',(-22.1125459768857,-74.0914493532944,
60.7457925788283));
#178613=CARTESIAN_POINT('Ctrl Pts',(-22.0938847507034,-73.2839428084524,
60.8326551856262));
#178614=CARTESIAN_POINT('Ctrl Pts',(-22.063245005785,-72.0048933676573,
61.1003054905414));
#178615=CARTESIAN_POINT('Ctrl Pts',(-22.0515411627234,-71.5254756547257,
61.2314758584835));
#178616=CARTESIAN_POINT('Ctrl Pts',(-22.0209260472362,-70.2880648252244,
61.6523557925693));
#178617=CARTESIAN_POINT('Ctrl Pts',(-22.0022602890765,-69.5485755014501,
61.9888304199635));
#178618=CARTESIAN_POINT('Ctrl Pts',(-21.9690290795513,-68.3241280300276,
62.6999682773972));
#178619=CARTESIAN_POINT('Ctrl Pts',(-21.9547717612397,-67.8237715270789,
63.042487347291));
#178620=CARTESIAN_POINT('Ctrl Pts',(-21.9217104988849,-66.7178005343234,
63.9266360087504));
#178621=CARTESIAN_POINT('Ctrl Pts',(-21.9029757870737,-66.136578207952,
64.494243126718));
#178622=CARTESIAN_POINT('Ctrl Pts',(-21.8653891778259,-65.1091821708323,
65.7187331359601));
#178623=CARTESIAN_POINT('Ctrl Pts',(-21.8470031674235,-64.6621100433805,
66.3698646914459));
#178624=CARTESIAN_POINT('Ctrl Pts',(-21.8101616320894,-63.8953533310233,
67.75600756508));
#178625=CARTESIAN_POINT('Ctrl Pts',(-21.7914281262343,-63.5788434313785,
68.488511004103));
#178626=CARTESIAN_POINT('Ctrl Pts',(-21.7537889598953,-63.0880856771948,
70.0181228372959));
#178627=CARTESIAN_POINT('Ctrl Pts',(-21.7351258049263,-62.91769907343,70.8123875774607));
#178628=CARTESIAN_POINT('Ctrl Pts',(-21.7031420584741,-62.765088256904,
72.1671592343946));
#178629=CARTESIAN_POINT('Ctrl Pts',(-21.6901134131729,-62.7404674381057,
72.7202445362462));
#178630=CARTESIAN_POINT('Ctrl Pts',(-21.6582246746268,-62.7721055193404,
74.0835589830707));
#178631=CARTESIAN_POINT('Ctrl Pts',(-21.6395302786362,-62.8713194665633,
74.8901552818726));
#178632=CARTESIAN_POINT('Ctrl Pts',(-21.6112531073854,-63.135734420121,
76.0639095032712));
#178633=CARTESIAN_POINT('Ctrl Pts',(-21.6020182292371,-63.2403416970923,
76.4424359642614));
#178634=CARTESIAN_POINT('Ctrl Pts',(-21.5738426915193,-63.6160958930757,
77.5852015375517));
#178635=CARTESIAN_POINT('Ctrl Pts',(-21.5551762657695,-63.9450352018044,
78.3280944544134));
#178636=CARTESIAN_POINT('Ctrl Pts',(-21.5216559429986,-64.6497030909703,
79.5703354249273));
#178637=CARTESIAN_POINT('Ctrl Pts',(-21.5071141918457,-64.9946922910918,
80.0838101461263));
#178638=CARTESIAN_POINT('Ctrl Pts',(-21.4737845652494,-65.8782661389111,
81.205510704053));
#178639=CARTESIAN_POINT('Ctrl Pts',(-21.455041961911,-66.4415023030875,
81.7906510242567));
#178640=CARTESIAN_POINT('Ctrl Pts',(-21.417405567818,-67.660078510766,82.8282291929578));
#178641=CARTESIAN_POINT('Ctrl Pts',(-21.3989810463424,-68.3099656213873,
83.2811438588942));
#178642=CARTESIAN_POINT('Ctrl Pts',(-21.3620612013757,-69.6937755080575,
84.0587466666254));
#178643=CARTESIAN_POINT('Ctrl Pts',(-21.3432906153452,-70.4250670072927,
84.380453808053));
#178644=CARTESIAN_POINT('Ctrl Pts',(-21.3056407689123,-71.9525150275356,
84.8814166417609));
#178645=CARTESIAN_POINT('Ctrl Pts',(-21.2869740863415,-72.7457946001394,
85.0569433530397));
#178646=CARTESIAN_POINT('Ctrl Pts',(-21.2565786399345,-74.0317092661945,
85.2101695732384));
#178647=CARTESIAN_POINT('Ctrl Pts',(-21.2451685319971,-74.5157019649551,
85.23888938658));
#178648=CARTESIAN_POINT('Ctrl Pts',(-21.2338306941238,-75.,85.23888938658));
#178649=CARTESIAN_POINT('Ctrl Pts',(-21.9012048916249,-75.,85.23888938658));
#178650=CARTESIAN_POINT('Ctrl Pts',(-21.9125782707414,-74.5114573603728,
85.23888938658));
#178651=CARTESIAN_POINT('Ctrl Pts',(-21.9239044356528,-74.0230636781948,
85.2096639342135));
#178652=CARTESIAN_POINT('Ctrl Pts',(-21.9478457964892,-73.0096501981885,
85.087798589088));
#178653=CARTESIAN_POINT('Ctrl Pts',(-21.9603725158002,-72.4865450089706,
84.9900411043488));
#178654=CARTESIAN_POINT('Ctrl Pts',(-21.9917799006034,-71.1859644289943,
84.6581988150706));
#178655=CARTESIAN_POINT('Ctrl Pts',(-22.0104607484747,-70.4223137584041,
84.3803088616168));
#178656=CARTESIAN_POINT('Ctrl Pts',(-22.0386708144301,-69.3400888442793,
83.8599584523561));
#178657=CARTESIAN_POINT('Ctrl Pts',(-22.0478553964703,-68.9967264445139,
83.6741804109702));
#178658=CARTESIAN_POINT('Ctrl Pts',(-22.0759893549854,-67.9694339540432,
83.0531878838158));
#178659=CARTESIAN_POINT('Ctrl Pts',(-22.0946509382444,-67.3193440801203,
82.5662839438867));
#178660=CARTESIAN_POINT('Ctrl Pts',(-22.1256282833728,-66.3456250945475,
81.6736541886862));
#178661=CARTESIAN_POINT('Ctrl Pts',(-22.1376648627038,-65.9911004793198,
81.3053234731041));
#178662=CARTESIAN_POINT('Ctrl Pts',(-22.1686009432322,-65.1360879987814,
80.2979754269664));
#178663=CARTESIAN_POINT('Ctrl Pts',(-22.1872716604109,-64.6742010588965,
79.6294747767257));
#178664=CARTESIAN_POINT('Ctrl Pts',(-22.2225387722643,-63.9469199604427,
78.3152463805165));
#178665=CARTESIAN_POINT('Ctrl Pts',(-22.2387949208875,-63.6639320783142,
77.6829525209448));
#178666=CARTESIAN_POINT('Ctrl Pts',(-22.2640205862288,-63.306769682862,
76.6609265485124));
#178667=CARTESIAN_POINT('Ctrl Pts',(-22.2730903437162,-63.1954908104488,
76.2857142817879));
#178668=CARTESIAN_POINT('Ctrl Pts',(-22.3062121802276,-62.8573307832031,
74.9064206931231));
#178669=CARTESIAN_POINT('Ctrl Pts',(-22.3304595909478,-62.7392060524829,
73.8801134406065));
#178670=CARTESIAN_POINT('Ctrl Pts',(-22.3635705750701,-62.7552096258592,
72.4566520932503));
#178671=CARTESIAN_POINT('Ctrl Pts',(-22.3727336918797,-62.7787026048876,
72.062575462975));
#178672=CARTESIAN_POINT('Ctrl Pts',(-22.3941777178521,-62.8771211376457,
71.1535425627586));
#178673=CARTESIAN_POINT('Ctrl Pts',(-22.4064273726188,-62.9659068575163,
70.6408488965085));
#178674=CARTESIAN_POINT('Ctrl Pts',(-22.4375685235945,-63.2758137808868,
69.347044370216));
#178675=CARTESIAN_POINT('Ctrl Pts',(-22.4562432421102,-63.5424162842912,
68.579427704002));
#178676=CARTESIAN_POINT('Ctrl Pts',(-22.4843567532244,-64.0451923873106,
67.4930690325406));
#178677=CARTESIAN_POINT('Ctrl Pts',(-22.4934557790672,-64.2240147061549,
67.150225775991));
#178678=CARTESIAN_POINT('Ctrl Pts',(-22.5215089054144,-64.8268883784244,
66.1167412905581));
#178679=CARTESIAN_POINT('Ctrl Pts',(-22.5401698467046,-65.3034247356707,
65.4592781454081));
#178680=CARTESIAN_POINT('Ctrl Pts',(-22.5802146006489,-66.4381635310434,
64.1817854434283));
#178681=CARTESIAN_POINT('Ctrl Pts',(-22.6013239012438,-67.1071103148403,
63.5775965683758));
#178682=CARTESIAN_POINT('Ctrl Pts',(-22.6314002579322,-68.1559973975493,
62.821409300512));
#178683=CARTESIAN_POINT('Ctrl Pts',(-22.6405576459214,-68.4868433151611,
62.6063650022873));
#178684=CARTESIAN_POINT('Ctrl Pts',(-22.6616871474955,-69.2651501216567,
62.1523432814897));
#178685=CARTESIAN_POINT('Ctrl Pts',(-22.6736287675801,-69.7182351649998,
61.924432935029));
#178686=CARTESIAN_POINT('Ctrl Pts',(-22.7044733471793,-70.9293950006989,
61.4065912085476));
#178687=CARTESIAN_POINT('Ctrl Pts',(-22.7231424866878,-71.7044473564294,
61.1626986090622));
#178688=CARTESIAN_POINT('Ctrl Pts',(-22.7516484377097,-72.8930797710573,
60.9146870002823));
#178689=CARTESIAN_POINT('Ctrl Pts',(-22.7611557181722,-73.2921072485263,
60.8518148159533));
#178690=CARTESIAN_POINT('Ctrl Pts',(-22.7896132260569,-74.4988970480152,
60.7223695192334));
#178691=CARTESIAN_POINT('Ctrl Pts',(-22.8082741749799,-75.3108695269922,
60.7160750506029));
#178692=CARTESIAN_POINT('Ctrl Pts',(-22.848284711387,-77.0109977858797,
60.8718176690941));
#178693=CARTESIAN_POINT('Ctrl Pts',(-22.8693612475713,-77.8928146678276,
61.0515873940069));
#178694=CARTESIAN_POINT('Ctrl Pts',(-22.899402690759,-79.1224479328808,
61.4466458197849));
#178695=CARTESIAN_POINT('Ctrl Pts',(-22.9085577406908,-79.4917949500698,
61.5853048049218));
#178696=CARTESIAN_POINT('Ctrl Pts',(-22.9295606185864,-80.3141866489313,
61.9402090237461));
#178697=CARTESIAN_POINT('Ctrl Pts',(-22.9413782193905,-80.7619300973313,
62.1669634645486));
#178698=CARTESIAN_POINT('Ctrl Pts',(-22.9721031811024,-81.8937436046736,
62.8303613381045));
#178699=CARTESIAN_POINT('Ctrl Pts',(-22.9907704545007,-82.5505733677596,
63.3085880388868));
#178700=CARTESIAN_POINT('Ctrl Pts',(-23.0246481285778,-83.6275270917642,
64.2694450891077));
#178701=CARTESIAN_POINT('Ctrl Pts',(-23.0395412175759,-84.0663591901492,
64.7266821152755));
#178702=CARTESIAN_POINT('Ctrl Pts',(-23.0714953847188,-84.9353750704311,
65.785169794588));
#178703=CARTESIAN_POINT('Ctrl Pts',(-23.0885313434982,-85.350533922909,
66.3955822364597));
#178704=CARTESIAN_POINT('Ctrl Pts',(-23.115121820679,-85.8998462468878,
67.3843050696062));
#178705=CARTESIAN_POINT('Ctrl Pts',(-23.124395924343,-86.0746091169767,
67.7380754007731));
#178706=CARTESIAN_POINT('Ctrl Pts',(-23.152600459397,-86.5555332339301,
68.8428995309868));
#178707=CARTESIAN_POINT('Ctrl Pts',(-23.171275342588,-86.8044920144504,
69.6164202927912));
#178708=CARTESIAN_POINT('Ctrl Pts',(-23.1994228629323,-87.0569153815377,
70.7880363075798));
#178709=CARTESIAN_POINT('Ctrl Pts',(-23.2085556457866,-87.1205556841311,
71.1708978212189));
#178710=CARTESIAN_POINT('Ctrl Pts',(-23.2366418715287,-87.2606654242543,
72.3606066348551));
#178711=CARTESIAN_POINT('Ctrl Pts',(-23.2553027772918,-87.2753795146351,
73.1724963721619));
#178712=CARTESIAN_POINT('Ctrl Pts',(-23.2851263749657,-87.17244042403,74.4408006941545));
#178713=CARTESIAN_POINT('Ctrl Pts',(-23.2960263103336,-87.1089602337673,
74.8992388899376));
#178714=CARTESIAN_POINT('Ctrl Pts',(-23.3258610568216,-86.8633929460291,
76.1477690985458));
#178715=CARTESIAN_POINT('Ctrl Pts',(-23.3445220065786,-86.6286267135887,
76.9250870117486));
#178716=CARTESIAN_POINT('Ctrl Pts',(-23.3845289600388,-85.9758005354618,
78.5024246708648));
#178717=CARTESIAN_POINT('Ctrl Pts',(-23.4056020650923,-85.5427152277301,
79.2911461895476));
#178718=CARTESIAN_POINT('Ctrl Pts',(-23.4356398538035,-84.8009272233128,
80.3482224326073));
#178719=CARTESIAN_POINT('Ctrl Pts',(-23.4447946602598,-84.5589973564942,
80.6598428167345));
#178720=CARTESIAN_POINT('Ctrl Pts',(-23.46578440528,-83.9765759341496,81.3396051526625));
#178721=CARTESIAN_POINT('Ctrl Pts',(-23.4775891431064,-83.6276689178653,
81.6996126601055));
#178722=CARTESIAN_POINT('Ctrl Pts',(-23.508301690374,-82.6590475139244,
82.5835950680837));
#178723=CARTESIAN_POINT('Ctrl Pts',(-23.5269687829504,-82.0076454016134,
83.0691816056367));
#178724=CARTESIAN_POINT('Ctrl Pts',(-23.5607709951479,-80.7735138332313,
83.8113406047466));
#178725=CARTESIAN_POINT('Ctrl Pts',(-23.5755899146944,-80.2097333843237,
84.0937349816615));
#178726=CARTESIAN_POINT('Ctrl Pts',(-23.6073721691478,-78.9485792488077,
84.6081692691668));
#178727=CARTESIAN_POINT('Ctrl Pts',(-23.6243049028971,-78.2469636135959,
84.8234222667961));
#178728=CARTESIAN_POINT('Ctrl Pts',(-23.6507796690209,-77.1450156533659,
85.0560554886073));
#178729=CARTESIAN_POINT('Ctrl Pts',(-23.6600426239509,-76.7559946324765,
85.1187728869583));
#178730=CARTESIAN_POINT('Ctrl Pts',(-23.679943295204,-75.9112525200789,
85.2134651605353));
#178731=CARTESIAN_POINT('Ctrl Pts',(-23.6905408363261,-75.4556659020494,
85.23888938658));
#178732=CARTESIAN_POINT('Ctrl Pts',(-23.7011390782975,-75.,85.23888938658));
#178733=CARTESIAN_POINT('Origin',(-30.2175364832709,-75.,72.98888938658));
#178734=CARTESIAN_POINT('',(-25.5022222432624,-75.0000000426705,85.23888938658));
#178735=CARTESIAN_POINT('',(-24.8339325830033,-75.0000000321728,85.23888938658));
#178736=CARTESIAN_POINT('',(-30.2175364832709,-75.,85.23888938658));
#178737=CARTESIAN_POINT('Ctrl Pts',(-24.8339325837594,-75.0000000321906,
85.23888938658));
#178738=CARTESIAN_POINT('Ctrl Pts',(-24.8240890920827,-75.4186207774789,
85.23888938548));
#178739=CARTESIAN_POINT('Ctrl Pts',(-24.8142463699096,-75.8372234157294,
85.2174310040483));
#178740=CARTESIAN_POINT('Ctrl Pts',(-24.7917842720247,-76.7930051185784,
85.1190611901574));
#178741=CARTESIAN_POINT('Ctrl Pts',(-24.779240029544,-77.3275829231129,
85.0279214181392));
#178742=CARTESIAN_POINT('Ctrl Pts',(-24.7477156335147,-78.642378545885,
84.7128899054087));
#178743=CARTESIAN_POINT('Ctrl Pts',(-24.7285714438196,-79.4097119983233,
84.4463563610969));
#178744=CARTESIAN_POINT('Ctrl Pts',(-24.6983710047082,-80.5840955968139,
83.9028429934588));
#178745=CARTESIAN_POINT('Ctrl Pts',(-24.6871669947593,-81.0106812213281,
83.673842227766));
#178746=CARTESIAN_POINT('Ctrl Pts',(-24.6569802944016,-82.1124568073987,
82.9954752621748));
#178747=CARTESIAN_POINT('Ctrl Pts',(-24.6378436148025,-82.7584751441121,
82.503345126547));
#178748=CARTESIAN_POINT('Ctrl Pts',(-24.6079844560184,-83.6948921980658,
81.6307689182165));
#178749=CARTESIAN_POINT('Ctrl Pts',(-24.5971019203464,-84.019905075365,
81.2909700641096));
#178750=CARTESIAN_POINT('Ctrl Pts',(-24.5672361820081,-84.8499465114587,
80.3167309303754));
#178751=CARTESIAN_POINT('Ctrl Pts',(-24.5481022126914,-85.3128399117216,
79.6495232492781));
#178752=CARTESIAN_POINT('Ctrl Pts',(-24.5183347636273,-85.9329599516399,
78.5341685650817));
#178753=CARTESIAN_POINT('Ctrl Pts',(-24.5075385009762,-86.136010627728,
78.1142187159543));
#178754=CARTESIAN_POINT('Ctrl Pts',(-24.4777588966594,-86.6250909168048,
76.9355262006453));
#178755=CARTESIAN_POINT('Ctrl Pts',(-24.4586257282933,-86.8605662093157,
76.1583771809833));
#178756=CARTESIAN_POINT('Ctrl Pts',(-24.4212195702551,-87.1714573790356,
74.5851242120943));
#178757=CARTESIAN_POINT('Ctrl Pts',(-24.4028352669799,-87.2492868048642,
73.7934445278655));
#178758=CARTESIAN_POINT('Ctrl Pts',(-24.3586717168977,-87.2509629528297,
71.9154303363282));
#178759=CARTESIAN_POINT('Ctrl Pts',(-24.3337053505123,-87.1079379062421,
70.8356943427115));
#178760=CARTESIAN_POINT('Ctrl Pts',(-24.2990942202318,-86.7225084636294,
69.4114237720193));
#178761=CARTESIAN_POINT('Ctrl Pts',(-24.2898811077845,-86.6023221799552,
69.0390051751667));
#178762=CARTESIAN_POINT('Ctrl Pts',(-24.2624431493016,-86.190382005262,
67.9447527514958));
#178763=CARTESIAN_POINT('Ctrl Pts',(-24.2444727175805,-85.8474759337272,
67.2443071888604));
#178764=CARTESIAN_POINT('Ctrl Pts',(-24.2079540895495,-85.029865504896,
65.9121354125224));
#178765=CARTESIAN_POINT('Ctrl Pts',(-24.1894233646458,-84.5559184545767,
65.284145526537));
#178766=CARTESIAN_POINT('Ctrl Pts',(-24.1603876187993,-83.7140917278025,
64.3668975747821));
#178767=CARTESIAN_POINT('Ctrl Pts',(-24.1497308430971,-83.3841817416666,
64.045756103363));
#178768=CARTESIAN_POINT('Ctrl Pts',(-24.1200904967253,-82.42567845459,63.2124925373835));
#178769=CARTESIAN_POINT('Ctrl Pts',(-24.1009586935858,-81.7631562505982,
62.7429947730267));
#178770=CARTESIAN_POINT('Ctrl Pts',(-24.0726494833285,-80.7082953049164,
62.1426530032964));
#178771=CARTESIAN_POINT('Ctrl Pts',(-24.0632861415975,-80.3477750630805,
61.960436157542));
#178772=CARTESIAN_POINT('Ctrl Pts',(-24.0349981776565,-79.2383522775918,
61.4669175319571));
#178773=CARTESIAN_POINT('Ctrl Pts',(-24.0158499568544,-78.4669173928705,
61.2117952476941));
#178774=CARTESIAN_POINT('Ctrl Pts',(-23.9782996418965,-76.8978858706879,
60.8605644697829));
#178775=CARTESIAN_POINT('Ctrl Pts',(-23.9598787486126,-76.1046638010944,
60.7627717972648));
#178776=CARTESIAN_POINT('Ctrl Pts',(-23.9225209070743,-74.5163021095262,
60.7228769149453));
#178777=CARTESIAN_POINT('Ctrl Pts',(-23.9040340644223,-73.724947833655,
60.7797421661867));
#178778=CARTESIAN_POINT('Ctrl Pts',(-23.867818555596,-72.1897988286059,
61.0410216104658));
#178779=CARTESIAN_POINT('Ctrl Pts',(-23.8498266245349,-71.4486738007521,
61.2399809173404));
#178780=CARTESIAN_POINT('Ctrl Pts',(-23.816353900739,-70.1109997955915,
61.7373249692391));
#178781=CARTESIAN_POINT('Ctrl Pts',(-23.801028173916,-69.510696748442,62.0176736513018));
#178782=CARTESIAN_POINT('Ctrl Pts',(-23.7667340773171,-68.2317222814234,
62.7463376623581));
#178783=CARTESIAN_POINT('Ctrl Pts',(-23.7475858108103,-67.5690325328267,
63.2164706046294));
#178784=CARTESIAN_POINT('Ctrl Pts',(-23.7168375815155,-66.5758610383385,
64.0808839610502));
#178785=CARTESIAN_POINT('Ctrl Pts',(-23.7051159936441,-66.2150360684201,
64.4365162843896));
#178786=CARTESIAN_POINT('Ctrl Pts',(-23.6841121303596,-65.6140585796894,
65.1071305224153));
#178787=CARTESIAN_POINT('Ctrl Pts',(-23.6748340888881,-65.3652061057705,
65.4133522204306));
#178788=CARTESIAN_POINT('Ctrl Pts',(-23.6444357926001,-64.5991970897933,
66.4548887387677));
#178789=CARTESIAN_POINT('Ctrl Pts',(-23.6236457131505,-64.148089732302,
67.2351162176928));
#178790=CARTESIAN_POINT('Ctrl Pts',(-23.5837708328748,-63.4603125304579,
68.7991125321045));
#178791=CARTESIAN_POINT('Ctrl Pts',(-23.5646396113034,-63.2085878053367,
69.5711096082091));
#178792=CARTESIAN_POINT('Ctrl Pts',(-23.5272447654636,-62.8648131988296,
71.1371207779274));
#178793=CARTESIAN_POINT('Ctrl Pts',(-23.5088651754443,-62.7703863033566,
71.9266510474476));
#178794=CARTESIAN_POINT('Ctrl Pts',(-23.4717864698385,-62.7357437305451,
73.5030121464496));
#178795=CARTESIAN_POINT('Ctrl Pts',(-23.4535349993682,-62.7937115313033,
74.2861295015583));
#178796=CARTESIAN_POINT('Ctrl Pts',(-23.4164551921254,-63.0630028917562,
75.8572822715988));
#178797=CARTESIAN_POINT('Ctrl Pts',(-23.397351434627,-63.2789054964409,
76.6406718202847));
#178798=CARTESIAN_POINT('Ctrl Pts',(-23.3646755460105,-63.7812321879032,
77.9431193759609));
#178799=CARTESIAN_POINT('Ctrl Pts',(-23.3511192603518,-64.030745028914,
78.4734669276472));
#178800=CARTESIAN_POINT('Ctrl Pts',(-23.3185857738792,-64.7138240613626,
79.6906692077356));
#178801=CARTESIAN_POINT('Ctrl Pts',(-23.2994388168291,-65.1795868250031,
80.3563008656006));
#178802=CARTESIAN_POINT('Ctrl Pts',(-23.2690174517819,-66.0287446225397,
81.3448392015911));
#178803=CARTESIAN_POINT('Ctrl Pts',(-23.2576049321812,-66.3720958714854,
81.6989174992544));
#178804=CARTESIAN_POINT('Ctrl Pts',(-23.2272100597294,-67.3338647368048,
82.5779054743888));
#178805=CARTESIAN_POINT('Ctrl Pts',(-23.2080718369678,-67.9846391961632,
83.0637875831979));
#178806=CARTESIAN_POINT('Ctrl Pts',(-23.1800799565349,-69.0123713578003,
83.6829363660246));
#178807=CARTESIAN_POINT('Ctrl Pts',(-23.1710384235269,-69.3555489192395,
83.8679752644891));
#178808=CARTESIAN_POINT('Ctrl Pts',(-23.1430907969932,-70.4380163692609,
84.386605489894));
#178809=CARTESIAN_POINT('Ctrl Pts',(-23.123946444744,-71.2020358155108,
84.6634382317728));
#178810=CARTESIAN_POINT('Ctrl Pts',(-23.0926812947613,-72.4989119323465,
84.9924359645458));
#178811=CARTESIAN_POINT('Ctrl Pts',(-23.080469709526,-73.0178851199722,
85.0889634234049));
#178812=CARTESIAN_POINT('Ctrl Pts',(-23.0567980047726,-74.0257569555179,
85.2098250434086));
#178813=CARTESIAN_POINT('Ctrl Pts',(-23.045311437801,-74.5128050445081,
85.23888938658));
#178814=CARTESIAN_POINT('Ctrl Pts',(-23.0338668482845,-75.,85.23888938658));
#178815=CARTESIAN_POINT('',(-24.5016804832958,-70.810146674246,61.4773938111869));
#178816=CARTESIAN_POINT('Ctrl Pts',(-23.7011390782975,-75.,85.23888938658));
#178817=CARTESIAN_POINT('Ctrl Pts',(-23.7093709734307,-74.6460739496634,
85.23888938658));
#178818=CARTESIAN_POINT('Ctrl Pts',(-23.7176237986497,-74.2921005445638,
85.2235510126129));
#178819=CARTESIAN_POINT('Ctrl Pts',(-23.7426439198799,-73.2305729145749,
85.1312697475636));
#178820=CARTESIAN_POINT('Ctrl Pts',(-23.7593555478455,-72.5287710103631,
85.0080952031386));
#178821=CARTESIAN_POINT('Ctrl Pts',(-23.7850339826181,-71.4635413204302,
84.7238411137035));
#178822=CARTESIAN_POINT('Ctrl Pts',(-23.7941069531373,-71.0905026313075,
84.6048896260841));
#178823=CARTESIAN_POINT('Ctrl Pts',(-23.8216922606333,-69.9830109634707,
84.1923369604305));
#178824=CARTESIAN_POINT('Ctrl Pts',(-23.8403638222321,-69.2706713170174,
83.8453258300852));
#178825=CARTESIAN_POINT('Ctrl Pts',(-23.8760448608956,-67.9669247983626,
83.0459347916159));
#178826=CARTESIAN_POINT('Ctrl Pts',(-23.8931306014014,-67.3733273244117,
82.6035745495171));
#178827=CARTESIAN_POINT('Ctrl Pts',(-23.9197763709446,-66.5293923328939,
81.8470500810306));
#178828=CARTESIAN_POINT('Ctrl Pts',(-23.9290554590638,-66.2484678470804,
81.5696172793188));
#178829=CARTESIAN_POINT('Ctrl Pts',(-23.9572633824639,-65.4328354167441,
80.6823258149776));
#178830=CARTESIAN_POINT('Ctrl Pts',(-23.9759397936857,-64.9448372571729,
80.0325605683808));
#178831=CARTESIAN_POINT('Ctrl Pts',(-24.0041197058617,-64.32286214134,79.0065862565139));
#178832=CARTESIAN_POINT('Ctrl Pts',(-24.0132818683174,-64.1370893885365,
78.6643736992936));
#178833=CARTESIAN_POINT('Ctrl Pts',(-24.0413961707415,-63.6157767100914,
77.5843454866065));
#178834=CARTESIAN_POINT('Ctrl Pts',(-24.0600570986652,-63.3368680992437,
76.8216572022194));
#178835=CARTESIAN_POINT('Ctrl Pts',(-24.0902184752852,-63.0167121988657,
75.5754738617746));
#178836=CARTESIAN_POINT('Ctrl Pts',(-24.1014510015581,-62.9251664533932,
75.1073798151019));
#178837=CARTESIAN_POINT('Ctrl Pts',(-24.1316095233761,-62.7522382278562,
73.8322716919893));
#178838=CARTESIAN_POINT('Ctrl Pts',(-24.1502711001275,-62.7232758076924,
73.0205744395089));
#178839=CARTESIAN_POINT('Ctrl Pts',(-24.1812446426325,-62.8070419418149,
71.7024373076537));
#178840=CARTESIAN_POINT('Ctrl Pts',(-24.1932775224243,-62.871247683176,
71.1954139308815));
#178841=CARTESIAN_POINT('Ctrl Pts',(-24.2242100206175,-63.1187580708244,
69.8976782655188));
#178842=CARTESIAN_POINT('Ctrl Pts',(-24.2428806807743,-63.3492624146768,
69.1185135556219));
#178843=CARTESIAN_POINT('Ctrl Pts',(-24.2713913813562,-63.8073238446275,
67.9939421274307));
#178844=CARTESIAN_POINT('Ctrl Pts',(-24.2808987546529,-63.9780136014144,
67.6277967580806));
#178845=CARTESIAN_POINT('Ctrl Pts',(-24.3093553707275,-64.5445985287478,
66.5543506278136));
#178846=CARTESIAN_POINT('Ctrl Pts',(-24.3280161641349,-64.9928562708749,
65.8772242217274));
#178847=CARTESIAN_POINT('Ctrl Pts',(-24.3580370491845,-65.8020589964969,
64.8844487304048));
#178848=CARTESIAN_POINT('Ctrl Pts',(-24.3691318118908,-66.1202442711813,
64.5370247261621));
#178849=CARTESIAN_POINT('Ctrl Pts',(-24.4003010084835,-67.0732939630522,
63.6097814939158));
#178850=CARTESIAN_POINT('Ctrl Pts',(-24.4200738965064,-67.7502537057925,
63.0772037825501));
#178851=CARTESIAN_POINT('Ctrl Pts',(-24.4503832105327,-68.8430267947801,
62.3897936348474));
#178852=CARTESIAN_POINT('Ctrl Pts',(-24.4605586043277,-69.2206343750692,
62.1792601721665));
#178853=CARTESIAN_POINT('Ctrl Pts',(-24.4808914428694,-69.9997531482767,
61.7973829963986));
#178854=CARTESIAN_POINT('Ctrl Pts',(-24.4910333535345,-70.4008833660698,
61.6266532065697));
#178855=CARTESIAN_POINT('Ctrl Pts',(-24.5011646348533,-70.8102538861047,
61.4776545483405));
#178856=CARTESIAN_POINT('Ctrl Pts',(-24.5020520203782,-70.8102354594193,
61.477661255121));
#178857=CARTESIAN_POINT('Ctrl Pts',(-24.5170138898973,-71.4199016714757,
61.2557598343783));
#178858=CARTESIAN_POINT('Ctrl Pts',(-24.5316546309711,-72.0462294868208,
61.0826445498868));
#178859=CARTESIAN_POINT('Ctrl Pts',(-24.5602757693805,-73.2632244680831,
60.8482598525762));
#178860=CARTESIAN_POINT('Ctrl Pts',(-24.574394247675,-73.8504440319907,
60.7786574268127));
#178861=CARTESIAN_POINT('Ctrl Pts',(-24.607621744178,-75.2350038732028,
60.7153392574193));
#178862=CARTESIAN_POINT('Ctrl Pts',(-24.6264802640425,-76.0312995082613,
60.7564850607017));
#178863=CARTESIAN_POINT('Ctrl Pts',(-24.6563175955979,-77.3098798478237,
60.9483588610369));
#178864=CARTESIAN_POINT('Ctrl Pts',(-24.6676078796724,-77.7968319565327,
61.0520702099325));
#178865=CARTESIAN_POINT('Ctrl Pts',(-24.6863694883698,-78.5884181136076,
61.2717739860067));
#178866=CARTESIAN_POINT('Ctrl Pts',(-24.6937985887024,-78.8971436095272,
61.3708083634057));
#178867=CARTESIAN_POINT('Ctrl Pts',(-24.7389586259458,-80.7111991001541,
62.0331827774839));
#178868=CARTESIAN_POINT('Ctrl Pts',(-24.7776288169391,-82.0977571612455,
62.876148472946));
#178869=CARTESIAN_POINT('Ctrl Pts',(-24.8289724910095,-83.7555283971949,
64.3972525522298));
#178870=CARTESIAN_POINT('Ctrl Pts',(-24.8436758327869,-84.1941175156466,
64.8683164559407));
#178871=CARTESIAN_POINT('Ctrl Pts',(-24.8751693428624,-85.0173546005428,
65.9051592990021));
#178872=CARTESIAN_POINT('Ctrl Pts',(-24.8916156475598,-85.3957345879719,
66.4731130419377));
#178873=CARTESIAN_POINT('Ctrl Pts',(-24.9260540953204,-86.1004262191091,
67.7499114359243));
#178874=CARTESIAN_POINT('Ctrl Pts',(-24.9438298919491,-86.4103320355067,
68.4644349344013));
#178875=CARTESIAN_POINT('Ctrl Pts',(-24.9744933033455,-86.8256403399536,
69.7426445824062));
#178876=CARTESIAN_POINT('Ctrl Pts',(-24.9874728304087,-86.9631792015539,
70.2932967638212));
#178877=CARTESIAN_POINT('Ctrl Pts',(-25.0174918160325,-87.1839460707716,
71.5391680548982));
#178878=CARTESIAN_POINT('Ctrl Pts',(-25.0343743520946,-87.2467711270798,
72.2359985628576));
#178879=CARTESIAN_POINT('Ctrl Pts',(-25.069373645407,-87.2533583404747,
73.716367234393));
#178880=CARTESIAN_POINT('Ctrl Pts',(-25.0872874990229,-87.1819520576795,
74.4968924469779));
#178881=CARTESIAN_POINT('Ctrl Pts',(-25.1182337732407,-86.9299022857364,
75.8296327205571));
#178882=CARTESIAN_POINT('Ctrl Pts',(-25.1313641354787,-86.7836145760966,
76.3857733755451));
#178883=CARTESIAN_POINT('Ctrl Pts',(-25.1616235200426,-86.3730977679734,
77.5940615491839));
#178884=CARTESIAN_POINT('Ctrl Pts',(-25.1785926128937,-86.0906692279497,
78.237892470731));
#178885=CARTESIAN_POINT('Ctrl Pts',(-25.2137063690154,-85.3797439980679,
79.5414950453244));
#178886=CARTESIAN_POINT('Ctrl Pts',(-25.2316490835065,-84.9397667151215,
80.1914373133926));
#178887=CARTESIAN_POINT('Ctrl Pts',(-25.2636264458116,-84.046639685404,
81.2716017676295));
#178888=CARTESIAN_POINT('Ctrl Pts',(-25.2777934774843,-83.6169840088397,
81.7177314162769));
#178889=CARTESIAN_POINT('Ctrl Pts',(-25.3087673989437,-82.6450152742699,
82.5849394841047));
#178890=CARTESIAN_POINT('Ctrl Pts',(-25.3252836739824,-82.0973367114445,
82.9967993332136));
#178891=CARTESIAN_POINT('Ctrl Pts',(-25.3535589933042,-81.0836659351523,
83.6338335088741));
#178892=CARTESIAN_POINT('Ctrl Pts',(-25.3654650593838,-80.632456500941,
83.879310321471));
#178893=CARTESIAN_POINT('Ctrl Pts',(-25.3895534221763,-79.6802738010836,
84.3222881724379));
#178894=CARTESIAN_POINT('Ctrl Pts',(-25.4016967561352,-79.1790002497226,
84.516544952236));
#178895=CARTESIAN_POINT('Ctrl Pts',(-25.4219677213753,-78.3401187098178,
84.7796989058047));
#178896=CARTESIAN_POINT('Ctrl Pts',(-25.4299951547185,-78.009492109492,
84.8683899617203));
#178897=CARTESIAN_POINT('Ctrl Pts',(-25.4542801353021,-77.0137116115949,
85.0912648777087));
#178898=CARTESIAN_POINT('Ctrl Pts',(-25.470647235657,-76.340671534467,85.1841811302934));
#178899=CARTESIAN_POINT('Ctrl Pts',(-25.4918825248931,-75.4424234399546,
85.2328976122229));
#178900=CARTESIAN_POINT('Ctrl Pts',(-25.4970704667471,-75.2212078057676,
85.238889385809));
#178901=CARTESIAN_POINT('Ctrl Pts',(-25.5022222442556,-75.0000000426936,
85.23888938658));
#178902=CARTESIAN_POINT('Origin',(-30.2175364832709,-75.,72.98888938658));
#178903=CARTESIAN_POINT('',(-27.3010916068384,-75.,85.23888938658));
#178904=CARTESIAN_POINT('',(-26.6339799854461,-75.,85.23888938658));
#178905=CARTESIAN_POINT('',(-30.2175364832709,-75.,85.23888938658));
#178906=CARTESIAN_POINT('',(-25.633313136734,-70.8103134300187,61.4777794235982));
#178907=CARTESIAN_POINT('Ctrl Pts',(-26.6339799854461,-75.,85.23888938658));
#178908=CARTESIAN_POINT('Ctrl Pts',(-26.6191344608489,-75.6381113181522,
85.23888938658));
#178909=CARTESIAN_POINT('Ctrl Pts',(-26.6038014874433,-76.2753923550697,
85.1890298364595));
#178910=CARTESIAN_POINT('Ctrl Pts',(-26.55107738843,-78.4651155960251,84.8441233862049));
#178911=CARTESIAN_POINT('Ctrl Pts',(-26.5162064900661,-79.9621477761098,
84.2995345190604));
#178912=CARTESIAN_POINT('Ctrl Pts',(-26.4650951794551,-81.8044674005743,
83.1912670902666));
#178913=CARTESIAN_POINT('Ctrl Pts',(-26.4514103903528,-82.2730949941767,
82.8626618849234));
#178914=CARTESIAN_POINT('Ctrl Pts',(-26.4174837873031,-83.390798188754,
81.9560294276125));
#178915=CARTESIAN_POINT('Ctrl Pts',(-26.3977171030397,-84.0045770730602,
81.3394994348124));
#178916=CARTESIAN_POINT('Ctrl Pts',(-26.3402521639579,-85.5705161864811,
79.3912524177552));
#178917=CARTESIAN_POINT('Ctrl Pts',(-26.3007334647644,-86.328511742847,
77.9276020172795));
#178918=CARTESIAN_POINT('Ctrl Pts',(-26.2463389567453,-86.9800758096105,
75.6502720095092));
#178919=CARTESIAN_POINT('Ctrl Pts',(-26.2295436539528,-87.1184104644288,
74.9252011693067));
#178920=CARTESIAN_POINT('Ctrl Pts',(-26.1926456748223,-87.2711508562067,
73.3776538247701));
#178921=CARTESIAN_POINT('Ctrl Pts',(-26.173035722336,-87.2697165201255,
72.5571854533876));
#178922=CARTESIAN_POINT('Ctrl Pts',(-26.1356161371819,-87.1065512939891,
70.9611978811798));
#178923=CARTESIAN_POINT('Ctrl Pts',(-26.1178365702095,-86.9515753283765,
70.1888978228139));
#178924=CARTESIAN_POINT('Ctrl Pts',(-26.0845253654628,-86.5340109045882,
68.8107300735781));
#178925=CARTESIAN_POINT('Ctrl Pts',(-26.068876771263,-86.2944863433289,
68.2008865799041));
#178926=CARTESIAN_POINT('Ctrl Pts',(-26.0144120081656,-85.2910502638115,
66.1462570722396));
#178927=CARTESIAN_POINT('Ctrl Pts',(-25.9783338713947,-84.2886487783204,
64.8373035794661));
#178928=CARTESIAN_POINT('Ctrl Pts',(-25.9261162342618,-82.6338842686394,
63.3917374287345));
#178929=CARTESIAN_POINT('Ctrl Pts',(-25.9125953639996,-82.1833250516838,
63.0500080545254));
#178930=CARTESIAN_POINT('Ctrl Pts',(-25.8784056924184,-80.9705478192564,
62.2558564345393));
#178931=CARTESIAN_POINT('Ctrl Pts',(-25.8582495348373,-80.1799566242127,
61.8527550569305));
#178932=CARTESIAN_POINT('Ctrl Pts',(-25.8097366847142,-78.208345513547,
61.1032577663287));
#178933=CARTESIAN_POINT('Ctrl Pts',(-25.7800416048472,-77.0050537713077,
60.8422261194989));
#178934=CARTESIAN_POINT('Ctrl Pts',(-25.7334192216211,-75.0137007310833,
60.7146562684266));
#178935=CARTESIAN_POINT('Ctrl Pts',(-25.7159396638928,-74.2413171425731,
60.7381187694672));
#178936=CARTESIAN_POINT('Ctrl Pts',(-25.6770209109218,-72.5663055900796,
60.9480963661747));
#178937=CARTESIAN_POINT('Ctrl Pts',(-25.6549234401735,-71.672029307235,
61.1639951908746));
#178938=CARTESIAN_POINT('Ctrl Pts',(-25.6332414813969,-70.8102679226971,
61.4776494394493));
#178939=CARTESIAN_POINT('Ctrl Pts',(-25.6339066113238,-70.8102535523114,
61.4776546698313));
#178940=CARTESIAN_POINT('Ctrl Pts',(-25.6242937099174,-70.4261322987331,
61.6174633608416));
#178941=CARTESIAN_POINT('Ctrl Pts',(-25.6147024533179,-70.0492486347529,
61.7764115896691));
#178942=CARTESIAN_POINT('Ctrl Pts',(-25.5956768735074,-69.3152583045736,
62.1302028533648));
#178943=CARTESIAN_POINT('Ctrl Pts',(-25.5862533550733,-68.9584906670528,
62.3245785057338));
#178944=CARTESIAN_POINT('Ctrl Pts',(-25.5582468647041,-67.9316626967255,
62.9521117335403));
#178945=CARTESIAN_POINT('Ctrl Pts',(-25.5394278437801,-67.2935121541466,
63.4333497677411));
#178946=CARTESIAN_POINT('Ctrl Pts',(-25.5085183005986,-66.320848898401,
64.3280781054394));
#178947=CARTESIAN_POINT('Ctrl Pts',(-25.4963674127205,-65.9582084371738,
64.7073846238268));
#178948=CARTESIAN_POINT('Ctrl Pts',(-25.4652733071935,-65.0995746277491,
65.7293388705268));
#178949=CARTESIAN_POINT('Ctrl Pts',(-25.4461251728386,-64.641045296391,
66.4001451516963));
#178950=CARTESIAN_POINT('Ctrl Pts',(-25.415270760131,-64.0072048647155,
67.5591971914811));
#178951=CARTESIAN_POINT('Ctrl Pts',(-25.4034486513504,-63.7905065049081,
68.0219630866319));
#178952=CARTESIAN_POINT('Ctrl Pts',(-25.3726450418276,-63.3062091384989,
69.2506789863387));
#178953=CARTESIAN_POINT('Ctrl Pts',(-25.353504210212,-63.0846211875859,
70.0320819483146));
#178954=CARTESIAN_POINT('Ctrl Pts',(-25.3160474904702,-62.8016579372957,
71.6122576979627));
#178955=CARTESIAN_POINT('Ctrl Pts',(-25.297643697917,-62.7380386506744,
72.4066832473265));
#178956=CARTESIAN_POINT('Ctrl Pts',(-25.2604576408576,-62.7655029750708,
73.987755581599));
#178957=CARTESIAN_POINT('Ctrl Pts',(-25.2421276488185,-62.8548071581125,
74.7707279630282));
#178958=CARTESIAN_POINT('Ctrl Pts',(-25.2063268678832,-63.1753222669767,
76.2762133792397));
#178959=CARTESIAN_POINT('Ctrl Pts',(-25.1886072384691,-63.3996928090884,
76.9966778852067));
#178960=CARTESIAN_POINT('Ctrl Pts',(-25.1558679715698,-63.9358357907009,
78.2861385950576));
#178961=CARTESIAN_POINT('Ctrl Pts',(-25.1409607315228,-64.2293208450733,
78.8599241544918));
#178962=CARTESIAN_POINT('Ctrl Pts',(-25.1070825164293,-64.9912250232401,
80.0983083637154));
#178963=CARTESIAN_POINT('Ctrl Pts',(-25.0879342663996,-65.483397982614,
80.7447709155075));
#178964=CARTESIAN_POINT('Ctrl Pts',(-25.0598334224574,-66.3035771689732,
81.6253876379661));
#178965=CARTESIAN_POINT('Ctrl Pts',(-25.0507113522975,-66.5850369338083,
81.8998528009869));
#178966=CARTESIAN_POINT('Ctrl Pts',(-25.0227044718996,-67.4861461452905,
82.6977361539544));
#178967=CARTESIAN_POINT('Ctrl Pts',(-25.0035760654612,-68.1449440694906,
83.1735792585048));
#178968=CARTESIAN_POINT('Ctrl Pts',(-24.9715809479598,-69.3277697208447,
83.8608207678011));
#178969=CARTESIAN_POINT('Ctrl Pts',(-24.9586751843249,-69.8281865474364,
84.1075868446727));
#178970=CARTESIAN_POINT('Ctrl Pts',(-24.926790186775,-71.0931893099014,
84.6274461047887));
#178971=CARTESIAN_POINT('Ctrl Pts',(-24.9076447817233,-71.8714347608642,
84.8603362697242));
#178972=CARTESIAN_POINT('Ctrl Pts',(-24.8795977432193,-73.051108394981,
85.0891972153212));
#178973=CARTESIAN_POINT('Ctrl Pts',(-24.8705154761017,-73.4386120474841,
85.1452743685051));
#178974=CARTESIAN_POINT('Ctrl Pts',(-24.8522935929042,-74.2178734886321,
85.2201639890821));
#178975=CARTESIAN_POINT('Ctrl Pts',(-24.8431278920032,-74.6089450166963,
85.2388893876076));
#178976=CARTESIAN_POINT('Ctrl Pts',(-24.8339325837594,-75.0000000321906,
85.23888938658));
#178977=CARTESIAN_POINT('Ctrl Pts',(-25.5022222442556,-75.0000000426936,
85.23888938658));
#178978=CARTESIAN_POINT('Ctrl Pts',(-25.5084713324199,-74.7316757969748,
85.2388893875151));
#178979=CARTESIAN_POINT('Ctrl Pts',(-25.514666650198,-74.4633631194671,
85.2300733235928));
#178980=CARTESIAN_POINT('Ctrl Pts',(-25.5333912487406,-73.6492987417742,
85.1764949934327));
#178981=CARTESIAN_POINT('Ctrl Pts',(-25.5457654009036,-73.1061275916619,
85.1039777725178));
#178982=CARTESIAN_POINT('Ctrl Pts',(-25.5723880952531,-71.9740141827245,
84.8748141893723));
#178983=CARTESIAN_POINT('Ctrl Pts',(-25.5869006846059,-71.3882048389132,
84.7100966808637));
#178984=CARTESIAN_POINT('Ctrl Pts',(-25.6202442386018,-70.0801474247998,
84.2348780670153));
#178985=CARTESIAN_POINT('Ctrl Pts',(-25.6388269630157,-69.370629083816,
83.8970251730161));
#178986=CARTESIAN_POINT('Ctrl Pts',(-25.667453495464,-68.3075408310235,
83.2592888459669));
#178987=CARTESIAN_POINT('Ctrl Pts',(-25.6778214458911,-67.930189470185,
83.0032737999176));
#178988=CARTESIAN_POINT('Ctrl Pts',(-25.6994148362723,-67.1782982274196,
82.429428653647));
#178989=CARTESIAN_POINT('Ctrl Pts',(-25.710669108433,-66.8068287781899,
82.1089083842358));
#178990=CARTESIAN_POINT('Ctrl Pts',(-25.7390813344379,-65.947071862009,
81.2720365269247));
#178991=CARTESIAN_POINT('Ctrl Pts',(-25.7562503973109,-65.4825513593372,
80.7338373895999));
#178992=CARTESIAN_POINT('Ctrl Pts',(-25.7916170646537,-64.6076916526716,
79.5218014400891));
#178993=CARTESIAN_POINT('Ctrl Pts',(-25.809620682919,-64.2104203022293,
78.8424351649142));
#178994=CARTESIAN_POINT('Ctrl Pts',(-25.8418020885287,-63.618477832722,
77.5621262871115));
#178995=CARTESIAN_POINT('Ctrl Pts',(-25.8561163156436,-63.39990155571,76.9752736162829));
#178996=CARTESIAN_POINT('Ctrl Pts',(-25.8872534907432,-63.0380126342955,
75.7167863358488));
#178997=CARTESIAN_POINT('Ctrl Pts',(-25.9037721467167,-62.90435365929,75.044592911145));
#178998=CARTESIAN_POINT('Ctrl Pts',(-25.9320569832916,-62.7698421458036,
73.8545538722555));
#178999=CARTESIAN_POINT('Ctrl Pts',(-25.9439699925019,-62.7443072703597,
73.3412239802087));
#179000=CARTESIAN_POINT('Ctrl Pts',(-25.9680623120508,-62.7581191997014,
72.290953294684));
#179001=CARTESIAN_POINT('Ctrl Pts',(-25.9802029416912,-62.8004656078051,
71.7551487466587));
#179002=CARTESIAN_POINT('Ctrl Pts',(-26.000468032645,-62.9271055662463,
70.8853903304224));
#179003=CARTESIAN_POINT('Ctrl Pts',(-26.0084922369397,-62.9905403262234,
70.5491432531566));
#179004=CARTESIAN_POINT('Ctrl Pts',(-26.0327745664289,-63.2214967218882,
69.5553156321724));
#179005=CARTESIAN_POINT('Ctrl Pts',(-26.049142455272,-63.4296399047608,
68.9085279613618));
#179006=CARTESIAN_POINT('Ctrl Pts',(-26.0834613211641,-63.9882104728269,
67.5663054442032));
#179007=CARTESIAN_POINT('Ctrl Pts',(-26.1011950016354,-64.3534908965555,
66.8802249112739));
#179008=CARTESIAN_POINT('Ctrl Pts',(-26.1320399875461,-65.0989947316727,
65.7525420202517));
#179009=CARTESIAN_POINT('Ctrl Pts',(-26.1452507437363,-65.4503359376599,
65.2948302855941));
#179010=CARTESIAN_POINT('Ctrl Pts',(-26.1753704984884,-66.291534849655,
64.345749168081));
#179011=CARTESIAN_POINT('Ctrl Pts',(-26.192087918669,-66.793519764977,63.8677636821244));
#179012=CARTESIAN_POINT('Ctrl Pts',(-26.2268747712751,-67.9416175685551,
62.9464624790629));
#179013=CARTESIAN_POINT('Ctrl Pts',(-26.2447362273283,-68.5953162098822,
62.5174453487033));
#179014=CARTESIAN_POINT('Ctrl Pts',(-26.2756540367117,-69.7939413535712,
61.8852841361851));
#179015=CARTESIAN_POINT('Ctrl Pts',(-26.2888085887831,-70.3207606495648,
61.6532016257698));
#179016=CARTESIAN_POINT('Ctrl Pts',(-26.3190274266875,-71.5196809184391,
61.2229117616047));
#179017=CARTESIAN_POINT('Ctrl Pts',(-26.3359215262308,-72.1964195521106,
61.0435639041846));
#179018=CARTESIAN_POINT('Ctrl Pts',(-26.3694131377418,-73.5916853380126,
60.7989647952253));
#179019=CARTESIAN_POINT('Ctrl Pts',(-26.3859184135928,-74.308144060643,
60.737401243949));
#179020=CARTESIAN_POINT('Ctrl Pts',(-26.4177109943786,-75.7011732196679,
60.74034258804));
#179021=CARTESIAN_POINT('Ctrl Pts',(-26.4330985926661,-76.3751929350857,
60.7976060342426));
#179022=CARTESIAN_POINT('Ctrl Pts',(-26.4739857884841,-78.0711900623219,
61.0841949041665));
#179023=CARTESIAN_POINT('Ctrl Pts',(-26.499155897536,-79.0748638313095,
61.3893405302288));
#179024=CARTESIAN_POINT('Ctrl Pts',(-26.5394465847165,-80.6642260670412,
62.1046601011297));
#179025=CARTESIAN_POINT('Ctrl Pts',(-26.5551632226687,-81.2751974850627,
62.4450859704565));
#179026=CARTESIAN_POINT('Ctrl Pts',(-26.5845939189603,-82.3329564432275,
63.1591176833735));
#179027=CARTESIAN_POINT('Ctrl Pts',(-26.5983844180817,-82.7885729031909,
63.5160458859849));
#179028=CARTESIAN_POINT('Ctrl Pts',(-26.6309376155602,-83.7962167385299,
64.4274379540744));
#179029=CARTESIAN_POINT('Ctrl Pts',(-26.6494754220358,-84.3237927191043,
65.0052310096576));
#179030=CARTESIAN_POINT('Ctrl Pts',(-26.6835644303542,-85.2094407324633,
66.183687610807));
#179031=CARTESIAN_POINT('Ctrl Pts',(-26.6991835020518,-85.578253887105,
66.7724605973377));
#179032=CARTESIAN_POINT('Ctrl Pts',(-26.728358804406,-86.1570107765461,
67.898555466131));
#179033=CARTESIAN_POINT('Ctrl Pts',(-26.7419965753708,-86.3827231780006,
68.4255602597646));
#179034=CARTESIAN_POINT('Ctrl Pts',(-26.7742953617395,-86.8253937694119,
69.698908141503));
#179035=CARTESIAN_POINT('Ctrl Pts',(-26.792737966348,-87.0099148213698,
70.4539550779531));
#179036=CARTESIAN_POINT('Ctrl Pts',(-26.8263963701106,-87.2196775732373,
71.8925271405078));
#179037=CARTESIAN_POINT('Ctrl Pts',(-26.8416957334958,-87.2616311961265,
72.5706493668111));
#179038=CARTESIAN_POINT('Ctrl Pts',(-26.865152075445,-87.2399848251452,
73.5908530747913));
#179039=CARTESIAN_POINT('Ctrl Pts',(-26.8731285530494,-87.2183955747265,
73.9324971277993));
#179040=CARTESIAN_POINT('Ctrl Pts',(-26.8939927214038,-87.1262474567226,
74.8068612893775));
#179041=CARTESIAN_POINT('Ctrl Pts',(-26.9069422471566,-87.0349037508062,
75.3366528393326));
#179042=CARTESIAN_POINT('Ctrl Pts',(-26.93196383896,-86.788878395629,76.3575912142807));
#179043=CARTESIAN_POINT('Ctrl Pts',(-26.9440254854739,-86.6374386802978,
76.8484017458814));
#179044=CARTESIAN_POINT('Ctrl Pts',(-26.9717302316517,-86.2133448243849,
77.9679803642727));
#179045=CARTESIAN_POINT('Ctrl Pts',(-26.9871511958356,-85.9178672455006,
78.5862652773435));
#179046=CARTESIAN_POINT('Ctrl Pts',(-27.0172921810689,-85.256137022201,
79.7168904651298));
#179047=CARTESIAN_POINT('Ctrl Pts',(-27.0322121883741,-84.8990045324361,
80.2320943767446));
#179048=CARTESIAN_POINT('Ctrl Pts',(-27.0660250866552,-84.0086008696503,
81.3270148059124));
#179049=CARTESIAN_POINT('Ctrl Pts',(-27.0846480988713,-83.4556732047195,
81.8872515112947));
#179050=CARTESIAN_POINT('Ctrl Pts',(-27.119190643886,-82.3079336282323,
82.8459094481337));
#179051=CARTESIAN_POINT('Ctrl Pts',(-27.1351593915688,-81.7243938372151,
83.2528678063521));
#179052=CARTESIAN_POINT('Ctrl Pts',(-27.1628513724901,-80.6857202366822,
83.8504475038963));
#179053=CARTESIAN_POINT('Ctrl Pts',(-27.1744665975531,-80.2483714077816,
84.0683946597144));
#179054=CARTESIAN_POINT('Ctrl Pts',(-27.1970593913043,-79.3803882386793,
84.4379898624859));
#179055=CARTESIAN_POINT('Ctrl Pts',(-27.2079733236429,-78.9519631274399,
84.5928410494816));
#179056=CARTESIAN_POINT('Ctrl Pts',(-27.2375213755929,-77.7561380936208,
84.9511335733451));
#179057=CARTESIAN_POINT('Ctrl Pts',(-27.2557103241722,-76.976045372927,
85.1044514415865));
#179058=CARTESIAN_POINT('Ctrl Pts',(-27.2828493769064,-75.7921208368098,
85.219676211267));
#179059=CARTESIAN_POINT('Ctrl Pts',(-27.2918765948632,-75.396117741022,
85.23888938658));
#179060=CARTESIAN_POINT('Ctrl Pts',(-27.3010916068384,-75.,85.23888938658));
#179061=CARTESIAN_POINT('Origin',(-30.2175364832709,-75.,72.98888938658));
#179062=CARTESIAN_POINT('',(-28.5675339373409,-75.,85.23888938658));
#179063=CARTESIAN_POINT('',(-28.4332364523223,-75.,85.23888938658));
#179064=CARTESIAN_POINT('',(-30.2175364832709,-75.,85.23888938658));
#179065=CARTESIAN_POINT('',(-28.5670923992068,-69.49428841446,83.9313521779249));
#179066=CARTESIAN_POINT('Origin',(-28.5675339373409,-75.,72.98888938658));
#179067=CARTESIAN_POINT('Ctrl Pts',(-28.566799738496,-69.4940652583272,
83.9317949705847));
#179068=CARTESIAN_POINT('Ctrl Pts',(-28.5535796202282,-70.005706592258,
84.1892278593307));
#179069=CARTESIAN_POINT('Ctrl Pts',(-28.5405678519628,-70.5347700727441,
84.4104595782057));
#179070=CARTESIAN_POINT('Ctrl Pts',(-28.51473175451,-71.5927852950562,84.7680829344784));
#179071=CARTESIAN_POINT('Ctrl Pts',(-28.5017910892112,-72.1192331851877,
84.9077683006098));
#179072=CARTESIAN_POINT('Ctrl Pts',(-28.470017451143,-73.4269369811265,
85.163019254198));
#179073=CARTESIAN_POINT('Ctrl Pts',(-28.4514197440086,-74.2128528894147,
85.23888938658));
#179074=CARTESIAN_POINT('Ctrl Pts',(-28.4332364523223,-75.,85.23888938658));
#179075=CARTESIAN_POINT('Origin',(-30.2175364832709,-75.,72.98888938658));
#179076=CARTESIAN_POINT('',(-18.5675364832709,-75.,83.48888938658));
#179077=CARTESIAN_POINT('Origin',(-18.5675364832709,-75.,72.98888938658));
#179078=CARTESIAN_POINT('',(-16.5675364832709,-75.,83.48888938658));
#179079=CARTESIAN_POINT('',(-30.2175364832709,-75.,83.48888938658));
#179080=CARTESIAN_POINT('Origin',(-16.5675364832709,-75.,72.98888938658));
#179081=CARTESIAN_POINT('Origin',(-30.2175364832709,-75.,72.98888938658));
#179082=CARTESIAN_POINT('Ctrl Pts',(-28.4332364523223,-75.,85.23888938658));
#179083=CARTESIAN_POINT('Ctrl Pts',(-28.4272749810172,-75.2580696055256,
85.23888938658));
#179084=CARTESIAN_POINT('Ctrl Pts',(-28.4213453695568,-75.5162712590094,
85.2307343195952));
#179085=CARTESIAN_POINT('Ctrl Pts',(-28.4026862752731,-76.3283138333888,
85.1793092241826));
#179086=CARTESIAN_POINT('Ctrl Pts',(-28.3900005365992,-76.8793747916195,
85.1065915246954));
#179087=CARTESIAN_POINT('Ctrl Pts',(-28.3491296333933,-78.5779602068471,
84.7637573617779));
#179088=CARTESIAN_POINT('Ctrl Pts',(-28.3208970388223,-79.6927227764566,
84.3655227681864));
#179089=CARTESIAN_POINT('Ctrl Pts',(-28.2744393479831,-81.4747447009042,
83.4217145281043));
#179090=CARTESIAN_POINT('Ctrl Pts',(-28.2554501218592,-82.173743561816,
82.9540069009287));
#179091=CARTESIAN_POINT('Ctrl Pts',(-28.2169591966351,-83.4227685312124,
81.9182643494961));
#179092=CARTESIAN_POINT('Ctrl Pts',(-28.1981684404363,-83.9766830848617,
81.3612219855413));
#179093=CARTESIAN_POINT('Ctrl Pts',(-28.1616294311375,-84.9677267939973,
80.1523011524452));
#179094=CARTESIAN_POINT('Ctrl Pts',(-28.1439543387338,-85.4032183457479,
79.5037253200245));
#179095=CARTESIAN_POINT('Ctrl Pts',(-28.0882170797589,-86.5530413354272,
77.3785389502528));
#179096=CARTESIAN_POINT('Ctrl Pts',(-28.0486855424314,-87.035562094923,
75.7972772695498));
#179097=CARTESIAN_POINT('Ctrl Pts',(-27.998198245963,-87.2474686468745,
73.6060036740201));
#179098=CARTESIAN_POINT('Ctrl Pts',(-27.9852995732751,-87.2628958114621,
73.040908905797));
#179099=CARTESIAN_POINT('Ctrl Pts',(-27.9587146846565,-87.2157892732353,
71.9151151062079));
#179100=CARTESIAN_POINT('Ctrl Pts',(-27.9452213168172,-87.1536564102775,
71.3557522412607));
#179101=CARTESIAN_POINT('Ctrl Pts',(-27.9050939422032,-86.8517950145408,
69.6915179473661));
#179102=CARTESIAN_POINT('Ctrl Pts',(-27.8795411041813,-86.4975874087982,
68.6135998182178));
#179103=CARTESIAN_POINT('Ctrl Pts',(-27.8157427364997,-85.2837240160056,
66.1358619373885));
#179104=CARTESIAN_POINT('Ctrl Pts',(-27.7764672100201,-84.2817137597337,
64.8299194705179));
#179105=CARTESIAN_POINT('Ctrl Pts',(-27.7276820821519,-82.6784090297572,
63.431042310556));
#179106=CARTESIAN_POINT('Ctrl Pts',(-27.7162937230107,-82.2836321193268,
63.1268860837599));
#179107=CARTESIAN_POINT('Ctrl Pts',(-27.6857189744081,-81.2079789892142,
62.3980554752025));
#179108=CARTESIAN_POINT('Ctrl Pts',(-27.6664002680147,-80.5020014417848,
62.0147029161449));
#179109=CARTESIAN_POINT('Ctrl Pts',(-27.6273286349464,-78.9703639805918,
61.3682125268237));
#179110=CARTESIAN_POINT('Ctrl Pts',(-27.6077835078353,-78.1439873633118,
61.1179476012971));
#179111=CARTESIAN_POINT('Ctrl Pts',(-27.5502213684917,-75.690197005108,
60.6492701197406));
#179112=CARTESIAN_POINT('Ctrl Pts',(-27.510645118691,-74.0368111988532,
60.6675726774708));
#179113=CARTESIAN_POINT('Ctrl Pts',(-27.4593017697274,-71.8481262791416,
61.1360586866364));
#179114=CARTESIAN_POINT('Ctrl Pts',(-27.4455805910103,-71.2703427396734,
61.3049875462795));
#179115=CARTESIAN_POINT('Ctrl Pts',(-27.4042205380546,-69.6303259528372,
61.9185992688622));
#179116=CARTESIAN_POINT('Ctrl Pts',(-27.3766829939313,-68.6154260667505,
62.4711877981453));
#179117=CARTESIAN_POINT('Ctrl Pts',(-27.3306180247818,-67.0111323361636,
63.6635883552323));
#179118=CARTESIAN_POINT('Ctrl Pts',(-27.3114076338505,-66.3842576528396,
64.2394760263411));
#179119=CARTESIAN_POINT('Ctrl Pts',(-27.2666836146926,-65.1357009236572,
65.6518763485546));
#179120=CARTESIAN_POINT('Ctrl Pts',(-27.24195292677,-64.5506753257449,66.5121738831155));
#179121=CARTESIAN_POINT('Ctrl Pts',(-27.1972850869737,-63.6734096968681,
68.2371433892422));
#179122=CARTESIAN_POINT('Ctrl Pts',(-27.1769847565348,-63.3553270152619,
69.0809060502111));
#179123=CARTESIAN_POINT('Ctrl Pts',(-27.1369967096557,-62.9376635275748,
70.7129777021864));
#179124=CARTESIAN_POINT('Ctrl Pts',(-27.1181738246321,-62.8165549489823,
71.4910816820737));
#179125=CARTESIAN_POINT('Ctrl Pts',(-27.0815337674522,-62.7251842422228,
73.0571920400057));
#179126=CARTESIAN_POINT('Ctrl Pts',(-27.0637927592737,-62.7546442134893,
73.8415443202785));
#179127=CARTESIAN_POINT('Ctrl Pts',(-27.028524546933,-62.9577265860212,
75.3553303872461));
#179128=CARTESIAN_POINT('Ctrl Pts',(-27.0106861812567,-63.12369765144,76.0823979324076));
#179129=CARTESIAN_POINT('Ctrl Pts',(-26.9560904443609,-63.8360013351941,
78.2647375314558));
#179130=CARTESIAN_POINT('Ctrl Pts',(-26.9218022723306,-64.5932062142825,
79.6347969650691));
#179131=CARTESIAN_POINT('Ctrl Pts',(-26.8715478842229,-65.9470774062663,
81.2608741455193));
#179132=CARTESIAN_POINT('Ctrl Pts',(-26.858025490544,-66.3378175049943,
81.6691969574909));
#179133=CARTESIAN_POINT('Ctrl Pts',(-26.8233349394715,-67.424632085759,
82.6581833311752));
#179134=CARTESIAN_POINT('Ctrl Pts',(-26.8027190063633,-68.1593760086047,
83.1912081901998));
#179135=CARTESIAN_POINT('Ctrl Pts',(-26.7536317685482,-70.0151012546684,
84.2461241961342));
#179136=CARTESIAN_POINT('Ctrl Pts',(-26.7238224525624,-71.1695179694699,
84.6893982956736));
#179137=CARTESIAN_POINT('Ctrl Pts',(-26.676815145295,-73.1354002991896,
85.1214536861418));
#179138=CARTESIAN_POINT('Ctrl Pts',(-26.6590742007676,-73.9146647134644,
85.2158222533607));
#179139=CARTESIAN_POINT('Ctrl Pts',(-26.6386599166736,-74.7983961283731,
85.2376454334862));
#179140=CARTESIAN_POINT('Ctrl Pts',(-26.6363248807794,-74.899208394946,
85.23888938658));
#179141=CARTESIAN_POINT('Ctrl Pts',(-26.6339799854461,-75.,85.23888938658));
#179142=CARTESIAN_POINT('',(-28.2015531594526,-74.9999810209094,60.7388893865947));
#179143=CARTESIAN_POINT('Ctrl Pts',(-27.3010916068384,-75.,85.23888938658));
#179144=CARTESIAN_POINT('Ctrl Pts',(-27.305824079875,-74.796569279156,85.23888938658));
#179145=CARTESIAN_POINT('Ctrl Pts',(-27.3106166974195,-74.5931085679724,
85.2338219878376));
#179146=CARTESIAN_POINT('Ctrl Pts',(-27.3284384471618,-73.8432844854502,
85.1964254653508));
#179147=CARTESIAN_POINT('Ctrl Pts',(-27.3416352450666,-73.2992036660809,
85.1325800364409));
#179148=CARTESIAN_POINT('Ctrl Pts',(-27.3663355732002,-72.2793557765799,
84.9430020041002));
#179149=CARTESIAN_POINT('Ctrl Pts',(-27.3778535281864,-71.803301281166,
84.8245912456166));
#179150=CARTESIAN_POINT('Ctrl Pts',(-27.4049057657027,-70.6883464213871,
84.4750671390777));
#179151=CARTESIAN_POINT('Ctrl Pts',(-27.4202067577981,-70.0590493170962,
84.2187440789919));
#179152=CARTESIAN_POINT('Ctrl Pts',(-27.4436576488854,-69.1493981606462,
83.7568893364926));
#179153=CARTESIAN_POINT('Ctrl Pts',(-27.4516265373343,-68.8511998500405,
83.5894374249849));
#179154=CARTESIAN_POINT('Ctrl Pts',(-27.4724757847193,-68.1038032722249,
83.1275803988205));
#179155=CARTESIAN_POINT('Ctrl Pts',(-27.4854181878823,-67.6662498040756,
82.8157248435304));
#179156=CARTESIAN_POINT('Ctrl Pts',(-27.5104501434681,-66.8526039734047,
82.1511201466782));
#179157=CARTESIAN_POINT('Ctrl Pts',(-27.5225285306441,-66.4754907525204,
81.8013399821767));
#179158=CARTESIAN_POINT('Ctrl Pts',(-27.5502539247456,-65.6500072137001,
80.9329664608923));
#179159=CARTESIAN_POINT('Ctrl Pts',(-27.5656791229289,-65.2209437995513,
80.3983953344034));
#179160=CARTESIAN_POINT('Ctrl Pts',(-27.5957935746758,-64.4899240356691,
79.3127252958504));
#179161=CARTESIAN_POINT('Ctrl Pts',(-27.6106797998656,-64.1812230031144,
78.7687359234635));
#179162=CARTESIAN_POINT('Ctrl Pts',(-27.6444527628368,-63.5811713203051,
77.4932371811879));
#179163=CARTESIAN_POINT('Ctrl Pts',(-27.6630708869892,-63.316038462461,
76.7523815074266));
#179164=CARTESIAN_POINT('Ctrl Pts',(-27.6975854290323,-62.9498407995109,
75.3038255052403));
#179165=CARTESIAN_POINT('Ctrl Pts',(-27.7135322676883,-62.8360710496892,
74.6026073933139));
#179166=CARTESIAN_POINT('Ctrl Pts',(-27.7412936953252,-62.7471464229716,
73.404366222219));
#179167=CARTESIAN_POINT('Ctrl Pts',(-27.7530105228034,-62.7403494745055,
72.9114909306455));
#179168=CARTESIAN_POINT('Ctrl Pts',(-27.7757173040353,-62.784414674497,
71.9643874888223));
#179169=CARTESIAN_POINT('Ctrl Pts',(-27.7866415926275,-62.8309722130037,
71.5107501260004));
#179170=CARTESIAN_POINT('Ctrl Pts',(-27.8157863163464,-63.024804177098,
70.2946245194572));
#179171=CARTESIAN_POINT('Ctrl Pts',(-27.8335928030878,-63.2194193437323,
69.5418161954899));
#179172=CARTESIAN_POINT('Ctrl Pts',(-27.8653577822833,-63.6940768218159,
68.2329906182506));
#179173=CARTESIAN_POINT('Ctrl Pts',(-27.8794342347984,-63.9476674362967,
67.6702035356999));
#179174=CARTESIAN_POINT('Ctrl Pts',(-27.9071511898918,-64.5061430050634,
66.6449859021958));
#179175=CARTESIAN_POINT('Ctrl Pts',(-27.9204412958119,-64.8020938015374,
66.1794211021552));
#179176=CARTESIAN_POINT('Ctrl Pts',(-27.9450383556779,-65.4138928553907,
65.3467986623169));
#179177=CARTESIAN_POINT('Ctrl Pts',(-27.9563686515075,-65.7221002081431,
64.9754267364466));
#179178=CARTESIAN_POINT('Ctrl Pts',(-27.9832040188346,-66.5135494043126,
64.128831251076));
#179179=CARTESIAN_POINT('Ctrl Pts',(-27.998471703676,-67.0158708779765,
63.6736250058297));
#179180=CARTESIAN_POINT('Ctrl Pts',(-28.0307468331084,-68.1309914402376,
62.8198807146967));
#179181=CARTESIAN_POINT('Ctrl Pts',(-28.0481682387343,-68.7470322616654,
62.4298951177045));
#179182=CARTESIAN_POINT('Ctrl Pts',(-28.0837083826578,-70.0670980213893,
61.7504714027153));
#179183=CARTESIAN_POINT('Ctrl Pts',(-28.1015536528359,-70.770857774297,
61.4671731473188));
#179184=CARTESIAN_POINT('Ctrl Pts',(-28.1322886314172,-72.0496074031833,
61.085479821206));
#179185=CARTESIAN_POINT('Ctrl Pts',(-28.1453419850708,-72.6139403548083,
60.959646209966));
#179186=CARTESIAN_POINT('Ctrl Pts',(-28.1642049393277,-73.4257058037411,
60.8380326655313));
#179187=CARTESIAN_POINT('Ctrl Pts',(-28.1698402086512,-73.667394819608,
60.8091568487183));
#179188=CARTESIAN_POINT('Ctrl Pts',(-28.1841216233844,-74.2722848219316,
60.7551088154341));
#179189=CARTESIAN_POINT('Ctrl Pts',(-28.1928337586347,-74.6360383204453,
60.738889950456));
#179190=CARTESIAN_POINT('Ctrl Pts',(-28.2015531594526,-74.9999810209095,
60.7388893865947));
#179191=CARTESIAN_POINT('',(-28.5675342178229,-86.7327262929796,69.46672519));
#179192=CARTESIAN_POINT('Ctrl Pts',(-28.2015531594526,-74.9999810209094,
60.7388893865947));
#179193=CARTESIAN_POINT('Ctrl Pts',(-28.2115085777165,-75.4155143680877,
60.7388887428033));
#179194=CARTESIAN_POINT('Ctrl Pts',(-28.2214581486582,-75.8307807951183,
60.7600311204054));
#179195=CARTESIAN_POINT('Ctrl Pts',(-28.2563764973937,-77.2985729646583,
60.9098820884177));
#179196=CARTESIAN_POINT('Ctrl Pts',(-28.2802056089585,-78.3345430940372,
61.1539135737514));
#179197=CARTESIAN_POINT('Ctrl Pts',(-28.3161178277994,-79.7947420362231,
61.7051026614067));
#179198=CARTESIAN_POINT('Ctrl Pts',(-28.3279543485361,-80.2520597013501,
61.9105662236378));
#179199=CARTESIAN_POINT('Ctrl Pts',(-28.3551888069236,-81.2597771872479,
62.4397707987469));
#179200=CARTESIAN_POINT('Ctrl Pts',(-28.3704805414799,-81.8000694228291,
62.7796884624179));
#179201=CARTESIAN_POINT('Ctrl Pts',(-28.4005460677347,-82.8274228573546,
63.543917669771));
#179202=CARTESIAN_POINT('Ctrl Pts',(-28.4152665757593,-83.3123674267628,
63.9677699594752));
#179203=CARTESIAN_POINT('Ctrl Pts',(-28.4443880543649,-84.2043832438057,
64.8806906223373));
#179204=CARTESIAN_POINT('Ctrl Pts',(-28.458867085717,-84.6111720028112,
65.3672798388122));
#179205=CARTESIAN_POINT('Ctrl Pts',(-28.4987753663392,-85.5849460603147,
66.7347398350442));
#179206=CARTESIAN_POINT('Ctrl Pts',(-28.5239637024403,-86.0798870006963,
67.6605065258182));
#179207=CARTESIAN_POINT('Ctrl Pts',(-28.554878072722,-86.5549068914363,
68.9106765416828));
#179208=CARTESIAN_POINT('Ctrl Pts',(-28.5615651320878,-86.648794391744,
69.1871419701532));
#179209=CARTESIAN_POINT('Ctrl Pts',(-28.568231723297,-86.7327175810979,
69.4666971484707));
#179210=CARTESIAN_POINT('Origin',(-28.5675339373409,-75.,72.98888938658));
#179211=CARTESIAN_POINT('Origin',(-23.90845228375,-75.0031087425464,72.9873550812444));
#179212=CARTESIAN_POINT('Ctrl Pts',(-19.9173382169355,-75.0031141882852,
59.938705268027));
#179213=CARTESIAN_POINT('Ctrl Pts',(-19.9328718779449,-75.715458030901,
59.9387055653175));
#179214=CARTESIAN_POINT('Ctrl Pts',(-19.9485771854427,-76.4265935451757,
59.9970363718849));
#179215=CARTESIAN_POINT('Ctrl Pts',(-19.9794959376743,-77.8228375541618,
60.2276392928315));
#179216=CARTESIAN_POINT('Ctrl Pts',(-19.9946414269002,-78.5058787600641,
60.3980014898524));
#179217=CARTESIAN_POINT('Ctrl Pts',(-20.020231467096,-79.6151980199155,
60.7720050886729));
#179218=CARTESIAN_POINT('Ctrl Pts',(-20.0305208112033,-80.0501671806586,
60.9452065047758));
#179219=CARTESIAN_POINT('Ctrl Pts',(-20.054213345243,-81.0286408710152,
61.3971744171832));
#179220=CARTESIAN_POINT('Ctrl Pts',(-20.067452530708,-81.5637737295914,
61.6914708006862));
#179221=CARTESIAN_POINT('Ctrl Pts',(-20.1027340705551,-82.9258791914871,
62.5701115632893));
#179222=CARTESIAN_POINT('Ctrl Pts',(-20.1250778021996,-83.708848783791,
63.2149789388751));
#179223=CARTESIAN_POINT('Ctrl Pts',(-20.1617910749169,-84.8732817561689,
64.4261200658439));
#179224=CARTESIAN_POINT('Ctrl Pts',(-20.1762912027402,-85.2992739037134,
64.9434726307752));
#179225=CARTESIAN_POINT('Ctrl Pts',(-20.2096346355115,-86.1717387900149,
66.1865703941092));
#179226=CARTESIAN_POINT('Ctrl Pts',(-20.2284294933597,-86.590705502097,
66.9279345931321));
#179227=CARTESIAN_POINT('Ctrl Pts',(-20.2654139263425,-87.2765823618294,
68.4770834263672));
#179228=CARTESIAN_POINT('Ctrl Pts',(-20.2838971286937,-87.5427332229182,
69.2808047207612));
#179229=CARTESIAN_POINT('Ctrl Pts',(-20.3216439621127,-87.9198791768367,
70.9457471846908));
#179230=CARTESIAN_POINT('Ctrl Pts',(-20.3404122468529,-88.0265554601149,
71.8037332445827));
#179231=CARTESIAN_POINT('Ctrl Pts',(-20.3776586003379,-88.0683398576455,
73.4995953867203));
#179232=CARTESIAN_POINT('Ctrl Pts',(-20.3962184666146,-88.0089189581226,
74.3332937421367));
#179233=CARTESIAN_POINT('Ctrl Pts',(-20.4297101871404,-87.7558015577041,
75.8353949195096));
#179234=CARTESIAN_POINT('Ctrl Pts',(-20.4447248012191,-87.5875584191361,
76.5050437589806));
#179235=CARTESIAN_POINT('Ctrl Pts',(-20.4785976203819,-87.0971503765792,
77.9587940353662));
#179236=CARTESIAN_POINT('Ctrl Pts',(-20.4973862173595,-86.7499859099212,
78.7312154115928));
#179237=CARTESIAN_POINT('Ctrl Pts',(-20.5345168439657,-85.9099603117664,
80.2002547050643));
#179238=CARTESIAN_POINT('Ctrl Pts',(-20.5531508569545,-85.4186623477612,
80.8931484026368));
#179239=CARTESIAN_POINT('Ctrl Pts',(-20.5911521673481,-84.2980486921671,
82.1861153972118));
#179240=CARTESIAN_POINT('Ctrl Pts',(-20.6100199719696,-83.6690299106182,
82.7809710848248));
#179241=CARTESIAN_POINT('Ctrl Pts',(-20.6480352022366,-82.3046339052498,
83.8361641127842));
#179242=CARTESIAN_POINT('Ctrl Pts',(-20.6672699340158,-81.5729076168941,
84.2942852396785));
#179243=CARTESIAN_POINT('Ctrl Pts',(-20.6954072800321,-80.4284917150397,
84.8619396704294));
#179244=CARTESIAN_POINT('Ctrl Pts',(-20.7045221586876,-80.0469423802783,
85.0289613853488));
#179245=CARTESIAN_POINT('Ctrl Pts',(-20.731735648922,-78.8918403432668,
85.470052613439));
#179246=CARTESIAN_POINT('Ctrl Pts',(-20.7500010159105,-78.0997385821004,
85.6897502466688));
#179247=CARTESIAN_POINT('Ctrl Pts',(-20.7839394540462,-76.5895390569253,
85.9588632142663));
#179248=CARTESIAN_POINT('Ctrl Pts',(-20.7994854167175,-75.8777092140418,
86.0262147262174));
#179249=CARTESIAN_POINT('Ctrl Pts',(-20.8298991951288,-74.5003608331042,
86.0431939440437));
#179250=CARTESIAN_POINT('Ctrl Pts',(-20.8446904689427,-73.8371128676917,
86.0007379283836));
#179251=CARTESIAN_POINT('Ctrl Pts',(-20.8685712035894,-72.7666536364926,
85.8496943995477));
#179252=CARTESIAN_POINT('Ctrl Pts',(-20.8777014719356,-72.3563606926527,
85.7715730814768));
#179253=CARTESIAN_POINT('Ctrl Pts',(-20.9065548531477,-71.0782696750546,
85.4640440639101));
#179254=CARTESIAN_POINT('Ctrl Pts',(-20.9264586059087,-70.2299859384139,
85.1647691514107));
#179255=CARTESIAN_POINT('Ctrl Pts',(-20.9624085347492,-68.7596563066096,
84.468600318769));
#179256=CARTESIAN_POINT('Ctrl Pts',(-20.9782587817702,-68.1275196936063,
84.1015787332102));
#179257=CARTESIAN_POINT('Ctrl Pts',(-21.0071336160251,-67.0526430909996,
83.3505400372593));
#179258=CARTESIAN_POINT('Ctrl Pts',(-21.0200370278404,-66.5987049877021,
82.9859300348966));
#179259=CARTESIAN_POINT('Ctrl Pts',(-21.0492239418947,-65.6262671838517,
82.0916936008069));
#179260=CARTESIAN_POINT('Ctrl Pts',(-21.0652641583058,-65.1254637681109,
81.5457584363112));
#179261=CARTESIAN_POINT('Ctrl Pts',(-21.0948863457614,-64.3013963644586,
80.4781289460507));
#179262=CARTESIAN_POINT('Ctrl Pts',(-21.1083724510535,-63.9634103086122,
79.9704343269327));
#179263=CARTESIAN_POINT('Ctrl Pts',(-21.1381836626386,-63.2949339790157,
78.7957212388062));
#179264=CARTESIAN_POINT('Ctrl Pts',(-21.1542576021094,-62.9834791987738,
78.1202860235758));
#179265=CARTESIAN_POINT('Ctrl Pts',(-21.1860047343489,-62.4912225679133,
76.7580814372926));
#179266=CARTESIAN_POINT('Ctrl Pts',(-21.2016346300804,-62.3055693523857,
76.0757463349101));
#179267=CARTESIAN_POINT('Ctrl Pts',(-21.2333295592881,-62.0405658640461,
74.6560915237694));
#179268=CARTESIAN_POINT('Ctrl Pts',(-21.2492757946066,-61.9669310189405,
73.9202395860471));
#179269=CARTESIAN_POINT('Ctrl Pts',(-21.2746493609849,-61.9496509779779,
72.7626619893793));
#179270=CARTESIAN_POINT('Ctrl Pts',(-21.2838878379608,-61.963621017613,
72.3431459475744));
#179271=CARTESIAN_POINT('Ctrl Pts',(-21.3121226657287,-62.0680418283112,
71.0647864277703));
#179272=CARTESIAN_POINT('Ctrl Pts',(-21.3307504508386,-62.2234892052623,
70.2136295091217));
#179273=CARTESIAN_POINT('Ctrl Pts',(-21.3655718339773,-62.663661937125,
68.6816007166605));
#179274=CARTESIAN_POINT('Ctrl Pts',(-21.3817119942731,-62.9241567238436,
67.9973268503584));
#179275=CARTESIAN_POINT('Ctrl Pts',(-21.4142593504455,-63.5693474987497,
66.6538600285569));
#179276=CARTESIAN_POINT('Ctrl Pts',(-21.4306247728224,-63.9572718921026,
65.9992544828227));
#179277=CARTESIAN_POINT('Ctrl Pts',(-21.4583442250649,-64.6956589934538,
64.9697989149321));
#179278=CARTESIAN_POINT('Ctrl Pts',(-21.4695135597142,-65.0151944244029,
64.5750846690903));
#179279=CARTESIAN_POINT('Ctrl Pts',(-21.4994709654415,-65.9366671084101,
63.5635515538473));
#179280=CARTESIAN_POINT('Ctrl Pts',(-21.5179575508267,-66.577997966108,
62.9860578253547));
#179281=CARTESIAN_POINT('Ctrl Pts',(-21.5458585159931,-67.60573646322,62.2301116846202));
#179282=CARTESIAN_POINT('Ctrl Pts',(-21.5549743395996,-67.9514941991276,
62.0003566892381));
#179283=CARTESIAN_POINT('Ctrl Pts',(-21.5829649984971,-69.0472703839904,
61.3452814151252));
#179284=CARTESIAN_POINT('Ctrl Pts',(-21.6014757670978,-69.8289194391713,
60.9774568428056));
#179285=CARTESIAN_POINT('Ctrl Pts',(-21.6348096952452,-71.2682548922788,
60.4669345020941));
#179286=CARTESIAN_POINT('Ctrl Pts',(-21.6494761519027,-71.9115034436083,
60.2927878034823));
#179287=CARTESIAN_POINT('Ctrl Pts',(-21.6730783604569,-72.9745208716184,
60.0906236826485));
#179288=CARTESIAN_POINT('Ctrl Pts',(-21.6820869004331,-73.3873171477512,
60.0324306001988));
#179289=CARTESIAN_POINT('Ctrl Pts',(-21.6998459227287,-74.2016867105178,
59.957161428136));
#179290=CARTESIAN_POINT('Ctrl Pts',(-21.7085784447897,-74.6024198115221,
59.9387052680259));
#179291=CARTESIAN_POINT('Ctrl Pts',(-21.7173525905574,-75.0031087425464,
59.9387052680259));
#179292=CARTESIAN_POINT('Ctrl Pts',(-21.4178560137238,-75.0031087349823,
59.9387052680259));
#179293=CARTESIAN_POINT('Ctrl Pts',(-21.4165790214011,-74.9450765584729,
59.9387052680596));
#179294=CARTESIAN_POINT('Ctrl Pts',(-21.4153012122267,-74.8870410412435,
59.9390924039174));
#179295=CARTESIAN_POINT('Ctrl Pts',(-21.3982849488851,-74.114761740527,
59.9493975218163));
#179296=CARTESIAN_POINT('Ctrl Pts',(-21.3823795244862,-73.4025083610337,
60.0175605981627));
#179297=CARTESIAN_POINT('Ctrl Pts',(-21.3479674952683,-71.8722695165063,
60.2920289451095));
#179298=CARTESIAN_POINT('Ctrl Pts',(-21.3296902599154,-71.0613777063911,
60.519948827425));
#179299=CARTESIAN_POINT('Ctrl Pts',(-21.2919933924485,-69.4744729716801,
61.136421088153));
#179300=CARTESIAN_POINT('Ctrl Pts',(-21.2728381923279,-68.7038021304673,
61.5274600692303));
#179301=CARTESIAN_POINT('Ctrl Pts',(-21.2354813627788,-67.2705110473185,
62.4432674643334));
#179302=CARTESIAN_POINT('Ctrl Pts',(-21.2169686074118,-66.6088707468293,
62.9620066918454));
#179303=CARTESIAN_POINT('Ctrl Pts',(-21.1793329586012,-65.3823273712759,
64.1307437952212));
#179304=CARTESIAN_POINT('Ctrl Pts',(-21.1606856991897,-64.8225650507218,
64.7803135541843));
#179305=CARTESIAN_POINT('Ctrl Pts',(-21.1257642338435,-63.9114446212539,
66.0755869885543));
#179306=CARTESIAN_POINT('Ctrl Pts',(-21.1095322663368,-63.5430737896763,
66.7052261979723));
#179307=CARTESIAN_POINT('Ctrl Pts',(-21.0779527528966,-62.9262938930541,
67.9962232652629));
#179308=CARTESIAN_POINT('Ctrl Pts',(-21.0626602223071,-62.6751226930866,
68.6535785836184));
#179309=CARTESIAN_POINT('Ctrl Pts',(-21.0281203676375,-62.236057338798,
70.1563637592512));
#179310=CARTESIAN_POINT('Ctrl Pts',(-21.0089201382509,-62.0768047623284,
71.006752535638));
#179311=CARTESIAN_POINT('Ctrl Pts',(-20.9808474681184,-61.9667648876738,
72.2832005045049));
#179312=CARTESIAN_POINT('Ctrl Pts',(-20.9717060177443,-61.9508962789211,
72.7012706524723));
#179313=CARTESIAN_POINT('Ctrl Pts',(-20.9460321822843,-61.9627084972529,
73.8686767451884));
#179314=CARTESIAN_POINT('Ctrl Pts',(-20.9293704136499,-62.0348199990523,
74.6159276773357));
#179315=CARTESIAN_POINT('Ctrl Pts',(-20.8989581724167,-62.2855868778281,
75.9763025640758));
#179316=CARTESIAN_POINT('Ctrl Pts',(-20.8851892419988,-62.4457958755654,
76.590557376275));
#179317=CARTESIAN_POINT('Ctrl Pts',(-20.8550000675132,-62.8885918857284,
77.8918693461325));
#179318=CARTESIAN_POINT('Ctrl Pts',(-20.8385582738716,-63.1864282792172,
78.5714252713954));
#179319=CARTESIAN_POINT('Ctrl Pts',(-20.8068765314766,-63.8767920825402,
79.8406983324079));
#179320=CARTESIAN_POINT('Ctrl Pts',(-20.7916154146475,-64.2628204105242,
80.4311072859444));
#179321=CARTESIAN_POINT('Ctrl Pts',(-20.7598032915303,-65.1509763675334,
81.5755355948962));
#179322=CARTESIAN_POINT('Ctrl Pts',(-20.7433179736035,-65.6568374527347,
82.1234689105735));
#179323=CARTESIAN_POINT('Ctrl Pts',(-20.7130362566075,-66.6818828118141,
83.0590204971938));
#179324=CARTESIAN_POINT('Ctrl Pts',(-20.6990820858438,-67.1885491305867,
83.4570209699789));
#179325=CARTESIAN_POINT('Ctrl Pts',(-20.6683120568835,-68.3527778080183,
84.2397853814381));
#179326=CARTESIAN_POINT('Ctrl Pts',(-20.651540366393,-69.018853690199,84.6077160095614));
#179327=CARTESIAN_POINT('Ctrl Pts',(-20.6259743233929,-70.0928167066275,
85.0839993296045));
#179328=CARTESIAN_POINT('Ctrl Pts',(-20.6169658493251,-70.4803181726352,
85.2341561079651));
#179329=CARTESIAN_POINT('Ctrl Pts',(-20.5890207711908,-71.6956057981309,
85.639518631415));
#179330=CARTESIAN_POINT('Ctrl Pts',(-20.5698924184271,-72.5421199886465,
85.8310443509021));
#179331=CARTESIAN_POINT('Ctrl Pts',(-20.539134914783,-73.9442761892445,
86.0044754413283));
#179332=CARTESIAN_POINT('Ctrl Pts',(-20.5273091091971,-74.4908961418339,
86.0374197567479));
#179333=CARTESIAN_POINT('Ctrl Pts',(-20.4995210326799,-75.7648514863862,
86.0340165646542));
#179334=CARTESIAN_POINT('Ctrl Pts',(-20.4834920933317,-76.4903019509806,
85.9713405663449));
#179335=CARTESIAN_POINT('Ctrl Pts',(-20.4535479370001,-77.8431237815135,
85.7395487093813));
#179336=CARTESIAN_POINT('Ctrl Pts',(-20.4396368488468,-78.4705327621653,
85.5834299595451));
#179337=CARTESIAN_POINT('Ctrl Pts',(-20.4101052979605,-79.7569333901446,
85.1598911830048));
#179338=CARTESIAN_POINT('Ctrl Pts',(-20.3944867931946,-80.4108891481077,
84.8837995041944));
#179339=CARTESIAN_POINT('Ctrl Pts',(-20.3649983002911,-81.6094682018597,
84.2584261003021));
#179340=CARTESIAN_POINT('Ctrl Pts',(-20.3511423230588,-82.1569732220308,
83.9191094746264));
#179341=CARTESIAN_POINT('Ctrl Pts',(-20.3219006509759,-83.2417719994142,
83.1302807342162));
#179342=CARTESIAN_POINT('Ctrl Pts',(-20.306521295237,-83.7724726487,82.6751186986466));
#179343=CARTESIAN_POINT('Ctrl Pts',(-20.2767885721029,-84.7317940630188,
81.7086218141905));
#179344=CARTESIAN_POINT('Ctrl Pts',(-20.2624929320801,-85.1627526688423,
81.2025513754549));
#179345=CARTESIAN_POINT('Ctrl Pts',(-20.2330980141271,-85.9556603416621,
80.1131055038267));
#179346=CARTESIAN_POINT('Ctrl Pts',(-20.2180277182533,-86.31391656035,79.5295509346996));
#179347=CARTESIAN_POINT('Ctrl Pts',(-20.1867522576109,-86.9644172258488,
78.2553940587279));
#179348=CARTESIAN_POINT('Ctrl Pts',(-20.1706664885413,-87.2462963892034,
77.5622315936384));
#179349=CARTESIAN_POINT('Ctrl Pts',(-20.139673070264,-87.6655309470806,
76.208990273409));
#179350=CARTESIAN_POINT('Ctrl Pts',(-20.1248759571721,-87.8141821205888,
75.5548963316572));
#179351=CARTESIAN_POINT('Ctrl Pts',(-20.0917409474285,-88.0356832969413,
74.0538869219616));
#179352=CARTESIAN_POINT('Ctrl Pts',(-20.07343120113,-88.0774324955213,73.2054210066669));
#179353=CARTESIAN_POINT('Ctrl Pts',(-20.0456647480087,-88.0166106702952,
71.9440021368037));
#179354=CARTESIAN_POINT('Ctrl Pts',(-20.0364949274527,-87.9768030491948,
71.5302780244807));
#179355=CARTESIAN_POINT('Ctrl Pts',(-20.0084293209196,-87.7938052083768,
70.265274237822));
#179356=CARTESIAN_POINT('Ctrl Pts',(-19.9898157937922,-87.5858969951755,
69.4257428314119));
#179357=CARTESIAN_POINT('Ctrl Pts',(-19.9518799915304,-87.0076193181874,
67.8006083720809));
#179358=CARTESIAN_POINT('Ctrl Pts',(-19.9328676430594,-86.6387824155251,
67.0189616610644));
#179359=CARTESIAN_POINT('Ctrl Pts',(-19.9047804306668,-85.9773877236089,
65.9153979274948));
#179360=CARTESIAN_POINT('Ctrl Pts',(-19.8955052982431,-85.7415868499336,
65.562231245798));
#179361=CARTESIAN_POINT('Ctrl Pts',(-19.8716429626955,-85.0960133134504,
64.6905773924108));
#179362=CARTESIAN_POINT('Ctrl Pts',(-19.8569765233847,-84.663321493607,
64.1905640763602));
#179363=CARTESIAN_POINT('Ctrl Pts',(-19.8240096264381,-83.5979057628111,
63.1332419920548));
#179364=CARTESIAN_POINT('Ctrl Pts',(-19.8057428004871,-82.9453214349789,
62.6000867805438));
#179365=CARTESIAN_POINT('Ctrl Pts',(-19.7733639122021,-81.7270753051805,
61.7871439521476));
#179366=CARTESIAN_POINT('Ctrl Pts',(-19.759512466268,-81.183982720971,61.4785211743792));
#179367=CARTESIAN_POINT('Ctrl Pts',(-19.7353152738702,-80.1884174905541,
61.003639661926));
#179368=CARTESIAN_POINT('Ctrl Pts',(-19.7248456932155,-79.7448982524453,
60.8213247415312));
#179369=CARTESIAN_POINT('Ctrl Pts',(-19.6983318520157,-78.6076162272353,
60.4254897365281));
#179370=CARTESIAN_POINT('Ctrl Pts',(-19.6821871197268,-77.9042029224063,
60.2446481322081));
#179371=CARTESIAN_POINT('Ctrl Pts',(-19.650007434917,-76.4671189013943,
60.0004104549331));
#179372=CARTESIAN_POINT('Ctrl Pts',(-19.6340602481707,-75.7357661204461,
59.9387048126255));
#179373=CARTESIAN_POINT('Ctrl Pts',(-19.6178714446467,-75.0031006318965,
59.9387052680284));
#179374=CARTESIAN_POINT('Origin',(-29.0675369414309,-75.,72.98888938658));
#179375=CARTESIAN_POINT('',(-29.3659074908668,-88.048139596166,72.910724257937));
#179376=CARTESIAN_POINT('',(-29.0715747727696,-75.,60.2348484464093));
#179377=CARTESIAN_POINT('Ctrl Pts',(-29.3659074908668,-88.048139596166,
72.910724257937));
#179378=CARTESIAN_POINT('Ctrl Pts',(-29.3546070927136,-88.0320891389882,
72.1178290339509));
#179379=CARTESIAN_POINT('Ctrl Pts',(-29.3435513987386,-87.943946214938,
71.327216757012));
#179380=CARTESIAN_POINT('Ctrl Pts',(-29.3198744527459,-87.6154974982477,
69.7320276466834));
#179381=CARTESIAN_POINT('Ctrl Pts',(-29.307347194069,-87.3681853141254,
68.9317585165297));
#179382=CARTESIAN_POINT('Ctrl Pts',(-29.2716009614049,-86.4261070896003,
66.6770808862898));
#179383=CARTESIAN_POINT('Ctrl Pts',(-29.2493251734954,-85.5346342704723,
65.3168568070417));
#179384=CARTESIAN_POINT('Ctrl Pts',(-29.2008834203201,-83.2740044679819,
62.978809133931));
#179385=CARTESIAN_POINT('Ctrl Pts',(-29.1779340274024,-81.9179021187915,
62.0244452183611));
#179386=CARTESIAN_POINT('Ctrl Pts',(-29.1412176792203,-79.6470774108627,
61.0067126403781));
#179387=CARTESIAN_POINT('Ctrl Pts',(-29.1283139882113,-78.8387324105875,
60.7373079795366));
#179388=CARTESIAN_POINT('Ctrl Pts',(-29.1035475953469,-77.2063592530559,
60.3677278885152));
#179389=CARTESIAN_POINT('Ctrl Pts',(-29.0916996520762,-76.3859047406108,
60.2633970793085));
#179390=CARTESIAN_POINT('Ctrl Pts',(-29.0770376134035,-75.3744456229184,
60.233503939114));
#179391=CARTESIAN_POINT('Ctrl Pts',(-29.0743156629404,-75.1871357568877,
60.2321075556738));
#179392=CARTESIAN_POINT('Ctrl Pts',(-29.0715747727696,-75.,60.2348484464093));
#179393=CARTESIAN_POINT('',(-29.5675339851921,-75.,59.7388891318012));
#179394=CARTESIAN_POINT('',(-29.0675369414309,-75.,60.23888627858));
#179395=CARTESIAN_POINT('Origin',(-29.5675339847409,-75.,72.98888938658));
#179396=CARTESIAN_POINT('Ctrl Pts',(-29.0715747727696,-75.,60.2348484464093));
#179397=CARTESIAN_POINT('Ctrl Pts',(-29.0624830013418,-74.3792543948848,
60.2439402197103));
#179398=CARTESIAN_POINT('Ctrl Pts',(-29.0530879239002,-73.7604267662681,
60.298613478141));
#179399=CARTESIAN_POINT('Ctrl Pts',(-29.0196088358811,-71.5708262745697,
60.6545856066194));
#179400=CARTESIAN_POINT('Ctrl Pts',(-28.9970544073908,-70.0494382406995,
61.2063873466819));
#179401=CARTESIAN_POINT('Ctrl Pts',(-28.9605640939231,-67.9680269694554,
62.4497133389986));
#179402=CARTESIAN_POINT('Ctrl Pts',(-28.9479315721134,-67.3041712311103,
62.9401165236319));
#179403=CARTESIAN_POINT('Ctrl Pts',(-28.9236753448913,-66.0997830229611,
64.0256989173661));
#179404=CARTESIAN_POINT('Ctrl Pts',(-28.9120635621393,-65.5579519187452,
64.6158534956667));
#179405=CARTESIAN_POINT('Ctrl Pts',(-28.8757570605804,-64.0709138031728,
66.5825031309042));
#179406=CARTESIAN_POINT('Ctrl Pts',(-28.8499124305472,-63.3442409609021,
68.094175332673));
#179407=CARTESIAN_POINT('Ctrl Pts',(-28.8133913070736,-62.7300938236352,
70.4880258732612));
#179408=CARTESIAN_POINT('Ctrl Pts',(-28.8014073382016,-62.6053405970239,
71.2917639575562));
#179409=CARTESIAN_POINT('Ctrl Pts',(-28.7766246431217,-62.5156428752478,
72.9010220163151));
#179410=CARTESIAN_POINT('Ctrl Pts',(-28.7642803679076,-62.5480378309257,
73.7016986295373));
#179411=CARTESIAN_POINT('Ctrl Pts',(-28.7402659878244,-62.7645775607116,
75.2800816269133));
#179412=CARTESIAN_POINT('Ctrl Pts',(-28.7286237203234,-62.9475553373186,
76.0555728904185));
#179413=CARTESIAN_POINT('Ctrl Pts',(-28.6920185593442,-63.730299249319,
78.3547530244634));
#179414=CARTESIAN_POINT('Ctrl Pts',(-28.6664353682654,-64.5592604210176,
79.7818999885085));
#179415=CARTESIAN_POINT('Ctrl Pts',(-28.6175016536543,-66.7203052977945,
82.2305946258992));
#179416=CARTESIAN_POINT('Ctrl Pts',(-28.5917552851516,-68.0293736273903,
83.2219482748759));
#179417=CARTESIAN_POINT('Ctrl Pts',(-28.5670511147326,-69.4942820408445,
83.9313635516326));
#179418=CARTESIAN_POINT('',(-29.3655838523951,-81.601362674698,84.2438270474906));
#179419=CARTESIAN_POINT('Ctrl Pts',(-29.3655838526627,-81.6013626745626,
84.2438270472598));
#179420=CARTESIAN_POINT('Ctrl Pts',(-29.3515369276678,-81.860548904277,
84.075521599617));
#179421=CARTESIAN_POINT('Ctrl Pts',(-29.3375494753961,-82.1133189850824,
83.8983413632426));
#179422=CARTESIAN_POINT('Ctrl Pts',(-29.3235615282547,-82.3590602344623,
83.7127408512463));
#179423=CARTESIAN_POINT('Ctrl Pts',(-29.309689642279,-82.6027625130371,
83.5286803087355));
#179424=CARTESIAN_POINT('Ctrl Pts',(-29.2958172696116,-82.8395518899398,
83.3363387224601));
#179425=CARTESIAN_POINT('Ctrl Pts',(-29.281885923003,-83.0688548794704,
83.1362046562238));
#179426=CARTESIAN_POINT('Ctrl Pts',(-29.276907265287,-83.1508010925813,
83.064682567148));
#179427=CARTESIAN_POINT('Ctrl Pts',(-29.271921075776,-83.2317914308853,
82.9921656866292));
#179428=CARTESIAN_POINT('Ctrl Pts',(-29.2669246850387,-83.3118005600568,
82.9186776996054));
#179429=CARTESIAN_POINT('Ctrl Pts',(-29.253192592924,-83.5316978398292,
82.7167031423289));
#179430=CARTESIAN_POINT('Ctrl Pts',(-29.2393423955424,-83.7441786587935,
82.5073393284883));
#179431=CARTESIAN_POINT('Ctrl Pts',(-29.2254372276084,-83.9488227354,82.2911763378452));
#179432=CARTESIAN_POINT('Ctrl Pts',(-29.2113899558856,-84.155558171046,
82.0728042706827));
#179433=CARTESIAN_POINT('Ctrl Pts',(-29.1972865843269,-84.3542958316679,
81.8474936242021));
#179434=CARTESIAN_POINT('Ctrl Pts',(-29.1831922031099,-84.5446534894828,
81.6158677489123));
#179435=CARTESIAN_POINT('Ctrl Pts',(-29.1776338924619,-84.6197236170793,
81.5245229392932));
#179436=CARTESIAN_POINT('Ctrl Pts',(-29.1720769800155,-84.693491022277,
81.4321961088974));
#179437=CARTESIAN_POINT('Ctrl Pts',(-29.1665254579116,-84.7659344267727,
81.3389259770428));
#179438=CARTESIAN_POINT('Ctrl Pts',(-29.1526002959194,-84.947647860313,
81.1049718162184));
#179439=CARTESIAN_POINT('Ctrl Pts',(-29.1387540387589,-85.1210444797053,
80.8651301507358));
#179440=CARTESIAN_POINT('Ctrl Pts',(-29.1249636357172,-85.2857375273847,
80.6200008365142));
#179441=CARTESIAN_POINT('Ctrl Pts',(-29.1112138923695,-85.4499449932503,
80.3755942628011));
#179442=CARTESIAN_POINT('Ctrl Pts',(-29.097519674265,-85.6054999816377,
80.1259313935929));
#179443=CARTESIAN_POINT('Ctrl Pts',(-29.0838581339785,-85.7520621961525,
79.871635550916));
#179444=CARTESIAN_POINT('Ctrl Pts',(-29.0702192763375,-85.8983810692383,
79.6177619228867));
#179445=CARTESIAN_POINT('Ctrl Pts',(-29.0566129880928,-86.0357368606978,
79.3592709194749));
#179446=CARTESIAN_POINT('Ctrl Pts',(-29.0430165354333,-86.1638361835182,
79.0968081432393));
#179447=CARTESIAN_POINT('Ctrl Pts',(-29.0294524529149,-86.2916305302353,
78.8349702327174));
#179448=CARTESIAN_POINT('Ctrl Pts',(-29.0158981592047,-86.4102123109604,
78.5691796794727));
#179449=CARTESIAN_POINT('Ctrl Pts',(-29.0023310824778,-86.5193372434198,
78.300099265784));
#179450=CARTESIAN_POINT('Ctrl Pts',(-28.990922018484,-86.6111044945981,
78.0738194472896));
#179451=CARTESIAN_POINT('Ctrl Pts',(-28.9795039146485,-86.6961848660042,
77.8452135701712));
#179452=CARTESIAN_POINT('Ctrl Pts',(-28.968063347715,-86.7744598057493,
77.6146858321683));
#179453=CARTESIAN_POINT('Ctrl Pts',(-28.9545124222423,-86.8671735568285,
77.3416343116225));
#179454=CARTESIAN_POINT('Ctrl Pts',(-28.940872966952,-86.9503156261371,
77.0657889256945));
#179455=CARTESIAN_POINT('Ctrl Pts',(-28.9271816883291,-87.0237753974248,
76.7878423327904));
#179456=CARTESIAN_POINT('Ctrl Pts',(-28.9133962221623,-87.0977405265845,
76.5079836389328));
#179457=CARTESIAN_POINT('Ctrl Pts',(-28.8995582171853,-87.1618897070212,
76.2259950093752));
#179458=CARTESIAN_POINT('Ctrl Pts',(-28.8857051426604,-87.2161629265552,
75.9425807157966));
#179459=CARTESIAN_POINT('Ctrl Pts',(-28.8717987806009,-87.2706449146236,
75.658076234697));
#179460=CARTESIAN_POINT('Ctrl Pts',(-28.8578772328367,-87.3151748930747,
75.3721353741036));
#179461=CARTESIAN_POINT('Ctrl Pts',(-28.8439784026859,-87.3497444916918,
75.0854635881238));
#179462=CARTESIAN_POINT('Ctrl Pts',(-28.8299871301317,-87.3845440159028,
74.7968851216131));
#179463=CARTESIAN_POINT('Ctrl Pts',(-28.8160188783897,-87.4092503014884,
74.5075662463216));
#179464=CARTESIAN_POINT('Ctrl Pts',(-28.8021123121144,-87.4239066307403,
74.2182154033722));
#179465=CARTESIAN_POINT('Ctrl Pts',(-28.7906519385059,-87.4359848825266,
73.9797619491923));
#179466=CARTESIAN_POINT('Ctrl Pts',(-28.7792334578131,-87.4412388178587,
73.7412866412701));
#179467=CARTESIAN_POINT('Ctrl Pts',(-28.7678785097109,-87.4397181565358,
73.5031784169355));
#179468=CARTESIAN_POINT('Ctrl Pts',(-28.7538051587481,-87.4378334451043,
73.2080664905729));
#179469=CARTESIAN_POINT('Ctrl Pts',(-28.7397945616724,-87.425504114295,
72.913559041569));
#179470=CARTESIAN_POINT('Ctrl Pts',(-28.7257924240597,-87.4027855288179,
72.6203915837634));
#179471=CARTESIAN_POINT('Ctrl Pts',(-28.711890316212,-87.3802292424719,
72.3293184827444));
#179472=CARTESIAN_POINT('Ctrl Pts',(-28.6979965473919,-87.3474315684259,
72.0395665459303));
#179473=CARTESIAN_POINT('Ctrl Pts',(-28.6840579785028,-87.3044980173107,
71.7518582558201));
#179474=CARTESIAN_POINT('Ctrl Pts',(-28.679117116274,-87.2892791836744,
71.6498731069271));
#179475=CARTESIAN_POINT('Ctrl Pts',(-28.6741706248307,-87.2727872330889,
71.548144752287));
#179476=CARTESIAN_POINT('Ctrl Pts',(-28.6692161373386,-87.2550284427559,
71.4467053584759));
#179477=CARTESIAN_POINT('Ctrl Pts',(-28.6547265382072,-87.2030921418986,
71.1500417469918));
#179478=CARTESIAN_POINT('Ctrl Pts',(-28.6401112616259,-87.1402582756939,
70.8558425314034));
#179479=CARTESIAN_POINT('Ctrl Pts',(-28.6253112490708,-87.0667134280796,
70.5648824322376));
#179480=CARTESIAN_POINT('Ctrl Pts',(-28.6106590834898,-86.9939032678951,
70.2768289231913));
#179481=CARTESIAN_POINT('Ctrl Pts',(-28.5958258543958,-86.9105950271706,
69.9919503385699));
#179482=CARTESIAN_POINT('Ctrl Pts',(-28.5807542555651,-86.8170207690931,
69.7109948176848));
#179483=CARTESIAN_POINT('Ctrl Pts',(-28.576368234195,-86.789789504499,69.6292332917525));
#179484=CARTESIAN_POINT('Ctrl Pts',(-28.5719620257242,-86.7616891633537,
69.5478039687303));
#179485=CARTESIAN_POINT('Ctrl Pts',(-28.5675342178229,-86.7327262929796,
69.46672519));
#179486=CARTESIAN_POINT('',(-29.3666998404582,-88.0486437994879,72.9886184577035));
#179487=CARTESIAN_POINT('Ctrl Pts',(-29.3655838529309,-81.601362674698,
84.2438270474913));
#179488=CARTESIAN_POINT('Ctrl Pts',(-29.3663355387957,-82.5565513191003,
83.6844513479272));
#179489=CARTESIAN_POINT('Ctrl Pts',(-29.3681108351944,-83.4405607955859,
83.0049447002618));
#179490=CARTESIAN_POINT('Ctrl Pts',(-29.3658391655718,-85.0431672706073,
81.3984887424379));
#179491=CARTESIAN_POINT('Ctrl Pts',(-29.3646108212369,-85.7485241671463,
80.473804649592));
#179492=CARTESIAN_POINT('Ctrl Pts',(-29.3665216258898,-86.8761958843376,
78.5089048792641));
#179493=CARTESIAN_POINT('Ctrl Pts',(-29.3680011405059,-87.3057468920773,
77.4766733383828));
#179494=CARTESIAN_POINT('Ctrl Pts',(-29.3656365873995,-87.8956308654324,
75.2854002296071));
#179495=CARTESIAN_POINT('Ctrl Pts',(-29.3647732455976,-88.0472622045665,
74.1368535505306));
#179496=CARTESIAN_POINT('Ctrl Pts',(-29.3658340844142,-88.0483003098859,
72.9886310426174));
#179497=CARTESIAN_POINT('Ctrl Pts',(-29.3673261860752,-88.0488923027565,
72.9886093529381));
#179498=CARTESIAN_POINT('Ctrl Pts',(-29.3668532876724,-88.0487182780952,
72.9626462799095));
#179499=CARTESIAN_POINT('Ctrl Pts',(-29.3663803892696,-88.0484673808042,
72.9366844270783));
#179500=CARTESIAN_POINT('Ctrl Pts',(-29.3659074908668,-88.048139596166,
72.910724257937));
#179501=CARTESIAN_POINT('Origin',(-28.5675364832709,-75.,72.98888938658));
#179502=CARTESIAN_POINT('',(-27.5675364826718,-60.4999999999999,66.2250147575798));
#179503=CARTESIAN_POINT('',(-27.5675364826401,-60.5,79.7527640156553));
#179504=CARTESIAN_POINT('Ctrl Pts',(-27.5675364817658,-60.5,66.2250147580311));
#179505=CARTESIAN_POINT('Ctrl Pts',(-30.4269114864225,-60.5,72.9888893867033));
#179506=CARTESIAN_POINT('Ctrl Pts',(-27.5675364816388,-60.5,79.7527640154292));
#179507=CARTESIAN_POINT('',(-27.5675364826398,-61.8923127432075,63.8134583462433));
#179508=CARTESIAN_POINT('Origin',(-27.5675364832709,-75.,72.98888938658));
#179509=CARTESIAN_POINT('',(-27.5675364826717,-73.6076872567268,57.0495837172059));
#179510=CARTESIAN_POINT('Ctrl Pts',(-27.5675364817724,-73.6076872563213,
57.0495837174391));
#179511=CARTESIAN_POINT('Ctrl Pts',(-30.4269114864031,-67.7499999999193,
60.4315210317516));
#179512=CARTESIAN_POINT('Ctrl Pts',(-27.5675364816771,-61.8923127434824,
63.8134583460842));
#179513=CARTESIAN_POINT('',(-27.5675364826717,-76.3923127432731,57.0495837172059));
#179514=CARTESIAN_POINT('Origin',(-27.5675364832709,-75.,72.98888938658));
#179515=CARTESIAN_POINT('',(-27.5675364826398,-88.1076872567925,63.8134583462433));
#179516=CARTESIAN_POINT('Ctrl Pts',(-27.567536481677,-88.1076872565176,
63.8134583460842));
#179517=CARTESIAN_POINT('Ctrl Pts',(-30.426911486403,-82.2500000000807,
60.4315210317516));
#179518=CARTESIAN_POINT('Ctrl Pts',(-27.5675364817723,-76.3923127436787,
57.0495837174391));
#179519=CARTESIAN_POINT('',(-27.5675364826718,-89.5000000000001,66.2250147575798));
#179520=CARTESIAN_POINT('Origin',(-27.5675364832709,-75.,72.98888938658));
#179521=CARTESIAN_POINT('',(-27.5675364826718,-89.5,79.7527640155803));
#179522=CARTESIAN_POINT('Ctrl Pts',(-27.5675364817657,-89.5,66.2250147580311));
#179523=CARTESIAN_POINT('Ctrl Pts',(-30.4269114864094,-89.5,72.9888893866725));
#179524=CARTESIAN_POINT('Ctrl Pts',(-27.5675364816705,-89.5,79.7527640153542));
#179525=CARTESIAN_POINT('',(-27.5675364826398,-88.1076872567925,82.1643204269167));
#179526=CARTESIAN_POINT('Origin',(-27.5675364832709,-75.,72.98888938658));
#179527=CARTESIAN_POINT('',(-27.5675364826717,-76.3923127432731,88.9281950559541));
#179528=CARTESIAN_POINT('Ctrl Pts',(-27.5675364817723,-76.3923127436786,
88.9281950557209));
#179529=CARTESIAN_POINT('Ctrl Pts',(-30.426911486403,-82.2500000000806,
85.5462577414084));
#179530=CARTESIAN_POINT('Ctrl Pts',(-27.5675364816771,-88.1076872565176,
82.1643204270758));
#179531=CARTESIAN_POINT('',(-27.5675364816388,-75.,88.9888893864172));
#179532=CARTESIAN_POINT('Origin',(-27.5675364832709,-75.,72.98888938658));
#179533=CARTESIAN_POINT('',(-29.5675364841684,-75.,86.9888893874774));
#179534=CARTESIAN_POINT('',(-28.5675364832709,-75.,87.98888938658));
#179535=CARTESIAN_POINT('Origin',(-29.5675364832709,-75.,72.98888938658));
#179536=CARTESIAN_POINT('',(-27.5675364826399,-73.6076872567918,88.9281950559917));
#179537=CARTESIAN_POINT('Origin',(-27.5675364832709,-75.,72.98888938658));
#179538=CARTESIAN_POINT('',(-27.5675364826716,-61.8923127432725,82.1643204269542));
#179539=CARTESIAN_POINT('Ctrl Pts',(-27.5675364817723,-61.8923127436775,
82.1643204271884));
#179540=CARTESIAN_POINT('Ctrl Pts',(-30.426911486403,-67.7500000000795,
85.5462577415009));
#179541=CARTESIAN_POINT('Ctrl Pts',(-27.5675364816771,-73.6076872565163,
88.9281950558335));
#179542=CARTESIAN_POINT('Origin',(-27.5675364832709,-75.,72.98888938658));
#179543=CARTESIAN_POINT('Origin',(-17.5675364832709,-75.,72.98888938658));
#179544=CARTESIAN_POINT('',(-18.5675364839018,-60.5,66.2250147575047));
#179545=CARTESIAN_POINT('',(-18.56753648387,-60.5,79.7527640155803));
#179546=CARTESIAN_POINT('Ctrl Pts',(-18.5675364848006,-60.5,79.7527640151869));
#179547=CARTESIAN_POINT('Ctrl Pts',(-15.708161480161,-60.5,72.9888893866029));
#179548=CARTESIAN_POINT('Ctrl Pts',(-18.5675364847769,-60.5,66.225014758029));
#179549=CARTESIAN_POINT('',(-18.5675364838598,-61.8923127432938,82.1643204269666));
#179550=CARTESIAN_POINT('Origin',(-18.5675364832709,-75.,72.98888938658));
#179551=CARTESIAN_POINT('',(-18.567536483878,-73.6076872567433,88.9281950559637));
#179552=CARTESIAN_POINT('Ctrl Pts',(-18.5675364847385,-61.8923127437411,
82.1643204272252));
#179553=CARTESIAN_POINT('Ctrl Pts',(-15.7081614801807,-67.7500000000459,
85.5462577414815));
#179554=CARTESIAN_POINT('Ctrl Pts',(-18.5675364847937,-73.6076872563709,
88.9281950557496));
#179555=CARTESIAN_POINT('',(-18.567536483878,-76.3923127432567,88.9281950559637));
#179556=CARTESIAN_POINT('Origin',(-18.5675364832709,-75.,72.98888938658));
#179557=CARTESIAN_POINT('',(-18.5675364838598,-88.1076872567062,82.1643204269666));
#179558=CARTESIAN_POINT('Ctrl Pts',(-18.5675364847937,-76.392312743629,
88.9281950557496));
#179559=CARTESIAN_POINT('Ctrl Pts',(-15.7081614801807,-82.2499999999541,
85.5462577414815));
#179560=CARTESIAN_POINT('Ctrl Pts',(-18.5675364847385,-88.1076872562589,
82.1643204272251));
#179561=CARTESIAN_POINT('',(-18.56753648387,-89.5,79.7527640155802));
#179562=CARTESIAN_POINT('Origin',(-18.5675364832709,-75.,72.98888938658));
#179563=CARTESIAN_POINT('',(-18.5675364839017,-89.5,66.2250147575048));
#179564=CARTESIAN_POINT('Ctrl Pts',(-18.5675364848006,-89.5,79.7527640151868));
#179565=CARTESIAN_POINT('Ctrl Pts',(-15.7081614801611,-89.5,72.9888893866029));
#179566=CARTESIAN_POINT('Ctrl Pts',(-18.5675364847769,-89.5,66.2250147580291));
#179567=CARTESIAN_POINT('',(-18.5675364838598,-88.1076872567063,63.8134583461935));
#179568=CARTESIAN_POINT('Origin',(-18.5675364832709,-75.,72.98888938658));
#179569=CARTESIAN_POINT('',(-18.5675364838782,-76.3923127432566,57.0495837171963));
#179570=CARTESIAN_POINT('Ctrl Pts',(-18.5675364847385,-88.107687256259,
63.8134583459349));
#179571=CARTESIAN_POINT('Ctrl Pts',(-15.7081614801806,-82.249999999954,
60.4315210316784));
#179572=CARTESIAN_POINT('Ctrl Pts',(-18.5675364847938,-76.3923127436288,
57.0495837174103));
#179573=CARTESIAN_POINT('',(-18.5675364848006,-75.,56.9888893868452));
#179574=CARTESIAN_POINT('Origin',(-18.5675364832709,-75.,72.98888938658));
#179575=CARTESIAN_POINT('',(-16.5675364823734,-75.,58.9888893856825));
#179576=CARTESIAN_POINT('',(-17.5675364832709,-75.,57.98888938658));
#179577=CARTESIAN_POINT('Origin',(-16.5675364832709,-75.,72.98888938658));
#179578=CARTESIAN_POINT('',(-18.5675364838598,-73.6076872567056,57.0495837172181));
#179579=CARTESIAN_POINT('Origin',(-18.5675364832709,-75.,72.98888938658));
#179580=CARTESIAN_POINT('',(-18.5675364838783,-61.892312743256,63.8134583462153));
#179581=CARTESIAN_POINT('Ctrl Pts',(-18.5675364847385,-73.6076872562579,
57.0495837174757));
#179582=CARTESIAN_POINT('Ctrl Pts',(-15.7081614801806,-67.7499999999529,
60.4315210317322));
#179583=CARTESIAN_POINT('Ctrl Pts',(-18.5675364847938,-61.8923127436277,
63.8134583460004));
#179584=CARTESIAN_POINT('Origin',(-18.5675364832709,-75.,72.98888938658));
#179585=CARTESIAN_POINT('Origin',(-31.5405364832709,-75.,72.98888938658));
#179586=CARTESIAN_POINT('',(-27.5675364832709,-73.60768725693,57.04958371709));
#179587=CARTESIAN_POINT('',(-27.5675364832709,-76.39231274307,57.04958371709));
#179588=CARTESIAN_POINT('Origin',(-16.5675364832709,-75.,89.73204719308));
#179589=CARTESIAN_POINT('',(-27.5675364832709,-73.60768725693,88.92819505607));
#179590=CARTESIAN_POINT('',(-27.5675364832709,-61.89231274307,82.164320426837));
#179591=CARTESIAN_POINT('Origin',(-16.5675364832709,-75.,56.24573158008));
#179592=CARTESIAN_POINT('',(-27.5675364832709,-88.10768725693,63.813458346323));
#179593=CARTESIAN_POINT('Origin',(-16.5675364832709,-60.5,64.61731048333));
#179594=CARTESIAN_POINT('',(-27.5675364832709,-61.89231274307,63.813458346323));
#179595=CARTESIAN_POINT('Origin',(-31.5405364832709,-75.,72.98888938658));
#179596=CARTESIAN_POINT('',(-27.5675364832709,-89.5,66.225014757346));
#179597=CARTESIAN_POINT('Origin',(-31.5405364832709,-75.,72.98888938658));
#179598=CARTESIAN_POINT('',(-27.5675364832709,-60.5,66.225014757346));
#179599=CARTESIAN_POINT('Origin',(-16.5675364832709,-60.5,81.36046828983));
#179600=CARTESIAN_POINT('',(-27.5675364832709,-60.5,79.752764015814));
#179601=CARTESIAN_POINT('Origin',(-16.5675364832709,-89.5,81.36046828983));
#179602=CARTESIAN_POINT('',(-27.5675364832709,-88.10768725693,82.164320426837));
#179603=CARTESIAN_POINT('',(-27.5675364832709,-76.39231274307,88.92819505607));
#179604=CARTESIAN_POINT('Origin',(-31.5405364832709,-75.,72.98888938658));
#179605=CARTESIAN_POINT('Origin',(-31.5405364832709,-75.,72.98888938658));
#179606=CARTESIAN_POINT('',(-27.5675364832709,-89.5,79.752764015814));
#179607=CARTESIAN_POINT('Origin',(-31.5405364832709,-75.,72.98888938658));
#179608=CARTESIAN_POINT('Origin',(-16.5675364832709,-89.5,64.61731048333));
#179609=CARTESIAN_POINT('Origin',(-29.5675364832709,-75.,72.98888938658));
#179610=CARTESIAN_POINT('Ctrl Pts',(-29.4235335827009,-87.55585084311,76.731819067654));
#179611=CARTESIAN_POINT('Ctrl Pts',(-29.3785752787509,-88.14324409162,74.761378091484));
#179612=CARTESIAN_POINT('Ctrl Pts',(-29.2886586708509,-88.3725131074,70.540717962258));
#179613=CARTESIAN_POINT('Ctrl Pts',(-29.1537837590009,-85.80712443056,64.740945094149));
#179614=CARTESIAN_POINT('Ctrl Pts',(-29.0189088471409,-80.89008803912,60.73624495104));
#179615=CARTESIAN_POINT('Ctrl Pts',(-28.8840339352909,-74.691455216807,
59.3974994093));
#179616=CARTESIAN_POINT('Ctrl Pts',(-28.7491590234309,-68.559950359161,
61.01614190121));
#179617=CARTESIAN_POINT('Ctrl Pts',(-28.6142841115809,-63.82974243489,65.239934789744));
#179618=CARTESIAN_POINT('Ctrl Pts',(-28.4794091997309,-61.53007762407,71.14982987547));
#179619=CARTESIAN_POINT('Ctrl Pts',(-28.3445342878709,-62.1613422859,77.459886586808));
#179620=CARTESIAN_POINT('Ctrl Pts',(-28.2096593760209,-65.586178918236,
82.797096210383));
#179621=CARTESIAN_POINT('Ctrl Pts',(-28.0747844641709,-71.059375111067,
86.00013159165));
#179622=CARTESIAN_POINT('Ctrl Pts',(-27.9399095523109,-77.390014473847,
86.37204219574));
#179623=CARTESIAN_POINT('Ctrl Pts',(-27.8050346404609,-83.200609009059,
83.83190373521));
#179624=CARTESIAN_POINT('Ctrl Pts',(-27.6701597286009,-87.22682761174,78.932426619492));
#179625=CARTESIAN_POINT('Ctrl Pts',(-27.5352848167509,-88.59260271637,72.7396913102611));
#179626=CARTESIAN_POINT('Ctrl Pts',(-27.4004099049009,-87.00075441549,66.601179175152));
#179627=CARTESIAN_POINT('Ctrl Pts',(-27.2655349930409,-82.797654032634,
61.8525731252));
#179628=CARTESIAN_POINT('Ctrl Pts',(-27.1306600811909,-76.897856957019,
59.52712548816));
#179629=CARTESIAN_POINT('Ctrl Pts',(-26.9957851693409,-70.585103932253,
60.13083195176));
#179630=CARTESIAN_POINT('Ctrl Pts',(-26.8609102574809,-65.232991059679,
63.532331627755));
#179631=CARTESIAN_POINT('Ctrl Pts',(-26.7260353456309,-62.00608811552,68.991489954176));
#179632=CARTESIAN_POINT('Ctrl Pts',(-26.5911604337809,-61.60653904254,75.320445064586));
#179633=CARTESIAN_POINT('Ctrl Pts',(-26.4562855219229,-64.12128199053,81.142075432836));
#179634=CARTESIAN_POINT('Ctrl Pts',(-26.3214106100699,-69.003132368767,
85.18964866916));
#179635=CARTESIAN_POINT('Ctrl Pts',(-26.1865356982159,-75.1898451699075,
86.58245060783));
#179636=CARTESIAN_POINT('Ctrl Pts',(-26.0516607863629,-81.33524931199,85.01742067074));
#179637=CARTESIAN_POINT('Ctrl Pts',(-25.9167858745089,-86.10216283013,80.835094323236));
#179638=CARTESIAN_POINT('Ctrl Pts',(-25.7819109626559,-88.45334768832,74.945508333151));
#179639=CARTESIAN_POINT('Ctrl Pts',(-25.6470360508029,-87.87721613395,68.630175581195));
#179640=CARTESIAN_POINT('Ctrl Pts',(-25.5121611389499,-84.499098730494,
63.263275982751));
#179641=CARTESIAN_POINT('Ctrl Pts',(-25.3772862270959,-79.054155289863,
60.01251283554));
#179642=CARTESIAN_POINT('Ctrl Pts',(-25.2424113152429,-72.726732877904,
59.58553507798));
#179643=CARTESIAN_POINT('Ctrl Pts',(-25.1524947073409,-68.839040027706,
61.24456506882));
#179644=CARTESIAN_POINT('Ctrl Pts',(-25.1075364033899,-67.188343111843,
62.4704803028));
#179645=CARTESIAN_POINT('Ctrl Pts',(-29.5803515522709,-87.26716059124,76.645759801271));
#179646=CARTESIAN_POINT('Ctrl Pts',(-29.5353932483209,-87.84104820744,74.720624165918));
#179647=CARTESIAN_POINT('Ctrl Pts',(-29.4454766404109,-88.06504575808,70.597007514748));
#179648=CARTESIAN_POINT('Ctrl Pts',(-29.3106017285609,-85.55864175003,64.930585855648));
#179649=CARTESIAN_POINT('Ctrl Pts',(-29.1757268167109,-80.754660259608,
61.01796373317));
#179650=CARTESIAN_POINT('Ctrl Pts',(-29.0408519048509,-74.698549429079,
59.70999928245));
#179651=CARTESIAN_POINT('Ctrl Pts',(-28.9059769930009,-68.708023124285,
61.29142515603));
#179652=CARTESIAN_POINT('Ctrl Pts',(-28.7711020811409,-64.08657444972,65.418102536579));
#179653=CARTESIAN_POINT('Ctrl Pts',(-28.6362271692909,-61.83978465483,71.192114429511));
#179654=CARTESIAN_POINT('Ctrl Pts',(-28.5013522574409,-62.4565349714,77.357087236615));
#179655=CARTESIAN_POINT('Ctrl Pts',(-28.3664773455809,-65.802626088017,
82.571581131104));
#179656=CARTESIAN_POINT('Ctrl Pts',(-28.2316024337309,-71.149979882179,
85.70097075929));
#179657=CARTESIAN_POINT('Ctrl Pts',(-28.0967275218809,-77.335062094356,
86.06433021321));
#179658=CARTESIAN_POINT('Ctrl Pts',(-27.9618526100209,-83.012056603505,
83.58259585616));
#179659=CARTESIAN_POINT('Ctrl Pts',(-27.8269776981709,-86.94570242263,78.795769910022));
#179660=CARTESIAN_POINT('Ctrl Pts',(-27.6921027863109,-88.28007495933,72.7454209940753));
#179661=CARTESIAN_POINT('Ctrl Pts',(-27.5572278744609,-86.72482721166,66.748048526563));
#179662=CARTESIAN_POINT('Ctrl Pts',(-27.4223529626109,-82.618366564596,
62.108624745));
#179663=CARTESIAN_POINT('Ctrl Pts',(-27.2874780507509,-76.854220503396,
59.83664493523));
#179664=CARTESIAN_POINT('Ctrl Pts',(-27.1526031389009,-70.68661337782,60.42647068511));
#179665=CARTESIAN_POINT('Ctrl Pts',(-27.0177282270509,-65.457558897109,
63.749761420078));
#179666=CARTESIAN_POINT('Ctrl Pts',(-26.8828533151909,-62.30485048069,69.083400113308));
#179667=CARTESIAN_POINT('Ctrl Pts',(-26.7479784033409,-61.91448803505,75.266836798267));
#179668=CARTESIAN_POINT('Ctrl Pts',(-26.6131034914909,-64.37141078558,80.954613399192));
#179669=CARTESIAN_POINT('Ctrl Pts',(-26.4782285796339,-69.141015276789,
84.90912285579));
#179670=CARTESIAN_POINT('Ctrl Pts',(-26.3433536677799,-75.1854801570906,
86.26990081237));
#179671=CARTESIAN_POINT('Ctrl Pts',(-26.2084787559269,-81.189586167187,
84.74085480758));
#179672=CARTESIAN_POINT('Ctrl Pts',(-26.0736038440729,-85.84689648269,80.654690549114));
#179673=CARTESIAN_POINT('Ctrl Pts',(-25.9387289322199,-88.14402175087,74.900520795182));
#179674=CARTESIAN_POINT('Ctrl Pts',(-25.8038540203669,-87.58113689443,68.730393256763));
#179675=CARTESIAN_POINT('Ctrl Pts',(-25.6689791085129,-84.280690815386,
63.486892033801));
#179676=CARTESIAN_POINT('Ctrl Pts',(-25.5341041966599,-78.960940172354,
60.31087201977));
#179677=CARTESIAN_POINT('Ctrl Pts',(-25.3992292848069,-72.779000945297,
59.89371154324));
#179678=CARTESIAN_POINT('Ctrl Pts',(-25.3093126769049,-68.980695826933,
61.51459630666));
#179679=CARTESIAN_POINT('Ctrl Pts',(-25.2643543729539,-67.367952540366,
62.71232469914));
#179680=CARTESIAN_POINT('Ctrl Pts',(-29.7371695218309,-86.97847033937,76.559700534901));
#179681=CARTESIAN_POINT('Ctrl Pts',(-29.6922112178809,-87.53885232326,74.679870240367));
#179682=CARTESIAN_POINT('Ctrl Pts',(-29.6022946099809,-87.75757840877,70.653297067253));
#179683=CARTESIAN_POINT('Ctrl Pts',(-29.4674196981209,-85.31015906951,65.120226617163));
#179684=CARTESIAN_POINT('Ctrl Pts',(-29.3325447862709,-80.619232480115,
61.29968251531));
#179685=CARTESIAN_POINT('Ctrl Pts',(-29.1976698744209,-74.7056436413761,
60.02249915561));
#179686=CARTESIAN_POINT('Ctrl Pts',(-29.0627949625609,-68.856095889434,
61.56670841083));
#179687=CARTESIAN_POINT('Ctrl Pts',(-28.9279200507109,-64.34340646456,65.596270283389));
#179688=CARTESIAN_POINT('Ctrl Pts',(-28.7930451388509,-62.1494916856,71.23439898352));
#179689=CARTESIAN_POINT('Ctrl Pts',(-28.6581702270009,-62.75172765689,77.254287886388));
#179690=CARTESIAN_POINT('Ctrl Pts',(-28.5232953151509,-66.01907325777,82.346066051798));
#179691=CARTESIAN_POINT('Ctrl Pts',(-28.3884204032909,-71.240584653253,
85.40180992691));
#179692=CARTESIAN_POINT('Ctrl Pts',(-28.2535454914409,-77.280109714823,
85.75661823069));
#179693=CARTESIAN_POINT('Ctrl Pts',(-28.1186705795909,-82.823504197914,
83.33328797713));
#179694=CARTESIAN_POINT('Ctrl Pts',(-27.9837956677309,-86.66457723349,78.659113200594));
#179695=CARTESIAN_POINT('Ctrl Pts',(-27.8489207558809,-87.96754720229,72.7511506779378));
#179696=CARTESIAN_POINT('Ctrl Pts',(-27.7140458440209,-86.44890000785,66.894917878018));
#179697=CARTESIAN_POINT('Ctrl Pts',(-27.5791709321709,-82.439079096599,
62.36467636483));
#179698=CARTESIAN_POINT('Ctrl Pts',(-27.4442960203209,-76.810584049825,
60.1461643823));
#179699=CARTESIAN_POINT('Ctrl Pts',(-27.3094211084609,-70.788122823435,
60.72210941845));
#179700=CARTESIAN_POINT('Ctrl Pts',(-27.1745461966109,-65.682126734574,
63.967191212364));
#179701=CARTESIAN_POINT('Ctrl Pts',(-27.0396712847609,-62.60361284588,69.175310272392));
#179702=CARTESIAN_POINT('Ctrl Pts',(-26.9047963729009,-62.22243702755,75.213228531899));
#179703=CARTESIAN_POINT('Ctrl Pts',(-26.7699214610509,-64.6215395806,80.767151365512));
#179704=CARTESIAN_POINT('Ctrl Pts',(-26.6350465492009,-69.27889818477,84.62859704241));
#179705=CARTESIAN_POINT('Ctrl Pts',(-26.5001716373439,-75.1811151442317,
85.95735101692));
#179706=CARTESIAN_POINT('Ctrl Pts',(-26.3652967254909,-81.043923022351,
84.46428894445));
#179707=CARTESIAN_POINT('Ctrl Pts',(-26.2304218136369,-85.59163013523,80.47428677502));
#179708=CARTESIAN_POINT('Ctrl Pts',(-26.0955469017839,-87.83469581341,74.855533257242));
#179709=CARTESIAN_POINT('Ctrl Pts',(-25.9606719899309,-87.28505765493,68.830610932353));
#179710=CARTESIAN_POINT('Ctrl Pts',(-25.8257970780769,-84.062282900292,
63.710508084863));
#179711=CARTESIAN_POINT('Ctrl Pts',(-25.6909221662239,-78.867725054857,
60.609231204));
#179712=CARTESIAN_POINT('Ctrl Pts',(-25.5560472543709,-72.831269012692,
60.20188800851));
#179713=CARTESIAN_POINT('Ctrl Pts',(-25.4661306464689,-69.122351626158,
61.7846275445));
#179714=CARTESIAN_POINT('Ctrl Pts',(-25.4211723425179,-67.547561968885,
62.95416909548));
#179715=CARTESIAN_POINT('Ctrl Pts',(-29.8939874914009,-86.6897800875,76.473641268518));
#179716=CARTESIAN_POINT('Ctrl Pts',(-29.8490291874409,-87.23665643908,74.639116314802));
#179717=CARTESIAN_POINT('Ctrl Pts',(-29.7591125795409,-87.45011105946,70.709586619743));
#179718=CARTESIAN_POINT('Ctrl Pts',(-29.6242376676909,-85.06167638898,65.309867378662));
#179719=CARTESIAN_POINT('Ctrl Pts',(-29.4893627558309,-80.483804700603,
61.58140129744));
#179720=CARTESIAN_POINT('Ctrl Pts',(-29.3544878439809,-74.7127378536479,
60.33499902876));
#179721=CARTESIAN_POINT('Ctrl Pts',(-29.2196129321309,-69.004168654558,
61.84199166565));
#179722=CARTESIAN_POINT('Ctrl Pts',(-29.0847380202709,-64.60023847939,65.774438030224));
#179723=CARTESIAN_POINT('Ctrl Pts',(-28.9498631084209,-62.45919871637,71.276683537561));
#179724=CARTESIAN_POINT('Ctrl Pts',(-28.8149881965709,-63.04692034239,77.151488536196));
#179725=CARTESIAN_POINT('Ctrl Pts',(-28.6801132847109,-66.235520427551,
82.120550972519));
#179726=CARTESIAN_POINT('Ctrl Pts',(-28.5452383728609,-71.331189424365,
85.10264909454));
#179727=CARTESIAN_POINT('Ctrl Pts',(-28.4103634610009,-77.225157335332,
85.44890624816));
#179728=CARTESIAN_POINT('Ctrl Pts',(-28.2754885491509,-82.634951792361,
83.08398009808));
#179729=CARTESIAN_POINT('Ctrl Pts',(-28.1406136373009,-86.38345204438,78.522456491124));
#179730=CARTESIAN_POINT('Ctrl Pts',(-28.0057387254409,-87.65501944525,72.7568803617516));
#179731=CARTESIAN_POINT('Ctrl Pts',(-27.8708638135909,-86.17297280402,67.041787229428));
#179732=CARTESIAN_POINT('Ctrl Pts',(-27.7359889017409,-82.259791628561,
62.62072798463));
#179733=CARTESIAN_POINT('Ctrl Pts',(-27.6011139898809,-76.766947596202,
60.45568382937));
#179734=CARTESIAN_POINT('Ctrl Pts',(-27.4662390780309,-70.889632269001,
61.0177481518));
#179735=CARTESIAN_POINT('Ctrl Pts',(-27.3313641661709,-65.906694572004,
64.184621004688));
#179736=CARTESIAN_POINT('Ctrl Pts',(-27.1964892543209,-62.90237521105,69.267220431524));
#179737=CARTESIAN_POINT('Ctrl Pts',(-27.0616143424709,-62.53038602006,75.159620265581));
#179738=CARTESIAN_POINT('Ctrl Pts',(-26.9267394306109,-64.87166837565,80.579689331869));
#179739=CARTESIAN_POINT('Ctrl Pts',(-26.7918645187609,-69.416781092793,
84.34807122905));
#179740=CARTESIAN_POINT('Ctrl Pts',(-26.6569896069109,-75.1767501314152,
85.64480122147));
#179741=CARTESIAN_POINT('Ctrl Pts',(-26.5221146950539,-80.898259877549,
84.18772308129));
#179742=CARTESIAN_POINT('Ctrl Pts',(-26.3872397832009,-85.3363637878,80.293883000897));
#179743=CARTESIAN_POINT('Ctrl Pts',(-26.2523648713479,-87.52536987595,74.810545719273));
#179744=CARTESIAN_POINT('Ctrl Pts',(-26.1174899594939,-86.98897841541,68.93082860792));
#179745=CARTESIAN_POINT('Ctrl Pts',(-25.9826150476409,-83.843874985184,
63.934124135913));
#179746=CARTESIAN_POINT('Ctrl Pts',(-25.8477401357879,-78.774509937348,
60.90759038823));
#179747=CARTESIAN_POINT('Ctrl Pts',(-25.7128652239349,-72.883537080085,
60.51006447377));
#179748=CARTESIAN_POINT('Ctrl Pts',(-25.6229486160329,-69.264007425385,
62.05465878235));
#179749=CARTESIAN_POINT('Ctrl Pts',(-25.5779903120819,-67.727171397409,
63.196013491817));
#179750=CARTESIAN_POINT('Ctrl Pts',(-29.3659074908668,-88.0481395961661,
72.910724257937));
#179751=CARTESIAN_POINT('Ctrl Pts',(-29.3564982338821,-88.0460045428066,
72.4863077063651));
#179752=CARTESIAN_POINT('Ctrl Pts',(-29.3471083831415,-88.0232803767141,
72.061989631977));
#179753=CARTESIAN_POINT('Ctrl Pts',(-29.3281064149641,-87.934573512206,
71.2015622468502));
#179754=CARTESIAN_POINT('Ctrl Pts',(-29.3185886995406,-87.8671769059716,
70.7675430526915));
#179755=CARTESIAN_POINT('Ctrl Pts',(-29.2896717560233,-87.5960608923731,
69.4669196523705));
#179756=CARTESIAN_POINT('Ctrl Pts',(-29.2702173424168,-87.3252271347852,
68.6164798142884));
#179757=CARTESIAN_POINT('Ctrl Pts',(-29.2253010143824,-86.5131076515063,
66.742024930945));
#179758=CARTESIAN_POINT('Ctrl Pts',(-29.1996910935634,-85.9137974945729,
65.7401241308678));
#179759=CARTESIAN_POINT('Ctrl Pts',(-29.1554746269511,-84.6578977939495,
64.1717373950071));
#179760=CARTESIAN_POINT('Ctrl Pts',(-29.1369985236878,-84.0611558696511,
63.5616725854627));
#179761=CARTESIAN_POINT('Ctrl Pts',(-29.0982964749951,-82.7026349825422,
62.4171369804774));
#179762=CARTESIAN_POINT('Ctrl Pts',(-29.0780486887075,-81.9304516311765,
61.8944315877894));
#179763=CARTESIAN_POINT('Ctrl Pts',(-29.0439061828359,-80.5727347676091,
61.1728735765531));
#179764=CARTESIAN_POINT('Ctrl Pts',(-29.0302053743383,-80.0156938632889,
60.9255547302426));
#179765=CARTESIAN_POINT('Ctrl Pts',(-29.0050768977302,-78.9391594068913,
60.537100991496));
#179766=CARTESIAN_POINT('Ctrl Pts',(-28.9935432067017,-78.4270849802294,
60.3872937961839));
#179767=CARTESIAN_POINT('Ctrl Pts',(-28.9678777664002,-77.2694113129645,
60.1235667201636));
#179768=CARTESIAN_POINT('Ctrl Pts',(-28.9537517745064,-76.6200096747148,
60.0257507510677));
#179769=CARTESIAN_POINT('Ctrl Pts',(-28.9272328280987,-75.4132633020343,
59.93509232377));
#179770=CARTESIAN_POINT('Ctrl Pts',(-28.9148503310648,-74.8568225856496,
59.9285568053376));
#179771=CARTESIAN_POINT('Ctrl Pts',(-28.8942428497637,-73.9467752421308,
59.9765772975495));
#179772=CARTESIAN_POINT('Ctrl Pts',(-28.8862407188741,-73.5930365781412,
60.0099924734182));
#179773=CARTESIAN_POINT('Ctrl Pts',(-28.8628376106062,-72.5429562198852,
60.1535934566403));
#179774=CARTESIAN_POINT('Ctrl Pts',(-28.8477724295467,-71.8538171714245,
60.3060433724034));
#179775=CARTESIAN_POINT('Ctrl Pts',(-28.8184383628547,-70.5459349980751,
60.7072179776806));
#179776=CARTESIAN_POINT('Ctrl Pts',(-28.8041619638653,-69.9252544251782,
60.9501893074854));
#179777=CARTESIAN_POINT('Ctrl Pts',(-28.7788113746183,-68.8929646488808,
61.4474152891473));
#179778=CARTESIAN_POINT('Ctrl Pts',(-28.767835471829,-68.4708619183447,
61.6801004622464));
#179779=CARTESIAN_POINT('Ctrl Pts',(-28.7507664251534,-67.8354245741352,
62.0782315790565));
#179780=CARTESIAN_POINT('Ctrl Pts',(-28.7446895251965,-67.6123225281541,
62.2279161008187));
#179781=CARTESIAN_POINT('Ctrl Pts',(-28.7305582988274,-67.0953388264515,
62.5990202479308));
#179782=CARTESIAN_POINT('Ctrl Pts',(-28.7225808515193,-66.8062336479153,
62.8259709421714));
#179783=CARTESIAN_POINT('Ctrl Pts',(-28.7013578651677,-66.0558928438563,
63.4680002526907));
#179784=CARTESIAN_POINT('Ctrl Pts',(-28.6882686874363,-65.6133280976073,
63.9049486073402));
#179785=CARTESIAN_POINT('Ctrl Pts',(-28.6666858385585,-64.9489264935309,
64.6603239558346));
#179786=CARTESIAN_POINT('Ctrl Pts',(-28.6583249823005,-64.7068801937676,
64.9611121847821));
#179787=CARTESIAN_POINT('Ctrl Pts',(-28.6410882123786,-64.2464948877883,
65.5877306343096));
#179788=CARTESIAN_POINT('Ctrl Pts',(-28.6321488163013,-64.0285887231609,
65.9138981003384));
#179789=CARTESIAN_POINT('Ctrl Pts',(-28.6167537023254,-63.680887421671,
66.4890168565324));
#179790=CARTESIAN_POINT('Ctrl Pts',(-28.610328827005,-63.5436822219399,
66.7334806652167));
#179791=CARTESIAN_POINT('Ctrl Pts',(-28.5984854221818,-63.3019585873584,
67.1993026659102));
#179792=CARTESIAN_POINT('Ctrl Pts',(-28.5930704079703,-63.1957781442392,
67.419153535765));
#179793=CARTESIAN_POINT('Ctrl Pts',(-28.576222129306,-62.8802537249818,
68.1228949558838));
#179794=CARTESIAN_POINT('Ctrl Pts',(-28.5650682955872,-62.6941578388861,
68.6170188276551));
#179795=CARTESIAN_POINT('Ctrl Pts',(-28.545793745091,-62.4247797613169,
69.4876004126718));
#179796=CARTESIAN_POINT('Ctrl Pts',(-28.5376684957557,-62.3272961663442,
69.8596880564267));
#179797=CARTESIAN_POINT('Ctrl Pts',(-28.523233234306,-62.1855983227819,
70.5161434091827));
#179798=CARTESIAN_POINT('Ctrl Pts',(-28.5169819108951,-62.1341452449762,
70.7989808731062));
#179799=CARTESIAN_POINT('Ctrl Pts',(-28.4996699074065,-62.0197648406076,
71.5701861668623));
#179800=CARTESIAN_POINT('Ctrl Pts',(-28.4882982896073,-61.9748410256592,
72.0612406787676));
#179801=CARTESIAN_POINT('Ctrl Pts',(-28.471322229869,-61.9493875669456,
72.8005829324056));
#179802=CARTESIAN_POINT('Ctrl Pts',(-28.465664165641,-61.9479446733414,
73.0481500053425));
#179803=CARTESIAN_POINT('Ctrl Pts',(-28.4551716019025,-61.9587112129092,
73.5141902924898));
#179804=CARTESIAN_POINT('Ctrl Pts',(-28.4503395173441,-61.9693462642277,
73.7321878396621));
#179805=CARTESIAN_POINT('Ctrl Pts',(-28.4334128965999,-62.0269819057531,
74.5067571199237));
#179806=CARTESIAN_POINT('Ctrl Pts',(-28.4217088175756,-62.1046530214977,
75.0606813516689));
#179807=CARTESIAN_POINT('Ctrl Pts',(-28.4001844763301,-62.3107848251598,
76.0622387749575));
#179808=CARTESIAN_POINT('Ctrl Pts',(-28.3903752305105,-62.4285150974339,
76.5121139327343));
#179809=CARTESIAN_POINT('Ctrl Pts',(-28.3753344049142,-62.6379884110952,
77.1690374466618));
#179810=CARTESIAN_POINT('Ctrl Pts',(-28.3703383053425,-62.7118876037204,
77.3818208990407));
#179811=CARTESIAN_POINT('Ctrl Pts',(-28.3539567178157,-62.9679285208451,
78.0622418099726));
#179812=CARTESIAN_POINT('Ctrl Pts',(-28.3423086960805,-63.171521881072,
78.5218357355849));
#179813=CARTESIAN_POINT('Ctrl Pts',(-28.3257320578495,-63.5029030303266,
79.1662560371414));
#179814=CARTESIAN_POINT('Ctrl Pts',(-28.3206683556837,-63.6099001836908,
79.361775026428));
#179815=CARTESIAN_POINT('Ctrl Pts',(-28.311078153775,-63.8253072023904,
79.7321578643301));
#179816=CARTESIAN_POINT('Ctrl Pts',(-28.3065585803607,-63.9327431373142,
79.9070518827553));
#179817=CARTESIAN_POINT('Ctrl Pts',(-28.2903497084108,-64.3393885356207,
80.5346700381858));
#179818=CARTESIAN_POINT('Ctrl Pts',(-28.2790534863171,-64.6630411220953,
80.9710469608496));
#179819=CARTESIAN_POINT('Ctrl Pts',(-28.2617405540121,-65.1944127705644,
81.601837070945));
#179820=CARTESIAN_POINT('Ctrl Pts',(-28.2557863532672,-65.3834042483339,
81.8120284013624));
#179821=CARTESIAN_POINT('Ctrl Pts',(-28.2449075332595,-65.7347911648844,
82.1784473992999));
#179822=CARTESIAN_POINT('Ctrl Pts',(-28.2400168919111,-65.8948037059415,
82.3369738580753));
#179823=CARTESIAN_POINT('Ctrl Pts',(-28.2223958775441,-66.4743186188951,
82.8824448042067));
#179824=CARTESIAN_POINT('Ctrl Pts',(-28.2092075889706,-66.9152856827901,
83.2466708682746));
#179825=CARTESIAN_POINT('Ctrl Pts',(-28.1898112960037,-67.6013903950775,
83.7415470281434));
#179826=CARTESIAN_POINT('Ctrl Pts',(-28.1835238641599,-67.8297555272949,
83.8955205339695));
#179827=CARTESIAN_POINT('Ctrl Pts',(-28.1724260254509,-68.2475777068703,
84.1581830724215));
#179828=CARTESIAN_POINT('Ctrl Pts',(-28.1675783567341,-68.4353760998163,
84.2696982570266));
#179829=CARTESIAN_POINT('Ctrl Pts',(-28.149958700384,-69.1415449055238,
84.664823071593));
#179830=CARTESIAN_POINT('Ctrl Pts',(-28.1377313668127,-69.6768672641444,
84.9174692290254));
#179831=CARTESIAN_POINT('Ctrl Pts',(-28.1201770297299,-70.455680847885,
85.2226728581861));
#179832=CARTESIAN_POINT('Ctrl Pts',(-28.1149880895017,-70.6871188022322,
85.3059418428659));
#179833=CARTESIAN_POINT('Ctrl Pts',(-28.1050279728183,-71.1281712184913,
85.4508261624183));
#179834=CARTESIAN_POINT('Ctrl Pts',(-28.1002660044092,-71.3373373300875,
85.5138227899195));
#179835=CARTESIAN_POINT('Ctrl Pts',(-28.0843589237699,-72.0294388552241,
85.7036742906909));
#179836=CARTESIAN_POINT('Ctrl Pts',(-28.0729223312909,-72.5184809261174,
85.8084453254484));
#179837=CARTESIAN_POINT('Ctrl Pts',(-28.050883270265,-73.4700006659628,
85.9561309750036));
#179838=CARTESIAN_POINT('Ctrl Pts',(-28.0402809736981,-73.9319196816796,
86.0029343223826));
#179839=CARTESIAN_POINT('Ctrl Pts',(-28.0252281645065,-74.609077915433,
86.0347769534915));
#179840=CARTESIAN_POINT('Ctrl Pts',(-28.0205423787538,-74.8232630500173,
86.0394917038328));
#179841=CARTESIAN_POINT('Ctrl Pts',(-28.0070172334021,-75.4524680389126,
86.0374732751357));
#179842=CARTESIAN_POINT('Ctrl Pts',(-27.9983748948768,-75.8669829436328,
86.0160201738747));
#179843=CARTESIAN_POINT('Ctrl Pts',(-27.9842063416296,-76.5401689750176,
85.9489422436268));
#179844=CARTESIAN_POINT('Ctrl Pts',(-27.9787046285364,-76.8000028522898,
85.9151310849484));
#179845=CARTESIAN_POINT('Ctrl Pts',(-27.9680786331094,-77.2910612907271,
85.8362548589024));
#179846=CARTESIAN_POINT('Ctrl Pts',(-27.9629597312461,-77.5225283259899,
85.7926708694011));
#179847=CARTESIAN_POINT('Ctrl Pts',(-27.9459079923068,-78.2773135689571,
85.6295219742758));
#179848=CARTESIAN_POINT('Ctrl Pts',(-27.9336692048689,-78.7951050754462,
85.4840841657931));
#179849=CARTESIAN_POINT('Ctrl Pts',(-27.9131107193046,-79.6471742861783,
85.1874098991876));
#179850=CARTESIAN_POINT('Ctrl Pts',(-27.9047868360306,-79.9873185335186,
85.0528224331465));
#179851=CARTESIAN_POINT('Ctrl Pts',(-27.8904074150385,-80.5730290701081,
84.7919520042867));
#179852=CARTESIAN_POINT('Ctrl Pts',(-27.8842971545009,-80.8212953221514,
84.6717539991534));
#179853=CARTESIAN_POINT('Ctrl Pts',(-27.8698641651539,-81.4097433606845,
84.3630061942767));
#179854=CARTESIAN_POINT('Ctrl Pts',(-27.861710200252,-81.7452306837839,
84.166903060444));
#179855=CARTESIAN_POINT('Ctrl Pts',(-27.8453550084117,-82.3999208736734,
83.743847470235));
#179856=CARTESIAN_POINT('Ctrl Pts',(-27.8371328291244,-82.7192165073017,
83.5164356111363));
#179857=CARTESIAN_POINT('Ctrl Pts',(-27.8216158902492,-83.2835271823475,
83.0752714525562));
#179858=CARTESIAN_POINT('Ctrl Pts',(-27.8144342767874,-83.5319170271531,
82.8658224661742));
#179859=CARTESIAN_POINT('Ctrl Pts',(-27.7925141076131,-84.2572804367664,
82.2069105176513));
#179860=CARTESIAN_POINT('Ctrl Pts',(-27.7775244449214,-84.7095831907395,
81.7301117026834));
#179861=CARTESIAN_POINT('Ctrl Pts',(-27.7543237430217,-85.3612165647386,
80.9306647300642));
#179862=CARTESIAN_POINT('Ctrl Pts',(-27.7459456038675,-85.5862339849805,
80.6288772514887));
#179863=CARTESIAN_POINT('Ctrl Pts',(-27.7285710578544,-86.034427501779,
79.9691890098338));
#179864=CARTESIAN_POINT('Ctrl Pts',(-27.7197240144229,-86.2532168953495,
79.6100593961399));
#179865=CARTESIAN_POINT('Ctrl Pts',(-27.7023250909202,-86.6476929956993,
78.8856638739585));
#179866=CARTESIAN_POINT('Ctrl Pts',(-27.6936986564007,-86.8246641272642,
78.52105954023));
#179867=CARTESIAN_POINT('Ctrl Pts',(-27.6675797083516,-87.2965186957519,
77.4225764407828));
#179868=CARTESIAN_POINT('Ctrl Pts',(-27.6496751030241,-87.5431103114704,
76.6677537942569));
#179869=CARTESIAN_POINT('Ctrl Pts',(-27.6227789730324,-87.8109154077877,
75.5014481464235));
#179870=CARTESIAN_POINT('Ctrl Pts',(-27.61368927909,-87.8834238266364,75.1015430110265));
#179871=CARTESIAN_POINT('Ctrl Pts',(-27.5967623749459,-87.984714478606,
74.340769305862));
#179872=CARTESIAN_POINT('Ctrl Pts',(-27.5889116823622,-88.0174175457536,
73.9804215063339));
#179873=CARTESIAN_POINT('Ctrl Pts',(-27.5726952476485,-88.0537744436508,
73.2211702198945));
#179874=CARTESIAN_POINT('Ctrl Pts',(-27.5643023785365,-88.0543305131637,
72.8232192864537));
#179875=CARTESIAN_POINT('Ctrl Pts',(-27.5329917923186,-87.9902150124072,
71.3750406569378));
#179876=CARTESIAN_POINT('Ctrl Pts',(-27.5093033935216,-87.8166446035142,
70.3293263596883));
#179877=CARTESIAN_POINT('Ctrl Pts',(-27.4749412181969,-87.3846487974696,
68.8498644114641));
#179878=CARTESIAN_POINT('Ctrl Pts',(-27.4640850915678,-87.2212671356848,
68.387918239908));
#179879=CARTESIAN_POINT('Ctrl Pts',(-27.4356932887815,-86.7190227920006,
67.1895048707421));
#179880=CARTESIAN_POINT('Ctrl Pts',(-27.4185930823565,-86.3366767776217,
66.4766538853577));
#179881=CARTESIAN_POINT('Ctrl Pts',(-27.3825509135325,-85.4292391538904,
65.1036229345755));
#179882=CARTESIAN_POINT('Ctrl Pts',(-27.363866715291,-84.897958041126,64.4464312496957));
#179883=CARTESIAN_POINT('Ctrl Pts',(-27.3275858984294,-83.7515287572018,
63.2771098842675));
#179884=CARTESIAN_POINT('Ctrl Pts',(-27.3099850543915,-83.1410943648889,
62.7579304603558));
#179885=CARTESIAN_POINT('Ctrl Pts',(-27.2561001277643,-81.1125184247412,
61.3386319068994));
#179886=CARTESIAN_POINT('Ctrl Pts',(-27.2193312238702,-79.5515846505893,
60.6471229272152));
#179887=CARTESIAN_POINT('Ctrl Pts',(-27.163845282467,-77.1023224312657,
60.0821227070811));
#179888=CARTESIAN_POINT('Ctrl Pts',(-27.1454072056421,-76.2741375949993,
59.9740771483805));
#179889=CARTESIAN_POINT('Ctrl Pts',(-27.0942944771862,-73.9363035775581,
59.8985369954317));
#179890=CARTESIAN_POINT('Ctrl Pts',(-27.0619671031244,-72.4279016825108,
60.1092423462384));
#179891=CARTESIAN_POINT('Ctrl Pts',(-27.0204627867279,-70.6553575286048,
60.6781953554928));
#179892=CARTESIAN_POINT('Ctrl Pts',(-27.0122985285324,-70.3154085212424,
60.803211745673));
#179893=CARTESIAN_POINT('Ctrl Pts',(-26.987130500699,-69.2693881618042,
61.2394378446713));
#179894=CARTESIAN_POINT('Ctrl Pts',(-26.9704806532509,-68.5850108067239,
61.6001714360522));
#179895=CARTESIAN_POINT('Ctrl Pts',(-26.9358799470576,-67.2375402083574,
62.4688447909708));
#179896=CARTESIAN_POINT('Ctrl Pts',(-26.9179148479554,-66.5803550918046,
62.9864356224216));
#179897=CARTESIAN_POINT('Ctrl Pts',(-26.8896489617794,-65.6607017080844,
63.8646050038475));
#179898=CARTESIAN_POINT('Ctrl Pts',(-26.8796608922055,-65.35847761878,64.1837672662306));
#179899=CARTESIAN_POINT('Ctrl Pts',(-26.8613952628629,-64.8328716729229,
64.7991669455948));
#179900=CARTESIAN_POINT('Ctrl Pts',(-26.8532042088826,-64.6053354394027,
65.0903585287389));
#179901=CARTESIAN_POINT('Ctrl Pts',(-26.8358997393617,-64.1447400897498,
65.7347693972527));
#179902=CARTESIAN_POINT('Ctrl Pts',(-26.8268048243645,-63.9156848034059,
66.0908585456666));
#179903=CARTESIAN_POINT('Ctrl Pts',(-26.8007583416441,-63.3082892952384,
67.1434425427016));
#179904=CARTESIAN_POINT('Ctrl Pts',(-26.7838722948845,-62.9742535941638,
67.865720501512));
#179905=CARTESIAN_POINT('Ctrl Pts',(-26.7574958585418,-62.572988888465,
68.9894125283925));
#179906=CARTESIAN_POINT('Ctrl Pts',(-26.7484197854605,-62.4554671248045,
69.3730633903607));
#179907=CARTESIAN_POINT('Ctrl Pts',(-26.7296221149504,-62.2508872010353,
70.1712710218854));
#179908=CARTESIAN_POINT('Ctrl Pts',(-26.7199881481534,-62.1659703364768,
70.5860658314944));
#179909=CARTESIAN_POINT('Ctrl Pts',(-26.7009018638481,-62.0349643893737,
71.4411355624927));
#179910=CARTESIAN_POINT('Ctrl Pts',(-26.6914264825298,-61.9906394492088,
71.8799832795929));
#179911=CARTESIAN_POINT('Ctrl Pts',(-26.6644730958629,-61.9272184950069,
73.1416759741127));
#179912=CARTESIAN_POINT('Ctrl Pts',(-26.6471711074707,-61.9633743450345,
73.9674584135148));
#179913=CARTESIAN_POINT('Ctrl Pts',(-26.6221879434281,-62.1182970774639,
75.0896077813918));
#179914=CARTESIAN_POINT('Ctrl Pts',(-26.6152061769837,-62.1715478037406,
75.3952408793041));
#179915=CARTESIAN_POINT('Ctrl Pts',(-26.5981209290794,-62.3262333414433,
76.1278569753121));
#179916=CARTESIAN_POINT('Ctrl Pts',(-26.5879730364882,-62.4384930348096,
76.5525447979478));
#179917=CARTESIAN_POINT('Ctrl Pts',(-26.5727315788362,-62.6448972591376,
77.1974323838962));
#179918=CARTESIAN_POINT('Ctrl Pts',(-26.567469752788,-62.7237742836488,
77.4219902251026));
#179919=CARTESIAN_POINT('Ctrl Pts',(-26.5517149682415,-62.9821426894515,
78.0971663978203));
#179920=CARTESIAN_POINT('Ctrl Pts',(-26.5414479435043,-63.1810375963398,
78.5403282247619));
#179921=CARTESIAN_POINT('Ctrl Pts',(-26.5193724009043,-63.6608588511293,
79.4682464039048));
#179922=CARTESIAN_POINT('Ctrl Pts',(-26.5075648017411,-63.9497249456272,
79.9489618077733));
#179923=CARTESIAN_POINT('Ctrl Pts',(-26.4901011928254,-64.4043888612161,
80.6069925584686));
#179924=CARTESIAN_POINT('Ctrl Pts',(-26.4847749657926,-64.5463317191149,
80.8008845229701));
#179925=CARTESIAN_POINT('Ctrl Pts',(-26.4733338455652,-64.8570452251037,
81.2017922831271));
#179926=CARTESIAN_POINT('Ctrl Pts',(-26.4672136566416,-65.0270462099519,
81.4078623440487));
#179927=CARTESIAN_POINT('Ctrl Pts',(-26.4503871459154,-65.510322077725,
81.958356809343));
#179928=CARTESIAN_POINT('Ctrl Pts',(-26.4396561649183,-65.8361487294579,
82.2917405008153));
#179929=CARTESIAN_POINT('Ctrl Pts',(-26.4240726946724,-66.3536496820085,
82.7663707751346));
#179930=CARTESIAN_POINT('Ctrl Pts',(-26.4189237194656,-66.5325138718022,
82.9214875313808));
#179931=CARTESIAN_POINT('Ctrl Pts',(-26.4073473215465,-66.9492086440972,
83.2632709400261));
#179932=CARTESIAN_POINT('Ctrl Pts',(-26.4009613112974,-67.1896315259617,
83.4467584732397));
#179933=CARTESIAN_POINT('Ctrl Pts',(-26.3827457343307,-67.8953428672604,
83.9476351195622));
#179934=CARTESIAN_POINT('Ctrl Pts',(-26.3709709769733,-68.3756485690825,
84.2439355623144));
#179935=CARTESIAN_POINT('Ctrl Pts',(-26.3539767684834,-69.0667985912631,
84.6115656161261));
#179936=CARTESIAN_POINT('Ctrl Pts',(-26.349132940433,-69.2633580163022,
84.709903395342));
#179937=CARTESIAN_POINT('Ctrl Pts',(-26.338946669668,-69.6746542837514,
84.9029725362139));
#179938=CARTESIAN_POINT('Ctrl Pts',(-26.3336041872981,-69.8897244447453,
84.9970074859295));
#179939=CARTESIAN_POINT('Ctrl Pts',(-26.314231955768,-70.6735487500045,
85.3149592179739));
#179940=CARTESIAN_POINT('Ctrl Pts',(-26.3000246937031,-71.255992426112,
85.5051243484357));
#179941=CARTESIAN_POINT('Ctrl Pts',(-26.2816122099814,-72.0632443492675,
85.7060943795211));
#179942=CARTESIAN_POINT('Ctrl Pts',(-26.2768286975967,-72.2785241214213,
85.7537910136647));
#179943=CARTESIAN_POINT('Ctrl Pts',(-26.2660720341698,-72.7714956543973,
85.8498414623097));
#179944=CARTESIAN_POINT('Ctrl Pts',(-26.260134841256,-73.0499760709272,
85.8946831020152));
#179945=CARTESIAN_POINT('Ctrl Pts',(-26.2429700519115,-73.8615368526726,
85.9985253898064));
#179946=CARTESIAN_POINT('Ctrl Pts',(-26.2317986029984,-74.3976751519069,
86.0338075190741));
#179947=CARTESIAN_POINT('Ctrl Pts',(-26.2155064654886,-75.1493185610999,
86.0374428848513));
#179948=CARTESIAN_POINT('Ctrl Pts',(-26.2107555175633,-75.3647440062942,
86.0332104066427));
#179949=CARTESIAN_POINT('Ctrl Pts',(-26.2003640862362,-75.8285358965611,
86.0127296677718));
#179950=CARTESIAN_POINT('Ctrl Pts',(-26.1947077546196,-76.076831658566,
85.9947172503313));
#179951=CARTESIAN_POINT('Ctrl Pts',(-26.174118315283,-76.9727601170871,
85.9040944046082));
#179952=CARTESIAN_POINT('Ctrl Pts',(-26.1589940543832,-77.6162491189474,
85.7902962812833));
#179953=CARTESIAN_POINT('Ctrl Pts',(-26.1398650652927,-78.4544973207557,
85.575212258799));
#179954=CARTESIAN_POINT('Ctrl Pts',(-26.1352371189142,-78.6597702370693,
85.5170117907657));
#179955=CARTESIAN_POINT('Ctrl Pts',(-26.1249826697253,-79.1176792880076,
85.3747766623542));
#179956=CARTESIAN_POINT('Ctrl Pts',(-26.1193886159666,-79.36930568476,85.2879755540693));
#179957=CARTESIAN_POINT('Ctrl Pts',(-26.1032508837398,-80.0895803369744,
85.0145418610182));
#179958=CARTESIAN_POINT('Ctrl Pts',(-26.0927596236044,-80.5507285382675,
84.8081327170226));
#179959=CARTESIAN_POINT('Ctrl Pts',(-26.0768782923636,-81.2019710439065,
84.4706061229787));
#179960=CARTESIAN_POINT('Ctrl Pts',(-26.0718209580446,-81.4026693703699,
84.3598599506523));
#179961=CARTESIAN_POINT('Ctrl Pts',(-26.0604409945474,-81.841759782,84.1024337334988));
#179962=CARTESIAN_POINT('Ctrl Pts',(-26.0540874597251,-82.0786814708573,
83.9532153401487));
#179963=CARTESIAN_POINT('Ctrl Pts',(-26.0326197025067,-82.8583908629171,
83.426684350656));
#179964=CARTESIAN_POINT('Ctrl Pts',(-26.0173630094784,-83.3783347810282,
83.0154683355479));
#179965=CARTESIAN_POINT('Ctrl Pts',(-25.9978843357506,-84.0264784016952,
82.4162387348755));
#179966=CARTESIAN_POINT('Ctrl Pts',(-25.9930878128077,-84.1849799764002,
82.2618823059327));
#179967=CARTESIAN_POINT('Ctrl Pts',(-25.9825809313068,-84.5285903864206,
81.9094303283484));
#179968=CARTESIAN_POINT('Ctrl Pts',(-25.9769052402276,-84.7113090086692,
81.7097666897259));
#179969=CARTESIAN_POINT('Ctrl Pts',(-25.961608050232,-85.1874381789504,
81.155737120242));
#179970=CARTESIAN_POINT('Ctrl Pts',(-25.952000205556,-85.4687383554471,
80.7909734609118));
#179971=CARTESIAN_POINT('Ctrl Pts',(-25.9358149717999,-85.8922432586057,
80.1779994751828));
#179972=CARTESIAN_POINT('Ctrl Pts',(-25.9294938723795,-86.0466684166363,
79.9382093144296));
#179973=CARTESIAN_POINT('Ctrl Pts',(-25.9143737003665,-86.393063506594,
79.3600233212961));
#179974=CARTESIAN_POINT('Ctrl Pts',(-25.905510480436,-86.5782227926926,
79.0175079635106));
#179975=CARTESIAN_POINT('Ctrl Pts',(-25.8852182883946,-86.9668909989723,
78.2153442863922));
#179976=CARTESIAN_POINT('Ctrl Pts',(-25.8737960710766,-87.1600185044385,
77.7506301255387));
#179977=CARTESIAN_POINT('Ctrl Pts',(-25.8573459921238,-87.4051241865287,
77.0475922525296));
#179978=CARTESIAN_POINT('Ctrl Pts',(-25.8520764705073,-87.4783803834003,
76.8167470193745));
#179979=CARTESIAN_POINT('Ctrl Pts',(-25.8392195879066,-87.6438771631219,
76.2385212852944));
#179980=CARTESIAN_POINT('Ctrl Pts',(-25.8317245562172,-87.7281208555165,
75.8893932446823));
#179981=CARTESIAN_POINT('Ctrl Pts',(-25.8169812586108,-87.8643090925225,
75.2015789058741));
#179982=CARTESIAN_POINT('Ctrl Pts',(-25.8097174915849,-87.9175609186128,
74.8631684568653));
#179983=CARTESIAN_POINT('Ctrl Pts',(-25.7937813406749,-88.0030548038068,
74.1362254915934));
#179984=CARTESIAN_POINT('Ctrl Pts',(-25.7851028224779,-88.0313761686669,
73.7472133444228));
#179985=CARTESIAN_POINT('Ctrl Pts',(-25.7614798027027,-88.0612328413822,
72.6969835515868));
#179986=CARTESIAN_POINT('Ctrl Pts',(-25.7463802248193,-88.0303757281828,
72.0347225112334));
#179987=CARTESIAN_POINT('Ctrl Pts',(-25.7241993780915,-87.9089029806346,
71.0492587936999));
#179988=CARTESIAN_POINT('Ctrl Pts',(-25.7168688288055,-87.8556904339266,
70.7214147466801));
#179989=CARTESIAN_POINT('Ctrl Pts',(-25.7043057448399,-87.7404526520802,
70.152288399804));
#179990=CARTESIAN_POINT('Ctrl Pts',(-25.6990302602599,-87.6840409946244,
69.9103264370149));
#179991=CARTESIAN_POINT('Ctrl Pts',(-25.6886812995691,-87.5591558926574,
69.4368652277445));
#179992=CARTESIAN_POINT('Ctrl Pts',(-25.6836015556126,-87.4910407607913,
69.2051900647473));
#179993=CARTESIAN_POINT('Ctrl Pts',(-25.6710187955589,-87.3084196999825,
68.6423027329678));
#179994=CARTESIAN_POINT('Ctrl Pts',(-25.6634241156324,-87.1868554521697,
68.3133832130026));
#179995=CARTESIAN_POINT('Ctrl Pts',(-25.6469322102791,-86.8989917421115,
67.6208152365593));
#179996=CARTESIAN_POINT('Ctrl Pts',(-25.6380101285661,-86.7287897905199,
67.2587491966665));
#179997=CARTESIAN_POINT('Ctrl Pts',(-25.6094817159753,-86.1360404434086,
66.1334748648337));
#179998=CARTESIAN_POINT('Ctrl Pts',(-25.5897208421621,-85.6529542244707,
65.4019430271132));
#179999=CARTESIAN_POINT('Ctrl Pts',(-25.5633037283315,-84.8859514128838,
64.4631656614516));
#180000=CARTESIAN_POINT('Ctrl Pts',(-25.5560718741698,-84.661096504945,
64.2093152050967));
#180001=CARTESIAN_POINT('Ctrl Pts',(-25.5376322776274,-84.0614744011126,
63.5839901608553));
#180002=CARTESIAN_POINT('Ctrl Pts',(-25.5262669865481,-83.6735836414418,
63.2260754919771));
#180003=CARTESIAN_POINT('Ctrl Pts',(-25.5015769616827,-82.8034571212361,
62.5149304690227));
#180004=CARTESIAN_POINT('Ctrl Pts',(-25.4882596372729,-82.3154604851025,
62.1686024899682));
#180005=CARTESIAN_POINT('Ctrl Pts',(-25.4563913029029,-81.0970264860667,
61.4226454677198));
#180006=CARTESIAN_POINT('Ctrl Pts',(-25.4378456322442,-80.3465179806126,
61.0554992253828));
#180007=CARTESIAN_POINT('Ctrl Pts',(-25.4108569342881,-79.1794003752194,
60.6192454761137));
#180008=CARTESIAN_POINT('Ctrl Pts',(-25.4020110591221,-78.7848331540593,
60.4933124162824));
#180009=CARTESIAN_POINT('Ctrl Pts',(-25.3752278172481,-77.5928758295803,
60.1745015950223));
#180010=CARTESIAN_POINT('Ctrl Pts',(-25.3571272366448,-76.7800838228553,
60.0374753873656));
#180011=CARTESIAN_POINT('Ctrl Pts',(-25.3188691787239,-75.0556604521194,
59.909545036559));
#180012=CARTESIAN_POINT('Ctrl Pts',(-25.2986976871102,-74.142358408256,
59.9358960981425));
#180013=CARTESIAN_POINT('Ctrl Pts',(-25.2583479842648,-72.317055915739,
60.1832535945134));
#180014=CARTESIAN_POINT('Ctrl Pts',(-25.238105754833,-71.4094419108868,
60.4097518282593));
#180015=CARTESIAN_POINT('Ctrl Pts',(-25.2177843835793,-70.5373207047723,
60.7277886365121));
#180016=CARTESIAN_POINT('',(-25.21690938235,-70.5367618819012,60.7262027183532));
#180017=CARTESIAN_POINT('Ctrl Pts',(-29.4261514861327,-77.757911767464,
85.74414017529));
#180018=CARTESIAN_POINT('Ctrl Pts',(-29.3779431821827,-79.904349121914,
85.28004229623));
#180019=CARTESIAN_POINT('Ctrl Pts',(-29.2815265742827,-83.95514758824,83.24564128978));
#180020=CARTESIAN_POINT('Ctrl Pts',(-29.1369016624246,-87.79923337781,77.634595795182));
#180021=CARTESIAN_POINT('Ctrl Pts',(-28.9922767505727,-88.44943474654,70.864604569967));
#180022=CARTESIAN_POINT('Ctrl Pts',(-28.8476518387227,-85.74425521307,64.624573520997));
#180023=CARTESIAN_POINT('Ctrl Pts',(-28.7030269268629,-80.358422966095,
60.47138590026));
#180024=CARTESIAN_POINT('Ctrl Pts',(-28.5584020150127,-73.635715047619,
59.44121987509));
#180025=CARTESIAN_POINT('Ctrl Pts',(-28.4137771031546,-67.253383129327,
61.79109721394));
#180026=CARTESIAN_POINT('Ctrl Pts',(-28.2691521913028,-62.80377526215,66.934740200613));
#180027=CARTESIAN_POINT('Ctrl Pts',(-28.1245272794527,-61.39703449716,73.5888484027236));
#180028=CARTESIAN_POINT('Ctrl Pts',(-27.9799023675929,-63.38413245482,80.093271282679));
#180029=CARTESIAN_POINT('Ctrl Pts',(-27.8352774557427,-68.269302909975,
84.82520375033));
#180030=CARTESIAN_POINT('Ctrl Pts',(-27.6906525438927,-74.8337322064467,
86.60406386368));
#180031=CARTESIAN_POINT('Ctrl Pts',(-27.5460276320329,-81.439644079033,
84.98603926299));
#180032=CARTESIAN_POINT('Ctrl Pts',(-27.4014027201827,-86.43891267502,80.374815045269));
#180033=CARTESIAN_POINT('Ctrl Pts',(-27.2567778083246,-88.58425768156,73.9208573383313));
#180034=CARTESIAN_POINT('Ctrl Pts',(-27.1121528964728,-87.34043148427,67.234380562697));
#180035=CARTESIAN_POINT('Ctrl Pts',(-26.9675279846227,-83.017759463383,
61.98361091626));
#180036=CARTESIAN_POINT('Ctrl Pts',(-26.8229030727646,-76.694716120822,
59.47857635201));
#180037=CARTESIAN_POINT('Ctrl Pts',(-26.6782781609127,-69.94885371734,60.34426435248));
#180038=CARTESIAN_POINT('Ctrl Pts',(-26.5336532490595,-64.46321472334,64.36469220339));
#180039=CARTESIAN_POINT('Ctrl Pts',(-26.3890283372062,-61.60642524515,70.536793074933));
#180040=CARTESIAN_POINT('Ctrl Pts',(-26.2444034253522,-62.09123300285,77.320673726326));
#180041=CARTESIAN_POINT('Ctrl Pts',(-26.0997785134991,-65.796682053056,
83.02380642958));
#180042=CARTESIAN_POINT('Ctrl Pts',(-25.9551536016452,-71.798290489993,
86.22330197028));
#180043=CARTESIAN_POINT('Ctrl Pts',(-25.8105286897922,-78.59870145323,86.12091018816));
#180044=CARTESIAN_POINT('Ctrl Pts',(-25.665903777939,-84.50126382125,82.742176443924));
#180045=CARTESIAN_POINT('Ctrl Pts',(-25.5212788660852,-88.03332919063,76.930072003796));
#180046=CARTESIAN_POINT('Ctrl Pts',(-25.3766539542322,-88.31368479424,70.134664941592));
#180047=CARTESIAN_POINT('Ctrl Pts',(-25.2320290423791,-85.27234197776,64.051391343194));
#180048=CARTESIAN_POINT('Ctrl Pts',(-25.0874041305261,-79.668249953127,
60.1978610671));
#180049=CARTESIAN_POINT('Ctrl Pts',(-24.942779218673,-72.899002749005,59.53595519057));
#180050=CARTESIAN_POINT('Ctrl Pts',(-24.846362610771,-68.736775097357,61.33139849116));
#180051=CARTESIAN_POINT('Ctrl Pts',(-24.79815430682,-67.001564902287,62.6773649606));
#180052=CARTESIAN_POINT('Ctrl Pts',(-29.5486931499337,-77.757911767464,
85.74414017529));
#180053=CARTESIAN_POINT('Ctrl Pts',(-29.5004848459837,-79.904349121914,
85.28004229623));
#180054=CARTESIAN_POINT('Ctrl Pts',(-29.4040682380836,-83.95514758824,83.24564128978));
#180055=CARTESIAN_POINT('Ctrl Pts',(-29.2594433262332,-87.79923337781,77.634595795182));
#180056=CARTESIAN_POINT('Ctrl Pts',(-29.1148184143737,-88.44943474654,70.864604569967));
#180057=CARTESIAN_POINT('Ctrl Pts',(-28.9701935025236,-85.74425521307,64.624573520997));
#180058=CARTESIAN_POINT('Ctrl Pts',(-28.8255685906649,-80.358422966095,
60.47138590026));
#180059=CARTESIAN_POINT('Ctrl Pts',(-28.6809436788136,-73.635715047619,
59.44121987509));
#180060=CARTESIAN_POINT('Ctrl Pts',(-28.5363187669632,-67.253383129327,
61.79109721394));
#180061=CARTESIAN_POINT('Ctrl Pts',(-28.3916938551037,-62.80377526215,66.934740200613));
#180062=CARTESIAN_POINT('Ctrl Pts',(-28.2470689432536,-61.39703449716,73.5888484027236));
#180063=CARTESIAN_POINT('Ctrl Pts',(-28.1024440313949,-63.38413245482,80.093271282679));
#180064=CARTESIAN_POINT('Ctrl Pts',(-27.9578191195436,-68.269302909975,
84.82520375033));
#180065=CARTESIAN_POINT('Ctrl Pts',(-27.8131942076936,-74.8337322064467,
86.60406386368));
#180066=CARTESIAN_POINT('Ctrl Pts',(-27.6685692958349,-81.439644079033,
84.98603926299));
#180067=CARTESIAN_POINT('Ctrl Pts',(-27.5239443839836,-86.43891267502,80.374815045269));
#180068=CARTESIAN_POINT('Ctrl Pts',(-27.3793194721332,-88.58425768156,73.9208573383313));
#180069=CARTESIAN_POINT('Ctrl Pts',(-27.2346945602737,-87.34043148427,67.234380562697));
#180070=CARTESIAN_POINT('Ctrl Pts',(-27.0900696484237,-83.017759463383,
61.98361091626));
#180071=CARTESIAN_POINT('Ctrl Pts',(-26.9454447365732,-76.694716120822,
59.47857635201));
#180072=CARTESIAN_POINT('Ctrl Pts',(-26.8008198247137,-69.94885371734,60.34426435248));
#180073=CARTESIAN_POINT('Ctrl Pts',(-26.6561949128635,-64.46321472334,64.36469220339));
#180074=CARTESIAN_POINT('Ctrl Pts',(-26.5115700010092,-61.60642524515,70.536793074933));
#180075=CARTESIAN_POINT('Ctrl Pts',(-26.3669450891548,-62.09123300285,77.320673726326));
#180076=CARTESIAN_POINT('Ctrl Pts',(-26.2223201773017,-65.796682053056,
83.02380642958));
#180077=CARTESIAN_POINT('Ctrl Pts',(-26.0776952654478,-71.798290489993,
86.22330197028));
#180078=CARTESIAN_POINT('Ctrl Pts',(-25.9330703535948,-78.59870145323,86.12091018816));
#180079=CARTESIAN_POINT('Ctrl Pts',(-25.7884454417409,-84.50126382125,82.742176443924));
#180080=CARTESIAN_POINT('Ctrl Pts',(-25.6438205298878,-88.03332919063,76.930072003796));
#180081=CARTESIAN_POINT('Ctrl Pts',(-25.4991956180348,-88.31368479424,70.134664941592));
#180082=CARTESIAN_POINT('Ctrl Pts',(-25.3545707061817,-85.27234197776,64.051391343194));
#180083=CARTESIAN_POINT('Ctrl Pts',(-25.2099457943287,-79.668249953127,
60.1978610671));
#180084=CARTESIAN_POINT('Ctrl Pts',(-25.0653208824749,-72.899002749005,
59.53595519057));
#180085=CARTESIAN_POINT('Ctrl Pts',(-24.9689042745729,-68.736775097357,
61.33139849116));
#180086=CARTESIAN_POINT('Ctrl Pts',(-24.9206959706219,-67.001564902287,
62.6773649606));
#180087=CARTESIAN_POINT('Ctrl Pts',(-29.6712348137352,-77.757911767464,
85.74414017529));
#180088=CARTESIAN_POINT('Ctrl Pts',(-29.6230265097852,-79.904349121914,
85.28004229623));
#180089=CARTESIAN_POINT('Ctrl Pts',(-29.5266099018845,-83.95514758824,83.24564128978));
#180090=CARTESIAN_POINT('Ctrl Pts',(-29.3819849900345,-87.79923337781,77.634595795182));
#180091=CARTESIAN_POINT('Ctrl Pts',(-29.2373600781752,-88.44943474654,70.864604569967));
#180092=CARTESIAN_POINT('Ctrl Pts',(-29.0927351663245,-85.74425521307,64.624573520997));
#180093=CARTESIAN_POINT('Ctrl Pts',(-28.9481102544736,-80.358422966095,
60.47138590026));
#180094=CARTESIAN_POINT('Ctrl Pts',(-28.8034853426145,-73.635715047619,
59.44121987509));
#180095=CARTESIAN_POINT('Ctrl Pts',(-28.6588604307645,-67.253383129327,
61.79109721394));
#180096=CARTESIAN_POINT('Ctrl Pts',(-28.5142355189052,-62.80377526215,66.934740200613));
#180097=CARTESIAN_POINT('Ctrl Pts',(-28.3696106070545,-61.39703449716,73.5888484027236));
#180098=CARTESIAN_POINT('Ctrl Pts',(-28.2249856952036,-63.38413245482,80.093271282679));
#180099=CARTESIAN_POINT('Ctrl Pts',(-28.0803607833445,-68.269302909975,
84.82520375033));
#180100=CARTESIAN_POINT('Ctrl Pts',(-27.9357358714945,-74.8337322064467,
86.60406386368));
#180101=CARTESIAN_POINT('Ctrl Pts',(-27.7911109596436,-81.439644079033,
84.98603926299));
#180102=CARTESIAN_POINT('Ctrl Pts',(-27.6464860477845,-86.43891267502,80.374815045269));
#180103=CARTESIAN_POINT('Ctrl Pts',(-27.5018611359345,-88.58425768156,73.9208573383313));
#180104=CARTESIAN_POINT('Ctrl Pts',(-27.3572362240752,-87.34043148427,67.234380562697));
#180105=CARTESIAN_POINT('Ctrl Pts',(-27.2126113122245,-83.017759463383,
61.98361091626));
#180106=CARTESIAN_POINT('Ctrl Pts',(-27.0679864003745,-76.694716120822,
59.47857635201));
#180107=CARTESIAN_POINT('Ctrl Pts',(-26.9233614885152,-69.94885371734,60.34426435248));
#180108=CARTESIAN_POINT('Ctrl Pts',(-26.7787365766645,-64.46321472334,64.36469220339));
#180109=CARTESIAN_POINT('Ctrl Pts',(-26.6341116648141,-61.60642524515,70.536793074933));
#180110=CARTESIAN_POINT('Ctrl Pts',(-26.4894867529572,-62.09123300285,77.320673726326));
#180111=CARTESIAN_POINT('Ctrl Pts',(-26.3448618411036,-65.796682053056,
83.02380642958));
#180112=CARTESIAN_POINT('Ctrl Pts',(-26.2002369292505,-71.798290489993,
86.22330197028));
#180113=CARTESIAN_POINT('Ctrl Pts',(-26.0556120173974,-78.59870145323,86.12091018816));
#180114=CARTESIAN_POINT('Ctrl Pts',(-25.9109871055435,-84.50126382125,82.742176443924));
#180115=CARTESIAN_POINT('Ctrl Pts',(-25.7663621936905,-88.03332919063,76.930072003796));
#180116=CARTESIAN_POINT('Ctrl Pts',(-25.6217372818374,-88.31368479424,70.134664941592));
#180117=CARTESIAN_POINT('Ctrl Pts',(-25.4771123699836,-85.27234197776,64.051391343194));
#180118=CARTESIAN_POINT('Ctrl Pts',(-25.3324874581306,-79.668249953127,
60.1978610671));
#180119=CARTESIAN_POINT('Ctrl Pts',(-25.1878625462775,-72.899002749005,
59.53595519057));
#180120=CARTESIAN_POINT('Ctrl Pts',(-25.0914459383755,-68.736775097357,
61.33139849116));
#180121=CARTESIAN_POINT('Ctrl Pts',(-25.0432376344245,-67.001564902287,
62.6773649606));
#180122=CARTESIAN_POINT('Ctrl Pts',(-29.793776477544,-77.757911767464,85.74414017529));
#180123=CARTESIAN_POINT('Ctrl Pts',(-29.745568173594,-79.904349121914,85.28004229623));
#180124=CARTESIAN_POINT('Ctrl Pts',(-29.6491515656854,-83.95514758824,83.24564128978));
#180125=CARTESIAN_POINT('Ctrl Pts',(-29.5045266538354,-87.79923337781,77.634595795182));
#180126=CARTESIAN_POINT('Ctrl Pts',(-29.359901741984,-88.44943474654,70.864604569967));
#180127=CARTESIAN_POINT('Ctrl Pts',(-29.2152768301254,-85.74425521307,64.624573520997));
#180128=CARTESIAN_POINT('Ctrl Pts',(-29.0706519182754,-80.358422966095,
60.47138590026));
#180129=CARTESIAN_POINT('Ctrl Pts',(-28.9260270064154,-73.635715047619,
59.44121987509));
#180130=CARTESIAN_POINT('Ctrl Pts',(-28.7814020945654,-67.253383129327,
61.79109721394));
#180131=CARTESIAN_POINT('Ctrl Pts',(-28.636777182714,-62.80377526215,66.934740200613));
#180132=CARTESIAN_POINT('Ctrl Pts',(-28.4921522708554,-61.39703449716,73.5888484027236));
#180133=CARTESIAN_POINT('Ctrl Pts',(-28.3475273590054,-63.38413245482,80.093271282679));
#180134=CARTESIAN_POINT('Ctrl Pts',(-28.2029024471454,-68.269302909975,
84.82520375033));
#180135=CARTESIAN_POINT('Ctrl Pts',(-28.0582775352954,-74.8337322064467,
86.60406386368));
#180136=CARTESIAN_POINT('Ctrl Pts',(-27.9136526234454,-81.439644079033,
84.98603926299));
#180137=CARTESIAN_POINT('Ctrl Pts',(-27.7690277115854,-86.43891267502,80.374815045269));
#180138=CARTESIAN_POINT('Ctrl Pts',(-27.6244027997354,-88.58425768156,73.9208573383313));
#180139=CARTESIAN_POINT('Ctrl Pts',(-27.479777887884,-87.34043148427,67.234380562697));
#180140=CARTESIAN_POINT('Ctrl Pts',(-27.3351529760254,-83.017759463383,
61.98361091626));
#180141=CARTESIAN_POINT('Ctrl Pts',(-27.1905280641754,-76.694716120822,
59.47857635201));
#180142=CARTESIAN_POINT('Ctrl Pts',(-27.045903152324,-69.94885371734,60.34426435248));
#180143=CARTESIAN_POINT('Ctrl Pts',(-26.9012782404654,-64.46321472334,64.36469220339));
#180144=CARTESIAN_POINT('Ctrl Pts',(-26.7566533286154,-61.60642524515,70.536793074933));
#180145=CARTESIAN_POINT('Ctrl Pts',(-26.6120284167559,-62.09123300285,77.320673726326));
#180146=CARTESIAN_POINT('Ctrl Pts',(-26.4674035049062,-65.796682053056,
83.02380642958));
#180147=CARTESIAN_POINT('Ctrl Pts',(-26.3227785930532,-71.798290489993,
86.22330197028));
#180148=CARTESIAN_POINT('Ctrl Pts',(-26.1781536811993,-78.59870145323,86.12091018816));
#180149=CARTESIAN_POINT('Ctrl Pts',(-26.0335287693461,-84.50126382125,82.742176443924));
#180150=CARTESIAN_POINT('Ctrl Pts',(-25.8889038574932,-88.03332919063,76.930072003796));
#180151=CARTESIAN_POINT('Ctrl Pts',(-25.7442789456393,-88.31368479424,70.134664941592));
#180152=CARTESIAN_POINT('Ctrl Pts',(-25.5996540337862,-85.27234197776,64.051391343194));
#180153=CARTESIAN_POINT('Ctrl Pts',(-25.4550291219332,-79.668249953127,
60.1978610671));
#180154=CARTESIAN_POINT('Ctrl Pts',(-25.3104042100802,-72.899002749005,
59.53595519057));
#180155=CARTESIAN_POINT('Ctrl Pts',(-25.2139876021782,-68.736775097357,
61.33139849116));
#180156=CARTESIAN_POINT('Ctrl Pts',(-25.1657792982272,-67.001564902287,
62.6773649606));
#180157=CARTESIAN_POINT('Ctrl Pts',(-29.3655838523953,-81.6013626746983,
84.2438270474911));
#180158=CARTESIAN_POINT('Ctrl Pts',(-29.3303036656744,-82.9881381538602,
83.4317063126598));
#180159=CARTESIAN_POINT('Ctrl Pts',(-29.295627364516,-84.2015222616406,
82.3803230252726));
#180160=CARTESIAN_POINT('Ctrl Pts',(-29.2347381075074,-85.9289061095604,
80.2099621171966));
#180161=CARTESIAN_POINT('Ctrl Pts',(-29.1967714573928,-86.9123357997735,
78.737499184749));
#180162=CARTESIAN_POINT('Ctrl Pts',(-29.1127653603425,-87.9905194137987,
75.0668637575484));
#180163=CARTESIAN_POINT('Ctrl Pts',(-29.075894631943,-88.150447003745,73.3629071254178));
#180164=CARTESIAN_POINT('Ctrl Pts',(-28.9922442448894,-87.7751516038179,
69.5720079624225));
#180165=CARTESIAN_POINT('Ctrl Pts',(-28.9538064145164,-87.08512602708,67.9181509720035));
#180166=CARTESIAN_POINT('Ctrl Pts',(-28.8854503569788,-85.6164657565867,
65.1722907800833));
#180167=CARTESIAN_POINT('Ctrl Pts',(-28.8482263560423,-84.4707456685075,
63.8773740095143));
#180168=CARTESIAN_POINT('Ctrl Pts',(-28.7869286879839,-82.3077021213379,
62.1109491954591));
#180169=CARTESIAN_POINT('Ctrl Pts',(-28.749043597868,-80.8425902128494,
61.1249202595487));
#180170=CARTESIAN_POINT('Ctrl Pts',(-28.6656746731545,-77.2087891219336,
60.0229950603655));
#180171=CARTESIAN_POINT('Ctrl Pts',(-28.6291541528475,-75.523734318193,
59.8442380189927));
#180172=CARTESIAN_POINT('Ctrl Pts',(-28.5552353989383,-72.170375446941,
60.1356096181979));
#180173=CARTESIAN_POINT('Ctrl Pts',(-28.5179385729897,-70.5085301046633,
60.622769542381));
#180174=CARTESIAN_POINT('Ctrl Pts',(-28.4325907303431,-67.0540816724184,
62.4060056730254));
#180175=CARTESIAN_POINT('Ctrl Pts',(-28.3942903930223,-65.7896559531696,
63.6694196806761));
#180176=CARTESIAN_POINT('Ctrl Pts',(-28.3368489710222,-64.1046749841286,
65.6718124865969));
#180177=CARTESIAN_POINT('Ctrl Pts',(-28.2993959861414,-63.1656332196875,
67.1384103391823));
#180178=CARTESIAN_POINT('Ctrl Pts',(-28.2228502956743,-62.1131264080113,
70.4626573346813));
#180179=CARTESIAN_POINT('Ctrl Pts',(-28.1861287854086,-61.8461477642845,
72.1469332660689));
#180180=CARTESIAN_POINT('Ctrl Pts',(-28.1085461465717,-62.1183832603,75.6693497096584));
#180181=CARTESIAN_POINT('Ctrl Pts',(-28.071489187918,-62.5795360968161,
77.3267817400747));
#180182=CARTESIAN_POINT('Ctrl Pts',(-27.9868394695533,-64.3034330597131,
80.7751238150644));
#180183=CARTESIAN_POINT('Ctrl Pts',(-27.9484187558418,-65.548506983732,
82.0646263543977));
#180184=CARTESIAN_POINT('Ctrl Pts',(-27.8840027503118,-67.7671789913901,
83.9854448061143));
#180185=CARTESIAN_POINT('Ctrl Pts',(-27.8469128057308,-69.2644434892098,
84.8353927582126));
#180186=CARTESIAN_POINT('Ctrl Pts',(-27.7827496034337,-72.0399537191075,
85.7525454179823));
#180187=CARTESIAN_POINT('Ctrl Pts',(-27.7448787069659,-73.7589969853065,
86.1552553504063));
#180188=CARTESIAN_POINT('Ctrl Pts',(-27.6613031356659,-77.5561960000081,
85.8925693173151));
#180189=CARTESIAN_POINT('Ctrl Pts',(-27.6245645194847,-79.2040488916052,
85.454539118987));
#180190=CARTESIAN_POINT('Ctrl Pts',(-27.545723918875,-82.4335893984305,
83.8861011614419));
#180191=CARTESIAN_POINT('Ctrl Pts',(-27.5081701457295,-83.7695689881318,
82.7623462776217));
#180192=CARTESIAN_POINT('Ctrl Pts',(-27.431506954629,-86.0909832894995,
80.1533697833587));
#180193=CARTESIAN_POINT('Ctrl Pts',(-27.3938450433658,-86.871569728093,
78.585244494142));
#180194=CARTESIAN_POINT('Ctrl Pts',(-27.3365640377179,-87.7227218052663,
76.1182439307786));
#180195=CARTESIAN_POINT('Ctrl Pts',(-27.2985997691106,-88.1554259539642,
74.4007921117372));
#180196=CARTESIAN_POINT('Ctrl Pts',(-27.2144471677441,-87.9283326232303,
70.5744157048114));
#180197=CARTESIAN_POINT('Ctrl Pts',(-27.1780151180434,-87.5152757592269,
68.9354836726551));
#180198=CARTESIAN_POINT('Ctrl Pts',(-27.1051166195486,-86.1018611225955,
65.9319091457066));
#180199=CARTESIAN_POINT('Ctrl Pts',(-27.0686837698037,-85.1030263512263,
64.5683559877304));
#180200=CARTESIAN_POINT('Ctrl Pts',(-26.9839443790261,-82.2803880750339,
61.9357859485765));
#180201=CARTESIAN_POINT('Ctrl Pts',(-26.9459015379113,-80.6723964065564,
61.1819992045571));
#180202=CARTESIAN_POINT('Ctrl Pts',(-26.8876102860954,-78.1864303986462,
60.2477452459039));
#180203=CARTESIAN_POINT('Ctrl Pts',(-26.8502010969373,-76.4872594038116,
59.8797505089315));
#180204=CARTESIAN_POINT('Ctrl Pts',(-26.7761028839489,-73.1139235187851,
59.9992914624847));
#180205=CARTESIAN_POINT('Ctrl Pts',(-26.7384047115212,-71.3858814275703,
60.2955114455625));
#180206=CARTESIAN_POINT('Ctrl Pts',(-26.6585341496444,-68.0757772917095,
61.8029934063736));
#180207=CARTESIAN_POINT('Ctrl Pts',(-26.6217434954712,-66.685638534737,
62.7946497723639));
#180208=CARTESIAN_POINT('Ctrl Pts',(-26.5367444780904,-64.0190722193934,
65.6007532047943));
#180209=CARTESIAN_POINT('Ctrl Pts',(-26.4986415165783,-63.2510209027794,
67.2052974950793));
#180210=CARTESIAN_POINT('Ctrl Pts',(-26.4362248200088,-62.2166753702092,
69.854018890858));
#180211=CARTESIAN_POINT('Ctrl Pts',(-26.399137480781,-61.9174125243928,
71.5493285777501));
#180212=CARTESIAN_POINT('Ctrl Pts',(-26.3345682468581,-61.9819953219415,
74.4902614964466));
#180213=CARTESIAN_POINT('Ctrl Pts',(-26.2962027710617,-62.183439931008,
76.2685907288007));
#180214=CARTESIAN_POINT('Ctrl Pts',(-26.2116136533861,-63.739688531473,
79.7928374527053));
#180215=CARTESIAN_POINT('Ctrl Pts',(-26.1745142485159,-64.7236347634373,
81.2065457467117));
#180216=CARTESIAN_POINT('Ctrl Pts',(-26.0976814723829,-67.24032118938,83.6370669645294));
#180217=CARTESIAN_POINT('Ctrl Pts',(-26.061001678293,-68.699461980102,84.5148158415022));
#180218=CARTESIAN_POINT('Ctrl Pts',(-25.9817789563583,-72.0440939057269,
85.8700472606708));
#180219=CARTESIAN_POINT('Ctrl Pts',(-25.9440135851621,-73.7936835266116,
86.0461011698092));
#180220=CARTESIAN_POINT('Ctrl Pts',(-25.8883468613303,-76.3297703438795,
86.026800080011));
#180221=CARTESIAN_POINT('Ctrl Pts',(-25.8501294132487,-78.1034545947031,
85.8493490383469));
#180222=CARTESIAN_POINT('Ctrl Pts',(-25.7675740621284,-81.5634937701812,
84.3765890039492));
#180223=CARTESIAN_POINT('Ctrl Pts',(-25.7302992652139,-83.0209293484797,
83.4417113170998));
#180224=CARTESIAN_POINT('Ctrl Pts',(-25.6539646250139,-85.4607500576467,
80.9658198961807));
#180225=CARTESIAN_POINT('Ctrl Pts',(-25.6173876023457,-86.3989869481063,
79.5514735758963));
#180226=CARTESIAN_POINT('Ctrl Pts',(-25.53394245796,-87.8666834060939,76.0457160962318));
#180227=CARTESIAN_POINT('Ctrl Pts',(-25.4960524688697,-88.0394369527268,
74.2878474727088));
#180228=CARTESIAN_POINT('Ctrl Pts',(-25.4316021534887,-88.0588502759257,
71.3516283557702));
#180229=CARTESIAN_POINT('Ctrl Pts',(-25.3944251791231,-87.7342041208073,
69.6567021743647));
#180230=CARTESIAN_POINT('Ctrl Pts',(-25.3304167651469,-86.6305562570029,
66.9576863201386));
#180231=CARTESIAN_POINT('Ctrl Pts',(-25.2918432869613,-85.8084429463678,
65.3563934455804));
#180232=CARTESIAN_POINT('Ctrl Pts',(-25.2071469265164,-83.0931608647546,
62.6169175361423));
#180233=CARTESIAN_POINT('Ctrl Pts',(-25.170226450455,-81.6763364745364,
61.6526283543061));
#180234=CARTESIAN_POINT('Ctrl Pts',(-25.0872961958142,-78.2051085262274,
60.1648056900112));
#180235=CARTESIAN_POINT('Ctrl Pts',(-25.0495042431519,-76.455634995068,
59.9662747528024));
#180236=CARTESIAN_POINT('Ctrl Pts',(-24.9874702782534,-73.6301866430724,
59.9123510791511));
#180237=CARTESIAN_POINT('Ctrl Pts',(-24.9527649126985,-72.0454497036876,
60.1778193699471));
#180238=CARTESIAN_POINT('Ctrl Pts',(-24.9175248385795,-70.5373262934946,
60.7277865984718));
#180239=CARTESIAN_POINT('Ctrl Pts',(-24.5840827087049,-75.4257087102522,
60.79818693484));
#180240=CARTESIAN_POINT('Ctrl Pts',(-24.5542910420379,-74.1579666637678,
60.75391640706));
#180241=CARTESIAN_POINT('Ctrl Pts',(-24.4947077087039,-71.60879259167,61.06410883866));
#180242=CARTESIAN_POINT('Ctrl Pts',(-24.4053327087039,-68.112244415052,
62.68064695513));
#180243=CARTESIAN_POINT('Ctrl Pts',(-24.3159577087039,-65.280711439107,
65.292377040265));
#180244=CARTESIAN_POINT('Ctrl Pts',(-24.2265827087039,-63.38749595989,68.647152239787));
#180245=CARTESIAN_POINT('Ctrl Pts',(-24.1372077087039,-62.61539180617,72.4210925622802));
#180246=CARTESIAN_POINT('Ctrl Pts',(-24.0478327087039,-63.0389358374,76.249849747832));
#180247=CARTESIAN_POINT('Ctrl Pts',(-23.9584577087039,-64.61723898556,79.7637835434));
#180248=CARTESIAN_POINT('Ctrl Pts',(-23.8690827087039,-67.197926562624,
82.623647685499));
#180249=CARTESIAN_POINT('Ctrl Pts',(-23.7797077087039,-70.531850936755,
84.55334187238));
#180250=CARTESIAN_POINT('Ctrl Pts',(-23.6903327087039,-74.297144509849,
85.36656733984));
#180251=CARTESIAN_POINT('Ctrl Pts',(-23.6009577087039,-78.130293970206,
84.98481273641));
#180252=CARTESIAN_POINT('Ctrl Pts',(-23.5115827087039,-81.661234976842,
83.44493385557));
#180253=CARTESIAN_POINT('Ctrl Pts',(-23.4222077087039,-84.549079348228,
80.895595461536));
#180254=CARTESIAN_POINT('Ctrl Pts',(-23.3328327087039,-86.51502547987,77.582918723914));
#180255=CARTESIAN_POINT('Ctrl Pts',(-23.2434577087039,-87.36927473133,73.8267199037071));
#180256=CARTESIAN_POINT('Ctrl Pts',(-23.1540827087039,-87.02935518539,69.989634282714));
#180257=CARTESIAN_POINT('Ctrl Pts',(-23.0647077087039,-85.52808374721,66.442106209615));
#180258=CARTESIAN_POINT('Ctrl Pts',(-22.9753327087039,-83.01039789668,63.5266252341));
#180259=CARTESIAN_POINT('Ctrl Pts',(-22.8859577087039,-79.719362967031,
61.52466108548));
#180260=CARTESIAN_POINT('Ctrl Pts',(-22.7965827087039,-75.9727058508626,
60.62948969719));
#180261=CARTESIAN_POINT('Ctrl Pts',(-22.7072077087039,-72.132140643769,
60.92753373859));
#180262=CARTESIAN_POINT('Ctrl Pts',(-22.6178327087039,-68.568447624649,
62.39001909784));
#180263=CARTESIAN_POINT('Ctrl Pts',(-22.5284577087039,-65.625676958068,
64.875752825426));
#180264=CARTESIAN_POINT('Ctrl Pts',(-22.4390827087039,-63.58793300618,68.144754346856));
#180265=CARTESIAN_POINT('Ctrl Pts',(-22.3497077087039,-62.65194599751,71.881423944257));
#180266=CARTESIAN_POINT('Ctrl Pts',(-22.2603327087039,-62.90807907012,75.725011748597));
#180267=CARTESIAN_POINT('Ctrl Pts',(-22.1709577087039,-64.3316043293,79.304445669906));
#180268=CARTESIAN_POINT('Ctrl Pts',(-22.0815827087039,-66.785090156491,
82.274155867271));
#180269=CARTESIAN_POINT('Ctrl Pts',(-21.9922077087039,-70.031669291213,
84.34743715126));
#180270=CARTESIAN_POINT('Ctrl Pts',(-21.9028327087039,-73.757906743531,
85.32412840723));
#180271=CARTESIAN_POINT('Ctrl Pts',(-21.8134577087039,-77.604059796605,
85.10993678068));
#180272=CARTESIAN_POINT('Ctrl Pts',(-21.7240827087039,-81.198808703261,
83.72554100684));
#180273=CARTESIAN_POINT('Ctrl Pts',(-21.6347077087039,-84.195105065595,
81.304595020325));
#180274=CARTESIAN_POINT('Ctrl Pts',(-21.5453327087049,-86.30367698195,78.080824582763));
#180275=CARTESIAN_POINT('Ctrl Pts',(-21.4559577087049,-87.32095626873,74.365462660522));
#180276=CARTESIAN_POINT('Ctrl Pts',(-21.3665827087049,-87.1487315749,70.517202012466));
#180277=CARTESIAN_POINT('Ctrl Pts',(-21.2772077087049,-85.80363001565,66.907565859634));
#180278=CARTESIAN_POINT('Ctrl Pts',(-21.1878327087049,-83.415511938176,
63.885039861635));
#180279=CARTESIAN_POINT('Ctrl Pts',(-21.0984577087049,-80.214933794219,
61.74142821188));
#180280=CARTESIAN_POINT('Ctrl Pts',(-21.0090827087049,-76.510889492969,
60.68368194036));
#180281=CARTESIAN_POINT('Ctrl Pts',(-20.9197077087049,-72.660979154464,
60.81391920844));
#180282=CARTESIAN_POINT('Ctrl Pts',(-20.8303327087049,-69.036885266062,
62.11956649947));
#180283=CARTESIAN_POINT('Ctrl Pts',(-20.7409577087049,-65.988489282763,
64.474572505729));
#180284=CARTESIAN_POINT('Ctrl Pts',(-20.6515827087049,-63.81009296796,67.651577519286));
#180285=CARTESIAN_POINT('Ctrl Pts',(-20.5622077087049,-62.71200557292,71.343863455311));
#180286=CARTESIAN_POINT('Ctrl Pts',(-20.4728327087049,-62.80023991832,75.194965383434));
#180287=CARTESIAN_POINT('Ctrl Pts',(-20.3834577087049,-64.06627758214,78.833085776478));
#180288=CARTESIAN_POINT('Ctrl Pts',(-20.2940827087049,-66.387891295025,
81.90698901644));
#180289=CARTESIAN_POINT('Ctrl Pts',(-20.2047077087049,-69.540945146354,
84.11991078892));
#180290=CARTESIAN_POINT('Ctrl Pts',(-20.1153327087049,-73.22103337205,85.25820864606));
#180291=CARTESIAN_POINT('Ctrl Pts',(-20.0259577087049,-77.07286864717,85.21198772236));
#180292=CARTESIAN_POINT('Ctrl Pts',(-19.9365827087049,-80.724582644921,
83.98571033155));
#180293=CARTESIAN_POINT('Ctrl Pts',(-19.8472077087049,-83.823627377769,
81.697765160933));
#180294=CARTESIAN_POINT('Ctrl Pts',(-19.7578327087049,-86.0708112925,78.569037653464));
#180295=CARTESIAN_POINT('Ctrl Pts',(-19.6684577087049,-87.24918416519,74.90158503273));
#180296=CARTESIAN_POINT('Ctrl Pts',(-19.5790827087049,-87.24498216486,71.049474737007));
#180297=CARTESIAN_POINT('Ctrl Pts',(-19.4897077087049,-86.05861095495,67.384601665003));
#180298=CARTESIAN_POINT('Ctrl Pts',(-19.4003327087049,-83.804606594842,
64.260784146057));
#180299=CARTESIAN_POINT('Ctrl Pts',(-19.3109577087049,-80.700577622844,
61.97960566264));
#180300=CARTESIAN_POINT('Ctrl Pts',(-19.2215827087049,-77.046197354344,
60.7612973129));
#180301=CARTESIAN_POINT('Ctrl Pts',(-19.1322077087049,-73.194269067977,
60.72348241298));
#180302=CARTESIAN_POINT('Ctrl Pts',(-19.0428327087049,-69.51667797846,61.86979685924));
#180303=CARTESIAN_POINT('Ctrl Pts',(-18.9534577087039,-66.368440815114,
64.089627347503));
#180304=CARTESIAN_POINT('Ctrl Pts',(-18.8938743753709,-64.82521925324,66.1421806368));
#180305=CARTESIAN_POINT('Ctrl Pts',(-18.8640827087039,-64.2296876317,67.262212718386));
#180306=CARTESIAN_POINT('Ctrl Pts',(-24.7409006782679,-75.4362219922699,
60.49712592814));
#180307=CARTESIAN_POINT('Ctrl Pts',(-24.7111090116019,-74.1371718486303,
60.45176209751));
#180308=CARTESIAN_POINT('Ctrl Pts',(-24.6515256782679,-71.52504349515,60.76961502662));
#180309=CARTESIAN_POINT('Ctrl Pts',(-24.5621506782679,-67.942144731418,
62.42607509136));
#180310=CARTESIAN_POINT('Ctrl Pts',(-24.4727756782679,-65.04068435206,65.102304338201));
#180311=CARTESIAN_POINT('Ctrl Pts',(-24.3834006782679,-63.10071411361,68.539928906151));
#180312=CARTESIAN_POINT('Ctrl Pts',(-24.2940256782679,-62.3095421125,72.4070702789702));
#180313=CARTESIAN_POINT('Ctrl Pts',(-24.2046506782679,-62.74354596694,76.330382269486));
#180314=CARTESIAN_POINT('Ctrl Pts',(-24.1152756782679,-64.36082681442,79.931096006583));
#180315=CARTESIAN_POINT('Ctrl Pts',(-24.0259006782679,-67.005246928886,
82.861587217225));
#180316=CARTESIAN_POINT('Ctrl Pts',(-23.9365256782679,-70.421505740455,
84.83893703977));
#180317=CARTESIAN_POINT('Ctrl Pts',(-23.8471506782679,-74.2797868241642,
85.67224588461));
#180318=CARTESIAN_POINT('Ctrl Pts',(-23.7577756782679,-78.207599560894,
85.28106348769));
#180319=CARTESIAN_POINT('Ctrl Pts',(-23.6684006782679,-81.825740518334,
83.70315583141));
#180320=CARTESIAN_POINT('Ctrl Pts',(-23.5790256782679,-84.784902956671,
81.090859097905));
#180321=CARTESIAN_POINT('Ctrl Pts',(-23.4896506782679,-86.79940000028,77.696372653464));
#180322=CARTESIAN_POINT('Ctrl Pts',(-23.4002756782679,-87.67474575053,73.8474109262253));
#180323=CARTESIAN_POINT('Ctrl Pts',(-23.3109006782679,-87.32643156769,69.915564821625));
#180324=CARTESIAN_POINT('Ctrl Pts',(-23.2215256782679,-85.78808480163,66.280427164319));
#180325=CARTESIAN_POINT('Ctrl Pts',(-23.1321506782679,-83.208222301335,
63.292945609594));
#180326=CARTESIAN_POINT('Ctrl Pts',(-23.0427756782679,-79.835912129926,
61.24154104977));
#180327=CARTESIAN_POINT('Ctrl Pts',(-22.9534006782679,-75.9967277481947,
60.32426255155));
#180328=CARTESIAN_POINT('Ctrl Pts',(-22.8640256782679,-72.061316125801,
60.62966707439));
#180329=CARTESIAN_POINT('Ctrl Pts',(-22.7746506782679,-68.409614313737,
62.12826990236));
#180330=CARTESIAN_POINT('Ctrl Pts',(-22.6852756782679,-65.394169123036,
64.675391191609));
#180331=CARTESIAN_POINT('Ctrl Pts',(-22.5959006782679,-63.30610114364,68.0251238188));
#180332=CARTESIAN_POINT('Ctrl Pts',(-22.5065256782679,-62.34699904441,71.854074030477));
#180333=CARTESIAN_POINT('Ctrl Pts',(-22.4171506782679,-62.60945756717,75.792582896034));
#180334=CARTESIAN_POINT('Ctrl Pts',(-22.3277756782679,-64.06813813831,79.460414346857));
#180335=CARTESIAN_POINT('Ctrl Pts',(-22.2384006782679,-66.582215134543,
82.503464365711));
#180336=CARTESIAN_POINT('Ctrl Pts',(-22.1490256782679,-69.908971632833,
84.62794730547));
#180337=CARTESIAN_POINT('Ctrl Pts',(-22.0596506782679,-73.727232067669,
85.62875888215));
#180338=CARTESIAN_POINT('Ctrl Pts',(-21.9702756782679,-77.668369533221,
85.4092775894));
#180339=CARTESIAN_POINT('Ctrl Pts',(-21.8809006782679,-81.351894187539,
83.99069284351));
#180340=CARTESIAN_POINT('Ctrl Pts',(-21.7915256782679,-84.422186942024,
81.509959290305));
#180341=CARTESIAN_POINT('Ctrl Pts',(-21.7021506782679,-86.58283204993,78.206574771673));
#180342=CARTESIAN_POINT('Ctrl Pts',(-21.6127756782679,-87.62523401748,74.399458448487));
#180343=CARTESIAN_POINT('Ctrl Pts',(-21.5234006782689,-87.44875607083,70.456161338886));
#180344=CARTESIAN_POINT('Ctrl Pts',(-21.4340256782689,-86.07043594758,66.757381783671));
#180345=CARTESIAN_POINT('Ctrl Pts',(-21.3446506782689,-83.623341019893,
63.660211627688));
#180346=CARTESIAN_POINT('Ctrl Pts',(-21.2552756782689,-80.343721550643,
61.4636614468));
#180347=CARTESIAN_POINT('Ctrl Pts',(-21.1659006782689,-76.548202347877,
60.37979312378));
#180348=CARTESIAN_POINT('Ctrl Pts',(-21.0765256782689,-72.603214807152,
60.51324672522));
#180349=CARTESIAN_POINT('Ctrl Pts',(-20.9871506782689,-68.889620468817,
61.85113821951));
#180350=CARTESIAN_POINT('Ctrl Pts',(-20.8977756782689,-65.765941443611,
64.264303341857));
#180351=CARTESIAN_POINT('Ctrl Pts',(-20.8084006782689,-63.53374755725,67.519767519802));
#180352=CARTESIAN_POINT('Ctrl Pts',(-20.7190256782689,-62.40854184824,71.303237973316));
#180353=CARTESIAN_POINT('Ctrl Pts',(-20.6296506782689,-62.49895522482,75.2494465311));
#180354=CARTESIAN_POINT('Ctrl Pts',(-20.5402756782689,-63.79625889445,78.977413771966));
#180355=CARTESIAN_POINT('Ctrl Pts',(-20.4509006782689,-66.175207068926,
82.127229979831));
#180356=CARTESIAN_POINT('Ctrl Pts',(-20.3615256782689,-69.406128587882,
84.39480196293));
#180357=CARTESIAN_POINT('Ctrl Pts',(-20.2721506782689,-73.177100096994,
85.5612111697));
#180358=CARTESIAN_POINT('Ctrl Pts',(-20.1827756782689,-77.124060112478,
85.51384877627));
#180359=CARTESIAN_POINT('Ctrl Pts',(-20.0934006782689,-80.865956665065,
84.25728729746));
#180360=CARTESIAN_POINT('Ctrl Pts',(-20.0040256782689,-84.041535258926,
81.912839141965));
#180361=CARTESIAN_POINT('Ctrl Pts',(-19.9146506782689,-86.34421552051,78.706844729098));
#180362=CARTESIAN_POINT('Ctrl Pts',(-19.8252756782689,-87.5516894335,74.948820873245));
#180363=CARTESIAN_POINT('Ctrl Pts',(-19.7359006782689,-87.54738366077,71.001579045262));
#180364=CARTESIAN_POINT('Ctrl Pts',(-19.6465256782689,-86.331713884,67.246198442551));
#180365=CARTESIAN_POINT('Ctrl Pts',(-19.5571506782689,-84.022044739653,
64.045235275048));
#180366=CARTESIAN_POINT('Ctrl Pts',(-19.4677756782689,-80.841358816111,
61.70772091653));
#180367=CARTESIAN_POINT('Ctrl Pts',(-19.3784006782689,-77.096730146679,
60.45932528185));
#180368=CARTESIAN_POINT('Ctrl Pts',(-19.2890256782679,-73.149674822947,
60.42057650697));
#180369=CARTESIAN_POINT('Ctrl Pts',(-19.1996506782679,-69.381262119169,
61.59520028015));
#180370=CARTESIAN_POINT('Ctrl Pts',(-19.1102756782679,-66.155276240892,
63.869851596353));
#180371=CARTESIAN_POINT('Ctrl Pts',(-19.0506923449349,-64.57394335288,65.973094643852));
#180372=CARTESIAN_POINT('Ctrl Pts',(-19.0209006782679,-63.9637045108,67.120786984341));
#180373=CARTESIAN_POINT('Ctrl Pts',(-24.8977186478319,-75.4467352742876,
60.19606492144));
#180374=CARTESIAN_POINT('Ctrl Pts',(-24.8679269811659,-74.1163770334926,
60.14960778797));
#180375=CARTESIAN_POINT('Ctrl Pts',(-24.8083436478319,-71.441294398629,
60.47512121458));
#180376=CARTESIAN_POINT('Ctrl Pts',(-24.7189686478319,-67.772045047785,
62.1715032276));
#180377=CARTESIAN_POINT('Ctrl Pts',(-24.6295936478319,-64.80065726501,64.912231636138));
#180378=CARTESIAN_POINT('Ctrl Pts',(-24.5402186478319,-62.81393226732,68.432705572515));
#180379=CARTESIAN_POINT('Ctrl Pts',(-24.4508436478319,-62.00369241884,72.393047995661));
#180380=CARTESIAN_POINT('Ctrl Pts',(-24.3614686478319,-62.44815609648,76.41091479114));
#180381=CARTESIAN_POINT('Ctrl Pts',(-24.2720936478319,-64.10441464328,80.098408469768));
#180382=CARTESIAN_POINT('Ctrl Pts',(-24.1827186478319,-66.812567295151,
83.09952674895));
#180383=CARTESIAN_POINT('Ctrl Pts',(-24.0933436478319,-70.311160544158,
85.12453220716));
#180384=CARTESIAN_POINT('Ctrl Pts',(-24.0039686478319,-74.2624291384833,
85.97792442938));
#180385=CARTESIAN_POINT('Ctrl Pts',(-23.9145936478319,-78.284905151586,
85.57731423897));
#180386=CARTESIAN_POINT('Ctrl Pts',(-23.8252186478319,-81.99024605983,83.96137780724));
#180387=CARTESIAN_POINT('Ctrl Pts',(-23.7358436478319,-85.02072656512,81.286122734268));
#180388=CARTESIAN_POINT('Ctrl Pts',(-23.6464686478319,-87.08377452069,77.809826583006));
#180389=CARTESIAN_POINT('Ctrl Pts',(-23.5570936478319,-87.98021676974,73.8681019487347));
#180390=CARTESIAN_POINT('Ctrl Pts',(-23.4677186478319,-87.62350794999,69.841495360525));
#180391=CARTESIAN_POINT('Ctrl Pts',(-23.3783436478319,-86.04808585604,66.118748119013));
#180392=CARTESIAN_POINT('Ctrl Pts',(-23.2889686478319,-83.406046705982,
63.059265985079));
#180393=CARTESIAN_POINT('Ctrl Pts',(-23.1995936478319,-79.952461292809,
60.95842101407));
#180394=CARTESIAN_POINT('Ctrl Pts',(-23.1102186478319,-76.020749645512,
60.01903540591));
#180395=CARTESIAN_POINT('Ctrl Pts',(-23.0208436478319,-71.990491607817,
60.33180041019));
#180396=CARTESIAN_POINT('Ctrl Pts',(-22.9314686478319,-68.250781002811,
61.8665207069));
#180397=CARTESIAN_POINT('Ctrl Pts',(-22.8420936478319,-65.162661287992,
64.475029557805));
#180398=CARTESIAN_POINT('Ctrl Pts',(-22.7527186478319,-63.02426928109,67.905493290763));
#180399=CARTESIAN_POINT('Ctrl Pts',(-22.6633436478319,-62.04205209131,71.826724116717));
#180400=CARTESIAN_POINT('Ctrl Pts',(-22.5739686478319,-62.31083606423,75.860154043494));
#180401=CARTESIAN_POINT('Ctrl Pts',(-22.4845936478319,-63.80467194732,79.616383023829));
#180402=CARTESIAN_POINT('Ctrl Pts',(-22.3952186478319,-66.379340112613,
82.732772864167));
#180403=CARTESIAN_POINT('Ctrl Pts',(-22.3058436478319,-69.786273974476,
84.90845745969));
#180404=CARTESIAN_POINT('Ctrl Pts',(-22.2164686478319,-73.696557391833,
85.93338935707));
#180405=CARTESIAN_POINT('Ctrl Pts',(-22.1270936478319,-77.732679269865,
85.70861839811));
#180406=CARTESIAN_POINT('Ctrl Pts',(-22.0377186478319,-81.504979671842,
84.25584468017));
#180407=CARTESIAN_POINT('Ctrl Pts',(-21.9483436478319,-84.649268818474,
81.715323560263));
#180408=CARTESIAN_POINT('Ctrl Pts',(-21.8589686478319,-86.86198711791,78.332324960555));
#180409=CARTESIAN_POINT('Ctrl Pts',(-21.7695936478319,-87.92951176624,74.43345423642));
#180410=CARTESIAN_POINT('Ctrl Pts',(-21.6802186478319,-87.74878056675,70.395120665275));
#180411=CARTESIAN_POINT('Ctrl Pts',(-21.5908436478319,-86.3372418795,66.607197707679));
#180412=CARTESIAN_POINT('Ctrl Pts',(-21.5014686478319,-83.831170101586,
63.435383393718));
#180413=CARTESIAN_POINT('Ctrl Pts',(-21.4120936478329,-80.472509307037,
61.18589468171));
#180414=CARTESIAN_POINT('Ctrl Pts',(-21.3227186478329,-76.585515202752,
60.07590430719));
#180415=CARTESIAN_POINT('Ctrl Pts',(-21.2333436478329,-72.545450459805,
60.212574242));
#180416=CARTESIAN_POINT('Ctrl Pts',(-21.1439686478329,-68.742355671542,
61.58270993957));
#180417=CARTESIAN_POINT('Ctrl Pts',(-21.0545936478329,-65.543393604434,
64.054034178009));
#180418=CARTESIAN_POINT('Ctrl Pts',(-20.9652186478329,-63.25740214652,67.387957520349));
#180419=CARTESIAN_POINT('Ctrl Pts',(-20.8758436478329,-62.10507812355,71.262612491355));
#180420=CARTESIAN_POINT('Ctrl Pts',(-20.7864686478329,-62.19767053133,75.3039276788));
#180421=CARTESIAN_POINT('Ctrl Pts',(-20.6970936478329,-63.52624020677,79.121741767484));
#180422=CARTESIAN_POINT('Ctrl Pts',(-20.6077186478329,-65.96252284285,82.347470943245));
#180423=CARTESIAN_POINT('Ctrl Pts',(-20.5183436478329,-69.271312029438,
84.66969313695));
#180424=CARTESIAN_POINT('Ctrl Pts',(-20.4289686478329,-73.133166821969,
85.86421369334));
#180425=CARTESIAN_POINT('Ctrl Pts',(-20.3395936478329,-77.175251577815,
85.81570983017));
#180426=CARTESIAN_POINT('Ctrl Pts',(-20.2502186478329,-81.007330685234,
84.52886426336));
#180427=CARTESIAN_POINT('Ctrl Pts',(-20.1608436478329,-84.259443140101,
82.127913122978));
#180428=CARTESIAN_POINT('Ctrl Pts',(-20.0714686478329,-86.61761974852,78.844651804709));
#180429=CARTESIAN_POINT('Ctrl Pts',(-19.9820936478329,-87.85419470181,74.996056713737));
#180430=CARTESIAN_POINT('Ctrl Pts',(-19.8927186478329,-87.84978515668,70.953683353497));
#180431=CARTESIAN_POINT('Ctrl Pts',(-19.8033436478329,-86.60481681305,67.107795220083));
#180432=CARTESIAN_POINT('Ctrl Pts',(-19.7139686478329,-84.239482884453,
63.829686404028));
#180433=CARTESIAN_POINT('Ctrl Pts',(-19.6245936478329,-80.982140009367,
61.43583617042));
#180434=CARTESIAN_POINT('Ctrl Pts',(-19.5352186478319,-77.147262939005,
60.15735325081));
#180435=CARTESIAN_POINT('Ctrl Pts',(-19.4458436478319,-73.105080577911,
60.11767060096));
#180436=CARTESIAN_POINT('Ctrl Pts',(-19.3564686478319,-69.245846259876,
61.32060370107));
#180437=CARTESIAN_POINT('Ctrl Pts',(-19.2670936478319,-65.94211166667,63.650075845204));
#180438=CARTESIAN_POINT('Ctrl Pts',(-19.2075103144989,-64.32266745252,65.804008650901));
#180439=CARTESIAN_POINT('Ctrl Pts',(-19.1777186478319,-63.6977213899,66.979361250291));
#180440=CARTESIAN_POINT('Ctrl Pts',(-25.0545366173959,-75.4572485563053,
59.89500391474));
#180441=CARTESIAN_POINT('Ctrl Pts',(-25.0247449507299,-74.0955822183551,
59.84745347843));
#180442=CARTESIAN_POINT('Ctrl Pts',(-24.9651616173959,-71.357545302109,
60.18062740255));
#180443=CARTESIAN_POINT('Ctrl Pts',(-24.8757866173959,-67.601945364152,
61.91693136384));
#180444=CARTESIAN_POINT('Ctrl Pts',(-24.7864116173959,-64.56063017797,64.722158934074));
#180445=CARTESIAN_POINT('Ctrl Pts',(-24.6970366173959,-62.52715042104,68.325482238879));
#180446=CARTESIAN_POINT('Ctrl Pts',(-24.6076616173959,-61.69784272518,72.379025712351));
#180447=CARTESIAN_POINT('Ctrl Pts',(-24.5182866173959,-62.15276622603,76.491447312794));
#180448=CARTESIAN_POINT('Ctrl Pts',(-24.4289116173959,-63.84800247215,80.265720932952));
#180449=CARTESIAN_POINT('Ctrl Pts',(-24.3395366173959,-66.619887661413,
83.33746628068));
#180450=CARTESIAN_POINT('Ctrl Pts',(-24.2501616173959,-70.200815347859,
85.41012737455));
#180451=CARTESIAN_POINT('Ctrl Pts',(-24.1607866173959,-74.2450714527985,
86.28360297416));
#180452=CARTESIAN_POINT('Ctrl Pts',(-24.0714116173959,-78.362210742274,
85.87356499026));
#180453=CARTESIAN_POINT('Ctrl Pts',(-23.9820366173959,-82.154751601322,
84.21959978308));
#180454=CARTESIAN_POINT('Ctrl Pts',(-23.8926616173959,-85.25655017356,81.481386370637));
#180455=CARTESIAN_POINT('Ctrl Pts',(-23.8032866173959,-87.3681490411,77.923280512555));
#180456=CARTESIAN_POINT('Ctrl Pts',(-23.7139116173959,-88.28568778894,73.8887929712528));
#180457=CARTESIAN_POINT('Ctrl Pts',(-23.6245366173959,-87.92058433229,69.767425899435));
#180458=CARTESIAN_POINT('Ctrl Pts',(-23.5351616173959,-86.30808691046,65.957069073716));
#180459=CARTESIAN_POINT('Ctrl Pts',(-23.4457866173959,-83.603871110638,
62.82558636057));
#180460=CARTESIAN_POINT('Ctrl Pts',(-23.3564116173959,-80.069010455704,
60.67530097837));
#180461=CARTESIAN_POINT('Ctrl Pts',(-23.2670366173959,-76.044771542844,
59.71380826027));
#180462=CARTESIAN_POINT('Ctrl Pts',(-23.1776616173959,-71.919667089848,
60.03393374599));
#180463=CARTESIAN_POINT('Ctrl Pts',(-23.0882866173959,-68.091947691899,
61.60477151142));
#180464=CARTESIAN_POINT('Ctrl Pts',(-22.9989116173959,-64.93115345296,64.274667923988));
#180465=CARTESIAN_POINT('Ctrl Pts',(-22.9095366173959,-62.74243741855,67.785862762707));
#180466=CARTESIAN_POINT('Ctrl Pts',(-22.8201616173959,-61.73710513821,71.799374202937));
#180467=CARTESIAN_POINT('Ctrl Pts',(-22.7307866173959,-62.01221456129,75.927725190932));
#180468=CARTESIAN_POINT('Ctrl Pts',(-22.6414116173959,-63.54120575633,79.77235170078));
#180469=CARTESIAN_POINT('Ctrl Pts',(-22.5520366173959,-66.176465090666,
82.962081362607));
#180470=CARTESIAN_POINT('Ctrl Pts',(-22.4626616173959,-69.663576316097,
85.1889676139));
#180471=CARTESIAN_POINT('Ctrl Pts',(-22.3732866173959,-73.665882715971,
86.23801983199));
#180472=CARTESIAN_POINT('Ctrl Pts',(-22.2839116173959,-77.796989006481,
86.00795920683));
#180473=CARTESIAN_POINT('Ctrl Pts',(-22.1945366173959,-81.65806515612,84.52099651684));
#180474=CARTESIAN_POINT('Ctrl Pts',(-22.1051616173959,-84.876350694903,
81.920687830243));
#180475=CARTESIAN_POINT('Ctrl Pts',(-22.0157866173959,-87.14114218589,78.458075149464));
#180476=CARTESIAN_POINT('Ctrl Pts',(-21.9264116173959,-88.233789515,74.467450024384));
#180477=CARTESIAN_POINT('Ctrl Pts',(-21.8370366173959,-88.04880506268,70.334079991696));
#180478=CARTESIAN_POINT('Ctrl Pts',(-21.7476616173959,-86.60404781143,66.457013631716));
#180479=CARTESIAN_POINT('Ctrl Pts',(-21.6582866173959,-84.038999183303,
63.210555159771));
#180480=CARTESIAN_POINT('Ctrl Pts',(-21.5689116173959,-80.601297063461,
60.90812791663));
#180481=CARTESIAN_POINT('Ctrl Pts',(-21.4795366173959,-76.622828057659,
59.7720154906));
#180482=CARTESIAN_POINT('Ctrl Pts',(-21.3901616173959,-72.487686112493,
59.91190175878));
#180483=CARTESIAN_POINT('Ctrl Pts',(-21.3007866173969,-68.595090874297,
61.31428165962));
#180484=CARTESIAN_POINT('Ctrl Pts',(-21.2114116173969,-65.320845765281,
63.843765014137));
#180485=CARTESIAN_POINT('Ctrl Pts',(-21.1220366173969,-62.9810567358,67.256147520865));
#180486=CARTESIAN_POINT('Ctrl Pts',(-21.0326616173969,-61.80161439886,71.22198700936));
#180487=CARTESIAN_POINT('Ctrl Pts',(-20.9432866173969,-61.89638583783,75.358408826466));
#180488=CARTESIAN_POINT('Ctrl Pts',(-20.8539116173969,-63.25622151907,79.266069762973));
#180489=CARTESIAN_POINT('Ctrl Pts',(-20.7645366173969,-65.74983861675,82.567711906636));
#180490=CARTESIAN_POINT('Ctrl Pts',(-20.6751616173969,-69.136495470965,
84.94458431096));
#180491=CARTESIAN_POINT('Ctrl Pts',(-20.5857866173969,-73.089233546913,
86.16721621697));
#180492=CARTESIAN_POINT('Ctrl Pts',(-20.4964116173969,-77.226443043123,
86.11757088408));
#180493=CARTESIAN_POINT('Ctrl Pts',(-20.4070366173969,-81.148704705378,
84.80044122928));
#180494=CARTESIAN_POINT('Ctrl Pts',(-20.3176616173969,-84.477351021258,
82.34298710401));
#180495=CARTESIAN_POINT('Ctrl Pts',(-20.2282866173969,-86.89102397653,78.982458880342));
#180496=CARTESIAN_POINT('Ctrl Pts',(-20.1389116173969,-88.15669997012,75.043292554251));
#180497=CARTESIAN_POINT('Ctrl Pts',(-20.0495366173969,-88.15218665258,70.905787661752));
#180498=CARTESIAN_POINT('Ctrl Pts',(-19.9601616173959,-86.87791974211,66.969391997631));
#180499=CARTESIAN_POINT('Ctrl Pts',(-19.8707866173959,-84.456921029265,
63.614137533019));
#180500=CARTESIAN_POINT('Ctrl Pts',(-19.7814116173959,-81.122921202634,
61.16395142431));
#180501=CARTESIAN_POINT('Ctrl Pts',(-19.6920366173959,-77.19779573134,59.85538121976));
#180502=CARTESIAN_POINT('Ctrl Pts',(-19.6026616173959,-73.060486332881,
59.81476469495));
#180503=CARTESIAN_POINT('Ctrl Pts',(-19.5132866173959,-69.110430400585,
61.04600712199));
#180504=CARTESIAN_POINT('Ctrl Pts',(-19.4239116173959,-65.728947092448,
63.430300094054));
#180505=CARTESIAN_POINT('Ctrl Pts',(-19.3643282840629,-64.07139155217,65.634922657953));
#180506=CARTESIAN_POINT('Ctrl Pts',(-19.3345366173959,-63.431738269,66.837935516246));
#180507=CARTESIAN_POINT('Ctrl Pts',(-19.0011309998534,-67.124599619487,
63.6058883503008));
#180508=CARTESIAN_POINT('Ctrl Pts',(-19.0704950559586,-67.0389239813991,
63.5038382415724));
#180509=CARTESIAN_POINT('Ctrl Pts',(-19.1398591185752,-66.95324791439,63.4017884768216));
#180510=CARTESIAN_POINT('Ctrl Pts',(-19.2784798392654,-66.7820276024722,
63.197847668815));
#180511=CARTESIAN_POINT('Ctrl Pts',(-19.3477365383098,-66.6964833082578,
63.0959565641899));
#180512=CARTESIAN_POINT('Ctrl Pts',(-19.4169932345698,-66.6109385987686,
62.9940658153934));
#180513=CARTESIAN_POINT('',(-24.5011471556111,-70.8102632894868,61.4776867539786));
#180514=CARTESIAN_POINT('Ctrl Pts',(-18.9799062324529,-67.340715181151,
63.474668109995));
#180515=CARTESIAN_POINT('Ctrl Pts',(-18.9294356932999,-65.751498900725,
64.932060456454));
#180516=CARTESIAN_POINT('Ctrl Pts',(-18.8284946149979,-63.4247304556,68.654743887637));
#180517=CARTESIAN_POINT('Ctrl Pts',(-18.7275535366989,-63.30638992216,72.8921974616309));
#180518=CARTESIAN_POINT('Ctrl Pts',(-18.6770829975479,-63.77070234627,74.847875926051));
#180519=CARTESIAN_POINT('Ctrl Pts',(-19.1367242020169,-67.151809631229,
63.240013146138));
#180520=CARTESIAN_POINT('Ctrl Pts',(-19.0862536628639,-65.521252914769,
64.730686006568));
#180521=CARTESIAN_POINT('Ctrl Pts',(-18.9853125845619,-63.12987316536,68.542252716656));
#180522=CARTESIAN_POINT('Ctrl Pts',(-18.8843715062629,-63.00052245572,72.8890389661518));
#180523=CARTESIAN_POINT('Ctrl Pts',(-18.8339009671119,-63.47350284263,74.897076676965));
#180524=CARTESIAN_POINT('Ctrl Pts',(-19.2935421715809,-66.962904081306,
63.005358182281));
#180525=CARTESIAN_POINT('Ctrl Pts',(-19.2430716324269,-65.291006928818,
64.529311556686));
#180526=CARTESIAN_POINT('Ctrl Pts',(-19.1421305541259,-62.83501587512,68.429761545683));
#180527=CARTESIAN_POINT('Ctrl Pts',(-19.0411894758269,-62.6946549893,72.8858804706761));
#180528=CARTESIAN_POINT('Ctrl Pts',(-18.9907189366759,-63.176303339,74.94627742788));
#180529=CARTESIAN_POINT('Ctrl Pts',(-19.4503601411449,-66.773998531384,
62.77070321842));
#180530=CARTESIAN_POINT('Ctrl Pts',(-19.3998896019909,-65.060760942862,
64.327937106799));
#180531=CARTESIAN_POINT('Ctrl Pts',(-19.2989485236899,-62.54015858487,68.317270374702));
#180532=CARTESIAN_POINT('Ctrl Pts',(-19.1980074453909,-62.38878752287,72.8827219751971));
#180533=CARTESIAN_POINT('Ctrl Pts',(-19.1475369062399,-62.87910383536,74.995478178794));
#180534=CARTESIAN_POINT('Ctrl Pts',(-19.4175174361239,-66.6110703651319,
62.9926155500965));
#180535=CARTESIAN_POINT('Ctrl Pts',(-19.4032204672389,-66.137812315149,
63.4414112721957));
#180536=CARTESIAN_POINT('Ctrl Pts',(-19.3888608262407,-65.6990094831001,
63.9263196278806));
#180537=CARTESIAN_POINT('Ctrl Pts',(-19.3744395805111,-65.2989377577199,
64.4413732029171));
#180538=CARTESIAN_POINT('Ctrl Pts',(-19.3705423958786,-65.190822730123,
64.580560823402));
#180539=CARTESIAN_POINT('Ctrl Pts',(-19.3666407123033,-65.0855363738124,
64.7219496850546));
#180540=CARTESIAN_POINT('Ctrl Pts',(-19.3627345508503,-64.9831634543278,
64.8654214859086));
#180541=CARTESIAN_POINT('Ctrl Pts',(-19.3583084311856,-64.8671634380688,
65.0279911509681));
#180542=CARTESIAN_POINT('Ctrl Pts',(-19.3538768656123,-64.7549293313154,
65.1931996793288));
#180543=CARTESIAN_POINT('Ctrl Pts',(-19.3494392777582,-64.6465764817334,
65.3608767801899));
#180544=CARTESIAN_POINT('Ctrl Pts',(-19.3423986111131,-64.4746641007192,
65.6269128813334));
#180545=CARTESIAN_POINT('Ctrl Pts',(-19.3353359681682,-64.3125383180186,
65.8991738812957));
#180546=CARTESIAN_POINT('Ctrl Pts',(-19.3282589746446,-64.1606418137509,
66.1769664936579));
#180547=CARTESIAN_POINT('Ctrl Pts',(-19.321308349306,-64.0114576032676,
66.4497987866271));
#180548=CARTESIAN_POINT('Ctrl Pts',(-19.3143438813066,-63.8721403447319,
66.7279675738643));
#180549=CARTESIAN_POINT('Ctrl Pts',(-19.3073727951192,-63.7431498331095,
67.0108436589339));
#180550=CARTESIAN_POINT('Ctrl Pts',(-19.2983245975766,-63.5757251880965,
67.3780057666716));
#180551=CARTESIAN_POINT('Ctrl Pts',(-19.289246402415,-63.4254515690211,
67.7536630696148));
#180552=CARTESIAN_POINT('Ctrl Pts',(-19.2801213645055,-63.2937354273005,
68.136063387383));
#180553=CARTESIAN_POINT('Ctrl Pts',(-19.2782027682036,-63.2660412845564,
68.2164654462903));
#180554=CARTESIAN_POINT('Ctrl Pts',(-19.2762821010918,-63.2391674508634,
68.297165429793));
#180555=CARTESIAN_POINT('Ctrl Pts',(-19.2743592065957,-63.2131268729228,
68.3781467925786));
#180556=CARTESIAN_POINT('Ctrl Pts',(-19.2735558745621,-63.2022478410906,
68.4119785618106));
#180557=CARTESIAN_POINT('Ctrl Pts',(-19.272751612069,-63.1915151897248,
68.445859771803));
#180558=CARTESIAN_POINT('Ctrl Pts',(-19.2719468277686,-63.180929072759,
68.4797889760641));
#180559=CARTESIAN_POINT('Ctrl Pts',(-19.2713566720993,-63.1731661766147,
68.5046695710727));
#180560=CARTESIAN_POINT('Ctrl Pts',(-19.270766235899,-63.1654820780196,
68.5295759752021));
#180561=CARTESIAN_POINT('Ctrl Pts',(-19.2701755446975,-63.1578768357417,
68.5545076247395));
#180562=CARTESIAN_POINT('Ctrl Pts',(-19.2583305133496,-63.0053701910583,
69.0544578010007));
#180563=CARTESIAN_POINT('Ctrl Pts',(-19.2464062952225,-62.8846459609022,
69.5643192941634));
#180564=CARTESIAN_POINT('Ctrl Pts',(-19.2344955395952,-62.7961070134394,
70.0794616457634));
#180565=CARTESIAN_POINT('Ctrl Pts',(-19.2255648541586,-62.7297205041846,
70.4657154185047));
#180566=CARTESIAN_POINT('Ctrl Pts',(-19.2166306713089,-62.6813849908161,
70.8551919742191));
#180567=CARTESIAN_POINT('Ctrl Pts',(-19.2076647208652,-62.6513402357164,
71.2459541183865));
#180568=CARTESIAN_POINT('Ctrl Pts',(-19.2044523919758,-62.6405757735006,
71.3859567352259));
#180569=CARTESIAN_POINT('Ctrl Pts',(-19.2012374970565,-62.6321654850941,
71.5260384699883));
#180570=CARTESIAN_POINT('Ctrl Pts',(-19.1980166927661,-62.6261114628072,
71.666139079149));
#180571=CARTESIAN_POINT('Ctrl Pts',(-19.1933795896618,-62.6173952779637,
71.8678467617854));
#180572=CARTESIAN_POINT('Ctrl Pts',(-19.1887351237908,-62.6135660108167,
72.0695940567608));
#180573=CARTESIAN_POINT('Ctrl Pts',(-19.1840873605703,-62.6145893742609,
72.2711996352988));
#180574=CARTESIAN_POINT('Ctrl Pts',(-19.1794322607379,-62.6156143531102,
72.4731234533451));
#180575=CARTESIAN_POINT('Ctrl Pts',(-19.174773853138,-62.6215072801478,
72.6749059000198));
#180576=CARTESIAN_POINT('Ctrl Pts',(-19.1701162224702,-62.6322855183008,
72.8763672965785));
#180577=CARTESIAN_POINT('Ctrl Pts',(-19.1691220913338,-62.6345860403706,
72.9193674959065));
#180578=CARTESIAN_POINT('Ctrl Pts',(-19.1681279955922,-62.6371093117162,
72.9623530532898));
#180579=CARTESIAN_POINT('Ctrl Pts',(-19.1671339749643,-62.6398558076609,
73.00532218268));
#180580=CARTESIAN_POINT('Ctrl Pts',(-19.164564094539,-62.6469564310972,
73.1164119542729));
#180581=CARTESIAN_POINT('Ctrl Pts',(-19.1619911494633,-62.6555521718381,
73.227443772742));
#180582=CARTESIAN_POINT('Ctrl Pts',(-19.1594114054907,-62.6656570955864,
73.3383711450185));
#180583=CARTESIAN_POINT('Ctrl Pts',(-19.1547191646527,-62.6840367240996,
73.5401345571109));
#180584=CARTESIAN_POINT('Ctrl Pts',(-19.1500219576314,-62.7073564942426,
73.741558755367));
#180585=CARTESIAN_POINT('Ctrl Pts',(-19.1453140801805,-62.7357018617097,
73.9423640348264));
#180586=CARTESIAN_POINT('Ctrl Pts',(-19.1406652548524,-62.7636916859117,
74.1406505618012));
#180587=CARTESIAN_POINT('Ctrl Pts',(-19.1360060250999,-62.7965818773787,
74.3383335923708));
#180588=CARTESIAN_POINT('Ctrl Pts',(-19.1313308986451,-62.8344042122621,
74.5351501297222));
#180589=CARTESIAN_POINT('Ctrl Pts',(-19.1296852922034,-62.8477173661469,
74.6044279481571));
#180590=CARTESIAN_POINT('Ctrl Pts',(-19.1280377161879,-62.8616411390047,
74.6735984677276));
#180591=CARTESIAN_POINT('Ctrl Pts',(-19.1263879310737,-62.8761753834789,
74.7426504105179));
#180592=CARTESIAN_POINT('Ctrl Pts',(-19.7210834129279,-66.6679911229052,
62.9389668654546));
#180593=CARTESIAN_POINT('Ctrl Pts',(-19.0031848503602,-66.6679911229052,
62.9389668654546));
#180594=CARTESIAN_POINT('Ctrl Pts',(-19.7210834129279,-65.8978577481411,
63.6603901351978));
#180595=CARTESIAN_POINT('Ctrl Pts',(-19.0031848503602,-65.8978577481411,
63.6603901351978));
#180596=CARTESIAN_POINT('Ctrl Pts',(-19.7210834129279,-65.2182108438486,
64.4762669802466));
#180597=CARTESIAN_POINT('Ctrl Pts',(-19.0031848503602,-65.2182108438486,
64.4762669802466));
#180598=CARTESIAN_POINT('Ctrl Pts',(-19.7210834129279,-64.0409039909203,
66.2981609192099));
#180599=CARTESIAN_POINT('Ctrl Pts',(-19.0031848503602,-64.0409039909203,
66.2981609192099));
#180600=CARTESIAN_POINT('Ctrl Pts',(-19.7210834129279,-63.5546993668503,
67.315919751713));
#180601=CARTESIAN_POINT('Ctrl Pts',(-19.0031848503602,-63.5546993668503,
67.315919751713));
#180602=CARTESIAN_POINT('Ctrl Pts',(-19.7210834129279,-62.8715543789953,
69.4403738334441));
#180603=CARTESIAN_POINT('Ctrl Pts',(-19.0031848503602,-62.8715543789953,
69.4403738334441));
#180604=CARTESIAN_POINT('Ctrl Pts',(-19.7210834129279,-62.6742843975167,
70.5513335535036));
#180605=CARTESIAN_POINT('Ctrl Pts',(-19.0031848503602,-62.6742843975167,
70.5513335535036));
#180606=CARTESIAN_POINT('Ctrl Pts',(-19.7210834129279,-62.6020249954524,
72.2235418419717));
#180607=CARTESIAN_POINT('Ctrl Pts',(-19.0031848503602,-62.6020249954524,
72.2235418419717));
#180608=CARTESIAN_POINT('Ctrl Pts',(-19.7210834129279,-62.6151667392939,
72.7841104016103));
#180609=CARTESIAN_POINT('Ctrl Pts',(-19.0031848503602,-62.6151667392939,
72.7841104016103));
#180610=CARTESIAN_POINT('Ctrl Pts',(-19.7210834129279,-62.7109382443801,
73.8354475183249));
#180611=CARTESIAN_POINT('Ctrl Pts',(-19.0031848503602,-62.7109382443801,
73.8354475183249));
#180612=CARTESIAN_POINT('Ctrl Pts',(-19.7210834129279,-62.7860260362546,
74.3287972481997));
#180613=CARTESIAN_POINT('Ctrl Pts',(-19.0031848503602,-62.7860260362546,
74.3287972481997));
#180614=CARTESIAN_POINT('Ctrl Pts',(-19.7210834129279,-62.8923404913652,
74.8182427933889));
#180615=CARTESIAN_POINT('Ctrl Pts',(-19.0031848503602,-62.8923404913652,
74.8182427933889));
#180616=CARTESIAN_POINT('Ctrl Pts',(-19.7175219896827,-66.6111698442287,
62.9925212140073));
#180617=CARTESIAN_POINT('Ctrl Pts',(-19.7032357686158,-66.1380399280067,
63.4411857890246));
#180618=CARTESIAN_POINT('Ctrl Pts',(-19.6888822186527,-65.6993452916874,
63.9259433661227));
#180619=CARTESIAN_POINT('Ctrl Pts',(-19.6744617213196,-65.2993581486053,
64.4408320198377));
#180620=CARTESIAN_POINT('Ctrl Pts',(-19.6707792859395,-65.1972169551887,
64.5723145999073));
#180621=CARTESIAN_POINT('Ctrl Pts',(-19.6670924849657,-65.0976000062359,
64.7057617926725));
#180622=CARTESIAN_POINT('Ctrl Pts',(-19.6634013247513,-65.0005787608751,
64.8410738773966));
#180623=CARTESIAN_POINT('Ctrl Pts',(-19.6587526282975,-64.8783889091588,
65.0114877234196));
#180624=CARTESIAN_POINT('Ctrl Pts',(-19.6540986130407,-64.7603437515763,
65.1848208107002));
#180625=CARTESIAN_POINT('Ctrl Pts',(-19.6494392777599,-64.6465764817334,
65.3608767801898));
#180626=CARTESIAN_POINT('Ctrl Pts',(-19.6424230631589,-64.47526114775,65.6259889451786));
#180627=CARTESIAN_POINT('Ctrl Pts',(-19.6354021244996,-64.3136622764933,
65.8972863128408));
#180628=CARTESIAN_POINT('Ctrl Pts',(-19.6283648699486,-64.1622176497922,
66.1740854297641));
#180629=CARTESIAN_POINT('Ctrl Pts',(-19.6218433853392,-64.0218726054223,
66.4305975635544));
#180630=CARTESIAN_POINT('Ctrl Pts',(-19.6153078888229,-63.890248024282,
66.6918353088826));
#180631=CARTESIAN_POINT('Ctrl Pts',(-19.6087491550728,-63.7677253476843,
66.9572772307433));
#180632=CARTESIAN_POINT('Ctrl Pts',(-19.5999665130658,-63.603658189708,
67.3127240993296));
#180633=CARTESIAN_POINT('Ctrl Pts',(-19.5911412884054,-63.4558274535676,
67.675916413523));
#180634=CARTESIAN_POINT('Ctrl Pts',(-19.5822984309671,-63.3254298288066,
68.0451907172391));
#180635=CARTESIAN_POINT('Ctrl Pts',(-19.579653377898,-63.2864256223057,
68.1556471095548));
#180636=CARTESIAN_POINT('Ctrl Pts',(-19.5770067472021,-63.248980887577,
68.2666474635449));
#180637=CARTESIAN_POINT('Ctrl Pts',(-19.5743592065984,-63.2131268729228,
68.3781467925786));
#180638=CARTESIAN_POINT('Ctrl Pts',(-19.5735592697391,-63.2022938198484,
68.4118355764103));
#180639=CARTESIAN_POINT('Ctrl Pts',(-19.5727597867005,-63.1916069219557,
68.4455702452619));
#180640=CARTESIAN_POINT('Ctrl Pts',(-19.571960356956,-63.1810662645877,
68.4793492961659));
#180641=CARTESIAN_POINT('Ctrl Pts',(-19.5719568884247,-63.1810205312371,
68.4794958552583));
#180642=CARTESIAN_POINT('Ctrl Pts',(-19.5719534198934,-63.1809748006275,
68.4796424152244));
#180643=CARTESIAN_POINT('Ctrl Pts',(-19.5719499513622,-63.180929072759,
68.4797889760641));
#180644=CARTESIAN_POINT('Ctrl Pts',(-19.5599906187491,-63.0232615305662,
68.9851238653065));
#180645=CARTESIAN_POINT('Ctrl Pts',(-19.5480134164975,-62.8981803811709,
69.5008432106857));
#180646=CARTESIAN_POINT('Ctrl Pts',(-19.5359444704607,-62.806096716665,
70.0221345398778));
#180647=CARTESIAN_POINT('Ctrl Pts',(-19.5269013179855,-62.7370992568977,
70.4127334338935));
#180648=CARTESIAN_POINT('Ctrl Pts',(-19.5178062838736,-62.6865819724355,
70.8067205289833));
#180649=CARTESIAN_POINT('Ctrl Pts',(-19.5086971906096,-62.6547902527515,
71.2020880584462));
#180650=CARTESIAN_POINT('Ctrl Pts',(-19.5051350676615,-62.6423580587926,
71.3566970528696));
#180651=CARTESIAN_POINT('Ctrl Pts',(-19.5015738726351,-62.6327977573663,
71.511406589515));
#180652=CARTESIAN_POINT('Ctrl Pts',(-19.4980166927664,-62.6261114628072,
71.666139079149));
#180653=CARTESIAN_POINT('Ctrl Pts',(-19.4934105162437,-62.6174534094732,
71.8665014975118));
#180654=CARTESIAN_POINT('Ctrl Pts',(-19.4888065269332,-62.6136172626764,
72.066902646066));
#180655=CARTESIAN_POINT('Ctrl Pts',(-19.4841972065762,-62.6145695759266,
72.2671719933078));
#180656=CARTESIAN_POINT('Ctrl Pts',(-19.47958119344,-62.6155232719451,72.4677321336441));
#180657=CARTESIAN_POINT('Ctrl Pts',(-19.4749598337646,-62.6212793300511,
72.6681608772637));
#180658=CARTESIAN_POINT('Ctrl Pts',(-19.4703255764941,-62.6318559717216,
72.8682892798221));
#180659=CARTESIAN_POINT('Ctrl Pts',(-19.4694361642215,-62.6338858536111,
72.9066981654189));
#180660=CARTESIAN_POINT('Ctrl Pts',(-19.4685462768821,-62.6360934491295,
72.9450959748758));
#180661=CARTESIAN_POINT('Ctrl Pts',(-19.4676558610962,-62.6384791059619,
72.9834814859481));
#180662=CARTESIAN_POINT('Ctrl Pts',(-19.4649097591887,-62.64583663138,73.1018649724439));
#180663=CARTESIAN_POINT('Ctrl Pts',(-19.4621600849288,-62.6548904472578,
73.2201796537156));
#180664=CARTESIAN_POINT('Ctrl Pts',(-19.4594114054906,-62.6656570955864,
73.3383711450185));
#180665=CARTESIAN_POINT('Ctrl Pts',(-19.45468344815,-62.6841766265629,73.5416703443179));
#180666=CARTESIAN_POINT('Ctrl Pts',(-19.4499407562387,-62.7077104077423,
73.7446106609183));
#180667=CARTESIAN_POINT('Ctrl Pts',(-19.4451892350923,-62.7363450659676,
73.9469144504096));
#180668=CARTESIAN_POINT('Ctrl Pts',(-19.4404973026351,-62.7646206177726,
74.1466811539297));
#180669=CARTESIAN_POINT('Ctrl Pts',(-19.4357967610085,-62.7978699633399,
74.3458271887682));
#180670=CARTESIAN_POINT('Ctrl Pts',(-19.4310932961469,-62.8361259933756,
74.5440915419424));
#180671=CARTESIAN_POINT('Ctrl Pts',(-19.4295207442363,-62.848916477603,
74.6103790547806));
#180672=CARTESIAN_POINT('Ctrl Pts',(-19.4279478655588,-62.8622661963166,
74.676568064179));
#180673=CARTESIAN_POINT('Ctrl Pts',(-19.4263748726167,-62.8761750818273,
74.7426489773759));
#180674=CARTESIAN_POINT('Ctrl Pts',(-19.6963598728939,-66.773998531384,
62.77070321842));
#180675=CARTESIAN_POINT('Ctrl Pts',(-19.6458893337409,-65.060760942862,
64.327937106799));
#180676=CARTESIAN_POINT('Ctrl Pts',(-19.5449482554399,-62.54015858487,68.317270374702));
#180677=CARTESIAN_POINT('Ctrl Pts',(-19.4440071771409,-62.38878752287,72.8827219751971));
#180678=CARTESIAN_POINT('Ctrl Pts',(-19.3935366379889,-62.87910383536,74.995478178794));
#180679=CARTESIAN_POINT('Ctrl Pts',(-19.8531778424579,-66.962904081306,
63.005358182281));
#180680=CARTESIAN_POINT('Ctrl Pts',(-19.8027073033049,-65.291006928818,
64.529311556686));
#180681=CARTESIAN_POINT('Ctrl Pts',(-19.7017662250039,-62.83501587512,68.429761545683));
#180682=CARTESIAN_POINT('Ctrl Pts',(-19.6008251467039,-62.6946549893,72.8858804706761));
#180683=CARTESIAN_POINT('Ctrl Pts',(-19.5503546075529,-63.176303339,74.94627742788));
#180684=CARTESIAN_POINT('Ctrl Pts',(-20.0099958120219,-67.151809631229,
63.240013146138));
#180685=CARTESIAN_POINT('Ctrl Pts',(-19.9595252728689,-65.521252914769,
64.730686006568));
#180686=CARTESIAN_POINT('Ctrl Pts',(-19.8585841945679,-63.12987316536,68.542252716656));
#180687=CARTESIAN_POINT('Ctrl Pts',(-19.7576431162679,-63.00052245572,72.8890389661519));
#180688=CARTESIAN_POINT('Ctrl Pts',(-19.7071725771169,-63.47350284263,74.897076676965));
#180689=CARTESIAN_POINT('Ctrl Pts',(-20.1668137815859,-67.340715181151,
63.474668109995));
#180690=CARTESIAN_POINT('Ctrl Pts',(-20.1163432424329,-65.751498900725,
64.932060456454));
#180691=CARTESIAN_POINT('Ctrl Pts',(-20.0154021641319,-63.4247304556,68.654743887637));
#180692=CARTESIAN_POINT('Ctrl Pts',(-19.9144610858319,-63.30638992216,72.8921974616309));
#180693=CARTESIAN_POINT('Ctrl Pts',(-19.8639905466809,-63.77070234627,74.847875926051));
#180694=CARTESIAN_POINT('Ctrl Pts',(-19.7180890220136,-66.6111095357772,
62.994139891927));
#180695=CARTESIAN_POINT('Ctrl Pts',(-19.7872818346883,-66.6965738631944,
63.0959358861211));
#180696=CARTESIAN_POINT('Ctrl Pts',(-19.8564746631046,-66.7820377913851,
63.1977322539828));
#180697=CARTESIAN_POINT('Ctrl Pts',(-19.9950718525411,-66.9532260839772,
63.4016368988591));
#180698=CARTESIAN_POINT('Ctrl Pts',(-20.0644762246894,-67.038950459557,
63.5037451943941));
#180699=CARTESIAN_POINT('Ctrl Pts',(-20.1338805884022,-67.1246744025685,
63.6058538308434));
#180700=CARTESIAN_POINT('Ctrl Pts',(-25.3005363491459,-75.4572485563053,
59.89500391474));
#180701=CARTESIAN_POINT('Ctrl Pts',(-25.2707446824789,-74.0955822183551,
59.84745347843));
#180702=CARTESIAN_POINT('Ctrl Pts',(-25.2111613491459,-71.357545302109,
60.18062740255));
#180703=CARTESIAN_POINT('Ctrl Pts',(-25.1217863491459,-67.601945364152,
61.91693136384));
#180704=CARTESIAN_POINT('Ctrl Pts',(-25.0324113491459,-64.56063017797,64.722158934074));
#180705=CARTESIAN_POINT('Ctrl Pts',(-24.9430363491459,-62.52715042104,68.325482238879));
#180706=CARTESIAN_POINT('Ctrl Pts',(-24.8536613491459,-61.69784272518,72.3790257123511));
#180707=CARTESIAN_POINT('Ctrl Pts',(-24.7642863491459,-62.15276622603,76.491447312794));
#180708=CARTESIAN_POINT('Ctrl Pts',(-24.6749113491459,-63.84800247215,80.265720932952));
#180709=CARTESIAN_POINT('Ctrl Pts',(-24.5855363491449,-66.619887661413,
83.33746628068));
#180710=CARTESIAN_POINT('Ctrl Pts',(-24.4961613491449,-70.200815347859,
85.41012737455));
#180711=CARTESIAN_POINT('Ctrl Pts',(-24.4067863491449,-74.2450714527984,
86.28360297416));
#180712=CARTESIAN_POINT('Ctrl Pts',(-24.3174113491449,-78.362210742274,
85.87356499026));
#180713=CARTESIAN_POINT('Ctrl Pts',(-24.2280363491449,-82.154751601322,
84.21959978308));
#180714=CARTESIAN_POINT('Ctrl Pts',(-24.1386613491449,-85.25655017356,81.481386370637));
#180715=CARTESIAN_POINT('Ctrl Pts',(-24.0492863491449,-87.3681490411,77.923280512555));
#180716=CARTESIAN_POINT('Ctrl Pts',(-23.9599113491449,-88.28568778894,73.8887929712529));
#180717=CARTESIAN_POINT('Ctrl Pts',(-23.8705363491449,-87.92058433229,69.767425899435));
#180718=CARTESIAN_POINT('Ctrl Pts',(-23.7811613491449,-86.30808691046,65.957069073716));
#180719=CARTESIAN_POINT('Ctrl Pts',(-23.6917863491449,-83.603871110638,
62.82558636057));
#180720=CARTESIAN_POINT('Ctrl Pts',(-23.6024113491449,-80.069010455704,
60.67530097837));
#180721=CARTESIAN_POINT('Ctrl Pts',(-23.5130363491449,-76.044771542844,
59.71380826027));
#180722=CARTESIAN_POINT('Ctrl Pts',(-23.4236613491449,-71.919667089848,
60.03393374599));
#180723=CARTESIAN_POINT('Ctrl Pts',(-23.3342863491449,-68.091947691899,
61.60477151142));
#180724=CARTESIAN_POINT('Ctrl Pts',(-23.2449113491459,-64.93115345296,64.274667923988));
#180725=CARTESIAN_POINT('Ctrl Pts',(-23.1555363491459,-62.74243741855,67.785862762707));
#180726=CARTESIAN_POINT('Ctrl Pts',(-23.0661613491459,-61.73710513821,71.799374202937));
#180727=CARTESIAN_POINT('Ctrl Pts',(-22.9767863491459,-62.01221456129,75.927725190932));
#180728=CARTESIAN_POINT('Ctrl Pts',(-22.8874113491459,-63.54120575633,79.77235170078));
#180729=CARTESIAN_POINT('Ctrl Pts',(-22.7980363491459,-66.176465090666,
82.962081362607));
#180730=CARTESIAN_POINT('Ctrl Pts',(-22.7086613491459,-69.663576316097,
85.1889676139));
#180731=CARTESIAN_POINT('Ctrl Pts',(-22.6192863491459,-73.665882715971,
86.23801983199));
#180732=CARTESIAN_POINT('Ctrl Pts',(-22.5299113491459,-77.796989006481,
86.00795920683));
#180733=CARTESIAN_POINT('Ctrl Pts',(-22.4405363491459,-81.65806515612,84.52099651684));
#180734=CARTESIAN_POINT('Ctrl Pts',(-22.3511613491459,-84.876350694903,
81.920687830243));
#180735=CARTESIAN_POINT('Ctrl Pts',(-22.2617863491459,-87.14114218589,78.458075149464));
#180736=CARTESIAN_POINT('Ctrl Pts',(-22.1724113491459,-88.233789515,74.467450024384));
#180737=CARTESIAN_POINT('Ctrl Pts',(-22.0830363491459,-88.04880506268,70.334079991696));
#180738=CARTESIAN_POINT('Ctrl Pts',(-21.9936613491459,-86.60404781143,66.457013631716));
#180739=CARTESIAN_POINT('Ctrl Pts',(-21.9042863491459,-84.038999183303,
63.210555159771));
#180740=CARTESIAN_POINT('Ctrl Pts',(-21.8149113491459,-80.601297063461,
60.90812791663));
#180741=CARTESIAN_POINT('Ctrl Pts',(-21.7255363491459,-76.622828057659,
59.7720154906));
#180742=CARTESIAN_POINT('Ctrl Pts',(-21.6361613491459,-72.487686112493,
59.91190175878));
#180743=CARTESIAN_POINT('Ctrl Pts',(-21.5467863491459,-68.595090874297,
61.31428165962));
#180744=CARTESIAN_POINT('Ctrl Pts',(-21.4574113491459,-65.320845765281,
63.843765014137));
#180745=CARTESIAN_POINT('Ctrl Pts',(-21.3680363491459,-62.9810567358,67.256147520865));
#180746=CARTESIAN_POINT('Ctrl Pts',(-21.2786613491459,-61.80161439886,71.22198700936));
#180747=CARTESIAN_POINT('Ctrl Pts',(-21.1892863491459,-61.89638583783,75.358408826466));
#180748=CARTESIAN_POINT('Ctrl Pts',(-21.0999113491459,-63.25622151907,79.266069762973));
#180749=CARTESIAN_POINT('Ctrl Pts',(-21.0105363491459,-65.74983861675,82.567711906636));
#180750=CARTESIAN_POINT('Ctrl Pts',(-20.9211613491459,-69.136495470965,
84.94458431096));
#180751=CARTESIAN_POINT('Ctrl Pts',(-20.8317863491459,-73.089233546913,
86.16721621697));
#180752=CARTESIAN_POINT('Ctrl Pts',(-20.7424113491459,-77.226443043123,
86.11757088408));
#180753=CARTESIAN_POINT('Ctrl Pts',(-20.6530363491459,-81.148704705378,
84.80044122928));
#180754=CARTESIAN_POINT('Ctrl Pts',(-20.5636613491459,-84.477351021258,
82.34298710401));
#180755=CARTESIAN_POINT('Ctrl Pts',(-20.4742863491459,-86.89102397653,78.982458880342));
#180756=CARTESIAN_POINT('Ctrl Pts',(-20.3849113491459,-88.15669997012,75.043292554251));
#180757=CARTESIAN_POINT('Ctrl Pts',(-20.2955363491459,-88.15218665258,70.905787661752));
#180758=CARTESIAN_POINT('Ctrl Pts',(-20.2061613491459,-86.87791974211,66.969391997631));
#180759=CARTESIAN_POINT('Ctrl Pts',(-20.1167863491459,-84.456921029265,
63.614137533019));
#180760=CARTESIAN_POINT('Ctrl Pts',(-20.0274113491459,-81.122921202634,
61.16395142431));
#180761=CARTESIAN_POINT('Ctrl Pts',(-19.9380363491459,-77.19779573134,59.85538121976));
#180762=CARTESIAN_POINT('Ctrl Pts',(-19.8486613491459,-73.060486332881,
59.81476469495));
#180763=CARTESIAN_POINT('Ctrl Pts',(-19.7592863491459,-69.110430400585,
61.04600712199));
#180764=CARTESIAN_POINT('Ctrl Pts',(-19.6699113491459,-65.728947092449,
63.430300094054));
#180765=CARTESIAN_POINT('Ctrl Pts',(-19.6103280158119,-64.07139155217,65.634922657953));
#180766=CARTESIAN_POINT('Ctrl Pts',(-19.5805363491459,-63.431738269,66.837935516246));
#180767=CARTESIAN_POINT('Ctrl Pts',(-25.4573543187099,-75.4467352742876,
60.19606492144));
#180768=CARTESIAN_POINT('Ctrl Pts',(-25.4275626520429,-74.1163770334926,
60.14960778797));
#180769=CARTESIAN_POINT('Ctrl Pts',(-25.3679793187099,-71.441294398629,
60.47512121458));
#180770=CARTESIAN_POINT('Ctrl Pts',(-25.2786043187099,-67.772045047785,
62.1715032276));
#180771=CARTESIAN_POINT('Ctrl Pts',(-25.1892293187099,-64.80065726501,64.912231636138));
#180772=CARTESIAN_POINT('Ctrl Pts',(-25.0998543187099,-62.81393226732,68.432705572515));
#180773=CARTESIAN_POINT('Ctrl Pts',(-25.0104793187089,-62.00369241884,72.393047995661));
#180774=CARTESIAN_POINT('Ctrl Pts',(-24.9211043187089,-62.44815609648,76.41091479114));
#180775=CARTESIAN_POINT('Ctrl Pts',(-24.8317293187089,-64.10441464328,80.098408469768));
#180776=CARTESIAN_POINT('Ctrl Pts',(-24.7423543187089,-66.812567295151,
83.09952674895));
#180777=CARTESIAN_POINT('Ctrl Pts',(-24.6529793187089,-70.311160544158,
85.12453220716));
#180778=CARTESIAN_POINT('Ctrl Pts',(-24.5636043187089,-74.2624291384832,
85.97792442938));
#180779=CARTESIAN_POINT('Ctrl Pts',(-24.4742293187089,-78.284905151586,
85.57731423897));
#180780=CARTESIAN_POINT('Ctrl Pts',(-24.3848543187089,-81.99024605983,83.96137780724));
#180781=CARTESIAN_POINT('Ctrl Pts',(-24.2954793187089,-85.02072656512,81.286122734268));
#180782=CARTESIAN_POINT('Ctrl Pts',(-24.2061043187089,-87.08377452069,77.809826583006));
#180783=CARTESIAN_POINT('Ctrl Pts',(-24.1167293187089,-87.98021676974,73.8681019487348));
#180784=CARTESIAN_POINT('Ctrl Pts',(-24.0273543187089,-87.62350794999,69.841495360525));
#180785=CARTESIAN_POINT('Ctrl Pts',(-23.9379793187089,-86.04808585604,66.118748119013));
#180786=CARTESIAN_POINT('Ctrl Pts',(-23.8486043187089,-83.406046705982,
63.059265985079));
#180787=CARTESIAN_POINT('Ctrl Pts',(-23.7592293187089,-79.952461292809,
60.95842101407));
#180788=CARTESIAN_POINT('Ctrl Pts',(-23.6698543187089,-76.020749645512,
60.01903540591));
#180789=CARTESIAN_POINT('Ctrl Pts',(-23.5804793187089,-71.990491607817,
60.33180041019));
#180790=CARTESIAN_POINT('Ctrl Pts',(-23.4911043187089,-68.250781002811,
61.8665207069));
#180791=CARTESIAN_POINT('Ctrl Pts',(-23.4017293187089,-65.162661287992,
64.475029557805));
#180792=CARTESIAN_POINT('Ctrl Pts',(-23.3123543187089,-63.02426928109,67.905493290763));
#180793=CARTESIAN_POINT('Ctrl Pts',(-23.2229793187089,-62.04205209131,71.826724116717));
#180794=CARTESIAN_POINT('Ctrl Pts',(-23.1336043187099,-62.31083606423,75.860154043494));
#180795=CARTESIAN_POINT('Ctrl Pts',(-23.0442293187099,-63.80467194732,79.616383023829));
#180796=CARTESIAN_POINT('Ctrl Pts',(-22.9548543187099,-66.379340112614,
82.732772864167));
#180797=CARTESIAN_POINT('Ctrl Pts',(-22.8654793187099,-69.786273974476,
84.90845745969));
#180798=CARTESIAN_POINT('Ctrl Pts',(-22.7761043187099,-73.696557391833,
85.93338935707));
#180799=CARTESIAN_POINT('Ctrl Pts',(-22.6867293187099,-77.732679269865,
85.70861839811));
#180800=CARTESIAN_POINT('Ctrl Pts',(-22.5973543187099,-81.504979671842,
84.25584468017));
#180801=CARTESIAN_POINT('Ctrl Pts',(-22.5079793187099,-84.649268818474,
81.715323560263));
#180802=CARTESIAN_POINT('Ctrl Pts',(-22.4186043187099,-86.86198711791,78.332324960555));
#180803=CARTESIAN_POINT('Ctrl Pts',(-22.3292293187099,-87.92951176624,74.43345423642));
#180804=CARTESIAN_POINT('Ctrl Pts',(-22.2398543187099,-87.74878056675,70.395120665275));
#180805=CARTESIAN_POINT('Ctrl Pts',(-22.1504793187099,-86.3372418795,66.607197707679));
#180806=CARTESIAN_POINT('Ctrl Pts',(-22.0611043187099,-83.831170101586,
63.435383393718));
#180807=CARTESIAN_POINT('Ctrl Pts',(-21.9717293187099,-80.472509307037,
61.18589468171));
#180808=CARTESIAN_POINT('Ctrl Pts',(-21.8823543187099,-76.585515202752,
60.07590430719));
#180809=CARTESIAN_POINT('Ctrl Pts',(-21.7929793187099,-72.545450459805,
60.212574242));
#180810=CARTESIAN_POINT('Ctrl Pts',(-21.7036043187099,-68.742355671542,
61.58270993957));
#180811=CARTESIAN_POINT('Ctrl Pts',(-21.6142293187099,-65.543393604434,
64.054034178009));
#180812=CARTESIAN_POINT('Ctrl Pts',(-21.5248543187099,-63.25740214652,67.387957520349));
#180813=CARTESIAN_POINT('Ctrl Pts',(-21.4354793187099,-62.10507812355,71.262612491355));
#180814=CARTESIAN_POINT('Ctrl Pts',(-21.3461043187099,-62.19767053133,75.3039276788));
#180815=CARTESIAN_POINT('Ctrl Pts',(-21.2567293187099,-63.52624020677,79.121741767484));
#180816=CARTESIAN_POINT('Ctrl Pts',(-21.1673543187099,-65.96252284285,82.347470943245));
#180817=CARTESIAN_POINT('Ctrl Pts',(-21.0779793187099,-69.271312029438,
84.66969313695));
#180818=CARTESIAN_POINT('Ctrl Pts',(-20.9886043187099,-73.133166821969,
85.86421369334));
#180819=CARTESIAN_POINT('Ctrl Pts',(-20.8992293187099,-77.175251577815,
85.81570983017));
#180820=CARTESIAN_POINT('Ctrl Pts',(-20.8098543187099,-81.007330685234,
84.52886426336));
#180821=CARTESIAN_POINT('Ctrl Pts',(-20.7204793187099,-84.259443140101,
82.127913122978));
#180822=CARTESIAN_POINT('Ctrl Pts',(-20.6311043187099,-86.61761974852,78.844651804709));
#180823=CARTESIAN_POINT('Ctrl Pts',(-20.5417293187099,-87.85419470181,74.996056713737));
#180824=CARTESIAN_POINT('Ctrl Pts',(-20.4523543187099,-87.84978515668,70.953683353497));
#180825=CARTESIAN_POINT('Ctrl Pts',(-20.3629793187099,-86.60481681305,67.107795220083));
#180826=CARTESIAN_POINT('Ctrl Pts',(-20.2736043187099,-84.239482884453,
63.829686404028));
#180827=CARTESIAN_POINT('Ctrl Pts',(-20.1842293187099,-80.982140009367,
61.43583617042));
#180828=CARTESIAN_POINT('Ctrl Pts',(-20.0948543187099,-77.147262939005,
60.15735325081));
#180829=CARTESIAN_POINT('Ctrl Pts',(-20.0054793187099,-73.105080577911,
60.11767060096));
#180830=CARTESIAN_POINT('Ctrl Pts',(-19.9161043187099,-69.245846259876,
61.32060370107));
#180831=CARTESIAN_POINT('Ctrl Pts',(-19.8267293187099,-65.942111666671,
63.650075845203));
#180832=CARTESIAN_POINT('Ctrl Pts',(-19.7671459853759,-64.32266745252,65.804008650901));
#180833=CARTESIAN_POINT('Ctrl Pts',(-19.7373543187099,-63.6977213899,66.979361250291));
#180834=CARTESIAN_POINT('Ctrl Pts',(-25.6141722882739,-75.4362219922699,
60.49712592814));
#180835=CARTESIAN_POINT('Ctrl Pts',(-25.5843806216069,-74.1371718486303,
60.45176209751));
#180836=CARTESIAN_POINT('Ctrl Pts',(-25.5247972882739,-71.52504349515,60.76961502662));
#180837=CARTESIAN_POINT('Ctrl Pts',(-25.4354222882739,-67.942144731418,
62.42607509136));
#180838=CARTESIAN_POINT('Ctrl Pts',(-25.3460472882739,-65.04068435206,65.102304338201));
#180839=CARTESIAN_POINT('Ctrl Pts',(-25.2566722882729,-63.10071411361,68.539928906151));
#180840=CARTESIAN_POINT('Ctrl Pts',(-25.1672972882729,-62.3095421125,72.4070702789702));
#180841=CARTESIAN_POINT('Ctrl Pts',(-25.0779222882729,-62.74354596694,76.330382269486));
#180842=CARTESIAN_POINT('Ctrl Pts',(-24.9885472882729,-64.36082681442,79.931096006583));
#180843=CARTESIAN_POINT('Ctrl Pts',(-24.8991722882729,-67.005246928886,
82.861587217225));
#180844=CARTESIAN_POINT('Ctrl Pts',(-24.8097972882729,-70.421505740455,
84.83893703977));
#180845=CARTESIAN_POINT('Ctrl Pts',(-24.7204222882729,-74.2797868241642,
85.67224588461));
#180846=CARTESIAN_POINT('Ctrl Pts',(-24.6310472882729,-78.207599560894,
85.28106348769));
#180847=CARTESIAN_POINT('Ctrl Pts',(-24.5416722882729,-81.825740518334,
83.70315583141));
#180848=CARTESIAN_POINT('Ctrl Pts',(-24.4522972882729,-84.784902956671,
81.090859097905));
#180849=CARTESIAN_POINT('Ctrl Pts',(-24.3629222882729,-86.79940000028,77.696372653464));
#180850=CARTESIAN_POINT('Ctrl Pts',(-24.2735472882729,-87.67474575053,73.8474109262254));
#180851=CARTESIAN_POINT('Ctrl Pts',(-24.1841722882729,-87.32643156769,69.915564821625));
#180852=CARTESIAN_POINT('Ctrl Pts',(-24.0947972882729,-85.78808480163,66.280427164319));
#180853=CARTESIAN_POINT('Ctrl Pts',(-24.0054222882729,-83.208222301336,
63.292945609594));
#180854=CARTESIAN_POINT('Ctrl Pts',(-23.9160472882729,-79.835912129926,
61.24154104977));
#180855=CARTESIAN_POINT('Ctrl Pts',(-23.8266722882729,-75.9967277481948,
60.32426255155));
#180856=CARTESIAN_POINT('Ctrl Pts',(-23.7372972882729,-72.061316125801,
60.62966707439));
#180857=CARTESIAN_POINT('Ctrl Pts',(-23.6479222882729,-68.409614313737,
62.12826990236));
#180858=CARTESIAN_POINT('Ctrl Pts',(-23.5585472882729,-65.394169123036,
64.675391191609));
#180859=CARTESIAN_POINT('Ctrl Pts',(-23.4691722882729,-63.30610114364,68.0251238188));
#180860=CARTESIAN_POINT('Ctrl Pts',(-23.3797972882729,-62.34699904441,71.854074030477));
#180861=CARTESIAN_POINT('Ctrl Pts',(-23.2904222882729,-62.60945756717,75.792582896034));
#180862=CARTESIAN_POINT('Ctrl Pts',(-23.2010472882729,-64.06813813831,79.460414346857));
#180863=CARTESIAN_POINT('Ctrl Pts',(-23.1116722882729,-66.582215134543,
82.503464365711));
#180864=CARTESIAN_POINT('Ctrl Pts',(-23.0222972882739,-69.908971632833,
84.62794730547));
#180865=CARTESIAN_POINT('Ctrl Pts',(-22.9329222882739,-73.727232067669,
85.62875888215));
#180866=CARTESIAN_POINT('Ctrl Pts',(-22.8435472882739,-77.668369533221,
85.4092775894));
#180867=CARTESIAN_POINT('Ctrl Pts',(-22.7541722882739,-81.351894187539,
83.99069284351));
#180868=CARTESIAN_POINT('Ctrl Pts',(-22.6647972882739,-84.422186942024,
81.509959290305));
#180869=CARTESIAN_POINT('Ctrl Pts',(-22.5754222882739,-86.58283204993,78.206574771673));
#180870=CARTESIAN_POINT('Ctrl Pts',(-22.4860472882739,-87.62523401748,74.399458448487));
#180871=CARTESIAN_POINT('Ctrl Pts',(-22.3966722882739,-87.44875607083,70.456161338886));
#180872=CARTESIAN_POINT('Ctrl Pts',(-22.3072972882739,-86.07043594758,66.757381783671));
#180873=CARTESIAN_POINT('Ctrl Pts',(-22.2179222882739,-83.623341019893,
63.660211627688));
#180874=CARTESIAN_POINT('Ctrl Pts',(-22.1285472882739,-80.343721550643,
61.4636614468));
#180875=CARTESIAN_POINT('Ctrl Pts',(-22.0391722882739,-76.548202347877,
60.37979312378));
#180876=CARTESIAN_POINT('Ctrl Pts',(-21.9497972882739,-72.603214807152,
60.51324672522));
#180877=CARTESIAN_POINT('Ctrl Pts',(-21.8604222882739,-68.889620468817,
61.85113821951));
#180878=CARTESIAN_POINT('Ctrl Pts',(-21.7710472882739,-65.765941443611,
64.264303341857));
#180879=CARTESIAN_POINT('Ctrl Pts',(-21.6816722882739,-63.53374755725,67.519767519802));
#180880=CARTESIAN_POINT('Ctrl Pts',(-21.5922972882739,-62.40854184824,71.303237973316));
#180881=CARTESIAN_POINT('Ctrl Pts',(-21.5029222882739,-62.49895522482,75.2494465311));
#180882=CARTESIAN_POINT('Ctrl Pts',(-21.4135472882739,-63.79625889445,78.977413771966));
#180883=CARTESIAN_POINT('Ctrl Pts',(-21.3241722882739,-66.175207068926,
82.127229979831));
#180884=CARTESIAN_POINT('Ctrl Pts',(-21.2347972882739,-69.406128587882,
84.39480196293));
#180885=CARTESIAN_POINT('Ctrl Pts',(-21.1454222882739,-73.177100096994,
85.5612111697));
#180886=CARTESIAN_POINT('Ctrl Pts',(-21.0560472882739,-77.124060112478,
85.51384877627));
#180887=CARTESIAN_POINT('Ctrl Pts',(-20.9666722882739,-80.865956665065,
84.25728729746));
#180888=CARTESIAN_POINT('Ctrl Pts',(-20.8772972882739,-84.041535258926,
81.912839141965));
#180889=CARTESIAN_POINT('Ctrl Pts',(-20.7879222882739,-86.34421552051,78.706844729098));
#180890=CARTESIAN_POINT('Ctrl Pts',(-20.6985472882739,-87.5516894335,74.948820873245));
#180891=CARTESIAN_POINT('Ctrl Pts',(-20.6091722882739,-87.54738366077,71.001579045262));
#180892=CARTESIAN_POINT('Ctrl Pts',(-20.5197972882739,-86.331713884,67.246198442551));
#180893=CARTESIAN_POINT('Ctrl Pts',(-20.4304222882739,-84.022044739653,
64.045235275048));
#180894=CARTESIAN_POINT('Ctrl Pts',(-20.3410472882739,-80.841358816111,
61.70772091653));
#180895=CARTESIAN_POINT('Ctrl Pts',(-20.2516722882739,-77.096730146679,
60.45932528185));
#180896=CARTESIAN_POINT('Ctrl Pts',(-20.1622972882739,-73.149674822947,
60.42057650697));
#180897=CARTESIAN_POINT('Ctrl Pts',(-20.0729222882739,-69.381262119169,
61.59520028015));
#180898=CARTESIAN_POINT('Ctrl Pts',(-19.9835472882739,-66.155276240892,
63.869851596353));
#180899=CARTESIAN_POINT('Ctrl Pts',(-19.9239639549399,-64.57394335288,65.973094643852));
#180900=CARTESIAN_POINT('Ctrl Pts',(-19.8941722882739,-63.9637045108,67.120786984341));
#180901=CARTESIAN_POINT('Ctrl Pts',(-25.7709902578379,-75.4257087102522,
60.79818693484));
#180902=CARTESIAN_POINT('Ctrl Pts',(-25.7411985911709,-74.1579666637678,
60.75391640706));
#180903=CARTESIAN_POINT('Ctrl Pts',(-25.6816152578379,-71.60879259167,61.06410883866));
#180904=CARTESIAN_POINT('Ctrl Pts',(-25.5922402578369,-68.112244415052,
62.68064695513));
#180905=CARTESIAN_POINT('Ctrl Pts',(-25.5028652578369,-65.280711439107,
65.292377040265));
#180906=CARTESIAN_POINT('Ctrl Pts',(-25.4134902578369,-63.38749595989,68.647152239787));
#180907=CARTESIAN_POINT('Ctrl Pts',(-25.3241152578369,-62.61539180617,72.4210925622802));
#180908=CARTESIAN_POINT('Ctrl Pts',(-25.2347402578369,-63.0389358374,76.249849747832));
#180909=CARTESIAN_POINT('Ctrl Pts',(-25.1453652578369,-64.61723898556,79.7637835434));
#180910=CARTESIAN_POINT('Ctrl Pts',(-25.0559902578369,-67.197926562624,
82.623647685499));
#180911=CARTESIAN_POINT('Ctrl Pts',(-24.9666152578369,-70.531850936755,
84.55334187238));
#180912=CARTESIAN_POINT('Ctrl Pts',(-24.8772402578369,-74.297144509849,
85.36656733984));
#180913=CARTESIAN_POINT('Ctrl Pts',(-24.7878652578369,-78.130293970206,
84.98481273641));
#180914=CARTESIAN_POINT('Ctrl Pts',(-24.6984902578369,-81.661234976842,
83.44493385557));
#180915=CARTESIAN_POINT('Ctrl Pts',(-24.6091152578369,-84.549079348228,
80.895595461536));
#180916=CARTESIAN_POINT('Ctrl Pts',(-24.5197402578369,-86.51502547987,77.582918723914));
#180917=CARTESIAN_POINT('Ctrl Pts',(-24.4303652578369,-87.36927473133,73.8267199037072));
#180918=CARTESIAN_POINT('Ctrl Pts',(-24.3409902578369,-87.02935518539,69.989634282714));
#180919=CARTESIAN_POINT('Ctrl Pts',(-24.2516152578369,-85.52808374721,66.442106209615));
#180920=CARTESIAN_POINT('Ctrl Pts',(-24.1622402578369,-83.01039789668,63.526625234101));
#180921=CARTESIAN_POINT('Ctrl Pts',(-24.0728652578369,-79.719362967031,
61.52466108548));
#180922=CARTESIAN_POINT('Ctrl Pts',(-23.9834902578369,-75.9727058508626,
60.62948969719));
#180923=CARTESIAN_POINT('Ctrl Pts',(-23.8941152578369,-72.132140643769,
60.92753373859));
#180924=CARTESIAN_POINT('Ctrl Pts',(-23.8047402578369,-68.568447624649,
62.39001909784));
#180925=CARTESIAN_POINT('Ctrl Pts',(-23.7153652578369,-65.625676958068,
64.875752825426));
#180926=CARTESIAN_POINT('Ctrl Pts',(-23.6259902578369,-63.58793300618,68.144754346856));
#180927=CARTESIAN_POINT('Ctrl Pts',(-23.5366152578369,-62.65194599751,71.881423944257));
#180928=CARTESIAN_POINT('Ctrl Pts',(-23.4472402578369,-62.90807907012,75.725011748597));
#180929=CARTESIAN_POINT('Ctrl Pts',(-23.3578652578369,-64.3316043293,79.304445669906));
#180930=CARTESIAN_POINT('Ctrl Pts',(-23.2684902578369,-66.785090156491,
82.274155867272));
#180931=CARTESIAN_POINT('Ctrl Pts',(-23.1791152578369,-70.031669291213,
84.34743715126));
#180932=CARTESIAN_POINT('Ctrl Pts',(-23.0897402578369,-73.757906743531,
85.32412840723));
#180933=CARTESIAN_POINT('Ctrl Pts',(-23.0003652578379,-77.604059796605,
85.10993678068));
#180934=CARTESIAN_POINT('Ctrl Pts',(-22.9109902578379,-81.198808703261,
83.72554100684));
#180935=CARTESIAN_POINT('Ctrl Pts',(-22.8216152578379,-84.195105065595,
81.304595020325));
#180936=CARTESIAN_POINT('Ctrl Pts',(-22.7322402578379,-86.30367698195,78.080824582763));
#180937=CARTESIAN_POINT('Ctrl Pts',(-22.6428652578379,-87.32095626873,74.365462660522));
#180938=CARTESIAN_POINT('Ctrl Pts',(-22.5534902578379,-87.1487315749,70.517202012466));
#180939=CARTESIAN_POINT('Ctrl Pts',(-22.4641152578379,-85.80363001565,66.907565859634));
#180940=CARTESIAN_POINT('Ctrl Pts',(-22.3747402578379,-83.415511938176,
63.885039861635));
#180941=CARTESIAN_POINT('Ctrl Pts',(-22.2853652578379,-80.214933794219,
61.74142821188));
#180942=CARTESIAN_POINT('Ctrl Pts',(-22.1959902578379,-76.510889492969,
60.68368194036));
#180943=CARTESIAN_POINT('Ctrl Pts',(-22.1066152578379,-72.660979154464,
60.81391920844));
#180944=CARTESIAN_POINT('Ctrl Pts',(-22.0172402578379,-69.036885266062,
62.11956649947));
#180945=CARTESIAN_POINT('Ctrl Pts',(-21.9278652578379,-65.988489282763,
64.474572505729));
#180946=CARTESIAN_POINT('Ctrl Pts',(-21.8384902578379,-63.81009296796,67.651577519286));
#180947=CARTESIAN_POINT('Ctrl Pts',(-21.7491152578379,-62.71200557292,71.343863455311));
#180948=CARTESIAN_POINT('Ctrl Pts',(-21.6597402578379,-62.80023991832,75.194965383434));
#180949=CARTESIAN_POINT('Ctrl Pts',(-21.5703652578379,-64.06627758214,78.833085776477));
#180950=CARTESIAN_POINT('Ctrl Pts',(-21.4809902578379,-66.387891295025,
81.90698901644));
#180951=CARTESIAN_POINT('Ctrl Pts',(-21.3916152578379,-69.540945146354,
84.11991078892));
#180952=CARTESIAN_POINT('Ctrl Pts',(-21.3022402578379,-73.22103337205,85.25820864606));
#180953=CARTESIAN_POINT('Ctrl Pts',(-21.2128652578379,-77.07286864717,85.21198772236));
#180954=CARTESIAN_POINT('Ctrl Pts',(-21.1234902578379,-80.72458264492,83.98571033155));
#180955=CARTESIAN_POINT('Ctrl Pts',(-21.0341152578379,-83.823627377769,
81.697765160933));
#180956=CARTESIAN_POINT('Ctrl Pts',(-20.9447402578379,-86.0708112925,78.569037653464));
#180957=CARTESIAN_POINT('Ctrl Pts',(-20.8553652578379,-87.24918416519,74.90158503273));
#180958=CARTESIAN_POINT('Ctrl Pts',(-20.7659902578379,-87.24498216486,71.049474737007));
#180959=CARTESIAN_POINT('Ctrl Pts',(-20.6766152578379,-86.05861095495,67.384601665003));
#180960=CARTESIAN_POINT('Ctrl Pts',(-20.5872402578379,-83.804606594842,
64.260784146057));
#180961=CARTESIAN_POINT('Ctrl Pts',(-20.4978652578379,-80.700577622844,
61.97960566264));
#180962=CARTESIAN_POINT('Ctrl Pts',(-20.4084902578379,-77.046197354344,
60.7612973129));
#180963=CARTESIAN_POINT('Ctrl Pts',(-20.3191152578379,-73.194269067977,
60.72348241298));
#180964=CARTESIAN_POINT('Ctrl Pts',(-20.2297402578379,-69.51667797846,61.86979685924));
#180965=CARTESIAN_POINT('Ctrl Pts',(-20.1403652578379,-66.368440815114,
64.089627347503));
#180966=CARTESIAN_POINT('Ctrl Pts',(-20.0807819245039,-64.82521925324,66.1421806368));
#180967=CARTESIAN_POINT('Ctrl Pts',(-20.0509902578369,-64.2296876317,67.262212718386));
#180968=CARTESIAN_POINT('Ctrl Pts',(-29.0130799422609,-77.577883154178,
84.91151378796));
#180969=CARTESIAN_POINT('Ctrl Pts',(-28.9648716383109,-79.584207200809,
84.47771089461));
#180970=CARTESIAN_POINT('Ctrl Pts',(-28.8684550304109,-83.370581098091,
82.576109782766));
#180971=CARTESIAN_POINT('Ctrl Pts',(-28.7238301185509,-86.96373593251,77.331337332641));
#180972=CARTESIAN_POINT('Ctrl Pts',(-28.5792052067009,-87.57149401059,71.003271823318));
#180973=CARTESIAN_POINT('Ctrl Pts',(-28.4345802948509,-85.04290088059,65.170572201634));
#180974=CARTESIAN_POINT('Ctrl Pts',(-28.2899553829909,-80.008640399699,
61.28849282187));
#180975=CARTESIAN_POINT('Ctrl Pts',(-28.1453304711409,-73.724771677726,
60.32557309628));
#180976=CARTESIAN_POINT('Ctrl Pts',(-28.0007055592909,-67.759060181558,
62.52205714543));
#180977=CARTESIAN_POINT('Ctrl Pts',(-27.8560806474309,-63.59991002351,67.329937790089));
#180978=CARTESIAN_POINT('Ctrl Pts',(-27.7114557355809,-62.28499728294,73.5496847895006));
#180979=CARTESIAN_POINT('Ctrl Pts',(-27.5668308237209,-64.14238315408,79.629517497618));
#180980=CARTESIAN_POINT('Ctrl Pts',(-27.4222059118709,-68.708663616781,
84.05256291155));
#180981=CARTESIAN_POINT('Ctrl Pts',(-27.2775810000209,-74.8445856937055,
85.71530411088));
#180982=CARTESIAN_POINT('Ctrl Pts',(-27.1329560881609,-81.019282482511,
84.20289954075));
#180983=CARTESIAN_POINT('Ctrl Pts',(-26.9883311763109,-85.69221308489,79.892682886532));
#180984=CARTESIAN_POINT('Ctrl Pts',(-26.8437062644609,-87.69751608898,73.860021128897));
#180985=CARTESIAN_POINT('Ctrl Pts',(-26.6990813526009,-86.53488331788,67.610018484104));
#180986=CARTESIAN_POINT('Ctrl Pts',(-26.5544564407489,-82.494382996173,
62.70200410244));
#180987=CARTESIAN_POINT('Ctrl Pts',(-26.4098315288959,-76.58408988664,60.36049104895));
#180988=CARTESIAN_POINT('Ctrl Pts',(-26.2652066170419,-70.278578138388,
61.1696694061));
#180989=CARTESIAN_POINT('Ctrl Pts',(-26.1205817051879,-65.151026010211,
64.927655195095));
#180990=CARTESIAN_POINT('Ctrl Pts',(-25.9759567933349,-62.4807196002,70.696858927558));
#180991=CARTESIAN_POINT('Ctrl Pts',(-25.8313318814809,-62.93388049036,77.037907200944));
#180992=CARTESIAN_POINT('Ctrl Pts',(-25.6867069696279,-66.397448396289,
82.368755669438));
#180993=CARTESIAN_POINT('Ctrl Pts',(-25.5420820577749,-72.007288953952,
85.35939726776));
#180994=CARTESIAN_POINT('Ctrl Pts',(-25.3974571459209,-78.363788487576,
85.26368932913));
#180995=CARTESIAN_POINT('Ctrl Pts',(-25.2528322340679,-83.881048421187,
82.105509685936));
#180996=CARTESIAN_POINT('Ctrl Pts',(-25.1082073222149,-87.18255063842,76.672802844726));
#180997=CARTESIAN_POINT('Ctrl Pts',(-24.9635824103609,-87.44460542796,70.320980571748));
#180998=CARTESIAN_POINT('Ctrl Pts',(-24.8189574985079,-84.601792795156,
64.634805721403));
#180999=CARTESIAN_POINT('Ctrl Pts',(-24.6743325866549,-79.363519912305,
61.03282290959));
#181000=CARTESIAN_POINT('Ctrl Pts',(-24.5297076748019,-73.036149856491,
60.4141243606));
#181001=CARTESIAN_POINT('Ctrl Pts',(-24.4332910668999,-69.145620553249,
62.092366244));
#181002=CARTESIAN_POINT('Ctrl Pts',(-24.3850827629489,-67.523679930053,
63.350471861665));
#181003=CARTESIAN_POINT('Ctrl Pts',(-29.1698979118309,-77.641546433683,
85.2059543519));
#181004=CARTESIAN_POINT('Ctrl Pts',(-29.1216896078809,-79.697418563341,
84.76143828298));
#181005=CARTESIAN_POINT('Ctrl Pts',(-29.0252729999709,-83.57730056992,82.812875320713));
#181006=CARTESIAN_POINT('Ctrl Pts',(-28.8806480881209,-87.25919178487,77.438578220143));
#181007=CARTESIAN_POINT('Ctrl Pts',(-28.7360231762609,-87.88195902748,70.954235106618));
#181008=CARTESIAN_POINT('Ctrl Pts',(-28.5913982644109,-85.29091988206,64.977491413082));
#181009=CARTESIAN_POINT('Ctrl Pts',(-28.4467733525609,-80.132333544284,
60.99954038599));
#181010=CARTESIAN_POINT('Ctrl Pts',(-28.3021484407009,-73.693278699863,
60.01284044075));
#181011=CARTESIAN_POINT('Ctrl Pts',(-28.1575235288509,-67.580238276931,
62.26356875528));
#181012=CARTESIAN_POINT('Ctrl Pts',(-28.0128986170009,-63.31837394482,67.190184591183));
#181013=CARTESIAN_POINT('Ctrl Pts',(-27.8682737051409,-61.97098818188,73.5635341660382));
#181014=CARTESIAN_POINT('Ctrl Pts',(-27.7236487932909,-63.87424396596,79.793514132931));
#181015=CARTESIAN_POINT('Ctrl Pts',(-27.5790238814309,-68.553293073323,
84.32579086559));
#181016=CARTESIAN_POINT('Ctrl Pts',(-27.4343989695809,-74.8407475894004,
86.02959504233));
#181017=CARTESIAN_POINT('Ctrl Pts',(-27.2897740577309,-81.167934395797,
84.47984020103));
#181018=CARTESIAN_POINT('Ctrl Pts',(-27.1451491458709,-85.95626746961,80.063178641754));
#181019=CARTESIAN_POINT('Ctrl Pts',(-27.0005242340209,-88.01109334111,73.8815345568893));
#181020=CARTESIAN_POINT('Ctrl Pts',(-26.8558993221709,-86.81974824651,67.477182144676));
#181021=CARTESIAN_POINT('Ctrl Pts',(-26.7112744103109,-82.679463921444,
62.44795967377));
#181022=CARTESIAN_POINT('Ctrl Pts',(-26.5666494984599,-76.623210494983,
60.04862072552));
#181023=CARTESIAN_POINT('Ctrl Pts',(-26.4220245866059,-70.161978129137,
60.87778251281));
#181024=CARTESIAN_POINT('Ctrl Pts',(-26.2773996747519,-64.907796218,64.728575339723));
#181025=CARTESIAN_POINT('Ctrl Pts',(-26.1327747628989,-62.17154404815,70.640255052583));
#181026=CARTESIAN_POINT('Ctrl Pts',(-25.9881498510449,-62.63589617806,77.137901551893));
#181027=CARTESIAN_POINT('Ctrl Pts',(-25.8435249391919,-66.185000191906,
82.600400400082));
#181028=CARTESIAN_POINT('Ctrl Pts',(-25.6989000273379,-71.933381104597,
85.66489874077));
#181029=CARTESIAN_POINT('Ctrl Pts',(-25.5542751154849,-78.446860447733,
85.56682720345));
#181030=CARTESIAN_POINT('Ctrl Pts',(-25.4096502036319,-84.100374369695,
82.330653306324));
#181031=CARTESIAN_POINT('Ctrl Pts',(-25.2650252917779,-87.48341032833,76.763780595904));
#181032=CARTESIAN_POINT('Ctrl Pts',(-25.1204003799249,-87.75193681046,70.25509402282));
#181033=CARTESIAN_POINT('Ctrl Pts',(-24.9757754680719,-84.838918212374,
64.428493669391));
#181034=CARTESIAN_POINT('Ctrl Pts',(-24.8311505562189,-79.471281192081,
60.73755646174));
#181035=CARTESIAN_POINT('Ctrl Pts',(-24.6865256443659,-72.98765070695,60.10357856287));
#181036=CARTESIAN_POINT('Ctrl Pts',(-24.5901090364639,-69.001041077471,
61.82326622784));
#181037=CARTESIAN_POINT('Ctrl Pts',(-24.5419007325129,-67.33904508595,63.112441961868));
#181038=CARTESIAN_POINT('Ctrl Pts',(-29.3267158813909,-77.705209713196,
85.50039491585));
#181039=CARTESIAN_POINT('Ctrl Pts',(-29.2785075774409,-79.810629925882,
85.04516567134));
#181040=CARTESIAN_POINT('Ctrl Pts',(-29.1820909695409,-83.784020041757,
83.04964085865));
#181041=CARTESIAN_POINT('Ctrl Pts',(-29.0374660576809,-87.55464763724,77.545819107633));
#181042=CARTESIAN_POINT('Ctrl Pts',(-28.8928411458309,-88.19242404437,70.905198389902));
#181043=CARTESIAN_POINT('Ctrl Pts',(-28.7482162339709,-85.53893888352,64.784410624515));
#181044=CARTESIAN_POINT('Ctrl Pts',(-28.6035913221209,-80.256026688849,
60.7105879501));
#181045=CARTESIAN_POINT('Ctrl Pts',(-28.4589664102709,-73.661785721975,
59.70010778522));
#181046=CARTESIAN_POINT('Ctrl Pts',(-28.3143414984109,-67.40141637228,62.00508036515));
#181047=CARTESIAN_POINT('Ctrl Pts',(-28.1697165865609,-63.03683786611,67.050431392305));
#181048=CARTESIAN_POINT('Ctrl Pts',(-28.0250916747109,-61.65697908082,73.5773835426106));
#181049=CARTESIAN_POINT('Ctrl Pts',(-27.8804667628509,-63.60610477786,79.957510768277));
#181050=CARTESIAN_POINT('Ctrl Pts',(-27.7358418510009,-68.3979225299,84.59901881965));
#181051=CARTESIAN_POINT('Ctrl Pts',(-27.5912169391409,-74.836909485138,
86.34388597378));
#181052=CARTESIAN_POINT('Ctrl Pts',(-27.4465920272909,-81.316586309122,
84.75678086128));
#181053=CARTESIAN_POINT('Ctrl Pts',(-27.3019671154409,-86.22032185435,80.233674396936));
#181054=CARTESIAN_POINT('Ctrl Pts',(-27.1573422035809,-88.32467059324,73.903047984833));
#181055=CARTESIAN_POINT('Ctrl Pts',(-27.0127172917309,-87.10461317512,67.344345805202));
#181056=CARTESIAN_POINT('Ctrl Pts',(-26.8680923798809,-82.864544846674,
62.19391524507));
#181057=CARTESIAN_POINT('Ctrl Pts',(-26.7234674680209,-76.662331103274,
59.73675040207));
#181058=CARTESIAN_POINT('Ctrl Pts',(-26.5788425561709,-70.045378119837,
60.58589561953));
#181059=CARTESIAN_POINT('Ctrl Pts',(-26.4342176443159,-64.66456642575,64.52949548439));
#181060=CARTESIAN_POINT('Ctrl Pts',(-26.2895927324629,-61.8623684961,70.583651177657));
#181061=CARTESIAN_POINT('Ctrl Pts',(-26.1449678206089,-62.33791186577,77.237895902889));
#181062=CARTESIAN_POINT('Ctrl Pts',(-26.0003429087559,-65.972551987557,
82.832045130756));
#181063=CARTESIAN_POINT('Ctrl Pts',(-25.8557179969019,-71.859473255285,
85.9704002138));
#181064=CARTESIAN_POINT('Ctrl Pts',(-25.7110930850489,-78.529932407928,
85.86996507777));
#181065=CARTESIAN_POINT('Ctrl Pts',(-25.5664681731959,-84.319700318228,
82.555796926686));
#181066=CARTESIAN_POINT('Ctrl Pts',(-25.4218432613419,-87.78427001824,76.854758347052));
#181067=CARTESIAN_POINT('Ctrl Pts',(-25.2772183494889,-88.05926819295,70.189207473868));
#181068=CARTESIAN_POINT('Ctrl Pts',(-25.1325934376359,-85.07604362958,64.222181617367));
#181069=CARTESIAN_POINT('Ctrl Pts',(-24.9879685257829,-79.579042471845,
60.44229001389));
#181070=CARTESIAN_POINT('Ctrl Pts',(-24.8433436139299,-72.939151557407,
59.79303276515));
#181071=CARTESIAN_POINT('Ctrl Pts',(-24.7469270060279,-68.856461601694,
61.55416621167));
#181072=CARTESIAN_POINT('Ctrl Pts',(-24.6987187020769,-67.154410241852,
62.87441206207));
#181073=CARTESIAN_POINT('Ctrl Pts',(-29.4835338509509,-77.7688729927,85.79483547979));
#181074=CARTESIAN_POINT('Ctrl Pts',(-29.4353255470009,-79.923841288414,
85.32889305971));
#181075=CARTESIAN_POINT('Ctrl Pts',(-29.3389089391009,-83.990739513586,
83.2864063966));
#181076=CARTESIAN_POINT('Ctrl Pts',(-29.1942840272509,-87.85010348959,77.653059995135));
#181077=CARTESIAN_POINT('Ctrl Pts',(-29.0496591153909,-88.50288906125,70.856161673202));
#181078=CARTESIAN_POINT('Ctrl Pts',(-28.9050342035409,-85.78695788499,64.591329835963));
#181079=CARTESIAN_POINT('Ctrl Pts',(-28.7604092916909,-80.379719833434,
60.42163551422));
#181080=CARTESIAN_POINT('Ctrl Pts',(-28.6157843798309,-73.630292744112,
59.38737512969));
#181081=CARTESIAN_POINT('Ctrl Pts',(-28.4711594679809,-67.222594467652,
61.74659197501));
#181082=CARTESIAN_POINT('Ctrl Pts',(-28.3265345561209,-62.75530178742,66.9106781934));
#181083=CARTESIAN_POINT('Ctrl Pts',(-28.1819096442709,-61.34296997975,73.5912329191485));
#181084=CARTESIAN_POINT('Ctrl Pts',(-28.0372847324209,-63.33796558974,80.12150740359));
#181085=CARTESIAN_POINT('Ctrl Pts',(-27.8926598205609,-68.242551986442,
84.87224677369));
#181086=CARTESIAN_POINT('Ctrl Pts',(-27.7480349087109,-74.8330713808332,
86.65817690523));
#181087=CARTESIAN_POINT('Ctrl Pts',(-27.6034099968509,-81.465238222408,
85.03372152155));
#181088=CARTESIAN_POINT('Ctrl Pts',(-27.4587850850009,-86.48437623907,80.404170152158));
#181089=CARTESIAN_POINT('Ctrl Pts',(-27.3141601731509,-88.63824784537,73.924561412825));
#181090=CARTESIAN_POINT('Ctrl Pts',(-27.1695352612909,-87.38947810375,67.211509465773));
#181091=CARTESIAN_POINT('Ctrl Pts',(-27.0249103494409,-83.049625771945,
61.9398708164));
#181092=CARTESIAN_POINT('Ctrl Pts',(-26.8802854375909,-76.701451711617,
59.42488007864));
#181093=CARTESIAN_POINT('Ctrl Pts',(-26.7356605257309,-69.928778110586,
60.29400872623));
#181094=CARTESIAN_POINT('Ctrl Pts',(-26.5910356138809,-64.42133663353,64.330415629018));
#181095=CARTESIAN_POINT('Ctrl Pts',(-26.4464107020269,-61.55319294406,70.527047302681));
#181096=CARTESIAN_POINT('Ctrl Pts',(-26.3017857901729,-62.03992755347,77.337890253839));
#181097=CARTESIAN_POINT('Ctrl Pts',(-26.1571608783199,-65.760103783174,
83.0636898614));
#181098=CARTESIAN_POINT('Ctrl Pts',(-26.0125359664659,-71.78556540593,86.27590168681));
#181099=CARTESIAN_POINT('Ctrl Pts',(-25.8679110546129,-78.613004368084,
86.17310295209));
#181100=CARTESIAN_POINT('Ctrl Pts',(-25.7232861427599,-84.539026266736,
82.780940547073));
#181101=CARTESIAN_POINT('Ctrl Pts',(-25.5786612309059,-88.08512970815,76.94573609823));
#181102=CARTESIAN_POINT('Ctrl Pts',(-25.4340363190529,-88.36659957545,70.12332092494));
#181103=CARTESIAN_POINT('Ctrl Pts',(-25.2894114071999,-85.3131690468,64.015869565355));
#181104=CARTESIAN_POINT('Ctrl Pts',(-25.1447864953469,-79.686803751621,
60.14702356604));
#181105=CARTESIAN_POINT('Ctrl Pts',(-25.0001615834929,-72.890652407866,
59.48248696742));
#181106=CARTESIAN_POINT('Ctrl Pts',(-24.9037449755909,-68.711882125916,
61.28506619551));
#181107=CARTESIAN_POINT('Ctrl Pts',(-24.8555366716399,-66.96977539775,62.63638216227));
#181108=CARTESIAN_POINT('Origin',(-18.5675364832709,-75.,72.98888938658));
#181109=CARTESIAN_POINT('Origin',(-16.5675364832709,-75.,72.98888938658));
#181110=CARTESIAN_POINT('',(0.,0.,0.));
#181111=CARTESIAN_POINT('Origin',(80.4848979285703,-6.7762635780344E-18,
101.037257330549));
#181112=CARTESIAN_POINT('',(78.7746251576811,2.44276330247173E-16,103.143297948862));
#181113=CARTESIAN_POINT('Origin',(80.7934810513561,-6.7762635780344E-18,
102.787319184645));
#181114=CARTESIAN_POINT('',(79.3342829232298,-6.7762635780344E-18,106.317274859827));
#181115=CARTESIAN_POINT('',(78.4660420348953,-2.57828857403242E-16,101.393236094766));
#181116=CARTESIAN_POINT('',(83.3719947105798,-2.57828857403242E-16,105.605317331393));
#181117=CARTESIAN_POINT('Origin',(81.3531388169048,-6.7762635780344E-18,
105.96129609561));
#181118=CARTESIAN_POINT('Origin',(81.3531388169048,-6.7762635780344E-18,
105.96129609561));
#181119=CARTESIAN_POINT('Origin',(81.3531388169048,-6.7762635780344E-18,
105.96129609561));
#181120=CARTESIAN_POINT('',(81.5670324381031,-6.7762635780344E-18,107.174347100844));
#181121=CARTESIAN_POINT('',(83.3719947105798,-2.57828857403242E-16,105.605317331393));
#181122=CARTESIAN_POINT('Origin',(83.3215010572291,0.,102.341561049839));
#181123=CARTESIAN_POINT('Origin',(76.0518331668413,7.15881389286582E-15,
75.8960977421633));
#181124=CARTESIAN_POINT('',(75.2620568904884,5.41644264137289,76.9170539108621));
#181125=CARTESIAN_POINT('',(75.2383357389536,5.41644264172234,76.7825245640101));
#181126=CARTESIAN_POINT('',(75.1112777726958,5.41644264156718,76.061943035002));
#181127=CARTESIAN_POINT('',(74.0817004664548,-5.09516704230596,76.6496559375717));
#181128=CARTESIAN_POINT('Ctrl Pts',(75.2620568894032,5.4164426411786,76.9170539110535));
#181129=CARTESIAN_POINT('Ctrl Pts',(75.2754748959648,5.4188551225797,76.9143605053861));
#181130=CARTESIAN_POINT('Ctrl Pts',(75.28890236133,5.42121578956793,76.9116672629974));
#181131=CARTESIAN_POINT('Ctrl Pts',(75.3498183865431,5.43168291146175,76.899457787892));
#181132=CARTESIAN_POINT('Ctrl Pts',(75.397407342647,5.43919276600061,76.8899439198397));
#181133=CARTESIAN_POINT('Ctrl Pts',(75.5691587465013,5.46389865606945,76.8556799658338));
#181134=CARTESIAN_POINT('Ctrl Pts',(75.6938224042956,5.47733403583914,76.8309446188927));
#181135=CARTESIAN_POINT('Ctrl Pts',(76.0833251774047,5.50537123701008,76.753856710618));
#181136=CARTESIAN_POINT('Ctrl Pts',(76.3488690788813,5.50451815465259,76.7015654343039));
#181137=CARTESIAN_POINT('Ctrl Pts',(76.7819677492927,5.47054359542805,76.6158738562889));
#181138=CARTESIAN_POINT('Ctrl Pts',(76.9499775446775,5.44922571831477,76.5825354314886));
#181139=CARTESIAN_POINT('Ctrl Pts',(77.1989725367566,5.40542361949064,76.5328721896949));
#181140=CARTESIAN_POINT('Ctrl Pts',(77.2809009315948,5.38900486053439,76.5164900632926));
#181141=CARTESIAN_POINT('Ctrl Pts',(77.4319656140279,5.35499689484238,76.4861991522373));
#181142=CARTESIAN_POINT('Ctrl Pts',(77.5011997889919,5.33793639829778,76.4722832561289));
#181143=CARTESIAN_POINT('Ctrl Pts',(77.6607876106394,5.29517947399735,76.4401268178773));
#181144=CARTESIAN_POINT('Ctrl Pts',(77.7508508200501,5.2684672559417,76.421919232507));
#181145=CARTESIAN_POINT('Ctrl Pts',(77.9445111262649,5.2053902053854,76.3826415096026));
#181146=CARTESIAN_POINT('Ctrl Pts',(78.047793549123,5.16817231010113,76.3616135718207));
#181147=CARTESIAN_POINT('Ctrl Pts',(78.3982901530972,5.02946474761941,76.2900156163008));
#181148=CARTESIAN_POINT('Ctrl Pts',(78.6391363859982,4.91250429236052,76.2403820339988));
#181149=CARTESIAN_POINT('Ctrl Pts',(78.9640140544602,4.72343265372075,76.1733340345982));
#181150=CARTESIAN_POINT('Ctrl Pts',(79.0559021677069,4.6661656823457,76.1543616728065));
#181151=CARTESIAN_POINT('Ctrl Pts',(79.1876829550696,4.57840398389198,76.1271934223636));
#181152=CARTESIAN_POINT('Ctrl Pts',(79.2289357318011,4.55009352929507,76.1186948027529));
#181153=CARTESIAN_POINT('Ctrl Pts',(79.3045197382148,4.49666034899782,76.1031423463777));
#181154=CARTESIAN_POINT('Ctrl Pts',(79.33895565857,4.47170091527016,76.096064838527));
#181155=CARTESIAN_POINT('Ctrl Pts',(79.4306514898834,4.40357217899605,76.0772348049118));
#181156=CARTESIAN_POINT('Ctrl Pts',(79.4873689460504,4.35965364456593,76.0656040707921));
#181157=CARTESIAN_POINT('Ctrl Pts',(79.6190281180506,4.25344678811769,76.0386127554299));
#181158=CARTESIAN_POINT('Ctrl Pts',(79.6932142045313,4.19022250696668,76.0234095759825));
#181159=CARTESIAN_POINT('Ctrl Pts',(80.0374156191236,3.88045569768894,75.9527511024005));
#181160=CARTESIAN_POINT('Ctrl Pts',(80.2842085570211,3.60858291369714,75.901651476153));
#181161=CARTESIAN_POINT('Ctrl Pts',(80.5538836436764,3.24344014059142,75.8438652635243));
#181162=CARTESIAN_POINT('Ctrl Pts',(80.6039551022752,3.17213362785322,75.833039699647));
#181163=CARTESIAN_POINT('Ctrl Pts',(80.6918533153087,3.04036572112086,75.8138438069116));
#181164=CARTESIAN_POINT('Ctrl Pts',(80.7302383807383,2.98031315297712,75.805387912181));
#181165=CARTESIAN_POINT('Ctrl Pts',(80.8149271718713,2.84193599131267,75.7865565325153));
#181166=CARTESIAN_POINT('Ctrl Pts',(80.8604814075452,2.76316206775251,75.776297729902));
#181167=CARTESIAN_POINT('Ctrl Pts',(81.0353628071834,2.4426031910518,75.7363740307411));
#181168=CARTESIAN_POINT('Ctrl Pts',(81.1485813520934,2.19217891526517,75.7092258917502));
#181169=CARTESIAN_POINT('Ctrl Pts',(81.3286618770366,1.69898218475199,75.6635929150326));
#181170=CARTESIAN_POINT('Ctrl Pts',(81.3985430044552,1.45808072721642,75.6446119749557));
#181171=CARTESIAN_POINT('Ctrl Pts',(81.464836328048,1.15442628172622,75.6251491710594));
#181172=CARTESIAN_POINT('Ctrl Pts',(81.4767001255558,1.0955439347704,75.6215788870083));
#181173=CARTESIAN_POINT('Ctrl Pts',(81.494706390344,0.998097598559453,75.6160158592297));
#181174=CARTESIAN_POINT('Ctrl Pts',(81.501396495175,0.959646541580208,75.6139091227582));
#181175=CARTESIAN_POINT('Ctrl Pts',(81.5153461757035,0.87419372173092,75.6094250171015));
#181176=CARTESIAN_POINT('Ctrl Pts',(81.5224104509144,0.827162092638322,
75.6070883012019));
#181177=CARTESIAN_POINT('Ctrl Pts',(81.5444776036597,0.666321761140413,
75.5995310612406));
#181178=CARTESIAN_POINT('Ctrl Pts',(81.5565842571607,0.552118721185883,
75.5949037411769));
#181179=CARTESIAN_POINT('Ctrl Pts',(81.5811858603854,0.223914095366242,
75.5835685654046));
#181180=CARTESIAN_POINT('Ctrl Pts',(81.5849165887661,0.00941249962848681,
75.5785328573369));
#181181=CARTESIAN_POINT('Ctrl Pts',(81.5669627093228,-0.436628439375698,
75.5724285508419));
#181182=CARTESIAN_POINT('Ctrl Pts',(81.5431824625473,-0.667666921105809,
75.5717225500968));
#181183=CARTESIAN_POINT('Ctrl Pts',(81.4903615978844,-0.984792113831477,
75.5738885047287));
#181184=CARTESIAN_POINT('Ctrl Pts',(81.4735382064467,-1.07267417905273,
75.5748299440397));
#181185=CARTESIAN_POINT('Ctrl Pts',(81.4392804126417,-1.23087722059542,
75.5771350847878));
#181186=CARTESIAN_POINT('Ctrl Pts',(81.4225770648942,-1.30133700978203,
75.5783839377358));
#181187=CARTESIAN_POINT('Ctrl Pts',(81.3820113412801,-1.45870533700053,
75.5816717052041));
#181188=CARTESIAN_POINT('Ctrl Pts',(81.357403390545,-1.54539764611939,75.5838285392543));
#181189=CARTESIAN_POINT('Ctrl Pts',(81.3004508501523,-1.72894093691882,
75.5891397869368));
#181190=CARTESIAN_POINT('Ctrl Pts',(81.267523611845,-1.82557326085189,75.5923876027384));
#181191=CARTESIAN_POINT('Ctrl Pts',(81.1571132433896,-2.12255911783891,
75.6038073507318));
#181192=CARTESIAN_POINT('Ctrl Pts',(81.0706849500237,-2.31931492465621,
75.6134387538996));
#181193=CARTESIAN_POINT('Ctrl Pts',(80.8909345968818,-2.67162652378668,
75.6348655220105));
#181194=CARTESIAN_POINT('Ctrl Pts',(80.8009360595584,-2.82858838624564,
75.6460731196286));
#181195=CARTESIAN_POINT('Ctrl Pts',(80.6744272125664,-3.02622880126914,
75.6625920261535));
#181196=CARTESIAN_POINT('Ctrl Pts',(80.6446910284241,-3.07122708385836,
75.6665235973506));
#181197=CARTESIAN_POINT('Ctrl Pts',(80.5908504064156,-3.15017733247058,
75.6737350203911));
#181198=CARTESIAN_POINT('Ctrl Pts',(80.5670090336757,-3.18430657813894,
75.6769596532948));
#181199=CARTESIAN_POINT('Ctrl Pts',(80.505795028728,-3.26986786533731,75.6853142290436));
#181200=CARTESIAN_POINT('Ctrl Pts',(80.467923522806,-3.32092356857916,75.6905502345333));
#181201=CARTESIAN_POINT('Ctrl Pts',(80.3797407701987,-3.43562197010435,
75.7028708998814));
#181202=CARTESIAN_POINT('Ctrl Pts',(80.3288975903319,-3.4988249462727,75.7100646514684));
#181203=CARTESIAN_POINT('Ctrl Pts',(80.1361461507751,-3.72790334146643,
75.737594675469));
#181204=CARTESIAN_POINT('Ctrl Pts',(79.9859162441715,-3.88631031285377,
75.7595368878297));
#181205=CARTESIAN_POINT('Ctrl Pts',(79.6887002358404,-4.16442701220919,
75.8032680716101));
#181206=CARTESIAN_POINT('Ctrl Pts',(79.5441271611145,-4.28629294341588,
75.8246627276548));
#181207=CARTESIAN_POINT('Ctrl Pts',(79.3256304547381,-4.45185119459827,
75.8570015179661));
#181208=CARTESIAN_POINT('Ctrl Pts',(79.2564754918251,-4.50173872972957,
75.8672384238845));
#181209=CARTESIAN_POINT('Ctrl Pts',(79.1267894576786,-4.59073528490751,
75.8864280788308));
#181210=CARTESIAN_POINT('Ctrl Pts',(79.066593275645,-4.63030858391227,75.8953324794358));
#181211=CARTESIAN_POINT('Ctrl Pts',(78.9263188117953,-4.71858278959934,
75.916072038791));
#181212=CARTESIAN_POINT('Ctrl Pts',(78.8457387544382,-4.76642607583487,
75.9279781728946));
#181213=CARTESIAN_POINT('Ctrl Pts',(78.5423740529721,-4.93607949645029,
75.9727756950506));
#181214=CARTESIAN_POINT('Ctrl Pts',(78.3124722047592,-5.04422621065495,
76.0066565681112));
#181215=CARTESIAN_POINT('Ctrl Pts',(77.829034184455,-5.23142919103745,76.0781259275798));
#181216=CARTESIAN_POINT('Ctrl Pts',(77.57553792995,-5.30874219937458,76.1157201246387));
#181217=CARTESIAN_POINT('Ctrl Pts',(77.2613744437602,-5.37984977586853,
76.1630056636212));
#181218=CARTESIAN_POINT('Ctrl Pts',(77.2049732316613,-5.39166898964449,
76.171522191863));
#181219=CARTESIAN_POINT('Ctrl Pts',(77.1106473714662,-5.40986282727492,
76.185820895061));
#181220=CARTESIAN_POINT('Ctrl Pts',(77.0728198473076,-5.41674027081251,
76.1915702330033));
#181221=CARTESIAN_POINT('Ctrl Pts',(76.9874458561194,-5.43132033513407,
76.2045818145711));
#181222=CARTESIAN_POINT('Ctrl Pts',(76.9398661403242,-5.43879081781303,
76.2118571995347));
#181223=CARTESIAN_POINT('Ctrl Pts',(76.7707178504184,-5.46302850165962,
76.2377912634859));
#181224=CARTESIAN_POINT('Ctrl Pts',(76.6487101659722,-5.47627255080551,
76.2566244422886));
#181225=CARTESIAN_POINT('Ctrl Pts',(76.2772451744542,-5.50377573338375,
76.3141500007427));
#181226=CARTESIAN_POINT('Ctrl Pts',(76.0271968622321,-5.50482793264817,
76.3531135380574));
#181227=CARTESIAN_POINT('Ctrl Pts',(75.5904385492959,-5.47618087078442,
76.4208474296114));
#181228=CARTESIAN_POINT('Ctrl Pts',(75.4036881002443,-5.45405748105691,
76.449707646761));
#181229=CARTESIAN_POINT('Ctrl Pts',(75.134044336607,-5.40769034260733,76.4910798024161));
#181230=CARTESIAN_POINT('Ctrl Pts',(75.0500205098195,-5.39117040414606,
76.5039299457892));
#181231=CARTESIAN_POINT('Ctrl Pts',(74.8963813196968,-5.35714187775381,
76.5273409156258));
#181232=CARTESIAN_POINT('Ctrl Pts',(74.8266578676524,-5.34023319653329,
76.5379322689636));
#181233=CARTESIAN_POINT('Ctrl Pts',(74.6899154236981,-5.3041696216234,76.5586372141246));
#181234=CARTESIAN_POINT('Ctrl Pts',(74.6228894075215,-5.28509750715447,
76.5687538291483));
#181235=CARTESIAN_POINT('Ctrl Pts',(74.395584105041,-5.21563647174156,76.6029539396097));
#181236=CARTESIAN_POINT('Ctrl Pts',(74.2372332825469,-5.15905477625702,
76.6265903536784));
#181237=CARTESIAN_POINT('Ctrl Pts',(74.0817004664548,-5.09516704230593,
76.6496559375717));
#181238=CARTESIAN_POINT('',(79.7540569593757,-4.07954801327269,75.649466443673));
#181239=CARTESIAN_POINT('Origin',(76.1212924379081,7.15881389286582E-15,
76.2900208433682));
#181240=CARTESIAN_POINT('Ctrl Pts',(79.7540569593757,-4.07954801327269,
75.649466443673));
#181241=CARTESIAN_POINT('Ctrl Pts',(79.9550556064584,-3.89610083871904,
75.6210523034932));
#181242=CARTESIAN_POINT('Ctrl Pts',(80.1423230216256,-3.69778482906888,
75.5952486961923));
#181243=CARTESIAN_POINT('Ctrl Pts',(80.3562343526423,-3.43456767337074,
75.5661552350339));
#181244=CARTESIAN_POINT('Ctrl Pts',(80.3972895896231,-3.382133321999,75.5605900939294));
#181245=CARTESIAN_POINT('Ctrl Pts',(80.4707099816455,-3.2847719269421,75.5506576046304));
#181246=CARTESIAN_POINT('Ctrl Pts',(80.5033667439126,-3.24007982786696,
75.5462473578158));
#181247=CARTESIAN_POINT('Ctrl Pts',(80.5596008253803,-3.16063129437193,
75.5386577661436));
#181248=CARTESIAN_POINT('Ctrl Pts',(80.5834624070778,-3.12608747664255,
75.5354381457118));
#181249=CARTESIAN_POINT('Ctrl Pts',(80.6363530629559,-3.04761418133183,
75.5283058804656));
#181250=CARTESIAN_POINT('Ctrl Pts',(80.6651527602619,-3.00353353717,75.524426001573));
#181251=CARTESIAN_POINT('Ctrl Pts',(80.8478409371821,-2.71496953037959,
75.4998728557273));
#181252=CARTESIAN_POINT('Ctrl Pts',(80.9830572573553,-2.45897192043341,
75.482000099418));
#181253=CARTESIAN_POINT('Ctrl Pts',(81.1823475989033,-1.99788564595248,
75.4574826058732));
#181254=CARTESIAN_POINT('Ctrl Pts',(81.2556070490208,-1.79756030707335,
75.4491368303146));
#181255=CARTESIAN_POINT('Ctrl Pts',(81.3420230087736,-1.51152230905519,
75.4406024945352));
#181256=CARTESIAN_POINT('Ctrl Pts',(81.3648982333203,-1.42900607922151,
75.4385212107493));
#181257=CARTESIAN_POINT('Ctrl Pts',(81.4036544248634,-1.27561407896006,
75.4353608550889));
#181258=CARTESIAN_POINT('Ctrl Pts',(81.4200661527256,-1.20489424898321,
75.434177700621));
#181259=CARTESIAN_POINT('Ctrl Pts',(81.4543841896188,-1.04276060042251,
75.4320910447137));
#181260=CARTESIAN_POINT('Ctrl Pts',(81.4713946674952,-0.951177810721096,
75.4313617794898));
#181261=CARTESIAN_POINT('Ctrl Pts',(81.536412068738,-0.544957176818441,
75.430100047732));
#181262=CARTESIAN_POINT('Ctrl Pts',(81.5598456418334,-0.226990638240277,
75.4343482823491));
#181263=CARTESIAN_POINT('Ctrl Pts',(81.5535579234438,0.305419715144901,
75.449484331721));
#181264=CARTESIAN_POINT('Ctrl Pts',(81.5386878444932,0.519344982180364,
75.4577279527938));
#181265=CARTESIAN_POINT('Ctrl Pts',(81.5046293544219,0.785579410276051,
75.4703960790198));
#181266=CARTESIAN_POINT('Ctrl Pts',(81.4969606121235,0.839262145573826,
75.4730741056276));
#181267=CARTESIAN_POINT('Ctrl Pts',(81.482495066884,0.930896376042242,75.4778492770305));
#181268=CARTESIAN_POINT('Ctrl Pts',(81.4760872172513,0.968907308844052,
75.4798900109912));
#181269=CARTESIAN_POINT('Ctrl Pts',(81.460350056275,1.05665918084017,75.4847398795328));
#181270=CARTESIAN_POINT('Ctrl Pts',(81.4507352996072,1.10634194800698,75.4875901851627));
#181271=CARTESIAN_POINT('Ctrl Pts',(81.4135605586294,1.28526291080719,75.4982497703578));
#181272=CARTESIAN_POINT('Ctrl Pts',(81.3820665205496,1.41360171289019,75.5066444834221));
#181273=CARTESIAN_POINT('Ctrl Pts',(81.2853833688129,1.75449848831423,75.5311718921765));
#181274=CARTESIAN_POINT('Ctrl Pts',(81.2119666585506,1.96436331166959,75.5486561367009));
#181275=CARTESIAN_POINT('Ctrl Pts',(81.0469581347712,2.35840784715467,75.5867078861355));
#181276=CARTESIAN_POINT('Ctrl Pts',(80.9572801169381,2.54301636247878,75.6069141242577));
#181277=CARTESIAN_POINT('Ctrl Pts',(80.8158730901985,2.79710961068029,75.6383745935883));
#181278=CARTESIAN_POINT('Ctrl Pts',(80.7723632254629,2.87116481313088,75.6480087669995));
#181279=CARTESIAN_POINT('Ctrl Pts',(80.6892237466168,3.00538436733356,75.6663453150252));
#181280=CARTESIAN_POINT('Ctrl Pts',(80.6501029267193,3.06585474170003,75.6749466540032));
#181281=CARTESIAN_POINT('Ctrl Pts',(80.5586199607333,3.20134874172161,75.69500380147));
#181282=CARTESIAN_POINT('Ctrl Pts',(80.5055576271492,3.27585249528855,75.70659829089));
#181283=CARTESIAN_POINT('Ctrl Pts',(80.3153733318279,3.52922093305338,75.7480178038986));
#181284=CARTESIAN_POINT('Ctrl Pts',(80.1692329927724,3.70073220098829,75.7796229922203));
#181285=CARTESIAN_POINT('Ctrl Pts',(79.8912362588521,3.9887375940513,75.8391393499741));
#181286=CARTESIAN_POINT('Ctrl Pts',(79.7634556847928,4.10887402418649,75.8662988014842));
#181287=CARTESIAN_POINT('Ctrl Pts',(79.5745540055725,4.26989973790512,75.9060090474467));
#181288=CARTESIAN_POINT('Ctrl Pts',(79.5180016410818,4.31615484337398,75.9178448610913));
#181289=CARTESIAN_POINT('Ctrl Pts',(79.4142133639953,4.397574951187,75.9394533755029));
#181290=CARTESIAN_POINT('Ctrl Pts',(79.367301737562,4.43314718220199,75.9491801320532));
#181291=CARTESIAN_POINT('Ctrl Pts',(79.2864498579615,4.49238704884988,75.9658657738151));
#181292=CARTESIAN_POINT('Ctrl Pts',(79.2527991771433,4.51644961727751,75.9727872746673));
#181293=CARTESIAN_POINT('Ctrl Pts',(79.1714399308616,4.5732161079938,75.9894671128365));
#181294=CARTESIAN_POINT('Ctrl Pts',(79.1234793193192,4.60553833401426,75.9992567928688));
#181295=CARTESIAN_POINT('Ctrl Pts',(78.8770000517463,4.76591235420394,76.0493886449357));
#181296=CARTESIAN_POINT('Ctrl Pts',(78.670842711567,4.88141817520882,76.0907471250219));
#181297=CARTESIAN_POINT('Ctrl Pts',(78.2367696882436,5.08821168409858,76.1775656977172));
#181298=CARTESIAN_POINT('Ctrl Pts',(78.0088279413494,5.17814608798127,76.2230256174725));
#181299=CARTESIAN_POINT('Ctrl Pts',(77.6911731584347,5.27883551707747,76.2866039634875));
#181300=CARTESIAN_POINT('Ctrl Pts',(77.6059881237611,5.30351054739958,76.3036731028311));
#181301=CARTESIAN_POINT('Ctrl Pts',(77.4514940464848,5.34410114405924,76.3346776955947));
#181302=CARTESIAN_POINT('Ctrl Pts',(77.3823972277283,5.36077965847882,76.3485611405648));
#181303=CARTESIAN_POINT('Ctrl Pts',(77.2274214007911,5.39490906576752,76.3797414543912));
#181304=CARTESIAN_POINT('Ctrl Pts',(77.1414099253904,5.41162784306611,76.3970747006309));
#181305=CARTESIAN_POINT('Ctrl Pts',(76.8405040792983,5.46241168766167,76.4578121043415));
#181306=CARTESIAN_POINT('Ctrl Pts',(76.6240506280537,5.48535153572426,76.5016856039424));
#181307=CARTESIAN_POINT('Ctrl Pts',(76.1891201938785,5.50447128643675,76.5900118497044));
#181308=CARTESIAN_POINT('Ctrl Pts',(75.9710362730251,5.50056825728675,76.6343839354773));
#181309=CARTESIAN_POINT('Ctrl Pts',(75.639462516768,5.47408226077514,76.7016256038782));
#181310=CARTESIAN_POINT('Ctrl Pts',(75.5254715132157,5.4612361921884,76.7247000444197));
#181311=CARTESIAN_POINT('Ctrl Pts',(75.3654979479876,5.43792360047614,76.7569585898209));
#181312=CARTESIAN_POINT('Ctrl Pts',(75.3191290837197,5.43053577677619,76.7662939744724));
#181313=CARTESIAN_POINT('Ctrl Pts',(75.2613436702706,5.42054010557266,76.7779049741604));
#181314=CARTESIAN_POINT('Ctrl Pts',(75.2498364807966,5.4185104098025,76.780216012227));
#181315=CARTESIAN_POINT('Ctrl Pts',(75.2383357398202,5.41644264187749,76.7825245638573));
#181316=CARTESIAN_POINT('Origin',(76.0518331668413,7.15881389286582E-15,
75.8960977421633));
#181317=CARTESIAN_POINT('',(75.4009754336961,5.41644264156684,77.7049001130299));
#181318=CARTESIAN_POINT('',(75.3772542814629,5.41644264179018,77.5703707663353));
#181319=CARTESIAN_POINT('',(75.1112777726958,5.41644264156718,76.061943035002));
#181320=CARTESIAN_POINT('Ctrl Pts',(75.4009754336941,5.41644264156649,77.7049001130302));
#181321=CARTESIAN_POINT('Ctrl Pts',(75.4020729769854,5.41663997361865,77.704679802412));
#181322=CARTESIAN_POINT('Ctrl Pts',(75.4031705837651,5.41683695903492,77.7044594928459));
#181323=CARTESIAN_POINT('Ctrl Pts',(75.4452787908983,5.42438030488838,77.696008139894));
#181324=CARTESIAN_POINT('Ctrl Pts',(75.4863750017577,5.43124262170462,77.6877790728472));
#181325=CARTESIAN_POINT('Ctrl Pts',(75.6058154563448,5.44974047445724,77.6639096767692));
#181326=CARTESIAN_POINT('Ctrl Pts',(75.684346011331,5.46010407979348,77.6482745253597));
#181327=CARTESIAN_POINT('Ctrl Pts',(76.1815405376581,5.514400969188,77.5495361110557));
#181328=CARTESIAN_POINT('Ctrl Pts',(76.6039855001008,5.51004359234611,77.466636795253));
#181329=CARTESIAN_POINT('Ctrl Pts',(77.1376747354864,5.44058675271276,77.3606483411415));
#181330=CARTESIAN_POINT('Ctrl Pts',(77.2533426158265,5.4216121665109,77.337609825817));
#181331=CARTESIAN_POINT('Ctrl Pts',(77.4411559288904,5.38436680411922,77.3000613183583));
#181332=CARTESIAN_POINT('Ctrl Pts',(77.5137078564261,5.36838679584465,77.2855219480806));
#181333=CARTESIAN_POINT('Ctrl Pts',(77.6591786277079,5.33312432675046,77.256295596882));
#181334=CARTESIAN_POINT('Ctrl Pts',(77.7320707207943,5.31380021265953,77.2416128781552));
#181335=CARTESIAN_POINT('Ctrl Pts',(77.9256686146808,5.25803217267343,77.2025134307304));
#181336=CARTESIAN_POINT('Ctrl Pts',(78.0455467754778,5.21882418249065,77.1781935283756));
#181337=CARTESIAN_POINT('Ctrl Pts',(78.3296723279193,5.11456155376492,77.1203157462599));
#181338=CARTESIAN_POINT('Ctrl Pts',(78.4923367479489,5.04550175049125,77.0869823530995));
#181339=CARTESIAN_POINT('Ctrl Pts',(78.8518658917288,4.87130021871031,77.0130368007182));
#181340=CARTESIAN_POINT('Ctrl Pts',(79.0462544723592,4.7616095652405,76.9728592553762));
#181341=CARTESIAN_POINT('Ctrl Pts',(79.2826381127944,4.60806484841252,76.9241008976943));
#181342=CARTESIAN_POINT('Ctrl Pts',(79.3312901338968,4.57531974836113,76.9140717788956));
#181343=CARTESIAN_POINT('Ctrl Pts',(79.4133424573088,4.51812688394018,76.8971790129097));
#181344=CARTESIAN_POINT('Ctrl Pts',(79.4470046036712,4.49408357014091,76.8902556801653));
#181345=CARTESIAN_POINT('Ctrl Pts',(79.5272278095524,4.43537974882161,76.8737726094502));
#181346=CARTESIAN_POINT('Ctrl Pts',(79.5735201666139,4.40034596551875,76.8642735071764));
#181347=CARTESIAN_POINT('Ctrl Pts',(79.7723850516266,4.24474318335922,76.8234894983546));
#181348=CARTESIAN_POINT('Ctrl Pts',(79.9191117054783,4.11661816826673,76.7934530302152));
#181349=CARTESIAN_POINT('Ctrl Pts',(80.2638622600493,3.78116886457503,76.7224269910616));
#181350=CARTESIAN_POINT('Ctrl Pts',(80.4531485901211,3.56539863205374,76.6829956575978));
#181351=CARTESIAN_POINT('Ctrl Pts',(80.6787780408469,3.26307513276364,76.6347341520628));
#181352=CARTESIAN_POINT('Ctrl Pts',(80.7309999518845,3.18935447349107,76.6234621678859));
#181353=CARTESIAN_POINT('Ctrl Pts',(80.8214803160336,3.0546625416661,76.6037298444661));
#181354=CARTESIAN_POINT('Ctrl Pts',(80.8604024199354,2.9941780035497,76.595167702943));
#181355=CARTESIAN_POINT('Ctrl Pts',(80.9443058915359,2.85796510389816,76.5765371265833));
#181356=CARTESIAN_POINT('Ctrl Pts',(80.988681530533,2.7818746694691,76.566563067203));
#181357=CARTESIAN_POINT('Ctrl Pts',(81.1463780764141,2.49585703268448,76.5306529092568));
#181358=CARTESIAN_POINT('Ctrl Pts',(81.2479050651942,2.2795058314519,76.506559702183));
#181359=CARTESIAN_POINT('Ctrl Pts',(81.442853000442,1.78258182729151,76.4581168680367));
#181360=CARTESIAN_POINT('Ctrl Pts',(81.5285108441798,1.49962495282199,76.4350964575102));
#181361=CARTESIAN_POINT('Ctrl Pts',(81.6041246215021,1.15261992842301,76.4128846558187));
#181362=CARTESIAN_POINT('Ctrl Pts',(81.6158988443021,1.09409238604093,76.4093396837614));
#181363=CARTESIAN_POINT('Ctrl Pts',(81.6338115843297,0.997044222537231,
76.4038036237688));
#181364=CARTESIAN_POINT('Ctrl Pts',(81.6404871299318,0.958634294155849,
76.4017007422951));
#181365=CARTESIAN_POINT('Ctrl Pts',(81.6544464092353,0.873028147085903,
76.3972118927654));
#181366=CARTESIAN_POINT('Ctrl Pts',(81.6615290211364,0.825801121556553,
76.3948677969999));
#181367=CARTESIAN_POINT('Ctrl Pts',(81.683792191991,0.663193268090111,76.3872371519462));
#181368=CARTESIAN_POINT('Ctrl Pts',(81.6959842799855,0.547406690715393,
76.3825624941172));
#181369=CARTESIAN_POINT('Ctrl Pts',(81.7207781897654,0.211548296276864,
76.3710364535082));
#181370=CARTESIAN_POINT('Ctrl Pts',(81.7240070003098,-0.00904462314788024,
76.3659708117056));
#181371=CARTESIAN_POINT('Ctrl Pts',(81.7042080129052,-0.452474710442173,
76.3602340745503));
#181372=CARTESIAN_POINT('Ctrl Pts',(81.6808467751521,-0.674884822386066,
76.3596261769768));
#181373=CARTESIAN_POINT('Ctrl Pts',(81.6294851487584,-0.983685275673139,
76.3617239203034));
#181374=CARTESIAN_POINT('Ctrl Pts',(81.612650234701,-1.07171750319945,76.3626643100358));
#181375=CARTESIAN_POINT('Ctrl Pts',(81.5783843811993,-1.23007142514674,
76.3649678642025));
#181376=CARTESIAN_POINT('Ctrl Pts',(81.5616915987074,-1.30053330021413,
76.3662150605287));
#181377=CARTESIAN_POINT('Ctrl Pts',(81.5211878885947,-1.45775780560969,
76.3694960067721));
#181378=CARTESIAN_POINT('Ctrl Pts',(81.4966385721934,-1.54430627648585,
76.371646540938));
#181379=CARTESIAN_POINT('Ctrl Pts',(81.3954187544674,-1.87077914819239,
76.3810810293745));
#181380=CARTESIAN_POINT('Ctrl Pts',(81.3045982606598,-2.10592696902885,
76.3906096568055));
#181381=CARTESIAN_POINT('Ctrl Pts',(81.0980492338646,-2.54874766688467,
76.4143293583233));
#181382=CARTESIAN_POINT('Ctrl Pts',(80.984299133772,-2.75676566615468,76.4281952746031));
#181383=CARTESIAN_POINT('Ctrl Pts',(80.8263555253881,-3.00632693109112,
76.4487254522299));
#181384=CARTESIAN_POINT('Ctrl Pts',(80.7941999988036,-3.05539644322752,
76.4529623578508));
#181385=CARTESIAN_POINT('Ctrl Pts',(80.7378047895742,-3.13855245758497,
76.4604990868535));
#181386=CARTESIAN_POINT('Ctrl Pts',(80.713943322543,-3.1728950819609,76.4637193241671));
#181387=CARTESIAN_POINT('Ctrl Pts',(80.6553056567348,-3.25528640450156,
76.4717067610597));
#181388=CARTESIAN_POINT('Ctrl Pts',(80.6201469420956,-3.30304696015817,
76.4765552921622));
#181389=CARTESIAN_POINT('Ctrl Pts',(80.5397494552509,-3.40866383795519,
76.4877556768322));
#181390=CARTESIAN_POINT('Ctrl Pts',(80.4941165436365,-3.46619700066956,
76.4941888745555));
#181391=CARTESIAN_POINT('Ctrl Pts',(80.3357899666468,-3.65783274908615,
76.5167148035222));
#181392=CARTESIAN_POINT('Ctrl Pts',(80.2179230208658,-3.78739929961215,
76.5338187546947));
#181393=CARTESIAN_POINT('Ctrl Pts',(79.9325771620297,-4.07241960119109,
76.5755977565229));
#181394=CARTESIAN_POINT('Ctrl Pts',(79.7612179705992,-4.22342178265414,
76.6009428583409));
#181395=CARTESIAN_POINT('Ctrl Pts',(79.508729005858,-4.41923275774376,76.6383078424876));
#181396=CARTESIAN_POINT('Ctrl Pts',(79.4350477229229,-4.47345890814326,
76.6492155511054));
#181397=CARTESIAN_POINT('Ctrl Pts',(79.3010125527878,-4.56698842672564,
76.6690509309088));
#181398=CARTESIAN_POINT('Ctrl Pts',(79.24117105774,-4.60700315214091,76.6779043298694));
#181399=CARTESIAN_POINT('Ctrl Pts',(79.108301688471,-4.69208057689179,76.6975526569854));
#181400=CARTESIAN_POINT('Ctrl Pts',(79.0349697230675,-4.7366222454886,76.7083906944632));
#181401=CARTESIAN_POINT('Ctrl Pts',(78.7829382837485,-4.88164320501621,
76.7456179533184));
#181402=CARTESIAN_POINT('Ctrl Pts',(78.5996839502126,-4.97368642080729,
76.7726433327134));
#181403=CARTESIAN_POINT('Ctrl Pts',(78.2090201216121,-5.14290632603296,
76.8303142993207));
#181404=CARTESIAN_POINT('Ctrl Pts',(78.0012037239324,-5.21818701418991,
76.8610239264968));
#181405=CARTESIAN_POINT('Ctrl Pts',(77.6642970292578,-5.31737531769137,
76.9112002748036));
#181406=CARTESIAN_POINT('Ctrl Pts',(77.5378523013817,-5.34967297348176,
76.930118788903));
#181407=CARTESIAN_POINT('Ctrl Pts',(77.3615192121098,-5.38796516969839,
76.9567074737141));
#181408=CARTESIAN_POINT('Ctrl Pts',(77.3124930965134,-5.39789957191332,
76.9641218116638));
#181409=CARTESIAN_POINT('Ctrl Pts',(77.2258172860334,-5.41421121345534,
76.9772754314374));
#181410=CARTESIAN_POINT('Ctrl Pts',(77.1882232627926,-5.42087336868818,
76.9829960938603));
#181411=CARTESIAN_POINT('Ctrl Pts',(77.0974694270477,-5.43596330120389,
76.996842312823));
#181412=CARTESIAN_POINT('Ctrl Pts',(77.0442524423473,-5.44399427940258,
77.0049905360038));
#181413=CARTESIAN_POINT('Ctrl Pts',(76.7730296211376,-5.48077448131402,
77.0466356050011));
#181414=CARTESIAN_POINT('Ctrl Pts',(76.5536178044252,-5.49693060199017,
77.0807024432229));
#181415=CARTESIAN_POINT('Ctrl Pts',(76.0295409312807,-5.50330296947548,
77.1621358488257));
#181416=CARTESIAN_POINT('Ctrl Pts',(75.7254729986752,-5.48114096815827,
77.2094103944046));
#181417=CARTESIAN_POINT('Ctrl Pts',(75.3331039071907,-5.41878711386261,
77.2697131851974));
#181418=CARTESIAN_POINT('Ctrl Pts',(75.24183316856,-5.40185302300611,77.2836934343694));
#181419=CARTESIAN_POINT('Ctrl Pts',(75.0807363885537,-5.36763604698873,
77.3082732092191));
#181420=CARTESIAN_POINT('Ctrl Pts',(75.0107402169087,-5.35129974146552,
77.3189205734925));
#181421=CARTESIAN_POINT('Ctrl Pts',(74.8594488421186,-5.31278626645264,
77.3418602960457));
#181422=CARTESIAN_POINT('Ctrl Pts',(74.7782993351078,-5.29009305175616,
77.3541177625059));
#181423=CARTESIAN_POINT('Ctrl Pts',(74.5034103532694,-5.20623880419246,
77.3954805960167));
#181424=CARTESIAN_POINT('Ctrl Pts',(74.3125133201331,-5.13603057017492,
77.4239262159174));
#181425=CARTESIAN_POINT('Ctrl Pts',(73.9142066477073,-4.96351707623434,
77.4828457673159));
#181426=CARTESIAN_POINT('Ctrl Pts',(73.7084290046165,-4.85833694299808,
77.513017391783));
#181427=CARTESIAN_POINT('Ctrl Pts',(73.4275874254457,-4.69139566643611,
77.5541776277481));
#181428=CARTESIAN_POINT('Ctrl Pts',(73.3465964460926,-4.64030884468542,
77.5660471991354));
#181429=CARTESIAN_POINT('Ctrl Pts',(73.2283766489362,-4.56129508870328,
77.5834094423849));
#181430=CARTESIAN_POINT('Ctrl Pts',(73.1901007749669,-4.53499711030064,
77.5890367429091));
#181431=CARTESIAN_POINT('Ctrl Pts',(73.1153793664998,-4.48223603124923,
77.6000402064927));
#181432=CARTESIAN_POINT('Ctrl Pts',(73.0789166209474,-4.45580443452335,
77.6054185719554));
#181433=CARTESIAN_POINT('Ctrl Pts',(72.9731907493409,-4.3771434416892,77.6210298216499));
#181434=CARTESIAN_POINT('Ctrl Pts',(72.9048320949972,-4.32369868629183,
77.6311442986488));
#181435=CARTESIAN_POINT('Ctrl Pts',(72.7367403329871,-4.18569092517141,
77.6560110940905));
#181436=CARTESIAN_POINT('Ctrl Pts',(72.6386949300854,-4.09911462700645,
77.6705108504923));
#181437=CARTESIAN_POINT('Ctrl Pts',(72.3221781118181,-3.79876725713764,
77.7170723819862));
#181438=CARTESIAN_POINT('Ctrl Pts',(72.1183040429124,-3.57007414181092,
77.7466130640995));
#181439=CARTESIAN_POINT('Ctrl Pts',(71.8805936079935,-3.25411209035273,
77.7796698119892));
#181440=CARTESIAN_POINT('Ctrl Pts',(71.8286825384416,-3.18152245778924,
77.7867907924351));
#181441=CARTESIAN_POINT('Ctrl Pts',(71.7379596963361,-3.04795473113288,
77.799040617419));
#181442=CARTESIAN_POINT('Ctrl Pts',(71.6985485669373,-2.98741982906312,
77.8042890487759));
#181443=CARTESIAN_POINT('Ctrl Pts',(71.612770761583,-2.84986627949213,77.8155394100314));
#181444=CARTESIAN_POINT('Ctrl Pts',(71.5670652304035,-2.77244937745199,
77.8214110656497));
#181445=CARTESIAN_POINT('Ctrl Pts',(71.4742167268635,-2.60609163312333,
77.8330679582445));
#181446=CARTESIAN_POINT('Ctrl Pts',(71.4275666339812,-2.5169066993107,77.8387576010062));
#181447=CARTESIAN_POINT('Ctrl Pts',(71.2954432723988,-2.2467199983734,77.8543636886155));
#181448=CARTESIAN_POINT('Ctrl Pts',(71.2172493456322,-2.06226476071193,
77.8628851650492));
#181449=CARTESIAN_POINT('Ctrl Pts',(71.0709593663331,-1.6578019620809,77.8773406054602));
#181450=CARTESIAN_POINT('Ctrl Pts',(71.0062029630466,-1.43695961715027,
77.8826913878878));
#181451=CARTESIAN_POINT('Ctrl Pts',(70.9419958661517,-1.15410968631953,
77.8867725233147));
#181452=CARTESIAN_POINT('Ctrl Pts',(70.9296427566043,-1.09528970198231,
77.8874740063728));
#181453=CARTESIAN_POINT('Ctrl Pts',(70.9108368169774,-0.997913445835886,
77.8884038070268));
#181454=CARTESIAN_POINT('Ctrl Pts',(70.9038322756842,-0.959469711642977,
77.8887120344974));
#181455=CARTESIAN_POINT('Ctrl Pts',(70.8891883990514,-0.873990427797152,
77.8892692188217));
#181456=CARTESIAN_POINT('Ctrl Pts',(70.88174751564,-0.82692484798217,77.8894894333077));
#181457=CARTESIAN_POINT('Ctrl Pts',(70.8583903258539,-0.665779445539081,
77.8899350268585));
#181458=CARTESIAN_POINT('Ctrl Pts',(70.8454144177356,-0.551303327335231,
77.8897248713029));
#181459=CARTESIAN_POINT('Ctrl Pts',(70.8183772460396,-0.221792504260873,
77.8874682190748));
#181460=CARTESIAN_POINT('Ctrl Pts',(70.8132260150459,-0.00625418694376014,
77.883978481678));
#181461=CARTESIAN_POINT('Ctrl Pts',(70.8283287089504,0.439340093590735,
77.8720527215784));
#181462=CARTESIAN_POINT('Ctrl Pts',(70.8503748299958,0.668906897706618,
77.8632955563532));
#181463=CARTESIAN_POINT('Ctrl Pts',(70.900513282669,0.984611395727771,77.8473392703025));
#181464=CARTESIAN_POINT('Ctrl Pts',(70.9166457957842,1.07251793677072,77.8424691922593));
#181465=CARTESIAN_POINT('Ctrl Pts',(70.9496271307735,1.23074554550303,77.8329177709531));
#181466=CARTESIAN_POINT('Ctrl Pts',(70.9657485550732,1.30120564917606,77.8283787653097));
#181467=CARTESIAN_POINT('Ctrl Pts',(71.0049824167555,1.45855038017018,77.8175963874491));
#181468=CARTESIAN_POINT('Ctrl Pts',(71.0288346261726,1.54521911779411,77.8112090496226));
#181469=CARTESIAN_POINT('Ctrl Pts',(71.0701833899872,1.68239098540337,77.8003825271014));
#181470=CARTESIAN_POINT('Ctrl Pts',(71.0863337615349,1.73330312264484,77.7962040836166));
#181471=CARTESIAN_POINT('Ctrl Pts',(71.1273534154071,1.85642707029573,77.785710349855));
#181472=CARTESIAN_POINT('Ctrl Pts',(71.1529792845135,1.92836261467522,77.7792503968465));
#181473=CARTESIAN_POINT('Ctrl Pts',(71.2803750611764,2.26390069384434,77.7475803192595));
#181474=CARTESIAN_POINT('Ctrl Pts',(71.4006031665256,2.51970316168431,77.7188925668034));
#181475=CARTESIAN_POINT('Ctrl Pts',(71.5856552511088,2.84570286948372,77.6766585468788));
#181476=CARTESIAN_POINT('Ctrl Pts',(71.6335825210212,2.92534704552493,77.6658586588896));
#181477=CARTESIAN_POINT('Ctrl Pts',(71.710719898781,3.04643591043896,77.6487169441098));
#181478=CARTESIAN_POINT('Ctrl Pts',(71.7385303697219,3.08878084829776,77.6425812864957));
#181479=CARTESIAN_POINT('Ctrl Pts',(71.7908543550672,3.16608269784157,77.6311250739553));
#181480=CARTESIAN_POINT('Ctrl Pts',(71.8151978882991,3.20115246897619,77.6258289927339));
#181481=CARTESIAN_POINT('Ctrl Pts',(71.8813405265814,3.2940896995417,77.6115223418272));
#181482=CARTESIAN_POINT('Ctrl Pts',(71.9238614684829,3.35141741247608,77.6024099501953));
#181483=CARTESIAN_POINT('Ctrl Pts',(72.0264026356097,3.48413774177117,77.5805983463726));
#181484=CARTESIAN_POINT('Ctrl Pts',(72.0873116371339,3.55879082933397,77.5677657761391));
#181485=CARTESIAN_POINT('Ctrl Pts',(72.38187649175,3.90088479971365,77.5061255652904));
#181486=CARTESIAN_POINT('Ctrl Pts',(72.6390036122654,4.14623817745918,77.4534368313759));
#181487=CARTESIAN_POINT('Ctrl Pts',(72.9891238576085,4.4202247383,77.3816818103994));
#181488=CARTESIAN_POINT('Ctrl Pts',(73.0619162488184,4.47428803197506,77.3667672672356));
#181489=CARTESIAN_POINT('Ctrl Pts',(73.1944674744102,4.5676441899567,77.3396015043864));
#181490=CARTESIAN_POINT('Ctrl Pts',(73.253726106972,4.60763905340021,77.3274543564964));
#181491=CARTESIAN_POINT('Ctrl Pts',(73.3854622364641,4.6927802690722,77.3004409126648));
#181492=CARTESIAN_POINT('Ctrl Pts',(73.4582448808783,4.73739770708001,77.2855101356409));
#181493=CARTESIAN_POINT('Ctrl Pts',(73.7099649488329,4.88356583266327,77.2338498438234));
#181494=CARTESIAN_POINT('Ctrl Pts',(73.8935143340935,4.97645774825786,77.1961357341674));
#181495=CARTESIAN_POINT('Ctrl Pts',(74.3858621449977,5.19090980433098,77.095051778343));
#181496=CARTESIAN_POINT('Ctrl Pts',(74.7012287712784,5.29452021051441,77.0303520702087));
#181497=CARTESIAN_POINT('Ctrl Pts',(75.0791751485197,5.38053464508495,76.953875080421));
#181498=CARTESIAN_POINT('Ctrl Pts',(75.1344859300275,5.39219440762119,76.94271022217));
#181499=CARTESIAN_POINT('Ctrl Pts',(75.2139692185283,5.40762470150229,76.9267132106787));
#181500=CARTESIAN_POINT('Ctrl Pts',(75.2379978491272,5.41211696232847,76.9218832987225));
#181501=CARTESIAN_POINT('Ctrl Pts',(75.2620568894032,5.4164426411786,76.9170539110535));
#181502=CARTESIAN_POINT('Ctrl Pts',(75.2383357398202,5.41644264187749,76.7825245638573));
#181503=CARTESIAN_POINT('Ctrl Pts',(75.2121521933087,5.41173498888793,76.7877804051212));
#181504=CARTESIAN_POINT('Ctrl Pts',(75.1860020711149,5.40682999840865,76.7930233592625));
#181505=CARTESIAN_POINT('Ctrl Pts',(75.1024038764153,5.39049755800644,76.8097669147133));
#181506=CARTESIAN_POINT('Ctrl Pts',(75.0450984412981,5.37831386775064,76.8212180196962));
#181507=CARTESIAN_POINT('Ctrl Pts',(74.7415135912732,5.3084979358921,76.8817824744488));
#181508=CARTESIAN_POINT('Ctrl Pts',(74.4991796415597,5.2342303228491,76.9297908415526));
#181509=CARTESIAN_POINT('Ctrl Pts',(74.018956833578,5.04867940242845,77.0252976914753));
#181510=CARTESIAN_POINT('Ctrl Pts',(73.7821034336695,4.93652837570146,77.0726083068148));
#181511=CARTESIAN_POINT('Ctrl Pts',(73.4744025257356,4.7621007935674,77.1348164042042));
#181512=CARTESIAN_POINT('Ctrl Pts',(73.3957235924925,4.71478566949915,77.1507910210769));
#181513=CARTESIAN_POINT('Ctrl Pts',(73.2580036214972,4.62706724569614,77.1788875048521));
#181514=CARTESIAN_POINT('Ctrl Pts',(73.1984912924057,4.58746739010145,77.1910751414921));
#181515=CARTESIAN_POINT('Ctrl Pts',(73.0694694418116,4.49784470077418,77.2176038127324));
#181516=CARTESIAN_POINT('Ctrl Pts',(73.0003220028763,4.4473194661203,77.2318916857073));
#181517=CARTESIAN_POINT('Ctrl Pts',(72.7579862368154,4.26120605798702,77.2822166701101));
#181518=CARTESIAN_POINT('Ctrl Pts',(72.591804339521,4.1165748527632,77.3172095753566));
#181519=CARTESIAN_POINT('Ctrl Pts',(72.2560280777784,3.78623421995547,77.3887529344337));
#181520=CARTESIAN_POINT('Ctrl Pts',(72.0895177288582,3.59800189436022,77.4247702123249));
#181521=CARTESIAN_POINT('Ctrl Pts',(71.8941598829739,3.34382649608401,77.467293904684));
#181522=CARTESIAN_POINT('Ctrl Pts',(71.8530114834805,3.28813581640704,77.4762668156286));
#181523=CARTESIAN_POINT('Ctrl Pts',(71.7883621853077,3.19708372001615,77.4903748302629));
#181524=CARTESIAN_POINT('Ctrl Pts',(71.7642079502864,3.16221692451688,77.4956480612288));
#181525=CARTESIAN_POINT('Ctrl Pts',(71.711584544796,3.08434613997645,77.5071381125684));
#181526=CARTESIAN_POINT('Ctrl Pts',(71.6833093419003,3.04121116067894,77.5133140609048));
#181527=CARTESIAN_POINT('Ctrl Pts',(71.589852058798,2.89417158313358,77.5337520085294));
#181528=CARTESIAN_POINT('Ctrl Pts',(71.5274994425849,2.78843289923142,77.547430623301));
#181529=CARTESIAN_POINT('Ctrl Pts',(71.3450888938553,2.45404469313372,77.5877832333549));
#181530=CARTESIAN_POINT('Ctrl Pts',(71.237397826488,2.21878568298582,77.612128993392));
#181531=CARTESIAN_POINT('Ctrl Pts',(71.1080121568317,1.8740638942293,77.6428669571353));
#181532=CARTESIAN_POINT('Ctrl Pts',(71.0725614609184,1.77034848667076,77.6515083564749));
#181533=CARTESIAN_POINT('Ctrl Pts',(71.01234594322,1.57544236173901,77.6666693743536));
#181534=CARTESIAN_POINT('Ctrl Pts',(70.986790834954,1.48454867398283,77.6733142641214));
#181535=CARTESIAN_POINT('Ctrl Pts',(70.9457537174226,1.32283159845772,77.6844058694877));
#181536=CARTESIAN_POINT('Ctrl Pts',(70.9293163151625,1.25228498081761,77.6890027211672));
#181537=CARTESIAN_POINT('Ctrl Pts',(70.8964622778505,1.09763050748786,77.6985595523389));
#181538=CARTESIAN_POINT('Ctrl Pts',(70.8806014113748,1.01341870140014,77.7034314598606));
#181539=CARTESIAN_POINT('Ctrl Pts',(70.8378257514775,0.753343661745575,
77.7174630723712));
#181540=CARTESIAN_POINT('Ctrl Pts',(70.8173962056347,0.576477258031514,
77.7255938220399));
#181541=CARTESIAN_POINT('Ctrl Pts',(70.7877817867805,0.135522831024074,
77.7422923261319));
#181542=CARTESIAN_POINT('Ctrl Pts',(70.7888313221881,-0.128868983708147,
77.749163479209));
#181543=CARTESIAN_POINT('Ctrl Pts',(70.8179937594841,-0.518410544724735,
77.7541583840847));
#181544=CARTESIAN_POINT('Ctrl Pts',(70.8317133884968,-0.644228455132306,
77.7549692474054));
#181545=CARTESIAN_POINT('Ctrl Pts',(70.8566253349969,-0.817951762691666,
77.7548966361948));
#181546=CARTESIAN_POINT('Ctrl Pts',(70.8642111310004,-0.866335518835818,
77.7547469582022));
#181547=CARTESIAN_POINT('Ctrl Pts',(70.8789446777879,-0.952896077184336,
77.7542402835623));
#181548=CARTESIAN_POINT('Ctrl Pts',(70.8858572987662,-0.99110887256114,
77.7539320561222));
#181549=CARTESIAN_POINT('Ctrl Pts',(70.9040476538424,-1.08603293809349,
77.7529580365788));
#181550=CARTESIAN_POINT('Ctrl Pts',(70.915805846609,-1.14264588965931,77.7521918835438));
#181551=CARTESIAN_POINT('Ctrl Pts',(70.9966400809492,-1.50369803834474,
77.7461599782457));
#181552=CARTESIAN_POINT('Ctrl Pts',(71.0901531602512,-1.80199378840545,
77.7359688303058));
#181553=CARTESIAN_POINT('Ctrl Pts',(71.294814503612,-2.30290023895625,77.7111391720313));
#181554=CARTESIAN_POINT('Ctrl Pts',(71.3945097168636,-2.50941346181454,
77.6984149052664));
#181555=CARTESIAN_POINT('Ctrl Pts',(71.5496997562606,-2.78567500115383,
77.6781214950324));
#181556=CARTESIAN_POINT('Ctrl Pts',(71.5945543093198,-2.86124526161526,
77.6722085006193));
#181557=CARTESIAN_POINT('Ctrl Pts',(71.6795377149533,-2.99694033929104,
77.6609314004789));
#181558=CARTESIAN_POINT('Ctrl Pts',(71.7190846943736,-3.05741330551257,
77.6556570891415));
#181559=CARTESIAN_POINT('Ctrl Pts',(71.8113305673564,-3.19259728148929,
77.6432984916175));
#181560=CARTESIAN_POINT('Ctrl Pts',(71.8647181737838,-3.26680234942626,
77.6361076342326));
#181561=CARTESIAN_POINT('Ctrl Pts',(72.0849079142146,-3.55732360316079,
77.6062963075679));
#181562=CARTESIAN_POINT('Ctrl Pts',(72.2657482708563,-3.76227939437997,
77.5815024458824));
#181563=CARTESIAN_POINT('Ctrl Pts',(72.5667355642835,-4.05613328083324,
77.5394092855849));
#181564=CARTESIAN_POINT('Ctrl Pts',(72.6766765676104,-4.15511079295192,
77.5238822408153));
#181565=CARTESIAN_POINT('Ctrl Pts',(72.842297519081,-4.29251415957608,77.500168283517));
#181566=CARTESIAN_POINT('Ctrl Pts',(72.8949550200511,-4.33458406741912,
77.4925837229831));
#181567=CARTESIAN_POINT('Ctrl Pts',(72.9925448899275,-4.4096444188691,77.47843061017));
#181568=CARTESIAN_POINT('Ctrl Pts',(73.0372356872186,-4.4429440650664,77.4719135345937));
#181569=CARTESIAN_POINT('Ctrl Pts',(73.116280046932,-4.49998457155734,77.460315802271));
#181570=CARTESIAN_POINT('Ctrl Pts',(73.15041497695,-4.5240277274252,77.4552840918951));
#181571=CARTESIAN_POINT('Ctrl Pts',(73.2275322192475,-4.57703449428552,
77.4438667000694));
#181572=CARTESIAN_POINT('Ctrl Pts',(73.270653839837,-4.60577930332613,77.4374492249423));
#181573=CARTESIAN_POINT('Ctrl Pts',(73.4392280095897,-4.71471384940827,
77.4122536502627));
#181574=CARTESIAN_POINT('Ctrl Pts',(73.5674688040901,-4.79032344700966,
77.392859769059));
#181575=CARTESIAN_POINT('Ctrl Pts',(73.9003579009783,-4.96858524161559,
77.3422318222505));
#181576=CARTESIAN_POINT('Ctrl Pts',(74.1086129192137,-5.06367883902265,
77.310306566457));
#181577=CARTESIAN_POINT('Ctrl Pts',(74.4194043542642,-5.18239691820562,
77.2627355876975));
#181578=CARTESIAN_POINT('Ctrl Pts',(74.5176759813545,-5.21671295687675,
77.2477020090433));
#181579=CARTESIAN_POINT('Ctrl Pts',(74.7035470299226,-5.27564158540855,
77.2193160764269));
#181580=CARTESIAN_POINT('Ctrl Pts',(74.79090048902,-5.30092267401602,77.2059951253706));
#181581=CARTESIAN_POINT('Ctrl Pts',(74.9481748430708,-5.34215609552141,
77.1820597763068));
#181582=CARTESIAN_POINT('Ctrl Pts',(75.0178572037227,-5.35894632324996,
77.1714714752744));
#181583=CARTESIAN_POINT('Ctrl Pts',(75.1727593487285,-5.39301436110121,
77.1479746126819));
#181584=CARTESIAN_POINT('Ctrl Pts',(75.2581029384633,-5.40962850005149,
77.1350559930417));
#181585=CARTESIAN_POINT('Ctrl Pts',(75.5525379293687,-5.45957942654126,
77.0905799650977));
#181586=CARTESIAN_POINT('Ctrl Pts',(75.763158296969,-5.48264371527299,77.0589329916905));
#181587=CARTESIAN_POINT('Ctrl Pts',(76.2031083107582,-5.50470442258212,
76.9930053001465));
#181588=CARTESIAN_POINT('Ctrl Pts',(76.4321381119054,-5.50158111730431,
76.9587842793382));
#181589=CARTESIAN_POINT('Ctrl Pts',(76.7778117505877,-5.47478068866244,
76.9069064286742));
#181590=CARTESIAN_POINT('Ctrl Pts',(76.8950284368944,-5.46180750578279,
76.8892722822737));
#181591=CARTESIAN_POINT('Ctrl Pts',(77.0588441352381,-5.43820561287079,
76.8645012484794));
#181592=CARTESIAN_POINT('Ctrl Pts',(77.1058745110634,-5.43079127042049,
76.8573748042622));
#181593=CARTESIAN_POINT('Ctrl Pts',(77.1907922217253,-5.41624621809818,
76.8444741869013));
#181594=CARTESIAN_POINT('Ctrl Pts',(77.2287123172768,-5.4093307798965,76.8387007532665));
#181595=CARTESIAN_POINT('Ctrl Pts',(77.3240446776781,-5.39088435093823,
76.8241573179166));
#181596=CARTESIAN_POINT('Ctrl Pts',(77.3813491211584,-5.37882236830412,
76.8153894297389));
#181597=CARTESIAN_POINT('Ctrl Pts',(77.7316389432862,-5.29909788155163,
76.7616802485711));
#181598=CARTESIAN_POINT('Ctrl Pts',(78.0187853615487,-5.20789914584257,
76.7171931143448));
#181599=CARTESIAN_POINT('Ctrl Pts',(78.5112659258398,-5.00485783530604,
76.6415294713727));
#181600=CARTESIAN_POINT('Ctrl Pts',(78.7196983601689,-4.90282012808141,
76.6097211452971));
#181601=CARTESIAN_POINT('Ctrl Pts',(78.9971787737498,-4.74421036598674,
76.5679696080069));
#181602=CARTESIAN_POINT('Ctrl Pts',(79.0721774994365,-4.69890366171995,
76.5567467104564));
#181603=CARTESIAN_POINT('Ctrl Pts',(79.2066784165441,-4.61315623753092,
76.5367433574633));
#181604=CARTESIAN_POINT('Ctrl Pts',(79.2665276897541,-4.57331508060458,
76.5278886651764));
#181605=CARTESIAN_POINT('Ctrl Pts',(79.4000994295692,-4.48053721038469,
76.5082350430473));
#181606=CARTESIAN_POINT('Ctrl Pts',(79.4733346747886,-4.42691566143916,
76.4975366348576));
#181607=CARTESIAN_POINT('Ctrl Pts',(79.7674343965113,-4.20012295502978,
76.4548894379693));
#181608=CARTESIAN_POINT('Ctrl Pts',(79.9763759104936,-4.01174434706531,
76.4253680399994));
#181609=CARTESIAN_POINT('Ctrl Pts',(80.312547334382,-3.65830305259652,76.3788158169302));
#181610=CARTESIAN_POINT('Ctrl Pts',(80.4464875160721,-3.50057980144184,
76.3605768787784));
#181611=CARTESIAN_POINT('Ctrl Pts',(80.6054013897789,-3.29050908060458,
76.3390749291356));
#181612=CARTESIAN_POINT('Ctrl Pts',(80.6388208439128,-3.24488689350982,
76.3345613056508));
#181613=CARTESIAN_POINT('Ctrl Pts',(80.6957620322285,-3.1645856415478,76.3268759964784));
#181614=CARTESIAN_POINT('Ctrl Pts',(80.7195993186736,-3.1301422246151,76.3236596437455));
#181615=CARTESIAN_POINT('Ctrl Pts',(80.7718628968255,-3.05275144795981,
76.316611529833));
#181616=CARTESIAN_POINT('Ctrl Pts',(80.8000851405014,-3.00966984574559,
76.3128089705924));
#181617=CARTESIAN_POINT('Ctrl Pts',(80.9723565348599,-2.73848186189781,
76.2896498998373));
#181618=CARTESIAN_POINT('Ctrl Pts',(81.100202013198,-2.50032034648427,76.2727143209912));
#181619=CARTESIAN_POINT('Ctrl Pts',(81.2985503851231,-2.05591375978791,
76.2480088434532));
#181620=CARTESIAN_POINT('Ctrl Pts',(81.3752213309863,-1.85310640980372,
76.2391066952939));
#181621=CARTESIAN_POINT('Ctrl Pts',(81.4674153817168,-1.55849397041057,
76.2297273589077));
#181622=CARTESIAN_POINT('Ctrl Pts',(81.4927199099784,-1.47002736294592,
76.2273501434604));
#181623=CARTESIAN_POINT('Ctrl Pts',(81.5340308173649,-1.3108550459338,76.2238651703388));
#181624=CARTESIAN_POINT('Ctrl Pts',(81.5508659261796,-1.2403906198054,76.222595204656));
#181625=CARTESIAN_POINT('Ctrl Pts',(81.5850645110894,-1.08387228916386,
76.2203786905601));
#181626=CARTESIAN_POINT('Ctrl Pts',(81.6017818015406,-0.99769577303986,
76.2195577540585));
#181627=CARTESIAN_POINT('Ctrl Pts',(81.6479195926949,-0.725831036467185,
76.2182171837524));
#181628=CARTESIAN_POINT('Ctrl Pts',(81.6700247373493,-0.539032751148363,
76.2191168628233));
#181629=CARTESIAN_POINT('Ctrl Pts',(81.6996439911372,-0.1004184491931,76.2253393397779));
#181630=CARTESIAN_POINT('Ctrl Pts',(81.6996422416693,0.151466148174329,
76.2320565924228));
#181631=CARTESIAN_POINT('Ctrl Pts',(81.6742570886569,0.525901404841964,
76.2462693347977));
#181632=CARTESIAN_POINT('Ctrl Pts',(81.6617677500643,0.649080374668952,
76.2516309395885));
#181633=CARTESIAN_POINT('Ctrl Pts',(81.6386551601267,0.819894052676462,
76.2599523369802));
#181634=CARTESIAN_POINT('Ctrl Pts',(81.6315027187836,0.86798682132388,76.2623938315713));
#181635=CARTESIAN_POINT('Ctrl Pts',(81.6175023714575,0.954300350311613,
76.2669471105319));
#181636=CARTESIAN_POINT('Ctrl Pts',(81.6108835537444,0.992555762755746,
76.2690255334203));
#181637=CARTESIAN_POINT('Ctrl Pts',(81.5933384536794,1.08797908170858,76.2743636544716));
#181638=CARTESIAN_POINT('Ctrl Pts',(81.5819129050912,1.14504590945925,76.2776953201407));
#181639=CARTESIAN_POINT('Ctrl Pts',(81.5041935953292,1.50378100727494,76.2995640680046));
#181640=CARTESIAN_POINT('Ctrl Pts',(81.4137245164432,1.79941399668105,76.3217616414451));
#181641=CARTESIAN_POINT('Ctrl Pts',(81.2138632637073,2.29937308767846,76.3682314719863));
#181642=CARTESIAN_POINT('Ctrl Pts',(81.1152788842141,2.50734621611064,76.3904997446754));
#181643=CARTESIAN_POINT('Ctrl Pts',(80.9617550773446,2.78506257271953,76.4246767954518));
#181644=CARTESIAN_POINT('Ctrl Pts',(80.9175467239182,2.86071612019881,76.4344698593547));
#181645=CARTESIAN_POINT('Ctrl Pts',(80.8337984729699,2.99649370119639,76.4529464558072));
#181646=CARTESIAN_POINT('Ctrl Pts',(80.7948398271277,3.05696817881084,76.4615146114001));
#181647=CARTESIAN_POINT('Ctrl Pts',(80.7040035991729,3.19207134774167,76.4814354468358));
#181648=CARTESIAN_POINT('Ctrl Pts',(80.6514465144278,3.26619715537172,76.4929227184661));
#181649=CARTESIAN_POINT('Ctrl Pts',(80.4325587421269,3.55919652385153,76.5406075062608));
#181650=CARTESIAN_POINT('Ctrl Pts',(80.2519225397787,3.76640761543606,76.5796380533348));
#181651=CARTESIAN_POINT('Ctrl Pts',(79.9109054377401,4.10248313616084,76.6523450992438));
#181652=CARTESIAN_POINT('Ctrl Pts',(79.7572470283821,4.23763541335688,76.684809279144));
#181653=CARTESIAN_POINT('Ctrl Pts',(79.5505286470775,4.39956203760259,76.7278397659946));
#181654=CARTESIAN_POINT('Ctrl Pts',(79.5040742195071,4.43474706847252,76.7374702657068));
#181655=CARTESIAN_POINT('Ctrl Pts',(79.4236840042652,4.49360083442434,76.7540588173398));
#181656=CARTESIAN_POINT('Ctrl Pts',(79.3900262930399,4.51764875494748,76.7609809584647));
#181657=CARTESIAN_POINT('Ctrl Pts',(79.3081665181275,4.57471749697913,76.7777616449163));
#181658=CARTESIAN_POINT('Ctrl Pts',(79.2597018907612,4.60734063210637,76.7876528358797));
#181659=CARTESIAN_POINT('Ctrl Pts',(79.0201606754448,4.76295692565485,76.8363659483317));
#181660=CARTESIAN_POINT('Ctrl Pts',(78.822064602832,4.87441600835014,76.8761231658563));
#181661=CARTESIAN_POINT('Ctrl Pts',(78.4601385650249,5.04876078011816,76.9485274962522));
#181662=CARTESIAN_POINT('Ctrl Pts',(78.299080659993,5.11682025036021,76.9806703048635));
#181663=CARTESIAN_POINT('Ctrl Pts',(78.0173195421672,5.21989599301449,77.036977655885));
#181664=CARTESIAN_POINT('Ctrl Pts',(77.8981260804415,5.25878695607624,77.0608186087014));
#181665=CARTESIAN_POINT('Ctrl Pts',(77.7053427287116,5.31423596032044,77.099455942848));
#181666=CARTESIAN_POINT('Ctrl Pts',(77.6325461967876,5.33350858403807,77.1140626305387));
#181667=CARTESIAN_POINT('Ctrl Pts',(77.4870824509904,5.36872788955947,77.1432899705638));
#181668=CARTESIAN_POINT('Ctrl Pts',(77.4144396234916,5.38470734859668,77.157905251409));
#181669=CARTESIAN_POINT('Ctrl Pts',(77.2259253519114,5.42203777861132,77.1958863954788));
#181670=CARTESIAN_POINT('Ctrl Pts',(77.1096571961192,5.44105857751182,77.2193637990583));
#181671=CARTESIAN_POINT('Ctrl Pts',(76.6568029097262,5.49971206463977,77.3109870896955));
#181672=CARTESIAN_POINT('Ctrl Pts',(76.3175287645782,5.51084061050336,77.3800709114985));
#181673=CARTESIAN_POINT('Ctrl Pts',(75.8422763109589,5.48073681899623,77.4765294975149));
#181674=CARTESIAN_POINT('Ctrl Pts',(75.7054604318992,5.46669980131952,77.5042523148631));
#181675=CARTESIAN_POINT('Ctrl Pts',(75.5204176104763,5.44039768868911,77.5415814812565));
#181676=CARTESIAN_POINT('Ctrl Pts',(75.4716301663453,5.4327658233183,77.551407556646));
#181677=CARTESIAN_POINT('Ctrl Pts',(75.4077060172307,5.42184898014661,77.5642560808688));
#181678=CARTESIAN_POINT('Ctrl Pts',(75.3924745342712,5.41917915681955,77.5673155945721));
#181679=CARTESIAN_POINT('Ctrl Pts',(75.3772542827084,5.41644264201317,77.5703707661157));
#181680=CARTESIAN_POINT('Origin',(76.0518331668413,7.15881389286582E-15,
75.8960977421633));
#181681=CARTESIAN_POINT('',(75.5398939750202,5.41644264142069,78.4927463156221));
#181682=CARTESIAN_POINT('',(75.5161728235182,5.41644264177605,78.3582169687627));
#181683=CARTESIAN_POINT('',(75.1112777726958,5.41644264156718,76.061943035002));
#181684=CARTESIAN_POINT('Ctrl Pts',(75.539893974202,5.41644264127421,78.4927463157663));
#181685=CARTESIAN_POINT('Ctrl Pts',(75.5665177744018,5.42122944939478,78.4874021020774));
#181686=CARTESIAN_POINT('Ctrl Pts',(75.5931778794221,5.42581209806781,78.4820587179476));
#181687=CARTESIAN_POINT('Ctrl Pts',(75.6780941552782,5.43973924578088,78.4650625654341));
#181688=CARTESIAN_POINT('Ctrl Pts',(75.736472255955,5.44831432884837,78.4534128479944));
#181689=CARTESIAN_POINT('Ctrl Pts',(76.0388879342549,5.48758406675844,78.3932023552001));
#181690=CARTESIAN_POINT('Ctrl Pts',(76.2847154158278,5.50222399328912,78.3447107407262));
#181691=CARTESIAN_POINT('Ctrl Pts',(76.8039561365274,5.49695258744133,78.2422088614041));
#181692=CARTESIAN_POINT('Ctrl Pts',(77.0766369260728,5.47302616476621,78.1883248440585));
#181693=CARTESIAN_POINT('Ctrl Pts',(77.4341038940642,5.41354181212434,78.1170945890549));
#181694=CARTESIAN_POINT('Ctrl Pts',(77.5215466371534,5.39671587684082,78.099625106959));
#181695=CARTESIAN_POINT('Ctrl Pts',(77.6779665538692,5.36250843993205,78.0682829388475));
#181696=CARTESIAN_POINT('Ctrl Pts',(77.7470943070347,5.345927359775,78.0543988745758));
#181697=CARTESIAN_POINT('Ctrl Pts',(77.9002886642604,5.3059077551178,78.0235543818294));
#181698=CARTESIAN_POINT('Ctrl Pts',(77.9841565591565,5.28177314589311,78.0066165093496));
#181699=CARTESIAN_POINT('Ctrl Pts',(78.3605939814393,5.16331813944078,77.9303615599141));
#181700=CARTESIAN_POINT('Ctrl Pts',(78.6454063153438,5.04570520662327,77.8719908223492));
#181701=CARTESIAN_POINT('Ctrl Pts',(79.0316094029643,4.84556850245134,77.7924229256697));
#181702=CARTESIAN_POINT('Ctrl Pts',(79.1423525774821,4.783076466589,77.7695608083373));
#181703=CARTESIAN_POINT('Ctrl Pts',(79.3233867615088,4.67225345573668,77.7321965985497));
#181704=CARTESIAN_POINT('Ctrl Pts',(79.3949004820337,4.62610461423978,77.7174393964842));
#181705=CARTESIAN_POINT('Ctrl Pts',(79.5021780677057,4.55321638765529,77.6953345547157));
#181706=CARTESIAN_POINT('Ctrl Pts',(79.5387295261656,4.52771378140688,77.6878089896472));
#181707=CARTESIAN_POINT('Ctrl Pts',(79.6126288791184,4.47477958502922,77.6726118823387));
#181708=CARTESIAN_POINT('Ctrl Pts',(79.6499487686035,4.44731388034164,77.6649465238731));
#181709=CARTESIAN_POINT('Ctrl Pts',(79.763857294428,4.36120081958458,77.6415675260766));
#181710=CARTESIAN_POINT('Ctrl Pts',(79.8392665766835,4.3009554250436,77.6261146969504));
#181711=CARTESIAN_POINT('Ctrl Pts',(80.0885517739142,4.09062617508746,77.575007143717));
#181712=CARTESIAN_POINT('Ctrl Pts',(80.2546623615278,3.93136059134858,77.540901272547));
#181713=CARTESIAN_POINT('Ctrl Pts',(80.5469721753666,3.6130712372858,77.4801270270181));
#181714=CARTESIAN_POINT('Ctrl Pts',(80.675338443127,3.45664993780459,77.4531076505331));
#181715=CARTESIAN_POINT('Ctrl Pts',(80.8446335728154,3.22520743598249,77.4167701536957));
#181716=CARTESIAN_POINT('Ctrl Pts',(80.8928821644023,3.15593243815639,77.4063225217695));
#181717=CARTESIAN_POINT('Ctrl Pts',(80.9793699369941,3.02540562892804,77.3874092379275));
#181718=CARTESIAN_POINT('Ctrl Pts',(81.0180347572513,2.96446807389958,77.3788784977968));
#181719=CARTESIAN_POINT('Ctrl Pts',(81.103945991764,2.82295789762348,77.3597415211337));
#181720=CARTESIAN_POINT('Ctrl Pts',(81.1503673026584,2.74189385766077,77.34926377095));
#181721=CARTESIAN_POINT('Ctrl Pts',(81.3389322659218,2.39219405932335,77.3060957666568));
#181722=CARTESIAN_POINT('Ctrl Pts',(81.4608682045296,2.1128937399139,77.2765636093171));
#181723=CARTESIAN_POINT('Ctrl Pts',(81.6291238048297,1.62027344458349,77.2331341000539));
#181724=CARTESIAN_POINT('Ctrl Pts',(81.6869793911751,1.41182088629801,77.2172364300291));
#181725=CARTESIAN_POINT('Ctrl Pts',(81.744848212222,1.14376142834612,77.2001896136743));
#181726=CARTESIAN_POINT('Ctrl Pts',(81.756193292366,1.08693827933067,77.196766004603));
#181727=CARTESIAN_POINT('Ctrl Pts',(81.7736595126025,0.991782815014574,
77.1913585623123));
#181728=CARTESIAN_POINT('Ctrl Pts',(81.780267274009,0.95355062558589,77.1892733976972));
#181729=CARTESIAN_POINT('Ctrl Pts',(81.7942845049315,0.867106454502926,
77.1847574348103));
#181730=CARTESIAN_POINT('Ctrl Pts',(81.8014629076115,0.818858855285828,
77.1823747812565));
#181731=CARTESIAN_POINT('Ctrl Pts',(81.8232991949716,0.657647323237761,
77.1748585102432));
#181732=CARTESIAN_POINT('Ctrl Pts',(81.8351448082689,0.544306046995467,
77.1702997685963));
#181733=CARTESIAN_POINT('Ctrl Pts',(81.8601302274017,0.205323124238502,
77.1586740364029));
#181734=CARTESIAN_POINT('Ctrl Pts',(81.8630760930305,-0.0208904111426021,
77.153548546791));
#181735=CARTESIAN_POINT('Ctrl Pts',(81.8416333136685,-0.469678367629121,
77.1479806705861));
#181736=CARTESIAN_POINT('Ctrl Pts',(81.8176059884919,-0.691840792123546,
77.1474843552474));
#181737=CARTESIAN_POINT('Ctrl Pts',(81.7656605759851,-0.998399353691106,
77.1497162701339));
#181738=CARTESIAN_POINT('Ctrl Pts',(81.7489733665241,-1.08448547846655,
77.1506705045438));
#181739=CARTESIAN_POINT('Ctrl Pts',(81.7147973777085,-1.24091561850257,
77.1529962619806));
#181740=CARTESIAN_POINT('Ctrl Pts',(81.6979543901176,-1.31138186176718,
77.1542663758805));
#181741=CARTESIAN_POINT('Ctrl Pts',(81.6565793458909,-1.47065992964979,
77.1576425557935));
#181742=CARTESIAN_POINT('Ctrl Pts',(81.6312081541514,-1.55922839791175,
77.1598813253126));
#181743=CARTESIAN_POINT('Ctrl Pts',(81.5251334061915,-1.89754847118375,
77.1698397729302));
#181744=CARTESIAN_POINT('Ctrl Pts',(81.4290088648005,-2.14202658181963,
77.1800073105019));
#181745=CARTESIAN_POINT('Ctrl Pts',(81.2178244812093,-2.58447503603234,
77.2044962166762));
#181746=CARTESIAN_POINT('Ctrl Pts',(81.107078627218,-2.78391628561171,77.2180846176862));
#181747=CARTESIAN_POINT('Ctrl Pts',(80.9547211756227,-3.02249305235994,
77.23796019709));
#181748=CARTESIAN_POINT('Ctrl Pts',(80.9242504733597,-3.06867106612347,
77.2419864274865));
#181749=CARTESIAN_POINT('Ctrl Pts',(80.8694518813549,-3.14907872777962,
77.2493242229635));
#181750=CARTESIAN_POINT('Ctrl Pts',(80.8454142331833,-3.18350427181685,
77.2525748156828));
#181751=CARTESIAN_POINT('Ctrl Pts',(80.7903402315579,-3.26050184647792,
77.2600907351692));
#181752=CARTESIAN_POINT('Ctrl Pts',(80.759086106593,-3.30290706193398,77.2644021846048));
#181753=CARTESIAN_POINT('Ctrl Pts',(80.5529060598978,-3.57444877781847,
77.2931039888029));
#181754=CARTESIAN_POINT('Ctrl Pts',(80.3610916192709,-3.78981818478707,
77.3209626744609));
#181755=CARTESIAN_POINT('Ctrl Pts',(80.032894428121,-4.10457922742631,77.3691737981482));
#181756=CARTESIAN_POINT('Ctrl Pts',(79.9071760571658,-4.21456305559467,
77.3877536693471));
#181757=CARTESIAN_POINT('Ctrl Pts',(79.6964759482369,-4.3824785826316,77.4189258860813));
#181758=CARTESIAN_POINT('Ctrl Pts',(79.6145099103994,-4.4441013151181,77.4310606536501));
#181759=CARTESIAN_POINT('Ctrl Pts',(79.4714425315016,-4.5454659874014,77.4522343788641));
#181760=CARTESIAN_POINT('Ctrl Pts',(79.4111810034324,-4.58636957987044,
77.4611511255962));
#181761=CARTESIAN_POINT('Ctrl Pts',(79.2824435024045,-4.67002469736474,
77.4801913097735));
#181762=CARTESIAN_POINT('Ctrl Pts',(79.2138022409961,-4.7124840117394,77.4903382116346));
#181763=CARTESIAN_POINT('Ctrl Pts',(79.0088055627473,-4.8330554741738,77.520624817344));
#181764=CARTESIAN_POINT('Ctrl Pts',(78.8700136197773,-4.90677137793196,
77.5411063367843));
#181765=CARTESIAN_POINT('Ctrl Pts',(78.4666325986895,-5.09903904193516,
77.6006293258309));
#181766=CARTESIAN_POINT('Ctrl Pts',(78.19557530012,-5.2024695344964,77.6406004346359));
#181767=CARTESIAN_POINT('Ctrl Pts',(77.7923905848181,-5.32027052228391,
77.7006639132548));
#181768=CARTESIAN_POINT('Ctrl Pts',(77.6657863908134,-5.35232805272204,
77.7196129603252));
#181769=CARTESIAN_POINT('Ctrl Pts',(77.4902721291951,-5.39005450177877,
77.7460901716236));
#181770=CARTESIAN_POINT('Ctrl Pts',(77.4422228882026,-5.39969944360075,
77.7533598907504));
#181771=CARTESIAN_POINT('Ctrl Pts',(77.356371468833,-5.41571833554547,77.7663934223048));
#181772=CARTESIAN_POINT('Ctrl Pts',(77.3186187131513,-5.42234669763438,
77.7721406762334));
#181773=CARTESIAN_POINT('Ctrl Pts',(77.2252250163596,-5.4377188694759,77.7863951795287));
#181774=CARTESIAN_POINT('Ctrl Pts',(77.1695160911954,-5.44599317496177,
77.7949292800279));
#181775=CARTESIAN_POINT('Ctrl Pts',(76.8372154834731,-5.49003172615719,
77.8459811802899));
#181776=CARTESIAN_POINT('Ctrl Pts',(76.5584531980336,-5.50510778397451,
77.8893903313261));
#181777=CARTESIAN_POINT('Ctrl Pts',(76.1083264897795,-5.49440722766906,
77.9593238512352));
#181778=CARTESIAN_POINT('Ctrl Pts',(75.9371778566939,-5.48212687548678,
77.9858810115573));
#181779=CARTESIAN_POINT('Ctrl Pts',(75.6408816836138,-5.44655971238055,
78.0316220270123));
#181780=CARTESIAN_POINT('Ctrl Pts',(75.5154466702457,-5.42698022544971,
78.0509127230922));
#181781=CARTESIAN_POINT('Ctrl Pts',(75.3159703938534,-5.38857655219032,
78.0814341344305));
#181782=CARTESIAN_POINT('Ctrl Pts',(75.2414546673423,-5.37258453259202,
78.0928005470773));
#181783=CARTESIAN_POINT('Ctrl Pts',(75.0946146671494,-5.33779886895718,
78.1151245375217));
#181784=CARTESIAN_POINT('Ctrl Pts',(75.0222922080519,-5.31907169105309,
78.1260833502294));
#181785=CARTESIAN_POINT('Ctrl Pts',(74.8368021017929,-5.26690931205343,
78.1540949802533));
#181786=CARTESIAN_POINT('Ctrl Pts',(74.7242785253933,-5.23124996817579,
78.1709945634405));
#181787=CARTESIAN_POINT('Ctrl Pts',(74.3398078049906,-5.09540708842723,
78.2284402534059));
#181788=CARTESIAN_POINT('Ctrl Pts',(74.0746000097748,-4.97701955461648,
78.2675163437505));
#181789=CARTESIAN_POINT('Ctrl Pts',(73.7313011908467,-4.78946040492022,
78.3178752737851));
#181790=CARTESIAN_POINT('Ctrl Pts',(73.6439977997442,-4.73855022028711,
78.3306644366919));
#181791=CARTESIAN_POINT('Ctrl Pts',(73.4955764613371,-4.64635541206792,
78.3524227783711));
#181792=CARTESIAN_POINT('Ctrl Pts',(73.4337933629486,-4.60621428909561,
78.3614851758109));
#181793=CARTESIAN_POINT('Ctrl Pts',(73.3372492650909,-4.54065805615898,
78.3756732415354));
#181794=CARTESIAN_POINT('Ctrl Pts',(73.3019473937524,-4.51606972317767,
78.3808672337088));
#181795=CARTESIAN_POINT('Ctrl Pts',(73.226402737355,-4.46210813065752,78.391999609484));
#181796=CARTESIAN_POINT('Ctrl Pts',(73.1862635163578,-4.43259519678838,
78.3979245779364));
#181797=CARTESIAN_POINT('Ctrl Pts',(73.0624666791677,-4.33892590448478,
78.4162155966171));
#181798=CARTESIAN_POINT('Ctrl Pts',(72.9802457930082,-4.27287452337565,
78.4283886038132));
#181799=CARTESIAN_POINT('Ctrl Pts',(72.6913081152475,-4.02664801642228,
78.4711133431972));
#181800=CARTESIAN_POINT('Ctrl Pts',(72.4961623461945,-3.8332272260895,78.4998475892305));
#181801=CARTESIAN_POINT('Ctrl Pts',(72.2427783739239,-3.54140578457545,
78.5362132391252));
#181802=CARTESIAN_POINT('Ctrl Pts',(72.1720308182705,-3.45473404833687,
78.5462495398058));
#181803=CARTESIAN_POINT('Ctrl Pts',(72.0457369173167,-3.29004489748573,
78.5638980712231));
#181804=CARTESIAN_POINT('Ctrl Pts',(71.9894974938757,-3.21262862070271,
78.5716476851331));
#181805=CARTESIAN_POINT('Ctrl Pts',(71.8942240416732,-3.07406705999987,
78.5845613453887));
#181806=CARTESIAN_POINT('Ctrl Pts',(71.8543389364359,-3.01355190715957,
78.5898949500262));
#181807=CARTESIAN_POINT('Ctrl Pts',(71.7704073344689,-2.8806106621182,78.6009522410751));
#181808=CARTESIAN_POINT('Ctrl Pts',(71.726807506194,-2.80791750331427,78.6065880412601));
#181809=CARTESIAN_POINT('Ctrl Pts',(71.6004339582427,-2.58585417145264,
78.6225838289649));
#181810=CARTESIAN_POINT('Ctrl Pts',(71.5228300266418,-2.43358973231042,
78.6319284667187));
#181811=CARTESIAN_POINT('Ctrl Pts',(71.3402112241093,-2.03044610650507,
78.652656119707));
#181812=CARTESIAN_POINT('Ctrl Pts',(71.2462903045331,-1.77494639163289,
78.6619469790285));
#181813=CARTESIAN_POINT('Ctrl Pts',(71.1361186458503,-1.39041840739252,
78.6709859916902));
#181814=CARTESIAN_POINT('Ctrl Pts',(71.1050972657586,-1.26610252129917,
78.6731835867271));
#181815=CARTESIAN_POINT('Ctrl Pts',(71.0681546925613,-1.09275858434809,
78.675333330361));
#181816=CARTESIAN_POINT('Ctrl Pts',(71.0585497610332,-1.04456345494294,
78.6758346158716));
#181817=CARTESIAN_POINT('Ctrl Pts',(71.0425063765194,-0.958089087027191,
78.676568349917));
#181818=CARTESIAN_POINT('Ctrl Pts',(71.0358274989382,-0.91985910316115,
78.6768357216557));
#181819=CARTESIAN_POINT('Ctrl Pts',(71.0202391821798,-0.824762928478273,
78.6773571363275));
#181820=CARTESIAN_POINT('Ctrl Pts',(71.0118118691523,-0.767822499697789,
78.6775415709439));
#181821=CARTESIAN_POINT('Ctrl Pts',(70.9631488273098,-0.399653947324125,
78.6778684629793));
#181822=CARTESIAN_POINT('Ctrl Pts',(70.9484260216193,-0.0856397834854804,
78.6741369816039));
#181823=CARTESIAN_POINT('Ctrl Pts',(70.968621281735,0.456166789450836,78.6593018635788));
#181824=CARTESIAN_POINT('Ctrl Pts',(70.9911209463974,0.68367151133436,78.650497229422));
#181825=CARTESIAN_POINT('Ctrl Pts',(71.0414320539691,0.995821165341956,
78.6345756643245));
#181826=CARTESIAN_POINT('Ctrl Pts',(71.057461944349,1.0822404374931,78.6297541703661));
#181827=CARTESIAN_POINT('Ctrl Pts',(71.0903831498529,1.23899471873172,78.6202425210799));
#181828=CARTESIAN_POINT('Ctrl Pts',(71.1066171634054,1.30945506728566,78.6156810242576));
#181829=CARTESIAN_POINT('Ctrl Pts',(71.1464951642544,1.46835047768269,78.6047409343273));
#181830=CARTESIAN_POINT('Ctrl Pts',(71.1709546760956,1.5565475755069,78.5982036220449));
#181831=CARTESIAN_POINT('Ctrl Pts',(71.2765333922488,1.90376887941866,78.5706167117745));
#181832=CARTESIAN_POINT('Ctrl Pts',(71.3743113914344,2.15706435303863,78.5463327671822));
#181833=CARTESIAN_POINT('Ctrl Pts',(71.5538605775691,2.53655989634403,78.503714009829));
#181834=CARTESIAN_POINT('Ctrl Pts',(71.6229752197624,2.66852330555532,78.4876395622037));
#181835=CARTESIAN_POINT('Ctrl Pts',(71.7311117628383,2.85602254511148,78.4630476428724));
#181836=CARTESIAN_POINT('Ctrl Pts',(71.7659744502709,2.91396650301486,78.4551933440778));
#181837=CARTESIAN_POINT('Ctrl Pts',(71.8315758297514,3.01856094504793,78.4405610247926));
#181838=CARTESIAN_POINT('Ctrl Pts',(71.8619763120377,3.06542003597401,78.4338336662169));
#181839=CARTESIAN_POINT('Ctrl Pts',(71.9163318417643,3.14645162855411,78.4219058391388));
#181840=CARTESIAN_POINT('Ctrl Pts',(71.9399722326786,3.18083431925575,78.4167503194992));
#181841=CARTESIAN_POINT('Ctrl Pts',(71.9937660405051,3.25718009657928,78.4050877751693));
#181842=CARTESIAN_POINT('Ctrl Pts',(72.0241234831559,3.29898860917227,78.3985518950606));
#181843=CARTESIAN_POINT('Ctrl Pts',(72.2297334469484,3.57385211125529,78.3545483118859));
#181844=CARTESIAN_POINT('Ctrl Pts',(72.42264726793,3.79267421678239,78.3144783538201));
#181845=CARTESIAN_POINT('Ctrl Pts',(72.7499304046403,4.10878341039927,78.2470501284729));
#181846=CARTESIAN_POINT('Ctrl Pts',(72.8730484526604,4.21733885557447,78.221793698017));
#181847=CARTESIAN_POINT('Ctrl Pts',(73.0799640708631,4.38370528203187,78.1793791948582));
#181848=CARTESIAN_POINT('Ctrl Pts',(73.1608731819593,4.44508420747317,78.1628022110368));
#181849=CARTESIAN_POINT('Ctrl Pts',(73.302254780683,4.54618307035463,78.133828427201));
#181850=CARTESIAN_POINT('Ctrl Pts',(73.3619072495882,4.58704970840229,78.1216017655663));
#181851=CARTESIAN_POINT('Ctrl Pts',(73.4894959199848,4.67073247008104,78.0954416852499));
#181852=CARTESIAN_POINT('Ctrl Pts',(73.5575996432741,4.71324952918654,78.0814729018663));
#181853=CARTESIAN_POINT('Ctrl Pts',(73.7616905816327,4.8343910698883,78.0395943951052));
#181854=CARTESIAN_POINT('Ctrl Pts',(73.900125837051,4.90854005609326,78.0111636560783));
#181855=CARTESIAN_POINT('Ctrl Pts',(74.2994943305779,5.10033784862872,77.929141629216));
#181856=CARTESIAN_POINT('Ctrl Pts',(74.5666851817975,5.20314329706973,77.8742417152858));
#181857=CARTESIAN_POINT('Ctrl Pts',(74.9269828464728,5.30934202677185,77.8007639257383));
#181858=CARTESIAN_POINT('Ctrl Pts',(75.0139270501562,5.33258114578658,77.7830763097766));
#181859=CARTESIAN_POINT('Ctrl Pts',(75.166994885496,5.36934406062368,77.7520488281465));
#181860=CARTESIAN_POINT('Ctrl Pts',(75.2328687744806,5.38384044302114,77.7387317678352));
#181861=CARTESIAN_POINT('Ctrl Pts',(75.3329277893673,5.40386335678467,77.7185726417664));
#181862=CARTESIAN_POINT('Ctrl Pts',(75.3669210508875,5.41031985689093,77.7117358726658));
#181863=CARTESIAN_POINT('Ctrl Pts',(75.4009754336941,5.41644264156649,77.7049001130302));
#181864=CARTESIAN_POINT('Ctrl Pts',(75.3772542827084,5.41644264201317,77.5703707661157));
#181865=CARTESIAN_POINT('Ctrl Pts',(75.3551306632751,5.41246494086284,77.5748116554304));
#181866=CARTESIAN_POINT('Ctrl Pts',(75.3330307739513,5.40834633171858,77.5792433706657));
#181867=CARTESIAN_POINT('Ctrl Pts',(75.2571593468384,5.39370708975354,77.5944443211266));
#181868=CARTESIAN_POINT('Ctrl Pts',(75.2035167710473,5.38249264657263,77.6051681275127));
#181869=CARTESIAN_POINT('Ctrl Pts',(74.8673311105018,5.30675913195313,77.6722670827772));
#181870=CARTESIAN_POINT('Ctrl Pts',(74.5900166783592,5.2199703866233,77.727155541709));
#181871=CARTESIAN_POINT('Ctrl Pts',(74.1681931649929,5.04902273212223,77.8111284089395));
#181872=CARTESIAN_POINT('Ctrl Pts',(74.0183340153448,4.98004591998959,77.8410578583084));
#181873=CARTESIAN_POINT('Ctrl Pts',(73.7619402997817,4.84731565757822,77.8925954191191));
#181874=CARTESIAN_POINT('Ctrl Pts',(73.6540142440242,4.78660439634999,77.9143977290939));
#181875=CARTESIAN_POINT('Ctrl Pts',(73.4837556395166,4.68289376102598,77.9490048065502));
#181876=CARTESIAN_POINT('Ctrl Pts',(73.4200865652762,4.64224053912069,77.9619961894697));
#181877=CARTESIAN_POINT('Ctrl Pts',(73.2951293503213,4.55868535663434,77.9875984063133));
#181878=CARTESIAN_POINT('Ctrl Pts',(73.2338368344033,4.51582034164073,78.0002090200944));
#181879=CARTESIAN_POINT('Ctrl Pts',(73.0766053921483,4.40089612641961,78.0326981335471));
#181880=CARTESIAN_POINT('Ctrl Pts',(72.9821200638585,4.3268594986081,78.0523623813962));
#181881=CARTESIAN_POINT('Ctrl Pts',(72.6694402219715,4.06452273194333,78.1178964355982));
#181882=CARTESIAN_POINT('Ctrl Pts',(72.4636574405655,3.86172294495375,78.1618513475365));
#181883=CARTESIAN_POINT('Ctrl Pts',(72.2099623126922,3.56839580079293,78.2166814682362));
#181884=CARTESIAN_POINT('Ctrl Pts',(72.1472678171828,3.49178931474804,78.230289047022));
#181885=CARTESIAN_POINT('Ctrl Pts',(72.0421899545113,3.35603549676313,78.2531540813623));
#181886=CARTESIAN_POINT('Ctrl Pts',(71.9988559849183,3.29768821002673,78.2626022152662));
#181887=CARTESIAN_POINT('Ctrl Pts',(71.9318111555133,3.20356605885862,78.2772320799985));
#181888=CARTESIAN_POINT('Ctrl Pts',(71.9073496634705,3.16836087057786,78.2825723246921));
#181889=CARTESIAN_POINT('Ctrl Pts',(71.8551700506616,3.09135817231146,78.2939651380305));
#181890=CARTESIAN_POINT('Ctrl Pts',(71.8276048236484,3.04945806195616,78.2999855424708));
#181891=CARTESIAN_POINT('Ctrl Pts',(71.7427282493247,2.91652037943227,78.3185437502732));
#181892=CARTESIAN_POINT('Ctrl Pts',(71.6874823286298,2.82413590909042,78.3306544083646));
#181893=CARTESIAN_POINT('Ctrl Pts',(71.5022572925732,2.49271866192628,78.371525469451));
#181894=CARTESIAN_POINT('Ctrl Pts',(71.3871468829608,2.24549796197737,78.3974526902117));
#181895=CARTESIAN_POINT('Ctrl Pts',(71.2640528520746,1.92020105936863,78.4266332599623));
#181896=CARTESIAN_POINT('Ctrl Pts',(71.2388690923248,1.8493134666371,78.4327052831731));
#181897=CARTESIAN_POINT('Ctrl Pts',(71.1797768411235,1.67156520371003,78.4472397172474));
#181898=CARTESIAN_POINT('Ctrl Pts',(71.1476474192826,1.56412638737289,78.4554139430176));
#181899=CARTESIAN_POINT('Ctrl Pts',(71.0996585460341,1.38388449494464,78.4681484903561));
#181900=CARTESIAN_POINT('Ctrl Pts',(71.0819693264505,1.31162489661964,78.4729970910972));
#181901=CARTESIAN_POINT('Ctrl Pts',(71.0486482107059,1.16258278093309,78.482479040289));
#181902=CARTESIAN_POINT('Ctrl Pts',(71.0331777364175,1.08577989366263,78.4870864964874));
#181903=CARTESIAN_POINT('Ctrl Pts',(70.99501289964,0.873149227891994,78.4990803089403));
#181904=CARTESIAN_POINT('Ctrl Pts',(70.9757320723611,0.736737432565285,
78.5059261166379));
#181905=CARTESIAN_POINT('Ctrl Pts',(70.9413112111456,0.404602046368871,
78.520524399549));
#181906=CARTESIAN_POINT('Ctrl Pts',(70.9314168130957,0.208487155890121,
78.5274236904707));
#181907=CARTESIAN_POINT('Ctrl Pts',(70.9324223884411,-0.224800901825671,
78.5386663569182));
#181908=CARTESIAN_POINT('Ctrl Pts',(70.9480635829902,-0.461601469887723,
78.5421726518326));
#181909=CARTESIAN_POINT('Ctrl Pts',(70.9863635500486,-0.756066219738908,
78.5428292352717));
#181910=CARTESIAN_POINT('Ctrl Pts',(70.9950334161317,-0.815295897793722,
78.5427708069543));
#181911=CARTESIAN_POINT('Ctrl Pts',(71.0109206396469,-0.912915291205025,
78.5423486093226));
#181912=CARTESIAN_POINT('Ctrl Pts',(71.0175946239952,-0.951388755684431,
78.5420978021178));
#181913=CARTESIAN_POINT('Ctrl Pts',(71.0333257423385,-1.0367778158736,78.5413509608545));
#181914=CARTESIAN_POINT('Ctrl Pts',(71.0425812932071,-1.08365230719983,
78.5408135609644));
#181915=CARTESIAN_POINT('Ctrl Pts',(71.0764055856693,-1.24413800401546,
78.5385484675323));
#181916=CARTESIAN_POINT('Ctrl Pts',(71.1039042681785,-1.35709090290732,
78.5362195797992));
#181917=CARTESIAN_POINT('Ctrl Pts',(71.1934290721886,-1.68059364153978,
78.5275635981392));
#181918=CARTESIAN_POINT('Ctrl Pts',(71.2643449283296,-1.88840066118407,
78.5195369611606));
#181919=CARTESIAN_POINT('Ctrl Pts',(71.4322724944426,-2.29924745081154,
78.4991612329898));
#181920=CARTESIAN_POINT('Ctrl Pts',(71.5297081509498,-2.50166271137656,
78.4867348914563));
#181921=CARTESIAN_POINT('Ctrl Pts',(71.6827111072875,-2.77556385226428,
78.4667446956249));
#181922=CARTESIAN_POINT('Ctrl Pts',(71.7281923492761,-2.85253694011235,
78.4607526491086));
#181923=CARTESIAN_POINT('Ctrl Pts',(71.8137575012774,-2.98963833760957,
78.4494031203047));
#181924=CARTESIAN_POINT('Ctrl Pts',(71.8531959219295,-3.05015323918425,
78.4441452894191));
#181925=CARTESIAN_POINT('Ctrl Pts',(71.9442722491566,-3.18407814421525,
78.4319477378013));
#181926=CARTESIAN_POINT('Ctrl Pts',(71.9965330672359,-3.25703049324408,
78.424911617405));
#181927=CARTESIAN_POINT('Ctrl Pts',(72.1987427780659,-3.52521697386439,
78.3975484236171));
#181928=CARTESIAN_POINT('Ctrl Pts',(72.3598588773342,-3.71148662420113,
78.3754908419883));
#181929=CARTESIAN_POINT('Ctrl Pts',(72.7028229027418,-4.05804666259696,
78.3277333828107));
#181930=CARTESIAN_POINT('Ctrl Pts',(72.8839141088621,-4.21833837794861,
78.302148057298));
#181931=CARTESIAN_POINT('Ctrl Pts',(73.1163156600455,-4.39815580145707,
78.2684790005611));
#181932=CARTESIAN_POINT('Ctrl Pts',(73.1582928590878,-4.429680255181,78.2623662342311));
#181933=CARTESIAN_POINT('Ctrl Pts',(73.2345053836241,-4.48521880950411,
78.2512045193478));
#181934=CARTESIAN_POINT('Ctrl Pts',(73.2685780405339,-4.50945549544521,
78.2461917010365));
#181935=CARTESIAN_POINT('Ctrl Pts',(73.3481561464184,-4.56469790617357,
78.2344304348218));
#181936=CARTESIAN_POINT('Ctrl Pts',(73.3938535732458,-4.59540760812734,
78.2276380224887));
#181937=CARTESIAN_POINT('Ctrl Pts',(73.6190821478091,-4.74186784983181,
78.1940037271525));
#181938=CARTESIAN_POINT('Ctrl Pts',(73.8046980317652,-4.84759864289241,
78.1658127326164));
#181939=CARTESIAN_POINT('Ctrl Pts',(74.2420269907349,-5.06360827697723,
78.0990593564817));
#181940=CARTESIAN_POINT('Ctrl Pts',(74.496801694948,-5.16618469854028,78.059950463295));
#181941=CARTESIAN_POINT('Ctrl Pts',(74.8445615408675,-5.27626147679226,
78.0068425413925));
#181942=CARTESIAN_POINT('Ctrl Pts',(74.9316261869138,-5.30142343629455,
77.9935659997728));
#181943=CARTESIAN_POINT('Ctrl Pts',(75.0886038253393,-5.34253034104682,
77.9696763487962));
#181944=CARTESIAN_POINT('Ctrl Pts',(75.1582824926091,-5.35929844186769,
77.9590888645066));
#181945=CARTESIAN_POINT('Ctrl Pts',(75.3134418479235,-5.39337657997133,
77.9355535623203));
#181946=CARTESIAN_POINT('Ctrl Pts',(75.3990488143221,-5.41001011726648,
77.9225954843572));
#181947=CARTESIAN_POINT('Ctrl Pts',(75.7102093890379,-5.46266031799454,
77.8755946931989));
#181948=CARTESIAN_POINT('Ctrl Pts',(75.9375781786611,-5.48639139088477,
77.8414483751284));
#181949=CARTESIAN_POINT('Ctrl Pts',(76.4717560240562,-5.50797522293383,
77.7614291770985));
#181950=CARTESIAN_POINT('Ctrl Pts',(76.7782687619571,-5.49420419072485,
77.7156823754374));
#181951=CARTESIAN_POINT('Ctrl Pts',(77.1390469762435,-5.44696380195649,
77.6612324020674));
#181952=CARTESIAN_POINT('Ctrl Pts',(77.196053242006,-5.43856610476701,77.6526094692588));
#181953=CARTESIAN_POINT('Ctrl Pts',(77.2908545206037,-5.4230409792205,77.6382272438688));
#181954=CARTESIAN_POINT('Ctrl Pts',(77.3287278389919,-5.41642103018427,
77.632469865077));
#181955=CARTESIAN_POINT('Ctrl Pts',(77.4138797709276,-5.40059452945907,
77.6194973246863));
#181956=CARTESIAN_POINT('Ctrl Pts',(77.4611114023374,-5.39115805624824,
77.6122831750434));
#181957=CARTESIAN_POINT('Ctrl Pts',(77.6281990785717,-5.3554358377391,77.5867110065965));
#181958=CARTESIAN_POINT('Ctrl Pts',(77.7472809501946,-5.32568489488279,
77.5683925200686));
#181959=CARTESIAN_POINT('Ctrl Pts',(78.1053770441845,-5.22310057412976,
77.5132174135964));
#181960=CARTESIAN_POINT('Ctrl Pts',(78.3405070859524,-5.13767354331611,
77.4768790226374));
#181961=CARTESIAN_POINT('Ctrl Pts',(78.7404301020967,-4.96013116249166,
77.415616902084));
#181962=CARTESIAN_POINT('Ctrl Pts',(78.9078309619874,-4.875156892705,77.3901504149331));
#181963=CARTESIAN_POINT('Ctrl Pts',(79.1453763270134,-4.73866867900507,
77.3544256550122));
#181964=CARTESIAN_POINT('Ctrl Pts',(79.2191314864121,-4.69392572879059,
77.3433938929701));
#181965=CARTESIAN_POINT('Ctrl Pts',(79.351830212482,-4.6090497848127,77.32366616379));
#181966=CARTESIAN_POINT('Ctrl Pts',(79.4111012832259,-4.5694813702983,77.3149001516919));
#181967=CARTESIAN_POINT('Ctrl Pts',(79.5450674680594,-4.47620387280451,
77.2951948048033));
#181968=CARTESIAN_POINT('Ctrl Pts',(79.6192254649066,-4.4217385150286,77.2843663292351));
#181969=CARTESIAN_POINT('Ctrl Pts',(79.8661236949224,-4.23062963903575,
77.2485833938717));
#181970=CARTESIAN_POINT('Ctrl Pts',(80.0321020875712,-4.0853500526018,77.2249996989916));
#181971=CARTESIAN_POINT('Ctrl Pts',(80.3770877452172,-3.74458755207061,
77.1768042557059));
#181972=CARTESIAN_POINT('Ctrl Pts',(80.5516846779828,-3.54530748027666,
77.1529849231373));
#181973=CARTESIAN_POINT('Ctrl Pts',(80.7449291807962,-3.289671324393,77.1268388796537));
#181974=CARTESIAN_POINT('Ctrl Pts',(80.7778337073023,-3.24474172580001,
77.1223948018454));
#181975=CARTESIAN_POINT('Ctrl Pts',(80.8342795116069,-3.16516024457205,
77.1147763120518));
#181976=CARTESIAN_POINT('Ctrl Pts',(80.8581152007823,-3.13072857974572,
77.1115601736501));
#181977=CARTESIAN_POINT('Ctrl Pts',(80.9159704515299,-3.04508198641242,
77.103757919598));
#181978=CARTESIAN_POINT('Ctrl Pts',(80.9495317145112,-2.99355997477047,
77.0992367451616));
#181979=CARTESIAN_POINT('Ctrl Pts',(81.0806542452679,-2.78471121802515,
77.0816257209535));
#181980=CARTESIAN_POINT('Ctrl Pts',(81.1711708943279,-2.62301976716516,
77.0695947879003));
#181981=CARTESIAN_POINT('Ctrl Pts',(81.3846939471021,-2.19232821640308,
77.0420862662766));
#181982=CARTESIAN_POINT('Ctrl Pts',(81.494668396106,-1.91739730959131,77.0288802362698));
#181983=CARTESIAN_POINT('Ctrl Pts',(81.6092575918458,-1.54846266234088,
77.0172939596629));
#181984=CARTESIAN_POINT('Ctrl Pts',(81.6340076070984,-1.46136286947176,
77.0149840412515));
#181985=CARTESIAN_POINT('Ctrl Pts',(81.6747303956036,-1.30358551011628,
77.0115720452801));
#181986=CARTESIAN_POINT('Ctrl Pts',(81.6914641784746,-1.23312949497981,
77.0103209662707));
#181987=CARTESIAN_POINT('Ctrl Pts',(81.7257212797353,-1.07534102745151,
77.0081278597913));
#181988=CARTESIAN_POINT('Ctrl Pts',(81.7425374873427,-0.987874062180328,
77.0073233186233));
#181989=CARTESIAN_POINT('Ctrl Pts',(81.7984979681635,-0.654057669637169,
77.0058079408019));
#181990=CARTESIAN_POINT('Ctrl Pts',(81.8232638414437,-0.405590901814358,
77.0078914150837));
#181991=CARTESIAN_POINT('Ctrl Pts',(81.8408767982921,0.136259595556882,
77.0190341318126));
#181992=CARTESIAN_POINT('Ctrl Pts',(81.8273896706965,0.429076623559226,
77.0292306958749));
#181993=CARTESIAN_POINT('Ctrl Pts',(81.7839324949371,0.775010049311216,
77.0455679559407));
#181994=CARTESIAN_POINT('Ctrl Pts',(81.7760903008232,0.830602387995591,
77.0483262831829));
#181995=CARTESIAN_POINT('Ctrl Pts',(81.7614262060612,0.924244870551358,
77.0531885307232));
#181996=CARTESIAN_POINT('Ctrl Pts',(81.7550476793131,0.962362850263627,
77.0552281602543));
#181997=CARTESIAN_POINT('Ctrl Pts',(81.7395031108337,1.04963382120321,77.0600357087681));
#181998=CARTESIAN_POINT('Ctrl Pts',(81.7300698954508,1.09873251147178,77.0628421610904));
#181999=CARTESIAN_POINT('Ctrl Pts',(81.6922889676162,1.28195922764356,77.0737136548726));
#182000=CARTESIAN_POINT('Ctrl Pts',(81.6596380006978,1.41510979657309,77.0824176659593));
#182001=CARTESIAN_POINT('Ctrl Pts',(81.5331782405383,1.85902405533254,77.1144528298743));
#182002=CARTESIAN_POINT('Ctrl Pts',(81.4171056511614,2.16245303430398,77.141466786713));
#182003=CARTESIAN_POINT('Ctrl Pts',(81.2172769762977,2.57296674037598,77.1865563833648));
#182004=CARTESIAN_POINT('Ctrl Pts',(81.1549207734837,2.69013927909417,77.2004816465146));
#182005=CARTESIAN_POINT('Ctrl Pts',(81.0496810078485,2.87178631257707,77.2238139688302));
#182006=CARTESIAN_POINT('Ctrl Pts',(81.0095262863717,2.93784854735424,77.2326820075019));
#182007=CARTESIAN_POINT('Ctrl Pts',(80.9280209391364,3.06578982023334,77.2506219619903));
#182008=CARTESIAN_POINT('Ctrl Pts',(80.8867771179038,3.12771983020459,77.2596724989083));
#182009=CARTESIAN_POINT('Ctrl Pts',(80.778955250213,3.28270065381025,77.2832663043536));
#182010=CARTESIAN_POINT('Ctrl Pts',(80.7107247356784,3.37450706614495,77.2981368225682));
#182011=CARTESIAN_POINT('Ctrl Pts',(80.5475752770769,3.58023758284994,77.333547134879));
#182012=CARTESIAN_POINT('Ctrl Pts',(80.4508235937867,3.69253015902679,77.3544434884665));
#182013=CARTESIAN_POINT('Ctrl Pts',(80.1524629299034,4.01151090457892,77.4184755616101));
#182014=CARTESIAN_POINT('Ctrl Pts',(79.9390498331029,4.20600000770045,77.4637937421474));
#182015=CARTESIAN_POINT('Ctrl Pts',(79.6688042917803,4.41523690861074,77.5199665530783));
#182016=CARTESIAN_POINT('Ctrl Pts',(79.6257502800877,4.44754849985687,77.528881276898));
#182017=CARTESIAN_POINT('Ctrl Pts',(79.5485442093124,4.50369564896925,77.5447984217472));
#182018=CARTESIAN_POINT('Ctrl Pts',(79.5145842482227,4.52779303181809,77.5517759230397));
#182019=CARTESIAN_POINT('Ctrl Pts',(79.4276978569702,4.58793715953203,77.569571052899));
#182020=CARTESIAN_POINT('Ctrl Pts',(79.3744066450802,4.62343102526966,77.5804341139877));
#182021=CARTESIAN_POINT('Ctrl Pts',(79.2511332780576,4.70238535303766,77.6054685321576));
#182022=CARTESIAN_POINT('Ctrl Pts',(79.1807663898367,4.74519842856199,77.6196914080793));
#182023=CARTESIAN_POINT('Ctrl Pts',(78.9103347465932,4.90130966127014,77.6741742056773));
#182024=CARTESIAN_POINT('Ctrl Pts',(78.7041753801489,5.00322003312319,77.7153569978125));
#182025=CARTESIAN_POINT('Ctrl Pts',(78.3327149916367,5.15793848190996,77.7895567050763));
#182026=CARTESIAN_POINT('Ctrl Pts',(78.1701091356487,5.21656711419243,77.8220339134506));
#182027=CARTESIAN_POINT('Ctrl Pts',(77.9256536568818,5.29149181960343,77.870983437678));
#182028=CARTESIAN_POINT('Ctrl Pts',(77.8457258618932,5.31395573612381,77.8870064885063));
#182029=CARTESIAN_POINT('Ctrl Pts',(77.6961658935369,5.35223292687144,77.9170324916188));
#182030=CARTESIAN_POINT('Ctrl Pts',(77.6266711965583,5.36853309543603,77.9310017037321));
#182031=CARTESIAN_POINT('Ctrl Pts',(77.4643084553455,5.40317598499173,77.9636822491622));
#182032=CARTESIAN_POINT('Ctrl Pts',(77.3712464870708,5.42044161914755,77.9824470464339));
#182033=CARTESIAN_POINT('Ctrl Pts',(77.0448123127249,5.47200266632727,78.0483814223472));
#182034=CARTESIAN_POINT('Ctrl Pts',(76.8097572798377,5.49318038295565,78.0960720442571));
#182035=CARTESIAN_POINT('Ctrl Pts',(76.2989801747345,5.50493167208876,78.199847677639));
#182036=CARTESIAN_POINT('Ctrl Pts',(76.0237871485224,5.48976380034184,78.2558521585353));
#182037=CARTESIAN_POINT('Ctrl Pts',(75.6956875849196,5.44584497720425,78.322100559458));
#182038=CARTESIAN_POINT('Ctrl Pts',(75.6406274761654,5.43758927256413,78.3331992247991));
#182039=CARTESIAN_POINT('Ctrl Pts',(75.5624980574765,5.42461269953035,78.3489132435704));
#182040=CARTESIAN_POINT('Ctrl Pts',(75.5393227029819,5.42060485865232,78.3535700775961));
#182041=CARTESIAN_POINT('Ctrl Pts',(75.5161728246847,5.41644264198492,78.358216968557));
#182042=CARTESIAN_POINT('Origin',(76.1212924379081,7.15881389286582E-15,
76.2900208433682));
#182043=CARTESIAN_POINT('',(75.1812918055742,5.62353578632127,76.6693002371056));
#182044=CARTESIAN_POINT('',(75.1807370437626,5.41644264156715,76.4558661362069));
#182045=CARTESIAN_POINT('',(75.1807370437626,5.41644264156718,76.4558661362069));
#182046=CARTESIAN_POINT('Ctrl Pts',(75.1812918055743,5.62353578632128,76.6693002371056));
#182047=CARTESIAN_POINT('Ctrl Pts',(75.3571628611358,5.65249493893739,76.6356794593437));
#182048=CARTESIAN_POINT('Ctrl Pts',(75.5392018334951,5.67354545131171,76.6007060003843));
#182049=CARTESIAN_POINT('Ctrl Pts',(76.4013260614393,5.72703701773099,76.4347216202953));
#182050=CARTESIAN_POINT('Ctrl Pts',(77.0795952398394,5.64345323809595,76.3037649317242));
#182051=CARTESIAN_POINT('Ctrl Pts',(78.3313431664491,5.25009364564398,76.0645802175305));
#182052=CARTESIAN_POINT('Ctrl Pts',(78.9730340238476,4.9347614241347,75.9433917035655));
#182053=CARTESIAN_POINT('Ctrl Pts',(80.1203906190512,3.99017560718347,75.7178789883305));
#182054=CARTESIAN_POINT('Ctrl Pts',(80.579679906946,3.43286338982664,75.6247561696959));
#182055=CARTESIAN_POINT('Ctrl Pts',(81.2545152194198,2.20195736568136,75.486134896178));
#182056=CARTESIAN_POINT('Ctrl Pts',(81.4757538887496,1.53878263947313,75.4394015224678));
#182057=CARTESIAN_POINT('Ctrl Pts',(81.6668477957519,0.11632693193044,75.3839335879276));
#182058=CARTESIAN_POINT('Ctrl Pts',(81.6175680342668,-0.63462652993374,
75.3793749075201));
#182059=CARTESIAN_POINT('Ctrl Pts',(81.301051587549,-1.82835714239946,75.4171500760812));
#182060=CARTESIAN_POINT('Ctrl Pts',(81.1132524101206,-2.28694413181046,
75.4439714552156));
#182061=CARTESIAN_POINT('Ctrl Pts',(80.5715823219023,-3.22898572750882,
75.5247634044448));
#182062=CARTESIAN_POINT('Ctrl Pts',(80.1950180370635,-3.68900287460553,
75.5813656397829));
#182063=CARTESIAN_POINT('Ctrl Pts',(79.7540569593757,-4.07954801327268,
75.6494664436731));
#182064=CARTESIAN_POINT('Origin',(76.1212924379081,7.15881389286582E-15,
76.2900208433682));
#182065=CARTESIAN_POINT('Origin',(76.5901425176087,7.15881389286582E-15,
78.9490017765011));
#182066=CARTESIAN_POINT('',(77.4871784401325,-5.90884651804035,78.0363452943797));
#182067=CARTESIAN_POINT('',(77.5021200054788,-5.908846518253,78.1210831292301));
#182068=CARTESIAN_POINT('',(77.6162029475856,-5.90884651807327,78.7680796388589));
#182069=CARTESIAN_POINT('',(79.5631824082914,5.13997981404828,77.9850820082636));
#182070=CARTESIAN_POINT('Ctrl Pts',(77.4871784403164,-5.90884651800743,
78.0363452943473));
#182071=CARTESIAN_POINT('Ctrl Pts',(77.4934521895834,-5.90772748441951,
78.0353782935762));
#182072=CARTESIAN_POINT('Ctrl Pts',(77.4997242490394,-5.90659822221011,
78.0344119531403));
#182073=CARTESIAN_POINT('Ctrl Pts',(77.5491905020832,-5.89760890063681,
78.0267937527027));
#182074=CARTESIAN_POINT('Ctrl Pts',(77.5923018430072,-5.88927441212067,
78.0201728980026));
#182075=CARTESIAN_POINT('Ctrl Pts',(77.7226204751505,-5.86256270962865,
78.0002086856151));
#182076=CARTESIAN_POINT('Ctrl Pts',(77.809521806952,-5.84268235841269,77.9869632148244));
#182077=CARTESIAN_POINT('Ctrl Pts',(78.0252391937274,-5.7881465162295,77.9542074513322));
#182078=CARTESIAN_POINT('Ctrl Pts',(78.1534159958275,-5.75106742878112,
77.9348553780247));
#182079=CARTESIAN_POINT('Ctrl Pts',(78.6427061846875,-5.59132845044584,
77.8612129409205));
#182080=CARTESIAN_POINT('Ctrl Pts',(78.9931348457252,-5.4379969721673,77.8088954667391));
#182081=CARTESIAN_POINT('Ctrl Pts',(79.4129114087173,-5.20356389190537,
77.7459651290228));
#182082=CARTESIAN_POINT('Ctrl Pts',(79.4980462611288,-5.15317808949757,
77.7331925421746));
#182083=CARTESIAN_POINT('Ctrl Pts',(79.6433710922886,-5.06217692221251,
77.7113713228665));
#182084=CARTESIAN_POINT('Ctrl Pts',(79.7041421115543,-5.02255065225972,
77.702240540578));
#182085=CARTESIAN_POINT('Ctrl Pts',(79.8313313603613,-4.93624736284486,
77.6831207384009));
#182086=CARTESIAN_POINT('Ctrl Pts',(79.897552498061,-4.88930027149069,77.6731601456358));
#182087=CARTESIAN_POINT('Ctrl Pts',(80.0901498220812,-4.74673485561338,
77.6441837217559));
#182088=CARTESIAN_POINT('Ctrl Pts',(80.2137244739563,-4.64737175146598,
77.6255808618117));
#182089=CARTESIAN_POINT('Ctrl Pts',(80.5288369694172,-4.37257703915636,
77.5782399702202));
#182090=CARTESIAN_POINT('Ctrl Pts',(80.7132224137751,-4.1892832444789,77.5506310886405));
#182091=CARTESIAN_POINT('Ctrl Pts',(80.9924998716715,-3.87301939500085,
77.5095547870779));
#182092=CARTESIAN_POINT('Ctrl Pts',(81.0948131596446,-3.7472518757893,77.4947003301369));
#182093=CARTESIAN_POINT('Ctrl Pts',(81.2246072081861,-3.57387616237588,
77.4762834899382));
#182094=CARTESIAN_POINT('Ctrl Pts',(81.2566377307307,-3.52986284709273,
77.4717767011675));
#182095=CARTESIAN_POINT('Ctrl Pts',(81.312165945205,-3.45135528198662,77.4640408238861));
#182096=CARTESIAN_POINT('Ctrl Pts',(81.3359062018732,-3.41704355013873,
77.4607601686717));
#182097=CARTESIAN_POINT('Ctrl Pts',(81.3930224251975,-3.33264237448964,
77.4529327861897));
#182098=CARTESIAN_POINT('Ctrl Pts',(81.4260131437731,-3.28229100154471,
77.4484673199118));
#182099=CARTESIAN_POINT('Ctrl Pts',(81.5725537188299,-3.05119213104776,
77.4288659407011));
#182100=CARTESIAN_POINT('Ctrl Pts',(81.677320234815,-2.86490582309567,77.4155082355322));
#182101=CARTESIAN_POINT('Ctrl Pts',(81.9134163786765,-2.38767722651736,
77.3866762038847));
#182102=CARTESIAN_POINT('Ctrl Pts',(82.0320958321311,-2.09106969004154,
77.3734149465394));
#182103=CARTESIAN_POINT('Ctrl Pts',(82.1547121581883,-1.69705771604075,
77.3611545792717));
#182104=CARTESIAN_POINT('Ctrl Pts',(82.1804442516329,-1.60708685192427,
77.3587043525596));
#182105=CARTESIAN_POINT('Ctrl Pts',(82.2224391880432,-1.44627382091367,
77.3549381448688));
#182106=CARTESIAN_POINT('Ctrl Pts',(82.2395289392392,-1.37567029102757,
77.3534914232994));
#182107=CARTESIAN_POINT('Ctrl Pts',(82.2736990591403,-1.22253129794907,
77.3507994870256));
#182108=CARTESIAN_POINT('Ctrl Pts',(82.2903364210679,-1.13991171112005,
77.3496238249134));
#182109=CARTESIAN_POINT('Ctrl Pts',(82.3361142348001,-0.885313129490639,
77.3468556273716));
#182110=CARTESIAN_POINT('Ctrl Pts',(82.3595718363196,-0.712397746788869,
77.3461610483572));
#182111=CARTESIAN_POINT('Ctrl Pts',(82.402715406588,-0.243874795976445,
77.3476055428851));
#182112=CARTESIAN_POINT('Ctrl Pts',(82.408293118046,0.0525237387862707,
77.3520427942016));
#182113=CARTESIAN_POINT('Ctrl Pts',(82.3838007757034,0.506370742700034,
77.3650091906455));
#182114=CARTESIAN_POINT('Ctrl Pts',(82.3690904705875,0.66425556221823,77.3706817941234));
#182115=CARTESIAN_POINT('Ctrl Pts',(82.3419435601632,0.86904777868197,77.3796994117668));
#182116=CARTESIAN_POINT('Ctrl Pts',(82.335056535245,0.91667522339289,77.3819147345167));
#182117=CARTESIAN_POINT('Ctrl Pts',(82.3216087622276,1.00250647421022,77.3861266843378));
#182118=CARTESIAN_POINT('Ctrl Pts',(82.3152452153003,1.04074023492962,77.3880822416725));
#182119=CARTESIAN_POINT('Ctrl Pts',(82.3002681380371,1.12572747446224,77.3926081813163));
#182120=CARTESIAN_POINT('Ctrl Pts',(82.2914721862968,1.17244325089226,77.3952164770578));
#182121=CARTESIAN_POINT('Ctrl Pts',(82.2603860777859,1.32755435044431,77.4042695384468));
#182122=CARTESIAN_POINT('Ctrl Pts',(82.2356979403902,1.4354175678313,77.4112059067286));
#182123=CARTESIAN_POINT('Ctrl Pts',(82.1607155729078,1.72629187302632,77.4315751118181));
#182124=CARTESIAN_POINT('Ctrl Pts',(82.1047858091582,1.9076439630321,77.4460891739514));
#182125=CARTESIAN_POINT('Ctrl Pts',(81.9400767786863,2.36427339477832,77.487011271427));
#182126=CARTESIAN_POINT('Ctrl Pts',(81.8194709552043,2.63455885330743,77.51545158445));
#182127=CARTESIAN_POINT('Ctrl Pts',(81.6320905608724,2.98289882791018,77.5575958409496));
#182128=CARTESIAN_POINT('Ctrl Pts',(81.5823899803663,3.06997711289707,77.5686253574343));
#182129=CARTESIAN_POINT('Ctrl Pts',(81.4928895464382,3.21801555221704,77.5882400410595));
#182130=CARTESIAN_POINT('Ctrl Pts',(81.4541110955956,3.27958791484473,77.596666319509));
#182131=CARTESIAN_POINT('Ctrl Pts',(81.3699763322677,3.40791459938609,77.6148025710048));
#182132=CARTESIAN_POINT('Ctrl Pts',(81.3243735934911,3.47448429263782,77.624550124217));
#182133=CARTESIAN_POINT('Ctrl Pts',(81.1874713180948,3.66587946582856,77.6535890136189));
#182134=CARTESIAN_POINT('Ctrl Pts',(81.0926848879001,3.78804420079668,77.6734188213446));
#182135=CARTESIAN_POINT('Ctrl Pts',(80.8487045941295,4.07839506728686,77.7239267062195));
#182136=CARTESIAN_POINT('Ctrl Pts',(80.694582061473,4.24198142973002,77.7553891078798));
#182137=CARTESIAN_POINT('Ctrl Pts',(80.3991994696675,4.52183268944643,77.8153456803641));
#182138=CARTESIAN_POINT('Ctrl Pts',(80.2610490253404,4.64108636151601,77.843271634565));
#182139=CARTESIAN_POINT('Ctrl Pts',(80.0684362233177,4.79238834770303,77.8822816653051));
#182140=CARTESIAN_POINT('Ctrl Pts',(80.0185312143735,4.83031934508719,77.8923956293884));
#182141=CARTESIAN_POINT('Ctrl Pts',(79.9351129166709,4.89164994381174,77.9093250132792));
#182142=CARTESIAN_POINT('Ctrl Pts',(79.9019340398087,4.91551591261988,77.9160648202313));
#182143=CARTESIAN_POINT('Ctrl Pts',(79.8362690312939,4.96172044490222,77.9294181415151));
#182144=CARTESIAN_POINT('Ctrl Pts',(79.8038015726767,4.98408157776601,77.9360267919065));
#182145=CARTESIAN_POINT('Ctrl Pts',(79.7027226245189,5.0522090204933,77.9566151012401));
#182146=CARTESIAN_POINT('Ctrl Pts',(79.6334017069684,5.09683847834765,77.9707543688887));
#182147=CARTESIAN_POINT('Ctrl Pts',(79.5631824082903,5.1399798140475,77.9850820082609));
#182148=CARTESIAN_POINT('',(81.9970266959657,2.23885090499482,77.5559295935053));
#182149=CARTESIAN_POINT('Origin',(76.5149506510185,7.15881389286582E-15,
78.5225675105249));
#182150=CARTESIAN_POINT('Ctrl Pts',(81.9970266959657,2.23885090499483,77.5559295935053));
#182151=CARTESIAN_POINT('Ctrl Pts',(82.1120050374136,1.94599933596432,77.5297243427407));
#182152=CARTESIAN_POINT('Ctrl Pts',(82.2040639554934,1.64432695163046,77.5077093270866));
#182153=CARTESIAN_POINT('Ctrl Pts',(82.2828902621182,1.28846521688186,77.4864579936355));
#182154=CARTESIAN_POINT('Ctrl Pts',(82.2929691014602,1.24017294726578,77.4836714598941));
#182155=CARTESIAN_POINT('Ctrl Pts',(82.3109829666165,1.14824548678766,77.4785448540955));
#182156=CARTESIAN_POINT('Ctrl Pts',(82.3190311682852,1.10463675326511,77.476188302615));
#182157=CARTESIAN_POINT('Ctrl Pts',(82.3333026734869,1.02223313768075,77.4718722996966));
#182158=CARTESIAN_POINT('Ctrl Pts',(82.3396289029045,0.983459828563357,
77.4698979720648));
#182159=CARTESIAN_POINT('Ctrl Pts',(82.3552794816357,0.881281097813429,
77.4648469028044));
#182160=CARTESIAN_POINT('Ctrl Pts',(82.3639753086168,0.81777966209688,77.4618613282563));
#182161=CARTESIAN_POINT('Ctrl Pts',(82.4037315616389,0.488678616768583,
77.4472143836427));
#182162=CARTESIAN_POINT('Ctrl Pts',(82.4182052778017,0.221261346282158,
77.4380997327589));
#182163=CARTESIAN_POINT('Ctrl Pts',(82.4126053820003,-0.254384290371704,
77.4274857011276));
#182164=CARTESIAN_POINT('Ctrl Pts',(82.3995023391387,-0.462231518467035,
77.4247481407553));
#182165=CARTESIAN_POINT('Ctrl Pts',(82.3592317702824,-0.813793276268081,
77.4235226438736));
#182166=CARTESIAN_POINT('Ctrl Pts',(82.3374726948974,-0.957933874065452,
77.4240054560567));
#182167=CARTESIAN_POINT('Ctrl Pts',(82.2957859411768,-1.17996338745491,
77.4263009428648));
#182168=CARTESIAN_POINT('Ctrl Pts',(82.2794390815815,-1.25847397791779,
77.4274173744936));
#182169=CARTESIAN_POINT('Ctrl Pts',(82.2451426538702,-1.40834202947021,
77.4301338396418));
#182170=CARTESIAN_POINT('Ctrl Pts',(82.2274398314377,-1.47974197471554,
77.4316860734008));
#182171=CARTESIAN_POINT('Ctrl Pts',(82.1859290517851,-1.63508876171119,
77.4356259025677));
#182172=CARTESIAN_POINT('Ctrl Pts',(82.16160312302,-1.71887716814351,77.4381148156318));
#182173=CARTESIAN_POINT('Ctrl Pts',(82.0314402667802,-2.13374512299529,
77.4522364787784));
#182174=CARTESIAN_POINT('Ctrl Pts',(81.8992835045091,-2.45568309340538,
77.4690056300341));
#182175=CARTESIAN_POINT('Ctrl Pts',(81.6540035372506,-2.93205429856277,
77.5019645828343));
#182176=CARTESIAN_POINT('Ctrl Pts',(81.5598497780608,-3.09561905023603,
77.514897877802));
#182177=CARTESIAN_POINT('Ctrl Pts',(81.4279559246922,-3.30170314609991,
77.5331169759468));
#182178=CARTESIAN_POINT('Ctrl Pts',(81.3970410614265,-3.34854956798892,
77.5373935803693));
#182179=CARTESIAN_POINT('Ctrl Pts',(81.3420287649319,-3.42942212812094,
77.5450050301176));
#182180=CARTESIAN_POINT('Ctrl Pts',(81.3182238189387,-3.46364501950419,
77.5482985021127));
#182181=CARTESIAN_POINT('Ctrl Pts',(81.259670078947,-3.5459803155784,77.5563995283866));
#182182=CARTESIAN_POINT('Ctrl Pts',(81.2245630794915,-3.59382662288795,
77.5612575885879));
#182183=CARTESIAN_POINT('Ctrl Pts',(81.0081907320452,-3.87972658424919,
77.5912365319937));
#182184=CARTESIAN_POINT('Ctrl Pts',(80.8101623365004,-4.10430694848959,
77.6188510676246));
#182185=CARTESIAN_POINT('Ctrl Pts',(80.4195031361362,-4.48573602355154,
77.6745915981231));
#182186=CARTESIAN_POINT('Ctrl Pts',(80.2321879254854,-4.64722355638303,
77.7017544178822));
#182187=CARTESIAN_POINT('Ctrl Pts',(79.9648059334976,-4.85026875973001,
77.7412735775394));
#182188=CARTESIAN_POINT('Ctrl Pts',(79.8928521612124,-4.90241442964863,
77.7519745563073));
#182189=CARTESIAN_POINT('Ctrl Pts',(79.7606804873029,-4.99376143995268,
77.7717508694137));
#182190=CARTESIAN_POINT('Ctrl Pts',(79.7008594761873,-5.03352412250738,
77.7807442290716));
#182191=CARTESIAN_POINT('Ctrl Pts',(79.5661937244769,-5.11955905971487,
77.8010814218768));
#182192=CARTESIAN_POINT('Ctrl Pts',(79.4910194599769,-5.16526692889563,
77.8124955658833));
#182193=CARTESIAN_POINT('Ctrl Pts',(79.2441170644402,-5.30796930960743,
77.8501674622348));
#182194=CARTESIAN_POINT('Ctrl Pts',(79.0686545369416,-5.3980175855351,77.8772243415634));
#182195=CARTESIAN_POINT('Ctrl Pts',(78.8710996987854,-5.48722382101834,
77.9078893790354));
#182196=CARTESIAN_POINT('Ctrl Pts',(78.8530349866649,-5.49527192125009,
77.910695184472));
#182197=CARTESIAN_POINT('Ctrl Pts',(78.5893178613139,-5.61117664038048,
77.9516791282966));
#182198=CARTESIAN_POINT('Ctrl Pts',(78.3368168404352,-5.7021663598798,77.9912323511788));
#182199=CARTESIAN_POINT('Ctrl Pts',(77.9530337472602,-5.81147711804384,
78.0511492520113));
#182200=CARTESIAN_POINT('Ctrl Pts',(77.8258375173985,-5.84314371042114,
78.0709726385734));
#182201=CARTESIAN_POINT('Ctrl Pts',(77.6490436772768,-5.88091734003757,
78.0983870894309));
#182202=CARTESIAN_POINT('Ctrl Pts',(77.6002634438982,-5.89069249364619,
78.1059367113938));
#182203=CARTESIAN_POINT('Ctrl Pts',(77.5349624918954,-5.90291613519415,
78.1160187700405));
#182204=CARTESIAN_POINT('Ctrl Pts',(77.5185474885862,-5.90591638755581,
78.1185510884974));
#182205=CARTESIAN_POINT('Ctrl Pts',(77.502120004475,-5.90884651843273,78.1210831294071));
#182206=CARTESIAN_POINT('Origin',(76.5901425176087,7.15881389286582E-15,
78.9490017765011));
#182207=CARTESIAN_POINT('',(77.348259898075,-5.90884651802685,77.24849909196));
#182208=CARTESIAN_POINT('',(77.3632014635974,-5.90884651820819,77.333236926787));
#182209=CARTESIAN_POINT('',(77.6162029475856,-5.90884651807327,78.7680796388589));
#182210=CARTESIAN_POINT('Ctrl Pts',(77.3482598983342,-5.90884651798042,
77.2484990919142));
#182211=CARTESIAN_POINT('Ctrl Pts',(77.3790711546296,-5.9033507881994,77.2437500164688));
#182212=CARTESIAN_POINT('Ctrl Pts',(77.4098401728518,-5.89760861672904,
77.2390170943833));
#182213=CARTESIAN_POINT('Ctrl Pts',(77.501562216025,-5.8797319940699,77.2249346127144));
#182214=CARTESIAN_POINT('Ctrl Pts',(77.562377308269,-5.86687515734464,77.2156321567381));
#182215=CARTESIAN_POINT('Ctrl Pts',(77.9405526013235,-5.78064123208494,
77.1579631435909));
#182216=CARTESIAN_POINT('Ctrl Pts',(78.2518151643068,-5.6819190906891,77.1112503853703));
#182217=CARTESIAN_POINT('Ctrl Pts',(78.7418618598244,-5.48044949971028,
77.0378262550683));
#182218=CARTESIAN_POINT('Ctrl Pts',(78.9261672244682,-5.39327789775599,
77.0102487576707));
#182219=CARTESIAN_POINT('Ctrl Pts',(79.2053686633304,-5.2430917088901,76.9684103040856));
#182220=CARTESIAN_POINT('Ctrl Pts',(79.3035235189632,-5.18660181413933,
76.9536905486092));
#182221=CARTESIAN_POINT('Ctrl Pts',(79.4635324694679,-5.08829686726246,
76.9296712579722));
#182222=CARTESIAN_POINT('Ctrl Pts',(79.5263106521541,-5.0480759154954,76.9202413710357));
#182223=CARTESIAN_POINT('Ctrl Pts',(79.6520127638248,-4.96415347527391,
76.9013491550527));
#182224=CARTESIAN_POINT('Ctrl Pts',(79.7148830134044,-4.92039526150578,
76.8918945994209));
#182225=CARTESIAN_POINT('Ctrl Pts',(79.879772149375,-4.80082632931245,76.8670902431858));
#182226=CARTESIAN_POINT('Ctrl Pts',(79.9802552595864,-4.72292066317286,
76.8519655210317));
#182227=CARTESIAN_POINT('Ctrl Pts',(80.3221192294778,-4.43986699813035,
76.8005508123697));
#182228=CARTESIAN_POINT('Ctrl Pts',(80.5497370329911,-4.21858474499515,
76.7663686369115));
#182229=CARTESIAN_POINT('Ctrl Pts',(80.8628864069086,-3.86167787207753,
76.7203560288381));
#182230=CARTESIAN_POINT('Ctrl Pts',(80.962123058527,-3.73917687711185,76.7059627377435));
#182231=CARTESIAN_POINT('Ctrl Pts',(81.0889456663203,-3.56943530517014,
76.6879779509928));
#182232=CARTESIAN_POINT('Ctrl Pts',(81.1208104650228,-3.52556740371241,
76.6834972089735));
#182233=CARTESIAN_POINT('Ctrl Pts',(81.1762065078811,-3.4471071564848,76.67578463301));
#182234=CARTESIAN_POINT('Ctrl Pts',(81.1999741205713,-3.41269244219758,
76.6725025375769));
#182235=CARTESIAN_POINT('Ctrl Pts',(81.2522757136796,-3.33525784369304,
76.6653401115408));
#182236=CARTESIAN_POINT('Ctrl Pts',(81.2806215533048,-3.29211181479248,
76.6614991886975));
#182237=CARTESIAN_POINT('Ctrl Pts',(81.4240819304952,-3.06754095051699,
76.6422570588391));
#182238=CARTESIAN_POINT('Ctrl Pts',(81.5301074658421,-2.88033546349416,
76.6287048894998));
#182239=CARTESIAN_POINT('Ctrl Pts',(81.7249388642508,-2.4891327612249,76.6048534090641));
#182240=CARTESIAN_POINT('Ctrl Pts',(81.8129408029566,-2.28508773182132,
76.5946877522053));
#182241=CARTESIAN_POINT('Ctrl Pts',(81.940405056024,-1.93830330023256,76.5808603903746));
#182242=CARTESIAN_POINT('Ctrl Pts',(81.9861923877244,-1.79816460303819,
76.5761677964281));
#182243=CARTESIAN_POINT('Ctrl Pts',(82.0489133782399,-1.57950915023936,
76.5701836645833));
#182244=CARTESIAN_POINT('Ctrl Pts',(82.0694669501074,-1.50210727408618,
76.5683186584049));
#182245=CARTESIAN_POINT('Ctrl Pts',(82.1059623572793,-1.3528193124491,76.5652046839765));
#182246=CARTESIAN_POINT('Ctrl Pts',(82.1221396477114,-1.28100642980992,
76.5639183685895));
#182247=CARTESIAN_POINT('Ctrl Pts',(82.1546220855387,-1.1235063695837,76.5615601922676));
#182248=CARTESIAN_POINT('Ctrl Pts',(82.1703950677187,-1.03772539479227,
76.560572045764));
#182249=CARTESIAN_POINT('Ctrl Pts',(82.2423549207679,-0.592700687420132,
76.5569926245351));
#182250=CARTESIAN_POINT('Ctrl Pts',(82.2680465566833,-0.229268870135951,
76.5591978923104));
#182251=CARTESIAN_POINT('Ctrl Pts',(82.2583380429672,0.286661204992796,
76.570595657831));
#182252=CARTESIAN_POINT('Ctrl Pts',(82.2497471197123,0.438962422474809,
76.5749939124982));
#182253=CARTESIAN_POINT('Ctrl Pts',(82.2263542662663,0.687645543165331,
76.5840166942483));
#182254=CARTESIAN_POINT('Ctrl Pts',(82.21492486286,0.784297601861131,76.5879833909021));
#182255=CARTESIAN_POINT('Ctrl Pts',(82.194768278483,0.925711463427947,76.5945026284016));
#182256=CARTESIAN_POINT('Ctrl Pts',(82.1878370007862,0.97073003571516,76.5966852322672));
#182257=CARTESIAN_POINT('Ctrl Pts',(82.1740671847905,1.05396961486788,76.6009251065495));
#182258=CARTESIAN_POINT('Ctrl Pts',(82.1673661448697,1.09221162697219,76.6029537339398));
#182259=CARTESIAN_POINT('Ctrl Pts',(82.1491895578466,1.19042655666336,76.6083690200036));
#182260=CARTESIAN_POINT('Ctrl Pts',(82.1371792745618,1.25029001896446,76.6118671338245));
#182261=CARTESIAN_POINT('Ctrl Pts',(82.064585414926,1.58590373360737,76.6325603162671));
#182262=CARTESIAN_POINT('Ctrl Pts',(81.9858403894899,1.85714328109069,76.6533951204252));
#182263=CARTESIAN_POINT('Ctrl Pts',(81.7910062878038,2.38682890637765,76.7015560127701));
#182264=CARTESIAN_POINT('Ctrl Pts',(81.6750623746765,2.64458181563327,76.7288350528002));
#182265=CARTESIAN_POINT('Ctrl Pts',(81.4939444286058,2.9815273686733,76.7695777129513));
#182266=CARTESIAN_POINT('Ctrl Pts',(81.444134851852,3.06884551453978,76.7806327997634));
#182267=CARTESIAN_POINT('Ctrl Pts',(81.3545084364918,3.21715114439041,76.8002767458305));
#182268=CARTESIAN_POINT('Ctrl Pts',(81.3157233773698,3.27875691452185,76.8087051014778));
#182269=CARTESIAN_POINT('Ctrl Pts',(81.2316536267014,3.40702916211221,76.826828574464));
#182270=CARTESIAN_POINT('Ctrl Pts',(81.1861272193596,3.4735142940962,76.8365605450676));
#182271=CARTESIAN_POINT('Ctrl Pts',(81.0498137022408,3.66417376553156,76.8654768613902));
#182272=CARTESIAN_POINT('Ctrl Pts',(80.9555866343288,3.78572443843611,76.8851924187907));
#182273=CARTESIAN_POINT('Ctrl Pts',(80.7003998580471,4.0898034979418,76.9380288313144));
#182274=CARTESIAN_POINT('Ctrl Pts',(80.5328346307177,4.26622038163841,76.9722003664408));
#182275=CARTESIAN_POINT('Ctrl Pts',(80.2298897979858,4.5482561867141,77.0336466448138));
#182276=CARTESIAN_POINT('Ctrl Pts',(80.0997635343139,4.65926376273859,77.0599520613209));
#182277=CARTESIAN_POINT('Ctrl Pts',(79.9179005993073,4.80125665779067,77.0967897013079));
#182278=CARTESIAN_POINT('Ctrl Pts',(79.8701275289562,4.83739855541433,77.1064731815232));
#182279=CARTESIAN_POINT('Ctrl Pts',(79.7885004244674,4.89721923095609,77.1230412699453));
#182280=CARTESIAN_POINT('Ctrl Pts',(79.7549253471949,4.92128628346686,77.1298628035971));
#182281=CARTESIAN_POINT('Ctrl Pts',(79.6763953948476,4.97633645073748,77.1458349046398));
#182282=CARTESIAN_POINT('Ctrl Pts',(79.6312636859136,5.00704651151342,77.1550258115393));
#182283=CARTESIAN_POINT('Ctrl Pts',(79.4443191832341,5.13047922390375,77.1931258300298));
#182284=CARTESIAN_POINT('Ctrl Pts',(79.2990614268771,5.21760201718711,77.2227964476991));
#182285=CARTESIAN_POINT('Ctrl Pts',(78.8117241196203,5.48183729584794,77.3221809444067));
#182286=CARTESIAN_POINT('Ctrl Pts',(78.4562563747846,5.63121342866614,77.3943578700479));
#182287=CARTESIAN_POINT('Ctrl Pts',(78.0064008746293,5.76960453436242,77.4844734985378));
#182288=CARTESIAN_POINT('Ctrl Pts',(77.9233625740266,5.79313209926972,77.501062917018));
#182289=CARTESIAN_POINT('Ctrl Pts',(77.777894583183,5.83085649495309,77.5300452579002));
#182290=CARTESIAN_POINT('Ctrl Pts',(77.7156930208904,5.84589101948722,77.5424131537475));
#182291=CARTESIAN_POINT('Ctrl Pts',(77.5702205906742,5.87850881592332,77.5712819966631));
#182292=CARTESIAN_POINT('Ctrl Pts',(77.4867883261293,5.89529187836198,77.5877963769558));
#182293=CARTESIAN_POINT('Ctrl Pts',(77.2150462302528,5.94374270511737,77.6414583094041));
#182294=CARTESIAN_POINT('Ctrl Pts',(77.0255479271987,5.96792495921637,77.678680261191));
#182295=CARTESIAN_POINT('Ctrl Pts',(76.445302374834,6.01293012420287,77.7923154695296));
#182296=CARTESIAN_POINT('Ctrl Pts',(76.053333974953,6.00353165605279,77.8685610020757));
#182297=CARTESIAN_POINT('Ctrl Pts',(75.5997939959963,5.9463772184808,77.9578966183986));
#182298=CARTESIAN_POINT('Ctrl Pts',(75.5343822295999,5.93699207884127,77.970810439319));
#182299=CARTESIAN_POINT('Ctrl Pts',(75.4339566251156,5.92082094221347,77.9906963290684));
#182300=CARTESIAN_POINT('Ctrl Pts',(75.3988199902583,5.91482902391477,77.9976652378463));
#182301=CARTESIAN_POINT('Ctrl Pts',(75.3232260793335,5.90121690882146,78.0126859086396));
#182302=CARTESIAN_POINT('Ctrl Pts',(75.2827902663125,5.89348866586959,78.0207376197063));
#182303=CARTESIAN_POINT('Ctrl Pts',(75.1689451325475,5.87046671645901,78.0434493967771));
#182304=CARTESIAN_POINT('Ctrl Pts',(75.0957444824899,5.85417517188175,78.05810281632));
#182305=CARTESIAN_POINT('Ctrl Pts',(74.9226081481883,5.81209155188762,78.0928541545413));
#182306=CARTESIAN_POINT('Ctrl Pts',(74.8229986862839,5.78503765703722,78.1129214145716));
#182307=CARTESIAN_POINT('Ctrl Pts',(74.5293644421938,5.69679239969982,78.1722195273797));
#182308=CARTESIAN_POINT('Ctrl Pts',(74.3377158148959,5.62800899289595,78.2111055782549));
#182309=CARTESIAN_POINT('Ctrl Pts',(73.9261607085401,5.45539875536574,78.2946849963179));
#182310=CARTESIAN_POINT('Ctrl Pts',(73.7082718840324,5.34754434783662,78.3389780652637));
#182311=CARTESIAN_POINT('Ctrl Pts',(73.4191050630308,5.1812115851068,78.3976619386656));
#182312=CARTESIAN_POINT('Ctrl Pts',(73.341734327806,5.13428885305903,78.4133549735778));
#182313=CARTESIAN_POINT('Ctrl Pts',(73.2051865571293,5.04709178188457,78.4410347683695));
#182314=CARTESIAN_POINT('Ctrl Pts',(73.1456133762532,5.00749883950254,78.4531053170519));
#182315=CARTESIAN_POINT('Ctrl Pts',(73.0174347482399,4.91889378656908,78.4790670253055));
#182316=CARTESIAN_POINT('Ctrl Pts',(72.9491218632164,4.86946900215564,78.4928971678718));
#182317=CARTESIAN_POINT('Ctrl Pts',(72.7314466994745,4.70474331056752,78.536960058539));
#182318=CARTESIAN_POINT('Ctrl Pts',(72.5864399036769,4.58365033245454,78.5662997403279));
#182319=CARTESIAN_POINT('Ctrl Pts',(72.2746137359892,4.29680075109632,78.6295654834212));
#182320=CARTESIAN_POINT('Ctrl Pts',(72.1112863269271,4.12758368576147,78.662824149951));
#182321=CARTESIAN_POINT('Ctrl Pts',(71.870254344542,3.84617123736604,78.7125617755189));
#182322=CARTESIAN_POINT('Ctrl Pts',(71.7857151199448,3.7403609422746,78.73015609352));
#182323=CARTESIAN_POINT('Ctrl Pts',(71.6739037977066,3.59016605858873,78.7537385413431));
#182324=CARTESIAN_POINT('Ctrl Pts',(71.6435215104869,3.54822145999234,78.7601811517279));
#182325=CARTESIAN_POINT('Ctrl Pts',(71.589675654306,3.47180237440665,78.7716704755811));
#182326=CARTESIAN_POINT('Ctrl Pts',(71.566021381508,3.43747108256943,78.776744092307));
#182327=CARTESIAN_POINT('Ctrl Pts',(71.5127759890861,3.35842654316031,78.7882281483384));
#182328=CARTESIAN_POINT('Ctrl Pts',(71.4834223271711,3.31355398678824,78.794604725575));
#182329=CARTESIAN_POINT('Ctrl Pts',(71.3731186550481,3.13986488387529,78.8187289731598));
#182330=CARTESIAN_POINT('Ctrl Pts',(71.2964613761757,3.00830213076517,78.8358416008123));
#182331=CARTESIAN_POINT('Ctrl Pts',(71.0699360511242,2.5830752296688,78.8873185155843));
#182332=CARTESIAN_POINT('Ctrl Pts',(70.9390316471772,2.27961473842733,78.9184716013972));
#182333=CARTESIAN_POINT('Ctrl Pts',(70.793741379226,1.84909333335007,78.9546378643439));
#182334=CARTESIAN_POINT('Ctrl Pts',(70.7576786172596,1.73032602313077,78.9638216683378));
#182335=CARTESIAN_POINT('Ctrl Pts',(70.7053089628792,1.53670177999723,78.9775127723781));
#182336=CARTESIAN_POINT('Ctrl Pts',(70.6867404453154,1.46252648723218,78.9824599568782));
#182337=CARTESIAN_POINT('Ctrl Pts',(70.6526329864705,1.31448581690629,78.9917455664844));
#182338=CARTESIAN_POINT('Ctrl Pts',(70.6370597010095,1.24064310023762,78.9960904558766));
#182339=CARTESIAN_POINT('Ctrl Pts',(70.6008859877896,1.05180481822983,79.0064782899364));
#182340=CARTESIAN_POINT('Ctrl Pts',(70.5822089173517,0.936453033749791,
79.0121459354762));
#182341=CARTESIAN_POINT('Ctrl Pts',(70.547647527451,0.675688201192122,79.0234691328582));
#182342=CARTESIAN_POINT('Ctrl Pts',(70.53365214637,0.530084714729527,79.0287602942883));
#182343=CARTESIAN_POINT('Ctrl Pts',(70.511168771355,0.1548468983974,79.0398650660739));
#182344=CARTESIAN_POINT('Ctrl Pts',(70.5103891421052,-0.0750483832367587,
79.0442424183622));
#182345=CARTESIAN_POINT('Ctrl Pts',(70.5316925031723,-0.474866480038174,
79.0480731938147));
#182346=CARTESIAN_POINT('Ctrl Pts',(70.5479368463135,-0.644820250329008,
79.0485043567766));
#182347=CARTESIAN_POINT('Ctrl Pts',(70.5787862245697,-0.867792083769855,
79.0476629821568));
#182348=CARTESIAN_POINT('Ctrl Pts',(70.5869736099093,-0.921619971103457,
79.0473508686733));
#182349=CARTESIAN_POINT('Ctrl Pts',(70.6021924541813,-1.01334267755272,
79.0466406735422));
#182350=CARTESIAN_POINT('Ctrl Pts',(70.6088619904773,-1.05129344331039,
79.0462947299494));
#182351=CARTESIAN_POINT('Ctrl Pts',(70.6249718461223,-1.13809376561228,
79.0453851293205));
#182352=CARTESIAN_POINT('Ctrl Pts',(70.6346524000807,-1.18689417817707,
79.0447866916639));
#182353=CARTESIAN_POINT('Ctrl Pts',(70.6712937973917,-1.3603896976341,79.0423369674326));
#182354=CARTESIAN_POINT('Ctrl Pts',(70.7015870666288,-1.48433981778062,
79.0399903856353));
#182355=CARTESIAN_POINT('Ctrl Pts',(70.8026000397794,-1.84762710450015,
79.0311950830383));
#182356=CARTESIAN_POINT('Ctrl Pts',(70.8841796742249,-2.08362081173422,
79.0229686366062));
#182357=CARTESIAN_POINT('Ctrl Pts',(71.0707862949551,-2.53207699382992,
79.0018369181684));
#182358=CARTESIAN_POINT('Ctrl Pts',(71.1742102788551,-2.74473498325315,
78.9892155731601));
#182359=CARTESIAN_POINT('Ctrl Pts',(71.3347443186164,-3.03105382907638,
78.968378600483));
#182360=CARTESIAN_POINT('Ctrl Pts',(71.3816118572124,-3.11035158702119,
78.9621745532778));
#182361=CARTESIAN_POINT('Ctrl Pts',(71.4684473269855,-3.2499071597528,78.9504723569842));
#182362=CARTESIAN_POINT('Ctrl Pts',(71.5077265158003,-3.31058312849762,
78.9451100350719));
#182363=CARTESIAN_POINT('Ctrl Pts',(71.5960936674664,-3.44186749178316,
78.932902427639));
#182364=CARTESIAN_POINT('Ctrl Pts',(71.6456162909299,-3.51215564211777,
78.9259704064296));
#182365=CARTESIAN_POINT('Ctrl Pts',(71.8146426493901,-3.74149126023436,
78.9020342531127));
#182366=CARTESIAN_POINT('Ctrl Pts',(71.9404454150299,-3.89559576849619,
78.8837807151736));
#182367=CARTESIAN_POINT('Ctrl Pts',(72.2297353203445,-4.21610106855887,
78.8411401613391));
#182368=CARTESIAN_POINT('Ctrl Pts',(72.3957240070386,-4.37973303814544,
78.816274006793));
#182369=CARTESIAN_POINT('Ctrl Pts',(72.6725242425283,-4.62236988992999,
78.7746531372064));
#182370=CARTESIAN_POINT('Ctrl Pts',(72.7772884530262,-4.70806953415733,
78.7588711913758));
#182371=CARTESIAN_POINT('Ctrl Pts',(72.9274027854656,-4.8225353462917,78.7363153631312));
#182372=CARTESIAN_POINT('Ctrl Pts',(72.9703847679667,-4.85440024466689,
78.7298634022445));
#182373=CARTESIAN_POINT('Ctrl Pts',(73.0475398544281,-4.9099972657163,78.7183013521376));
#182374=CARTESIAN_POINT('Ctrl Pts',(73.0815439835835,-4.93396034159707,
78.7132128792356));
#182375=CARTESIAN_POINT('Ctrl Pts',(73.1659269131394,-4.99210585650185,
78.7006021159989));
#182376=CARTESIAN_POINT('Ctrl Pts',(73.2165817224597,-5.02587092036607,
78.693045298111));
#182377=CARTESIAN_POINT('Ctrl Pts',(73.3311489404276,-5.09971428759275,
78.6759705361697));
#182378=CARTESIAN_POINT('Ctrl Pts',(73.3953215155522,-5.1393619065739,78.6664177369671));
#182379=CARTESIAN_POINT('Ctrl Pts',(73.6129231495262,-5.26812685262055,
78.6340284769649));
#182380=CARTESIAN_POINT('Ctrl Pts',(73.7695454363004,-5.35154195486914,
78.6107184103544));
#182381=CARTESIAN_POINT('Ctrl Pts',(74.1717066871822,-5.54305552232619,
78.5505973776636));
#182382=CARTESIAN_POINT('Ctrl Pts',(74.4212115348581,-5.64166994582414,
78.5130477600194));
#182383=CARTESIAN_POINT('Ctrl Pts',(74.7586908077126,-5.749142779127,78.4616710070052));
#182384=CARTESIAN_POINT('Ctrl Pts',(74.8415569552713,-5.77353818135924,
78.4490123123479));
#182385=CARTESIAN_POINT('Ctrl Pts',(74.9951687471143,-5.81511054217018,
78.4254640122467));
#182386=CARTESIAN_POINT('Ctrl Pts',(75.0657594516289,-5.83281585205253,
78.4146110837366));
#182387=CARTESIAN_POINT('Ctrl Pts',(75.2139053425179,-5.86706368554338,
78.3917698370917));
#182388=CARTESIAN_POINT('Ctrl Pts',(75.2915015900023,-5.88335551660229,
78.3797693840146));
#182389=CARTESIAN_POINT('Ctrl Pts',(75.5108846805038,-5.92479857874658,
78.3457453120744));
#182390=CARTESIAN_POINT('Ctrl Pts',(75.6532739912601,-5.94630716369097,
78.3235490851347));
#182391=CARTESIAN_POINT('Ctrl Pts',(76.0004674690265,-5.98574690419399,
78.2692264031445));
#182392=CARTESIAN_POINT('Ctrl Pts',(76.2056770401233,-5.99818481926721,
78.2369480187758));
#182393=CARTESIAN_POINT('Ctrl Pts',(76.6757119567096,-6.00191587115732,
78.1629755805831));
#182394=CARTESIAN_POINT('Ctrl Pts',(76.9401480940848,-5.98608198242611,
78.1213282851397));
#182395=CARTESIAN_POINT('Ctrl Pts',(77.2656229967027,-5.94435941151455,
78.0706370856789));
#182396=CARTESIAN_POINT('Ctrl Pts',(77.3283927806842,-5.93527647940671,
78.0608882287249));
#182397=CARTESIAN_POINT('Ctrl Pts',(77.4231095424685,-5.92000016877387,
78.046230927269));
#182398=CARTESIAN_POINT('Ctrl Pts',(77.4551659898521,-5.9145565019064,78.041279515172));
#182399=CARTESIAN_POINT('Ctrl Pts',(77.4871784403164,-5.90884651800743,
78.0363452943473));
#182400=CARTESIAN_POINT('Ctrl Pts',(77.502120004475,-5.90884651843273,78.1210831294071));
#182401=CARTESIAN_POINT('Ctrl Pts',(77.4810781240556,-5.91259970809392,
78.1243264076644));
#182402=CARTESIAN_POINT('Ctrl Pts',(77.4600157665999,-5.91623785047641,
78.1275692307462));
#182403=CARTESIAN_POINT('Ctrl Pts',(77.38652458514,-5.92851876326947,78.138872518064));
#182404=CARTESIAN_POINT('Ctrl Pts',(77.3339985198352,-5.9365641204623,78.1469306821317));
#182405=CARTESIAN_POINT('Ctrl Pts',(77.1211780008003,-5.96620813885608,
78.1795132683561));
#182406=CARTESIAN_POINT('Ctrl Pts',(76.9601266461478,-5.981887537296,78.2040189643669));
#182407=CARTESIAN_POINT('Ctrl Pts',(76.5105549554249,-6.00696129925713,
78.2722875244955));
#182408=CARTESIAN_POINT('Ctrl Pts',(76.2216665999468,-6.0017606095316,78.3160155976274));
#182409=CARTESIAN_POINT('Ctrl Pts',(75.7637031404583,-5.95963661516321,
78.3856978496139));
#182410=CARTESIAN_POINT('Ctrl Pts',(75.5938297520057,-5.93647412939509,
78.4116204353954));
#182411=CARTESIAN_POINT('Ctrl Pts',(75.3433402575683,-5.8910709563988,78.4499957144422));
#182412=CARTESIAN_POINT('Ctrl Pts',(75.2618009254828,-5.87449363876011,
78.4625111231067));
#182413=CARTESIAN_POINT('Ctrl Pts',(75.1105319573522,-5.84037625291913,
78.4857723924628));
#182414=CARTESIAN_POINT('Ctrl Pts',(75.0407197676059,-5.82327804644709,
78.4965250099047));
#182415=CARTESIAN_POINT('Ctrl Pts',(74.8815225455768,-5.78117587108564,
78.5210809497447));
#182416=CARTESIAN_POINT('Ctrl Pts',(74.7923774225082,-5.75532525174935,
78.5348579223328));
#182417=CARTESIAN_POINT('Ctrl Pts',(74.4060712149261,-5.63331180874198,
78.5946473582739));
#182418=CARTESIAN_POINT('Ctrl Pts',(74.1161143044717,-5.51562633175389,
78.6397838540036));
#182419=CARTESIAN_POINT('Ctrl Pts',(73.6468058642806,-5.28019114583707,
78.7124137024077));
#182420=CARTESIAN_POINT('Ctrl Pts',(73.4621587323749,-5.17475206926377,
78.7408586373746));
#182421=CARTESIAN_POINT('Ctrl Pts',(73.2321074079956,-5.0264736214097,78.775795459682));
#182422=CARTESIAN_POINT('Ctrl Pts',(73.1812939893964,-4.99260329560031,
78.7834786146529));
#182423=CARTESIAN_POINT('Ctrl Pts',(73.0967382406848,-4.93434360302729,
78.7961950097605));
#182424=CARTESIAN_POINT('Ctrl Pts',(73.0627215504062,-4.91037663159999,
78.8012912367867));
#182425=CARTESIAN_POINT('Ctrl Pts',(72.9856581580757,-4.85486450461443,
78.8127897631209));
#182426=CARTESIAN_POINT('Ctrl Pts',(72.9427758341716,-4.82309218052059,
78.8191552554317));
#182427=CARTESIAN_POINT('Ctrl Pts',(72.7931050519905,-4.7090566090581,78.8412692764551));
#182428=CARTESIAN_POINT('Ctrl Pts',(72.6886349444853,-4.62372059008446,
78.8565169546274));
#182429=CARTESIAN_POINT('Ctrl Pts',(72.4039859753521,-4.37467338128644,
78.8976814089308));
#182430=CARTESIAN_POINT('Ctrl Pts',(72.2306731758408,-4.20330302562194,
78.9222989569011));
#182431=CARTESIAN_POINT('Ctrl Pts',(71.9405115839662,-3.87909173876399,
78.9630949173958));
#182432=CARTESIAN_POINT('Ctrl Pts',(71.8196909512825,-3.73034426439076,
78.9799252905244));
#182433=CARTESIAN_POINT('Ctrl Pts',(71.6556021569751,-3.50731890321708,
79.0026172808806));
#182434=CARTESIAN_POINT('Ctrl Pts',(71.6065277460403,-3.43755535910792,
79.0093788895633));
#182435=CARTESIAN_POINT('Ctrl Pts',(71.5186060903433,-3.30673921365021,
79.0214467493572));
#182436=CARTESIAN_POINT('Ctrl Pts',(71.4793467394119,-3.24598871286321,
79.0268167850708));
#182437=CARTESIAN_POINT('Ctrl Pts',(71.3929507637437,-3.10686101821857,
79.0385889666235));
#182438=CARTESIAN_POINT('Ctrl Pts',(71.3464815763088,-3.02808218467929,
79.0448879448201));
#182439=CARTESIAN_POINT('Ctrl Pts',(71.1732662685583,-2.71854836124091,
79.0682170633539));
#182440=CARTESIAN_POINT('Ctrl Pts',(71.059826609919,-2.48053914474249,79.0831758788176));
#182441=CARTESIAN_POINT('Ctrl Pts',(70.87762297681,-2.02378725445234,79.1060554196966));
#182442=CARTESIAN_POINT('Ctrl Pts',(70.8050609226306,-1.8071080843895,79.1146268697831));
#182443=CARTESIAN_POINT('Ctrl Pts',(70.7125899545345,-1.46899309363459,
79.1241600181274));
#182444=CARTESIAN_POINT('Ctrl Pts',(70.6839124547786,-1.35022793137998,
79.1268028904188));
#182445=CARTESIAN_POINT('Ctrl Pts',(70.6487186515115,-1.18262561859743,
79.1294800780258));
#182446=CARTESIAN_POINT('Ctrl Pts',(70.6392080797634,-1.13445836139378,
79.1301289722111));
#182447=CARTESIAN_POINT('Ctrl Pts',(70.6232574819972,-1.04823304989988,
79.131069623875));
#182448=CARTESIAN_POINT('Ctrl Pts',(70.6165963389618,-1.01022021113656,
79.1314075839071));
#182449=CARTESIAN_POINT('Ctrl Pts',(70.6012615705156,-0.917569688070223,
79.1320459311201));
#182450=CARTESIAN_POINT('Ctrl Pts',(70.5929680129487,-0.862872580580845,
79.1322671359214));
#182451=CARTESIAN_POINT('Ctrl Pts',(70.5627346772902,-0.643450582698795,
79.1325498134125));
#182452=CARTESIAN_POINT('Ctrl Pts',(70.5467657719953,-0.477974560331505,
79.1314044998789));
#182453=CARTESIAN_POINT('Ctrl Pts',(70.521663444057,-0.0251427074124011,
79.1248599627512));
#182454=CARTESIAN_POINT('Ctrl Pts',(70.5260487930265,0.262494154087383,
79.1169911629691));
#182455=CARTESIAN_POINT('Ctrl Pts',(70.5655475721158,0.719976509478051,
79.0990956027503));
#182456=CARTESIAN_POINT('Ctrl Pts',(70.5876117910516,0.890583935872148,
79.0912035618539));
#182457=CARTESIAN_POINT('Ctrl Pts',(70.6311727026352,1.14260324412469,79.0777610855297));
#182458=CARTESIAN_POINT('Ctrl Pts',(70.6471684543172,1.22492153072512,79.0730821924442));
#182459=CARTESIAN_POINT('Ctrl Pts',(70.6801838701324,1.37779463145153,79.0638525873169));
#182460=CARTESIAN_POINT('Ctrl Pts',(70.6967740834076,1.44843046558834,79.0593699300092));
#182461=CARTESIAN_POINT('Ctrl Pts',(70.7377323678504,1.60972366911964,79.0486279769844));
#182462=CARTESIAN_POINT('Ctrl Pts',(70.7629472190068,1.70013719355725,79.0422355131372));
#182463=CARTESIAN_POINT('Ctrl Pts',(70.8805364802515,2.08674377854459,79.0132655185377));
#182464=CARTESIAN_POINT('Ctrl Pts',(70.9934843634689,2.37592268581678,78.9874405353129));
#182465=CARTESIAN_POINT('Ctrl Pts',(71.2229170769758,2.85166682606951,78.9368555082872));
#182466=CARTESIAN_POINT('Ctrl Pts',(71.3284077329428,3.04302851677477,78.9140470136933));
#182467=CARTESIAN_POINT('Ctrl Pts',(71.4760285704928,3.27944355035933,78.8822923739797));
#182468=CARTESIAN_POINT('Ctrl Pts',(71.5088874030224,3.33033713097156,78.8752327065569));
#182469=CARTESIAN_POINT('Ctrl Pts',(71.5655851247415,3.41530682124252,78.8630539710332));
#182470=CARTESIAN_POINT('Ctrl Pts',(71.5890239088569,3.44965503660483,78.858019595707));
#182471=CARTESIAN_POINT('Ctrl Pts',(71.6435649328426,3.5278250279607,78.8463038884903));
#182472=CARTESIAN_POINT('Ctrl Pts',(71.6748987077456,3.57147175199422,78.8395735696086));
#182473=CARTESIAN_POINT('Ctrl Pts',(71.7875306116366,3.72398881884504,78.815396461354));
#182474=CARTESIAN_POINT('Ctrl Pts',(71.8718967596723,3.83044081293952,78.7973152906231));
#182475=CARTESIAN_POINT('Ctrl Pts',(72.1173743245025,4.1193241886586,78.7449465808484));
#182476=CARTESIAN_POINT('Ctrl Pts',(72.2860272109715,4.2947358349363,78.7092428954034));
#182477=CARTESIAN_POINT('Ctrl Pts',(72.6029311674239,4.58606108534071,78.6430380342528));
#182478=CARTESIAN_POINT('Ctrl Pts',(72.746917174894,4.70626857602331,78.6132358570681));
#182479=CARTESIAN_POINT('Ctrl Pts',(72.9634341270755,4.87011521940609,78.5688789991628));
#182480=CARTESIAN_POINT('Ctrl Pts',(73.0316353584405,4.91945385069203,78.5549676410381));
#182481=CARTESIAN_POINT('Ctrl Pts',(73.1597199523187,5.00797520060226,78.5289533627614));
#182482=CARTESIAN_POINT('Ctrl Pts',(73.2193106901141,5.04756568761081,78.5168933569081));
#182483=CARTESIAN_POINT('Ctrl Pts',(73.3560480084358,5.13483989891192,78.4893145598342));
#182484=CARTESIAN_POINT('Ctrl Pts',(73.4335998210645,5.18183611589787,78.473739092791));
#182485=CARTESIAN_POINT('Ctrl Pts',(73.8472898215732,5.41954965747258,78.3909712517236));
#182486=CARTESIAN_POINT('Ctrl Pts',(74.2002983826242,5.57814411593327,78.3215025719002));
#182487=CARTESIAN_POINT('Ctrl Pts',(74.6972246977593,5.74441791578092,78.2238544198736));
#182488=CARTESIAN_POINT('Ctrl Pts',(74.8299523029251,5.7836151406408,78.1977768096684));
#182489=CARTESIAN_POINT('Ctrl Pts',(75.0520380985231,5.84065928275357,78.1540273375639));
#182490=CARTESIAN_POINT('Ctrl Pts',(75.1406763966927,5.86121586993014,78.1365360630712));
#182491=CARTESIAN_POINT('Ctrl Pts',(75.2728302167312,5.88860389802947,78.1103785416352));
#182492=CARTESIAN_POINT('Ctrl Pts',(75.3160189773529,5.8970424523266,78.1018176240498));
#182493=CARTESIAN_POINT('Ctrl Pts',(75.3970911722438,5.91192600531271,78.0857189003032));
#182494=CARTESIAN_POINT('Ctrl Pts',(75.4349516088338,5.91848767271836,78.0781888264813));
#182495=CARTESIAN_POINT('Ctrl Pts',(75.5339014319438,5.934623700944,78.058480720372));
#182496=CARTESIAN_POINT('Ctrl Pts',(75.5950776266932,5.94359557818371,78.0462686714658));
#182497=CARTESIAN_POINT('Ctrl Pts',(75.9757280691111,5.99319809033613,77.9701531281212));
#182498=CARTESIAN_POINT('Ctrl Pts',(76.2977978117972,6.00802499345337,77.9052178004773));
#182499=CARTESIAN_POINT('Ctrl Pts',(76.8195846727865,5.98838131167724,77.8002835312188));
#182500=CARTESIAN_POINT('Ctrl Pts',(77.0192096687312,5.97043414084938,77.7601943237206));
#182501=CARTESIAN_POINT('Ctrl Pts',(77.3294097530175,5.92619233449805,77.6981085906362));
#182502=CARTESIAN_POINT('Ctrl Pts',(77.4407802797377,5.90696307478835,77.6758595635005));
#182503=CARTESIAN_POINT('Ctrl Pts',(77.6239732150371,5.8697771405178,77.6393361917661));
#182504=CARTESIAN_POINT('Ctrl Pts',(77.6961242916996,5.85368736183456,77.6249704165238));
#182505=CARTESIAN_POINT('Ctrl Pts',(77.8413934735073,5.81836088217616,77.5960830339961));
#182506=CARTESIAN_POINT('Ctrl Pts',(77.9144839370153,5.79906566072541,77.5815677452047));
#182507=CARTESIAN_POINT('Ctrl Pts',(78.1068734326261,5.74423246994479,77.5434041952723));
#182508=CARTESIAN_POINT('Ctrl Pts',(78.2254723420467,5.70626788348198,77.519923810019));
#182509=CARTESIAN_POINT('Ctrl Pts',(78.6574950837772,5.5525025884081,77.4344842268919));
#182510=CARTESIAN_POINT('Ctrl Pts',(78.9623111365041,5.41346751704915,77.3744216644624));
#182511=CARTESIAN_POINT('Ctrl Pts',(79.3764899869024,5.17966590290425,77.2920348161791));
#182512=CARTESIAN_POINT('Ctrl Pts',(79.4966476933306,5.10599116173046,77.2680262770202));
#182513=CARTESIAN_POINT('Ctrl Pts',(79.6576903960397,4.99905313457317,77.2355871212688));
#182514=CARTESIAN_POINT('Ctrl Pts',(79.7009208729756,4.96950313728936,77.226852099324));
#182515=CARTESIAN_POINT('Ctrl Pts',(79.777747666932,4.91546146768861,77.2112717208417));
#182516=CARTESIAN_POINT('Ctrl Pts',(79.8114875006111,4.89118692514048,77.2044084912291));
#182517=CARTESIAN_POINT('Ctrl Pts',(79.895823206784,4.82913759845088,77.1872024718257));
#182518=CARTESIAN_POINT('Ctrl Pts',(79.9460778900933,4.7908962215886,77.1769035287751));
#182519=CARTESIAN_POINT('Ctrl Pts',(80.1635838218191,4.61977149189244,77.1321536635723));
#182520=CARTESIAN_POINT('Ctrl Pts',(80.324250531467,4.47853374837999,77.0986403117906));
#182521=CARTESIAN_POINT('Ctrl Pts',(80.6271125494264,4.18164522231204,77.0349406725622));
#182522=CARTESIAN_POINT('Ctrl Pts',(80.7693767387962,4.02650400762146,77.0047506848111));
#182523=CARTESIAN_POINT('Ctrl Pts',(80.9464266728784,3.81158112524013,76.9669685334703));
#182524=CARTESIAN_POINT('Ctrl Pts',(80.988708242165,3.75843012390612,76.9579275000913));
#182525=CARTESIAN_POINT('Ctrl Pts',(81.094494076567,3.62068772935883,76.935265544543));
#182526=CARTESIAN_POINT('Ctrl Pts',(81.1566958367114,3.53508461845458,76.9219001376667));
#182527=CARTESIAN_POINT('Ctrl Pts',(81.2581845445671,3.38733004669684,76.9000287062213));
#182528=CARTESIAN_POINT('Ctrl Pts',(81.2986414263839,3.32604764074379,76.8912909143801));
#182529=CARTESIAN_POINT('Ctrl Pts',(81.3801382552093,3.19752908873205,76.873647889353));
#182530=CARTESIAN_POINT('Ctrl Pts',(81.4210032529613,3.13019425222693,76.8647774825469));
#182531=CARTESIAN_POINT('Ctrl Pts',(81.5302614429409,2.94192024819869,76.8409875721766));
#182532=CARTESIAN_POINT('Ctrl Pts',(81.595837516978,2.81933548504786,76.8266243436442));
#182533=CARTESIAN_POINT('Ctrl Pts',(81.8163083064221,2.37053073248376,76.7779182144174));
#182534=CARTESIAN_POINT('Ctrl Pts',(81.9462949306246,2.0324542334475,76.7484150510847));
#182535=CARTESIAN_POINT('Ctrl Pts',(82.0860301786864,1.54156316515938,76.7140107508896));
#182536=CARTESIAN_POINT('Ctrl Pts',(82.1214375435231,1.39718988972072,76.7048636066006));
#182537=CARTESIAN_POINT('Ctrl Pts',(82.1619880194072,1.20078932387463,76.6935951612618));
#182538=CARTESIAN_POINT('Ctrl Pts',(82.1718276334386,1.14982724721509,76.6907763887375));
#182539=CARTESIAN_POINT('Ctrl Pts',(82.1878037718395,1.06094329259262,76.6860353501978));
#182540=CARTESIAN_POINT('Ctrl Pts',(82.1942371025926,1.02308124160296,76.6840703902107));
#182541=CARTESIAN_POINT('Ctrl Pts',(82.2083632519552,0.934859770359395,
76.6796183635456));
#182542=CARTESIAN_POINT('Ctrl Pts',(82.2157814810488,0.884458353110544,
76.6771710938632));
#182543=CARTESIAN_POINT('Ctrl Pts',(82.2402686356171,0.702136256874164,
76.6686771064589));
#182544=CARTESIAN_POINT('Ctrl Pts',(82.253628329319,0.569729862771318,76.6631852551421));
#182545=CARTESIAN_POINT('Ctrl Pts',(82.2784185771159,0.20409861249248,76.6500244617369));
#182546=CARTESIAN_POINT('Ctrl Pts',(82.2807799093679,-0.0295626711262976,
76.6438537772989));
#182547=CARTESIAN_POINT('Ctrl Pts',(82.2618435769026,-0.429656464211375,
76.6374850989974));
#182548=CARTESIAN_POINT('Ctrl Pts',(82.2471003818093,-0.596109657678972,
76.6360872992544));
#182549=CARTESIAN_POINT('Ctrl Pts',(82.2091099180954,-0.888187784942348,
76.6359207005032));
#182550=CARTESIAN_POINT('Ctrl Pts',(82.1887110791273,-1.01407673316437,
76.6366073461182));
#182551=CARTESIAN_POINT('Ctrl Pts',(82.1496475626092,-1.21509340448372,
76.6389362792751));
#182552=CARTESIAN_POINT('Ctrl Pts',(82.133467177538,-1.29066879784691,76.6400952949064));
#182553=CARTESIAN_POINT('Ctrl Pts',(82.0989573437285,-1.43812881980057,
76.642912701163));
#182554=CARTESIAN_POINT('Ctrl Pts',(82.0807435178298,-1.51002677651945,
76.6445488752448));
#182555=CARTESIAN_POINT('Ctrl Pts',(82.0313831230445,-1.69095525957267,
76.6493277639895));
#182556=CARTESIAN_POINT('Ctrl Pts',(81.9985020893052,-1.79947293740234,
76.6528089312253));
#182557=CARTESIAN_POINT('Ctrl Pts',(81.9175082166549,-2.04216298327549,
76.6619633365268));
#182558=CARTESIAN_POINT('Ctrl Pts',(81.8676790502401,-2.17567721545636,
76.6679676089574));
#182559=CARTESIAN_POINT('Ctrl Pts',(81.679944505087,-2.62934070051116,76.6916039852982));
#182560=CARTESIAN_POINT('Ctrl Pts',(81.5193074149887,-2.93907591727265,
76.7134752678841));
#182561=CARTESIAN_POINT('Ctrl Pts',(81.300880019114,-3.28356934743988,76.743633219079));
#182562=CARTESIAN_POINT('Ctrl Pts',(81.26804731515,-3.33367980522927,76.7481743819701));
#182563=CARTESIAN_POINT('Ctrl Pts',(81.2110942589947,-3.41782967137207,
76.7560540634447));
#182564=CARTESIAN_POINT('Ctrl Pts',(81.1873569589511,-3.45212657124492,
76.7593384248907));
#182565=CARTESIAN_POINT('Ctrl Pts',(81.1311145705204,-3.53160460917959,
76.7671194910825));
#182566=CARTESIAN_POINT('Ctrl Pts',(81.0983370790566,-3.57658288754655,
76.7716546612521));
#182567=CARTESIAN_POINT('Ctrl Pts',(80.9572400205273,-3.76464870121624,
76.7911976352345));
#182568=CARTESIAN_POINT('Ctrl Pts',(80.8431966105938,-3.90323958614348,
76.807045383938));
#182569=CARTESIAN_POINT('Ctrl Pts',(80.4697695933691,-4.31770968784781,
76.8594890092059));
#182570=CARTESIAN_POINT('Ctrl Pts',(80.1905711106454,-4.5740449840216,76.8995081864004));
#182571=CARTESIAN_POINT('Ctrl Pts',(79.819426840938,-4.85499887651365,76.9543868997662));
#182572=CARTESIAN_POINT('Ctrl Pts',(79.7482501543278,-4.9064451016579,76.9649759886891));
#182573=CARTESIAN_POINT('Ctrl Pts',(79.6168402424332,-4.99707237235025,
76.9846435149406));
#182574=CARTESIAN_POINT('Ctrl Pts',(79.5569772963478,-5.03677689086184,
76.9936454847934));
#182575=CARTESIAN_POINT('Ctrl Pts',(79.4213475048184,-5.1232370496266,77.0141332886399));
#182576=CARTESIAN_POINT('Ctrl Pts',(79.3452276705649,-5.16938833648931,
77.0256944149413));
#182577=CARTESIAN_POINT('Ctrl Pts',(79.0730678742054,-5.32613513134418,
77.067233631847));
#182578=CARTESIAN_POINT('Ctrl Pts',(78.8719291333387,-5.4271895740849,77.098305064101));
#182579=CARTESIAN_POINT('Ctrl Pts',(78.4557044736368,-5.60734040904606,
77.1630302216307));
#182580=CARTESIAN_POINT('Ctrl Pts',(78.2407864104021,-5.68586241316359,
77.1966643107356));
#182581=CARTESIAN_POINT('Ctrl Pts',(77.8754000295744,-5.795686413567,77.2537453323072));
#182582=CARTESIAN_POINT('Ctrl Pts',(77.727247794333,-5.83397582908958,77.2768607482368));
#182583=CARTESIAN_POINT('Ctrl Pts',(77.5314975681942,-5.8764784791733,77.3072295801729));
#182584=CARTESIAN_POINT('Ctrl Pts',(77.4850966509068,-5.88596643852881,
77.3144155863192));
#182585=CARTESIAN_POINT('Ctrl Pts',(77.4134884056225,-5.89970727127574,
77.3254808150766));
#182586=CARTESIAN_POINT('Ctrl Pts',(77.3883598281107,-5.90435908116652,
77.3293591566146));
#182587=CARTESIAN_POINT('Ctrl Pts',(77.3632014628439,-5.90884651834311,
77.3332369269199));
#182588=CARTESIAN_POINT('Origin',(79.767904168913,7.105427357601E-15,96.9709836566246));
#182589=CARTESIAN_POINT('',(78.0997797390488,-6.8936542710855,80.5105799046739));
#182590=CARTESIAN_POINT('Origin',(76.9027092374091,7.105427357601E-15,80.7216557319231));
#182591=CARTESIAN_POINT('',(80.8781505817192,-6.89365427108549,96.2675039528693));
#182592=CARTESIAN_POINT('',(80.9649746705526,-6.89365427108549,96.7599078293754));
#182593=CARTESIAN_POINT('',(74.7871667585286,-4.93000669486554,97.3415087399564));
#182594=CARTESIAN_POINT('Origin',(79.6810800800795,7.105427357601E-15,96.4785797801185));
#182595=CARTESIAN_POINT('',(74.3530463143613,-4.93000669486554,94.8794893574259));
#182596=CARTESIAN_POINT('',(74.873990847362,-4.93000669486554,97.8339126164625));
#182597=CARTESIAN_POINT('',(72.9876403879442,2.93305265169617,95.1202472618724));
#182598=CARTESIAN_POINT('Origin',(79.2469596359123,7.105427357601E-15,94.016560397588));
#182599=CARTESIAN_POINT('',(73.4217608321114,2.93305265169629,97.5822666444029));
#182600=CARTESIAN_POINT('',(73.5085849209449,2.93305265169617,98.074670520909));
#182601=CARTESIAN_POINT('',(84.5749934016305,4.93000669486556,95.6156508202806));
#182602=CARTESIAN_POINT('Origin',(79.6810800800795,7.105427357601E-15,96.4785797801185));
#182603=CARTESIAN_POINT('',(84.1408729574633,4.93000669486556,93.1536314377501));
#182604=CARTESIAN_POINT('',(84.661817490464,4.93000669486556,96.1080546967868));
#182605=CARTESIAN_POINT('',(85.5062788838804,-2.93305265169616,92.9128735333036));
#182606=CARTESIAN_POINT('Origin',(79.2469596359123,7.105427357601E-15,94.016560397588));
#182607=CARTESIAN_POINT('',(85.9403993280477,-2.93305265169627,95.3748929158341));
#182608=CARTESIAN_POINT('',(86.0272234168811,-2.93305265169616,95.8672967923402));
#182609=CARTESIAN_POINT('Origin',(79.6810800800795,7.105427357601E-15,96.4785797801185));
#182610=CARTESIAN_POINT('Origin',(79.6810800800795,7.105427357601E-15,96.4785797801185));
#182611=CARTESIAN_POINT('',(84.8261737214021,3.98351688341827,96.0790742588248));
#182612=CARTESIAN_POINT('',(73.672941151883,1.98656284024889,98.0456900829471));
#182613=CARTESIAN_POINT('Origin',(79.767904168913,7.105427357601E-15,96.9709836566246));
#182614=CARTESIAN_POINT('Ctrl Pts',(84.8261737218292,3.98351688369324,96.0790742592051));
#182615=CARTESIAN_POINT('Ctrl Pts',(84.7893586077452,4.12739717890119,96.0163852530348));
#182616=CARTESIAN_POINT('Ctrl Pts',(84.7515513858236,4.27253790876338,95.949354543555));
#182617=CARTESIAN_POINT('Ctrl Pts',(84.7127017230961,4.41924001707104,95.8779910058261));
#182618=CARTESIAN_POINT('Ctrl Pts',(84.6731714183888,4.56851233079177,95.805377186468));
#182619=CARTESIAN_POINT('Ctrl Pts',(84.6325609344404,4.71940100607333,95.7282775447341));
#182620=CARTESIAN_POINT('Ctrl Pts',(84.5908237439362,4.87217012300172,95.6467002846453));
#182621=CARTESIAN_POINT('Ctrl Pts',(84.5855648573402,4.89141903390341,95.636421548716));
#182622=CARTESIAN_POINT('Ctrl Pts',(84.5802881016179,4.91069773355134,95.6260717228448));
#182623=CARTESIAN_POINT('Ctrl Pts',(84.5749934016305,4.93000669486555,95.6156508202806));
#182624=CARTESIAN_POINT('Ctrl Pts',(73.4217608321114,2.93305265169625,97.5822666444029));
#182625=CARTESIAN_POINT('Ctrl Pts',(73.5563352960282,2.44228015705305,97.8471329035571));
#182626=CARTESIAN_POINT('Ctrl Pts',(73.6729411519522,1.98656284058742,98.0456900836835));
#182627=CARTESIAN_POINT('Origin',(76.9027092374091,7.31897349866028E-15,
80.7216557319231));
#182628=CARTESIAN_POINT('',(77.4879453938384,-5.17024070331411,78.7906949060641));
#182629=CARTESIAN_POINT('Origin',(76.5901425176087,7.31897349866028E-15,
78.9490017765011));
#182630=CARTESIAN_POINT('',(77.8005121136389,-5.17024070331411,80.5633488614862));
#182631=CARTESIAN_POINT('',(77.8005121136389,-5.17024070331411,80.5633488614862));
#182632=CARTESIAN_POINT('Origin',(76.9027092374091,7.31897349866028E-15,
80.7216557319231));
#182633=CARTESIAN_POINT('Origin',(76.5901425176087,7.15881389286582E-15,
78.9490017765011));
#182634=CARTESIAN_POINT('',(79.8067669160619,-4.75889434981443,76.1478855621002));
#182635=CARTESIAN_POINT('Ctrl Pts',(77.3632014628439,-5.90884651834311,
77.3332369269199));
#182636=CARTESIAN_POINT('Ctrl Pts',(77.3506260636621,-5.91108956208624,
77.3351752289124));
#182637=CARTESIAN_POINT('Ctrl Pts',(77.3380432219561,-5.91329153709518,
77.3371133880793));
#182638=CARTESIAN_POINT('Ctrl Pts',(77.2788465225023,-5.92345162954785,
77.3462257796284));
#182639=CARTESIAN_POINT('Ctrl Pts',(77.2321445292669,-5.9308869101996,77.3533979555682));
#182640=CARTESIAN_POINT('Ctrl Pts',(77.0753511513317,-5.95390907536924,
77.3774304758976));
#182641=CARTESIAN_POINT('Ctrl Pts',(76.9649056251977,-5.9669307645459,77.3942823635277));
#182642=CARTESIAN_POINT('Ctrl Pts',(76.6618859723424,-5.99395217460897,
77.4404025166063));
#182643=CARTESIAN_POINT('Ctrl Pts',(76.4688807497412,-6.00159982251535,
77.4696551679202));
#182644=CARTESIAN_POINT('Ctrl Pts',(75.9898225965994,-5.99694049464808,
77.5423125383788));
#182645=CARTESIAN_POINT('Ctrl Pts',(75.7043666432232,-5.97324907454268,
77.5856654911142));
#182646=CARTESIAN_POINT('Ctrl Pts',(75.3230929585664,-5.91332269699863,
77.6439595581747));
#182647=CARTESIAN_POINT('Ctrl Pts',(75.2248337194123,-5.8952978858626,77.6590155272321));
#182648=CARTESIAN_POINT('Ctrl Pts',(75.0561701016533,-5.85988616248508,
77.684917889718));
#182649=CARTESIAN_POINT('Ctrl Pts',(74.9855423687038,-5.84368697446087,
77.6957823251515));
#182650=CARTESIAN_POINT('Ctrl Pts',(74.8372974880923,-5.80678452955541,
77.7186216711591));
#182651=CARTESIAN_POINT('Ctrl Pts',(74.7597673880015,-5.78578732540409,
77.7305870417884));
#182652=CARTESIAN_POINT('Ctrl Pts',(74.5352351900356,-5.72000753864354,
77.7652901398945));
#182653=CARTESIAN_POINT('Ctrl Pts',(74.389509133096,-5.67103491114391,77.7878786138494));
#182654=CARTESIAN_POINT('Ctrl Pts',(74.0177569941561,-5.52966843690258,
77.8455618419822));
#182655=CARTESIAN_POINT('Ctrl Pts',(73.7951963689168,-5.42880121446908,
77.8801607875621));
#182656=CARTESIAN_POINT('Ctrl Pts',(73.4255301441766,-5.23281058087107,
77.9372382592266));
#182657=CARTESIAN_POINT('Ctrl Pts',(73.2752940405537,-5.14445614402073,
77.9603122637607));
#182658=CARTESIAN_POINT('Ctrl Pts',(73.0802293981269,-5.0178726511131,77.9899098159128));
#182659=CARTESIAN_POINT('Ctrl Pts',(73.0318522668943,-4.98546007820204,
77.9972189074484));
#182660=CARTESIAN_POINT('Ctrl Pts',(72.9498300101684,-4.92874514196303,
78.0095469802084));
#182661=CARTESIAN_POINT('Ctrl Pts',(72.915955360544,-4.90479576543907,78.0146186542405));
#182662=CARTESIAN_POINT('Ctrl Pts',(72.836423503911,-4.84731282746839,78.0264783303979));
#182663=CARTESIAN_POINT('Ctrl Pts',(72.7909846540467,-4.81347588462272,
78.03321724325));
#182664=CARTESIAN_POINT('Ctrl Pts',(72.5809447832021,-4.65236574538632,
78.0642156668819));
#182665=CARTESIAN_POINT('Ctrl Pts',(72.4224651225121,-4.51709693169309,
78.0871660182166));
#182666=CARTESIAN_POINT('Ctrl Pts',(72.0296418436112,-4.14463632815574,
78.1433767271642));
#182667=CARTESIAN_POINT('Ctrl Pts',(71.8072999109357,-3.89551556024683,
78.1745250907942));
#182668=CARTESIAN_POINT('Ctrl Pts',(71.5513795944523,-3.5555689415051,78.2099820159938));
#182669=CARTESIAN_POINT('Ctrl Pts',(71.4977899533019,-3.48087799896882,
78.2173775353426));
#182670=CARTESIAN_POINT('Ctrl Pts',(71.4051153999581,-3.34525020110468,
78.2301158055585));
#182671=CARTESIAN_POINT('Ctrl Pts',(71.3653820729729,-3.28478818682766,
78.2355588725799));
#182672=CARTESIAN_POINT('Ctrl Pts',(71.2813539430398,-3.15175759703652,
78.2470274246441));
#182673=CARTESIAN_POINT('Ctrl Pts',(71.2374838575667,-3.07893390829918,
78.2529873714572));
#182674=CARTESIAN_POINT('Ctrl Pts',(71.1048247433324,-2.84779572722359,
78.2709097487272));
#182675=CARTESIAN_POINT('Ctrl Pts',(71.0216063385146,-2.68633845119482,
78.2820050938437));
#182676=CARTESIAN_POINT('Ctrl Pts',(70.8091330343852,-2.22411028493838,
78.3096974484067));
#182677=CARTESIAN_POINT('Ctrl Pts',(70.6967675289738,-1.91613684032428,
78.3235569903442));
#182678=CARTESIAN_POINT('Ctrl Pts',(70.5766394231886,-1.48087712938312,
78.3360310584553));
#182679=CARTESIAN_POINT('Ctrl Pts',(70.5472829598692,-1.36027592592621,
78.3387604631571));
#182680=CARTESIAN_POINT('Ctrl Pts',(70.5113396586785,-1.19025983035946,
78.3415245968309));
#182681=CARTESIAN_POINT('Ctrl Pts',(70.5016583997892,-1.14154227312012,
78.3421934823646));
#182682=CARTESIAN_POINT('Ctrl Pts',(70.4855292057251,-1.05487694172736,
78.3431589091541));
#182683=CARTESIAN_POINT('Ctrl Pts',(70.4788445963702,-1.01697766904155,
78.3435049055603));
#182684=CARTESIAN_POINT('Ctrl Pts',(70.4637261463444,-0.926274313297555,
78.3441515691997));
#182685=CARTESIAN_POINT('Ctrl Pts',(70.455625741196,-0.873418202764558,
78.3443827825314));
#182686=CARTESIAN_POINT('Ctrl Pts',(70.4250964594316,-0.655148517543934,
78.3447546257627));
#182687=CARTESIAN_POINT('Ctrl Pts',(70.4087458166207,-0.48895652997662,
78.34366374263));
#182688=CARTESIAN_POINT('Ctrl Pts',(70.3798662879664,0.0166250587345677,
78.3365136485946));
#182689=CARTESIAN_POINT('Ctrl Pts',(70.3888296273098,0.356518233400312,
78.326530536891));
#182690=CARTESIAN_POINT('Ctrl Pts',(70.4415658323201,0.833400722205972,
78.3059594061294));
#182691=CARTESIAN_POINT('Ctrl Pts',(70.4618608837099,0.972495747144222,
78.2991498327544));
#182692=CARTESIAN_POINT('Ctrl Pts',(70.5011356182525,1.18873727561341,78.2873061484214));
#182693=CARTESIAN_POINT('Ctrl Pts',(70.5168337837154,1.26645557188026,78.2827915143711));
#182694=CARTESIAN_POINT('Ctrl Pts',(70.5500690224069,1.41581376705768,78.273614099924));
#182695=CARTESIAN_POINT('Ctrl Pts',(70.5673989816729,1.48748708892914,78.2689843157469));
#182696=CARTESIAN_POINT('Ctrl Pts',(70.6128044119319,1.66129737124357,78.2571996893161));
#182697=CARTESIAN_POINT('Ctrl Pts',(70.642258742329,1.76303311942229,78.2498276593441));
#182698=CARTESIAN_POINT('Ctrl Pts',(70.6949391624486,1.92857311319152,78.2370314251777));
#182699=CARTESIAN_POINT('Ctrl Pts',(70.7166006604831,1.9928695374001,78.2318590157327));
#182700=CARTESIAN_POINT('Ctrl Pts',(70.8094864699728,2.25394775023938,78.2100092635616));
#182701=CARTESIAN_POINT('Ctrl Pts',(70.8898007168674,2.44721072860713,78.1918547977842));
#182702=CARTESIAN_POINT('Ctrl Pts',(71.0747122441781,2.83410173331591,78.1510290794821));
#182703=CARTESIAN_POINT('Ctrl Pts',(71.1802104402173,3.0269305080173,78.1282031026571));
#182704=CARTESIAN_POINT('Ctrl Pts',(71.3292924509109,3.26722079926652,78.0961262804633));
#182705=CARTESIAN_POINT('Ctrl Pts',(71.3635404686114,3.32052102532757,78.0887675174631));
#182706=CARTESIAN_POINT('Ctrl Pts',(71.4217690184604,3.40806744445403,78.0762596672505));
#182707=CARTESIAN_POINT('Ctrl Pts',(71.4452824694775,3.44263164095962,78.0712093974405));
#182708=CARTESIAN_POINT('Ctrl Pts',(71.4993108488769,3.52029558856277,78.0596037690665));
#182709=CARTESIAN_POINT('Ctrl Pts',(71.5300341330659,3.56323833170345,78.0530043439425));
#182710=CARTESIAN_POINT('Ctrl Pts',(71.6461020388339,3.72101862213893,78.0280875790888));
#182711=CARTESIAN_POINT('Ctrl Pts',(71.7349337633283,3.83311675573491,78.0090475772363));
#182712=CARTESIAN_POINT('Ctrl Pts',(72.0518191055356,4.2047051751801,77.9414605108095));
#182713=CARTESIAN_POINT('Ctrl Pts',(72.2980985427034,4.44711785572191,77.8895214891883));
#182714=CARTESIAN_POINT('Ctrl Pts',(72.6559002459519,4.74230537440079,77.8155831897031));
#182715=CARTESIAN_POINT('Ctrl Pts',(72.7502668035142,4.81544297399608,77.7962031870972));
#182716=CARTESIAN_POINT('Ctrl Pts',(72.9074560487902,4.92977041751769,77.7641243732399));
#182717=CARTESIAN_POINT('Ctrl Pts',(72.9689814971273,4.97273749254529,77.7516164529573));
#182718=CARTESIAN_POINT('Ctrl Pts',(73.0936312062421,5.05627187149365,77.7263700008674));
#182719=CARTESIAN_POINT('Ctrl Pts',(73.156744392514,5.09683099428538,77.7136337322795));
#182720=CARTESIAN_POINT('Ctrl Pts',(73.3214067522893,5.19822833535625,77.6805191138512));
#182721=CARTESIAN_POINT('Ctrl Pts',(73.4240327992625,5.25720186420739,77.659990011575));
#182722=CARTESIAN_POINT('Ctrl Pts',(73.6606155811364,5.38374880961076,77.6128761954652));
#182723=CARTESIAN_POINT('Ctrl Pts',(73.7955091067059,5.44934283602376,77.5861614370359));
#182724=CARTESIAN_POINT('Ctrl Pts',(74.140470117322,5.60092360028518,77.5180840535909));
#182725=CARTESIAN_POINT('Ctrl Pts',(74.3532445281378,5.67993183846909,77.4763128793733));
#182726=CARTESIAN_POINT('Ctrl Pts',(74.7203187609538,5.79230262124935,77.4041621495857));
#182727=CARTESIAN_POINT('Ctrl Pts',(74.8724353469321,5.83218901281933,77.3742355919039));
#182728=CARTESIAN_POINT('Ctrl Pts',(75.0722053480645,5.87598185418345,77.3347496705309));
#182729=CARTESIAN_POINT('Ctrl Pts',(75.1186194837403,5.88556141947755,77.3255627041334));
#182730=CARTESIAN_POINT('Ctrl Pts',(75.2025522413787,5.90181368406663,77.308920105476));
#182731=CARTESIAN_POINT('Ctrl Pts',(75.24003145447,5.90868791565307,77.301477788033));
#182732=CARTESIAN_POINT('Ctrl Pts',(75.3235256948871,5.92315162420742,77.2848720637462));
#182733=CARTESIAN_POINT('Ctrl Pts',(75.3695672465983,5.93055540832166,77.2756983035838));
#182734=CARTESIAN_POINT('Ctrl Pts',(75.5226945858303,5.95328362363035,77.2451414975433));
#182735=CARTESIAN_POINT('Ctrl Pts',(75.6300968331472,5.96615666075899,77.2236346384187));
#182736=CARTESIAN_POINT('Ctrl Pts',(75.9218011656577,5.99283711972101,77.1651094690613));
#182737=CARTESIAN_POINT('Ctrl Pts',(76.1064794439842,6.00082178650795,77.1279387445323));
#182738=CARTESIAN_POINT('Ctrl Pts',(76.5850612752272,5.99852002942558,77.0316465318224));
#182739=CARTESIAN_POINT('Ctrl Pts',(76.8784014654325,5.97466202938466,76.9726769545909));
#182740=CARTESIAN_POINT('Ctrl Pts',(77.2664482155399,5.91305785057169,76.8950884073305));
#182741=CARTESIAN_POINT('Ctrl Pts',(77.3636815927662,5.89505524682198,76.8756798841097));
#182742=CARTESIAN_POINT('Ctrl Pts',(77.5307533009132,5.85967239758531,76.8423898515985));
#182743=CARTESIAN_POINT('Ctrl Pts',(77.6008057072906,5.84346835431527,76.8284494608582));
#182744=CARTESIAN_POINT('Ctrl Pts',(77.7479925249043,5.80652352441267,76.7991949427111));
#182745=CARTESIAN_POINT('Ctrl Pts',(77.8250405021964,5.78548336087124,76.783901965347));
#182746=CARTESIAN_POINT('Ctrl Pts',(78.0487572363214,5.71939886286866,76.7395484291761));
#182747=CARTESIAN_POINT('Ctrl Pts',(78.1941581527879,5.67010858638246,76.7107881629974));
#182748=CARTESIAN_POINT('Ctrl Pts',(78.5663566420792,5.52727369620649,76.6372268322258));
#182749=CARTESIAN_POINT('Ctrl Pts',(78.7896214687844,5.42500736946267,76.5931669259759));
#182750=CARTESIAN_POINT('Ctrl Pts',(79.160632137667,5.22586915268047,76.5195382731795));
#182751=CARTESIAN_POINT('Ctrl Pts',(79.3115795691863,5.13586652517762,76.4894516652793));
#182752=CARTESIAN_POINT('Ctrl Pts',(79.5038555214824,5.00914213561933,76.4507513777024));
#182753=CARTESIAN_POINT('Ctrl Pts',(79.5489743655254,4.97849234524775,76.441641459805));
#182754=CARTESIAN_POINT('Ctrl Pts',(79.6274610622036,4.92355615436399,76.4257345869609));
#182755=CARTESIAN_POINT('Ctrl Pts',(79.6610090100303,4.8995421684983,76.4189152439638));
#182756=CARTESIAN_POINT('Ctrl Pts',(79.7416892754808,4.84049101512612,76.4024663000907));
#182757=CARTESIAN_POINT('Ctrl Pts',(79.7885578906264,4.80509302272123,76.3928705667529));
#182758=CARTESIAN_POINT('Ctrl Pts',(79.8916332410604,4.72478546413949,76.3716886627046));
#182759=CARTESIAN_POINT('Ctrl Pts',(79.9475670358848,4.67953047094111,76.360140774091));
#182760=CARTESIAN_POINT('Ctrl Pts',(80.1271121698391,4.52872849850527,76.3229253994331));
#182761=CARTESIAN_POINT('Ctrl Pts',(80.2472493340549,4.41902999173157,76.2977918688098));
#182762=CARTESIAN_POINT('Ctrl Pts',(80.5696849700015,4.09923023111786,76.2299111378373));
#182763=CARTESIAN_POINT('Ctrl Pts',(80.7614230962109,3.87874331358182,76.1890571508917));
#182764=CARTESIAN_POINT('Ctrl Pts',(80.9927935034548,3.56951527749707,76.1394227644377));
#182765=CARTESIAN_POINT('Ctrl Pts',(81.0473347237524,3.49292103560964,76.1276911222302));
#182766=CARTESIAN_POINT('Ctrl Pts',(81.1405709663592,3.35523550989101,76.107582479175));
#182767=CARTESIAN_POINT('Ctrl Pts',(81.1799975354418,3.29468449084741,76.0990605515274));
#182768=CARTESIAN_POINT('Ctrl Pts',(81.2623716164879,3.16303589907158,76.0812131678088));
#182769=CARTESIAN_POINT('Ctrl Pts',(81.3049619008457,3.09172341205876,76.0719586563723));
#182770=CARTESIAN_POINT('Ctrl Pts',(81.4292432532612,2.87348182997442,76.044860509596));
#182771=CARTESIAN_POINT('Ctrl Pts',(81.5063177107551,2.72391007910021,76.0279273419392));
#182772=CARTESIAN_POINT('Ctrl Pts',(81.6927602095248,2.32160531003179,75.9864652001521));
#182773=CARTESIAN_POINT('Ctrl Pts',(81.7913600207955,2.06412738630946,75.9639957786357));
#182774=CARTESIAN_POINT('Ctrl Pts',(81.9249316956424,1.62823816926073,75.9318082406385));
#182775=CARTESIAN_POINT('Ctrl Pts',(81.9700452684845,1.45350869865743,75.9203794176626));
#182776=CARTESIAN_POINT('Ctrl Pts',(82.0187776624722,1.22248114638955,75.9069646256192));
#182777=CARTESIAN_POINT('Ctrl Pts',(82.0295164684856,1.16784487494401,75.9039140647558));
#182778=CARTESIAN_POINT('Ctrl Pts',(82.0464149938574,1.07511273889118,75.8989335929142));
#182779=CARTESIAN_POINT('Ctrl Pts',(82.0529673022251,1.03709562752515,75.8969472069984));
#182780=CARTESIAN_POINT('Ctrl Pts',(82.066971480648,0.950918421918528,75.8925681038923));
#182781=CARTESIAN_POINT('Ctrl Pts',(82.0742060528834,0.902725105582203,
75.8902069326183));
#182782=CARTESIAN_POINT('Ctrl Pts',(82.0971797447513,0.735989630105551,
75.8823506794407));
#182783=CARTESIAN_POINT('Ctrl Pts',(82.1099904223252,0.617051596595321,
75.8772911226832));
#182784=CARTESIAN_POINT('Ctrl Pts',(82.1363147537706,0.279113023273343,
75.8645656645264));
#182785=CARTESIAN_POINT('Ctrl Pts',(82.1414933687785,0.0596010719977289,
75.8582576433233));
#182786=CARTESIAN_POINT('Ctrl Pts',(82.1271196127539,-0.413320012160215,
75.8492799132833));
#182787=CARTESIAN_POINT('Ctrl Pts',(82.1035997858041,-0.666205737284208,
75.8473448774582));
#182788=CARTESIAN_POINT('Ctrl Pts',(82.0487369542072,-1.01733616280022,
75.8488792407423));
#182789=CARTESIAN_POINT('Ctrl Pts',(82.0305389796217,-1.11737104404053,
75.8498024922732));
#182790=CARTESIAN_POINT('Ctrl Pts',(81.99493222973,-1.28870363351042,75.8522258344588));
#182791=CARTESIAN_POINT('Ctrl Pts',(81.9787186485675,-1.36022969830393,
75.8534933047212));
#182792=CARTESIAN_POINT('Ctrl Pts',(81.941917219994,-1.51001194890346,75.8566852883709));
#182793=CARTESIAN_POINT('Ctrl Pts',(81.9210543179682,-1.58818430196483,
75.8586638568195));
#182794=CARTESIAN_POINT('Ctrl Pts',(81.856190435138,-1.81316741604527,75.8652583773005));
#182795=CARTESIAN_POINT('Ctrl Pts',(81.8082105628448,-1.95874004854391,
75.8706492320269));
#182796=CARTESIAN_POINT('Ctrl Pts',(81.6711855215464,-2.32709193130458,
75.8871040486295));
#182797=CARTESIAN_POINT('Ctrl Pts',(81.5743894861488,-2.54662762678099,
75.8996428677812));
#182798=CARTESIAN_POINT('Ctrl Pts',(81.3847491872626,-2.91570447120974,
75.9251142739667));
#182799=CARTESIAN_POINT('Ctrl Pts',(81.2978939989466,-3.06805259948355,
75.937024633462));
#182800=CARTESIAN_POINT('Ctrl Pts',(81.1709742064106,-3.26967982502136,
75.9545410210959));
#182801=CARTESIAN_POINT('Ctrl Pts',(81.1365636227905,-3.32248553230666,
75.9592997389913));
#182802=CARTESIAN_POINT('Ctrl Pts',(81.07789208696,-3.40949631070709,75.9674168694879));
#182803=CARTESIAN_POINT('Ctrl Pts',(81.0540897440679,-3.44400996024434,
75.9707103972316));
#182804=CARTESIAN_POINT('Ctrl Pts',(80.9991535597465,-3.52190824564898,
75.9783106934124));
#182805=CARTESIAN_POINT('Ctrl Pts',(80.9678002885372,-3.56512955816831,
75.9826485134425));
#182806=CARTESIAN_POINT('Ctrl Pts',(80.8475726083012,-3.72629742944358,
75.9992977067868));
#182807=CARTESIAN_POINT('Ctrl Pts',(80.7549573052134,-3.84133200312724,
76.0121547757447));
#182808=CARTESIAN_POINT('Ctrl Pts',(80.4011471605722,-4.24904527589804,
76.0616512699248));
#182809=CARTESIAN_POINT('Ctrl Pts',(80.1159069052643,-4.51904987235405,
76.1023284270222));
#182810=CARTESIAN_POINT('Ctrl Pts',(79.8067669160617,-4.75889434981455,
76.1478855621002));
#182811=CARTESIAN_POINT('',(81.8428871748401,-1.8061545077823,75.7888626245105));
#182812=CARTESIAN_POINT('Origin',(76.2081165267415,7.15881389286582E-15,
76.7824247198743));
#182813=CARTESIAN_POINT('Ctrl Pts',(81.8428871748402,-1.80615450778233,
75.7888626245105));
#182814=CARTESIAN_POINT('Ctrl Pts',(81.8719591200265,-1.71384756498248,
75.7859369317609));
#182815=CARTESIAN_POINT('Ctrl Pts',(81.8988209402735,-1.62084823720603,
75.783363797681));
#182816=CARTESIAN_POINT('Ctrl Pts',(81.9414678617161,-1.45874647804823,
75.7795189822176));
#182817=CARTESIAN_POINT('Ctrl Pts',(81.9582877020607,-1.38994087930884,
75.7780837356329));
#182818=CARTESIAN_POINT('Ctrl Pts',(81.9919918961584,-1.24079612489533,
75.7753965271836));
#182819=CARTESIAN_POINT('Ctrl Pts',(82.0084588570063,-1.16037622702758,
75.7742100949194));
#182820=CARTESIAN_POINT('Ctrl Pts',(82.0502944111701,-0.932667162109909,
75.7715953418392));
#182821=CARTESIAN_POINT('Ctrl Pts',(82.0718649456886,-0.784736073153573,
75.7707670718751));
#182822=CARTESIAN_POINT('Ctrl Pts',(82.1248190677507,-0.296004956785859,
75.7709825018011));
#182823=CARTESIAN_POINT('Ctrl Pts',(82.1328882059776,0.0466209745666767,
75.7757830109125));
#182824=CARTESIAN_POINT('Ctrl Pts',(82.1032487033638,0.536187394768259,
75.7903772288093));
#182825=CARTESIAN_POINT('Ctrl Pts',(82.0888706662041,0.683984223392767,
75.7958101691392));
#182826=CARTESIAN_POINT('Ctrl Pts',(82.0622311512114,0.882500704085245,
75.8046183533348));
#182827=CARTESIAN_POINT('Ctrl Pts',(82.054674676326,0.933839851342049,75.8070339409384));
#182828=CARTESIAN_POINT('Ctrl Pts',(82.0403903414168,1.02299497322353,75.8114760667689));
#182829=CARTESIAN_POINT('Ctrl Pts',(82.0339575547002,1.06085711266835,75.8134409606314));
#182830=CARTESIAN_POINT('Ctrl Pts',(82.0181600449413,1.14880983024054,75.8181884159474));
#182831=CARTESIAN_POINT('Ctrl Pts',(82.0085252681318,1.19884487504578,75.8210272401984));
#182832=CARTESIAN_POINT('Ctrl Pts',(81.9714478062439,1.37919586364177,75.8317477580379));
#182833=CARTESIAN_POINT('Ctrl Pts',(81.9403737538009,1.50868227430673,75.8403693110471));
#182834=CARTESIAN_POINT('Ctrl Pts',(81.8433187776311,1.86158388404592,75.8662781775486));
#182835=CARTESIAN_POINT('Ctrl Pts',(81.7687221410804,2.08226963852465,75.8851850182932));
#182836=CARTESIAN_POINT('Ctrl Pts',(81.6116193328735,2.47131842309215,75.9230950963684));
#182837=CARTESIAN_POINT('Ctrl Pts',(81.5336133417445,2.64124781514955,75.9413344553659));
#182838=CARTESIAN_POINT('Ctrl Pts',(81.394729232647,2.90996236340653,75.9728640143506));
#182839=CARTESIAN_POINT('Ctrl Pts',(81.3386481307373,3.01117114244377,75.9853929419478));
#182840=CARTESIAN_POINT('Ctrl Pts',(81.2414477063021,3.17518445276843,76.0067862102487));
#182841=CARTESIAN_POINT('Ctrl Pts',(81.2020008151637,3.23897707256013,76.0153902214272));
#182842=CARTESIAN_POINT('Ctrl Pts',(81.1200795984946,3.36604487126458,76.0331079746245));
#182843=CARTESIAN_POINT('Ctrl Pts',(81.0775737603586,3.42928237584866,76.0422261208518));
#182844=CARTESIAN_POINT('Ctrl Pts',(80.9626061256834,3.59344072359707,76.0667036341991));
#182845=CARTESIAN_POINT('Ctrl Pts',(80.8882011516666,3.69290889956414,76.0823626843461));
#182846=CARTESIAN_POINT('Ctrl Pts',(80.6130650129921,4.03768555344912,76.1397170584641));
#182847=CARTESIAN_POINT('Ctrl Pts',(80.3961140625166,4.26891458069115,76.1839440755937));
#182848=CARTESIAN_POINT('Ctrl Pts',(80.0436117577074,4.58900749139795,76.255380878693));
#182849=CARTESIAN_POINT('Ctrl Pts',(79.920897396206,4.69166634996503,76.280189675214));
#182850=CARTESIAN_POINT('Ctrl Pts',(79.7515027263841,4.82206715821595,76.3145137516457));
#182851=CARTESIAN_POINT('Ctrl Pts',(79.7082905702292,4.8543971396338,76.3232763498851));
#182852=CARTESIAN_POINT('Ctrl Pts',(79.6311903049683,4.91044715210589,76.3389310648733));
#182853=CARTESIAN_POINT('Ctrl Pts',(79.5974802293685,4.93441508779282,76.3457829725679));
#182854=CARTESIAN_POINT('Ctrl Pts',(79.5218274625517,4.98701329821702,76.361175204221));
#182855=CARTESIAN_POINT('Ctrl Pts',(79.4797651296251,5.01545681278895,76.3697426672664));
#182856=CARTESIAN_POINT('Ctrl Pts',(79.3002442708058,5.13349170842509,76.4063335220491));
#182857=CARTESIAN_POINT('Ctrl Pts',(79.1595328922465,5.21777990329696,76.4350738233895));
#182858=CARTESIAN_POINT('Ctrl Pts',(78.7944474871663,5.41611206244016,76.5095290878208));
#182859=CARTESIAN_POINT('Ctrl Pts',(78.5660108502608,5.52169887877698,76.5560039856362));
#182860=CARTESIAN_POINT('Ctrl Pts',(78.186723520633,5.66798482125429,76.6325975572483));
#182861=CARTESIAN_POINT('Ctrl Pts',(78.0397052596335,5.71800865899628,76.6621582554536));
#182862=CARTESIAN_POINT('Ctrl Pts',(77.8140839918658,5.78479494632151,76.7072965901127));
#182863=CARTESIAN_POINT('Ctrl Pts',(77.7368192802543,5.8059330580852,76.7227154060273));
#182864=CARTESIAN_POINT('Ctrl Pts',(77.5894755964486,5.84297486225297,76.7520450604194));
#182865=CARTESIAN_POINT('Ctrl Pts',(77.5194883824299,5.85919028039403,76.7659452401102));
#182866=CARTESIAN_POINT('Ctrl Pts',(77.3530083503173,5.89450921836859,76.7989390410556));
#182867=CARTESIAN_POINT('Ctrl Pts',(77.256297925221,5.91246240871852,76.8180495583339));
#182868=CARTESIAN_POINT('Ctrl Pts',(76.7884656538769,5.98702227382939,76.9102605580226));
#182869=CARTESIAN_POINT('Ctrl Pts',(76.4129196105907,6.00985752920379,76.9835054943814));
#182870=CARTESIAN_POINT('Ctrl Pts',(75.904700495134,5.99126318801624,77.0828782420069));
#182871=CARTESIAN_POINT('Ctrl Pts',(75.771767669737,5.98179104230586,77.1089021860041));
#182872=CARTESIAN_POINT('Ctrl Pts',(75.5509353441074,5.95836103982866,77.1522968390795));
#182873=CARTESIAN_POINT('Ctrl Pts',(75.4628157142397,5.94695194115564,77.1696566124335));
#182874=CARTESIAN_POINT('Ctrl Pts',(75.3318495589169,5.92691525344628,77.1955554370579));
#182875=CARTESIAN_POINT('Ctrl Pts',(75.2887800430601,5.91982575875605,77.2040884920697));
#182876=CARTESIAN_POINT('Ctrl Pts',(75.2078065139503,5.90555294357244,77.2201664611838));
#182877=CARTESIAN_POINT('Ctrl Pts',(75.169886550822,5.89847674541259,77.2277108500253));
#182878=CARTESIAN_POINT('Ctrl Pts',(75.0704421201887,5.8788872767805,77.2475319267741));
#182879=CARTESIAN_POINT('Ctrl Pts',(75.0090448498644,5.86574995822574,77.259805687597));
#182880=CARTESIAN_POINT('Ctrl Pts',(74.6882691700557,5.79162882224948,77.3240859886824));
#182881=CARTESIAN_POINT('Ctrl Pts',(74.4330489335526,5.71375314748594,77.3757491470365));
#182882=CARTESIAN_POINT('Ctrl Pts',(73.9108641123216,5.51416832098742,77.4816962347188));
#182883=CARTESIAN_POINT('Ctrl Pts',(73.6458310683007,5.3892457266918,77.5356035375481));
#182884=CARTESIAN_POINT('Ctrl Pts',(73.3072122383926,5.19732746331094,77.6043330533111));
#182885=CARTESIAN_POINT('Ctrl Pts',(73.2246214523536,5.14778774217879,77.6210869910811));
#182886=CARTESIAN_POINT('Ctrl Pts',(73.0825611618591,5.05774457682096,77.6498866465396));
#182887=CARTESIAN_POINT('Ctrl Pts',(73.0225620910214,5.01815203667619,77.6620444395812));
#182888=CARTESIAN_POINT('Ctrl Pts',(72.895983527477,4.93124852791776,77.6876837107054));
#182889=CARTESIAN_POINT('Ctrl Pts',(72.8296260867835,4.88362757161157,77.7011188406143));
#182890=CARTESIAN_POINT('Ctrl Pts',(72.6321153230523,4.73556285251598,77.7411011869603));
#182891=CARTESIAN_POINT('Ctrl Pts',(72.5040920182839,4.63091085363375,77.7670055485619));
#182892=CARTESIAN_POINT('Ctrl Pts',(72.3289838485916,4.47506284305219,77.8025008632107));
#182893=CARTESIAN_POINT('Ctrl Pts',(72.2782280441991,4.42827291545422,77.8127978397302));
#182894=CARTESIAN_POINT('Ctrl Pts',(72.0623293565463,4.22214170727489,77.8566603970351));
#182895=CARTESIAN_POINT('Ctrl Pts',(71.9055440613095,4.05401419205986,77.8886679947361));
#182896=CARTESIAN_POINT('Ctrl Pts',(71.7044004765138,3.81150794798109,77.9303447454054));
#182897=CARTESIAN_POINT('Ctrl Pts',(71.6514310915522,3.74477867114699,77.9413865579926));
#182898=CARTESIAN_POINT('Ctrl Pts',(71.5597852808818,3.62408567351391,77.9606436757048));
#182899=CARTESIAN_POINT('Ctrl Pts',(71.5205492818374,3.57057870151534,77.9689417561));
#182900=CARTESIAN_POINT('Ctrl Pts',(71.4578667079739,3.48202676119671,77.9823026922628));
#182901=CARTESIAN_POINT('Ctrl Pts',(71.4338879269392,3.44737718493032,77.9874403431168));
#182902=CARTESIAN_POINT('Ctrl Pts',(71.3816229694524,3.37011238400974,77.9987015054357));
#182903=CARTESIAN_POINT('Ctrl Pts',(71.3535125235248,3.32737971828664,78.0047998540314));
#182904=CARTESIAN_POINT('Ctrl Pts',(71.2662696451409,3.19096399125769,78.0238495217737));
#182905=CARTESIAN_POINT('Ctrl Pts',(71.2091762194463,3.09596283196378,78.036501483874));
#182906=CARTESIAN_POINT('Ctrl Pts',(71.0379664607983,2.79227821644302,78.0749481162468));
#182907=CARTESIAN_POINT('Ctrl Pts',(70.9335308783647,2.57820490389664,78.0991683841703));
#182908=CARTESIAN_POINT('Ctrl Pts',(70.757100608402,2.15462571188343,78.1412735040649));
#182909=CARTESIAN_POINT('Ctrl Pts',(70.6834171712819,1.94626824508627,78.1594618326851));
#182910=CARTESIAN_POINT('Ctrl Pts',(70.5965129130708,1.64997726713302,78.181759359022));
#182911=CARTESIAN_POINT('Ctrl Pts',(70.5736320346361,1.56520715477846,78.1877443021302));
#182912=CARTESIAN_POINT('Ctrl Pts',(70.5352767090858,1.40980413738651,78.1980000643091));
#182913=CARTESIAN_POINT('Ctrl Pts',(70.5192115349662,1.33934191401665,78.2023858682363));
#182914=CARTESIAN_POINT('Ctrl Pts',(70.4859425970943,1.18041816187274,78.211688558623));
#182915=CARTESIAN_POINT('Ctrl Pts',(70.4694380299398,1.09182034121506,78.2164687191469));
#182916=CARTESIAN_POINT('Ctrl Pts',(70.4208886899886,0.794745074487697,
78.2311615562803));
#182917=CARTESIAN_POINT('Ctrl Pts',(70.3976831131773,0.584901259477872,
78.2393541283082));
#182918=CARTESIAN_POINT('Ctrl Pts',(70.3694861764948,0.101162741297917,
78.2535234503463));
#182919=CARTESIAN_POINT('Ctrl Pts',(70.371951631181,-0.172730905845747,
78.2581045926711));
#182920=CARTESIAN_POINT('Ctrl Pts',(70.4030275290813,-0.578271616274934,
78.2604392843645));
#182921=CARTESIAN_POINT('Ctrl Pts',(70.4175532912998,-0.710622889317259,
78.2604933345498));
#182922=CARTESIAN_POINT('Ctrl Pts',(70.4435634754622,-0.892259226385203,
78.2596788716901));
#182923=CARTESIAN_POINT('Ctrl Pts',(70.4513262536437,-0.942040066818519,
78.259362969781));
#182924=CARTESIAN_POINT('Ctrl Pts',(70.466113725168,-1.02967383407506,78.2586497579256));
#182925=CARTESIAN_POINT('Ctrl Pts',(70.4728799543504,-1.06756670307819,
78.2582897173655));
#182926=CARTESIAN_POINT('Ctrl Pts',(70.48994323149,-1.15812897158568,78.2573049861004));
#182927=CARTESIAN_POINT('Ctrl Pts',(70.5005796137709,-1.21072984648261,
78.2566312819108));
#182928=CARTESIAN_POINT('Ctrl Pts',(70.5462490698922,-1.42209918843184,
78.2534972905141));
#182929=CARTESIAN_POINT('Ctrl Pts',(70.5869606291509,-1.57955875111542,
78.2501860690012));
#182930=CARTESIAN_POINT('Ctrl Pts',(70.7184668646324,-2.01525440478615,
78.2379951539103));
#182931=CARTESIAN_POINT('Ctrl Pts',(70.8230993559022,-2.28878080897071,
78.2267782649833));
#182932=CARTESIAN_POINT('Ctrl Pts',(71.0203438686532,-2.71054483735033,
78.203093985243));
#182933=CARTESIAN_POINT('Ctrl Pts',(71.1004191817987,-2.8642613652786,78.1930106878791));
#182934=CARTESIAN_POINT('Ctrl Pts',(71.2288745573352,-3.0870245578603,78.1761591723132));
#182935=CARTESIAN_POINT('Ctrl Pts',(71.272325092367,-3.1588813259545,78.170360548172));
#182936=CARTESIAN_POINT('Ctrl Pts',(71.3560277230687,-3.29101901361857,
78.1590136893739));
#182937=CARTESIAN_POINT('Ctrl Pts',(71.3958988942966,-3.35152926486004,
78.1535404459856));
#182938=CARTESIAN_POINT('Ctrl Pts',(71.4896724508966,-3.48842304696753,
78.1405195282612));
#182939=CARTESIAN_POINT('Ctrl Pts',(71.5442729109051,-3.56429186663778,
78.132832846811));
#182940=CARTESIAN_POINT('Ctrl Pts',(71.7906540096913,-3.89038865240792,
78.0977307529199));
#182941=CARTESIAN_POINT('Ctrl Pts',(71.9999369287116,-4.12637041442099,
78.0668325506397));
#182942=CARTESIAN_POINT('Ctrl Pts',(72.3796812003209,-4.49198116248029,
78.0099984305344));
#182943=CARTESIAN_POINT('Ctrl Pts',(72.5404353036647,-4.631011607848,77.9857555140472));
#182944=CARTESIAN_POINT('Ctrl Pts',(72.7564840271555,-4.79851050232391,
77.9532751212576));
#182945=CARTESIAN_POINT('Ctrl Pts',(72.8053421584588,-4.83519606355928,
77.9459365106532));
#182946=CARTESIAN_POINT('Ctrl Pts',(72.8884135976851,-4.89558659048793,
77.9334815957941));
#182947=CARTESIAN_POINT('Ctrl Pts',(72.9223284084198,-4.91969992549469,
77.9284033245493));
#182948=CARTESIAN_POINT('Ctrl Pts',(73.0002989528576,-4.97390937553228,
77.9167450209659));
#182949=CARTESIAN_POINT('Ctrl Pts',(73.0445097027769,-5.00376947507537,
77.9101454846803));
#182950=CARTESIAN_POINT('Ctrl Pts',(73.2103579530749,-5.1125521989381,77.8854141938693));
#182951=CARTESIAN_POINT('Ctrl Pts',(73.3344442080653,-5.18757649789067,
77.8669599165302));
#182952=CARTESIAN_POINT('Ctrl Pts',(73.6698945540302,-5.37394192361085,
77.8170121825215));
#182953=CARTESIAN_POINT('Ctrl Pts',(73.8853873666549,-5.47712857415794,
77.7848589719973));
#182954=CARTESIAN_POINT('Ctrl Pts',(74.2782576057679,-5.63680376075511,
77.7257310415124));
#182955=CARTESIAN_POINT('Ctrl Pts',(74.4532461325465,-5.69848676943401,
77.6992283193579));
#182956=CARTESIAN_POINT('Ctrl Pts',(74.711371125651,-5.77599892194807,77.6598294477604));
#182957=CARTESIAN_POINT('Ctrl Pts',(74.7924675727333,-5.79846782118944,
77.6474094354249));
#182958=CARTESIAN_POINT('Ctrl Pts',(74.9435712038005,-5.8368637282888,77.6241894887138));
#182959=CARTESIAN_POINT('Ctrl Pts',(75.0134466410989,-5.85326368132142,
77.6134212609044));
#182960=CARTESIAN_POINT('Ctrl Pts',(75.1728585393736,-5.88761072186219,
77.5887880308129));
#182961=CARTESIAN_POINT('Ctrl Pts',(75.2625420519347,-5.90475683466136,
77.5748820450661));
#182962=CARTESIAN_POINT('Ctrl Pts',(75.7325036040162,-5.9832933221517,77.5017899383352));
#182963=CARTESIAN_POINT('Ctrl Pts',(76.1175034016835,-6.00918872011661,
77.4410845524726));
#182964=CARTESIAN_POINT('Ctrl Pts',(76.6422572293234,-5.99273176795224,
77.3585511041752));
#182965=CARTESIAN_POINT('Ctrl Pts',(76.7820434835449,-5.98332275946202,
77.3365946589979));
#182966=CARTESIAN_POINT('Ctrl Pts',(77.0128440490101,-5.95945447064461,
77.3005139876206));
#182967=CARTESIAN_POINT('Ctrl Pts',(77.1040797843196,-5.94784500323426,
77.2862962950022));
#182968=CARTESIAN_POINT('Ctrl Pts',(77.2389014114205,-5.92745907971508,
77.2653882840629));
#182969=CARTESIAN_POINT('Ctrl Pts',(77.2827078619588,-5.92032636533896,
77.258610896689));
#182970=CARTESIAN_POINT('Ctrl Pts',(77.3337116152199,-5.91142730893575,
77.2507420206451));
#182971=CARTESIAN_POINT('Ctrl Pts',(77.3409869335096,-5.91014377924753,
77.2496201062063));
#182972=CARTESIAN_POINT('Ctrl Pts',(77.3482598983342,-5.90884651798042,
77.2484990919142));
#182973=CARTESIAN_POINT('Origin',(76.5149506510185,7.15881389286582E-15,
78.5225675105249));
#182974=CARTESIAN_POINT('',(80.6284101054663,-3.63675684748494,78.0903820385128));
#182975=CARTESIAN_POINT('',(77.5109869441485,-5.49094931682848,78.5957139706103));
#182976=CARTESIAN_POINT('Ctrl Pts',(77.5109869441485,-5.49094931682847,
78.5957139706103));
#182977=CARTESIAN_POINT('Ctrl Pts',(78.1896918683254,-5.35556772975862,
78.4841869022237));
#182978=CARTESIAN_POINT('Ctrl Pts',(78.7554088112724,-5.1055662767554,78.393188160418));
#182979=CARTESIAN_POINT('Ctrl Pts',(79.7377353752645,-4.52841761382738,
78.234158897099));
#182980=CARTESIAN_POINT('Ctrl Pts',(80.2236625868063,-4.11908110158411,
78.1550172499348));
#182981=CARTESIAN_POINT('Ctrl Pts',(80.6284101060512,-3.63675684793529,
78.0903820388149));
#182982=CARTESIAN_POINT('',(81.5941173588847,2.04265365340621,77.9201017942693));
#182983=CARTESIAN_POINT('Origin',(76.5650785620786,7.15881389286582E-15,
78.8068570211757));
#182984=CARTESIAN_POINT('Origin',(22.3114963328544,145.306839242356,89.0571204175862));
#182985=CARTESIAN_POINT('Ctrl Pts',(79.5631824082928,5.13997981405092,77.9850820082628));
#182986=CARTESIAN_POINT('Ctrl Pts',(79.144532880795,5.38518891260996,78.0646192810899));
#182987=CARTESIAN_POINT('Ctrl Pts',(78.6966575569264,5.57679262082688,78.1497307045318));
#182988=CARTESIAN_POINT('Ctrl Pts',(77.8259665816532,5.82815848696469,78.3136925708069));
#182989=CARTESIAN_POINT('Ctrl Pts',(77.4081857473062,5.90127337120631,78.3917886262775));
#182990=CARTESIAN_POINT('Ctrl Pts',(76.5284259338047,5.95799929590254,78.5555726318262));
#182991=CARTESIAN_POINT('Ctrl Pts',(75.8630971584906,5.94870954755889,78.6785004071637));
#182992=CARTESIAN_POINT('Ctrl Pts',(74.3473318554912,5.52279212407711,78.9648707259658));
#182993=CARTESIAN_POINT('Ctrl Pts',(73.6512982737334,5.16369081654802,79.097653170836));
#182994=CARTESIAN_POINT('Ctrl Pts',(72.5306476584885,4.26987919295954,79.3103869139622));
#182995=CARTESIAN_POINT('Ctrl Pts',(72.0833704466692,3.77061895417284,79.3950648833961));
#182996=CARTESIAN_POINT('Ctrl Pts',(71.3290937718838,2.54917482922943,79.5447002438745));
#182997=CARTESIAN_POINT('Ctrl Pts',(71.0583979266505,1.81538535021859,79.6026474139665));
#182998=CARTESIAN_POINT('Ctrl Pts',(70.8269162740687,0.386676405105633,
79.6589560215703));
#182999=CARTESIAN_POINT('Ctrl Pts',(70.8324701147635,-0.296931580282131,
79.6638068701898));
#183000=CARTESIAN_POINT('Ctrl Pts',(71.0981688558512,-1.70847266736971,
79.6329869040131));
#183001=CARTESIAN_POINT('Ctrl Pts',(71.3889392755114,-2.42207361322268,
79.5923592140419));
#183002=CARTESIAN_POINT('Ctrl Pts',(72.1805383634408,-3.63125885150102,
79.4694000462425));
#183003=CARTESIAN_POINT('Ctrl Pts',(72.6575318459149,-4.13689966793945,
79.3916265768121));
#183004=CARTESIAN_POINT('Ctrl Pts',(73.8589324237686,-5.01033879056241,
79.1962536241068));
#183005=CARTESIAN_POINT('Ctrl Pts',(74.554062491525,-5.29847388859498,79.0841805175807));
#183006=CARTESIAN_POINT('Ctrl Pts',(75.8658885405282,-5.60208752807489,
78.8686428509867));
#183007=CARTESIAN_POINT('Ctrl Pts',(76.5406155618653,-5.63487017566596,
78.7559603591494));
#183008=CARTESIAN_POINT('Ctrl Pts',(77.3072788239429,-5.52853753302272,
78.6292461832499));
#183009=CARTESIAN_POINT('Ctrl Pts',(77.4103761181366,-5.51101820511365,
78.6122466788217));
#183010=CARTESIAN_POINT('Ctrl Pts',(77.5109869441485,-5.49094931682847,
78.5957139706103));
#183011=CARTESIAN_POINT('',(77.5410110809953,-5.90884651807327,78.3416453728827));
#183012=CARTESIAN_POINT('Origin',(76.1212924379081,7.14546725904962E-15,
76.2900208433682));
#183013=CARTESIAN_POINT('',(76.9605608422114,-4.33315411413756,76.6497484855763));
#183014=CARTESIAN_POINT('',(75.4556722114252,4.33315411325374,76.9151009541453));
#183015=CARTESIAN_POINT('Origin',(76.2081165267415,7.14546725904962E-15,
76.7824247198743));
#183016=CARTESIAN_POINT('',(76.0634408332593,4.33315411325374,80.361928089688));
#183017=CARTESIAN_POINT('',(75.3688481225918,4.33315411325374,76.4226970776392));
#183018=CARTESIAN_POINT('Origin',(76.8158851485756,7.14546725904962E-15,
80.229251855417));
#183019=CARTESIAN_POINT('Origin',(76.2081165267415,7.14546725904962E-15,
76.7824247198743));
#183020=CARTESIAN_POINT('Origin',(76.8158851485756,7.19646783916074E-15,
80.229251855417));
#183021=CARTESIAN_POINT('',(79.2648504730746,-0.865626271753975,80.3051464998313));
#183022=CARTESIAN_POINT('',(77.3387849203051,-2.51125977018251,80.6447638243076));
#183023=CARTESIAN_POINT('Origin',(76.9027092374091,7.19646783916074E-15,
80.7216557319231));
#183024=CARTESIAN_POINT('',(79.2648504730747,0.865626271753664,80.3051464998313));
#183025=CARTESIAN_POINT('Origin',(76.9027092374091,7.19646783916074E-15,
80.7216557319231));
#183026=CARTESIAN_POINT('',(82.0432213157451,0.865626271753682,96.0620705480267));
#183027=CARTESIAN_POINT('',(80.6540358944099,0.865626271753672,88.183608523929));
#183028=CARTESIAN_POINT('',(79.2450043973393,2.51125977018097,96.5554716886163));
#183029=CARTESIAN_POINT('Origin',(79.6810800800795,7.19646783916074E-15,
96.4785797801185));
#183030=CARTESIAN_POINT('',(82.043221315745,-0.865626271753956,96.0620705480267));
#183031=CARTESIAN_POINT('Origin',(79.6810800800795,7.19646783916074E-15,
96.4785797801185));
#183032=CARTESIAN_POINT('',(80.6540358944098,-0.865626271753965,88.1836085239291));
#183033=CARTESIAN_POINT('Origin',(79.6810800800795,7.19646783916074E-15,
96.4785797801185));
#183034=CARTESIAN_POINT('Ctrl Pts',(82.043221315745,0.865626271753621,96.0620705480265));
#183035=CARTESIAN_POINT('Ctrl Pts',(82.0992182044097,0.72751926106728,96.057947244922));
#183036=CARTESIAN_POINT('Ctrl Pts',(82.1409660117247,0.58564103397652,96.0548556380306));
#183037=CARTESIAN_POINT('Ctrl Pts',(82.2309139993029,0.128835088516363,
96.048187545496));
#183038=CARTESIAN_POINT('Ctrl Pts',(82.2265395302818,-0.219618264988888,
96.0485181512139));
#183039=CARTESIAN_POINT('Ctrl Pts',(82.1191291777162,-0.657108269115395,
96.0564710052956));
#183040=CARTESIAN_POINT('Ctrl Pts',(82.0847823537726,-0.763122885228353,
96.0590102216189));
#183041=CARTESIAN_POINT('Ctrl Pts',(82.0432213157448,-0.865626271754031,
96.0620705480265));
#183042=CARTESIAN_POINT('',(79.246323450496,3.00366364624538,97.0629524103545));
#183043=CARTESIAN_POINT('',(79.2450043973393,2.51125977018115,96.5554716886164));
#183044=CARTESIAN_POINT('Origin',(79.767904168913,7.19646783916074E-15,
96.9709836566246));
#183045=CARTESIAN_POINT('Origin',(76.8158851485756,7.19646783916074E-15,
80.229251855417));
#183046=CARTESIAN_POINT('Ctrl Pts',(79.2648504732428,-0.865626271722663,
80.3051465007115));
#183047=CARTESIAN_POINT('Ctrl Pts',(79.3741062412579,-0.586356325647426,
80.2742536009109));
#183048=CARTESIAN_POINT('Ctrl Pts',(79.4277739616774,-0.283930880250993,
80.2591373622784));
#183049=CARTESIAN_POINT('Ctrl Pts',(79.4277739616774,-7.39557098644699E-30,
80.2591373622784));
#183050=CARTESIAN_POINT('Ctrl Pts',(79.4277739616774,0.283930880250773,
80.2591373622784));
#183051=CARTESIAN_POINT('Ctrl Pts',(79.3741062412579,0.58635632564696,80.2742536009109));
#183052=CARTESIAN_POINT('Ctrl Pts',(79.2648504732431,0.86562627172201,80.3051465007115));
#183053=CARTESIAN_POINT('',(77.3374658671472,-3.00366364668724,80.1372831021155));
#183054=CARTESIAN_POINT('',(77.3374658671472,-3.00366364668724,80.1372831021155));
#183055=CARTESIAN_POINT('Origin',(76.8158851485756,7.19646783916074E-15,
80.229251855417));
#183056=CARTESIAN_POINT('Origin',(76.1212924379081,7.15881389286582E-15,
76.2900208433682));
#183057=CARTESIAN_POINT('Origin',(76.1212924379081,7.15881389286582E-15,
76.2900208433682));
#183058=CARTESIAN_POINT('',(77.1196285163625,-5.58066418896375,76.2833680310246));
#183059=CARTESIAN_POINT('Ctrl Pts',(77.1196277140212,-5.58095582281337,
76.283067472893));
#183060=CARTESIAN_POINT('Ctrl Pts',(76.9928283292005,-5.59398387932902,
76.2953436706019));
#183061=CARTESIAN_POINT('Ctrl Pts',(76.8409545289557,-5.60874287494297,
76.3141618693424));
#183062=CARTESIAN_POINT('Ctrl Pts',(76.5747214953194,-5.61991440458212,
76.3473866361007));
#183063=CARTESIAN_POINT('Ctrl Pts',(76.4795857142021,-5.62178133713042,
76.359292303505));
#183064=CARTESIAN_POINT('Ctrl Pts',(76.3528445946748,-5.6205988089503,76.3751832134439));
#183065=CARTESIAN_POINT('Ctrl Pts',(76.331876307243,-5.62025437321422,76.3778119200945));
#183066=CARTESIAN_POINT('Ctrl Pts',(76.2865965392702,-5.61926007964262,
76.3834857866538));
#183067=CARTESIAN_POINT('Ctrl Pts',(76.2191382964961,-5.61735584476887,
76.3919355893989));
#183068=CARTESIAN_POINT('Ctrl Pts',(76.1530768483827,-5.61426740474037,
76.4002001849428));
#183069=CARTESIAN_POINT('Ctrl Pts',(75.7623791796731,-5.59141776986316,
76.4490321459133));
#183070=CARTESIAN_POINT('Ctrl Pts',(75.455903832143,-5.54095283542196,76.4869797101295));
#183071=CARTESIAN_POINT('Ctrl Pts',(74.9267679368036,-5.41933799813517,
76.5515711076113));
#183072=CARTESIAN_POINT('Ctrl Pts',(74.7038794990428,-5.34810738982767,
76.5782551240242));
#183073=CARTESIAN_POINT('Ctrl Pts',(74.3361966660066,-5.21233203848455,
76.62132814975));
#183074=CARTESIAN_POINT('Ctrl Pts',(74.1912453772525,-5.14773003290795,
76.6377448236165));
#183075=CARTESIAN_POINT('Ctrl Pts',(74.0817004664548,-5.09516704230596,
76.6496559375717));
#183076=CARTESIAN_POINT('Ctrl Pts',(81.8428871744966,-1.80615450764722,
75.7888626250267));
#183077=CARTESIAN_POINT('Ctrl Pts',(81.7921281915313,-1.9400359292157,75.7901202345789));
#183078=CARTESIAN_POINT('Ctrl Pts',(81.736482277759,-2.07298945865901,75.7923157524007));
#183079=CARTESIAN_POINT('Ctrl Pts',(81.6758444736533,-2.20457874696473,
75.7954174203319));
#183080=CARTESIAN_POINT('Ctrl Pts',(81.6158044677516,-2.33487076137691,
75.7984885104488));
#183081=CARTESIAN_POINT('Ctrl Pts',(81.5508702154952,-2.46382504862596,
75.8024480243678));
#183082=CARTESIAN_POINT('Ctrl Pts',(81.4809800071083,-2.59098807599447,
75.8072580498469));
#183083=CARTESIAN_POINT('Ctrl Pts',(81.4121175334748,-2.71628117243014,
75.8119973439537));
#183084=CARTESIAN_POINT('Ctrl Pts',(81.3384435597397,-2.83983499752331,
75.8175623600099));
#183085=CARTESIAN_POINT('Ctrl Pts',(81.2599420646749,-2.96119065762395,
75.8239092506691));
#183086=CARTESIAN_POINT('Ctrl Pts',(81.2088340415657,-3.04019868002837,
75.8280413634933));
#183087=CARTESIAN_POINT('Ctrl Pts',(81.1556807075916,-3.11827448547332,
75.8325047261173));
#183088=CARTESIAN_POINT('Ctrl Pts',(81.1004883555888,-3.19528657070903,
75.8372853496264));
#183089=CARTESIAN_POINT('Ctrl Pts',(81.0027104922194,-3.33171991472714,
75.8457546236349));
#183090=CARTESIAN_POINT('Ctrl Pts',(80.8983883938494,-3.46483276372604,
75.8551462426669));
#183091=CARTESIAN_POINT('Ctrl Pts',(80.7877291090633,-3.59398652754898,
75.8655119707144));
#183092=CARTESIAN_POINT('Ctrl Pts',(80.677602856128,-3.72251817394275,75.8758277683542));
#183093=CARTESIAN_POINT('Ctrl Pts',(80.5612002832816,-3.84712861067232,
75.8871083198699));
#183094=CARTESIAN_POINT('Ctrl Pts',(80.4387761426652,-3.96719064408858,
75.899395708375));
#183095=CARTESIAN_POINT('Ctrl Pts',(80.3172662063421,-4.08635611228608,
75.9115913406033));
#183096=CARTESIAN_POINT('Ctrl Pts',(80.1898242819621,-4.20104068895251,
75.9247788317873));
#183097=CARTESIAN_POINT('Ctrl Pts',(80.0567498702629,-4.31063582828496,
75.9389904400899));
#183098=CARTESIAN_POINT('Ctrl Pts',(80.0274847959161,-4.33473745578535,
75.9421157875421));
#183099=CARTESIAN_POINT('Ctrl Pts',(79.9979475148131,-4.3585929681685,75.9452906295833));
#183100=CARTESIAN_POINT('Ctrl Pts',(79.9681415442571,-4.38219593621601,
75.9485152507764));
#183101=CARTESIAN_POINT('Ctrl Pts',(79.8517313649804,-4.47437967291755,
75.9611093292171));
#183102=CARTESIAN_POINT('Ctrl Pts',(79.7312463819954,-4.56269272089981,
75.9744637622036));
#183103=CARTESIAN_POINT('Ctrl Pts',(79.6069578462149,-4.64669689424489,
75.9885545936021));
#183104=CARTESIAN_POINT('Ctrl Pts',(79.4968333490383,-4.7211278728727,76.0010396205825));
#183105=CARTESIAN_POINT('Ctrl Pts',(79.3837235417294,-4.79217618243141,
76.0141026401752));
#183106=CARTESIAN_POINT('Ctrl Pts',(79.2678476526638,-4.85955146850915,
76.0277216023301));
#183107=CARTESIAN_POINT('Ctrl Pts',(79.1445198768333,-4.93125960593888,
76.0422163891682));
#183108=CARTESIAN_POINT('Ctrl Pts',(79.0180581340044,-4.99880154775553,
76.0573371091365));
#183109=CARTESIAN_POINT('Ctrl Pts',(78.8887553248201,-5.06182011558757,
76.0730252949464));
#183110=CARTESIAN_POINT('Ctrl Pts',(78.824103920228,-5.09332939950359,76.0808693878514));
#183111=CARTESIAN_POINT('Ctrl Pts',(78.7587427054292,-5.12370793042999,
76.0888549612484));
#183112=CARTESIAN_POINT('Ctrl Pts',(78.692710765976,-5.15291179036842,76.0969723772704));
#183113=CARTESIAN_POINT('Ctrl Pts',(78.6759572861809,-5.16032133007703,
76.0990319103757));
#183114=CARTESIAN_POINT('Ctrl Pts',(78.6574625598256,-5.16840084401436,
76.1013076781226));
#183115=CARTESIAN_POINT('Ctrl Pts',(78.6383605611387,-5.17660867914664,
76.1036565734103));
#183116=CARTESIAN_POINT('Ctrl Pts',(78.6198183797459,-5.18457596939512,
76.1059366302364));
#183117=CARTESIAN_POINT('Ctrl Pts',(78.6007039910472,-5.19266389923966,
76.1082855925168));
#183118=CARTESIAN_POINT('Ctrl Pts',(78.5820713772747,-5.20042139045395,
76.1105696052704));
#183119=CARTESIAN_POINT('Ctrl Pts',(78.5442436021413,-5.21617058360719,
76.1152065886747));
#183120=CARTESIAN_POINT('Ctrl Pts',(78.5068893167332,-5.23121722635507,
76.1197706818044));
#183121=CARTESIAN_POINT('Ctrl Pts',(78.4700318597412,-5.24559853331115,
76.1242565665862));
#183122=CARTESIAN_POINT('Ctrl Pts',(78.3883262999547,-5.27747899472131,
76.1342008697788));
#183123=CARTESIAN_POINT('Ctrl Pts',(78.3090658667927,-5.30608739681267,
76.1437570191419));
#183124=CARTESIAN_POINT('Ctrl Pts',(78.2324656107456,-5.33182355776652,
76.1528794079931));
#183125=CARTESIAN_POINT('Ctrl Pts',(78.1547737950188,-5.3579264610403,76.1621317916037));
#183126=CARTESIAN_POINT('Ctrl Pts',(78.0798181702974,-5.38107504391943,
76.1709380246403));
#183127=CARTESIAN_POINT('Ctrl Pts',(78.0077749223473,-5.40166281994532,
76.1792590199731));
#183128=CARTESIAN_POINT('Ctrl Pts',(77.9342932975165,-5.42266164047438,
76.1877461478395));
#183129=CARTESIAN_POINT('Ctrl Pts',(77.8638411785452,-5.44099673380601,
76.1957285260235));
#183130=CARTESIAN_POINT('Ctrl Pts',(77.7965607960489,-5.45705568395242,
76.2031725645302));
#183131=CARTESIAN_POINT('Ctrl Pts',(77.7601365449749,-5.46574967780942,
76.2072026178312));
#183132=CARTESIAN_POINT('Ctrl Pts',(77.724641169074,-5.4737760041616,76.2110750177584));
#183133=CARTESIAN_POINT('Ctrl Pts',(77.6900924558518,-5.48119208907128,
76.2147852774337));
#183134=CARTESIAN_POINT('Ctrl Pts',(77.6622650361554,-5.487165408713,76.2177737231249));
#183135=CARTESIAN_POINT('Ctrl Pts',(77.6350517701762,-5.49274348408649,
76.220657656134));
#183136=CARTESIAN_POINT('Ctrl Pts',(77.608460664494,-5.49795545559569,76.2234355226819));
#183137=CARTESIAN_POINT('Ctrl Pts',(77.5951651116529,-5.50056144135029,
76.2248244559558));
#183138=CARTESIAN_POINT('Ctrl Pts',(77.5820250984651,-5.5030758890797,76.2261868850227));
#183139=CARTESIAN_POINT('Ctrl Pts',(77.5690415015584,-5.5055023205584,76.2275226353722));
#183140=CARTESIAN_POINT('Ctrl Pts',(77.5625497031051,-5.50671553629776,
76.2281905105469));
#183141=CARTESIAN_POINT('Ctrl Pts',(77.5560970086979,-5.50790674721655,
76.2288517168236));
#183142=CARTESIAN_POINT('Ctrl Pts',(77.5496835246463,-5.50907638729464,
76.2295062352176));
#183143=CARTESIAN_POINT('Ctrl Pts',(77.5432700405948,-5.51024602737273,
76.2301607536115));
#183144=CARTESIAN_POINT('Ctrl Pts',(77.5413605897286,-5.51058776576927,
76.2303549106995));
#183145=CARTESIAN_POINT('Ctrl Pts',(77.5385278758308,-5.51110395017645,
76.2306491841668));
#183146=CARTESIAN_POINT('Ctrl Pts',(77.5225317368859,-5.51401880772868,
76.2323109260301));
#183147=CARTESIAN_POINT('Ctrl Pts',(77.502582434596,-5.51771225018848,76.2345019296031));
#183148=CARTESIAN_POINT('Ctrl Pts',(77.478663446348,-5.52205119172725,76.2372223822825));
#183149=CARTESIAN_POINT('Ctrl Pts',(77.4686964321468,-5.52385922355061,
76.2383559917064));
#183150=CARTESIAN_POINT('Ctrl Pts',(77.4580400637286,-5.52577871842334,
76.2395815452476));
#183151=CARTESIAN_POINT('Ctrl Pts',(77.4466929185927,-5.52779738571318,
76.2408990964935));
#183152=CARTESIAN_POINT('Ctrl Pts',(77.4194074079591,-5.53265150251016,
76.244067299429));
#183153=CARTESIAN_POINT('Ctrl Pts',(77.3881218669215,-5.53808546284043,
76.2477697163581));
#183154=CARTESIAN_POINT('Ctrl Pts',(77.3528552281582,-5.54401610952996,
76.252128643664));
#183155=CARTESIAN_POINT('Ctrl Pts',(77.3176159848871,-5.54994214923138,
76.2564841849097));
#183156=CARTESIAN_POINT('Ctrl Pts',(77.2784018478733,-5.55636409410674,
76.2614952132098));
#183157=CARTESIAN_POINT('Ctrl Pts',(77.2352213445396,-5.56314807052285,
76.2672855671192));
#183158=CARTESIAN_POINT('Ctrl Pts',(77.1994176836357,-5.56877309043764,
76.2720867123556));
#183159=CARTESIAN_POINT('Ctrl Pts',(77.1608868982291,-5.5746461130262,76.2774236884735));
#183160=CARTESIAN_POINT('Ctrl Pts',(77.1196285163624,-5.58066418896375,
76.2833680310246));
#183161=CARTESIAN_POINT('Ctrl Pts',(79.8067669157806,-4.75889434936128,
76.1478855624836));
#183162=CARTESIAN_POINT('Ctrl Pts',(79.4656552079978,-5.01633075955975,
76.2018288074578));
#183163=CARTESIAN_POINT('Ctrl Pts',(79.0981355517893,-5.2365440434876,76.2609701371046));
#183164=CARTESIAN_POINT('Ctrl Pts',(78.3757278221193,-5.56975423607527,
76.3785120140568));
#183165=CARTESIAN_POINT('Ctrl Pts',(78.0265892492644,-5.6926809850576,76.435791673461));
#183166=CARTESIAN_POINT('Ctrl Pts',(76.8543141967377,-5.98292457650376,
76.6272413549088));
#183167=CARTESIAN_POINT('Ctrl Pts',(76.0974424409179,-5.98222296632208,
76.7478529844076));
#183168=CARTESIAN_POINT('Ctrl Pts',(74.6929136633325,-5.77853241831115,
76.9740755107651));
#183169=CARTESIAN_POINT('Ctrl Pts',(73.9580143194339,-5.51877391939185,
77.0943934768112));
#183170=CARTESIAN_POINT('Ctrl Pts',(72.5747907323043,-4.69148727568362,
77.3177645343406));
#183171=CARTESIAN_POINT('Ctrl Pts',(72.0363102921168,-4.15598183372999,
77.4001313101903));
#183172=CARTESIAN_POINT('Ctrl Pts',(71.1810125590293,-3.02645959146061,
77.5298563962522));
#183173=CARTESIAN_POINT('Ctrl Pts',(70.83788218017,-2.32584157011803,77.5812538303274));
#183174=CARTESIAN_POINT('Ctrl Pts',(70.4329407787015,-0.802505729524864,
77.6328633583142));
#183175=CARTESIAN_POINT('Ctrl Pts',(70.4190230992651,-0.110255556371649,
77.6238715966117));
#183176=CARTESIAN_POINT('Ctrl Pts',(70.5275290426684,1.16543508448252,77.584711597924));
#183177=CARTESIAN_POINT('Ctrl Pts',(70.7286009034737,1.88783880921538,77.5393814133449));
#183178=CARTESIAN_POINT('Ctrl Pts',(71.3304192343141,3.10035853351918,77.4161289475591));
#183179=CARTESIAN_POINT('Ctrl Pts',(71.6869328784452,3.59894115111939,77.3445010729964));
#183180=CARTESIAN_POINT('Ctrl Pts',(72.5636028466731,4.48202484744894,77.1700775369511));
#183181=CARTESIAN_POINT('Ctrl Pts',(73.0815743965425,4.85387547286764,77.0691439922034));
#183182=CARTESIAN_POINT('Ctrl Pts',(74.0850504198822,5.34589610631609,76.8774557325446));
#183183=CARTESIAN_POINT('Ctrl Pts',(74.5994115705933,5.52772264370202,76.7805366540467));
#183184=CARTESIAN_POINT('Ctrl Pts',(75.1812918055743,5.62353578632127,76.6693002371056));
#183185=CARTESIAN_POINT('Origin',(76.1212924379081,7.14546725904962E-15,
76.2900208433682));
#183186=CARTESIAN_POINT('',(76.9592417890559,-4.82555798975984,76.1422677642937));
#183187=CARTESIAN_POINT('',(76.9592417890559,-4.82555798975984,76.1422677642937));
#183188=CARTESIAN_POINT('Origin',(76.1212924379081,7.14546725904962E-15,
76.2900208433682));
#183189=CARTESIAN_POINT('Origin',(76.0518331668413,7.15881389286582E-15,
75.8960977421633));
#183190=CARTESIAN_POINT('Ctrl Pts',(75.5161728246847,5.41644264198492,78.358216968557));
#183191=CARTESIAN_POINT('Ctrl Pts',(75.5019149418088,5.41387915560342,78.3610789631734));
#183192=CARTESIAN_POINT('Ctrl Pts',(75.4876667227446,5.41125711006823,78.3639371859045));
#183193=CARTESIAN_POINT('Ctrl Pts',(75.4255327841992,5.39955948906885,78.3763939104315));
#183194=CARTESIAN_POINT('Ctrl Pts',(75.3777553338061,5.38988133650626,78.3859530367993));
#183195=CARTESIAN_POINT('Ctrl Pts',(75.2023141057831,5.35181947554724,78.4209996640597));
#183196=CARTESIAN_POINT('Ctrl Pts',(75.0755278459142,5.31936972243571,78.4462199050885));
#183197=CARTESIAN_POINT('Ctrl Pts',(74.6674556431858,5.19871369377775,78.5273043409168));
#183198=CARTESIAN_POINT('Ctrl Pts',(74.3920524632714,5.09175193265122,78.5819143797841));
#183199=CARTESIAN_POINT('Ctrl Pts',(73.9919408034663,4.89679158174202,78.6620851728623));
#183200=CARTESIAN_POINT('Ctrl Pts',(73.8599693046185,4.82546805467803,78.6886699615825));
#183201=CARTESIAN_POINT('Ctrl Pts',(73.6629669240141,4.70803963466444,78.7286451726162));
#183202=CARTESIAN_POINT('Ctrl Pts',(73.5957227552475,4.66590460711774,78.7423440581148));
#183203=CARTESIAN_POINT('Ctrl Pts',(73.4687887813162,4.58238632244558,78.7683135508873));
#183204=CARTESIAN_POINT('Ctrl Pts',(73.4089578080457,4.54125565481166,78.780603409025));
#183205=CARTESIAN_POINT('Ctrl Pts',(73.2654826725282,4.43827687708175,78.8101969773947));
#183206=CARTESIAN_POINT('Ctrl Pts',(73.1827468240741,4.37517614643283,78.8273672647575));
#183207=CARTESIAN_POINT('Ctrl Pts',(73.0495032370545,4.26730323720836,78.8551891400921));
#183208=CARTESIAN_POINT('Ctrl Pts',(72.9979344986233,4.22392769921173,78.8660009081038));
#183209=CARTESIAN_POINT('Ctrl Pts',(72.7827710205176,4.03595398318632,78.9112892023277));
#183210=CARTESIAN_POINT('Ctrl Pts',(72.627068258779,3.8823362887325,78.9445183303616));
#183211=CARTESIAN_POINT('Ctrl Pts',(72.3674197499554,3.59322919644399,79.0004698999691));
#183212=CARTESIAN_POINT('Ctrl Pts',(72.2598282531279,3.4615325016442,79.0238463367233));
#183213=CARTESIAN_POINT('Ctrl Pts',(72.126388683757,3.28171624248632,79.0529321788238));
#183214=CARTESIAN_POINT('Ctrl Pts',(72.0949627144026,3.2380401493282,79.0597893570272));
#183215=CARTESIAN_POINT('Ctrl Pts',(72.0404809863824,3.15992587534142,79.0716818753935));
#183216=CARTESIAN_POINT('Ctrl Pts',(72.0171680308165,3.12568260712866,79.0767715519963));
#183217=CARTESIAN_POINT('Ctrl Pts',(71.9593347984207,3.03863717839425,79.089402433447));
#183218=CARTESIAN_POINT('Ctrl Pts',(71.9253246649039,2.9854892560426,79.0968358170441));
#183219=CARTESIAN_POINT('Ctrl Pts',(71.8500401207917,2.86326329726773,79.1133239695357));
#183220=CARTESIAN_POINT('Ctrl Pts',(71.8093429626874,2.79383145203852,79.1222618700749));
#183221=CARTESIAN_POINT('Ctrl Pts',(71.6654843506123,2.53559462668064,79.1540154782844));
#183222=CARTESIAN_POINT('Ctrl Pts',(71.5717832067193,2.34152844530379,79.1750271418635));
#183223=CARTESIAN_POINT('Ctrl Pts',(71.4159783056354,1.96386996730712,79.2111860569441));
#183224=CARTESIAN_POINT('Ctrl Pts',(71.3517094868113,1.78156216556626,79.2266902222285));
#183225=CARTESIAN_POINT('Ctrl Pts',(71.272853425363,1.51393382236065,79.2468650840652));
#183226=CARTESIAN_POINT('Ctrl Pts',(71.2505335000483,1.43114006228905,79.2527590812826));
#183227=CARTESIAN_POINT('Ctrl Pts',(71.212916840445,1.27749925141115,79.2630706292337));
#183228=CARTESIAN_POINT('Ctrl Pts',(71.197071431527,1.20681212166726,79.2675741632235));
#183229=CARTESIAN_POINT('Ctrl Pts',(71.1638143965143,1.04352771391044,79.2774301779147));
#183230=CARTESIAN_POINT('Ctrl Pts',(71.1473653971733,0.950748675231593,
79.282630338281));
#183231=CARTESIAN_POINT('Ctrl Pts',(71.0987046297217,0.628832684220777,
79.2992969798653));
#183232=CARTESIAN_POINT('Ctrl Pts',(71.0784338737235,0.398042190567016,
79.3088657223877));
#183233=CARTESIAN_POINT('Ctrl Pts',(71.0650214629203,-0.13113768080772,
79.3251419784573));
#183234=CARTESIAN_POINT('Ctrl Pts',(71.0813306320572,-0.429099154274402,
79.3302279709137));
#183235=CARTESIAN_POINT('Ctrl Pts',(71.1286500525202,-0.779286089998552,
79.3306584459885));
#183236=CARTESIAN_POINT('Ctrl Pts',(71.1368848392822,-0.834095414260751,
79.3305615796118));
#183237=CARTESIAN_POINT('Ctrl Pts',(71.1522371201957,-0.926906342177754,
79.3301095991703));
#183238=CARTESIAN_POINT('Ctrl Pts',(71.1589381318611,-0.964972346206565,
79.3298411076599));
#183239=CARTESIAN_POINT('Ctrl Pts',(71.1753298565719,-1.05277088847189,
79.3290287122979));
#183240=CARTESIAN_POINT('Ctrl Pts',(71.1853014783743,-1.1024457498079,79.3284261440093));
#183241=CARTESIAN_POINT('Ctrl Pts',(71.2261589107154,-1.29259243577014,
79.3255871590964));
#183242=CARTESIAN_POINT('Ctrl Pts',(71.2617679606139,-1.43197521063083,
79.3223860395607));
#183243=CARTESIAN_POINT('Ctrl Pts',(71.4090577741653,-1.92785125636295,
79.3072806067895));
#183244=CARTESIAN_POINT('Ctrl Pts',(71.5510006743666,-2.27410091233366,
79.2897519371849));
#183245=CARTESIAN_POINT('Ctrl Pts',(71.7754390299161,-2.69487242563776,
79.2606492921813));
#183246=CARTESIAN_POINT('Ctrl Pts',(71.826896158828,-2.78512661122168,79.2539029608224));
#183247=CARTESIAN_POINT('Ctrl Pts',(71.9189679329408,-2.93653286876974,
79.2417296143842));
#183248=CARTESIAN_POINT('Ctrl Pts',(71.9583209799575,-2.99843401826528,
79.2364978787745));
#183249=CARTESIAN_POINT('Ctrl Pts',(72.0434992184156,-3.12669664354118,
79.2251191556414));
#183250=CARTESIAN_POINT('Ctrl Pts',(72.0895680780906,-3.19287197127436,
79.2189343525147));
#183251=CARTESIAN_POINT('Ctrl Pts',(72.2304430038765,-3.38605207521559,
79.199933250951));
#183252=CARTESIAN_POINT('Ctrl Pts',(72.3292654508852,-3.50996138898529,
79.1864945487062));
#183253=CARTESIAN_POINT('Ctrl Pts',(72.6168449375001,-3.84023719191283,
79.1470199875352));
#183254=CARTESIAN_POINT('Ctrl Pts',(72.8161068343242,-4.03660894689595,
79.1192919068448));
#183255=CARTESIAN_POINT('Ctrl Pts',(73.1094564606271,-4.28461633682236,
79.0774156999498));
#183256=CARTESIAN_POINT('Ctrl Pts',(73.1916002571427,-4.3501070553025,79.0655847117028));
#183257=CARTESIAN_POINT('Ctrl Pts',(73.3137340347841,-4.44186336852166,
79.0477974946372));
#183258=CARTESIAN_POINT('Ctrl Pts',(73.3522957056441,-4.47005161992967,
79.0421540435315));
#183259=CARTESIAN_POINT('Ctrl Pts',(73.4271308736361,-4.52326632580226,
79.031143255864));
#183260=CARTESIAN_POINT('Ctrl Pts',(73.4633484032115,-4.5483667910836,79.0257881593876));
#183261=CARTESIAN_POINT('Ctrl Pts',(73.566677842625,-4.61814369924548,79.0104447268446));
#183262=CARTESIAN_POINT('Ctrl Pts',(73.6344655101185,-4.66176507802685,
79.0003025959736));
#183263=CARTESIAN_POINT('Ctrl Pts',(73.9024839516428,-4.82594167559996,
78.9599816255767));
#183264=CARTESIAN_POINT('Ctrl Pts',(74.1092700384102,-4.93495932705819,
78.9284116951794));
#183265=CARTESIAN_POINT('Ctrl Pts',(74.5219033964116,-5.11948179653936,
78.8652810353659));
#183266=CARTESIAN_POINT('Ctrl Pts',(74.7266043825922,-5.1964998340706,78.8339045344074));
#183267=CARTESIAN_POINT('Ctrl Pts',(75.0174649885859,-5.28619211479614,
78.7895055849814));
#183268=CARTESIAN_POINT('Ctrl Pts',(75.1001675666155,-5.3095446850927,78.7768999599303));
#183269=CARTESIAN_POINT('Ctrl Pts',(75.2528642273895,-5.34874328073306,
78.7536706468873));
#183270=CARTESIAN_POINT('Ctrl Pts',(75.3226869820234,-5.36518820000155,
78.7430656007244));
#183271=CARTESIAN_POINT('Ctrl Pts',(75.4828898687353,-5.39955722672238,
78.7187754382765));
#183272=CARTESIAN_POINT('Ctrl Pts',(75.5734412371254,-5.41656560554987,
78.705076482505));
#183273=CARTESIAN_POINT('Ctrl Pts',(75.7677510392994,-5.44792394359072,
78.6757449020032));
#183274=CARTESIAN_POINT('Ctrl Pts',(75.8715819611401,-5.46158604813196,
78.6601102245746));
#183275=CARTESIAN_POINT('Ctrl Pts',(76.1955068481785,-5.49462859427088,
78.6114320409621));
#183276=CARTESIAN_POINT('Ctrl Pts',(76.4164408094107,-5.50349609385866,
78.5783790890833));
#183277=CARTESIAN_POINT('Ctrl Pts',(76.8264814201847,-5.49471278816749,
78.5169938339591));
#183278=CARTESIAN_POINT('Ctrl Pts',(77.0153368711548,-5.48068641639614,
78.4887018730051));
#183279=CARTESIAN_POINT('Ctrl Pts',(77.2631393744103,-5.44907856650256,
78.4513197607304));
#183280=CARTESIAN_POINT('Ctrl Pts',(77.3230922441702,-5.44040040345994,
78.4422549071447));
#183281=CARTESIAN_POINT('Ctrl Pts',(77.4211723865814,-5.42450795093904,
78.4273798256251));
#183282=CARTESIAN_POINT('Ctrl Pts',(77.459391273806,-5.41789022187502,78.4215718442162));
#183283=CARTESIAN_POINT('Ctrl Pts',(77.5433125088904,-5.40242226517557,
78.4087904923963));
#183284=CARTESIAN_POINT('Ctrl Pts',(77.5889775534055,-5.39339114855114,
78.4018180259825));
#183285=CARTESIAN_POINT('Ctrl Pts',(77.7415687203998,-5.36115028822013,
78.3784729769647));
#183286=CARTESIAN_POINT('Ctrl Pts',(77.8479066865757,-5.33527112735,78.362127963739));
#183287=CARTESIAN_POINT('Ctrl Pts',(78.1430861425216,-5.25383017668497,
78.3166717234678));
#183288=CARTESIAN_POINT('Ctrl Pts',(78.3298148192446,-5.19112432475122,
78.2878219349732));
#183289=CARTESIAN_POINT('Ctrl Pts',(78.7276144333097,-5.03285944303159,
78.226638195943));
#183290=CARTESIAN_POINT('Ctrl Pts',(78.9368612656805,-4.9336454417792,78.1946390778234));
#183291=CARTESIAN_POINT('Ctrl Pts',(79.2233659394255,-4.77463192830892,
78.1514113034689));
#183292=CARTESIAN_POINT('Ctrl Pts',(79.3062001766343,-4.72574070304795,
78.138985175048));
#183293=CARTESIAN_POINT('Ctrl Pts',(79.4489054552507,-4.63633164728317,
78.1177189040025));
#183294=CARTESIAN_POINT('Ctrl Pts',(79.5093338267788,-4.59677817372079,
78.1087597913681));
#183295=CARTESIAN_POINT('Ctrl Pts',(79.6380270678341,-4.50884314507245,
78.0897833287989));
#183296=CARTESIAN_POINT('Ctrl Pts',(79.7060070644152,-4.46006503839995,
78.0798246067159));
#183297=CARTESIAN_POINT('Ctrl Pts',(79.9261175419339,-4.29434283709644,
78.0477958785182));
#183298=CARTESIAN_POINT('Ctrl Pts',(80.0733094384252,-4.17088753725781,
78.0267340503367));
#183299=CARTESIAN_POINT('Ctrl Pts',(80.4435224762492,-3.82569632497984,
77.9745685540693));
#183300=CARTESIAN_POINT('Ctrl Pts',(80.6546844161734,-3.59195896072616,
77.9456958990509));
#183301=CARTESIAN_POINT('Ctrl Pts',(80.8763084599508,-3.29977353857334,
77.9157044089384));
#183302=CARTESIAN_POINT('Ctrl Pts',(80.9071830097525,-3.2578466048847,77.9115334181342));
#183303=CARTESIAN_POINT('Ctrl Pts',(80.9618405150334,-3.18137248074178,
77.9041549939482));
#183304=CARTESIAN_POINT('Ctrl Pts',(80.9858308882512,-3.1469821006614,77.9009179604996));
#183305=CARTESIAN_POINT('Ctrl Pts',(81.0409034323538,-3.0660800580017,77.8934894978799));
#183306=CARTESIAN_POINT('Ctrl Pts',(81.0716756915484,-3.01936048596812,
77.889342011522));
#183307=CARTESIAN_POINT('Ctrl Pts',(81.1380644623453,-2.91514807754056,
77.8804152753713));
#183308=CARTESIAN_POINT('Ctrl Pts',(81.1733472509728,-2.85744933248507,
77.8756854361699));
#183309=CARTESIAN_POINT('Ctrl Pts',(81.282563414097,-2.67124958080769,77.8611250684101));
#183310=CARTESIAN_POINT('Ctrl Pts',(81.3524121887182,-2.5403807460344,77.8519394815153));
#183311=CARTESIAN_POINT('Ctrl Pts',(81.536092933521,-2.16031416155188,77.8284470977737));
#183312=CARTESIAN_POINT('Ctrl Pts',(81.6369084892845,-1.90518109225111,
77.8164300331646));
#183313=CARTESIAN_POINT('Ctrl Pts',(81.7459537131316,-1.55609387454003,
77.8053525438637));
#183314=CARTESIAN_POINT('Ctrl Pts',(81.771123771013,-1.46795901744542,77.8029916390186));
#183315=CARTESIAN_POINT('Ctrl Pts',(81.8122918970464,-1.30912810093927,
77.7995243082641));
#183316=CARTESIAN_POINT('Ctrl Pts',(81.8291022640084,-1.23866852137733,
77.7982588784447));
#183317=CARTESIAN_POINT('Ctrl Pts',(81.8633131017034,-1.08185818454473,
77.7960479721345));
#183318=CARTESIAN_POINT('Ctrl Pts',(81.8800532043596,-0.995382030637029,
77.7952308719302));
#183319=CARTESIAN_POINT('Ctrl Pts',(81.9330459170107,-0.682226280151792,
77.7937155384981));
#183320=CARTESIAN_POINT('Ctrl Pts',(81.9574005939911,-0.453763238979424,
77.7953287042204));
#183321=CARTESIAN_POINT('Ctrl Pts',(81.9815657321761,0.086629399831015,
77.8052474935193));
#183322=CARTESIAN_POINT('Ctrl Pts',(81.969468143672,0.398269146113887,77.8157320320428));
#183323=CARTESIAN_POINT('Ctrl Pts',(81.9242594577514,0.764723751114935,
77.8329103575786));
#183324=CARTESIAN_POINT('Ctrl Pts',(81.9162429635908,0.822257264086457,
77.8357499805543));
#183325=CARTESIAN_POINT('Ctrl Pts',(81.9013645814289,0.918001651934274,
77.8407042968495));
#183326=CARTESIAN_POINT('Ctrl Pts',(81.8950021199262,0.956288855472329,
77.8427465556726));
#183327=CARTESIAN_POINT('Ctrl Pts',(81.8797511257293,1.04245205493504,77.8474788586767));
#183328=CARTESIAN_POINT('Ctrl Pts',(81.8706330494829,1.09028123627393,77.8502020435365));
#183329=CARTESIAN_POINT('Ctrl Pts',(81.8476565059013,1.20272803807061,77.8568415540689));
#183330=CARTESIAN_POINT('Ctrl Pts',(81.8332705881775,1.26722546027236,77.86083586845));
#183331=CARTESIAN_POINT('Ctrl Pts',(81.7591987326617,1.57344650824585,77.8807376895099));
#183332=CARTESIAN_POINT('Ctrl Pts',(81.6844629328004,1.81106002175706,77.8989976824651));
#183333=CARTESIAN_POINT('Ctrl Pts',(81.5941173588847,2.04265365340619,77.9201017942693));
#183334=CARTESIAN_POINT('Ctrl Pts',(80.6284101054663,-3.63675684748496,
78.0903820385128));
#183335=CARTESIAN_POINT('Ctrl Pts',(80.3940563201404,-3.90523957448573,
78.1240877061337));
#183336=CARTESIAN_POINT('Ctrl Pts',(80.1345088331788,-4.14997445340766,
78.1625085719411));
#183337=CARTESIAN_POINT('Ctrl Pts',(79.7808318845804,-4.42352325093256,
78.214849052098));
#183338=CARTESIAN_POINT('Ctrl Pts',(79.70702012462,-4.47769516956664,78.2257760341449));
#183339=CARTESIAN_POINT('Ctrl Pts',(79.5728538380439,-4.57104850857269,
78.2456304732333));
#183340=CARTESIAN_POINT('Ctrl Pts',(79.5130143459865,-4.61094720078165,
78.254483335969));
#183341=CARTESIAN_POINT('Ctrl Pts',(79.3791100287484,-4.69644052719069,
78.2742841118123));
#183342=CARTESIAN_POINT('Ctrl Pts',(79.304711396019,-4.74146424476193,78.2852793300036));
#183343=CARTESIAN_POINT('Ctrl Pts',(79.0466088760025,-4.88930872787319,
78.3234016379376));
#183344=CARTESIAN_POINT('Ctrl Pts',(78.8580956201264,-4.98317373919724,
78.3512001122266));
#183345=CARTESIAN_POINT('Ctrl Pts',(78.4521140551989,-5.15662113600593,
78.4111396390857));
#183346=CARTESIAN_POINT('Ctrl Pts',(78.2340367450712,-5.23368833686723,
78.4433767616099));
#183347=CARTESIAN_POINT('Ctrl Pts',(77.8978367225211,-5.32877478829362,
78.4935205671464));
#183348=CARTESIAN_POINT('Ctrl Pts',(77.7828455378757,-5.35724758987058,
78.510749844654));
#183349=CARTESIAN_POINT('Ctrl Pts',(77.6204150291118,-5.39183777626021,
78.5352634496791));
#183350=CARTESIAN_POINT('Ctrl Pts',(77.5736585053054,-5.40114850324744,
78.5423401715031));
#183351=CARTESIAN_POINT('Ctrl Pts',(77.4888987347911,-5.41686141270102,
78.5552117338151));
#183352=CARTESIAN_POINT('Ctrl Pts',(77.4509374536727,-5.42347852051812,
78.5609926054656));
#183353=CARTESIAN_POINT('Ctrl Pts',(77.3552234922236,-5.43910673546241,
78.5756056383617));
#183354=CARTESIAN_POINT('Ctrl Pts',(77.2973938582507,-5.44758530027873,
78.5844681789869));
#183355=CARTESIAN_POINT('Ctrl Pts',(76.9408425364603,-5.49394270818737,
78.6392701766296));
#183356=CARTESIAN_POINT('Ctrl Pts',(76.6396746582074,-5.50761552944876,
78.6862191406364));
#183357=CARTESIAN_POINT('Ctrl Pts',(76.1081481615792,-5.48707644632523,
78.7687619288734));
#183358=CARTESIAN_POINT('Ctrl Pts',(75.8781766930943,-5.46329221801716,
78.8043742861795));
#183359=CARTESIAN_POINT('Ctrl Pts',(75.5642555778109,-5.41023515989713,
78.8525584951231));
#183360=CARTESIAN_POINT('Ctrl Pts',(75.4785158118147,-5.39358996277604,
78.8656756805764));
#183361=CARTESIAN_POINT('Ctrl Pts',(75.3232229171448,-5.35950561308275,
78.8893455537025));
#183362=CARTESIAN_POINT('Ctrl Pts',(75.2535458744884,-5.34275035193755,
78.8999331124092));
#183363=CARTESIAN_POINT('Ctrl Pts',(75.0967208734763,-5.30171714388795,
78.9236863785074));
#183364=CARTESIAN_POINT('Ctrl Pts',(75.0098001927731,-5.27662465662882,
78.9367973825715));
#183365=CARTESIAN_POINT('Ctrl Pts',(74.6573841534686,-5.16522700102426,
78.9897383307418));
#183366=CARTESIAN_POINT('Ctrl Pts',(74.3979441995,-5.06054142428486,79.0281768308309));
#183367=CARTESIAN_POINT('Ctrl Pts',(73.9624528718956,-4.84432950924887,
79.0922309979064));
#183368=CARTESIAN_POINT('Ctrl Pts',(73.7826456927854,-4.74187732155216,
79.1185340890117));
#183369=CARTESIAN_POINT('Ctrl Pts',(73.5619592860798,-4.59885388815738,
79.1509129254303));
#183370=CARTESIAN_POINT('Ctrl Pts',(73.5153486181535,-4.5676108729711,79.1577577753707));
#183371=CARTESIAN_POINT('Ctrl Pts',(73.4349332402378,-4.51188419364041,
79.1695871865049));
#183372=CARTESIAN_POINT('Ctrl Pts',(73.4009149150978,-4.48772543288065,
79.1745986299192));
#183373=CARTESIAN_POINT('Ctrl Pts',(73.3255623119591,-4.43289659231789,
79.1857137727034));
#183374=CARTESIAN_POINT('Ctrl Pts',(73.2843775456728,-4.40202593011779,
79.1917980324538));
#183375=CARTESIAN_POINT('Ctrl Pts',(73.0278240876535,-4.20397924862833,
79.2297260779207));
#183376=CARTESIAN_POINT('Ctrl Pts',(72.8246717576473,-4.02129618245288,
79.2598638888135));
#183377=CARTESIAN_POINT('Ctrl Pts',(72.5288581331804,-3.71241269160276,
79.3029618475044));
#183378=CARTESIAN_POINT('Ctrl Pts',(72.4266454204006,-3.59625080900249,
79.317684432372));
#183379=CARTESIAN_POINT('Ctrl Pts',(72.2944934548233,-3.43267559169422,
79.336379003805));
#183380=CARTESIAN_POINT('Ctrl Pts',(72.2602379570709,-3.38894090182474,
79.3411912480854));
#183381=CARTESIAN_POINT('Ctrl Pts',(72.1709185412686,-3.27129332051794,
79.3536413916588));
#183382=CARTESIAN_POINT('Ctrl Pts',(72.1170219598297,-3.19649294736063,
79.3610508654127));
#183383=CARTESIAN_POINT('Ctrl Pts',(72.0242364371869,-3.06069810282558,
79.3736026796211));
#183384=CARTESIAN_POINT('Ctrl Pts',(71.984632835931,-3.00023200104705,79.3788874996497));
#183385=CARTESIAN_POINT('Ctrl Pts',(71.8998700738488,-2.86513080676946,
79.3900292429983));
#183386=CARTESIAN_POINT('Ctrl Pts',(71.855261605413,-2.79016461705903,79.3957777141826));
#183387=CARTESIAN_POINT('Ctrl Pts',(71.7199375449584,-2.55006098473281,
79.4128375044416));
#183388=CARTESIAN_POINT('Ctrl Pts',(71.635799810449,-2.38128295559807,79.4228577158204));
#183389=CARTESIAN_POINT('Ctrl Pts',(71.4596352730075,-1.9778330699217,79.4424495112208));
#183390=CARTESIAN_POINT('Ctrl Pts',(71.3746112017346,-1.74049959752493,
79.4507174097963));
#183391=CARTESIAN_POINT('Ctrl Pts',(71.2721440191207,-1.37894573163261,
79.4590399499996));
#183392=CARTESIAN_POINT('Ctrl Pts',(71.2423410997523,-1.25861494621162,
79.4611340684039));
#183393=CARTESIAN_POINT('Ctrl Pts',(71.2064670197567,-1.08976108210987,
79.4632119915069));
#183394=CARTESIAN_POINT('Ctrl Pts',(71.1969755268986,-1.04200825367281,
79.4637051033297));
#183395=CARTESIAN_POINT('Ctrl Pts',(71.1810361070769,-0.955908735576465,
79.4644308674772));
#183396=CARTESIAN_POINT('Ctrl Pts',(71.1743609744854,-0.917608665010389,
79.4646965431651));
#183397=CARTESIAN_POINT('Ctrl Pts',(71.1586852474065,-0.821725018920534,
79.4652164002841));
#183398=CARTESIAN_POINT('Ctrl Pts',(71.1501877132287,-0.764064033727843,
79.4653979356255));
#183399=CARTESIAN_POINT('Ctrl Pts',(71.1076577202557,-0.440270866784525,
79.4656456398651));
#183400=CARTESIAN_POINT('Ctrl Pts',(71.0920073221885,-0.172091960468779,
79.4629227734747));
#183401=CARTESIAN_POINT('Ctrl Pts',(71.0991580243968,0.350936268173423,
79.4508351450115));
#183402=CARTESIAN_POINT('Ctrl Pts',(71.1200712756766,0.605142448434162,
79.4418208995794));
#183403=CARTESIAN_POINT('Ctrl Pts',(71.1723404022888,0.950155925792415,
79.4248786898478));
#183404=CARTESIAN_POINT('Ctrl Pts',(71.1888257930237,1.04302556978188,79.4198443371493));
#183405=CARTESIAN_POINT('Ctrl Pts',(71.2221157607872,1.20640586945421,79.4101341632058));
#183406=CARTESIAN_POINT('Ctrl Pts',(71.2379598424545,1.27709975656437,79.4056461538721));
#183407=CARTESIAN_POINT('Ctrl Pts',(71.275538324518,1.43068751965561,79.3952648021893));
#183408=CARTESIAN_POINT('Ctrl Pts',(71.2978148466917,1.51342192875155,79.3892660070318));
#183409=CARTESIAN_POINT('Ctrl Pts',(71.3755412456854,1.7776551228409,79.3687943117415));
#183410=CARTESIAN_POINT('Ctrl Pts',(71.4383370514556,1.95673625253443,79.3528961839455));
#183411=CARTESIAN_POINT('Ctrl Pts',(71.5927942206316,2.33404340058379,79.3151060344769));
#183412=CARTESIAN_POINT('Ctrl Pts',(71.687250033547,2.53072517927569,79.2927029141657));
#183413=CARTESIAN_POINT('Ctrl Pts',(71.8323248734623,2.79183004607981,79.2594347535072));
#183414=CARTESIAN_POINT('Ctrl Pts',(71.873168083406,2.86165644053519,79.25017236789));
#183415=CARTESIAN_POINT('Ctrl Pts',(71.9487109790548,2.9844787968286,79.2332448050653));
#183416=CARTESIAN_POINT('Ctrl Pts',(71.9828186985332,3.03783417992675,79.2256697004847));
#183417=CARTESIAN_POINT('Ctrl Pts',(72.0407671796245,3.1251013311687,79.2129215174997));
#183418=CARTESIAN_POINT('Ctrl Pts',(72.0640851696806,3.15936321495012,79.2078229453833));
#183419=CARTESIAN_POINT('Ctrl Pts',(72.1184875630804,3.23737116557289,79.195999609947));
#183420=CARTESIAN_POINT('Ctrl Pts',(72.1498286991465,3.28092604623859,79.1892387131608));
#183421=CARTESIAN_POINT('Ctrl Pts',(72.2889760397257,3.46839919845321,79.1594124026569));
#183422=CARTESIAN_POINT('Ctrl Pts',(72.4031530541565,3.60729666314041,79.1354176121167));
#183423=CARTESIAN_POINT('Ctrl Pts',(72.6669339258392,3.89764530905349,79.0805469864712));
#183424=CARTESIAN_POINT('Ctrl Pts',(72.818955314213,4.04641685705457,79.0492630652738));
#183425=CARTESIAN_POINT('Ctrl Pts',(73.0552477582408,4.25194759286441,79.0007659498778));
#183426=CARTESIAN_POINT('Ctrl Pts',(73.1331654950865,4.31598509597362,78.9847941829096));
#183427=CARTESIAN_POINT('Ctrl Pts',(73.283061693228,4.43231073131682,78.9540751337371));
#183428=CARTESIAN_POINT('Ctrl Pts',(73.3546414089213,4.48507802032732,78.9394088384307));
#183429=CARTESIAN_POINT('Ctrl Pts',(73.4859728498022,4.57696959325129,78.9124922524133));
#183430=CARTESIAN_POINT('Ctrl Pts',(73.545273544558,4.61672886589895,78.9003359173442));
#183431=CARTESIAN_POINT('Ctrl Pts',(73.6795295275472,4.70292096621732,78.8728043387005));
#183432=CARTESIAN_POINT('Ctrl Pts',(73.7548601082599,4.74870513158792,78.8573497454659));
#183433=CARTESIAN_POINT('Ctrl Pts',(74.0288519637286,4.90612330707909,78.8011143468831));
#183434=CARTESIAN_POINT('Ctrl Pts',(74.2332640466902,5.00681107205553,78.7591039745079));
#183435=CARTESIAN_POINT('Ctrl Pts',(74.6382203141554,5.17503856381936,78.6759928941913));
#183436=CARTESIAN_POINT('Ctrl Pts',(74.8376431273674,5.24429695495903,78.6351170892154));
#183437=CARTESIAN_POINT('Ctrl Pts',(75.1492114923075,5.33209345712713,78.5716548166039));
#183438=CARTESIAN_POINT('Ctrl Pts',(75.2587846491163,5.35922531673406,78.5494115242861));
#183439=CARTESIAN_POINT('Ctrl Pts',(75.4148252560965,5.39260979731577,78.517902015241));
#183440=CARTESIAN_POINT('Ctrl Pts',(75.4606446248287,5.4017802055123,78.5086697873934));
#183441=CARTESIAN_POINT('Ctrl Pts',(75.5176778258127,5.41241160737266,78.4972071924153));
#183442=CARTESIAN_POINT('Ctrl Pts',(75.5287827382832,5.41444490413952,78.4949766817791));
#183443=CARTESIAN_POINT('Ctrl Pts',(75.539893974202,5.41644264127421,78.4927463157663));
#183444=CARTESIAN_POINT('Origin',(81.0480631074551,0.,102.742429499351));
#183445=CARTESIAN_POINT('',(68.2357429722793,-7.92639144670273E-16,67.3531585631293));
#183446=CARTESIAN_POINT('Origin',(74.6098026240559,0.,66.2292398698762));
#183447=CARTESIAN_POINT('',(68.1557866073341,-7.92639144670273E-16,66.8997034842526));
#183448=CARTESIAN_POINT('',(74.6740034556784,-7.92639144670273E-16,103.866348192604));
#183449=CARTESIAN_POINT('Origin',(74.5298462591107,0.,65.7757847909995));
#183450=CARTESIAN_POINT('Origin',(74.404241366658,0.,65.0634440479771));
#183451=CARTESIAN_POINT('',(67.9045768224286,-7.9263914467027E-16,65.4750219982078));
#183452=CARTESIAN_POINT('Origin',(68.6509091160486,-7.15449274600975E-16,
66.0779117527394));
#183453=CARTESIAN_POINT('Origin',(74.2786364742053,0.,64.3511033049547));
#183454=CARTESIAN_POINT('Origin',(81.0480631074551,0.,102.742429499351));
#183455=CARTESIAN_POINT('',(67.8248987953766,-7.92639144670271E-16,65.0231454519647));
#183456=CARTESIAN_POINT('',(74.6740034556784,-7.92639144670271E-16,103.866348192604));
#183457=CARTESIAN_POINT('Origin',(74.1989584471533,0.,63.8992267587115));
#183458=CARTESIAN_POINT('Origin',(78.1406475300671,0.,87.742352664884));
#183459=CARTESIAN_POINT('',(90.3032326828481,1.10218211923262E-15,104.890866373114));
#183460=CARTESIAN_POINT('',(72.5766931286283,-1.10218211923262E-15,108.016533571118));
#183461=CARTESIAN_POINT('Origin',(81.4399629057382,0.,106.453699972116));
#183462=CARTESIAN_POINT('',(69.2773777529572,-1.10218211923262E-15,89.3051862638862));
#183463=CARTESIAN_POINT('',(69.2773777529572,-1.10218211923262E-15,89.3051862638862));
#183464=CARTESIAN_POINT('Origin',(78.1406475300671,0.,87.742352664884));
#183465=CARTESIAN_POINT('Origin',(81.4399629057382,0.,106.453699972116));
#183466=CARTESIAN_POINT('Origin',(81.5267869945717,5.42101086242752E-17,
106.946103848622));
#183467=CARTESIAN_POINT('',(71.9391817309499,-1.17043669052308E-15,110.159797254809));
#183468=CARTESIAN_POINT('Origin',(81.787259261072,5.42101086242752E-17,
108.42331547814));
#183469=CARTESIAN_POINT('',(71.765533553283,-1.17043669052308E-15,109.174989501797));
#183470=CARTESIAN_POINT('',(71.6787094644496,-1.17043669052308E-15,108.682585625291));
#183471=CARTESIAN_POINT('',(91.4616886135273,1.27885690777163E-15,105.702025948459));
#183472=CARTESIAN_POINT('Origin',(81.6136110834051,5.42101086242752E-17,
107.438507725128));
#183473=CARTESIAN_POINT('Origin',(81.6136110834051,5.42101086242752E-17,
107.438507725128));
#183474=CARTESIAN_POINT('Origin',(81.787259261072,5.42101086242752E-17,
108.42331547814));
#183475=CARTESIAN_POINT('',(72.5184096962895,-1.10920435056572E-15,110.565377042483));
#183476=CARTESIAN_POINT('Origin',(81.8740833499055,5.42101086242752E-17,
108.915719354647));
#183477=CARTESIAN_POINT('Origin',(72.431585607456,-1.10920435056571E-15,
110.072973165976));
#183478=CARTESIAN_POINT('Origin',(81.6136110834051,5.42101086242752E-17,
107.438507725128));
#183479=CARTESIAN_POINT('',(90.8824606481877,-1.10920435056571E-15,105.296446160786));
#183480=CARTESIAN_POINT('Origin',(81.5267869945717,5.42101086242752E-17,
106.946103848622));
#183481=CARTESIAN_POINT('Origin',(90.9692847370211,-1.10920435056571E-15,
105.788850037292));
#183482=CARTESIAN_POINT('Origin',(81.4399629057382,0.,106.453699972116));
#183483=CARTESIAN_POINT('Origin',(90.7956365593542,-1.16341445918999E-15,
104.80404228428));
#183484=CARTESIAN_POINT('Origin',(78.1406475300671,0.,87.742352664884));
#183485=CARTESIAN_POINT('',(70.2621855059694,-9.79717439317882E-16,89.1315380862193));
#183486=CARTESIAN_POINT('Origin',(78.1406475300671,0.,87.742352664884));
#183487=CARTESIAN_POINT('',(73.5615008816405,-9.79717439317882E-16,107.842885393451));
#183488=CARTESIAN_POINT('',(70.2621855059694,-9.79717439317882E-16,89.1315380862193));
#183489=CARTESIAN_POINT('Origin',(81.4399629057382,0.,106.453699972116));
#183490=CARTESIAN_POINT('Origin',(81.4399629057382,0.,106.453699972116));
#183491=CARTESIAN_POINT('',(74.1407288469801,-9.18485099360508E-16,108.248465181124));
#183492=CARTESIAN_POINT('Origin',(74.0539047581466,-9.18485099360515E-16,
107.756061304618));
#183493=CARTESIAN_POINT('Origin',(81.5267869945717,0.,106.946103848622));
#183494=CARTESIAN_POINT('Origin',(81.5267869945717,0.,106.946103848622));
#183495=CARTESIAN_POINT('',(84.4241289406192,-4.89858719658941E-16,100.342664619881));
#183496=CARTESIAN_POINT('Origin',(80.4848979285703,0.,101.037257330549));
#183497=CARTESIAN_POINT('',(85.4660180066205,-4.89858719658941E-16,106.251511137954));
#183498=CARTESIAN_POINT('',(85.4660180066205,-4.89858719658941E-16,106.251511137954));
#183499=CARTESIAN_POINT('Origin',(81.5267869945717,0.,106.946103848622));
#183500=CARTESIAN_POINT('Origin',(81.0480631074551,0.,102.742429499351));
#183501=CARTESIAN_POINT('',(78.4660420348953,-2.827108640986E-16,101.393236094766));
#183502=CARTESIAN_POINT('Origin',(80.7394799846693,0.,100.992367645255));
#183503=CARTESIAN_POINT('',(72.336364674282,-2.827108640986E-16,66.6301083193878));
#183504=CARTESIAN_POINT('',(78.7746251576811,-2.827108640986E-16,103.143297948862));
#183505=CARTESIAN_POINT('Origin',(74.609802624056,0.,66.2292398698762));
#183506=CARTESIAN_POINT('Origin',(80.4848979285703,0.,101.037257330549));
#183507=CARTESIAN_POINT('Origin',(81.5267869945717,0.,106.946103848622));
#183508=CARTESIAN_POINT('Origin',(81.8740833499055,5.42101086242752E-17,
108.915719354647));
#183509=CARTESIAN_POINT('Origin',(78.1406475300671,0.,87.742352664884));
#183510=CARTESIAN_POINT('Origin',(74.1989584471533,0.,63.8992267587115));
#183511=CARTESIAN_POINT('Origin',(80.9838622758326,0.,65.1053211766231));
#183512=CARTESIAN_POINT('Ctrl Pts',(75.1292776351945,5.33099171449205,76.0772561825838));
#183513=CARTESIAN_POINT('Ctrl Pts',(73.7606186056544,5.08490089911617,76.3524352506115));
#183514=CARTESIAN_POINT('Ctrl Pts',(71.234833133868,3.43952652893016,76.8654944842279));
#183515=CARTESIAN_POINT('Ctrl Pts',(70.2709209865568,-1.04183990292265,
77.13700086402));
#183516=CARTESIAN_POINT('Ctrl Pts',(72.7198166924919,-4.91215295642792,
76.8067371393112));
#183517=CARTESIAN_POINT('Ctrl Pts',(77.1504659164359,-5.90856770039853,
76.1270368002636));
#183518=CARTESIAN_POINT('Ctrl Pts',(80.9793450358789,-3.43952652893015,
75.5534447668232));
#183519=CARTESIAN_POINT('Ctrl Pts',(81.9779868187236,1.04183990292267,75.4788999376335));
#183520=CARTESIAN_POINT('Ctrl Pts',(79.5638207483218,4.91215295642794,76.0061252129447));
#183521=CARTESIAN_POINT('Ctrl Pts',(75.1679011599112,5.90856770039855,76.8827871025948));
#183522=CARTESIAN_POINT('Ctrl Pts',(71.3737516760015,3.43952652893017,77.6533406866376));
#183523=CARTESIAN_POINT('Ctrl Pts',(70.4098395286903,-1.04183990292265,
77.9248470664298));
#183524=CARTESIAN_POINT('Ctrl Pts',(72.8587352346254,-4.91215295642792,
77.594583341721));
#183525=CARTESIAN_POINT('Ctrl Pts',(77.2893844585694,-5.90856770039853,
76.9148830026733));
#183526=CARTESIAN_POINT('Ctrl Pts',(81.1182635780125,-3.43952652893014,
76.3412909692329));
#183527=CARTESIAN_POINT('Ctrl Pts',(82.1169053608571,1.04183990292266,76.2667461400432));
#183528=CARTESIAN_POINT('Ctrl Pts',(79.7027392904554,4.91215295642793,76.7939714153545));
#183529=CARTESIAN_POINT('Ctrl Pts',(75.3068197020447,5.90856770039855,77.6706333050046));
#183530=CARTESIAN_POINT('Ctrl Pts',(71.512670218135,3.43952652893016,78.4411868890474));
#183531=CARTESIAN_POINT('Ctrl Pts',(70.5487580708238,-1.04183990292265,
78.7126932688396));
#183532=CARTESIAN_POINT('Ctrl Pts',(72.9976537767589,-4.91215295642791,
78.3824295441307));
#183533=CARTESIAN_POINT('Ctrl Pts',(77.4283030007029,-5.90856770039854,
77.7027292050831));
#183534=CARTESIAN_POINT('Ctrl Pts',(81.257182120146,-3.43952652893014,77.1291371716427));
#183535=CARTESIAN_POINT('Ctrl Pts',(82.2558239029906,1.04183990292265,77.054592342453));
#183536=CARTESIAN_POINT('Ctrl Pts',(79.8416578325889,4.91215295642793,77.5818176177643));
#183537=CARTESIAN_POINT('Ctrl Pts',(75.4457382441782,5.90856770039855,78.4584795074144));
#183538=CARTESIAN_POINT('Ctrl Pts',(71.6515887602686,3.43952652893016,79.2290330914572));
#183539=CARTESIAN_POINT('Ctrl Pts',(70.6876766129573,-1.04183990292266,
79.5005394712493));
#183540=CARTESIAN_POINT('Ctrl Pts',(73.1365723188924,-4.91215295642791,
79.1702757465405));
#183541=CARTESIAN_POINT('Ctrl Pts',(77.5672215428365,-5.90856770039854,
78.4905754074929));
#183542=CARTESIAN_POINT('Ctrl Pts',(81.3961006622795,-3.43952652893014,
77.9169833740525));
#183543=CARTESIAN_POINT('Ctrl Pts',(82.3947424451241,1.04183990292264,77.8424385448628));
#183544=CARTESIAN_POINT('Ctrl Pts',(79.9805763747224,4.91215295642793,78.369663820174));
#183545=CARTESIAN_POINT('Ctrl Pts',(75.5846567863118,5.90856770039855,79.2463257098241));
#183546=CARTESIAN_POINT('Ctrl Pts',(71.7905073024021,3.43952652893017,80.016879293867));
#183547=CARTESIAN_POINT('Ctrl Pts',(70.8265951550908,-1.04183990292266,
80.2883856736591));
#183548=CARTESIAN_POINT('Ctrl Pts',(73.2754908610259,-4.91215295642791,
79.9581219489503));
#183549=CARTESIAN_POINT('Ctrl Pts',(77.70614008497,-5.90856770039854,79.2784216099027));
#183550=CARTESIAN_POINT('Ctrl Pts',(81.535019204413,-3.43952652893014,78.7048295764623));
#183551=CARTESIAN_POINT('Ctrl Pts',(82.5336609872576,1.04183990292264,78.6302847472725));
#183552=CARTESIAN_POINT('Ctrl Pts',(80.1194949168559,4.91215295642793,79.1575100225838));
#183553=CARTESIAN_POINT('Ctrl Pts',(75.7235753284453,5.90856770039854,80.0341719122339));
#183554=CARTESIAN_POINT('Ctrl Pts',(71.9294258445356,3.4395265289302,80.8047254962767));
#183555=CARTESIAN_POINT('Ctrl Pts',(70.9655136972244,-1.04183990292267,
81.0762318760689));
#183556=CARTESIAN_POINT('Ctrl Pts',(73.4144094031595,-4.91215295642791,
80.7459681513601));
#183557=CARTESIAN_POINT('Ctrl Pts',(77.8450586271034,-5.90856770039855,
80.0662678123124));
#183558=CARTESIAN_POINT('Ctrl Pts',(81.6739377465466,-3.43952652893014,
79.492675778872));
#183559=CARTESIAN_POINT('Ctrl Pts',(82.6725795293912,1.04183990292264,79.4181309496823));
#183560=CARTESIAN_POINT('Ctrl Pts',(80.2584134589894,4.91215295642795,79.9453562249936));
#183561=CARTESIAN_POINT('Ctrl Pts',(75.8624938705788,5.90856770039853,80.8220181146437));
#183562=CARTESIAN_POINT('Ctrl Pts',(72.0683443866692,3.4395265289302,81.5925716986865));
#183563=CARTESIAN_POINT('Ctrl Pts',(71.294008903086,-0.160470683265631,
81.810679774696));
#183564=CARTESIAN_POINT('Ctrl Pts',(71.9717750339029,-2.06421305036014,
81.738895603627));
#183565=CARTESIAN_POINT('Ctrl Pts',(72.248017627255,-2.57465544021205,81.704063311873));
#183566=CARTESIAN_POINT('Ctrl Pts',(75.0835432977388,5.96755461207746,76.4642667723862));
#183567=CARTESIAN_POINT('Ctrl Pts',(73.5507643062705,5.69207859205401,76.7683846177746));
#183568=CARTESIAN_POINT('Ctrl Pts',(70.7219975874206,3.8502334087825,77.334867619897));
#183569=CARTESIAN_POINT('Ctrl Pts',(69.6409131499095,-1.16624389057502,
77.6270346358428));
#183570=CARTESIAN_POINT('Ctrl Pts',(72.3801530226782,-5.49870316824427,
77.2455754008299));
#183571=CARTESIAN_POINT('Ctrl Pts',(77.3377835776619,-6.61409777385948,
76.4729540347903));
#183572=CARTESIAN_POINT('Ctrl Pts',(81.621787881687,-3.85023340878249,75.8191111517082));
#183573=CARTESIAN_POINT('Ctrl Pts',(82.7376019547315,1.16624389057504,75.7239056863648));
#183574=CARTESIAN_POINT('Ctrl Pts',(80.0330917174962,5.49870316824429,76.3023264719802));
#183575=CARTESIAN_POINT('Ctrl Pts',(75.1101907980458,6.61409777385949,77.2719093886222));
#183576=CARTESIAN_POINT('Ctrl Pts',(70.8609161295542,3.8502334087825,78.1227138223068));
#183577=CARTESIAN_POINT('Ctrl Pts',(69.779831692043,-1.16624389057502,78.4148808382526));
#183578=CARTESIAN_POINT('Ctrl Pts',(72.5190715648117,-5.49870316824427,
78.0334216032397));
#183579=CARTESIAN_POINT('Ctrl Pts',(77.4767021197954,-6.61409777385948,
77.2608002372001));
#183580=CARTESIAN_POINT('Ctrl Pts',(81.7607064238205,-3.85023340878248,
76.606957354118));
#183581=CARTESIAN_POINT('Ctrl Pts',(82.876520496865,1.16624389057503,76.5117518887746));
#183582=CARTESIAN_POINT('Ctrl Pts',(80.1720102596297,5.49870316824428,77.0901726743899));
#183583=CARTESIAN_POINT('Ctrl Pts',(75.2491093401794,6.6140977738595,78.059755591032));
#183584=CARTESIAN_POINT('Ctrl Pts',(70.9998346716877,3.85023340878249,78.9105600247165));
#183585=CARTESIAN_POINT('Ctrl Pts',(69.9187502341765,-1.16624389057502,
79.2027270406623));
#183586=CARTESIAN_POINT('Ctrl Pts',(72.6579901069452,-5.49870316824426,
78.8212678056494));
#183587=CARTESIAN_POINT('Ctrl Pts',(77.615620661929,-6.61409777385948,78.0486464396098));
#183588=CARTESIAN_POINT('Ctrl Pts',(81.899624965954,-3.85023340878247,77.3948035565277));
#183589=CARTESIAN_POINT('Ctrl Pts',(83.0154390389986,1.16624389057501,77.2995980911844));
#183590=CARTESIAN_POINT('Ctrl Pts',(80.3109288017633,5.49870316824428,77.8780188767997));
#183591=CARTESIAN_POINT('Ctrl Pts',(75.3880278823129,6.61409777385949,78.8476017934417));
#183592=CARTESIAN_POINT('Ctrl Pts',(71.1387532138212,3.8502334087825,79.6984062271263));
#183593=CARTESIAN_POINT('Ctrl Pts',(70.0576687763101,-1.16624389057503,
79.9905732430721));
#183594=CARTESIAN_POINT('Ctrl Pts',(72.7969086490787,-5.49870316824426,
79.6091140080592));
#183595=CARTESIAN_POINT('Ctrl Pts',(77.7545392040625,-6.61409777385948,
78.8364926420196));
#183596=CARTESIAN_POINT('Ctrl Pts',(82.0385435080876,-3.85023340878247,
78.1826497589375));
#183597=CARTESIAN_POINT('Ctrl Pts',(83.1543575811321,1.16624389057501,78.0874442935942));
#183598=CARTESIAN_POINT('Ctrl Pts',(80.4498473438968,5.49870316824428,78.6658650792095));
#183599=CARTESIAN_POINT('Ctrl Pts',(75.5269464244464,6.61409777385949,79.6354479958515));
#183600=CARTESIAN_POINT('Ctrl Pts',(71.2776717559547,3.8502334087825,80.4862524295361));
#183601=CARTESIAN_POINT('Ctrl Pts',(70.1965873184436,-1.16624389057503,
80.7784194454819));
#183602=CARTESIAN_POINT('Ctrl Pts',(72.9358271912123,-5.49870316824426,
80.396960210469));
#183603=CARTESIAN_POINT('Ctrl Pts',(77.893457746196,-6.61409777385948,79.6243388444294));
#183604=CARTESIAN_POINT('Ctrl Pts',(82.1774620502211,-3.85023340878248,
78.9704959613473));
#183605=CARTESIAN_POINT('Ctrl Pts',(83.2932761232656,1.16624389057501,78.8752904960039));
#183606=CARTESIAN_POINT('Ctrl Pts',(80.5887658860303,5.49870316824428,79.4537112816192));
#183607=CARTESIAN_POINT('Ctrl Pts',(75.6658649665799,6.61409777385948,80.4232941982613));
#183608=CARTESIAN_POINT('Ctrl Pts',(71.4165902980883,3.85023340878254,81.2740986319458));
#183609=CARTESIAN_POINT('Ctrl Pts',(70.3355058605771,-1.16624389057504,
81.5662656478916));
#183610=CARTESIAN_POINT('Ctrl Pts',(73.0747457333458,-5.49870316824426,
81.1848064128787));
#183611=CARTESIAN_POINT('Ctrl Pts',(78.0323762883295,-6.61409777385949,
80.4121850468392));
#183612=CARTESIAN_POINT('Ctrl Pts',(82.3163805923546,-3.85023340878247,
79.7583421637571));
#183613=CARTESIAN_POINT('Ctrl Pts',(83.4321946653991,1.166243890575,79.6631366984137));
#183614=CARTESIAN_POINT('Ctrl Pts',(80.7276844281638,5.49870316824431,80.241557484029));
#183615=CARTESIAN_POINT('Ctrl Pts',(75.8047835087135,6.61409777385948,81.2111404006711));
#183616=CARTESIAN_POINT('Ctrl Pts',(71.5555088402218,3.85023340878254,82.0619448343556));
#183617=CARTESIAN_POINT('Ctrl Pts',(70.6870458344909,-0.179632161764912,
82.296650132147));
#183618=CARTESIAN_POINT('Ctrl Pts',(71.4447681147403,-2.31069653991403,
82.2107675346595));
#183619=CARTESIAN_POINT('Ctrl Pts',(71.7537129129724,-2.88208981923202,
82.1701689618565));
#183620=CARTESIAN_POINT('Ctrl Pts',(74.9476130689139,5.96755461207746,75.6933681369149));
#183621=CARTESIAN_POINT('Ctrl Pts',(73.4148340774456,5.69207859205401,75.9974859823033));
#183622=CARTESIAN_POINT('Ctrl Pts',(70.5860673585957,3.8502334087825,76.5639689844257));
#183623=CARTESIAN_POINT('Ctrl Pts',(69.5049829210846,-1.16624389057502,
76.8561360003715));
#183624=CARTESIAN_POINT('Ctrl Pts',(72.2442227938533,-5.49870316824427,
76.4746767653586));
#183625=CARTESIAN_POINT('Ctrl Pts',(77.201853348837,-6.61409777385948,75.702055399319));
#183626=CARTESIAN_POINT('Ctrl Pts',(81.4858576528621,-3.85023340878249,
75.0482125162369));
#183627=CARTESIAN_POINT('Ctrl Pts',(82.6016717259066,1.16624389057504,74.9530070508935));
#183628=CARTESIAN_POINT('Ctrl Pts',(79.8971614886713,5.49870316824429,75.5314278365089));
#183629=CARTESIAN_POINT('Ctrl Pts',(74.9742605692209,6.61409777385949,76.5010107531509));
#183630=CARTESIAN_POINT('Ctrl Pts',(70.7249859007293,3.8502334087825,77.3518151868354));
#183631=CARTESIAN_POINT('Ctrl Pts',(69.6439014632181,-1.16624389057502,
77.6439822027812));
#183632=CARTESIAN_POINT('Ctrl Pts',(72.3831413359868,-5.49870316824427,
77.2625229677683));
#183633=CARTESIAN_POINT('Ctrl Pts',(77.3407718909705,-6.61409777385948,
76.4899016017287));
#183634=CARTESIAN_POINT('Ctrl Pts',(81.6247761949956,-3.85023340878248,
75.8360587186467));
#183635=CARTESIAN_POINT('Ctrl Pts',(82.7405902680401,1.16624389057503,75.7408532533033));
#183636=CARTESIAN_POINT('Ctrl Pts',(80.0360800308048,5.49870316824428,76.3192740389186));
#183637=CARTESIAN_POINT('Ctrl Pts',(75.1131791113545,6.6140977738595,77.2888569555607));
#183638=CARTESIAN_POINT('Ctrl Pts',(70.8639044428628,3.85023340878249,78.1396613892452));
#183639=CARTESIAN_POINT('Ctrl Pts',(69.7828200053516,-1.16624389057502,
78.431828405191));
#183640=CARTESIAN_POINT('Ctrl Pts',(72.5220598781203,-5.49870316824426,
78.0503691701781));
#183641=CARTESIAN_POINT('Ctrl Pts',(77.479690433104,-6.61409777385948,77.2777478041385));
#183642=CARTESIAN_POINT('Ctrl Pts',(81.7636947371291,-3.85023340878247,
76.6239049210564));
#183643=CARTESIAN_POINT('Ctrl Pts',(82.8795088101737,1.16624389057501,76.5286994557131));
#183644=CARTESIAN_POINT('Ctrl Pts',(80.1749985729384,5.49870316824428,77.1071202413284));
#183645=CARTESIAN_POINT('Ctrl Pts',(75.252097653488,6.61409777385949,78.0767031579704));
#183646=CARTESIAN_POINT('Ctrl Pts',(71.0028229849963,3.8502334087825,78.927507591655));
#183647=CARTESIAN_POINT('Ctrl Pts',(69.9217385474851,-1.16624389057503,
79.2196746076008));
#183648=CARTESIAN_POINT('Ctrl Pts',(72.6609784202538,-5.49870316824426,
78.8382153725879));
#183649=CARTESIAN_POINT('Ctrl Pts',(77.6186089752376,-6.61409777385948,
78.0655940065483));
#183650=CARTESIAN_POINT('Ctrl Pts',(81.9026132792626,-3.85023340878247,
77.4117511234662));
#183651=CARTESIAN_POINT('Ctrl Pts',(83.0184273523072,1.16624389057501,77.3165456581228));
#183652=CARTESIAN_POINT('Ctrl Pts',(80.3139171150719,5.49870316824428,77.8949664437382));
#183653=CARTESIAN_POINT('Ctrl Pts',(75.3910161956215,6.61409777385949,78.8645493603802));
#183654=CARTESIAN_POINT('Ctrl Pts',(71.1417415271298,3.8502334087825,79.7153537940648));
#183655=CARTESIAN_POINT('Ctrl Pts',(70.0606570896187,-1.16624389057503,
80.0075208100106));
#183656=CARTESIAN_POINT('Ctrl Pts',(72.7998969623873,-5.49870316824426,
79.6260615749977));
#183657=CARTESIAN_POINT('Ctrl Pts',(77.7575275173711,-6.61409777385948,
78.8534402089581));
#183658=CARTESIAN_POINT('Ctrl Pts',(82.0415318213962,-3.85023340878248,
78.199597325876));
#183659=CARTESIAN_POINT('Ctrl Pts',(83.1573458944407,1.16624389057501,78.1043918605326));
#183660=CARTESIAN_POINT('Ctrl Pts',(80.4528356572054,5.49870316824428,78.6828126461479));
#183661=CARTESIAN_POINT('Ctrl Pts',(75.529934737755,6.61409777385948,79.65239556279));
#183662=CARTESIAN_POINT('Ctrl Pts',(71.2806600692634,3.85023340878254,80.5031999964745));
#183663=CARTESIAN_POINT('Ctrl Pts',(70.1995756317522,-1.16624389057504,
80.7953670124203));
#183664=CARTESIAN_POINT('Ctrl Pts',(72.9388155045209,-5.49870316824426,
80.4139077774074));
#183665=CARTESIAN_POINT('Ctrl Pts',(77.8964460595046,-6.61409777385949,
79.6412864113678));
#183666=CARTESIAN_POINT('Ctrl Pts',(82.1804503635297,-3.85023340878247,
78.9874435282857));
#183667=CARTESIAN_POINT('Ctrl Pts',(83.2962644365742,1.166243890575,78.8922380629424));
#183668=CARTESIAN_POINT('Ctrl Pts',(80.5917541993389,5.49870316824431,79.4706588485577));
#183669=CARTESIAN_POINT('Ctrl Pts',(75.6688532798886,6.61409777385948,80.4402417651997));
#183670=CARTESIAN_POINT('Ctrl Pts',(71.4195786113969,3.85023340878254,81.2910461988843));
#183671=CARTESIAN_POINT('Ctrl Pts',(70.551115605666,-0.179632161764912,
81.5257514966757));
#183672=CARTESIAN_POINT('Ctrl Pts',(71.3088378859154,-2.31069653991403,
81.4398688991882));
#183673=CARTESIAN_POINT('Ctrl Pts',(71.6177826841475,-2.88208981923202,
81.3992703263852));
#183674=CARTESIAN_POINT('Ctrl Pts',(75.1229547057303,5.33099171449205,76.0413970676667));
#183675=CARTESIAN_POINT('Ctrl Pts',(73.7542956761902,5.08490089911617,76.3165761356943));
#183676=CARTESIAN_POINT('Ctrl Pts',(71.2285102044038,3.43952652893016,76.8296353693107));
#183677=CARTESIAN_POINT('Ctrl Pts',(70.2645980570925,-1.04183990292265,
77.1011417491029));
#183678=CARTESIAN_POINT('Ctrl Pts',(72.7134937630276,-4.91215295642792,
76.770878024394));
#183679=CARTESIAN_POINT('Ctrl Pts',(77.1441429869717,-5.90856770039853,
76.0911776853464));
#183680=CARTESIAN_POINT('Ctrl Pts',(80.9730221064147,-3.43952652893015,
75.517585651906));
#183681=CARTESIAN_POINT('Ctrl Pts',(81.9716638892593,1.04183990292267,75.4430408227163));
#183682=CARTESIAN_POINT('Ctrl Pts',(79.5574978188576,4.91215295642794,75.9702660980275));
#183683=CARTESIAN_POINT('Ctrl Pts',(75.161578230447,5.90856770039855,76.8469279876776));
#183684=CARTESIAN_POINT('Ctrl Pts',(71.3674287465373,3.43952652893017,77.6174815717205));
#183685=CARTESIAN_POINT('Ctrl Pts',(70.4035165992261,-1.04183990292265,
77.8889879515126));
#183686=CARTESIAN_POINT('Ctrl Pts',(72.8524123051612,-4.91215295642792,
77.5587242268038));
#183687=CARTESIAN_POINT('Ctrl Pts',(77.2830615291052,-5.90856770039853,
76.8790238877561));
#183688=CARTESIAN_POINT('Ctrl Pts',(81.1119406485482,-3.43952652893014,
76.3054318543158));
#183689=CARTESIAN_POINT('Ctrl Pts',(82.1105824313929,1.04183990292266,76.2308870251261));
#183690=CARTESIAN_POINT('Ctrl Pts',(79.6964163609912,4.91215295642793,76.7581123004373));
#183691=CARTESIAN_POINT('Ctrl Pts',(75.3004967725805,5.90856770039855,77.6347741900874));
#183692=CARTESIAN_POINT('Ctrl Pts',(71.5063472886708,3.43952652893016,78.4053277741302));
#183693=CARTESIAN_POINT('Ctrl Pts',(70.5424351413596,-1.04183990292265,
78.6768341539224));
#183694=CARTESIAN_POINT('Ctrl Pts',(72.9913308472947,-4.91215295642791,
78.3465704292136));
#183695=CARTESIAN_POINT('Ctrl Pts',(77.4219800712387,-5.90856770039854,
77.6668700901659));
#183696=CARTESIAN_POINT('Ctrl Pts',(81.2508591906818,-3.43952652893014,
77.0932780567255));
#183697=CARTESIAN_POINT('Ctrl Pts',(82.2495009735264,1.04183990292265,77.0187332275358));
#183698=CARTESIAN_POINT('Ctrl Pts',(79.8353349031247,4.91215295642793,77.5459585028471));
#183699=CARTESIAN_POINT('Ctrl Pts',(75.439415314714,5.90856770039855,78.4226203924972));
#183700=CARTESIAN_POINT('Ctrl Pts',(71.6452658308043,3.43952652893016,79.19317397654));
#183701=CARTESIAN_POINT('Ctrl Pts',(70.6813536834931,-1.04183990292266,
79.4646803563322));
#183702=CARTESIAN_POINT('Ctrl Pts',(73.1302493894282,-4.91215295642791,
79.1344166316234));
#183703=CARTESIAN_POINT('Ctrl Pts',(77.5608986133722,-5.90856770039854,
78.4547162925757));
#183704=CARTESIAN_POINT('Ctrl Pts',(81.3897777328153,-3.43952652893014,
77.8811242591353));
#183705=CARTESIAN_POINT('Ctrl Pts',(82.3884195156599,1.04183990292264,77.8065794299456));
#183706=CARTESIAN_POINT('Ctrl Pts',(79.9742534452582,4.91215295642793,78.3338047052569));
#183707=CARTESIAN_POINT('Ctrl Pts',(75.5783338568476,5.90856770039855,79.2104665949069));
#183708=CARTESIAN_POINT('Ctrl Pts',(71.7841843729379,3.43952652893017,79.9810201789498));
#183709=CARTESIAN_POINT('Ctrl Pts',(70.8202722256266,-1.04183990292266,
80.2525265587419));
#183710=CARTESIAN_POINT('Ctrl Pts',(73.2691679315617,-4.91215295642791,
79.9222628340331));
#183711=CARTESIAN_POINT('Ctrl Pts',(77.6998171555057,-5.90856770039854,
79.2425624949855));
#183712=CARTESIAN_POINT('Ctrl Pts',(81.5286962749488,-3.43952652893014,
78.6689704615451));
#183713=CARTESIAN_POINT('Ctrl Pts',(82.5273380577934,1.04183990292264,78.5944256323554));
#183714=CARTESIAN_POINT('Ctrl Pts',(80.1131719873917,4.91215295642793,79.1216509076666));
#183715=CARTESIAN_POINT('Ctrl Pts',(75.7172523989811,5.90856770039854,79.9983127973167));
#183716=CARTESIAN_POINT('Ctrl Pts',(71.9231029150714,3.4395265289302,80.7688663813595));
#183717=CARTESIAN_POINT('Ctrl Pts',(70.9591907677601,-1.04183990292267,
81.0403727611517));
#183718=CARTESIAN_POINT('Ctrl Pts',(73.4080864736952,-4.91215295642791,
80.7101090364429));
#183719=CARTESIAN_POINT('Ctrl Pts',(77.8387356976392,-5.90856770039855,
80.0304086973952));
#183720=CARTESIAN_POINT('Ctrl Pts',(81.6676148170823,-3.43952652893014,
79.4568166639549));
#183721=CARTESIAN_POINT('Ctrl Pts',(82.666256599927,1.04183990292264,79.3822718347651));
#183722=CARTESIAN_POINT('Ctrl Pts',(80.2520905295252,4.91215295642795,79.9094971100764));
#183723=CARTESIAN_POINT('Ctrl Pts',(75.8561709411146,5.90856770039853,80.7861589997265));
#183724=CARTESIAN_POINT('Ctrl Pts',(72.0620214572049,3.4395265289302,81.5567125837693));
#183725=CARTESIAN_POINT('Ctrl Pts',(71.2876859736217,-0.160470683265631,
81.7748206597788));
#183726=CARTESIAN_POINT('Ctrl Pts',(71.9654521044387,-2.06421305036014,
81.7030364887098));
#183727=CARTESIAN_POINT('Ctrl Pts',(72.2416946977908,-2.57465544021205,
81.6682041969559));
#183728=CARTESIAN_POINT('Origin',(79.2469596359123,7.105427357601E-15,94.016560397588));
#183729=CARTESIAN_POINT('',(72.7191598750949,4.47917030439226,95.1675876200822));
#183730=CARTESIAN_POINT('Origin',(72.7191598750949,4.47917030439226,95.1675876200822));
#183731=CARTESIAN_POINT('',(74.7096346164239,-3.98351688341825,97.8628930544244));
#183732=CARTESIAN_POINT('Ctrl Pts',(74.7096346161526,-3.98351688369326,
97.8628930549279));
#183733=CARTESIAN_POINT('Ctrl Pts',(74.7227886043145,-4.12739717889162,
97.7913931478345));
#183734=CARTESIAN_POINT('Ctrl Pts',(74.7353899189023,-4.27253790874392,
97.7154740533153));
#183735=CARTESIAN_POINT('Ctrl Pts',(74.7474888928844,-4.41924001704132,
97.6351268963102));
#183736=CARTESIAN_POINT('Ctrl Pts',(74.7597998396111,-4.56851233076134,
97.5533720656115));
#183737=CARTESIAN_POINT('Ctrl Pts',(74.7715915811878,-4.71940100604202,
97.4670324976694));
#183738=CARTESIAN_POINT('Ctrl Pts',(74.7829106449292,-4.87217012296937,
97.3760999884628));
#183739=CARTESIAN_POINT('Ctrl Pts',(74.7843368471221,-4.89141903388181,
97.3646424910054));
#183740=CARTESIAN_POINT('Ctrl Pts',(74.785755526609,-4.91069773354052,97.353112079253));
#183741=CARTESIAN_POINT('Ctrl Pts',(74.7871667585286,-4.93000669486555,
97.3415087399564));
#183742=CARTESIAN_POINT('',(73.2401044080956,4.47917030439226,98.1220108791188));
#183743=CARTESIAN_POINT('Origin',(79.2469596359123,7.105427357601E-15,94.016560397588));
#183744=CARTESIAN_POINT('',(85.7747593967297,-4.47917030439225,92.8655331750938));
#183745=CARTESIAN_POINT('Origin',(85.7747593967297,-4.47917030439225,92.8655331750938));
#183746=CARTESIAN_POINT('',(85.862867185943,-1.98656284024888,95.8962772303022));
#183747=CARTESIAN_POINT('',(86.2957039297304,-4.47917030439225,95.8199564341304));
#183748=CARTESIAN_POINT('Ctrl Pts',(85.9403993280472,-2.93305265169037,
95.3748929158375));
#183749=CARTESIAN_POINT('Ctrl Pts',(85.9045302932766,-2.44228015705023,
95.6698129624946));
#183750=CARTESIAN_POINT('Ctrl Pts',(85.8628671861297,-1.98656284058723,
95.8962772310178));
#183751=CARTESIAN_POINT('Origin',(76.8158851485756,7.14546725904962E-15,
80.229251855417));
#183752=CARTESIAN_POINT('Origin',(76.1212924379081,7.15881389286582E-15,
76.2900208433682));
#183753=CARTESIAN_POINT('Origin',(76.9027092374091,7.105427357601E-15,80.7216557319231));
#183754=CARTESIAN_POINT('Origin',(79.6810800800795,7.105427357601E-15,96.4785797801185));
#183755=CARTESIAN_POINT('Origin',(79.767904168913,7.105427357601E-15,96.9709836566246));
#183756=CARTESIAN_POINT('Origin',(79.767904168913,7.105427357601E-15,96.9709836566246));
#183757=CARTESIAN_POINT('',(0.,0.,0.));
#183758=CARTESIAN_POINT('Origin',(-30.5675339847409,-75.,72.98888938658));
#183759=CARTESIAN_POINT('',(-29.5675339847409,-99.4919512992173,62.8698826100749));
#183760=CARTESIAN_POINT('Origin',(-29.5675339847409,-75.,72.98888938658));
#183761=CARTESIAN_POINT('',(-30.5675339847409,-100.416176300248,62.4880331226987));
#183762=CARTESIAN_POINT('Origin',(-30.5675339847409,-99.491951707512,62.8698824413853));
#183763=CARTESIAN_POINT('Origin',(-30.5675339847409,-75.,72.98888938658));
#183764=CARTESIAN_POINT('Origin',(-50.5675339847409,-75.,72.98888938658));
#183765=CARTESIAN_POINT('',(-50.5675339847409,-100.416176300248,62.4880331226987));
#183766=CARTESIAN_POINT('',(-50.5675339847409,-100.416176300248,62.4880331226987));
#183767=CARTESIAN_POINT('Origin',(-50.5675339847409,-75.,72.98888938658));
#183768=CARTESIAN_POINT('Origin',(-50.5675339847409,-75.,72.98888938658));
#183769=CARTESIAN_POINT('',(-30.6675339847409,-77.8309143973437,85.0614170289143));
#183770=CARTESIAN_POINT('',(-30.6675339847409,-81.5157715065078,83.5389946787084));
#183771=CARTESIAN_POINT('Origin',(-30.6675339847409,-75.,72.98888938658));
#183772=CARTESIAN_POINT('',(-31.1675339847409,-77.8309143973437,85.0614170289143));
#183773=CARTESIAN_POINT('',(-31.1675339847409,-77.8309143973437,85.0614170289143));
#183774=CARTESIAN_POINT('',(-31.1675339847409,-81.5157715065078,83.5389946787084));
#183775=CARTESIAN_POINT('Origin',(-31.1675339847409,-75.,72.98888938658));
#183776=CARTESIAN_POINT('',(-31.1675339847409,-81.5157715065078,83.5389946787084));
#183777=CARTESIAN_POINT('Origin',(-50.5675339847409,-79.7349315517137,84.4492743365101));
#183778=CARTESIAN_POINT('Origin',(-30.6675339847409,-79.7349315517137,84.4492743365101));
#183779=CARTESIAN_POINT('Origin',(-31.1675339847409,-79.7349315517137,84.4492743365101));
#183780=CARTESIAN_POINT('Origin',(-30.5675339847409,-75.,72.98888938658));
#183781=CARTESIAN_POINT('',(-30.5675339847409,-99.9540640038802,62.678957782042));
#183782=CARTESIAN_POINT('Origin',(-30.5675339847409,-75.,72.98888938658));
#183783=CARTESIAN_POINT('',(-30.0675339847409,-99.491951707512,62.8698824413853));
#183784=CARTESIAN_POINT('Origin',(-30.5675339847409,-99.491951707512,62.8698824413853));
#183785=CARTESIAN_POINT('Origin',(-30.0675339847409,-75.,72.98888938658));
#183786=CARTESIAN_POINT('Origin',(-50.5675339847409,-75.,72.98888938658));
#183787=CARTESIAN_POINT('',(-50.5675339847409,-99.9540640038802,62.678957782042));
#183788=CARTESIAN_POINT('Origin',(-50.5675339847409,-75.,72.98888938658));
#183789=CARTESIAN_POINT('',(-50.5675339847409,-99.9540640038802,62.678957782042));
#183790=CARTESIAN_POINT('Origin',(-30.6175339847409,-75.,72.98888938658));
#183791=CARTESIAN_POINT('',(-30.0675339847409,-89.730914394206,66.9027176170056));
#183792=CARTESIAN_POINT('Origin',(-30.0675339847409,-75.,72.98888938658));
#183793=CARTESIAN_POINT('',(-31.1675339847409,-88.5756336532856,67.3800292653638));
#183794=CARTESIAN_POINT('',(-30.6175339847409,-89.1532740237459,67.1413734411847));
#183795=CARTESIAN_POINT('Origin',(-31.1675339847409,-75.,72.98888938658));
#183796=CARTESIAN_POINT('Origin',(-30.0675339847409,-75.,72.98888938658));
#183797=CARTESIAN_POINT('Origin',(-31.1675339847409,-75.,72.98888938658));
#183798=CARTESIAN_POINT('Origin',(-30.6675339847409,-75.,72.98888938658));
#183799=CARTESIAN_POINT('',(-30.6675339847409,-88.4012565946763,67.4520742656244));
#183800=CARTESIAN_POINT('Origin',(-30.6675339847409,-75.,72.98888938658));
#183801=CARTESIAN_POINT('Origin',(-30.1175339847409,-75.,72.98888938658));
#183802=CARTESIAN_POINT('',(-29.5675339847409,-89.5565373355967,66.9747626172662));
#183803=CARTESIAN_POINT('',(-30.1175339847409,-88.9788969651366,67.2134184414453));
#183804=CARTESIAN_POINT('Origin',(-29.5675339847409,-75.,72.98888938658));
#183805=CARTESIAN_POINT('Origin',(-29.5675339847409,-75.,72.98888938658));
#183806=CARTESIAN_POINT('Origin',(-50.5675339847409,-75.,72.98888938658));
#183807=CARTESIAN_POINT('',(0.,0.,0.));
#183808=CARTESIAN_POINT('Origin',(114.28108174878,1.45439216225896E-14,
64.7979697995068));
#183809=CARTESIAN_POINT('',(114.543318806555,-13.8999677591299,63.4488784306985));
#183810=CARTESIAN_POINT('',(114.524364138745,-13.9,63.5463966488937));
#183811=CARTESIAN_POINT('',(114.28108174878,-13.9,64.7979697995068));
#183812=CARTESIAN_POINT('',(122.504911944309,-11.2745028192005,65.0976651712153));
#183813=CARTESIAN_POINT('Ctrl Pts',(114.543277020905,-13.8999999999995,
63.4490800523684));
#183814=CARTESIAN_POINT('Ctrl Pts',(115.963658533117,-13.9000003730414,
63.7423954021979));
#183815=CARTESIAN_POINT('Ctrl Pts',(117.375536377089,-13.6730345732275,
64.0328163031302));
#183816=CARTESIAN_POINT('Ctrl Pts',(119.398830937964,-13.005804924131,64.4519447188775));
#183817=CARTESIAN_POINT('Ctrl Pts',(120.052705348276,-12.7312234003918,
64.5876385202321));
#183818=CARTESIAN_POINT('Ctrl Pts',(121.318245112142,-12.0781519615802,
64.8504007864608));
#183819=CARTESIAN_POINT('Ctrl Pts',(121.927541701631,-11.6997943110756,
64.9769801574177));
#183820=CARTESIAN_POINT('Ctrl Pts',(122.504912016709,-11.2745030813742,
65.0976657537235));
#183821=CARTESIAN_POINT('Origin',(114.524364387726,1.45439216225896E-14,
63.5463953680056));
#183822=CARTESIAN_POINT('Origin',(114.28108174878,1.45439216225896E-14,
64.7979697995068));
#183823=CARTESIAN_POINT('',(114.734115976417,-13.9,62.4673223247922));
#183824=CARTESIAN_POINT('',(114.700601321121,-13.899802441188,62.6397761140198));
#183825=CARTESIAN_POINT('',(114.28108174878,-13.9,64.7979697995068));
#183826=CARTESIAN_POINT('Ctrl Pts',(114.543319397432,-13.8999999999999,
63.4488737117307));
#183827=CARTESIAN_POINT('Ctrl Pts',(114.095666858061,-13.8999999556334,
63.3565847360325));
#183828=CARTESIAN_POINT('Ctrl Pts',(113.648290388235,-13.8774585757879,
63.26433528182));
#183829=CARTESIAN_POINT('Ctrl Pts',(112.763519724712,-13.7880783064319,
63.0817266868347));
#183830=CARTESIAN_POINT('Ctrl Pts',(112.326596578786,-13.7219076525622,
62.991467458277));
#183831=CARTESIAN_POINT('Ctrl Pts',(111.04717373429,-13.4626911120813,62.7271043930887));
#183832=CARTESIAN_POINT('Ctrl Pts',(110.218606810636,-13.2094152370216,
62.5560384754181));
#183833=CARTESIAN_POINT('Ctrl Pts',(108.807977651217,-12.6241766275,62.2636692196187));
#183834=CARTESIAN_POINT('Ctrl Pts',(108.215659315782,-12.3255326627123,
62.1405161583243));
#183835=CARTESIAN_POINT('Ctrl Pts',(107.153869499696,-11.6883047558964,
61.9194894819314));
#183836=CARTESIAN_POINT('Ctrl Pts',(106.679601671333,-11.3609608995555,
61.8206212074063));
#183837=CARTESIAN_POINT('Ctrl Pts',(105.514845982761,-10.4426739187582,
61.5767317628101));
#183838=CARTESIAN_POINT('Ctrl Pts',(104.859172139605,-9.81046764030742,
61.4383282488724));
#183839=CARTESIAN_POINT('Ctrl Pts',(103.886795108932,-8.66655667634508,
61.2317970762891));
#183840=CARTESIAN_POINT('Ctrl Pts',(103.532920024943,-8.19162093957372,
61.1561537548604));
#183841=CARTESIAN_POINT('Ctrl Pts',(102.722495520566,-6.94462140645532,
60.981105216045));
#183842=CARTESIAN_POINT('Ctrl Pts',(102.307663196382,-6.14760569873943,
60.8898131920288));
#183843=CARTESIAN_POINT('Ctrl Pts',(101.515929828871,-4.18733815719314,
60.7114347669576));
#183844=CARTESIAN_POINT('Ctrl Pts',(101.208308156127,-3.00297326747312,
60.6371461238094));
#183845=CARTESIAN_POINT('Ctrl Pts',(100.965362890981,-1.06678823885153,
60.5673269685623));
#183846=CARTESIAN_POINT('Ctrl Pts',(100.930699011687,-0.334633476992079,
60.5521801336653));
#183847=CARTESIAN_POINT('Ctrl Pts',(100.972382330946,1.04335826550525,60.5440932546729));
#183848=CARTESIAN_POINT('Ctrl Pts',(101.036197286776,1.6876291483366,60.5488319398315));
#183849=CARTESIAN_POINT('Ctrl Pts',(101.263726472942,3.035974669637,60.5772361096543));
#183850=CARTESIAN_POINT('Ctrl Pts',(101.437780966737,3.73635802861391,60.6027837747792));
#183851=CARTESIAN_POINT('Ctrl Pts',(101.869716219272,5.03914724483873,60.6706094706755));
#183852=CARTESIAN_POINT('Ctrl Pts',(102.117613064756,5.6429504599671,60.7110521206048));
#183853=CARTESIAN_POINT('Ctrl Pts',(102.661437777928,6.74317933045791,60.8025239489437));
#183854=CARTESIAN_POINT('Ctrl Pts',(102.947976024289,7.24287385664565,60.8515898869089));
#183855=CARTESIAN_POINT('Ctrl Pts',(103.643933464606,8.299582680346,60.9720271090248));
#183856=CARTESIAN_POINT('Ctrl Pts',(104.065499529978,8.84648795263345,61.0457170265283));
#183857=CARTESIAN_POINT('Ctrl Pts',(104.911710572345,9.78996260364795,61.1953631768537));
#183858=CARTESIAN_POINT('Ctrl Pts',(105.324276576804,10.1956581742615,61.2688935280097));
#183859=CARTESIAN_POINT('Ctrl Pts',(106.448827986222,11.1703231066037,61.4700161663888));
#183860=CARTESIAN_POINT('Ctrl Pts',(107.19343788303,11.6960002788795,61.603803779604));
#183861=CARTESIAN_POINT('Ctrl Pts',(108.505403938263,12.438609519224,61.8411856915302));
#183862=CARTESIAN_POINT('Ctrl Pts',(109.045785726917,12.6989811367864,61.9392443328906));
#183863=CARTESIAN_POINT('Ctrl Pts',(110.15911199204,13.147279214675,62.1414081656069));
#183864=CARTESIAN_POINT('Ctrl Pts',(110.730986829252,13.3343797093401,62.2453201503661));
#183865=CARTESIAN_POINT('Ctrl Pts',(111.877370220333,13.6265072769908,62.454157501314));
#183866=CARTESIAN_POINT('Ctrl Pts',(112.450103197555,13.7335642527326,62.5587283502245));
#183867=CARTESIAN_POINT('Ctrl Pts',(113.925491520917,13.9114597597983,62.8279600194855));
#183868=CARTESIAN_POINT('Ctrl Pts',(114.831555553521,13.928957848391,62.9931269391823));
#183869=CARTESIAN_POINT('Ctrl Pts',(116.30312027824,13.8089226881333,63.2618155048913));
#183870=CARTESIAN_POINT('Ctrl Pts',(116.870184897286,13.7260270358041,63.3653591437266));
#183871=CARTESIAN_POINT('Ctrl Pts',(118.301747125635,13.4225894299414,63.6262596268049));
#183872=CARTESIAN_POINT('Ctrl Pts',(119.153252298888,13.1519152204113,63.7810545565729));
#183873=CARTESIAN_POINT('Ctrl Pts',(121.10410515881,12.312096190463,64.1354159651481));
#183874=CARTESIAN_POINT('Ctrl Pts',(122.165901283655,11.672408931806,64.3269975888839));
#183875=CARTESIAN_POINT('Ctrl Pts',(123.690027133608,10.446406698609,64.6004070749153));
#183876=CARTESIAN_POINT('Ctrl Pts',(124.215010895498,9.95156385919201,64.6941085162938));
#183877=CARTESIAN_POINT('Ctrl Pts',(125.133313068973,8.93931931230886,64.8564485403229));
#183878=CARTESIAN_POINT('Ctrl Pts',(125.533534293469,8.43101852891742,64.9265388233358));
#183879=CARTESIAN_POINT('Ctrl Pts',(126.300234608229,7.30386579935176,65.0597252056201));
#183880=CARTESIAN_POINT('Ctrl Pts',(126.657350831049,6.68070642598612,65.1208713547891));
#183881=CARTESIAN_POINT('Ctrl Pts',(127.245535158981,5.44319417078767,65.2190752083594));
#183882=CARTESIAN_POINT('Ctrl Pts',(127.484400106291,4.83478584246649,65.2577526502302));
#183883=CARTESIAN_POINT('Ctrl Pts',(127.853344441209,3.66119464150078,65.3152211153698));
#183884=CARTESIAN_POINT('Ctrl Pts',(127.992529580459,3.10039807508109,65.3356435666504));
#183885=CARTESIAN_POINT('Ctrl Pts',(128.222566968736,1.85097788176063,65.3655174364438));
#183886=CARTESIAN_POINT('Ctrl Pts',(128.297861298161,1.16097522242937,65.3719024044926));
#183887=CARTESIAN_POINT('Ctrl Pts',(128.342829339017,-0.114099057704563,
65.3658051851043));
#183888=CARTESIAN_POINT('Ctrl Pts',(128.327381754698,-0.697112821076571,
65.3561374270146));
#183889=CARTESIAN_POINT('Ctrl Pts',(128.195199470171,-2.1923670140522,65.3129742889966));
#183890=CARTESIAN_POINT('Ctrl Pts',(128.025491438625,-3.09677295482776,
65.2690355788747));
#183891=CARTESIAN_POINT('Ctrl Pts',(127.600229675744,-4.55878546281939,
65.1687354873144));
#183892=CARTESIAN_POINT('Ctrl Pts',(127.393875146453,-5.12829977345572,
65.1216451956539));
#183893=CARTESIAN_POINT('Ctrl Pts',(126.908088047125,-6.23919834028285,
65.0129688012945));
#183894=CARTESIAN_POINT('Ctrl Pts',(126.628771211294,-6.77919527132568,
64.9514195832402));
#183895=CARTESIAN_POINT('Ctrl Pts',(126.01203208648,-7.80184336414442,64.8175344690342));
#183896=CARTESIAN_POINT('Ctrl Pts',(125.677332042665,-8.28471927884472,
64.7457179487588));
#183897=CARTESIAN_POINT('Ctrl Pts',(124.748081073692,-9.45857911508621,
64.5475333442691));
#183898=CARTESIAN_POINT('Ctrl Pts',(124.11459511956,-10.1137542204333,64.413440583838));
#183899=CARTESIAN_POINT('Ctrl Pts',(122.98384959728,-11.0716104050755,64.1762880080513));
#183900=CARTESIAN_POINT('Ctrl Pts',(122.522981749875,-11.4144946474593,
64.0800199875524));
#183901=CARTESIAN_POINT('Ctrl Pts',(121.295261360778,-12.2125098687246,
63.8240049791676));
#183902=CARTESIAN_POINT('Ctrl Pts',(120.503393423168,-12.6225011135906,
63.6593592767822));
#183903=CARTESIAN_POINT('Ctrl Pts',(118.538928359555,-13.4043707646203,
63.2526584710292));
#183904=CARTESIAN_POINT('Ctrl Pts',(117.345142289443,-13.6989780332306,
63.0057991772094));
#183905=CARTESIAN_POINT('Ctrl Pts',(115.665401057228,-13.8755975852762,
62.6593395765601));
#183906=CARTESIAN_POINT('Ctrl Pts',(115.199873509996,-13.9000000006544,
62.5633870594715));
#183907=CARTESIAN_POINT('Ctrl Pts',(114.734115967029,-13.9,62.4673223229672));
#183908=CARTESIAN_POINT('',(108.175215076124,-12.3034455984317,62.3120820166501));
#183909=CARTESIAN_POINT('Origin',(114.524364387726,1.45439216225896E-14,
63.5463953680056));
#183910=CARTESIAN_POINT('Ctrl Pts',(108.175253011541,-12.3034472057424,
62.311902880219));
#183911=CARTESIAN_POINT('Ctrl Pts',(107.829254740664,-12.1176623915642,
62.2397973760768));
#183912=CARTESIAN_POINT('Ctrl Pts',(107.491277563595,-11.9167369790387,
62.1692332067497));
#183913=CARTESIAN_POINT('Ctrl Pts',(106.831310016517,-11.4844746236066,
62.0313407147435));
#183914=CARTESIAN_POINT('Ctrl Pts',(106.509733403427,-11.2531712530537,
61.9640985330967));
#183915=CARTESIAN_POINT('Ctrl Pts',(105.602344025973,-10.5384778680501,
61.7742112359076));
#183916=CARTESIAN_POINT('Ctrl Pts',(105.04545782268,-10.0192730233713,61.6575406729719));
#183917=CARTESIAN_POINT('Ctrl Pts',(103.760334761446,-8.60418667222819,
61.3859000074079));
#183918=CARTESIAN_POINT('Ctrl Pts',(103.095170897116,-7.65697825411397,
61.2419655442359));
#183919=CARTESIAN_POINT('Ctrl Pts',(102.124067674928,-5.82764326895935,
61.028631765501));
#183920=CARTESIAN_POINT('Ctrl Pts',(101.774591739413,-4.9774463721549,60.9505465000764));
#183921=CARTESIAN_POINT('Ctrl Pts',(101.16866552192,-2.96220367212895,60.8090494773863));
#183922=CARTESIAN_POINT('Ctrl Pts',(100.971876285014,-1.78602280028819,
60.7559125155545));
#183923=CARTESIAN_POINT('Ctrl Pts',(100.882216640194,0.451211526356952,
60.7119554141485));
#183924=CARTESIAN_POINT('Ctrl Pts',(100.956917923202,1.50253571188173,60.7150089831391));
#183925=CARTESIAN_POINT('Ctrl Pts',(101.356286852974,3.66982229471046,60.7676413643215));
#183926=CARTESIAN_POINT('Ctrl Pts',(101.703424332697,4.77356625794603,60.8205557150018));
#183927=CARTESIAN_POINT('Ctrl Pts',(102.539106412512,6.60966146675549,60.9591717826443));
#183928=CARTESIAN_POINT('Ctrl Pts',(102.969573248346,7.36229662531501,61.0332292093258));
#183929=CARTESIAN_POINT('Ctrl Pts',(104.508490782369,9.55311376250124,61.3021821784205));
#183930=CARTESIAN_POINT('Ctrl Pts',(105.827682525528,10.81452146383,61.5354704994559));
#183931=CARTESIAN_POINT('Ctrl Pts',(107.865340341772,12.1108218284781,61.9041305156421));
#183932=CARTESIAN_POINT('Ctrl Pts',(108.403950897371,12.4045022658587,62.0020176235738));
#183933=CARTESIAN_POINT('Ctrl Pts',(110.007432795916,13.1429611170253,62.2928996629309));
#183934=CARTESIAN_POINT('Ctrl Pts',(111.110541210227,13.4891653894966,62.4925723628407));
#183935=CARTESIAN_POINT('Ctrl Pts',(112.965752884932,13.8198863955061,62.8310419799776));
#183936=CARTESIAN_POINT('Ctrl Pts',(113.697498351287,13.8893915556794,62.9650733315565));
#183937=CARTESIAN_POINT('Ctrl Pts',(115.59178945293,13.9138787699293,63.3115985440927));
#183938=CARTESIAN_POINT('Ctrl Pts',(116.749786876645,13.7786142098174,63.5218867436072));
#183939=CARTESIAN_POINT('Ctrl Pts',(119.049155845185,13.2027979487908,63.9403577904306));
#183940=CARTESIAN_POINT('Ctrl Pts',(120.177786278009,12.7527836771607,64.1467207138746));
#183941=CARTESIAN_POINT('Ctrl Pts',(121.753889642778,11.8653084912738,64.4316950775613));
#183942=CARTESIAN_POINT('Ctrl Pts',(122.254588513511,11.5384354163202,64.5215824075115));
#183943=CARTESIAN_POINT('Ctrl Pts',(124.180794774509,10.0927655755584,64.866524455924));
#183944=CARTESIAN_POINT('Ctrl Pts',(125.40356229856,8.72635832711256,65.085168210104));
#183945=CARTESIAN_POINT('Ctrl Pts',(126.770953942903,6.41826960404145,65.3183833253468));
#183946=CARTESIAN_POINT('Ctrl Pts',(127.140959249248,5.63790441019896,65.3797443818023));
#183947=CARTESIAN_POINT('Ctrl Pts',(127.83023994192,3.75404615250889,65.4904859045506));
#183948=CARTESIAN_POINT('Ctrl Pts',(128.0911700665,2.63526781093659,65.5290708030479));
#183949=CARTESIAN_POINT('Ctrl Pts',(128.315084764473,0.5730578530517,65.5478115641301));
#183950=CARTESIAN_POINT('Ctrl Pts',(128.324290676776,-0.358476281530813,
65.5380796946296));
#183951=CARTESIAN_POINT('Ctrl Pts',(128.141415510887,-2.41660215404027,
65.4784331948131));
#183952=CARTESIAN_POINT('Ctrl Pts',(127.904389136551,-3.53226331065458,
65.4203161659102));
#183953=CARTESIAN_POINT('Ctrl Pts',(127.306122110614,-5.27960018632084,
65.282161846537));
#183954=CARTESIAN_POINT('Ctrl Pts',(127.024821956496,-5.93425990435274,
65.2186308296363));
#183955=CARTESIAN_POINT('Ctrl Pts',(125.99183594923,-7.90815734164247,64.9909955785248));
#183956=CARTESIAN_POINT('Ctrl Pts',(125.07553331115,-9.12479661675895,64.7969688624804));
#183957=CARTESIAN_POINT('Ctrl Pts',(123.303414517789,-10.8138306825123,
64.4228647444522));
#183958=CARTESIAN_POINT('Ctrl Pts',(122.559121563029,-11.3895644829671,
64.2663923791376));
#183959=CARTESIAN_POINT('Ctrl Pts',(120.823677322221,-12.4652132965739,
63.9049518929865));
#183960=CARTESIAN_POINT('Ctrl Pts',(119.818584531465,-12.9290262905671,
63.6977086298234));
#183961=CARTESIAN_POINT('Ctrl Pts',(117.453078853571,-13.68568167006,63.2079891353038));
#183962=CARTESIAN_POINT('Ctrl Pts',(116.081021780324,-13.8999991869096,
62.9238711704367));
#183963=CARTESIAN_POINT('Ctrl Pts',(114.700619831036,-13.8999999999977,
62.6396862741661));
#183964=CARTESIAN_POINT('Origin',(114.28108174878,1.45439216225896E-14,
64.7979697995068));
#183965=CARTESIAN_POINT('',(114.924931416105,-13.9,61.4856668343432));
#183966=CARTESIAN_POINT('',(114.891525389284,-13.9,61.6575251889163));
#183967=CARTESIAN_POINT('',(114.28108174878,-13.9,64.7979697995068));
#183968=CARTESIAN_POINT('Ctrl Pts',(114.734115967029,-13.9,62.4673223229672));
#183969=CARTESIAN_POINT('Ctrl Pts',(114.635896167658,-13.899999999862,62.4470640162828));
#183970=CARTESIAN_POINT('Ctrl Pts',(114.537666032757,-13.8989147967141,
62.4268012395597));
#183971=CARTESIAN_POINT('Ctrl Pts',(113.752677260478,-13.8815634299461,
62.264853343907));
#183972=CARTESIAN_POINT('Ctrl Pts',(113.068056815718,-13.8133361697656,
62.123426082441));
#183973=CARTESIAN_POINT('Ctrl Pts',(111.829864962314,-13.5924920938731,
61.8678210539804));
#183974=CARTESIAN_POINT('Ctrl Pts',(111.275045072243,-13.4564272681486,
61.7533165731196));
#183975=CARTESIAN_POINT('Ctrl Pts',(109.870150650892,-13.0150078958601,
61.4627690581557));
#183976=CARTESIAN_POINT('Ctrl Pts',(109.038517459101,-12.6583388104979,
61.2901654699463));
#183977=CARTESIAN_POINT('Ctrl Pts',(107.718273635188,-11.9275483923215,
61.0158078887912));
#183978=CARTESIAN_POINT('Ctrl Pts',(107.208712096802,-11.5990803884342,
60.9096883303051));
#183979=CARTESIAN_POINT('Ctrl Pts',(106.131717685568,-10.798078129996,60.6844050688731));
#183980=CARTESIAN_POINT('Ctrl Pts',(105.576928927187,-10.3110560287063,
60.5677004564676));
#183981=CARTESIAN_POINT('Ctrl Pts',(104.657889985637,-9.36269681458055,
60.373623394926));
#183982=CARTESIAN_POINT('Ctrl Pts',(104.279094634271,-8.91861240693393,
60.2932285124025));
#183983=CARTESIAN_POINT('Ctrl Pts',(103.540356978776,-7.93230470128705,
60.1351062031801));
#183984=CARTESIAN_POINT('Ctrl Pts',(103.188067335821,-7.38588896166875,
60.0588505195161));
#183985=CARTESIAN_POINT('Ctrl Pts',(102.593852577201,-6.30515520550776,
59.9289116231603));
#183986=CARTESIAN_POINT('Ctrl Pts',(102.344893342825,-5.77648160515211,
59.8738146532213));
#183987=CARTESIAN_POINT('Ctrl Pts',(101.791855358639,-4.38196891390696,
59.7488082625675));
#183988=CARTESIAN_POINT('Ctrl Pts',(101.537992795468,-3.4984291459401,59.6885085713535));
#183989=CARTESIAN_POINT('Ctrl Pts',(101.26454815401,-2.01541232078002,59.6179020922508));
#183990=CARTESIAN_POINT('Ctrl Pts',(101.193967076518,-1.42873676667916,
59.5973940526453));
#183991=CARTESIAN_POINT('Ctrl Pts',(101.108757269638,0.0615188109527515,
59.5633717388363));
#183992=CARTESIAN_POINT('Ctrl Pts',(101.143503601298,0.965396462221698,
59.5594450102026));
#183993=CARTESIAN_POINT('Ctrl Pts',(101.428127128293,3.07839382916166,59.5901666994286));
#183994=CARTESIAN_POINT('Ctrl Pts',(101.750431932911,4.26993893037958,59.6382183554188));
#183995=CARTESIAN_POINT('Ctrl Pts',(102.443128861265,5.93313458782272,59.7519764190383));
#183996=CARTESIAN_POINT('Ctrl Pts',(102.695991991924,6.44883437696944,59.7945232341841));
#183997=CARTESIAN_POINT('Ctrl Pts',(103.326935038705,7.55777733348192,59.9022182410436));
#183998=CARTESIAN_POINT('Ctrl Pts',(103.719479497111,8.14070209233188,59.9701279554908));
#183999=CARTESIAN_POINT('Ctrl Pts',(104.512005893588,9.14488540591357,60.109218648897));
#184000=CARTESIAN_POINT('Ctrl Pts',(104.897914135787,9.57560031567484,60.1775771644449));
#184001=CARTESIAN_POINT('Ctrl Pts',(105.958829077431,10.6200285364352,60.3663401625124));
#184002=CARTESIAN_POINT('Ctrl Pts',(106.66916132764,11.1925712253983,60.4934665576179));
#184003=CARTESIAN_POINT('Ctrl Pts',(107.945900174839,12.0271566367378,60.7238116492156));
#184004=CARTESIAN_POINT('Ctrl Pts',(108.483813730122,12.3289135698586,60.8211984225643));
#184005=CARTESIAN_POINT('Ctrl Pts',(109.556520553774,12.8383026118733,61.0156177886013));
#184006=CARTESIAN_POINT('Ctrl Pts',(110.087792735784,13.0505821597941,61.1120025791216));
#184007=CARTESIAN_POINT('Ctrl Pts',(111.172997793677,13.4064287005963,61.3094289387588));
#184008=CARTESIAN_POINT('Ctrl Pts',(111.725862323305,13.5496736965118,61.4102746261987));
#184009=CARTESIAN_POINT('Ctrl Pts',(112.886581533898,13.773013657989,61.6219503369437));
#184010=CARTESIAN_POINT('Ctrl Pts',(113.494209256948,13.8475220551837,61.7327298295075));
#184011=CARTESIAN_POINT('Ctrl Pts',(115.007418048799,13.9291643173604,62.0087394679497));
#184012=CARTESIAN_POINT('Ctrl Pts',(115.91260292229,13.8867665782517,62.1742559777357));
#184013=CARTESIAN_POINT('Ctrl Pts',(117.373453579555,13.6697583322359,62.4406714400258));
#184014=CARTESIAN_POINT('Ctrl Pts',(117.934073416039,13.5495724553436,62.5427423827476));
#184015=CARTESIAN_POINT('Ctrl Pts',(119.153592051578,13.2056843393237,62.764742210071));
#184016=CARTESIAN_POINT('Ctrl Pts',(119.806488951848,12.9659861092103,62.8836291520487));
#184017=CARTESIAN_POINT('Ctrl Pts',(120.955170085647,12.441007372748,63.091997273171));
#184018=CARTESIAN_POINT('Ctrl Pts',(121.456708344703,12.1726380502158,63.1826825581831));
#184019=CARTESIAN_POINT('Ctrl Pts',(122.97630808687,11.232849257144,63.4568125567142));
#184020=CARTESIAN_POINT('Ctrl Pts',(123.923874073463,10.4551372939055,63.6270106756665));
#184021=CARTESIAN_POINT('Ctrl Pts',(125.369961924471,8.90556080816441,63.8829353842257));
#184022=CARTESIAN_POINT('Ctrl Pts',(125.917271364093,8.19140609685299,63.9789988095767));
#184023=CARTESIAN_POINT('Ctrl Pts',(126.703248248531,6.93030851442651,64.1144186025104));
#184024=CARTESIAN_POINT('Ctrl Pts',(126.982319565787,6.41264139321977,64.1617037292598));
#184025=CARTESIAN_POINT('Ctrl Pts',(127.541630646307,5.19825218776111,64.2546543347858));
#184026=CARTESIAN_POINT('Ctrl Pts',(127.800300720684,4.49331540503752,64.2963683058652));
#184027=CARTESIAN_POINT('Ctrl Pts',(128.166003036208,3.1821969109469,64.3516255255006));
#184028=CARTESIAN_POINT('Ctrl Pts',(128.291875485707,2.58340175081135,64.3688768980793));
#184029=CARTESIAN_POINT('Ctrl Pts',(128.509038325966,1.06866058858028,64.3930768310356));
#184030=CARTESIAN_POINT('Ctrl Pts',(128.550514139004,0.148384806139156,
64.3907044141276));
#184031=CARTESIAN_POINT('Ctrl Pts',(128.4722674771,-1.35045934555967,64.357941167705));
#184032=CARTESIAN_POINT('Ctrl Pts',(128.406112151684,-1.92921059428031,
64.3381726626449));
#184033=CARTESIAN_POINT('Ctrl Pts',(128.1826243107,-3.18904527889961,64.2797455896531));
#184034=CARTESIAN_POINT('Ctrl Pts',(128.010029513088,-3.86569409566474,
64.2382398556052));
#184035=CARTESIAN_POINT('Ctrl Pts',(127.605269446791,-5.07121511591131,
64.1447082622545));
#184036=CARTESIAN_POINT('Ctrl Pts',(127.38916685262,-5.6040859641453,64.095885838586));
#184037=CARTESIAN_POINT('Ctrl Pts',(126.865819217611,-6.69649725754257,
63.9798490677641));
#184038=CARTESIAN_POINT('Ctrl Pts',(126.551735609575,-7.25116162208593,
63.9114670898447));
#184039=CARTESIAN_POINT('Ctrl Pts',(125.794462386711,-8.39749772082035,
63.7482436542481));
#184040=CARTESIAN_POINT('Ctrl Pts',(125.339869226604,-8.97894230383076,
63.6511060823714));
#184041=CARTESIAN_POINT('Ctrl Pts',(124.226088892404,-10.1899136983897,
63.4150725084999));
#184042=CARTESIAN_POINT('Ctrl Pts',(123.546627179499,-10.7953448027287,
63.2725735105477));
#184043=CARTESIAN_POINT('Ctrl Pts',(122.331099553002,-11.6783291334865,
63.0184528822517));
#184044=CARTESIAN_POINT('Ctrl Pts',(121.826691068776,-11.9962788257679,
62.9132163000579));
#184045=CARTESIAN_POINT('Ctrl Pts',(120.82300537439,-12.5399590865741,62.7046068003729));
#184046=CARTESIAN_POINT('Ctrl Pts',(120.327563078071,-12.7706032396118,
62.6019474893253));
#184047=CARTESIAN_POINT('Ctrl Pts',(119.249420650729,-13.1948381797639,
62.3786746269096));
#184048=CARTESIAN_POINT('Ctrl Pts',(118.664740636947,-13.3798201465247,
62.2576574802116));
#184049=CARTESIAN_POINT('Ctrl Pts',(117.19430633689,-13.7362978133568,61.9536683022571));
#184050=CARTESIAN_POINT('Ctrl Pts',(116.300198006568,-13.8593883826947,
61.769436047561));
#184051=CARTESIAN_POINT('Ctrl Pts',(115.242206907773,-13.8971693108471,
61.5511440092589));
#184052=CARTESIAN_POINT('Ctrl Pts',(115.08355907857,-13.9000000002285,61.5184055635395));
#184053=CARTESIAN_POINT('Ctrl Pts',(114.924931416059,-13.9,61.4856668345648));
#184054=CARTESIAN_POINT('Ctrl Pts',(114.891525389284,-13.9,61.6575251889163));
#184055=CARTESIAN_POINT('Ctrl Pts',(115.021517509571,-13.9,61.6843424943502));
#184056=CARTESIAN_POINT('Ctrl Pts',(115.15154264268,-13.898099124399,61.71117858686));
#184057=CARTESIAN_POINT('Ctrl Pts',(115.785600842462,-13.8795440287187,
61.8421018209282));
#184058=CARTESIAN_POINT('Ctrl Pts',(116.28840999186,-13.8362123171273,61.9461231274097));
#184059=CARTESIAN_POINT('Ctrl Pts',(117.268922403503,-13.6953797895739,
62.1490977346866));
#184060=CARTESIAN_POINT('Ctrl Pts',(117.746179025309,-13.599993637292,62.2479495590594));
#184061=CARTESIAN_POINT('Ctrl Pts',(118.738264858113,-13.3447687463504,
62.4529212773574));
#184062=CARTESIAN_POINT('Ctrl Pts',(119.250894910031,-13.179435075753,62.558577125659));
#184063=CARTESIAN_POINT('Ctrl Pts',(120.325277327308,-12.7600767453057,
62.7804514601469));
#184064=CARTESIAN_POINT('Ctrl Pts',(120.882475216428,-12.497292281585,62.8958055946432));
#184065=CARTESIAN_POINT('Ctrl Pts',(121.84406935716,-11.9605109365751,63.0958726894617));
#184066=CARTESIAN_POINT('Ctrl Pts',(122.255123020173,-11.7011005126847,
63.1817430709072));
#184067=CARTESIAN_POINT('Ctrl Pts',(123.136431562167,-11.0763349546819,
63.366455028576));
#184068=CARTESIAN_POINT('Ctrl Pts',(123.598645354841,-10.7009020034612,
63.4637544100384));
#184069=CARTESIAN_POINT('Ctrl Pts',(124.234286386822,-10.1118424866292,
63.5974713979145));
#184070=CARTESIAN_POINT('Ctrl Pts',(124.427635187138,-9.92171607736547,
63.6381411877191));
#184071=CARTESIAN_POINT('Ctrl Pts',(125.277745172076,-9.03476459572254,
63.8172342067226));
#184072=CARTESIAN_POINT('Ctrl Pts',(125.867547960082,-8.2748881592662,63.9424827405772));
#184073=CARTESIAN_POINT('Ctrl Pts',(126.645136494603,-7.02388795670556,
64.1111991518969));
#184074=CARTESIAN_POINT('Ctrl Pts',(126.891368446709,-6.57415787600783,
64.1653507515486));
#184075=CARTESIAN_POINT('Ctrl Pts',(127.325060840968,-5.66681791284177,
64.2620232394482));
#184076=CARTESIAN_POINT('Ctrl Pts',(127.514129745694,-5.21083948500054,
64.3048420588134));
#184077=CARTESIAN_POINT('Ctrl Pts',(127.861323649825,-4.23072694869992,
64.3844376577583));
#184078=CARTESIAN_POINT('Ctrl Pts',(128.01371730787,-3.70535502299583,64.4200630029777));
#184079=CARTESIAN_POINT('Ctrl Pts',(128.274360541119,-2.56195304650751,
64.483761209423));
#184080=CARTESIAN_POINT('Ctrl Pts',(128.372764495814,-1.94280823956164,
64.5099416324965));
#184081=CARTESIAN_POINT('Ctrl Pts',(128.474610308618,-0.827970181223037,
64.5428973473318));
#184082=CARTESIAN_POINT('Ctrl Pts',(128.493747115742,-0.334873068718832,
64.5525859719842));
#184083=CARTESIAN_POINT('Ctrl Pts',(128.478985407369,0.761119158531955,
64.5631206489104));
#184084=CARTESIAN_POINT('Ctrl Pts',(128.432356989912,1.36288458641404,64.5615132169177));
#184085=CARTESIAN_POINT('Ctrl Pts',(128.30907551438,2.23113739090421,64.5477121398652));
#184086=CARTESIAN_POINT('Ctrl Pts',(128.262687436482,2.50131657915118,64.5417815305607));
#184087=CARTESIAN_POINT('Ctrl Pts',(128.017240688512,3.71790181147584,64.5079189575195));
#184088=CARTESIAN_POINT('Ctrl Pts',(127.729400730189,4.64315108149147,64.4625703173702));
#184089=CARTESIAN_POINT('Ctrl Pts',(127.147070503319,6.00326429112005,64.3669441910773));
#184090=CARTESIAN_POINT('Ctrl Pts',(126.919053240595,6.46411574179415,64.328910658348));
#184091=CARTESIAN_POINT('Ctrl Pts',(126.423685186711,7.34061665366765,64.2449910986012));
#184092=CARTESIAN_POINT('Ctrl Pts',(126.158564659135,7.75670657393927,64.1995238686699));
#184093=CARTESIAN_POINT('Ctrl Pts',(125.555578569915,8.60099508833629,64.0944220572823));
#184094=CARTESIAN_POINT('Ctrl Pts',(125.213496478063,9.025047166611,64.0339304875756));
#184095=CARTESIAN_POINT('Ctrl Pts',(124.42917356429,9.88804004712674,63.8945068210594));
#184096=CARTESIAN_POINT('Ctrl Pts',(123.980503315742,10.3193027551998,63.8143463347171));
#184097=CARTESIAN_POINT('Ctrl Pts',(123.13034835435,11.0323519590428,63.6622509853));
#184098=CARTESIAN_POINT('Ctrl Pts',(122.739785572062,11.3259013103544,63.5923016600345));
#184099=CARTESIAN_POINT('Ctrl Pts',(121.839552196591,11.930058660532,63.4307172654153));
#184100=CARTESIAN_POINT('Ctrl Pts',(121.323660417594,12.2292977528083,63.3378938876921));
#184101=CARTESIAN_POINT('Ctrl Pts',(120.547959842612,12.6137155897992,63.1972748218409));
#184102=CARTESIAN_POINT('Ctrl Pts',(120.302087869348,12.7265544829315,63.1525682883864));
#184103=CARTESIAN_POINT('Ctrl Pts',(119.17445997396,13.2038002162657,62.9472262321971));
#184104=CARTESIAN_POINT('Ctrl Pts',(118.260137061622,13.4814294916997,62.780101043474));
#184105=CARTESIAN_POINT('Ctrl Pts',(116.826657287953,13.7555605107813,62.5190274253581));
#184106=CARTESIAN_POINT('Ctrl Pts',(116.323702084606,13.8225979074876,62.4275511452423));
#184107=CARTESIAN_POINT('Ctrl Pts',(115.332506604706,13.8981158963788,62.2472519725531));
#184108=CARTESIAN_POINT('Ctrl Pts',(114.845160031885,13.9087234874643,62.1585880743205));
#184109=CARTESIAN_POINT('Ctrl Pts',(113.819835237767,13.8753613438994,61.9713914397251));
#184110=CARTESIAN_POINT('Ctrl Pts',(113.282866416028,13.8255034635852,61.8730175292959));
#184111=CARTESIAN_POINT('Ctrl Pts',(112.140587816258,13.6498105473389,61.664013944062));
#184112=CARTESIAN_POINT('Ctrl Pts',(111.537912411116,13.5142507755298,61.5539177122545));
#184113=CARTESIAN_POINT('Ctrl Pts',(110.480592181834,13.1989780922456,61.3615532677561));
#184114=CARTESIAN_POINT('Ctrl Pts',(110.022521143674,13.035051444953,61.2784815831576));
#184115=CARTESIAN_POINT('Ctrl Pts',(109.025614601247,12.6165234382339,61.0981056687943));
#184116=CARTESIAN_POINT('Ctrl Pts',(108.492530134448,12.3503037033032,61.0019403084735));
#184117=CARTESIAN_POINT('Ctrl Pts',(107.744331939226,11.9131177471869,60.8666669881906));
#184118=CARTESIAN_POINT('Ctrl Pts',(107.514517861371,11.7694762972824,60.8250816542274));
#184119=CARTESIAN_POINT('Ctrl Pts',(106.49321331107,11.0880370533729,60.6404070889773));
#184120=CARTESIAN_POINT('Ctrl Pts',(105.754016041265,10.4740821218333,60.5073233445586));
#184121=CARTESIAN_POINT('Ctrl Pts',(104.72604115033,9.42135323739642,60.3250723201675));
#184122=CARTESIAN_POINT('Ctrl Pts',(104.389062285477,9.03569380088552,60.2658583482805));
#184123=CARTESIAN_POINT('Ctrl Pts',(103.770875999386,8.2438164311981,60.1580662167428));
#184124=CARTESIAN_POINT('Ctrl Pts',(103.488453887321,7.8395331923433,60.1092372159773));
#184125=CARTESIAN_POINT('Ctrl Pts',(102.939377720663,6.95727124887921,60.0146220051358));
#184126=CARTESIAN_POINT('Ctrl Pts',(102.678123595837,6.47681012098997,59.9698476723705));
#184127=CARTESIAN_POINT('Ctrl Pts',(102.17950710498,5.41662042944942,59.8859619836853));
#184128=CARTESIAN_POINT('Ctrl Pts',(101.951417578421,4.83371858962455,59.8486741937301));
#184129=CARTESIAN_POINT('Ctrl Pts',(101.613901059843,3.76731863456407,59.7962242624089));
#184130=CARTESIAN_POINT('Ctrl Pts',(101.489806550648,3.28973362356727,59.7780742275802));
#184131=CARTESIAN_POINT('Ctrl Pts',(101.270167196467,2.2167708119723,59.7487779054115));
#184132=CARTESIAN_POINT('Ctrl Pts',(101.187172359889,1.61975726573154,59.7400916512792));
#184133=CARTESIAN_POINT('Ctrl Pts',(101.122228509132,0.74626456947289,59.7376166869233));
#184134=CARTESIAN_POINT('Ctrl Pts',(101.109868852085,0.472759272948751,
59.7382958864607));
#184135=CARTESIAN_POINT('Ctrl Pts',(101.08981902723,-0.768734755580033,
59.7482469682073));
#184136=CARTESIAN_POINT('Ctrl Pts',(101.173492250125,-1.73534846174754,
59.775116930826));
#184137=CARTESIAN_POINT('Ctrl Pts',(101.451206389597,-3.18937214438392,
59.8466594858126));
#184138=CARTESIAN_POINT('Ctrl Pts',(101.574883950745,-3.68780863158581,
59.8769745944806));
#184139=CARTESIAN_POINT('Ctrl Pts',(101.871213089228,-4.6531841180264,59.9469716119864));
#184140=CARTESIAN_POINT('Ctrl Pts',(102.042026207939,-5.11992789505063,
59.9862814979261));
#184141=CARTESIAN_POINT('Ctrl Pts',(102.342523343261,-5.82278618631986,
60.0536013283003));
#184142=CARTESIAN_POINT('Ctrl Pts',(102.454944775281,-6.06612496004753,
60.0784902116731));
#184143=CARTESIAN_POINT('Ctrl Pts',(103.01347300846,-7.18909438449888,60.2011326425552));
#184144=CARTESIAN_POINT('Ctrl Pts',(103.544191229289,-8.0216124532401,60.3151449486792));
#184145=CARTESIAN_POINT('Ctrl Pts',(104.481086804791,-9.19514871257436,
60.5152325808007));
#184146=CARTESIAN_POINT('Ctrl Pts',(104.827298019057,-9.58191908442061,
60.5889330427703));
#184147=CARTESIAN_POINT('Ctrl Pts',(105.537693130351,-10.2905018848784,
60.7394373549886));
#184148=CARTESIAN_POINT('Ctrl Pts',(105.898861062892,-10.6143841362858,
60.8156374241978));
#184149=CARTESIAN_POINT('Ctrl Pts',(106.488905730394,-11.0893326319013,
60.9392043510138));
#184150=CARTESIAN_POINT('Ctrl Pts',(106.706657769267,-11.2540641417708,
60.984640004462));
#184151=CARTESIAN_POINT('Ctrl Pts',(107.688853630776,-11.9516505663239,
61.1891647643256));
#184152=CARTESIAN_POINT('Ctrl Pts',(108.500681383012,-12.4107006906213,
61.3573224772473));
#184153=CARTESIAN_POINT('Ctrl Pts',(109.801882807888,-12.9784814785239,
61.6273485841689));
#184154=CARTESIAN_POINT('Ctrl Pts',(110.26203464034,-13.1499501636883,61.7228850392036));
#184155=CARTESIAN_POINT('Ctrl Pts',(111.032303895836,-13.389784861275,61.8826911150567));
#184156=CARTESIAN_POINT('Ctrl Pts',(111.337488778907,-13.4730735079182,
61.9459739257766));
#184157=CARTESIAN_POINT('Ctrl Pts',(111.967082523259,-13.6211283345275,
62.0763086497608));
#184158=CARTESIAN_POINT('Ctrl Pts',(112.291527670746,-13.6848247953573,
62.1433284130294));
#184159=CARTESIAN_POINT('Ctrl Pts',(113.307033292684,-13.845309617044,62.3526423976342));
#184160=CARTESIAN_POINT('Ctrl Pts',(114.003376205078,-13.9000006098779,
62.4957211308413));
#184161=CARTESIAN_POINT('Ctrl Pts',(114.700691784751,-13.8999999999949,
62.6393364838496));
#184162=CARTESIAN_POINT('Origin',(114.28108174878,1.45439216225896E-14,
64.7979697995068));
#184163=CARTESIAN_POINT('',(115.096794126421,-13.9,60.6015143527077));
#184164=CARTESIAN_POINT('',(115.082307292334,-13.9,60.6760422812756));
#184165=CARTESIAN_POINT('',(114.28108174878,-13.9,64.7979697995068));
#184166=CARTESIAN_POINT('',(123.077303486518,-11.2745052982129,62.1528545153591));
#184167=CARTESIAN_POINT('Origin',(115.096794126421,1.45439216225896E-14,
60.6015143527085));
#184168=CARTESIAN_POINT('Ctrl Pts',(114.924931416059,-13.9,61.4856668345648));
#184169=CARTESIAN_POINT('Ctrl Pts',(114.514032905067,-13.8999999994081,
61.4008626158395));
#184170=CARTESIAN_POINT('Ctrl Pts',(114.103271002266,-13.8810065652294,
61.3160502304064));
#184171=CARTESIAN_POINT('Ctrl Pts',(113.006182867517,-13.7793020447828,
61.0896353703607));
#184172=CARTESIAN_POINT('Ctrl Pts',(112.32419036809,-13.6622179299309,60.9490390673702));
#184173=CARTESIAN_POINT('Ctrl Pts',(111.106950010177,-13.3545824949699,
60.6975111533049));
#184174=CARTESIAN_POINT('Ctrl Pts',(110.568961845001,-13.1818078541457,
60.586132889826));
#184175=CARTESIAN_POINT('Ctrl Pts',(108.91912136123,-12.5345900895855,60.2442150329164));
#184176=CARTESIAN_POINT('Ctrl Pts',(107.857503443739,-11.9433566579271,
60.0238958361878));
#184177=CARTESIAN_POINT('Ctrl Pts',(106.173466873143,-10.6844216139425,
59.6714179578747));
#184178=CARTESIAN_POINT('Ctrl Pts',(105.513242632352,-10.081920690969,59.5327614426922));
#184179=CARTESIAN_POINT('Ctrl Pts',(104.523379834472,-8.98380083103208,
59.3229804851965));
#184180=CARTESIAN_POINT('Ctrl Pts',(104.15931632535,-8.52420686601659,59.2452356543091));
#184181=CARTESIAN_POINT('Ctrl Pts',(103.30517093681,-7.2928162897431,59.0614402579498));
#184182=CARTESIAN_POINT('Ctrl Pts',(102.859450925484,-6.49242222282162,
58.964368624448));
#184183=CARTESIAN_POINT('Ctrl Pts',(102.261852437951,-5.11731025732404,
58.8305990211956));
#184184=CARTESIAN_POINT('Ctrl Pts',(102.062610649424,-4.56717406095993,
58.7849104071466));
#184185=CARTESIAN_POINT('Ctrl Pts',(101.71435217156,-3.37913966085079,58.7027126279407));
#184186=CARTESIAN_POINT('Ctrl Pts',(101.574294195277,-2.73995530396663,
58.6680256235161));
#184187=CARTESIAN_POINT('Ctrl Pts',(101.393312344925,-1.5113723845637,58.618385959947));
#184188=CARTESIAN_POINT('Ctrl Pts',(101.343988993651,-0.924703340505352,
58.6018489958612));
#184189=CARTESIAN_POINT('Ctrl Pts',(101.315244654731,0.407964465518804,
58.5805764040955));
#184190=CARTESIAN_POINT('Ctrl Pts',(101.357898658598,1.15271149000324,58.5803684918613));
#184191=CARTESIAN_POINT('Ctrl Pts',(101.542502280734,2.50059787146857,58.600446000922));
#184192=CARTESIAN_POINT('Ctrl Pts',(101.665786419606,3.10444337802267,58.617143174642));
#184193=CARTESIAN_POINT('Ctrl Pts',(102.069967945765,4.58382249217927,58.6776442243802));
#184194=CARTESIAN_POINT('Ctrl Pts',(102.397525016489,5.4431673293882,58.7308805870588));
#184195=CARTESIAN_POINT('Ctrl Pts',(103.064680271925,6.7830002870378,58.8430135639024));
#184196=CARTESIAN_POINT('Ctrl Pts',(103.35516433932,7.28554395667475,58.8925726843135));
#184197=CARTESIAN_POINT('Ctrl Pts',(104.062374500383,8.35032525702672,59.0150167603172));
#184198=CARTESIAN_POINT('Ctrl Pts',(104.491755830537,8.90195101712393,59.0904842415158));
#184199=CARTESIAN_POINT('Ctrl Pts',(105.344507528353,9.84178792739701,59.2413541929351));
#184200=CARTESIAN_POINT('Ctrl Pts',(105.754255712011,10.2406402662997,59.3141925519481));
#184201=CARTESIAN_POINT('Ctrl Pts',(107.122754069782,11.4164295324604,59.5587960795008));
#184202=CARTESIAN_POINT('Ctrl Pts',(108.160106711424,12.0890355007076,59.7462993795098));
#184203=CARTESIAN_POINT('Ctrl Pts',(110.078924821598,12.9923761103421,60.0939475105977));
#184204=CARTESIAN_POINT('Ctrl Pts',(110.920715000775,13.2915055588507,60.2472450692554));
#184205=CARTESIAN_POINT('Ctrl Pts',(112.342677018892,13.6434122958441,60.5063323924851));
#184206=CARTESIAN_POINT('Ctrl Pts',(112.908261903787,13.7455949846953,60.6093794931222));
#184207=CARTESIAN_POINT('Ctrl Pts',(114.172016931903,13.8913552454079,60.8398216962434));
#184208=CARTESIAN_POINT('Ctrl Pts',(114.87051676782,13.9172606779213,60.9674917987822));
#184209=CARTESIAN_POINT('Ctrl Pts',(116.203888882048,13.8629451010672,61.2109335502684));
#184210=CARTESIAN_POINT('Ctrl Pts',(116.837324029176,13.791939857829,61.3264299018168));
#184211=CARTESIAN_POINT('Ctrl Pts',(118.353143398592,13.5121776196015,61.6026464272976));
#184212=CARTESIAN_POINT('Ctrl Pts',(119.224454202326,13.2587478523551,61.7615785305218));
#184213=CARTESIAN_POINT('Ctrl Pts',(120.59777205431,12.7048673823582,62.0109666833633));
#184214=CARTESIAN_POINT('Ctrl Pts',(121.116878562841,12.4561119004247,62.1049571011554));
#184215=CARTESIAN_POINT('Ctrl Pts',(122.217063387199,11.8402934230996,62.3038804658098));
#184216=CARTESIAN_POINT('Ctrl Pts',(122.789544908906,11.4605812750697,62.4072577213345));
#184217=CARTESIAN_POINT('Ctrl Pts',(123.783277266587,10.6881250419808,62.5856140216536));
#184218=CARTESIAN_POINT('Ctrl Pts',(124.21282752135,10.3089754707472,62.6622838804847));
#184219=CARTESIAN_POINT('Ctrl Pts',(125.075773853561,9.44596303813536,62.815560484972));
#184220=CARTESIAN_POINT('Ctrl Pts',(125.501319723255,8.95596589329347,62.8908115068038));
#184221=CARTESIAN_POINT('Ctrl Pts',(126.323317115303,7.86364683973198,63.0346672225302));
#184222=CARTESIAN_POINT('Ctrl Pts',(126.710597312391,7.25657985429476,63.1014266317697));
#184223=CARTESIAN_POINT('Ctrl Pts',(127.352388534624,6.05554858354794,63.2101158813461));
#184224=CARTESIAN_POINT('Ctrl Pts',(127.615921914817,5.46871259357983,63.2539703214335));
#184225=CARTESIAN_POINT('Ctrl Pts',(128.093264497884,4.17553995924312,63.3307657133324));
#184226=CARTESIAN_POINT('Ctrl Pts',(128.293738852582,3.46619690256007,63.3610404174184));
#184227=CARTESIAN_POINT('Ctrl Pts',(128.673000277598,1.56923636877742,63.4120136903323));
#184228=CARTESIAN_POINT('Ctrl Pts',(128.757672525873,0.36863099498387,63.4148707438064));
#184229=CARTESIAN_POINT('Ctrl Pts',(128.639806890499,-1.72310636947871,
63.367256121098));
#184230=CARTESIAN_POINT('Ctrl Pts',(128.504352669513,-2.61119350013773,
63.3306392426059));
#184231=CARTESIAN_POINT('Ctrl Pts',(128.136508695066,-4.07342267385892,
63.2415897240375));
#184232=CARTESIAN_POINT('Ctrl Pts',(127.948721632206,-4.65644810255506,
63.1978490645046));
#184233=CARTESIAN_POINT('Ctrl Pts',(127.485560144224,-5.82663164171815,
63.0929549316484));
#184234=CARTESIAN_POINT('Ctrl Pts',(127.206225739339,-6.41058075592392,
63.0312083948543));
#184235=CARTESIAN_POINT('Ctrl Pts',(126.410934235089,-7.81401565086172,
62.8578407190614));
#184236=CARTESIAN_POINT('Ctrl Pts',(125.848656697341,-8.60208290761153,
62.7369504890977));
#184237=CARTESIAN_POINT('Ctrl Pts',(124.892306848933,-9.68288574856614,
62.5341475014423));
#184238=CARTESIAN_POINT('Ctrl Pts',(124.556191186077,-10.0249117786789,
62.4632588863853));
#184239=CARTESIAN_POINT('Ctrl Pts',(123.844304826822,-10.6772111200816,
62.3135416149205));
#184240=CARTESIAN_POINT('Ctrl Pts',(123.468460925162,-10.9863827970222,
62.2347035333859));
#184241=CARTESIAN_POINT('Ctrl Pts',(123.077309244396,-11.2745153368956,
62.1528629199185));
#184242=CARTESIAN_POINT('Ctrl Pts',(115.082307292334,-13.9,60.6760422812756));
#184243=CARTESIAN_POINT('Ctrl Pts',(115.616042419255,-13.9,60.7863377957508));
#184244=CARTESIAN_POINT('Ctrl Pts',(116.149634438892,-13.8679498804623,
60.8967905452979));
#184245=CARTESIAN_POINT('Ctrl Pts',(116.946936389828,-13.7717115486751,
61.061755407262));
#184246=CARTESIAN_POINT('Ctrl Pts',(117.212533291068,-13.7314886459556,
61.1166912867009));
#184247=CARTESIAN_POINT('Ctrl Pts',(118.058063530176,-13.5772256862302,
61.2913498752852));
#184248=CARTESIAN_POINT('Ctrl Pts',(118.63202293339,-13.4326778464348,61.4095142855781));
#184249=CARTESIAN_POINT('Ctrl Pts',(119.65540216623,-13.1015576008644,61.6206050814545));
#184250=CARTESIAN_POINT('Ctrl Pts',(120.107752768997,-12.9276543277861,
61.7140590829468));
#184251=CARTESIAN_POINT('Ctrl Pts',(121.112079230007,-12.4778568600849,
61.922240800819));
#184252=CARTESIAN_POINT('Ctrl Pts',(121.656709267083,-12.1876122794215,
62.0356533688479));
#184253=CARTESIAN_POINT('Ctrl Pts',(122.637702808448,-11.5752608259786,
62.2407023161625));
#184254=CARTESIAN_POINT('Ctrl Pts',(123.078203837442,-11.2623240489777,
62.3330930100192));
#184255=CARTESIAN_POINT('Ctrl Pts',(123.880316903993,-10.6175110244167,
62.5012349232633));
#184256=CARTESIAN_POINT('Ctrl Pts',(124.244876846336,-10.2908004521861,
62.5775759420006));
#184257=CARTESIAN_POINT('Ctrl Pts',(124.952272283699,-9.58500997890699,
62.7262780048108));
#184258=CARTESIAN_POINT('Ctrl Pts',(125.293078977684,-9.20488912953273,
62.7982419353592));
#184259=CARTESIAN_POINT('Ctrl Pts',(126.211888674503,-8.05785265431681,
62.9938494152688));
#184260=CARTESIAN_POINT('Ctrl Pts',(126.732937187918,-7.24745216020387,
63.1070284739973));
#184261=CARTESIAN_POINT('Ctrl Pts',(127.290192843733,-6.14485975785458,
63.2304683910818));
#184262=CARTESIAN_POINT('Ctrl Pts',(127.406144983826,-5.89773198881215,
63.2563162977466));
#184263=CARTESIAN_POINT('Ctrl Pts',(127.753979347159,-5.09636088709482,
63.3342323360609));
#184264=CARTESIAN_POINT('Ctrl Pts',(127.957747600777,-4.53011485428487,
63.3804385621099));
#184265=CARTESIAN_POINT('Ctrl Pts',(128.261382968012,-3.47927944773119,
63.4516246852519));
#184266=CARTESIAN_POINT('Ctrl Pts',(128.373194866698,-2.99932782019874,
63.4788843546972));
#184267=CARTESIAN_POINT('Ctrl Pts',(128.569617455717,-1.89790121626044,
63.5300247297703));
#184268=CARTESIAN_POINT('Ctrl Pts',(128.638435764157,-1.27455906081511,
63.55094843465));
#184269=CARTESIAN_POINT('Ctrl Pts',(128.689531621346,-0.101454672421391,
63.5752427187126));
#184270=CARTESIAN_POINT('Ctrl Pts',(128.68158699367,0.446648417759629,63.5804639802709));
#184271=CARTESIAN_POINT('Ctrl Pts',(128.606179419164,1.48672707588937,63.5780323923241));
#184272=CARTESIAN_POINT('Ctrl Pts',(128.544566093058,1.97829567180721,63.5715333723782));
#184273=CARTESIAN_POINT('Ctrl Pts',(128.366572414747,2.97249783873833,63.5481323985874));
#184274=CARTESIAN_POINT('Ctrl Pts',(128.24820971207,3.47400340878646,63.5308423597815));
#184275=CARTESIAN_POINT('Ctrl Pts',(127.829616911276,4.89484609785691,63.4664837943271));
#184276=CARTESIAN_POINT('Ctrl Pts',(127.462058360269,5.79061623110116,63.4069342778574));
#184277=CARTESIAN_POINT('Ctrl Pts',(126.877033908554,6.88125971934158,63.3083363147176));
#184278=CARTESIAN_POINT('Ctrl Pts',(126.740900778362,7.11814862389404,63.2851835530943));
#184279=CARTESIAN_POINT('Ctrl Pts',(126.283699321691,7.86248825818054,63.2066156482955));
#184280=CARTESIAN_POINT('Ctrl Pts',(125.937145253471,8.3528907924079,63.1458494828957));
#184281=CARTESIAN_POINT('Ctrl Pts',(125.252238119632,9.20011035830848,63.0248814256844));
#184282=CARTESIAN_POINT('Ctrl Pts',(124.924354826569,9.56439601985719,62.9666725938142));
#184283=CARTESIAN_POINT('Ctrl Pts',(124.138148244168,10.3496691989574,62.826808246281));
#184284=CARTESIAN_POINT('Ctrl Pts',(123.669443924711,10.7584001750359,62.7432475923838));
#184285=CARTESIAN_POINT('Ctrl Pts',(122.743379339098,11.4614950219372,62.5776001878554));
#184286=CARTESIAN_POINT('Ctrl Pts',(122.29285359685,11.7631683164195,62.4967919984508));
#184287=CARTESIAN_POINT('Ctrl Pts',(121.404162725771,12.2846322865785,62.3362733997077));
#184288=CARTESIAN_POINT('Ctrl Pts',(120.96960683995,12.5091320194283,62.2572813338858));
#184289=CARTESIAN_POINT('Ctrl Pts',(120.060775742327,12.9181750767093,62.0918192503852));
#184290=CARTESIAN_POINT('Ctrl Pts',(119.586306221414,13.1004134272832,62.0053087095122));
#184291=CARTESIAN_POINT('Ctrl Pts',(118.195315425746,13.5466241728586,61.7519341860998));
#184292=CARTESIAN_POINT('Ctrl Pts',(117.260151082802,13.7406847319864,61.5820527436966));
#184293=CARTESIAN_POINT('Ctrl Pts',(116.04439728924,13.861072793064,61.3608528118971));
#184294=CARTESIAN_POINT('Ctrl Pts',(115.775250170044,13.8795782638137,61.3118446162619));
#184295=CARTESIAN_POINT('Ctrl Pts',(114.913034024137,13.9128676342894,61.1545495648881));
#184296=CARTESIAN_POINT('Ctrl Pts',(114.319565819352,13.8965307205244,61.0457880281624));
#184297=CARTESIAN_POINT('Ctrl Pts',(113.245906885706,13.7957133502246,60.8492540105891));
#184298=CARTESIAN_POINT('Ctrl Pts',(112.765518849037,13.7242469493173,60.7614011010939));
#184299=CARTESIAN_POINT('Ctrl Pts',(111.685322670308,13.503367218759,60.5643911481585));
#184300=CARTESIAN_POINT('Ctrl Pts',(111.089648626595,13.3383375189148,60.4561504802148));
#184301=CARTESIAN_POINT('Ctrl Pts',(109.99776166544,12.9536271210321,60.2582703242228));
#184302=CARTESIAN_POINT('Ctrl Pts',(109.499440057304,12.7438116788286,60.1681709780323));
#184303=CARTESIAN_POINT('Ctrl Pts',(108.576410199111,12.2885127699548,60.0009762219196));
#184304=CARTESIAN_POINT('Ctrl Pts',(108.149895260732,12.0487187087438,59.9235464531746));
#184305=CARTESIAN_POINT('Ctrl Pts',(107.306974834155,11.5132291035049,59.770895615366));
#184306=CARTESIAN_POINT('Ctrl Pts',(106.892338827584,11.2160690548295,59.6960157522552));
#184307=CARTESIAN_POINT('Ctrl Pts',(105.748255525778,10.2955095149837,59.490636811986));
#184308=CARTESIAN_POINT('Ctrl Pts',(105.065145034467,9.61726589596268,59.3697513499223));
#184309=CARTESIAN_POINT('Ctrl Pts',(104.284373986162,8.66154336740987,59.2331048386539));
#184310=CARTESIAN_POINT('Ctrl Pts',(104.118177886365,8.44542689187018,59.2041080132545));
#184311=CARTESIAN_POINT('Ctrl Pts',(103.606088880832,7.7373363137978,59.1148865726734));
#184312=CARTESIAN_POINT('Ctrl Pts',(103.285444400724,7.22741273759473,59.0591706368313));
#184313=CARTESIAN_POINT('Ctrl Pts',(102.764153800281,6.26596019965551,58.9700200913392));
#184314=CARTESIAN_POINT('Ctrl Pts',(102.552653497572,5.8216494695253,58.9344326041966));
#184315=CARTESIAN_POINT('Ctrl Pts',(102.123916224237,4.78411018662792,58.8641116583317));
#184316=CARTESIAN_POINT('Ctrl Pts',(101.922322452508,4.18538019375447,58.8325372374376));
#184317=CARTESIAN_POINT('Ctrl Pts',(101.623149665034,3.05050736773772,58.7887482353137));
#184318=CARTESIAN_POINT('Ctrl Pts',(101.515164850384,2.51842728831526,58.7744579515986));
#184319=CARTESIAN_POINT('Ctrl Pts',(101.368885248289,1.49967186218422,58.7580890921657));
#184320=CARTESIAN_POINT('Ctrl Pts',(101.324659557079,1.01467517101568,58.7548810859808));
#184321=CARTESIAN_POINT('Ctrl Pts',(101.285112281498,0.0114122663443761,
58.7583228663086));
#184322=CARTESIAN_POINT('Ctrl Pts',(101.293079029211,-0.506241660897844,
58.7656095365548));
#184323=CARTESIAN_POINT('Ctrl Pts',(101.398004428674,-2.00028658790661,
58.8031822068209));
#184324=CARTESIAN_POINT('Ctrl Pts',(101.567963780223,-2.96801928523241,
58.8482895099458));
#184325=CARTESIAN_POINT('Ctrl Pts',(101.910574633612,-4.16888091616166,
58.9301184296819));
#184326=CARTESIAN_POINT('Ctrl Pts',(101.992103359967,-4.42630460544285,
58.9492298026959));
#184327=CARTESIAN_POINT('Ctrl Pts',(102.255238441565,-5.18079723970398,
59.0097829781108));
#184328=CARTESIAN_POINT('Ctrl Pts',(102.457520147463,-5.66982859382182,
59.0549538480031));
#184329=CARTESIAN_POINT('Ctrl Pts',(102.90556751856,-6.6002090175857,59.1535439611523));
#184330=CARTESIAN_POINT('Ctrl Pts',(103.148609140187,-7.04201895481002,
59.2064251158288));
#184331=CARTESIAN_POINT('Ctrl Pts',(103.887615213688,-8.22840482019988,
59.3662531375783));
#184332=CARTESIAN_POINT('Ctrl Pts',(104.431623533809,-8.93876189614676,
59.483025537428));
#184333=CARTESIAN_POINT('Ctrl Pts',(105.237619187511,-9.80311033484269,
59.6542754953128));
#184334=CARTESIAN_POINT('Ctrl Pts',(105.442623035857,-10.0094114411752,
59.6976895506399));
#184335=CARTESIAN_POINT('Ctrl Pts',(106.117163864108,-10.6463276054636,
59.8398879420105));
#184336=CARTESIAN_POINT('Ctrl Pts',(106.609823911186,-11.0502853987451,
59.9426924543749));
#184337=CARTESIAN_POINT('Ctrl Pts',(107.523221854039,-11.6979896699392,
60.1328517011599));
#184338=CARTESIAN_POINT('Ctrl Pts',(107.932543165812,-11.9565322526303,
60.2179289757807));
#184339=CARTESIAN_POINT('Ctrl Pts',(108.967397295296,-12.5351469137784,
60.4330520455173));
#184340=CARTESIAN_POINT('Ctrl Pts',(109.605317936245,-12.8291602920116,
60.5657223077177));
#184341=CARTESIAN_POINT('Ctrl Pts',(110.724017809939,-13.2422308406029,
60.7980531082487));
#184342=CARTESIAN_POINT('Ctrl Pts',(111.194200639975,-13.3870156589866,
60.8955857317533));
#184343=CARTESIAN_POINT('Ctrl Pts',(111.932428159116,-13.570514401821,61.0480714609832));
#184344=CARTESIAN_POINT('Ctrl Pts',(112.195614063017,-13.6275518090732,
61.1023215125712));
#184345=CARTESIAN_POINT('Ctrl Pts',(113.26277014282,-13.8252777392009,61.3221063681588));
#184346=CARTESIAN_POINT('Ctrl Pts',(114.076510955031,-13.9,61.4893881436234));
#184347=CARTESIAN_POINT('Ctrl Pts',(114.891525389284,-13.9,61.6575251889163));
#184348=CARTESIAN_POINT('Origin',(114.885904346743,1.45439216225896E-14,
61.6864428015861));
#184349=CARTESIAN_POINT('',(115.190201331893,-11.58843628952,60.1209783366866));
#184350=CARTESIAN_POINT('',(115.190201331893,11.5884362895886,60.1209783366842));
#184351=CARTESIAN_POINT('Origin',(115.190201331893,1.45439216225896E-14,
60.1209783366866));
#184352=CARTESIAN_POINT('',(114.581607361595,11.6998171366511,63.251907266478));
#184353=CARTESIAN_POINT('',(114.885904346743,11.64412671312,61.6864428015861));
#184354=CARTESIAN_POINT('Origin',(114.581607361595,1.45439216225896E-14,
63.2519072664759));
#184355=CARTESIAN_POINT('Origin',(115.190201331893,1.45439216225896E-14,
60.1209783366866));
#184356=CARTESIAN_POINT('Origin',(115.185539912945,1.45439216225896E-14,
60.1449591385841));
#184357=CARTESIAN_POINT('',(115.27674466279,-11.40026076189,59.6757537179573));
#184358=CARTESIAN_POINT('Origin',(115.185539912945,-10.88886271061,60.1449591385841));
#184359=CARTESIAN_POINT('Origin',(115.27674466279,1.45439216225896E-14,
59.6757537179573));
#184360=CARTESIAN_POINT('Origin',(115.446124912502,1.45439216225896E-14,
58.8043722225089));
#184361=CARTESIAN_POINT('',(115.446124912502,-11.05,58.8043722225089));
#184362=CARTESIAN_POINT('Origin',(115.446124912502,-12.35,58.8043722225089));
#184363=CARTESIAN_POINT('Origin',(115.446124912502,1.45439216225896E-14,
58.8043722225089));
#184364=CARTESIAN_POINT('Origin',(120.341492634982,15.3,58.5138990734244));
#184365=CARTESIAN_POINT('',(120.484600069656,-9.97697348898956,57.7776788196001));
#184366=CARTESIAN_POINT('',(120.198385200308,-9.97697348898956,59.2501193272487));
#184367=CARTESIAN_POINT('Ctrl Pts',(120.198385200308,-9.97697348898973,
59.2501193272487));
#184368=CARTESIAN_POINT('Ctrl Pts',(120.292749480214,-9.93120612242623,
59.2684619766829));
#184369=CARTESIAN_POINT('Ctrl Pts',(120.396910139201,-9.88061692723551,
59.268852030833));
#184370=CARTESIAN_POINT('Ctrl Pts',(120.597619254378,-9.7837357700295,59.2262362233364));
#184371=CARTESIAN_POINT('Ctrl Pts',(120.694200988075,-9.73750614463925,
59.1832454067965));
#184372=CARTESIAN_POINT('Ctrl Pts',(120.847180488313,-9.66686754951251,
59.0747124853458));
#184373=CARTESIAN_POINT('Ctrl Pts',(120.916107916634,-9.63634449458131,
59.0055914641224));
#184374=CARTESIAN_POINT('Ctrl Pts',(121.022448949448,-9.59481532313076,
58.842901490205));
#184375=CARTESIAN_POINT('Ctrl Pts',(121.059784384477,-9.58397099327854,
58.7492402067744));
#184376=CARTESIAN_POINT('Ctrl Pts',(121.095641393136,-9.58397099327854,
58.5647728094222));
#184377=CARTESIAN_POINT('Ctrl Pts',(121.09611090338,-9.59481532313077,58.4639454803748));
#184378=CARTESIAN_POINT('Ctrl Pts',(121.058458308044,-9.63634449458134,
58.2732658408284));
#184379=CARTESIAN_POINT('Ctrl Pts',(121.020443267736,-9.6668675495125,58.1833572057576));
#184380=CARTESIAN_POINT('Ctrl Pts',(120.91926058826,-9.73750614463925,58.0254199147028));
#184381=CARTESIAN_POINT('Ctrl Pts',(120.845816349612,-9.78373577002951,
57.9493792321698));
#184382=CARTESIAN_POINT('Ctrl Pts',(120.675686475446,-9.88061692723553,
57.8346792675662));
#184383=CARTESIAN_POINT('Ctrl Pts',(120.578964349562,-9.93120612242623,
57.7960214690343));
#184384=CARTESIAN_POINT('Ctrl Pts',(120.484600069656,-9.97697348898973,
57.7776788196001));
#184385=CARTESIAN_POINT('',(120.484600069656,-10.3082491238812,57.7776788196002));
#184386=CARTESIAN_POINT('',(120.484600069656,-9.97697348898999,57.7776788196002));
#184387=CARTESIAN_POINT('',(120.198385200308,-10.3082491238812,59.2501193272487));
#184388=CARTESIAN_POINT('Ctrl Pts',(120.484600069656,-10.3082491238815,
57.7776788196001));
#184389=CARTESIAN_POINT('Ctrl Pts',(120.578839835416,-10.2640110301723,
57.7959972658154));
#184390=CARTESIAN_POINT('Ctrl Pts',(120.675458711172,-10.2151256546928,
57.8345897929314));
#184391=CARTESIAN_POINT('Ctrl Pts',(120.845400127855,-10.1215699520295,
57.9490347799076));
#184392=CARTESIAN_POINT('Ctrl Pts',(120.918755915055,-10.076961159343,58.0248881638909));
#184393=CARTESIAN_POINT('Ctrl Pts',(121.020177899851,-10.008616368515,58.1827179406788));
#184394=CARTESIAN_POINT('Ctrl Pts',(121.058344974172,-9.97903582116519,
58.2728599212221));
#184395=CARTESIAN_POINT('Ctrl Pts',(121.096127121178,-9.93883620340095,
58.4638600184146));
#184396=CARTESIAN_POINT('Ctrl Pts',(121.095641986383,-9.92836844602397,
58.5647697574433));
#184397=CARTESIAN_POINT('Ctrl Pts',(121.059783791229,-9.92836844602397,
58.7492432587533));
#184398=CARTESIAN_POINT('Ctrl Pts',(121.022431971555,-9.93883620340095,
58.8429868044173));
#184399=CARTESIAN_POINT('Ctrl Pts',(120.915850774513,-9.97903582116519,
59.0059253701314));
#184400=CARTESIAN_POINT('Ctrl Pts',(120.846694969659,-10.008616368515,59.0752057921387));
#184401=CARTESIAN_POINT('Ctrl Pts',(120.6935338653,-10.076961159343,59.1835493824068));
#184402=CARTESIAN_POINT('Ctrl Pts',(120.597104305892,-10.1215699520295,
59.2263996735356));
#184403=CARTESIAN_POINT('Ctrl Pts',(120.39666544206,-10.2151256546928,59.2688496678139));
#184404=CARTESIAN_POINT('Ctrl Pts',(120.292624966069,-10.2640110301723,
59.2684377734639));
#184405=CARTESIAN_POINT('Ctrl Pts',(120.198385200308,-10.3082491238815,
59.2501193272487));
#184406=CARTESIAN_POINT('',(120.198385200308,-9.97697348898999,59.2501193272487));
#184407=CARTESIAN_POINT('Origin',(120.341492634982,15.3,58.5138990734244));
#184408=CARTESIAN_POINT('',(120.484600069656,10.3082491238813,57.7776788196002));
#184409=CARTESIAN_POINT('',(120.198385200308,10.3082491238812,59.2501193272487));
#184410=CARTESIAN_POINT('Ctrl Pts',(120.198385200308,10.3082491238815,59.2501193272487));
#184411=CARTESIAN_POINT('Ctrl Pts',(120.292624966069,10.2640110301723,59.2684377734639));
#184412=CARTESIAN_POINT('Ctrl Pts',(120.39666544206,10.2151256546929,59.2688496678139));
#184413=CARTESIAN_POINT('Ctrl Pts',(120.597104305892,10.1215699520295,59.2263996735356));
#184414=CARTESIAN_POINT('Ctrl Pts',(120.6935338653,10.076961159343,59.1835493824068));
#184415=CARTESIAN_POINT('Ctrl Pts',(120.846694969659,10.008616368515,59.0752057921387));
#184416=CARTESIAN_POINT('Ctrl Pts',(120.915850774513,9.97903582116521,59.0059253701314));
#184417=CARTESIAN_POINT('Ctrl Pts',(121.022431971555,9.93883620340097,58.8429868044173));
#184418=CARTESIAN_POINT('Ctrl Pts',(121.059783791229,9.928368446024,58.7492432587533));
#184419=CARTESIAN_POINT('Ctrl Pts',(121.095641986383,9.928368446024,58.5647697574433));
#184420=CARTESIAN_POINT('Ctrl Pts',(121.096127121178,9.93883620340099,58.4638600184146));
#184421=CARTESIAN_POINT('Ctrl Pts',(121.058344974172,9.97903582116522,58.2728599212221));
#184422=CARTESIAN_POINT('Ctrl Pts',(121.020177899851,10.008616368515,58.1827179406788));
#184423=CARTESIAN_POINT('Ctrl Pts',(120.918755915055,10.076961159343,58.0248881638909));
#184424=CARTESIAN_POINT('Ctrl Pts',(120.845400127855,10.1215699520295,57.9490347799076));
#184425=CARTESIAN_POINT('Ctrl Pts',(120.675458711172,10.2151256546929,57.8345897929314));
#184426=CARTESIAN_POINT('Ctrl Pts',(120.578839835416,10.2640110301723,57.7959972658154));
#184427=CARTESIAN_POINT('Ctrl Pts',(120.484600069656,10.3082491238815,57.7776788196001));
#184428=CARTESIAN_POINT('',(120.484600069656,9.97697348898955,57.7776788196002));
#184429=CARTESIAN_POINT('',(120.484600069656,10.30824912388,57.7776788196002));
#184430=CARTESIAN_POINT('',(120.198385200308,9.97697348898959,59.2501193272487));
#184431=CARTESIAN_POINT('Ctrl Pts',(120.484600069656,9.97697348898976,57.7776788196002));
#184432=CARTESIAN_POINT('Ctrl Pts',(120.576159926688,9.93256628805063,57.7954763417287));
#184433=CARTESIAN_POINT('Ctrl Pts',(120.670285760103,9.88345309913906,57.8324795460311));
#184434=CARTESIAN_POINT('Ctrl Pts',(120.836868483474,9.78905064146605,57.9420247394531));
#184435=CARTESIAN_POINT('Ctrl Pts',(120.909354963944,9.74381820661306,58.01457069919));
#184436=CARTESIAN_POINT('Ctrl Pts',(121.013972591701,9.67185393609447,58.1696730234398));
#184437=CARTESIAN_POINT('Ctrl Pts',(121.054855180413,9.63958427480582,58.2616338615531));
#184438=CARTESIAN_POINT('Ctrl Pts',(121.096047489807,9.59555522790789,58.4575893251544));
#184439=CARTESIAN_POINT('Ctrl Pts',(121.096249195621,9.58397099327857,58.5616459523084));
#184440=CARTESIAN_POINT('Ctrl Pts',(121.059784384477,9.58397099327857,58.7492402067744));
#184441=CARTESIAN_POINT('Ctrl Pts',(121.022448949448,9.59481532313079,58.842901490205));
#184442=CARTESIAN_POINT('Ctrl Pts',(120.916107916634,9.63634449458134,59.0055914641224));
#184443=CARTESIAN_POINT('Ctrl Pts',(120.847180488313,9.66686754951253,59.0747124853458));
#184444=CARTESIAN_POINT('Ctrl Pts',(120.694200988075,9.73750614463928,59.1832454067965));
#184445=CARTESIAN_POINT('Ctrl Pts',(120.597619254378,9.78373577002953,59.2262362233364));
#184446=CARTESIAN_POINT('Ctrl Pts',(120.396910139201,9.88061692723554,59.268852030833));
#184447=CARTESIAN_POINT('Ctrl Pts',(120.292749480214,9.93120612242626,59.2684619766829));
#184448=CARTESIAN_POINT('Ctrl Pts',(120.198385200308,9.97697348898976,59.2501193272487));
#184449=CARTESIAN_POINT('',(120.198385200308,10.30824912388,59.2501193272487));
#184450=CARTESIAN_POINT('Origin',(113.780205727422,1.45439216225896E-14,
67.3747406878918));
#184451=CARTESIAN_POINT('',(115.535656926088,-11.05,58.3437722409808));
#184452=CARTESIAN_POINT('',(113.780205727422,-11.05,67.3747406878918));
#184453=CARTESIAN_POINT('',(110.872928651868,-9.97697348898956,57.4374251547129));
#184454=CARTESIAN_POINT('Origin',(115.535656926088,1.45439216225896E-14,
58.3437722409808));
#184455=CARTESIAN_POINT('',(111.159143521215,-9.97697348898956,55.9649846470644));
#184456=CARTESIAN_POINT('Ctrl Pts',(110.872928651867,-9.97697348898916,
57.4374251547129));
#184457=CARTESIAN_POINT('Ctrl Pts',(110.778564371961,-9.93120612242566,
57.4190825052788));
#184458=CARTESIAN_POINT('Ctrl Pts',(110.681842246077,-9.88061692723491,
57.3804247067468));
#184459=CARTESIAN_POINT('Ctrl Pts',(110.511712371911,-9.78373577002886,
57.2657247421432));
#184460=CARTESIAN_POINT('Ctrl Pts',(110.438268133263,-9.7375061446386,57.1896840596102));
#184461=CARTESIAN_POINT('Ctrl Pts',(110.337085453787,-9.66686754951184,
57.0317467685554));
#184462=CARTESIAN_POINT('Ctrl Pts',(110.299070413479,-9.63634449458064,
56.9418381334846));
#184463=CARTESIAN_POINT('Ctrl Pts',(110.261417818143,-9.59481532313007,
56.7511584939382));
#184464=CARTESIAN_POINT('Ctrl Pts',(110.261887328387,-9.58397099327785,
56.6503311648909));
#184465=CARTESIAN_POINT('Ctrl Pts',(110.279815832717,-9.58397099327785,
56.5580974662147));
#184466=CARTESIAN_POINT('Ctrl Pts',(110.297744337046,-9.58397099327785,
56.4658637675386));
#184467=CARTESIAN_POINT('Ctrl Pts',(110.335079772075,-9.59481532313008,
56.372202484108));
#184468=CARTESIAN_POINT('Ctrl Pts',(110.441420804889,-9.63634449458065,
56.2095125101906));
#184469=CARTESIAN_POINT('Ctrl Pts',(110.51034823321,-9.66686754951184,56.1403914889672));
#184470=CARTESIAN_POINT('Ctrl Pts',(110.663327733448,-9.7375061446386,56.0318585675165));
#184471=CARTESIAN_POINT('Ctrl Pts',(110.759909467145,-9.78373577002887,
55.9888677509767));
#184472=CARTESIAN_POINT('Ctrl Pts',(110.960618582322,-9.88061692723491,
55.94625194348));
#184473=CARTESIAN_POINT('Ctrl Pts',(111.064779241308,-9.93120612242564,
55.9466419976302));
#184474=CARTESIAN_POINT('Ctrl Pts',(111.159143521215,-9.97697348898915,
55.9649846470643));
#184475=CARTESIAN_POINT('',(115.821871795436,-11.05,56.8713317333323));
#184476=CARTESIAN_POINT('Origin',(115.821871795436,1.45439216225896E-14,
56.8713317333323));
#184477=CARTESIAN_POINT('',(117.329270107334,-11.05,49.11647839305));
#184478=CARTESIAN_POINT('',(113.780205727422,-11.05,67.3747406878918));
#184479=CARTESIAN_POINT('Origin',(117.329270107334,1.45439216225896E-14,
49.11647839305));
#184480=CARTESIAN_POINT('Origin',(115.821871795436,1.45439216225896E-14,
56.8713317333323));
#184481=CARTESIAN_POINT('Origin',(115.535656926088,1.45439216225896E-14,
58.3437722409808));
#184482=CARTESIAN_POINT('',(106.028205189487,-4.7499999999999,54.9676262909075));
#184483=CARTESIAN_POINT('',(106.028205189487,4.74999999999992,54.9676262909075));
#184484=CARTESIAN_POINT('Origin',(115.821871795436,1.45439216225896E-14,
56.8713317333323));
#184485=CARTESIAN_POINT('',(105.741990320139,-4.7499999999999,56.440066798556));
#184486=CARTESIAN_POINT('Ctrl Pts',(106.028205189487,-4.75,54.9676262909075));
#184487=CARTESIAN_POINT('Ctrl Pts',(106.073131672458,-4.84613048481368,
54.9763591581351));
#184488=CARTESIAN_POINT('Ctrl Pts',(106.119072126072,-4.94845182674208,
55.0051459502539));
#184489=CARTESIAN_POINT('Ctrl Pts',(106.198883665765,-5.13734179585313,
55.102289721472));
#184490=CARTESIAN_POINT('Ctrl Pts',(106.232695166959,-5.22394595989023,
55.1706265418024));
#184491=CARTESIAN_POINT('Ctrl Pts',(106.276137509157,-5.35340561126171,
55.3173401922386));
#184492=CARTESIAN_POINT('Ctrl Pts',(106.290643570149,-5.40787766025428,
55.4026791218385));
#184493=CARTESIAN_POINT('Ctrl Pts',(106.297065507605,-5.48122203006144,
55.5872881061577));
#184494=CARTESIAN_POINT('Ctrl Pts',(106.288808122004,-5.5,55.6866016180312));
#184495=CARTESIAN_POINT('Ctrl Pts',(106.25234331086,-5.5,55.8741958724972));
#184496=CARTESIAN_POINT('Ctrl Pts',(106.221489017615,-5.47994696416173,
55.972215794829));
#184497=CARTESIAN_POINT('Ctrl Pts',(106.143065389029,-5.4021212359169,56.144920159399));
#184498=CARTESIAN_POINT('Ctrl Pts',(106.095652440797,-5.34444274328869,
56.219717998098));
#184499=CARTESIAN_POINT('Ctrl Pts',(105.999768021207,-5.21215219369169,
56.3358464779124));
#184500=CARTESIAN_POINT('Ctrl Pts',(105.94441759979,-5.12715501869964,56.383543337138));
#184501=CARTESIAN_POINT('Ctrl Pts',(105.837296341422,-4.94273061003997,
56.4398856004814));
#184502=CARTESIAN_POINT('Ctrl Pts',(105.785581627802,-4.84327357189262,
56.4485401326993));
#184503=CARTESIAN_POINT('Ctrl Pts',(105.741990320139,-4.75,56.440066798556));
#184504=CARTESIAN_POINT('',(105.741990320139,4.74999999999992,56.440066798556));
#184505=CARTESIAN_POINT('Origin',(115.535656926088,1.45439216225896E-14,
58.3437722409808));
#184506=CARTESIAN_POINT('Ctrl Pts',(105.741990320139,4.75,56.440066798556));
#184507=CARTESIAN_POINT('Ctrl Pts',(105.78691680311,4.84613048481368,56.4487996657836));
#184508=CARTESIAN_POINT('Ctrl Pts',(105.840295789827,4.94845182674209,56.4393187135207));
#184509=CARTESIAN_POINT('Ctrl Pts',(105.950686570531,5.13734179585313,56.3791467126385));
#184510=CARTESIAN_POINT('Ctrl Pts',(106.007635566774,5.22394595989023,56.3284520338962));
#184511=CARTESIAN_POINT('Ctrl Pts',(106.102874729734,5.35340561126171,56.2086954718268));
#184512=CARTESIAN_POINT('Ctrl Pts',(106.148293178739,5.40787766025429,56.1350047451325));
#184513=CARTESIAN_POINT('Ctrl Pts',(106.223403553673,5.48122203006144,55.9662441159878));
#184514=CARTESIAN_POINT('Ctrl Pts',(106.252951113345,5.5,55.8710690153834));
#184515=CARTESIAN_POINT('Ctrl Pts',(106.270879617674,5.5,55.7788353167073));
#184516=CARTESIAN_POINT('Ctrl Pts',(106.288808122004,5.5,55.6866016180312));
#184517=CARTESIAN_POINT('Ctrl Pts',(106.297065507605,5.48122203006144,55.5872881061577));
#184518=CARTESIAN_POINT('Ctrl Pts',(106.290643570149,5.40787766025429,55.4026791218385));
#184519=CARTESIAN_POINT('Ctrl Pts',(106.276137509157,5.35340561126171,55.3173401922386));
#184520=CARTESIAN_POINT('Ctrl Pts',(106.232695166959,5.22394595989023,55.1706265418024));
#184521=CARTESIAN_POINT('Ctrl Pts',(106.198883665765,5.13734179585313,55.102289721472));
#184522=CARTESIAN_POINT('Ctrl Pts',(106.119072126072,4.94845182674209,55.0051459502538));
#184523=CARTESIAN_POINT('Ctrl Pts',(106.073131672458,4.84613048481368,54.9763591581351));
#184524=CARTESIAN_POINT('Ctrl Pts',(106.028205189487,4.75,54.9676262909075));
#184525=CARTESIAN_POINT('',(125.329323532037,4.74999999999993,60.2474776834056));
#184526=CARTESIAN_POINT('',(125.329323532037,-4.7499999999999,60.2474776834056));
#184527=CARTESIAN_POINT('Origin',(115.535656926088,1.45439216225896E-14,
58.3437722409808));
#184528=CARTESIAN_POINT('',(125.615538401385,-4.7499999999999,58.775037175757));
#184529=CARTESIAN_POINT('Ctrl Pts',(125.329323532037,-4.75,60.2474776834055));
#184530=CARTESIAN_POINT('Ctrl Pts',(125.285732224375,-4.84327357189262,
60.2390043492623));
#184531=CARTESIAN_POINT('Ctrl Pts',(125.24102527291,-4.94273061003997,60.2116072504476));
#184532=CARTESIAN_POINT('Ctrl Pts',(125.162810527679,-5.12715501869964,
60.1192391376523));
#184533=CARTESIAN_POINT('Ctrl Pts',(125.129358189981,-5.21215219369169,
60.0542806845177));
#184534=CARTESIAN_POINT('Ctrl Pts',(125.083958466883,-5.34444274328869,
59.9106892123244));
#184535=CARTESIAN_POINT('Ctrl Pts',(125.068017873183,-5.4021212359169,59.8235766311058));
#184536=CARTESIAN_POINT('Ctrl Pts',(125.060001298882,-5.47994696416173,
59.6340699093286));
#184537=CARTESIAN_POINT('Ctrl Pts',(125.068112797035,-5.5,59.5316292133956));
#184538=CARTESIAN_POINT('Ctrl Pts',(125.104577608179,-5.5,59.3440349589296));
#184539=CARTESIAN_POINT('Ctrl Pts',(125.134125167851,-5.48122203006144,
59.2488598583252));
#184540=CARTESIAN_POINT('Ctrl Pts',(125.209235542785,-5.40787766025429,
59.0800992291805));
#184541=CARTESIAN_POINT('Ctrl Pts',(125.25465399179,-5.35340561126171,59.0064085024862));
#184542=CARTESIAN_POINT('Ctrl Pts',(125.34989315475,-5.22394595989023,58.8866519404169));
#184543=CARTESIAN_POINT('Ctrl Pts',(125.406842150993,-5.13734179585313,
58.8359572616745));
#184544=CARTESIAN_POINT('Ctrl Pts',(125.517232931697,-4.94845182674209,
58.7757852607923));
#184545=CARTESIAN_POINT('Ctrl Pts',(125.570611918414,-4.84613048481368,
58.7663043085294));
#184546=CARTESIAN_POINT('Ctrl Pts',(125.615538401385,-4.75,58.775037175757));
#184547=CARTESIAN_POINT('',(125.615538401385,4.74999999999992,58.775037175757));
#184548=CARTESIAN_POINT('Origin',(115.821871795436,1.45439216225896E-14,
56.8713317333323));
#184549=CARTESIAN_POINT('Ctrl Pts',(125.615538401385,4.75,58.775037175757));
#184550=CARTESIAN_POINT('Ctrl Pts',(125.570611918414,4.84613048481368,58.7663043085294));
#184551=CARTESIAN_POINT('Ctrl Pts',(125.517232931697,4.94845182674209,58.7757852607923));
#184552=CARTESIAN_POINT('Ctrl Pts',(125.406842150993,5.13734179585314,58.8359572616745));
#184553=CARTESIAN_POINT('Ctrl Pts',(125.34989315475,5.22394595989023,58.8866519404169));
#184554=CARTESIAN_POINT('Ctrl Pts',(125.25465399179,5.35340561126171,59.0064085024862));
#184555=CARTESIAN_POINT('Ctrl Pts',(125.209235542785,5.40787766025429,59.0800992291805));
#184556=CARTESIAN_POINT('Ctrl Pts',(125.134125167851,5.48122203006144,59.2488598583252));
#184557=CARTESIAN_POINT('Ctrl Pts',(125.104577608179,5.5,59.3440349589296));
#184558=CARTESIAN_POINT('Ctrl Pts',(125.08664910385,5.5,59.4362686576057));
#184559=CARTESIAN_POINT('Ctrl Pts',(125.06872059952,5.5,59.5285023562819));
#184560=CARTESIAN_POINT('Ctrl Pts',(125.060463213919,5.48122203006144,59.6278158681553));
#184561=CARTESIAN_POINT('Ctrl Pts',(125.066885151375,5.40787766025429,59.8124248524745));
#184562=CARTESIAN_POINT('Ctrl Pts',(125.081391212367,5.35340561126171,59.8977637820744));
#184563=CARTESIAN_POINT('Ctrl Pts',(125.124833554565,5.22394595989023,60.0444774325106));
#184564=CARTESIAN_POINT('Ctrl Pts',(125.158645055759,5.13734179585314,60.112814252841));
#184565=CARTESIAN_POINT('Ctrl Pts',(125.238456595452,4.94845182674209,60.2099580240592));
#184566=CARTESIAN_POINT('Ctrl Pts',(125.284397049066,4.84613048481368,60.238744816178));
#184567=CARTESIAN_POINT('Ctrl Pts',(125.329323532037,4.75,60.2474776834055));
#184568=CARTESIAN_POINT('',(111.159143521215,9.97697348898959,55.9649846470644));
#184569=CARTESIAN_POINT('Origin',(115.821871795436,1.45439216225896E-14,
56.8713317333323));
#184570=CARTESIAN_POINT('',(110.872928651868,9.97697348898959,57.4374251547129));
#184571=CARTESIAN_POINT('Ctrl Pts',(111.159143521215,9.97697348898918,55.9649846470643));
#184572=CARTESIAN_POINT('Ctrl Pts',(111.064779241308,9.93120612242567,55.9466419976301));
#184573=CARTESIAN_POINT('Ctrl Pts',(110.960618582322,9.88061692723494,55.94625194348));
#184574=CARTESIAN_POINT('Ctrl Pts',(110.759909467145,9.7837357700289,55.9888677509767));
#184575=CARTESIAN_POINT('Ctrl Pts',(110.663327733448,9.73750614463863,56.0318585675165));
#184576=CARTESIAN_POINT('Ctrl Pts',(110.51034823321,9.66686754951186,56.1403914889672));
#184577=CARTESIAN_POINT('Ctrl Pts',(110.441420804889,9.63634449458068,56.2095125101906));
#184578=CARTESIAN_POINT('Ctrl Pts',(110.335079772075,9.59481532313011,56.372202484108));
#184579=CARTESIAN_POINT('Ctrl Pts',(110.297744337046,9.58397099327788,56.4658637675386));
#184580=CARTESIAN_POINT('Ctrl Pts',(110.279815832717,9.58397099327788,56.5580974662147));
#184581=CARTESIAN_POINT('Ctrl Pts',(110.261887328387,9.58397099327788,56.6503311648909));
#184582=CARTESIAN_POINT('Ctrl Pts',(110.261417818143,9.5948153231301,56.7511584939382));
#184583=CARTESIAN_POINT('Ctrl Pts',(110.299070413479,9.63634449458067,56.9418381334846));
#184584=CARTESIAN_POINT('Ctrl Pts',(110.337085453787,9.66686754951186,57.0317467685554));
#184585=CARTESIAN_POINT('Ctrl Pts',(110.438268133263,9.73750614463863,57.1896840596102));
#184586=CARTESIAN_POINT('Ctrl Pts',(110.511712371911,9.78373577002889,57.2657247421432));
#184587=CARTESIAN_POINT('Ctrl Pts',(110.681842246077,9.88061692723494,57.3804247067468));
#184588=CARTESIAN_POINT('Ctrl Pts',(110.778564371961,9.93120612242567,57.4190825052787));
#184589=CARTESIAN_POINT('Ctrl Pts',(110.872928651867,9.97697348898919,57.4374251547129));
#184590=CARTESIAN_POINT('Origin',(115.535656926088,1.45439216225896E-14,
58.3437722409808));
#184591=CARTESIAN_POINT('Origin',(130.697657538777,-4.75,60.5269436545036));
#184592=CARTESIAN_POINT('',(125.940727510726,-4.75000000000024,58.8382478507961));
#184593=CARTESIAN_POINT('',(125.654512641378,-4.75000000000024,60.3106883584446));
#184594=CARTESIAN_POINT('Ctrl Pts',(125.654512641378,-4.75,60.3106883584446));
#184595=CARTESIAN_POINT('Ctrl Pts',(125.61230630101,-4.84330877665233,60.3024842360155));
#184596=CARTESIAN_POINT('Ctrl Pts',(125.569148299058,-4.94281444512932,
60.2753683060694));
#184597=CARTESIAN_POINT('Ctrl Pts',(125.493987021831,-5.12726283579728,
60.1835533615843));
#184598=CARTESIAN_POINT('Ctrl Pts',(125.462039039804,-5.21223335422367,
60.1188649340508));
#184599=CARTESIAN_POINT('Ctrl Pts',(125.419010017904,-5.34458926875733,
59.9756676934244));
#184600=CARTESIAN_POINT('Ctrl Pts',(125.404170373857,-5.40227743227456,
59.8886474008104));
#184601=CARTESIAN_POINT('Ctrl Pts',(125.397688170697,-5.4800270257108,59.6994100150999));
#184602=CARTESIAN_POINT('Ctrl Pts',(125.406220154262,-5.5,59.597150653446));
#184603=CARTESIAN_POINT('Ctrl Pts',(125.442648041529,-5.5,59.4097463549116));
#184604=CARTESIAN_POINT('Ctrl Pts',(125.471841952088,-5.4812216429014,59.3144170644385));
#184605=CARTESIAN_POINT('Ctrl Pts',(125.545702507498,-5.40768895518066,
59.1451182185494));
#184606=CARTESIAN_POINT('Ctrl Pts',(125.590233936868,-5.35302314086569,
59.0710512789374));
#184607=CARTESIAN_POINT('Ctrl Pts',(125.683192588985,-5.22334909571738,
58.9510054589944));
#184608=CARTESIAN_POINT('Ctrl Pts',(125.738518670655,-5.13686749643077,
58.9001654212853));
#184609=CARTESIAN_POINT('Ctrl Pts',(125.845604198444,-4.94821117453347,
58.8395692861344));
#184610=CARTESIAN_POINT('Ctrl Pts',(125.897302203287,-4.84600364015159,
58.8298067839887));
#184611=CARTESIAN_POINT('Ctrl Pts',(125.940727510726,-4.75,58.8382478507961));
#184612=CARTESIAN_POINT('',(125.940727510725,-4.75,58.8382478507959));
#184613=CARTESIAN_POINT('',(125.654512641377,-4.75,60.3106883584444));
#184614=CARTESIAN_POINT('Origin',(130.697657538777,-4.75,60.5269436545036));
#184615=CARTESIAN_POINT('',(105.703016080146,-4.75000000000024,54.9044156158684));
#184616=CARTESIAN_POINT('',(106.028205189486,-4.75,54.9676262909074));
#184617=CARTESIAN_POINT('',(105.416801210798,-4.75000000000024,56.376856123517));
#184618=CARTESIAN_POINT('Ctrl Pts',(105.703016080146,-4.75,54.9044156158684));
#184619=CARTESIAN_POINT('Ctrl Pts',(105.746441387585,-4.84600364015159,
54.9128566826758));
#184620=CARTESIAN_POINT('Ctrl Pts',(105.790717792192,-4.94821117453345,
54.9412748132961));
#184621=CARTESIAN_POINT('Ctrl Pts',(105.867305872833,-5.13686749643076,
55.0375736593997));
#184622=CARTESIAN_POINT('Ctrl Pts',(105.899558182295,-5.22334909571738,
55.1054372968028));
#184623=CARTESIAN_POINT('Ctrl Pts',(105.940777714848,-5.35302314086569,
55.2515648439157));
#184624=CARTESIAN_POINT('Ctrl Pts',(105.954320413686,-5.40768895518066,
55.3369203068544));
#184625=CARTESIAN_POINT('Ctrl Pts',(105.95938191906,-5.4812216429014,55.5215601238718));
#184626=CARTESIAN_POINT('Ctrl Pts',(105.950738875149,-5.5,55.6208841180915));
#184627=CARTESIAN_POINT('Ctrl Pts',(105.914310987882,-5.5,55.8082884166259));
#184628=CARTESIAN_POINT('Ctrl Pts',(105.883914490959,-5.4800270257108,55.9062977262052));
#184629=CARTESIAN_POINT('Ctrl Pts',(105.807014400979,-5.40227743227456,
56.0793271551169));
#184630=CARTESIAN_POINT('Ctrl Pts',(105.7606568068,-5.34458926875733,56.1544518502842));
#184631=CARTESIAN_POINT('Ctrl Pts',(105.667118143852,-5.21223335422367,
56.2711028896394));
#184632=CARTESIAN_POINT('Ctrl Pts',(105.613263689509,-5.12726283579729,
56.3191129298369));
#184633=CARTESIAN_POINT('Ctrl Pts',(105.509180776692,-4.94281444512933,
56.3760861593815));
#184634=CARTESIAN_POINT('Ctrl Pts',(105.459007551167,-4.84330877665234,
56.385060245946));
#184635=CARTESIAN_POINT('Ctrl Pts',(105.416801210798,-4.75,56.3768561235169));
#184636=CARTESIAN_POINT('',(105.741990320138,-4.75,56.4400667985559));
#184637=CARTESIAN_POINT('Origin',(113.780205727422,1.45439216225896E-14,
67.3747406878918));
#184638=CARTESIAN_POINT('',(117.291108124754,-11.35,49.3128037940699));
#184639=CARTESIAN_POINT('Origin',(117.291108124754,1.45439216225896E-14,
49.3128037940698));
#184640=CARTESIAN_POINT('',(115.821871795436,-11.35,56.8713317333323));
#184641=CARTESIAN_POINT('',(113.780205727422,-11.35,67.3747406878918));
#184642=CARTESIAN_POINT('',(111.159143521215,-10.3082491238812,55.9649846470643));
#184643=CARTESIAN_POINT('Origin',(115.821871795436,1.45439216225896E-14,
56.8713317333323));
#184644=CARTESIAN_POINT('',(110.872928651867,-10.3082491238812,57.4374251547129));
#184645=CARTESIAN_POINT('Ctrl Pts',(111.159143521215,-10.3082491238809,
55.9649846470643));
#184646=CARTESIAN_POINT('Ctrl Pts',(111.064903755454,-10.2640110301717,
55.9466662008491));
#184647=CARTESIAN_POINT('Ctrl Pts',(110.960863279463,-10.2151256546922,
55.9462543064991));
#184648=CARTESIAN_POINT('Ctrl Pts',(110.760424415631,-10.1215699520289,
55.9887043007774));
#184649=CARTESIAN_POINT('Ctrl Pts',(110.663994856223,-10.0769611593424,
56.0315545919063));
#184650=CARTESIAN_POINT('Ctrl Pts',(110.510833751864,-10.0086163685144,
56.1398981821743));
#184651=CARTESIAN_POINT('Ctrl Pts',(110.44167794701,-9.97903582116453,56.2091786041817));
#184652=CARTESIAN_POINT('Ctrl Pts',(110.335096749968,-9.93883620340028,
56.3721171698957));
#184653=CARTESIAN_POINT('Ctrl Pts',(110.297744930294,-9.92836844602331,
56.4658607155597));
#184654=CARTESIAN_POINT('Ctrl Pts',(110.279815832717,-9.92836844602331,
56.5580974662147));
#184655=CARTESIAN_POINT('Ctrl Pts',(110.26188673514,-9.92836844602331,56.6503342168697));
#184656=CARTESIAN_POINT('Ctrl Pts',(110.261401600345,-9.93883620340028,
56.7512439558984));
#184657=CARTESIAN_POINT('Ctrl Pts',(110.299183747351,-9.97903582116453,
56.9422440530909));
#184658=CARTESIAN_POINT('Ctrl Pts',(110.337350821672,-10.0086163685144,
57.0323860336342));
#184659=CARTESIAN_POINT('Ctrl Pts',(110.438772806468,-10.0769611593424,
57.1902158104221));
#184660=CARTESIAN_POINT('Ctrl Pts',(110.512128593668,-10.1215699520289,
57.2660691944054));
#184661=CARTESIAN_POINT('Ctrl Pts',(110.682070010351,-10.2151256546922,
57.3805141813816));
#184662=CARTESIAN_POINT('Ctrl Pts',(110.778688886107,-10.2640110301717,
57.4191067084976));
#184663=CARTESIAN_POINT('Ctrl Pts',(110.872928651867,-10.308249123881,57.4374251547129));
#184664=CARTESIAN_POINT('',(115.535656926088,-11.35,58.3437722409808));
#184665=CARTESIAN_POINT('Origin',(115.535656926088,1.45439216225896E-14,
58.3437722409808));
#184666=CARTESIAN_POINT('',(115.446124912503,-11.35,58.804372222509));
#184667=CARTESIAN_POINT('',(113.780205727422,-11.35,67.3747406878918));
#184668=CARTESIAN_POINT('Origin',(115.446124912502,1.45439216225896E-14,
58.8043722225089));
#184669=CARTESIAN_POINT('Origin',(115.535656926088,1.45439216225896E-14,
58.3437722409808));
#184670=CARTESIAN_POINT('Origin',(115.821871795436,1.45439216225896E-14,
56.8713317333323));
#184671=CARTESIAN_POINT('',(125.940727510726,4.75000000000027,58.8382478507961));
#184672=CARTESIAN_POINT('Origin',(115.821871795436,1.45439216225896E-14,
56.8713317333323));
#184673=CARTESIAN_POINT('',(125.654512641378,4.75000000000027,60.3106883584446));
#184674=CARTESIAN_POINT('Origin',(115.535656926088,1.45439216225896E-14,
58.3437722409808));
#184675=CARTESIAN_POINT('Ctrl Pts',(125.654512641378,4.75,60.3106883584447));
#184676=CARTESIAN_POINT('Ctrl Pts',(125.61230630101,4.84330877665233,60.3024842360155));
#184677=CARTESIAN_POINT('Ctrl Pts',(125.569148299058,4.94281444512933,60.2753683060694));
#184678=CARTESIAN_POINT('Ctrl Pts',(125.493987021832,5.12726283579729,60.1835533615843));
#184679=CARTESIAN_POINT('Ctrl Pts',(125.462039039804,5.21223335422367,60.1188649340508));
#184680=CARTESIAN_POINT('Ctrl Pts',(125.419010017904,5.34458926875732,59.9756676934244));
#184681=CARTESIAN_POINT('Ctrl Pts',(125.404170373857,5.40227743227456,59.8886474008104));
#184682=CARTESIAN_POINT('Ctrl Pts',(125.397688170697,5.4800270257108,59.6994100150999));
#184683=CARTESIAN_POINT('Ctrl Pts',(125.406220154262,5.5,59.597150653446));
#184684=CARTESIAN_POINT('Ctrl Pts',(125.424718943952,5.5,59.5019831055666));
#184685=CARTESIAN_POINT('Ctrl Pts',(125.442648041529,5.5,59.4097463549116));
#184686=CARTESIAN_POINT('Ctrl Pts',(125.471841952088,5.4812216429014,59.3144170644385));
#184687=CARTESIAN_POINT('Ctrl Pts',(125.545702507498,5.40768895518066,59.1451182185494));
#184688=CARTESIAN_POINT('Ctrl Pts',(125.590233936868,5.35302314086569,59.0710512789374));
#184689=CARTESIAN_POINT('Ctrl Pts',(125.683192588985,5.22334909571738,58.9510054589944));
#184690=CARTESIAN_POINT('Ctrl Pts',(125.738518670655,5.13686749643077,58.9001654212853));
#184691=CARTESIAN_POINT('Ctrl Pts',(125.845604198444,4.94821117453347,58.8395692861344));
#184692=CARTESIAN_POINT('Ctrl Pts',(125.897302203287,4.84600364015159,58.8298067839887));
#184693=CARTESIAN_POINT('Ctrl Pts',(125.940727510726,4.75,58.8382478507961));
#184694=CARTESIAN_POINT('',(105.416801210798,4.75000000000027,56.376856123517));
#184695=CARTESIAN_POINT('Origin',(115.535656926088,1.45439216225896E-14,
58.3437722409808));
#184696=CARTESIAN_POINT('',(105.703016080146,4.75000000000027,54.9044156158684));
#184697=CARTESIAN_POINT('Origin',(115.821871795436,1.45439216225896E-14,
56.8713317333323));
#184698=CARTESIAN_POINT('Ctrl Pts',(105.703016080146,4.75,54.9044156158684));
#184699=CARTESIAN_POINT('Ctrl Pts',(105.746441387585,4.84600364015159,54.9128566826759));
#184700=CARTESIAN_POINT('Ctrl Pts',(105.790717792192,4.94821117453345,54.9412748132961));
#184701=CARTESIAN_POINT('Ctrl Pts',(105.867305872833,5.13686749643076,55.0375736593997));
#184702=CARTESIAN_POINT('Ctrl Pts',(105.899558182295,5.22334909571738,55.1054372968028));
#184703=CARTESIAN_POINT('Ctrl Pts',(105.940777714848,5.35302314086569,55.2515648439157));
#184704=CARTESIAN_POINT('Ctrl Pts',(105.954320413686,5.40768895518066,55.3369203068544));
#184705=CARTESIAN_POINT('Ctrl Pts',(105.95938191906,5.4812216429014,55.5215601238718));
#184706=CARTESIAN_POINT('Ctrl Pts',(105.950738875149,5.5,55.6208841180915));
#184707=CARTESIAN_POINT('Ctrl Pts',(105.932809777572,5.5,55.7131208687465));
#184708=CARTESIAN_POINT('Ctrl Pts',(105.914310987882,5.5,55.8082884166259));
#184709=CARTESIAN_POINT('Ctrl Pts',(105.883914490959,5.4800270257108,55.9062977262052));
#184710=CARTESIAN_POINT('Ctrl Pts',(105.807014400979,5.40227743227456,56.0793271551169));
#184711=CARTESIAN_POINT('Ctrl Pts',(105.7606568068,5.34458926875732,56.1544518502842));
#184712=CARTESIAN_POINT('Ctrl Pts',(105.667118143852,5.21223335422367,56.2711028896394));
#184713=CARTESIAN_POINT('Ctrl Pts',(105.613263689509,5.12726283579728,56.3191129298369));
#184714=CARTESIAN_POINT('Ctrl Pts',(105.509180776692,4.94281444512933,56.3760861593815));
#184715=CARTESIAN_POINT('Ctrl Pts',(105.459007551167,4.84330877665233,56.385060245946));
#184716=CARTESIAN_POINT('Ctrl Pts',(105.416801210798,4.75,56.3768561235169));
#184717=CARTESIAN_POINT('',(111.159143521215,10.3082491238812,55.9649846470643));
#184718=CARTESIAN_POINT('Origin',(115.821871795436,1.45439216225896E-14,
56.8713317333323));
#184719=CARTESIAN_POINT('',(110.872928651867,10.3082491238812,57.4374251547129));
#184720=CARTESIAN_POINT('Origin',(115.535656926088,1.45439216225896E-14,
58.3437722409808));
#184721=CARTESIAN_POINT('Ctrl Pts',(110.872928651867,10.308249123881,57.4374251547129));
#184722=CARTESIAN_POINT('Ctrl Pts',(110.778688886107,10.2640110301718,57.4191067084976));
#184723=CARTESIAN_POINT('Ctrl Pts',(110.682070010351,10.2151256546923,57.3805141813816));
#184724=CARTESIAN_POINT('Ctrl Pts',(110.512128593668,10.1215699520289,57.2660691944054));
#184725=CARTESIAN_POINT('Ctrl Pts',(110.438772806468,10.0769611593424,57.1902158104221));
#184726=CARTESIAN_POINT('Ctrl Pts',(110.337350821672,10.0086163685144,57.0323860336342));
#184727=CARTESIAN_POINT('Ctrl Pts',(110.299183747351,9.97903582116456,56.9422440530909));
#184728=CARTESIAN_POINT('Ctrl Pts',(110.261401600345,9.93883620340031,56.7512439558984));
#184729=CARTESIAN_POINT('Ctrl Pts',(110.26188673514,9.92836844602334,56.6503342168697));
#184730=CARTESIAN_POINT('Ctrl Pts',(110.279815832717,9.92836844602334,56.5580974662147));
#184731=CARTESIAN_POINT('Ctrl Pts',(110.297744930294,9.92836844602334,56.4658607155597));
#184732=CARTESIAN_POINT('Ctrl Pts',(110.335096749968,9.93883620340031,56.3721171698957));
#184733=CARTESIAN_POINT('Ctrl Pts',(110.44167794701,9.97903582116456,56.2091786041817));
#184734=CARTESIAN_POINT('Ctrl Pts',(110.510833751864,10.0086163685144,56.1398981821743));
#184735=CARTESIAN_POINT('Ctrl Pts',(110.663994856223,10.0769611593424,56.0315545919063));
#184736=CARTESIAN_POINT('Ctrl Pts',(110.760424415631,10.1215699520289,55.9887043007774));
#184737=CARTESIAN_POINT('Ctrl Pts',(110.960863279463,10.2151256546923,55.9462543064991));
#184738=CARTESIAN_POINT('Ctrl Pts',(111.064903755454,10.2640110301718,55.9466662008491));
#184739=CARTESIAN_POINT('Ctrl Pts',(111.159143521215,10.308249123881,55.9649846470643));
#184740=CARTESIAN_POINT('Origin',(117.291108124754,1.45439216225896E-14,
49.3128037940698));
#184741=CARTESIAN_POINT('',(117.386513081203,-10.84999988564,48.8219902915204));
#184742=CARTESIAN_POINT('Origin',(117.386513081203,1.45439216225896E-14,
48.8219902915203));
#184743=CARTESIAN_POINT('Origin',(117.291108124754,-10.85,49.3128037940698));
#184744=CARTESIAN_POINT('Origin',(113.780205727422,1.45439216225896E-14,
67.3747406878918));
#184745=CARTESIAN_POINT('',(117.291108124754,-9.84999999999999,49.3128037940699));
#184746=CARTESIAN_POINT('Origin',(117.291108124754,1.45439216225896E-14,
49.3128037940698));
#184747=CARTESIAN_POINT('',(117.386513081204,-9.84999999999999,48.8219902915204));
#184748=CARTESIAN_POINT('',(113.780205727422,-9.84999999999999,67.3747406878918));
#184749=CARTESIAN_POINT('Origin',(117.386513081203,1.45439216225896E-14,
48.8219902915203));
#184750=CARTESIAN_POINT('Origin',(113.780205727422,1.45439216225896E-14,
67.3747406878918));
#184751=CARTESIAN_POINT('',(117.329270107334,-10.15,49.11647839305));
#184752=CARTESIAN_POINT('Origin',(117.329270107334,1.45439216225896E-14,
49.11647839305));
#184753=CARTESIAN_POINT('',(117.233865150885,-10.15,49.6072918955995));
#184754=CARTESIAN_POINT('',(113.780205727422,-10.15,67.3747406878918));
#184755=CARTESIAN_POINT('Origin',(117.233865150885,1.45439216225896E-14,
49.6072918955995));
#184756=CARTESIAN_POINT('Origin',(115.446124912502,1.45439216225896E-14,
58.8043722225089));
#184757=CARTESIAN_POINT('',(115.315832412722,-11.6194313553,59.4746656805513));
#184758=CARTESIAN_POINT('Origin',(115.446124912502,-12.35,58.8043722225089));
#184759=CARTESIAN_POINT('Origin',(115.315832412723,1.45439216225896E-14,
59.4746656805514));
#184760=CARTESIAN_POINT('Origin',(115.185539912945,1.45439216225896E-14,
60.1449591385841));
#184761=CARTESIAN_POINT('',(115.192199082871,-11.88825353763,60.1107008501589));
#184762=CARTESIAN_POINT('Origin',(115.185539912945,-10.88886271061,60.1449591385841));
#184763=CARTESIAN_POINT('',(115.192199082871,11.888253537687,60.1107008501569));
#184764=CARTESIAN_POINT('Origin',(115.192199082871,1.45439216225896E-14,
60.110700850159));
#184765=CARTESIAN_POINT('Origin',(115.192199082871,1.45439216225896E-14,
60.110700850159));
#184766=CARTESIAN_POINT('Origin',(114.886903222233,1.45439216225896E-14,
61.6813040583175));
#184767=CARTESIAN_POINT('',(114.581607361595,11.999999999933,63.2519072664783));
#184768=CARTESIAN_POINT('Origin',(114.581607361595,1.45439216225896E-14,
63.2519072664759));
#184769=CARTESIAN_POINT('',(114.886903222233,11.94412676881,61.6813040583175));
#184770=CARTESIAN_POINT('Origin',(114.28108174878,1.45439216225896E-14,
64.7979697995068));
#184771=CARTESIAN_POINT('',(114.772417274494,-12.25,62.2702802613768));
#184772=CARTESIAN_POINT('Origin',(114.772417274494,1.45439216225896E-14,
62.2702802613769));
#184773=CARTESIAN_POINT('',(117.386513081203,-12.25,48.8219902915203));
#184774=CARTESIAN_POINT('',(114.28108174878,-12.25,64.7979697995068));
#184775=CARTESIAN_POINT('Origin',(117.386513081203,1.45439216225896E-14,
48.8219902915203));
#184776=CARTESIAN_POINT('Origin',(114.28108174878,1.45439216225896E-14,
64.7979697995068));
#184777=CARTESIAN_POINT('',(114.581607361595,-12.75,63.2519072664759));
#184778=CARTESIAN_POINT('Origin',(114.581607361595,1.45439216225896E-14,
63.2519072664759));
#184779=CARTESIAN_POINT('',(114.772417274494,-12.75,62.2702802613768));
#184780=CARTESIAN_POINT('',(114.28108174878,-12.75,64.7979697995068));
#184781=CARTESIAN_POINT('Origin',(114.772417274494,1.45439216225896E-14,
62.2702802613769));
#184782=CARTESIAN_POINT('Origin',(114.28108174878,1.45439216225896E-14,
64.7979697995068));
#184783=CARTESIAN_POINT('',(115.383008995769,-13.1,59.12907384506));
#184784=CARTESIAN_POINT('Origin',(115.383008995769,1.45439216225896E-14,
59.12907384506));
#184785=CARTESIAN_POINT('',(115.096794126421,-13.1,60.6015143527085));
#184786=CARTESIAN_POINT('',(114.28108174878,-13.1,64.7979697995068));
#184787=CARTESIAN_POINT('Origin',(115.096794126421,1.45439216225896E-14,
60.6015143527085));
#184788=CARTESIAN_POINT('Origin',(114.28108174878,1.45439216225896E-14,
64.7979697995068));
#184789=CARTESIAN_POINT('',(121.534871381197,-13.,50.1377119242634));
#184790=CARTESIAN_POINT('',(121.534871381197,13.,50.1377119242634));
#184791=CARTESIAN_POINT('Origin',(117.291108124754,1.45439216225896E-14,
49.3128037940698));
#184792=CARTESIAN_POINT('',(121.057846598951,13.,52.591779437011));
#184793=CARTESIAN_POINT('',(121.057846598951,13.,52.591779437011));
#184794=CARTESIAN_POINT('',(112.570320086065,13.,50.9419631766238));
#184795=CARTESIAN_POINT('Origin',(116.814083342508,1.45439216225896E-14,
51.7668713068174));
#184796=CARTESIAN_POINT('',(113.047344868311,13.,48.4878956638762));
#184797=CARTESIAN_POINT('',(112.570320086065,13.,50.9419631766238));
#184798=CARTESIAN_POINT('',(113.047344868311,-13.,48.4878956638762));
#184799=CARTESIAN_POINT('Origin',(117.291108124754,1.45439216225896E-14,
49.3128037940698));
#184800=CARTESIAN_POINT('',(112.570320086065,-13.,50.9419631766238));
#184801=CARTESIAN_POINT('',(112.570320086065,-13.,50.9419631766238));
#184802=CARTESIAN_POINT('',(116.814083342508,-13.7,51.7668713068173));
#184803=CARTESIAN_POINT('Origin',(116.814083342508,1.45439216225896E-14,
51.7668713068174));
#184804=CARTESIAN_POINT('',(115.383008995769,-13.7,59.12907384506));
#184805=CARTESIAN_POINT('',(114.28108174878,-13.7,64.7979697995068));
#184806=CARTESIAN_POINT('Origin',(115.383008995769,1.45439216225896E-14,
59.12907384506));
#184807=CARTESIAN_POINT('',(121.057846598951,-13.,52.591779437011));
#184808=CARTESIAN_POINT('Origin',(116.814083342508,1.45439216225896E-14,
51.7668713068174));
#184809=CARTESIAN_POINT('',(121.057846598951,-13.,52.591779437011));
#184810=CARTESIAN_POINT('Origin',(114.476661909501,1.45439216225896E-14,
63.7918021192803));
#184811=CARTESIAN_POINT('',(105.907189290968,-10.2076212837564,62.3807362902962));
#184812=CARTESIAN_POINT('Ctrl Pts',(122.504911634294,-11.2745024089981,
65.0976651926838));
#184813=CARTESIAN_POINT('Ctrl Pts',(123.229846581212,-10.7328655109838,
65.2453382804213));
#184814=CARTESIAN_POINT('Ctrl Pts',(123.900533178686,-10.1186901216539,
65.3827789616297));
#184815=CARTESIAN_POINT('Ctrl Pts',(125.097983067777,-8.78240845240083,
65.6289243192982));
#184816=CARTESIAN_POINT('Ctrl Pts',(125.626442830263,-8.06472399520229,
65.7379736981974));
#184817=CARTESIAN_POINT('Ctrl Pts',(126.393898186431,-6.77838906626577,
65.8984097879606));
#184818=CARTESIAN_POINT('Ctrl Pts',(126.670869901367,-6.23612244254981,
65.9569283595829));
#184819=CARTESIAN_POINT('Ctrl Pts',(127.225281497024,-4.94994463554516,
66.0752469001846));
#184820=CARTESIAN_POINT('Ctrl Pts',(127.477101999605,-4.19597408503903,
66.1299606016456));
#184821=CARTESIAN_POINT('Ctrl Pts',(127.87399481505,-2.556029182679,66.2194221298755));
#184822=CARTESIAN_POINT('Ctrl Pts',(128.000343146586,-1.66956325408612,
66.2508298482742));
#184823=CARTESIAN_POINT('Ctrl Pts',(128.083737879612,0.118285322566095,
66.2805335003563));
#184824=CARTESIAN_POINT('Ctrl Pts',(128.040024208525,1.01687449567218,66.2785232628767));
#184825=CARTESIAN_POINT('Ctrl Pts',(127.78178873694,2.79232894127849,66.2414913384502));
#184826=CARTESIAN_POINT('Ctrl Pts',(127.567388976971,3.66503480243605,66.2067639194195));
#184827=CARTESIAN_POINT('Ctrl Pts',(126.979550286204,5.34528302425291,66.1059142543956));
#184828=CARTESIAN_POINT('Ctrl Pts',(126.608529648767,6.1512620066344,66.0401808204024));
#184829=CARTESIAN_POINT('Ctrl Pts',(125.713026001603,7.68934214784707,65.8793328936045));
#184830=CARTESIAN_POINT('Ctrl Pts',(125.187964517677,8.416928907309,65.7842870607944));
#184831=CARTESIAN_POINT('Ctrl Pts',(124.022781859346,9.73914833353154,65.5711253909796));
#184832=CARTESIAN_POINT('Ctrl Pts',(123.38722814423,10.3351025591763,65.4538764821083));
#184833=CARTESIAN_POINT('Ctrl Pts',(121.994162172805,11.4094174928648,65.1963808819556));
#184834=CARTESIAN_POINT('Ctrl Pts',(121.235991649557,11.8820277086889,65.0560519275869));
#184835=CARTESIAN_POINT('Ctrl Pts',(119.670104692157,12.6544884296133,64.7649352454329));
#184836=CARTESIAN_POINT('Ctrl Pts',(118.866867650534,12.9590403586294,64.6150367011459));
#184837=CARTESIAN_POINT('Ctrl Pts',(117.183754765794,13.4163303616198,64.3012694177438));
#184838=CARTESIAN_POINT('Ctrl Pts',(116.305307807354,13.5622060315306,64.1375519447353));
#184839=CARTESIAN_POINT('Ctrl Pts',(114.554928431228,13.6746520928841,63.8106529013362));
#184840=CARTESIAN_POINT('Ctrl Pts',(113.685441741559,13.6450888740068,63.6479984642041));
#184841=CARTESIAN_POINT('Ctrl Pts',(111.968639264187,13.4149320799642,63.3277473758802));
#184842=CARTESIAN_POINT('Ctrl Pts',(111.124955522097,13.2160582326946,63.1705638324682));
#184843=CARTESIAN_POINT('Ctrl Pts',(109.483290565272,12.6550171724688,62.8646119243846));
#184844=CARTESIAN_POINT('Ctrl Pts',(108.687973652607,12.2926589715997,62.7164434632677));
#184845=CARTESIAN_POINT('Ctrl Pts',(107.187366760791,11.4204732223485,62.4382823800872));
#184846=CARTESIAN_POINT('Ctrl Pts',(106.484490876799,10.9150751365952,62.3083969275442));
#184847=CARTESIAN_POINT('Ctrl Pts',(105.174918063374,9.76687727465901,62.0669615265641));
#184848=CARTESIAN_POINT('Ctrl Pts',(104.57216745938,9.12421627830972,61.9563161154106));
#184849=CARTESIAN_POINT('Ctrl Pts',(103.509288763409,7.74134958430475,61.7632882078509));
#184850=CARTESIAN_POINT('Ctrl Pts',(103.048965082131,7.0071913416104,61.6804785057821));
#184851=CARTESIAN_POINT('Ctrl Pts',(102.464674510065,5.84285378745556,61.5766532538355));
#184852=CARTESIAN_POINT('Ctrl Pts',(102.287086002315,5.44206810749397,61.5453754575537));
#184853=CARTESIAN_POINT('Ctrl Pts',(101.808535655182,4.20443804160805,61.4623588099708));
#184854=CARTESIAN_POINT('Ctrl Pts',(101.569522799854,3.34540366653471,61.4229519012272));
#184855=CARTESIAN_POINT('Ctrl Pts',(101.264583014311,1.61740419385571,61.3770688000621));
#184856=CARTESIAN_POINT('Ctrl Pts',(101.194723999211,0.751309308118347,
61.3698094353778));
#184857=CARTESIAN_POINT('Ctrl Pts',(101.219594865846,-0.992579368004674,
61.3879182276713));
#184858=CARTESIAN_POINT('Ctrl Pts',(101.316557330348,-1.8675772424215,61.4137312965633));
#184859=CARTESIAN_POINT('Ctrl Pts',(101.646121445148,-3.44371817065294,
61.4900696530388));
#184860=CARTESIAN_POINT('Ctrl Pts',(101.8536256679,-4.14832309282748,61.5358101090581));
#184861=CARTESIAN_POINT('Ctrl Pts',(102.518194464448,-5.87573706785547,
61.6790675863199));
#184862=CARTESIAN_POINT('Ctrl Pts',(103.04740164905,-6.8647922843056,61.7908934513442));
#184863=CARTESIAN_POINT('Ctrl Pts',(104.003808267056,-8.21865358302084,
61.9894116642463));
#184864=CARTESIAN_POINT('Ctrl Pts',(104.344782045948,-8.6437972103183,62.0597593868494));
#184865=CARTESIAN_POINT('Ctrl Pts',(105.085067467861,-9.45883829531425,
62.2121067994063));
#184866=CARTESIAN_POINT('Ctrl Pts',(105.484930025179,-9.8467254250202,62.2942672565808));
#184867=CARTESIAN_POINT('Ctrl Pts',(105.907189290968,-10.2076212837564,
62.3807362902962));
#184868=CARTESIAN_POINT('',(124.256736260291,-8.90570865984179,65.9470463235759));
#184869=CARTESIAN_POINT('Origin',(114.428959431277,1.45439216225896E-14,
64.0372088705551));
#184870=CARTESIAN_POINT('',(114.489783311165,-13.7191326559559,63.7243240965168));
#184871=CARTESIAN_POINT('Ctrl Pts',(124.256949391325,-8.90590330286328,
65.9470620427268));
#184872=CARTESIAN_POINT('Ctrl Pts',(123.99775328236,-9.224088446109,65.8841924187124));
#184873=CARTESIAN_POINT('Ctrl Pts',(123.723345529523,-9.53003896735735,
65.8186626717206));
#184874=CARTESIAN_POINT('Ctrl Pts',(123.435091579848,-9.82251828793179,
65.750626757231));
#184875=CARTESIAN_POINT('Ctrl Pts',(123.146396551434,-10.1154451527995,
65.6824867359444));
#184876=CARTESIAN_POINT('Ctrl Pts',(122.843813501118,-10.3948605139533,
65.6118329845868));
#184877=CARTESIAN_POINT('Ctrl Pts',(122.528671502062,-10.6595503748197,
65.5388118757864));
#184878=CARTESIAN_POINT('Ctrl Pts',(122.443732266683,-10.7308914035053,
65.5191307251729));
#184879=CARTESIAN_POINT('Ctrl Pts',(122.357880424489,-10.8011628143638,
65.4992775469335));
#184880=CARTESIAN_POINT('Ctrl Pts',(122.271141391864,-10.8703410420963,
65.479255089113));
#184881=CARTESIAN_POINT('Ctrl Pts',(121.891332759646,-11.1732552810398,
65.3915817304382));
#184882=CARTESIAN_POINT('Ctrl Pts',(121.494697233621,-11.455394761453,65.3005532770298));
#184883=CARTESIAN_POINT('Ctrl Pts',(121.083308218077,-11.7144688895035,
65.2065620719827));
#184884=CARTESIAN_POINT('Ctrl Pts',(120.704121940928,-11.9532631946719,
65.1199283171187));
#184885=CARTESIAN_POINT('Ctrl Pts',(120.312402038618,-12.1724609188301,
65.0307775938138));
#184886=CARTESIAN_POINT('Ctrl Pts',(119.910345037359,-12.3712103911295,
64.9395284962991));
#184887=CARTESIAN_POINT('Ctrl Pts',(119.491215508411,-12.5783993529999,
64.8444046926132));
#184888=CARTESIAN_POINT('Ctrl Pts',(119.060715016913,-12.7631480604679,
64.7471209483971));
#184889=CARTESIAN_POINT('Ctrl Pts',(118.621220734337,-12.9244627256754,
64.6481704279395));
#184890=CARTESIAN_POINT('Ctrl Pts',(118.18172645176,-13.0857773908829,64.5492199074818));
#184891=CARTESIAN_POINT('Ctrl Pts',(117.733237756405,-13.2236578222968,
64.4486024899362));
#184892=CARTESIAN_POINT('Ctrl Pts',(117.278172251404,-13.3370690493505,
64.3468191987493));
#184893=CARTESIAN_POINT('Ctrl Pts',(116.848023284575,-13.4442705876078,
64.2506089233859));
#184894=CARTESIAN_POINT('Ctrl Pts',(116.411989460296,-13.5297146283601,
64.1532941007664));
#184895=CARTESIAN_POINT('Ctrl Pts',(115.972297165646,-13.5927197612154,
64.0551965812453));
#184896=CARTESIAN_POINT('Ctrl Pts',(115.745509457432,-13.6252170095407,
64.0045991250144));
#184897=CARTESIAN_POINT('Ctrl Pts',(115.517747807483,-13.651745239074,63.9537933154996));
#184898=CARTESIAN_POINT('Ctrl Pts',(115.28931310856,-13.6722136550253,63.9028224206965));
#184899=CARTESIAN_POINT('Ctrl Pts',(115.023553746488,-13.6960264697663,
63.8435232312522));
#184900=CARTESIAN_POINT('Ctrl Pts',(114.7568835816,-13.7116373409563,63.7840006322766));
#184901=CARTESIAN_POINT('Ctrl Pts',(114.489783311165,-13.7191326559559,
63.7243240965168));
#184902=CARTESIAN_POINT('Ctrl Pts',(114.489803604467,-13.7190747033231,
63.7242257846487));
#184903=CARTESIAN_POINT('Ctrl Pts',(113.409266451882,-13.7491677927584,
63.4832965023283));
#184904=CARTESIAN_POINT('Ctrl Pts',(112.321523697456,-13.6449312950591,
63.2409659995486));
#184905=CARTESIAN_POINT('Ctrl Pts',(110.195514536491,-13.1698942968648,
62.7659222693647));
#184906=CARTESIAN_POINT('Ctrl Pts',(109.157373226761,-12.7991074634966,
62.5332333584385));
#184907=CARTESIAN_POINT('Ctrl Pts',(108.175183023666,-12.30344424038,62.3122333729097));
#184908=CARTESIAN_POINT('Origin',(114.28108174878,1.45439216225896E-14,
64.7979697995068));
#184909=CARTESIAN_POINT('',(114.428959431276,-12.75,64.037208870555));
#184910=CARTESIAN_POINT('Origin',(114.428959431277,1.45439216225896E-14,
64.0372088705551));
#184911=CARTESIAN_POINT('',(114.524364387726,-12.75,63.5463953680055));
#184912=CARTESIAN_POINT('',(114.28108174878,-12.75,64.7979697995068));
#184913=CARTESIAN_POINT('Origin',(114.524364387726,1.45439216225896E-14,
63.5463953680056));
#184914=CARTESIAN_POINT('Ctrl Pts',(118.491253192553,-12.7183023352,63.7707658968246));
#184915=CARTESIAN_POINT('Ctrl Pts',(116.466184337262,-13.35843074567,63.3507673831021));
#184916=CARTESIAN_POINT('Ctrl Pts',(112.105678659218,-13.60903770072,62.4504406331449));
#184917=CARTESIAN_POINT('Ctrl Pts',(106.15470984369,-10.81093357074,61.2145945848077));
#184918=CARTESIAN_POINT('Ctrl Pts',(102.187393024908,-5.49082338424599,
60.3643333489951));
#184919=CARTESIAN_POINT('Ctrl Pts',(101.132039193786,1.11008681820601,60.0801032035486));
#184920=CARTESIAN_POINT('Ctrl Pts',(103.238445493676,7.45205865399302,60.4104600367413));
#184921=CARTESIAN_POINT('Ctrl Pts',(108.018664973673,12.05569208811,61.2605560960788));
#184922=CARTESIAN_POINT('Ctrl Pts',(114.361086873968,13.84710498951,62.4143150601738));
#184923=CARTESIAN_POINT('Ctrl Pts',(120.789672201652,12.40841498499,63.5848225814906));
#184924=CARTESIAN_POINT('Ctrl Pts',(125.808286596475,8.07522435927901,64.4812581493247));
#184925=CARTESIAN_POINT('Ctrl Pts',(128.249697402688,1.85833282744001,64.8767335869671));
#184926=CARTESIAN_POINT('Ctrl Pts',(127.547854389266,-4.79205045842999,
64.6612193264683));
#184927=CARTESIAN_POINT('Ctrl Pts',(123.869931462632,-10.32459610784,63.8672108455791));
#184928=CARTESIAN_POINT('Ctrl Pts',(118.077330243317,-13.44873178266,62.66214849318));
#184929=CARTESIAN_POINT('Ctrl Pts',(111.524741598597,-13.43569294448,61.309358812883));
#184930=CARTESIAN_POINT('Ctrl Pts',(105.744138033829,-10.28852115219,60.1066285799213));
#184931=CARTESIAN_POINT('Ctrl Pts',(102.087411734415,-4.74135456058899,
59.3167403265448));
#184932=CARTESIAN_POINT('Ctrl Pts',(101.411019797005,1.91182387847601,59.1061732787571));
#184933=CARTESIAN_POINT('Ctrl Pts',(103.876199192475,8.11903274642801,59.5062688851827));
#184934=CARTESIAN_POINT('Ctrl Pts',(108.911355151527,12.43232157685,60.4059198234309));
#184935=CARTESIAN_POINT('Ctrl Pts',(115.345396602207,13.84553306015,61.5774879129147));
#184936=CARTESIAN_POINT('Ctrl Pts',(121.68091561507,12.02900852572,62.729905084921));
#184937=CARTESIAN_POINT('Ctrl Pts',(126.443486502869,7.40648714394101,63.576570588332));
#184938=CARTESIAN_POINT('Ctrl Pts',(128.525603902826,1.05626065173001,63.9022061140864));
#184939=CARTESIAN_POINT('Ctrl Pts',(127.445029542533,-5.54035890633199,
63.6130735699189));
#184940=CARTESIAN_POINT('Ctrl Pts',(123.457283904857,-10.84458346349,62.7588413541581));
#184941=CARTESIAN_POINT('Ctrl Pts',(117.496039897072,-13.61910129622,61.5209980008064));
#184942=CARTESIAN_POINT('Ctrl Pts',(110.95533052156,-13.21670165587,60.1705174280637));
#184943=CARTESIAN_POINT('Ctrl Pts',(105.364346129962,-9.73125672786299,
59.0046456125342));
#184944=CARTESIAN_POINT('Ctrl Pts',(102.030787974481,-3.97579561520298,
58.2775751963556));
#184945=CARTESIAN_POINT('Ctrl Pts',(101.735573576727,2.70704381218202,58.141101926309));
#184946=CARTESIAN_POINT('Ctrl Pts',(104.551599204905,8.75860830718901,58.6093954722332));
#184947=CARTESIAN_POINT('Ctrl Pts',(108.066051618942,11.43042410411,59.2398131494504));
#184948=CARTESIAN_POINT('Ctrl Pts',(110.029513630199,12.2704525675,59.5951103675036));
#184949=CARTESIAN_POINT('Ctrl Pts',(118.575698917339,-12.91976003203,63.6631452639466));
#184950=CARTESIAN_POINT('Ctrl Pts',(116.518474788798,-13.57002806584,63.2368963670782));
#184951=CARTESIAN_POINT('Ctrl Pts',(112.088742340823,-13.82460463088,62.3231132290306));
#184952=CARTESIAN_POINT('Ctrl Pts',(106.043275629434,-10.98217857815,61.0688985588191));
#184953=CARTESIAN_POINT('Ctrl Pts',(102.012881929328,-5.57779793505799,
60.2063763581299));
#184954=CARTESIAN_POINT('Ctrl Pts',(100.940576662033,1.12767057488801,59.9188511708367));
#184955=CARTESIAN_POINT('Ctrl Pts',(103.080113753482,7.57009913876102,60.2556480096718));
#184956=CARTESIAN_POINT('Ctrl Pts',(107.935817181206,12.24665404968,61.1204167353237));
#184957=CARTESIAN_POINT('Ctrl Pts',(114.378468289507,14.06644290155,62.2936583810791));
#184958=CARTESIAN_POINT('Ctrl Pts',(120.90864765245,12.60496407136,63.4839138809234));
#184959=CARTESIAN_POINT('Ctrl Pts',(126.006522166478,8.20313577842201,64.3957561321142));
#184960=CARTESIAN_POINT('Ctrl Pts',(128.486370230037,1.88776878842501,64.7987030530064));
#184961=CARTESIAN_POINT('Ctrl Pts',(127.773175385898,-4.86795645775498,
64.5809822091322));
#184962=CARTESIAN_POINT('Ctrl Pts',(124.03675957236,-10.48813753796,63.7756038060656));
#184963=CARTESIAN_POINT('Ctrl Pts',(118.152168997266,-13.66175946975,62.5526604450219));
#184964=CARTESIAN_POINT('Ctrl Pts',(111.495552808624,-13.6485140966,61.1796497576808));
#184965=CARTESIAN_POINT('Ctrl Pts',(105.623149930727,-10.45149115561,59.959075456798));
#184966=CARTESIAN_POINT('Ctrl Pts',(101.908266498638,-4.81645753773299,
59.1578825455907));
#184967=CARTESIAN_POINT('Ctrl Pts',(101.220925875135,1.94210713682301,58.9451872781849));
#184968=CARTESIAN_POINT('Ctrl Pts',(103.724919022004,8.24763808969801,59.3528275512662));
#184969=CARTESIAN_POINT('Ctrl Pts',(108.839597118367,12.62924934324,60.2679361042754));
#184970=CARTESIAN_POINT('Ctrl Pts',(115.375319029201,14.06484607286,61.4592689716785));
#184971=CARTESIAN_POINT('Ctrl Pts',(121.81095790845,12.21954782011,62.6311475713711));
#184972=CARTESIAN_POINT('Ctrl Pts',(126.648733190572,7.52380577674502,63.4924314011583));
#184973=CARTESIAN_POINT('Ctrl Pts',(128.763596646313,1.07299180282801,63.8244321471129));
#184974=CARTESIAN_POINT('Ctrl Pts',(127.665671357083,-5.62811809899199,
63.5319269071945));
#184975=CARTESIAN_POINT('Ctrl Pts',(123.614525245928,-11.01636148465,62.6653708262899));
#184976=CARTESIAN_POINT('Ctrl Pts',(117.558620583404,-13.83482763357,61.4091272137953));
#184977=CARTESIAN_POINT('Ctrl Pts',(110.9140718314,-13.42605398962,60.0384622102139));
#184978=CARTESIAN_POINT('Ctrl Pts',(105.234291691218,-9.88539967209599,
58.8553301634914));
#184979=CARTESIAN_POINT('Ctrl Pts',(101.847695381066,-4.03877215141899,
58.1179501229642));
#184980=CARTESIAN_POINT('Ctrl Pts',(101.547570143079,2.74992334101601,57.9805222775116));
#184981=CARTESIAN_POINT('Ctrl Pts',(104.407966921148,8.89734451667401,58.4574407443087));
#184982=CARTESIAN_POINT('Ctrl Pts',(107.977931770066,11.61148183125,59.0986489996371));
#184983=CARTESIAN_POINT('Ctrl Pts',(109.972416770466,12.46481633148,59.4599765059926));
#184984=CARTESIAN_POINT('Ctrl Pts',(118.660144642124,-13.12121772886,63.5555246310785));
#184985=CARTESIAN_POINT('Ctrl Pts',(116.570765240331,-13.78162538602,63.123025351064));
#184986=CARTESIAN_POINT('Ctrl Pts',(112.071806022429,-14.04017156104,62.1957858249163));
#184987=CARTESIAN_POINT('Ctrl Pts',(105.931841415176,-11.15342358557,60.9232025328403));
#184988=CARTESIAN_POINT('Ctrl Pts',(101.838370833747,-5.66477248586999,
60.0484193672646));
#184989=CARTESIAN_POINT('Ctrl Pts',(100.749114130278,1.14525433156901,59.7575991381346));
#184990=CARTESIAN_POINT('Ctrl Pts',(102.921782013287,7.68813962352701,60.1008359826022));
#184991=CARTESIAN_POINT('Ctrl Pts',(107.852969388734,12.43761601124,60.9802773745779));
#184992=CARTESIAN_POINT('Ctrl Pts',(114.39584970504,14.28578081359,62.1730017019832));
#184993=CARTESIAN_POINT('Ctrl Pts',(121.027623103238,12.80151315773,63.3830051803645));
#184994=CARTESIAN_POINT('Ctrl Pts',(126.204757736472,8.33104719757401,64.3102541149019));
#184995=CARTESIAN_POINT('Ctrl Pts',(128.723043057384,1.91720474942301,64.7206725190554));
#184996=CARTESIAN_POINT('Ctrl Pts',(127.99849638253,-4.94386245706599,64.5007450917961));
#184997=CARTESIAN_POINT('Ctrl Pts',(124.203587682101,-10.65167896807,63.6839967665646));
#184998=CARTESIAN_POINT('Ctrl Pts',(118.227007751235,-13.87478715684,62.4431723968677));
#184999=CARTESIAN_POINT('Ctrl Pts',(111.466364018676,-13.86133524872,61.0499407024733));
#185000=CARTESIAN_POINT('Ctrl Pts',(105.502161827646,-10.61446115905,59.8115223336785));
#185001=CARTESIAN_POINT('Ctrl Pts',(101.729121262874,-4.89156051490299,
58.9990247646287));
#185002=CARTESIAN_POINT('Ctrl Pts',(101.030831953255,1.97239039513901,58.7842012776108));
#185003=CARTESIAN_POINT('Ctrl Pts',(103.573638851525,8.37624343293902,59.199386217338));
#185004=CARTESIAN_POINT('Ctrl Pts',(108.767839085174,12.82617710962,60.1299523851135));
#185005=CARTESIAN_POINT('Ctrl Pts',(115.405241456157,14.28415908557,61.341050030425));
#185006=CARTESIAN_POINT('Ctrl Pts',(121.941000201793,12.41008711451,62.532390057814));
#185007=CARTESIAN_POINT('Ctrl Pts',(126.853979878247,7.64112440958602,63.408292213969));
#185008=CARTESIAN_POINT('Ctrl Pts',(129.001589389788,1.08972295397001,63.7466581801474));
#185009=CARTESIAN_POINT('Ctrl Pts',(127.886313171645,-5.71587729160999,
63.4507802444622));
#185010=CARTESIAN_POINT('Ctrl Pts',(123.771766587033,-11.18813950578,62.5719002984386));
#185011=CARTESIAN_POINT('Ctrl Pts',(117.621201269786,-14.05055397091,61.2972564267837));
#185012=CARTESIAN_POINT('Ctrl Pts',(110.872813141286,-13.63540632339,59.9064069923831));
#185013=CARTESIAN_POINT('Ctrl Pts',(105.104237252503,-10.03954261636,58.7060147144545));
#185014=CARTESIAN_POINT('Ctrl Pts',(101.664602787659,-4.10174868768399,
57.9583250495846));
#185015=CARTESIAN_POINT('Ctrl Pts',(101.359566709432,2.79280286980002,57.8199426287141));
#185016=CARTESIAN_POINT('Ctrl Pts',(104.264334637359,9.03608072612001,58.3054860163884));
#185017=CARTESIAN_POINT('Ctrl Pts',(107.889811921153,11.79253955836,58.9574848498063));
#185018=CARTESIAN_POINT('Ctrl Pts',(109.91531991069,12.65918009544,59.3248426444734));
#185019=CARTESIAN_POINT('Ctrl Pts',(118.74459036691,-13.32267542569,63.4479039982005));
#185020=CARTESIAN_POINT('Ctrl Pts',(116.623055691866,-13.99322270619,63.0091543350402));
#185021=CARTESIAN_POINT('Ctrl Pts',(112.054869704034,-14.2557384912,62.068458420802));
#185022=CARTESIAN_POINT('Ctrl Pts',(105.820407200921,-11.32466859299,60.7775065068516));
#185023=CARTESIAN_POINT('Ctrl Pts',(101.663859738167,-5.75174703668099,
59.8904623763993));
#185024=CARTESIAN_POINT('Ctrl Pts',(100.557651598525,1.16283808825201,59.5963471054226));
#185025=CARTESIAN_POINT('Ctrl Pts',(102.763450273093,7.80618010829502,59.9460239555327));
#185026=CARTESIAN_POINT('Ctrl Pts',(107.770121596268,12.62857797281,60.840138013823));
#185027=CARTESIAN_POINT('Ctrl Pts',(114.413231120579,14.50511872564,62.0523450228885));
#185028=CARTESIAN_POINT('Ctrl Pts',(121.146598554036,12.9980622441,63.2820964797973));
#185029=CARTESIAN_POINT('Ctrl Pts',(126.402993306465,8.45895861671701,64.2247520976895));
#185030=CARTESIAN_POINT('Ctrl Pts',(128.959715884732,1.94664071040801,64.6426419850946));
#185031=CARTESIAN_POINT('Ctrl Pts',(128.223817379161,-5.01976845639098,
64.4205079744699));
#185032=CARTESIAN_POINT('Ctrl Pts',(124.37041579183,-10.81522039819,63.5923897270511));
#185033=CARTESIAN_POINT('Ctrl Pts',(118.301846505182,-14.08781484393,62.3336843487194));
#185034=CARTESIAN_POINT('Ctrl Pts',(111.437175228705,-14.07415640083,60.9202316472613));
#185035=CARTESIAN_POINT('Ctrl Pts',(105.381173724543,-10.77743116247,59.6639692105651));
#185036=CARTESIAN_POINT('Ctrl Pts',(101.549976027089,-4.96666349204699,
58.8401669836628));
#185037=CARTESIAN_POINT('Ctrl Pts',(100.840738031383,2.00267365348601,58.6232152770484));
#185038=CARTESIAN_POINT('Ctrl Pts',(103.422358681056,8.50484877620901,59.0459448834116));
#185039=CARTESIAN_POINT('Ctrl Pts',(108.696081052011,13.02310487601,59.9919686659676));
#185040=CARTESIAN_POINT('Ctrl Pts',(115.435163883153,14.50347209828,61.222831089179));
#185041=CARTESIAN_POINT('Ctrl Pts',(122.07104249517,12.60062640889,62.4336325442737));
#185042=CARTESIAN_POINT('Ctrl Pts',(127.059226565942,7.75844304239001,63.3241530267836));
#185043=CARTESIAN_POINT('Ctrl Pts',(129.239582133274,1.10645410506801,63.6688842131738));
#185044=CARTESIAN_POINT('Ctrl Pts',(128.106954986187,-5.80363648426999,
63.369633581726));
#185045=CARTESIAN_POINT('Ctrl Pts',(123.929007928104,-11.35991752694,62.4784297705705));
#185046=CARTESIAN_POINT('Ctrl Pts',(117.683781956121,-14.26628030825,61.1853856397628));
#185047=CARTESIAN_POINT('Ctrl Pts',(110.831554451127,-13.84475865714,59.7743517745333));
#185048=CARTESIAN_POINT('Ctrl Pts',(104.97418281375,-10.1936855606,58.5566992654099));
#185049=CARTESIAN_POINT('Ctrl Pts',(101.481510194244,-4.16472522390098,
57.7986999761932));
#185050=CARTESIAN_POINT('Ctrl Pts',(101.171563275794,2.83568239863401,57.6593629799186));
#185051=CARTESIAN_POINT('Ctrl Pts',(104.120702353602,9.17481693560401,58.1535312884639));
#185052=CARTESIAN_POINT('Ctrl Pts',(107.801692072279,11.97359728549,58.8163206999831));
#185053=CARTESIAN_POINT('Ctrl Pts',(109.858223050957,12.85354385943,59.1897087829625));
#185054=CARTESIAN_POINT('',(114.640971711999,-13.3588720674388,62.9464971841653));
#185055=CARTESIAN_POINT('',(106.597794810055,10.1748376800446,58.9494679941055));
#185056=CARTESIAN_POINT('Ctrl Pts',(114.640904788072,-13.357524695892,62.9468179160091));
#185057=CARTESIAN_POINT('Ctrl Pts',(114.13304666145,-13.3578942130633,62.8417580704295));
#185058=CARTESIAN_POINT('Ctrl Pts',(113.625151177201,-13.3283693476066,
62.7366625756605));
#185059=CARTESIAN_POINT('Ctrl Pts',(112.651945528154,-13.2132690486779,
62.5351724262472));
#185060=CARTESIAN_POINT('Ctrl Pts',(112.185897821086,-13.131779068876,62.438598105965));
#185061=CARTESIAN_POINT('Ctrl Pts',(110.86466155124,-12.8224878570432,62.1648732340489));
#185062=CARTESIAN_POINT('Ctrl Pts',(110.025581150313,-12.5309381011058,
61.9911471537562));
#185063=CARTESIAN_POINT('Ctrl Pts',(108.546930020057,-11.842867295222,61.6840357448642));
#185064=CARTESIAN_POINT('Ctrl Pts',(107.896456525995,-11.4698948337182,
61.548539340477));
#185065=CARTESIAN_POINT('Ctrl Pts',(106.939222074391,-10.8062052962347,
61.347910397855));
#185066=CARTESIAN_POINT('Ctrl Pts',(106.607799893718,-10.5521992865497,
61.2781728990859));
#185067=CARTESIAN_POINT('Ctrl Pts',(106.121768221915,-10.1408419147875,
61.1754516486887));
#185068=CARTESIAN_POINT('Ctrl Pts',(105.957880515477,-9.99482870805906,
61.140751262454));
#185069=CARTESIAN_POINT('Ctrl Pts',(105.612695754859,-9.67101177218622,
61.0676578688006));
#185070=CARTESIAN_POINT('Ctrl Pts',(105.432895117018,-9.49210227679692,
61.0295659988766));
#185071=CARTESIAN_POINT('Ctrl Pts',(104.832010780966,-8.85843031270054,
60.9021190377937));
#185072=CARTESIAN_POINT('Ctrl Pts',(104.436926515002,-8.37796342960463,
60.8180630804526));
#185073=CARTESIAN_POINT('Ctrl Pts',(103.741955795032,-7.40238028037761,
60.6689588910643));
#185074=CARTESIAN_POINT('Ctrl Pts',(103.437181924747,-6.91072317790111,
60.6029579528933));
#185075=CARTESIAN_POINT('Ctrl Pts',(103.043287231502,-6.17374123906158,
60.5162504514931));
#185076=CARTESIAN_POINT('Ctrl Pts',(102.928200845802,-5.9427688350452,60.4907002080805));
#185077=CARTESIAN_POINT('Ctrl Pts',(102.699405821129,-5.44847187495716,
60.439368713644));
#185078=CARTESIAN_POINT('Ctrl Pts',(102.587263172405,-5.18439711493227,
60.4138551208945));
#185079=CARTESIAN_POINT('Ctrl Pts',(102.397216298565,-4.69348794710408,
60.3700056759946));
#185080=CARTESIAN_POINT('Ctrl Pts',(102.316716708879,-4.46771302769359,
60.3511964766176));
#185081=CARTESIAN_POINT('Ctrl Pts',(102.185025218202,-4.06408315937053,
60.3201206455682));
#185082=CARTESIAN_POINT('Ctrl Pts',(102.131448804967,-3.88739373852614,
60.3073740468952));
#185083=CARTESIAN_POINT('Ctrl Pts',(102.029090310271,-3.52270003785181,
60.2827933355699));
#185084=CARTESIAN_POINT('Ctrl Pts',(101.980712552168,-3.3346608650091,60.2710403841923));
#185085=CARTESIAN_POINT('Ctrl Pts',(101.798178471838,-2.55578924910197,
60.2260349284972));
#185086=CARTESIAN_POINT('Ctrl Pts',(101.699610622787,-1.95619866277338,
60.2000300640393));
#185087=CARTESIAN_POINT('Ctrl Pts',(101.610625441262,-1.03983478435559,
60.172252824418));
#185088=CARTESIAN_POINT('Ctrl Pts',(101.590977191464,-0.726006611478508,
60.1648406494029));
#185089=CARTESIAN_POINT('Ctrl Pts',(101.57531060063,-0.172071079279196,
60.1553272403031));
#185090=CARTESIAN_POINT('Ctrl Pts',(101.574798965633,0.0679138644798712,
60.1523838865166));
#185091=CARTESIAN_POINT('Ctrl Pts',(101.584821993279,0.483796087568609,
60.1492814152502));
#185092=CARTESIAN_POINT('Ctrl Pts',(101.592454895292,0.659766305083154,
60.1485899668375));
#185093=CARTESIAN_POINT('Ctrl Pts',(101.621674565384,1.12527544274108,60.1483860600609));
#185094=CARTESIAN_POINT('Ctrl Pts',(101.649105093071,1.41444195504571,60.1499043701699));
#185095=CARTESIAN_POINT('Ctrl Pts',(101.72091325271,1.97807314072567,60.1563133725514));
#185096=CARTESIAN_POINT('Ctrl Pts',(101.764513908999,2.25262977683502,60.1610657767085));
#185097=CARTESIAN_POINT('Ctrl Pts',(101.84054682363,2.65099254421983,60.1705467407519));
#185098=CARTESIAN_POINT('Ctrl Pts',(101.866287086771,2.77610820298583,60.173901059286));
#185099=CARTESIAN_POINT('Ctrl Pts',(101.923255407581,3.03413364715345,60.181627688659));
#185100=CARTESIAN_POINT('Ctrl Pts',(101.954735519064,3.16697189908343,60.1860533901494));
#185101=CARTESIAN_POINT('Ctrl Pts',(102.029106806634,3.46071636523449,60.1968163652399));
#185102=CARTESIAN_POINT('Ctrl Pts',(102.072983375827,3.62136124193086,60.2033598051749));
#185103=CARTESIAN_POINT('Ctrl Pts',(102.255161442947,4.24285204003838,60.2311772757719));
#185104=CARTESIAN_POINT('Ctrl Pts',(102.415166968247,4.69712640278496,60.2569152596301));
#185105=CARTESIAN_POINT('Ctrl Pts',(102.771763089177,5.5610456371751,60.3157856608415));
#185106=CARTESIAN_POINT('Ctrl Pts',(102.965847169219,5.97181244352332,60.3484295301969));
#185107=CARTESIAN_POINT('Ctrl Pts',(103.258015477615,6.51787531835683,60.3979413406901));
#185108=CARTESIAN_POINT('Ctrl Pts',(103.338934764958,6.66268499607493,60.4116872955399));
#185109=CARTESIAN_POINT('Ctrl Pts',(103.491557146343,6.92442733874645,60.4376497680994));
#185110=CARTESIAN_POINT('Ctrl Pts',(103.562438951009,7.04185656772653,60.4497205345221));
#185111=CARTESIAN_POINT('Ctrl Pts',(103.884876156801,7.55811042508076,60.5046572184889));
#185112=CARTESIAN_POINT('Ctrl Pts',(104.155453484377,7.94472372294211,60.5508111381471));
#185113=CARTESIAN_POINT('Ctrl Pts',(104.626711861602,8.54730141158604,60.6321141893237));
#185114=CARTESIAN_POINT('Ctrl Pts',(104.815519761776,8.7728585396044,60.6648944677146));
#185115=CARTESIAN_POINT('Ctrl Pts',(105.089172256251,9.07824165106905,60.7128567585429));
#185116=CARTESIAN_POINT('Ctrl Pts',(105.167794290818,9.16365274147528,60.7266871712758));
#185117=CARTESIAN_POINT('Ctrl Pts',(105.338775798923,9.34450156421968,60.7568670518337));
#185118=CARTESIAN_POINT('Ctrl Pts',(105.431442676693,9.43957023304213,60.7732841223262));
#185119=CARTESIAN_POINT('Ctrl Pts',(105.719210938087,9.72598188051344,60.8244230471412));
#185120=CARTESIAN_POINT('Ctrl Pts',(105.918820637734,9.91261159695927,60.860110349335));
#185121=CARTESIAN_POINT('Ctrl Pts',(106.45767539947,10.3860623669133,60.9568062099594));
#185122=CARTESIAN_POINT('Ctrl Pts',(106.805938440753,10.6622590205496,61.0196502005837));
#185123=CARTESIAN_POINT('Ctrl Pts',(107.37130808444,11.0663362138372,61.1216993410473));
#185124=CARTESIAN_POINT('Ctrl Pts',(107.579862313223,11.2066305252831,61.1593489157711));
#185125=CARTESIAN_POINT('Ctrl Pts',(107.900203246337,11.4091694152764,61.2171031647627));
#185126=CARTESIAN_POINT('Ctrl Pts',(108.009233602305,11.4759194192547,61.2367474916503));
#185127=CARTESIAN_POINT('Ctrl Pts',(108.223838497537,11.6030718995451,61.2753750687715));
#185128=CARTESIAN_POINT('Ctrl Pts',(108.329326260351,11.6636251040241,61.2943427192708));
#185129=CARTESIAN_POINT('Ctrl Pts',(108.71838722681,11.8798753972669,61.3642350011784));
#185130=CARTESIAN_POINT('Ctrl Pts',(109.006819513345,12.0266019269427,61.4159368321564));
#185131=CARTESIAN_POINT('Ctrl Pts',(109.589614463954,12.2964189745832,61.5204772214287));
#185132=CARTESIAN_POINT('Ctrl Pts',(109.883857650602,12.4197975079218,61.5732939196274));
#185133=CARTESIAN_POINT('Ctrl Pts',(110.366124575335,12.6013301593778,61.6601501351901));
#185134=CARTESIAN_POINT('Ctrl Pts',(110.551650540504,12.6663619514185,61.6936304822));
#185135=CARTESIAN_POINT('Ctrl Pts',(110.837901980005,12.7593314357167,61.7454400582351));
#185136=CARTESIAN_POINT('Ctrl Pts',(110.937582650568,12.7903554986743,61.763510348273));
#185137=CARTESIAN_POINT('Ctrl Pts',(111.157239307974,12.8557592462737,61.8033958907701));
#185138=CARTESIAN_POINT('Ctrl Pts',(111.277248983378,12.8895799988415,61.8252280723137));
#185139=CARTESIAN_POINT('Ctrl Pts',(111.731759509055,13.0105293791575,61.9080350703606));
#185140=CARTESIAN_POINT('Ctrl Pts',(112.069249071377,13.0858417092473,61.9697709998442));
#185141=CARTESIAN_POINT('Ctrl Pts',(112.748917318068,13.2092406064118,62.094238900772));
#185142=CARTESIAN_POINT('Ctrl Pts',(113.091094796768,13.2573335129592,62.1569699886093));
#185143=CARTESIAN_POINT('Ctrl Pts',(113.646626204469,13.3130789845115,62.2586363878786));
#185144=CARTESIAN_POINT('Ctrl Pts',(113.859163680795,13.3291654628939,62.2974904189975));
#185145=CARTESIAN_POINT('Ctrl Pts',(114.183570544218,13.3457674206309,62.3566696298158));
#185146=CARTESIAN_POINT('Ctrl Pts',(114.2952469085,13.3500498490439,62.3770192560691));
#185147=CARTESIAN_POINT('Ctrl Pts',(114.531678159406,13.3560865719153,62.420042125316));
#185148=CARTESIAN_POINT('Ctrl Pts',(114.656443115949,13.3574887819261,62.4427111977239));
#185149=CARTESIAN_POINT('Ctrl Pts',(115.114235986337,13.3560888231383,62.52579022643));
#185150=CARTESIAN_POINT('Ctrl Pts',(115.447276730587,13.3423610169083,62.5860363662682));
#185151=CARTESIAN_POINT('Ctrl Pts',(116.122663385045,13.2885137617653,62.7081014206246));
#185152=CARTESIAN_POINT('Ctrl Pts',(116.464959387862,13.2475121823014,62.7699081560095));
#185153=CARTESIAN_POINT('Ctrl Pts',(117.014012552028,13.1592593830363,62.8692040249979));
#185154=CARTESIAN_POINT('Ctrl Pts',(117.222101108764,13.120524924425,62.906873359065));
#185155=CARTESIAN_POINT('Ctrl Pts',(117.536777166574,13.0537945091799,62.9639462656728));
#185156=CARTESIAN_POINT('Ctrl Pts',(117.644142120415,13.0295682205426,62.9834384668156));
#185157=CARTESIAN_POINT('Ctrl Pts',(117.862349572319,12.977330759556,63.0231033782953));
#185158=CARTESIAN_POINT('Ctrl Pts',(117.973119772814,12.9492193191486,63.0432657062975));
#185159=CARTESIAN_POINT('Ctrl Pts',(118.321955664972,12.8556772957132,63.1068242587273));
#185160=CARTESIAN_POINT('Ctrl Pts',(118.55861118124,12.7847812121831,63.1500375013425));
#185161=CARTESIAN_POINT('Ctrl Pts',(119.158344923045,12.5861951733289,63.2596032859501));
#185162=CARTESIAN_POINT('Ctrl Pts',(119.518326470209,12.4488839811277,63.3254202861066));
#185163=CARTESIAN_POINT('Ctrl Pts',(120.014884681342,12.2340275500708,63.4158869726836));
#185164=CARTESIAN_POINT('Ctrl Pts',(120.156909005605,12.1695513992125,63.4417238991393));
#185165=CARTESIAN_POINT('Ctrl Pts',(120.414002169005,12.0472973300729,63.4883905620043));
#185166=CARTESIAN_POINT('Ctrl Pts',(120.529438477687,11.9903221868223,63.5093047926723));
#185167=CARTESIAN_POINT('Ctrl Pts',(120.74971540413,11.8775798137548,63.5491210550845));
#185168=CARTESIAN_POINT('Ctrl Pts',(120.854678807306,11.8220657143635,63.5680542592931));
#185169=CARTESIAN_POINT('Ctrl Pts',(121.139737692372,11.66636932674,63.6193774817783));
#185170=CARTESIAN_POINT('Ctrl Pts',(121.318348492923,11.5633469345845,63.6514294780892));
#185171=CARTESIAN_POINT('Ctrl Pts',(121.936950761117,11.1870749230793,63.7621547519484));
#185172=CARTESIAN_POINT('Ctrl Pts',(122.364104677741,10.8918150597322,63.8380952042949));
#185173=CARTESIAN_POINT('Ctrl Pts',(122.982618292788,10.4079138296809,63.9478893155293));
#185174=CARTESIAN_POINT('Ctrl Pts',(123.187627201529,10.2372507000208,63.9842507749081));
#185175=CARTESIAN_POINT('Ctrl Pts',(123.482893485197,9.97569886736661,64.0366568474352));
#185176=CARTESIAN_POINT('Ctrl Pts',(123.577259438626,9.88960137156063,64.0534113238723));
#185177=CARTESIAN_POINT('Ctrl Pts',(123.75454575661,9.72297861908504,64.0849101284806));
#185178=CARTESIAN_POINT('Ctrl Pts',(123.837624325387,9.6427765129703,64.099681658678));
#185179=CARTESIAN_POINT('Ctrl Pts',(124.24254908312,9.24124425607086,64.1717294617124));
#185180=CARTESIAN_POINT('Ctrl Pts',(124.548743051469,8.90393366013752,64.2263481457952));
#185181=CARTESIAN_POINT('Ctrl Pts',(125.036109703474,8.30848060673347,64.3126758184803));
#185182=CARTESIAN_POINT('Ctrl Pts',(125.22659224287,8.0582513325356,64.3462334918513));
#185183=CARTESIAN_POINT('Ctrl Pts',(125.484113128596,7.69433067021073,64.3910974689351));
#185184=CARTESIAN_POINT('Ctrl Pts',(125.558442486502,7.58598438779627,64.4039811197604));
#185185=CARTESIAN_POINT('Ctrl Pts',(125.717542070755,7.34670631634288,64.4314222542772));
#185186=CARTESIAN_POINT('Ctrl Pts',(125.801673439851,7.21533075686617,64.4458436783326));
#185187=CARTESIAN_POINT('Ctrl Pts',(126.171376844117,6.61557940636577,64.5088411145553));
#185188=CARTESIAN_POINT('Ctrl Pts',(126.431326233362,6.13076090329836,64.5520786961174));
#185189=CARTESIAN_POINT('Ctrl Pts',(126.780279820338,5.37293252424908,64.6089238011067));
#185190=CARTESIAN_POINT('Ctrl Pts',(126.89133380384,5.11032410667716,64.6267754663688));
#185191=CARTESIAN_POINT('Ctrl Pts',(127.069193557119,4.64946524302802,64.6550099767178));
#185192=CARTESIAN_POINT('Ctrl Pts',(127.139894121765,4.45276366113968,64.6661139986393));
#185193=CARTESIAN_POINT('Ctrl Pts',(127.249195142221,4.12464289832333,64.6831011863358));
#185194=CARTESIAN_POINT('Ctrl Pts',(127.290449168039,3.99413725472788,64.6894630103175));
#185195=CARTESIAN_POINT('Ctrl Pts',(127.375043346053,3.71135019989342,64.7024063481235));
#185196=CARTESIAN_POINT('Ctrl Pts',(127.417619770423,3.55911024014224,64.7088585538984));
#185197=CARTESIAN_POINT('Ctrl Pts',(127.557327739738,3.02279510302719,64.7297541786284));
#185198=CARTESIAN_POINT('Ctrl Pts',(127.640055702074,2.63503439590416,64.7415833085844));
#185199=CARTESIAN_POINT('Ctrl Pts',(127.732353209115,2.08601699603026,64.7533664684811));
#185200=CARTESIAN_POINT('Ctrl Pts',(127.75616800248,1.92723139664744,64.7561986023379));
#185201=CARTESIAN_POINT('Ctrl Pts',(127.799126716805,1.60195605970232,64.7607857850457));
#185202=CARTESIAN_POINT('Ctrl Pts',(127.818021103159,1.43543230925132,64.7624898441099));
#185203=CARTESIAN_POINT('Ctrl Pts',(127.851832881245,1.07953660699374,64.7647801264296));
#185204=CARTESIAN_POINT('Ctrl Pts',(127.86588332986,0.890077168074348,64.7651868304453));
#185205=CARTESIAN_POINT('Ctrl Pts',(127.906290085679,0.133790222627718,
64.7636271346906));
#185206=CARTESIAN_POINT('Ctrl Pts',(127.901608590714,-0.434766238665586,
64.7553360502631));
#185207=CARTESIAN_POINT('Ctrl Pts',(127.839502281003,-1.31798964527625,
64.7318073303138));
#185208=CARTESIAN_POINT('Ctrl Pts',(127.80613617809,-1.63455218091816,64.7212178660795));
#185209=CARTESIAN_POINT('Ctrl Pts',(127.728443943764,-2.18501095480177,
64.6990792097848));
#185210=CARTESIAN_POINT('Ctrl Pts',(127.68899934161,-2.41963383820523,64.688444509012));
#185211=CARTESIAN_POINT('Ctrl Pts',(127.610990645598,-2.81833512942862,
64.6683297623307));
#185212=CARTESIAN_POINT('Ctrl Pts',(127.575520933379,-2.98304090406737,
64.6594166434494));
#185213=CARTESIAN_POINT('Ctrl Pts',(127.463920336948,-3.45712537536408,
64.6320123940435));
#185214=CARTESIAN_POINT('Ctrl Pts',(127.379834488355,-3.76392998567303,
64.6121221090456));
#185215=CARTESIAN_POINT('Ctrl Pts',(127.185593936981,-4.38521353303955,
64.5670997996144));
#185216=CARTESIAN_POINT('Ctrl Pts',(127.074289841842,-4.69952565835987,
64.5417087831309));
#185217=CARTESIAN_POINT('Ctrl Pts',(126.864801569003,-5.22840183646511,
64.4942934614358));
#185218=CARTESIAN_POINT('Ctrl Pts',(126.772266854945,-5.44530138853266,
64.473468394417));
#185219=CARTESIAN_POINT('Ctrl Pts',(126.354258986003,-6.35860802414336,
64.3799200115085));
#185220=CARTESIAN_POINT('Ctrl Pts',(125.975394107594,-7.02968604150785,
64.2963647961218));
#185221=CARTESIAN_POINT('Ctrl Pts',(125.357727517744,-7.934022287407,64.1623214125837));
#185222=CARTESIAN_POINT('Ctrl Pts',(125.162470146833,-8.19848977855258,
64.1201938050918));
#185223=CARTESIAN_POINT('Ctrl Pts',(124.79007615719,-8.66546649467137,64.0403457523059));
#185224=CARTESIAN_POINT('Ctrl Pts',(124.616034928297,-8.87053820418804,
64.0032033395742));
#185225=CARTESIAN_POINT('Ctrl Pts',(124.256206717355,-9.26882654474569,
63.9267898520112));
#185226=CARTESIAN_POINT('Ctrl Pts',(124.070968901256,-9.46148931235269,
63.8876533053748));
#185227=CARTESIAN_POINT('Ctrl Pts',(123.639997309396,-9.88272035615241,
63.7969049457651));
#185228=CARTESIAN_POINT('Ctrl Pts',(123.391662550018,-10.1073027448131,
63.7447495300018));
#185229=CARTESIAN_POINT('Ctrl Pts',(122.806595195361,-10.5971434142374,
63.6219157172491));
#185230=CARTESIAN_POINT('Ctrl Pts',(122.464700240288,-10.8559748928838,
63.5502163113335));
#185231=CARTESIAN_POINT('Ctrl Pts',(121.621751717589,-11.4319571617041,
63.3736837492754));
#185232=CARTESIAN_POINT('Ctrl Pts',(121.110087858341,-11.7331363248134,
63.2667199064968));
#185233=CARTESIAN_POINT('Ctrl Pts',(119.932002719735,-12.3232369511335,
63.0210355140993));
#185234=CARTESIAN_POINT('Ctrl Pts',(119.256658901038,-12.5939329065661,
62.8805888329962));
#185235=CARTESIAN_POINT('Ctrl Pts',(118.209943403202,-12.9126257556509,
62.6637175782328));
#185236=CARTESIAN_POINT('Ctrl Pts',(117.852842553851,-13.0043295678821,
62.589882982709));
#185237=CARTESIAN_POINT('Ctrl Pts',(115.837578810976,-13.4295284185426,
62.1731546981305));
#185238=CARTESIAN_POINT('Ctrl Pts',(114.114959940367,-13.4482587470028,
61.8173097145917));
#185239=CARTESIAN_POINT('Ctrl Pts',(112.03054112538,-13.0573242410817,61.3854465567167));
#185240=CARTESIAN_POINT('Ctrl Pts',(111.611477861188,-12.9566211394342,
61.2985227316503));
#185241=CARTESIAN_POINT('Ctrl Pts',(110.397387606598,-12.5975714198071,
61.0467081907155));
#185242=CARTESIAN_POINT('Ctrl Pts',(109.620181202009,-12.2815155199788,
60.8855747287923));
#185243=CARTESIAN_POINT('Ctrl Pts',(108.189127318744,-11.5333105127569,
60.5879512297827));
#185244=CARTESIAN_POINT('Ctrl Pts',(107.530223181635,-11.1105921007965,
60.4504708231738));
#185245=CARTESIAN_POINT('Ctrl Pts',(106.565391608009,-10.3626609457922,
60.2477237874993));
#185246=CARTESIAN_POINT('Ctrl Pts',(106.230927857509,-10.0754372090119,
60.1771151717748));
#185247=CARTESIAN_POINT('Ctrl Pts',(105.755854574157,-9.62344263598964,
60.0762812382923));
#185248=CARTESIAN_POINT('Ctrl Pts',(105.603627976406,-9.47124093647704,
60.0438999584807));
#185249=CARTESIAN_POINT('Ctrl Pts',(105.28542516852,-9.1367100684019,59.9761891014369));
#185250=CARTESIAN_POINT('Ctrl Pts',(105.12078442685,-8.95342524094493,59.9411296926167));
#185251=CARTESIAN_POINT('Ctrl Pts',(104.484015436306,-8.20311836289615,
59.8053438764008));
#185252=CARTESIAN_POINT('Ctrl Pts',(104.053206909363,-7.59951364863668,
59.7130424172221));
#185253=CARTESIAN_POINT('Ctrl Pts',(103.493058578304,-6.6606480910518,59.5913850382532));
#185254=CARTESIAN_POINT('Ctrl Pts',(103.323834555591,-6.35003030243997,
59.5543429022173));
#185255=CARTESIAN_POINT('Ctrl Pts',(103.040169531912,-5.77712997366257,
59.4915643561494));
#185256=CARTESIAN_POINT('Ctrl Pts',(102.9214432161,-5.51702662733298,59.465021842453));
#185257=CARTESIAN_POINT('Ctrl Pts',(102.71687156982,-5.02842043346527,59.4186921025178));
#185258=CARTESIAN_POINT('Ctrl Pts',(102.628756185847,-4.80089832486037,
59.398485087806));
#185259=CARTESIAN_POINT('Ctrl Pts',(102.466176581298,-4.34458733978355,
59.3606248610168));
#185260=CARTESIAN_POINT('Ctrl Pts',(102.391532211094,-4.11586718307708,
59.3429390963345));
#185261=CARTESIAN_POINT('Ctrl Pts',(102.247983228326,-3.63207010985547,
59.308411029996));
#185262=CARTESIAN_POINT('Ctrl Pts',(102.180341702018,-3.37658064438319,
59.2918239647526));
#185263=CARTESIAN_POINT('Ctrl Pts',(102.081029130435,-2.95018503945331,
59.2670271651299));
#185264=CARTESIAN_POINT('Ctrl Pts',(102.045067128554,-2.78091983344021,
59.2579110564241));
#185265=CARTESIAN_POINT('Ctrl Pts',(101.962162099715,-2.34991924665055,
59.2364929455991));
#185266=CARTESIAN_POINT('Ctrl Pts',(101.919676027197,-2.08728907043755,
59.2251050769411));
#185267=CARTESIAN_POINT('Ctrl Pts',(101.834493987048,-1.44103113278861,
59.2009941404104));
#185268=CARTESIAN_POINT('Ctrl Pts',(101.800331278556,-1.05620878670474,
59.1899818655806));
#185269=CARTESIAN_POINT('Ctrl Pts',(101.761585684893,-0.222212896363878,
59.1729668446853));
#185270=CARTESIAN_POINT('Ctrl Pts',(101.762717532769,0.227301074504134,
59.1680686407415));
#185271=CARTESIAN_POINT('Ctrl Pts',(101.796075427552,0.87503831262595,59.1668789481708));
#185272=CARTESIAN_POINT('Ctrl Pts',(101.81068659318,1.07420437693522,59.1673186852143));
#185273=CARTESIAN_POINT('Ctrl Pts',(101.846198155655,1.44654474799569,59.1696260495175));
#185274=CARTESIAN_POINT('Ctrl Pts',(101.866069156421,1.6198226259679,59.1713059851813));
#185275=CARTESIAN_POINT('Ctrl Pts',(101.911383702352,1.95758477126266,59.1757530132773));
#185276=CARTESIAN_POINT('Ctrl Pts',(101.936531992671,2.12210891398788,59.1784643348455));
#185277=CARTESIAN_POINT('Ctrl Pts',(102.031055909962,2.6725213419252,59.1894571603034));
#185278=CARTESIAN_POINT('Ctrl Pts',(102.114153895364,3.0559900424101,59.2003078888467));
#185279=CARTESIAN_POINT('Ctrl Pts',(102.253498585011,3.5853398825905,59.2203022328071));
#185280=CARTESIAN_POINT('Ctrl Pts',(102.295647488564,3.73478678808129,59.2265221875798));
#185281=CARTESIAN_POINT('Ctrl Pts',(102.381229485447,4.01907104596501,59.2394736579373));
#185282=CARTESIAN_POINT('Ctrl Pts',(102.424134919428,4.15379101364896,59.2460946161624));
#185283=CARTESIAN_POINT('Ctrl Pts',(102.542551928911,4.50624815897289,59.2646659863145));
#185284=CARTESIAN_POINT('Ctrl Pts',(102.621562993342,4.72276527838593,59.2773442539343));
#185285=CARTESIAN_POINT('Ctrl Pts',(102.964754595082,5.59347480677453,59.3333488940382));
#185286=CARTESIAN_POINT('Ctrl Pts',(103.274674513585,6.22910346089313,59.385943733931));
#185287=CARTESIAN_POINT('Ctrl Pts',(103.732364324106,7.00825960094132,59.4644574231797));
#185288=CARTESIAN_POINT('Ctrl Pts',(103.837151023302,7.17797672653731,59.4824788168627));
#185289=CARTESIAN_POINT('Ctrl Pts',(104.020560831428,7.4608774878375,59.5140596166069));
#185290=CARTESIAN_POINT('Ctrl Pts',(104.097275873635,7.57534131046127,59.527279257401));
#185291=CARTESIAN_POINT('Ctrl Pts',(104.273213723829,7.82935854437856,59.5576041448866));
#185292=CARTESIAN_POINT('Ctrl Pts',(104.373373062807,7.96824228242872,59.57486702255));
#185293=CARTESIAN_POINT('Ctrl Pts',(104.711478063147,8.41867106841112,59.6331863903608));
#185294=CARTESIAN_POINT('Ctrl Pts',(104.960416178103,8.72171765659465,59.6762105652636));
#185295=CARTESIAN_POINT('Ctrl Pts',(105.38747103816,9.19694853716043,59.7506355611185));
#185296=CARTESIAN_POINT('Ctrl Pts',(105.557930481459,9.37624280645495,59.7804861710088));
#185297=CARTESIAN_POINT('Ctrl Pts',(105.816303686599,9.63297574535571,59.8260468283476));
#185298=CARTESIAN_POINT('Ctrl Pts',(105.900332501203,9.71424556620526,59.840912503126));
#185299=CARTESIAN_POINT('Ctrl Pts',(106.079180881687,9.88261487660262,59.8726521429693));
#185300=CARTESIAN_POINT('Ctrl Pts',(106.174146425296,9.96939657171607,59.8895602644886));
#185301=CARTESIAN_POINT('Ctrl Pts',(106.470262730222,10.2320900527407,59.9424259455987));
#185302=CARTESIAN_POINT('Ctrl Pts',(106.675495992491,10.4032103926802,59.9792654642311));
#185303=CARTESIAN_POINT('Ctrl Pts',(107.292909532275,10.8870065603853,60.0904594425795));
#185304=CARTESIAN_POINT('Ctrl Pts',(107.718584203814,11.1818520194149,60.1675803068146));
#185305=CARTESIAN_POINT('Ctrl Pts',(108.340583859555,11.5610238326694,60.2801760033078));
#185306=CARTESIAN_POINT('Ctrl Pts',(108.524180022238,11.6669882992912,60.3134002252302));
#185307=CARTESIAN_POINT('Ctrl Pts',(108.81701691476,11.8267595165838,60.3663234140233));
#185308=CARTESIAN_POINT('Ctrl Pts',(108.924666048635,11.883579416695,60.3857640028567));
#185309=CARTESIAN_POINT('Ctrl Pts',(109.147469865246,11.9972733932899,60.425958637828));
#185310=CARTESIAN_POINT('Ctrl Pts',(109.262709192914,12.0539752970978,60.4467233268338));
#185311=CARTESIAN_POINT('Ctrl Pts',(109.51836357355,12.1751596859855,60.4927474071913));
#185312=CARTESIAN_POINT('Ctrl Pts',(109.659131381816,12.2388786151289,60.5180632099643));
#185313=CARTESIAN_POINT('Ctrl Pts',(110.152966684795,12.4519996258401,60.6068411387627));
#185314=CARTESIAN_POINT('Ctrl Pts',(110.511477807722,12.5884291439847,60.6712321388829));
#185315=CARTESIAN_POINT('Ctrl Pts',(111.110761189675,12.7865223416564,60.7791792956319));
#185316=CARTESIAN_POINT('Ctrl Pts',(111.348534779621,12.8575951696771,60.8220871967081));
#185317=CARTESIAN_POINT('Ctrl Pts',(111.696982298278,12.9507766116275,60.8851758595882));
#185318=CARTESIAN_POINT('Ctrl Pts',(111.806257456764,12.9784523627262,60.9049904016825));
#185319=CARTESIAN_POINT('Ctrl Pts',(112.024768640315,13.030698595976,60.9446820508834));
#185320=CARTESIAN_POINT('Ctrl Pts',(112.133934046305,13.0552773269553,60.9645446522991));
#185321=CARTESIAN_POINT('Ctrl Pts',(112.460585923521,13.1243201292389,61.0240600354854));
#185322=CARTESIAN_POINT('Ctrl Pts',(112.678919291209,13.1645424546652,61.0639469246329));
#185323=CARTESIAN_POINT('Ctrl Pts',(113.27156198627,13.2579522062865,61.1723764068122));
#185324=CARTESIAN_POINT('Ctrl Pts',(113.647491875916,13.3003406800254,61.2413280404868));
#185325=CARTESIAN_POINT('Ctrl Pts',(114.323869233451,13.3469353335515,61.3652690251981));
#185326=CARTESIAN_POINT('Ctrl Pts',(114.623923271277,13.3572098583343,61.4202100941643));
#185327=CARTESIAN_POINT('Ctrl Pts',(115.046956661045,13.3571445088591,61.4974474842622));
#185328=CARTESIAN_POINT('Ctrl Pts',(115.169925101734,13.3553924193983,61.5198727043834));
#185329=CARTESIAN_POINT('Ctrl Pts',(115.405198708932,13.348725025691,61.5627134105093));
#185330=CARTESIAN_POINT('Ctrl Pts',(115.517510728658,13.3440949431127,61.5831347218507));
#185331=CARTESIAN_POINT('Ctrl Pts',(115.85758979214,13.3256873097016,61.644894804552));
#185332=CARTESIAN_POINT('Ctrl Pts',(116.085139378964,13.3073995152239,61.6861169571957));
#185333=CARTESIAN_POINT('Ctrl Pts',(116.713262388815,13.2403213543822,61.7997441406783));
#185334=CARTESIAN_POINT('Ctrl Pts',(117.112572439651,13.1788886262657,61.871796494688));
#185335=CARTESIAN_POINT('Ctrl Pts',(117.769680192754,13.0460469723418,61.9904708841293));
#185336=CARTESIAN_POINT('Ctrl Pts',(118.029533828077,12.9850907459908,62.0374286321465));
#185337=CARTESIAN_POINT('Ctrl Pts',(118.404079829578,12.8847539166844,62.1052535833919));
#185338=CARTESIAN_POINT('Ctrl Pts',(118.520445138148,12.8518033841174,62.1263457761989));
#185339=CARTESIAN_POINT('Ctrl Pts',(118.737422001928,12.7869995035274,62.1657239844516));
#185340=CARTESIAN_POINT('Ctrl Pts',(118.838040288695,12.7555738559908,62.1840062924034));
#185341=CARTESIAN_POINT('Ctrl Pts',(119.137574327383,12.6579173529554,62.2384868131258));
#185342=CARTESIAN_POINT('Ctrl Pts',(119.335274950334,12.5880145499723,62.2745161405742));
#185343=CARTESIAN_POINT('Ctrl Pts',(119.869220579337,12.3844301842922,62.3718950442556));
#185344=CARTESIAN_POINT('Ctrl Pts',(120.201944627898,12.2412666976497,62.4326547766958));
#185345=CARTESIAN_POINT('Ctrl Pts',(120.773855900682,11.9666068003245,62.5368216568667));
#185346=CARTESIAN_POINT('Ctrl Pts',(121.01578349039,11.8410179525605,62.5807963174894));
#185347=CARTESIAN_POINT('Ctrl Pts',(121.358280630884,11.6495832185981,62.6427789639281));
#185348=CARTESIAN_POINT('Ctrl Pts',(121.462064458879,11.5897146565807,62.661522730782));
#185349=CARTESIAN_POINT('Ctrl Pts',(121.673215832394,11.4640744742082,62.6995707144856));
#185350=CARTESIAN_POINT('Ctrl Pts',(121.780499512891,11.3981577294354,62.7188574787436));
#185351=CARTESIAN_POINT('Ctrl Pts',(122.101041998008,11.1948906646997,62.7763631439923));
#185352=CARTESIAN_POINT('Ctrl Pts',(122.311464895034,11.0528735255313,62.8139510442209));
#185353=CARTESIAN_POINT('Ctrl Pts',(122.893478721781,10.635360077766,62.9175878177493));
#185354=CARTESIAN_POINT('Ctrl Pts',(123.255529262677,10.3460087821746,62.9816631022324));
#185355=CARTESIAN_POINT('Ctrl Pts',(123.794068310345,9.86709086608706,63.0768008267119));
#185356=CARTESIAN_POINT('Ctrl Pts',(123.981558507471,9.69027869162565,63.10988691107));
#185357=CARTESIAN_POINT('Ctrl Pts',(124.253864150465,9.41782771610808,63.1579586157631));
#185358=CARTESIAN_POINT('Ctrl Pts',(124.342683808822,9.32632345901294,63.1736415257899));
#185359=CARTESIAN_POINT('Ctrl Pts',(124.510575252109,9.14818441900784,63.203302918294));
#185360=CARTESIAN_POINT('Ctrl Pts',(124.589777868112,9.06183428159915,63.2173044726143));
#185361=CARTESIAN_POINT('Ctrl Pts',(124.902783268493,8.71115180496017,63.2726704095001));
#185362=CARTESIAN_POINT('Ctrl Pts',(125.127074376163,8.438311997959,63.3124029319295));
#185363=CARTESIAN_POINT('Ctrl Pts',(125.570375822247,7.85306020050244,63.3905698715235));
#185364=CARTESIAN_POINT('Ctrl Pts',(125.787562475328,7.5392381035402,63.4286513981591));
#185365=CARTESIAN_POINT('Ctrl Pts',(126.06390060534,7.10159865812917,63.4763939227996));
#185366=CARTESIAN_POINT('Ctrl Pts',(126.134809761169,6.98547006954439,63.4885714921778));
#185367=CARTESIAN_POINT('Ctrl Pts',(126.279413224307,6.74047198977275,63.5132546095883));
#185368=CARTESIAN_POINT('Ctrl Pts',(126.35277927908,6.61139884496046,63.5256909653223));
#185369=CARTESIAN_POINT('Ctrl Pts',(126.57029275137,6.21376842058214,63.5623112512778));
#185370=CARTESIAN_POINT('Ctrl Pts',(126.707677361444,5.94136527396956,63.5850848026988));
#185371=CARTESIAN_POINT('Ctrl Pts',(127.097179258571,5.10017515670289,63.6486932939701));
#185372=CARTESIAN_POINT('Ctrl Pts',(127.320241730258,4.51740472396742,63.6837194836451));
#185373=CARTESIAN_POINT('Ctrl Pts',(127.55469395533,3.74917435090967,63.7190974658576));
#185374=CARTESIAN_POINT('Ctrl Pts',(127.603887272878,3.57555523236867,63.7264056878772));
#185375=CARTESIAN_POINT('Ctrl Pts',(127.6837414034,3.27024422545214,63.7380736540996));
#185376=CARTESIAN_POINT('Ctrl Pts',(127.715953475882,3.13897282342005,63.742712872544));
#185377=CARTESIAN_POINT('Ctrl Pts',(127.791469551845,2.8095227410864,63.7534204685536));
#185378=CARTESIAN_POINT('Ctrl Pts',(127.832183153652,2.61100261092291,63.7590386510351));
#185379=CARTESIAN_POINT('Ctrl Pts',(127.93608630686,2.03862105746458,63.7727656608263));
#185380=CARTESIAN_POINT('Ctrl Pts',(127.987954637871,1.66259288423845,63.778773729528));
#185381=CARTESIAN_POINT('Ctrl Pts',(128.042889127933,1.08870161315972,63.7830043603928));
#185382=CARTESIAN_POINT('Ctrl Pts',(128.057430979649,0.891963419645197,
63.7835724840572));
#185383=CARTESIAN_POINT('Ctrl Pts',(128.076766242742,0.52236522668691,63.7829731526187));
#185384=CARTESIAN_POINT('Ctrl Pts',(128.082540766683,0.349555808739192,
63.7820159683859));
#185385=CARTESIAN_POINT('Ctrl Pts',(128.089034112713,-0.0953612492450678,
63.7778356498596));
#185386=CARTESIAN_POINT('Ctrl Pts',(128.08494830738,-0.36754022781548,63.7736269984285));
#185387=CARTESIAN_POINT('Ctrl Pts',(128.054662620318,-1.04635916252852,
63.7590930615933));
#185388=CARTESIAN_POINT('Ctrl Pts',(128.018466256329,-1.45254861838066,
63.7467650667485));
#185389=CARTESIAN_POINT('Ctrl Pts',(127.905720865122,-2.29229219647711,
63.7138979305539));
#185390=CARTESIAN_POINT('Ctrl Pts',(127.826149809687,-2.72545598915823,
63.6927765111203));
#185391=CARTESIAN_POINT('Ctrl Pts',(127.682735756832,-3.33597312199448,
63.6571198256226));
#185392=CARTESIAN_POINT('Ctrl Pts',(127.636052598337,-3.51753650449608,
63.6457562053938));
#185393=CARTESIAN_POINT('Ctrl Pts',(127.537139474974,-3.87104890404324,
63.6221392418014));
#185394=CARTESIAN_POINT('Ctrl Pts',(127.48522892673,-4.04303671301638,63.609947395542));
#185395=CARTESIAN_POINT('Ctrl Pts',(127.35983215172,-4.42966896154413,63.5809245515613));
#185396=CARTESIAN_POINT('Ctrl Pts',(127.284403776974,-4.64333557414903,
63.5637370540283));
#185397=CARTESIAN_POINT('Ctrl Pts',(127.08810201439,-5.15742758929339,63.5194228349989));
#185398=CARTESIAN_POINT('Ctrl Pts',(126.961651796966,-5.45561033970457,
63.4911754126882));
#185399=CARTESIAN_POINT('Ctrl Pts',(126.721950285634,-5.96885125057334,
63.437899210874));
#185400=CARTESIAN_POINT('Ctrl Pts',(126.613244129366,-6.18612506944329,
63.4138376499016));
#185401=CARTESIAN_POINT('Ctrl Pts',(126.228806746939,-6.90557805916941,
63.3291014925126));
#185402=CARTESIAN_POINT('Ctrl Pts',(125.926999873965,-7.39329765439399,
63.2631398864311));
#185403=CARTESIAN_POINT('Ctrl Pts',(125.242339179045,-8.35710750634763,
63.1149355030169));
#185404=CARTESIAN_POINT('Ctrl Pts',(124.855268790752,-8.83025003519495,
63.0318724215669));
#185405=CARTESIAN_POINT('Ctrl Pts',(124.268174871789,-9.45390692713134,
62.9071577054099));
#185406=CARTESIAN_POINT('Ctrl Pts',(124.093503188441,-9.62922064665647,
62.8701909474783));
#185407=CARTESIAN_POINT('Ctrl Pts',(123.761317826565,-9.94398538855665,
62.8001646453368));
#185408=CARTESIAN_POINT('Ctrl Pts',(123.605431083467,-10.0845840004652,
62.76741912026));
#185409=CARTESIAN_POINT('Ctrl Pts',(123.117910263833,-10.5032208846779,
62.6651988756454));
#185410=CARTESIAN_POINT('Ctrl Pts',(122.775801999737,-10.7683585796145,
62.5936132799717));
#185411=CARTESIAN_POINT('Ctrl Pts',(121.942386100403,-11.3508099273098,
62.4193000587018));
#185412=CARTESIAN_POINT('Ctrl Pts',(121.441114511936,-11.6533540788972,
62.3145802764286));
#185413=CARTESIAN_POINT('Ctrl Pts',(119.91297790932,-12.4422557176493,61.995879137436));
#185414=CARTESIAN_POINT('Ctrl Pts',(118.837482177309,-12.8315201955363,
61.772265222769));
#185415=CARTESIAN_POINT('Ctrl Pts',(117.35376376487,-13.1521509064902,61.4653674022185));
#185416=CARTESIAN_POINT('Ctrl Pts',(116.97387542283,-13.2160641974833,61.3868775472256));
#185417=CARTESIAN_POINT('Ctrl Pts',(114.895288982598,-13.4699600416556,
60.9573247662507));
#185418=CARTESIAN_POINT('Ctrl Pts',(113.157173146467,-13.3361685680301,
60.5982366964183));
#185419=CARTESIAN_POINT('Ctrl Pts',(111.165941872547,-12.7716038830549,
60.1850714064443));
#185420=CARTESIAN_POINT('Ctrl Pts',(110.825714924704,-12.6593948278489,
60.1143910742432));
#185421=CARTESIAN_POINT('Ctrl Pts',(110.081186138087,-12.3780218950513,
59.9597634374073));
#185422=CARTESIAN_POINT('Ctrl Pts',(109.680637189306,-12.2025850285081,
59.8765714240575));
#185423=CARTESIAN_POINT('Ctrl Pts',(108.46463464669,-11.5951576663429,59.6237514982524));
#185424=CARTESIAN_POINT('Ctrl Pts',(107.681880334891,-11.0944295597603,
59.460619994412));
#185425=CARTESIAN_POINT('Ctrl Pts',(106.623565344028,-10.2492312356769,
59.2383053753914));
#185426=CARTESIAN_POINT('Ctrl Pts',(106.301217433876,-9.96510114004388,
59.1703134723297));
#185427=CARTESIAN_POINT('Ctrl Pts',(105.739246669316,-9.41843069592504,
59.0511155093957));
#185428=CARTESIAN_POINT('Ctrl Pts',(105.495040866814,-9.16082429711028,
58.9990100524303));
#185429=CARTESIAN_POINT('Ctrl Pts',(105.103487043763,-8.71224724580841,
58.9152489820056));
#185430=CARTESIAN_POINT('Ctrl Pts',(104.950598413732,-8.52690380625557,
58.8825085712831));
#185431=CARTESIAN_POINT('Ctrl Pts',(104.604870287619,-8.08352746608162,
58.8083691573518));
#185432=CARTESIAN_POINT('Ctrl Pts',(104.41606482338,-7.82212053329414,58.7677928385312));
#185433=CARTESIAN_POINT('Ctrl Pts',(103.981472604273,-7.17204939697519,
58.6740466758329));
#185434=CARTESIAN_POINT('Ctrl Pts',(103.745546727541,-6.77649136647243,
58.6228481668308));
#185435=CARTESIAN_POINT('Ctrl Pts',(103.303452588012,-5.94142311213269,
58.52590543329));
#185436=CARTESIAN_POINT('Ctrl Pts',(103.099458028566,-5.50062150387374,
58.4805791170773));
#185437=CARTESIAN_POINT('Ctrl Pts',(102.825741709879,-4.81516588624815,
58.4184742886835));
#185438=CARTESIAN_POINT('Ctrl Pts',(102.738518068587,-4.57774036248472,
58.3984238208679));
#185439=CARTESIAN_POINT('Ctrl Pts',(102.56938333461,-4.07420572585244,58.3589035424022));
#185440=CARTESIAN_POINT('Ctrl Pts',(102.488880017043,-3.80760221179232,
58.3396796064654));
#185441=CARTESIAN_POINT('Ctrl Pts',(102.306178391686,-3.12675766107656,
58.2949371640255));
#185442=CARTESIAN_POINT('Ctrl Pts',(102.215099288727,-2.70906488331788,
58.2715529161298));
#185443=CARTESIAN_POINT('Ctrl Pts',(102.115375507199,-2.11463595783645,
58.2446403449956));
#185444=CARTESIAN_POINT('Ctrl Pts',(102.089899349981,-1.94213566451076,
58.2375558423345));
#185445=CARTESIAN_POINT('Ctrl Pts',(102.031527226192,-1.48574817323299,
58.2206749328734));
#185446=CARTESIAN_POINT('Ctrl Pts',(102.004287148895,-1.20110288736358,
58.2120371922918));
#185447=CARTESIAN_POINT('Ctrl Pts',(101.957204748187,-0.465989413848542,
58.1943975671659));
#185448=CARTESIAN_POINT('Ctrl Pts',(101.950697245743,-0.0145871090450379,
58.1880603225808));
#185449=CARTESIAN_POINT('Ctrl Pts',(101.979497898391,0.81521207874154,58.1842042345649));
#185450=CARTESIAN_POINT('Ctrl Pts',(102.008341185183,1.19388032184666,58.1854458145418));
#185451=CARTESIAN_POINT('Ctrl Pts',(102.074590931882,1.75552159806408,58.1915920056869));
#185452=CARTESIAN_POINT('Ctrl Pts',(102.100154072651,1.93994144346426,58.1943089792539));
#185453=CARTESIAN_POINT('Ctrl Pts',(102.157017519422,2.29653190820955,58.200900148097));
#185454=CARTESIAN_POINT('Ctrl Pts',(102.187882370866,2.4687774732748,58.2046951060956));
#185455=CARTESIAN_POINT('Ctrl Pts',(102.290119650855,2.98212696715096,58.2178187143168));
#185456=CARTESIAN_POINT('Ctrl Pts',(102.371301149614,3.32123500972588,58.2289098849127));
#185457=CARTESIAN_POINT('Ctrl Pts',(102.530608203569,3.88849320977765,58.2520241834284));
#185458=CARTESIAN_POINT('Ctrl Pts',(102.601948116002,4.11859234001682,58.2627041296762));
#185459=CARTESIAN_POINT('Ctrl Pts',(102.723885069958,4.47716221201858,58.2815531894713));
#185460=CARTESIAN_POINT('Ctrl Pts',(102.770284317948,4.60692406344235,58.288842812769));
#185461=CARTESIAN_POINT('Ctrl Pts',(102.8705386318,4.8741570529312,58.3048171564709));
#185462=CARTESIAN_POINT('Ctrl Pts',(102.924685302567,5.01150270663102,58.3135625388303));
#185463=CARTESIAN_POINT('Ctrl Pts',(103.092914039189,5.41840244215338,58.3410419072278));
#185464=CARTESIAN_POINT('Ctrl Pts',(103.213569054479,5.68513865651778,58.3611408147348));
#185465=CARTESIAN_POINT('Ctrl Pts',(103.590998532217,6.45227214745571,58.4248524127774));
#185466=CARTESIAN_POINT('Ctrl Pts',(103.870623444065,6.9410893339289,58.4730448124913));
#185467=CARTESIAN_POINT('Ctrl Pts',(104.299957315108,7.59415472485762,58.5475262349333));
#185468=CARTESIAN_POINT('Ctrl Pts',(104.425277670601,7.77503149492879,58.5693158241309));
#185469=CARTESIAN_POINT('Ctrl Pts',(104.635865489267,8.06367459540217,58.6059582701477));
#185470=CARTESIAN_POINT('Ctrl Pts',(104.718521290145,8.17341224649394,58.6203468117229));
#185471=CARTESIAN_POINT('Ctrl Pts',(104.89667119073,8.40255547130351,58.6513570157837));
#185472=CARTESIAN_POINT('Ctrl Pts',(104.99255859074,8.52164582674666,58.6680434143177));
#185473=CARTESIAN_POINT('Ctrl Pts',(105.467611677194,9.09143480230328,58.7507175916747));
#185474=CARTESIAN_POINT('Ctrl Pts',(105.874241507033,9.51855185457868,58.8215420309538));
#185475=CARTESIAN_POINT('Ctrl Pts',(106.373042354692,9.97642146938205,58.9096250944761));
#185476=CARTESIAN_POINT('Ctrl Pts',(106.439498159346,10.0361782021163,58.9213831907577));
#185477=CARTESIAN_POINT('Ctrl Pts',(106.536842319661,10.121909575254,58.9386440145915));
#185478=CARTESIAN_POINT('Ctrl Pts',(106.56725522764,10.1484435821163,58.9440419953321));
#185479=CARTESIAN_POINT('Ctrl Pts',(106.597794810055,10.1748376800446,58.9494679941055));
#185480=CARTESIAN_POINT('',(108.748391092788,-12.3027435596069,59.3669505783331));
#185481=CARTESIAN_POINT('Ctrl Pts',(108.748724298952,-12.3019154543241,
59.3675684195169));
#185482=CARTESIAN_POINT('Ctrl Pts',(107.602691759852,-11.657374533869,59.14480114862));
#185483=CARTESIAN_POINT('Ctrl Pts',(106.54648133059,-10.8459005742635,58.9394936143287));
#185484=CARTESIAN_POINT('Ctrl Pts',(104.710420613127,-8.94979049702961,
58.5825977834728));
#185485=CARTESIAN_POINT('Ctrl Pts',(103.934314629432,-7.86845478333372,
58.4317373096063));
#185486=CARTESIAN_POINT('Ctrl Pts',(102.494214638211,-5.1163968120187,58.1518088312101));
#185487=CARTESIAN_POINT('Ctrl Pts',(101.978499526416,-3.38953146267605,
58.051563468104));
#185488=CARTESIAN_POINT('Ctrl Pts',(101.694535872802,-0.397371037757389,
57.9963662498825));
#185489=CARTESIAN_POINT('Ctrl Pts',(101.662183633473,1.4774576465605,57.9900775802182));
#185490=CARTESIAN_POINT('Ctrl Pts',(102.704999893562,4.95633168042048,58.1927815387717));
#185491=CARTESIAN_POINT('Ctrl Pts',(103.278228008759,6.181755194884,58.304206353048));
#185492=CARTESIAN_POINT('Ctrl Pts',(104.735425788297,8.38385488749155,58.5874583214079));
#185493=CARTESIAN_POINT('Ctrl Pts',(105.604862919118,9.35048684197738,58.7564606230372));
#185494=CARTESIAN_POINT('Ctrl Pts',(106.597794810055,10.1748376800446,58.9494679941055));
#185495=CARTESIAN_POINT('',(108.827755276219,-12.3460198217725,59.3829305619696));
#185496=CARTESIAN_POINT('Ctrl Pts',(108.827755276219,-12.3460198217725,
59.3829305619696));
#185497=CARTESIAN_POINT('Ctrl Pts',(108.801111662428,-12.3319613983389,
59.3775671848589));
#185498=CARTESIAN_POINT('Ctrl Pts',(108.774513616443,-12.3178132353077,
59.3722126652767));
#185499=CARTESIAN_POINT('Ctrl Pts',(108.747961719012,-12.3035756411923,
59.3668671161093));
#185500=CARTESIAN_POINT('Ctrl Pts',(108.827755276219,-12.3460198217725,
59.3829305619696));
#185501=CARTESIAN_POINT('Ctrl Pts',(109.261234383337,-12.5750413194122,
59.4732046875812));
#185502=CARTESIAN_POINT('Ctrl Pts',(109.706466269681,-12.7800813106308,
59.5658999124667));
#185503=CARTESIAN_POINT('Ctrl Pts',(110.41126587268,-13.0591110129488,59.7123004931389));
#185504=CARTESIAN_POINT('Ctrl Pts',(110.663792636116,-13.1504229782856,
59.7646880006138));
#185505=CARTESIAN_POINT('Ctrl Pts',(111.388554457391,-13.3881353111418,
59.9146985118048));
#185506=CARTESIAN_POINT('Ctrl Pts',(111.866231409931,-13.5160120037384,
60.0131245420342));
#185507=CARTESIAN_POINT('Ctrl Pts',(112.843955012572,-13.7205230380231,
60.2144696807969));
#185508=CARTESIAN_POINT('Ctrl Pts',(113.343506898725,-13.7957831208322,
60.3172903773583));
#185509=CARTESIAN_POINT('Ctrl Pts',(114.257307723694,-13.8808602579056,
60.5056637641811));
#185510=CARTESIAN_POINT('Ctrl Pts',(114.669849720597,-13.9,60.5908085805516));
#185511=CARTESIAN_POINT('Ctrl Pts',(115.082307292334,-13.9,60.6760422812756));
#185512=CARTESIAN_POINT('',(114.641143207841,-13.3595548147716,62.9456702505604));
#185513=CARTESIAN_POINT('Ctrl Pts',(124.127322289755,-8.93395457648499,
66.2032737914971));
#185514=CARTESIAN_POINT('Ctrl Pts',(122.805272603048,-10.43663118481,65.9217654640849));
#185515=CARTESIAN_POINT('Ctrl Pts',(119.481298892218,-12.81680175343,65.226593965893));
#185516=CARTESIAN_POINT('Ctrl Pts',(113.463801884159,-13.79335473887,63.9833253455664));
#185517=CARTESIAN_POINT('Ctrl Pts',(107.636855155043,-11.97726991923,62.7770961322029));
#185518=CARTESIAN_POINT('Ctrl Pts',(103.182583853411,-7.73653374972899,
61.8376893242906));
#185519=CARTESIAN_POINT('Ctrl Pts',(101.00559514138,-1.92956717280499,61.3409436191289));
#185520=CARTESIAN_POINT('Ctrl Pts',(101.549375432396,4.26802286533402,61.3730644730488));
#185521=CARTESIAN_POINT('Ctrl Pts',(104.706635557586,9.60158040629401,61.9131968801661));
#185522=CARTESIAN_POINT('Ctrl Pts',(109.840997033316,12.99135922774,62.8376407768088));
#185523=CARTESIAN_POINT('Ctrl Pts',(115.915831602521,13.75112083595,63.9448950363666));
#185524=CARTESIAN_POINT('Ctrl Pts',(121.704118510716,11.72705615912,64.9964497950401));
#185525=CARTESIAN_POINT('Ctrl Pts',(126.036844041747,7.32892445847002,65.7650706713404));
#185526=CARTESIAN_POINT('Ctrl Pts',(128.039674084356,1.44709807664901,66.0808034823172));
#185527=CARTESIAN_POINT('Ctrl Pts',(127.309907448893,-4.72768050995399,
65.8653706556117));
#185528=CARTESIAN_POINT('Ctrl Pts',(123.998186958828,-9.94538363148499,
65.1480543359445));
#185529=CARTESIAN_POINT('Ctrl Pts',(118.777305515395,-13.14965866642,64.0596328680601));
#185530=CARTESIAN_POINT('Ctrl Pts',(114.731505652229,-13.51125452112,63.2241518790638));
#185531=CARTESIAN_POINT('Ctrl Pts',(112.771522436493,-13.22996072786,62.818641216267));
#185532=CARTESIAN_POINT('Ctrl Pts',(124.14684851148,-8.93395457648499,66.102820590392));
#185533=CARTESIAN_POINT('Ctrl Pts',(122.824798824771,-10.43663118481,65.8213122629897));
#185534=CARTESIAN_POINT('Ctrl Pts',(119.500825113942,-12.81680175343,65.1261407647978));
#185535=CARTESIAN_POINT('Ctrl Pts',(113.483328105883,-13.79335473887,63.8828721444713));
#185536=CARTESIAN_POINT('Ctrl Pts',(107.656381376766,-11.97726991923,62.6766429311077));
#185537=CARTESIAN_POINT('Ctrl Pts',(103.202110075135,-7.73653374972899,
61.7372361231954));
#185538=CARTESIAN_POINT('Ctrl Pts',(101.025121363104,-1.92956717280499,
61.2404904180337));
#185539=CARTESIAN_POINT('Ctrl Pts',(101.568901654119,4.26802286533402,61.2726112719536));
#185540=CARTESIAN_POINT('Ctrl Pts',(104.72616177931,9.60158040629401,61.8127436790709));
#185541=CARTESIAN_POINT('Ctrl Pts',(109.860523255039,12.99135922774,62.7371875757135));
#185542=CARTESIAN_POINT('Ctrl Pts',(115.935357824245,13.75112083595,63.8444418352714));
#185543=CARTESIAN_POINT('Ctrl Pts',(121.72364473244,11.72705615912,64.8959965939449));
#185544=CARTESIAN_POINT('Ctrl Pts',(126.056370263471,7.32892445847002,65.6646174702451));
#185545=CARTESIAN_POINT('Ctrl Pts',(128.05920030608,1.44709807664901,65.980350281222));
#185546=CARTESIAN_POINT('Ctrl Pts',(127.329433670617,-4.72768050995399,
65.7649174545165));
#185547=CARTESIAN_POINT('Ctrl Pts',(124.017713180552,-9.94538363148499,
65.0476011348493));
#185548=CARTESIAN_POINT('Ctrl Pts',(118.796831737119,-13.14965866642,63.9591796669649));
#185549=CARTESIAN_POINT('Ctrl Pts',(114.751031873954,-13.51125452112,63.1236986779588));
#185550=CARTESIAN_POINT('Ctrl Pts',(112.791048658217,-13.22996072786,62.7181880151718));
#185551=CARTESIAN_POINT('Ctrl Pts',(124.166374733204,-8.93395457648499,
66.0023673892968));
#185552=CARTESIAN_POINT('Ctrl Pts',(122.844325046497,-10.43663118481,65.7208590618847));
#185553=CARTESIAN_POINT('Ctrl Pts',(119.520351335665,-12.81680175343,65.0256875637026));
#185554=CARTESIAN_POINT('Ctrl Pts',(113.502854327606,-13.79335473887,63.782418943376));
#185555=CARTESIAN_POINT('Ctrl Pts',(107.67590759849,-11.97726991923,62.5761897300125));
#185556=CARTESIAN_POINT('Ctrl Pts',(103.221636296858,-7.73653374972899,
61.6367829221002));
#185557=CARTESIAN_POINT('Ctrl Pts',(101.044647584827,-1.92956717280499,
61.1400372169385));
#185558=CARTESIAN_POINT('Ctrl Pts',(101.588427875843,4.26802286533402,61.1721580708584));
#185559=CARTESIAN_POINT('Ctrl Pts',(104.745688001033,9.60158040629401,61.7122904779757));
#185560=CARTESIAN_POINT('Ctrl Pts',(109.880049476763,12.99135922774,62.6367343746183));
#185561=CARTESIAN_POINT('Ctrl Pts',(115.954884045968,13.75112083595,63.7439886341762));
#185562=CARTESIAN_POINT('Ctrl Pts',(121.743170954163,11.72705615912,64.7955433928497));
#185563=CARTESIAN_POINT('Ctrl Pts',(126.075896485195,7.32892445847002,65.5641642691499));
#185564=CARTESIAN_POINT('Ctrl Pts',(128.078726527803,1.44709807664901,65.8798970801268));
#185565=CARTESIAN_POINT('Ctrl Pts',(127.34895989234,-4.72768050995399,65.6644642534212));
#185566=CARTESIAN_POINT('Ctrl Pts',(124.037239402277,-9.94538363148499,
64.9471479337443));
#185567=CARTESIAN_POINT('Ctrl Pts',(118.816357958844,-13.14965866642,63.8587264658599));
#185568=CARTESIAN_POINT('Ctrl Pts',(114.770558095677,-13.51125452112,63.0232454768636));
#185569=CARTESIAN_POINT('Ctrl Pts',(112.810574879942,-13.22996072786,62.6177348140668));
#185570=CARTESIAN_POINT('Ctrl Pts',(124.185900954927,-8.93395457648499,
65.9019141882016));
#185571=CARTESIAN_POINT('Ctrl Pts',(122.86385126822,-10.43663118481,65.6204058607894));
#185572=CARTESIAN_POINT('Ctrl Pts',(119.539877557389,-12.81680175343,64.9252343626074));
#185573=CARTESIAN_POINT('Ctrl Pts',(113.52238054933,-13.79335473887,63.6819657422808));
#185574=CARTESIAN_POINT('Ctrl Pts',(107.695433820213,-11.97726991923,62.4757365289173));
#185575=CARTESIAN_POINT('Ctrl Pts',(103.241162518582,-7.73653374972899,
61.536329721005));
#185576=CARTESIAN_POINT('Ctrl Pts',(101.064173806551,-1.92956717280499,
61.0395840158433));
#185577=CARTESIAN_POINT('Ctrl Pts',(101.607954097566,4.26802286533402,61.0717048697632));
#185578=CARTESIAN_POINT('Ctrl Pts',(104.765214222759,9.60158040629401,61.6118372768707));
#185579=CARTESIAN_POINT('Ctrl Pts',(109.899575698488,12.99135922774,62.5362811735133));
#185580=CARTESIAN_POINT('Ctrl Pts',(115.974410267694,13.75112083595,63.6435354330712));
#185581=CARTESIAN_POINT('Ctrl Pts',(121.762697175889,11.72705615912,64.6950901917447));
#185582=CARTESIAN_POINT('Ctrl Pts',(126.09542270692,7.32892445847002,65.4637110680449));
#185583=CARTESIAN_POINT('Ctrl Pts',(128.098252749529,1.44709807664901,65.7794438790217));
#185584=CARTESIAN_POINT('Ctrl Pts',(127.368486114066,-4.72768050995399,
65.5640110523162));
#185585=CARTESIAN_POINT('Ctrl Pts',(124.056765624,-9.94538363148499,64.8466947326491));
#185586=CARTESIAN_POINT('Ctrl Pts',(118.835884180567,-13.14965866642,63.7582732647647));
#185587=CARTESIAN_POINT('Ctrl Pts',(114.790084317401,-13.51125452112,62.9227922757684));
#185588=CARTESIAN_POINT('Ctrl Pts',(112.830101101666,-13.22996072786,62.5172816129716));
#185589=CARTESIAN_POINT('',(114.602947212677,-13.3588269031369,63.1421432529824));
#185590=CARTESIAN_POINT('',(114.602824644425,-13.358908889387,63.1427506256491));
#185591=CARTESIAN_POINT('',(122.863635671064,-10.2286061806799,65.6766524048838));
#185592=CARTESIAN_POINT('Ctrl Pts',(122.863760060438,-10.2287368491257,
65.6765769614792));
#185593=CARTESIAN_POINT('Ctrl Pts',(122.240146213124,-10.7632276682405,
65.5458260535504));
#185594=CARTESIAN_POINT('Ctrl Pts',(121.567667527631,-11.2386000580356,
65.4056673900111));
#185595=CARTESIAN_POINT('Ctrl Pts',(120.422256010174,-11.8971524039626,
65.1659826384782));
#185596=CARTESIAN_POINT('Ctrl Pts',(119.972280261939,-12.1223443916377,
65.0716961849902));
#185597=CARTESIAN_POINT('Ctrl Pts',(119.154752940445,-12.4727659840031,
64.90127152028));
#185598=CARTESIAN_POINT('Ctrl Pts',(118.792474245388,-12.6087267809308,
64.8260808448027));
#185599=CARTESIAN_POINT('Ctrl Pts',(117.712268209454,-12.9595326876314,
64.602483820945));
#185600=CARTESIAN_POINT('Ctrl Pts',(116.979574018507,-13.1284662514209,
64.4515484121121));
#185601=CARTESIAN_POINT('Ctrl Pts',(115.382030528533,-13.3538641526337,
64.1216421923012));
#185602=CARTESIAN_POINT('Ctrl Pts',(114.514268176837,-13.3888157087188,
63.94123680514));
#185603=CARTESIAN_POINT('Ctrl Pts',(112.882163285328,-13.2871455157589,
63.6027834419524));
#185604=CARTESIAN_POINT('Ctrl Pts',(112.117935990712,-13.168500674772,63.4451730291947));
#185605=CARTESIAN_POINT('Ctrl Pts',(110.576772771736,-12.7865358856342,
63.1269643432183));
#185606=CARTESIAN_POINT('Ctrl Pts',(109.800877120059,-12.5144474866061,
62.9664816746769));
#185607=CARTESIAN_POINT('Ctrl Pts',(108.744124181976,-12.0270341854416,
62.7459016018925));
#185608=CARTESIAN_POINT('Ctrl Pts',(108.437034204304,-11.8702494054068,
62.6816086394531));
#185609=CARTESIAN_POINT('Ctrl Pts',(107.367383543376,-11.2685768566542,
62.4577116956883));
#185610=CARTESIAN_POINT('Ctrl Pts',(106.644130952332,-10.7566383761923,
62.3068071526653));
#185611=CARTESIAN_POINT('Ctrl Pts',(105.39940592417,-9.6747655290772,62.0455752822621));
#185612=CARTESIAN_POINT('Ctrl Pts',(104.862872271295,-9.12003284756065,
61.9322384738739));
#185613=CARTESIAN_POINT('Ctrl Pts',(104.013688156968,-8.07338890431674,
61.7498632067556));
#185614=CARTESIAN_POINT('Ctrl Pts',(103.678542159989,-7.60034210331702,
61.6770036424679));
#185615=CARTESIAN_POINT('Ctrl Pts',(102.965863098996,-6.43776000726343,
61.5216204731177));
#185616=CARTESIAN_POINT('Ctrl Pts',(102.615546714304,-5.73384448039941,
61.4445272154993));
#185617=CARTESIAN_POINT('Ctrl Pts',(102.124533339922,-4.48787726460851,
61.3334637104734));
#185618=CARTESIAN_POINT('Ctrl Pts',(101.952461547406,-3.95857885737421,
61.2934636788593));
#185619=CARTESIAN_POINT('Ctrl Pts',(101.596124566779,-2.57950115143769,
61.2064914408388));
#185620=CARTESIAN_POINT('Ctrl Pts',(101.460405992341,-1.72069010498245,
61.1685699439471));
#185621=CARTESIAN_POINT('Ctrl Pts',(101.364478811265,-0.109464886862312,
61.1305919156548));
#185622=CARTESIAN_POINT('Ctrl Pts',(101.38098315129,0.634328801104304,61.1253212132384));
#185623=CARTESIAN_POINT('Ctrl Pts',(101.63922130165,3.13169786388764,61.1460319840433));
#185624=CARTESIAN_POINT('Ctrl Pts',(102.159133504572,4.82979500457738,61.2240371490054));
#185625=CARTESIAN_POINT('Ctrl Pts',(103.322134470119,6.99422477083511,61.4213202159224));
#185626=CARTESIAN_POINT('Ctrl Pts',(103.694429784937,7.57614415877838,61.485614547929));
#185627=CARTESIAN_POINT('Ctrl Pts',(104.504460129801,8.6506071400515,61.6264142201267));
#185628=CARTESIAN_POINT('Ctrl Pts',(104.938756384371,9.14611593047081,61.7021075136189));
#185629=CARTESIAN_POINT('Ctrl Pts',(106.013631261799,10.1996857606197,61.8923389269699));
#185630=CARTESIAN_POINT('Ctrl Pts',(106.673833749292,10.7324870133182,62.0107815663951));
#185631=CARTESIAN_POINT('Ctrl Pts',(107.929893822727,11.5626987947379,62.2370448228732));
#185632=CARTESIAN_POINT('Ctrl Pts',(108.509340409586,11.8861695854614,62.3417170605054));
#185633=CARTESIAN_POINT('Ctrl Pts',(109.416432484761,12.3056267423368,62.5053407714911));
#185634=CARTESIAN_POINT('Ctrl Pts',(109.728875559953,12.4355663395387,62.5616480894726));
#185635=CARTESIAN_POINT('Ctrl Pts',(110.70474560647,12.7968216736441,62.7380392767041));
#185636=CARTESIAN_POINT('Ctrl Pts',(111.382980529343,12.9861920178074,62.8613660333791));
#185637=CARTESIAN_POINT('Ctrl Pts',(112.897689287169,13.2803590562696,63.1372980237683));
#185638=CARTESIAN_POINT('Ctrl Pts',(113.73892015981,13.3607725717846,63.2908580231773));
#185639=CARTESIAN_POINT('Ctrl Pts',(115.336533881722,13.3577945987543,63.5814699441069));
#185640=CARTESIAN_POINT('Ctrl Pts',(116.089542267633,13.2900526257154,63.7178997427436));
#185641=CARTESIAN_POINT('Ctrl Pts',(117.93552764734,12.9565936607203,64.0535767474533));
#185642=CARTESIAN_POINT('Ctrl Pts',(119.009875870491,12.6151247506599,64.249334419709));
#185643=CARTESIAN_POINT('Ctrl Pts',(120.81305748656,11.7764189739414,64.5754658880205));
#185644=CARTESIAN_POINT('Ctrl Pts',(121.563089340139,11.3323021474241,64.7099299890663));
#185645=CARTESIAN_POINT('Ctrl Pts',(122.967289886509,10.2955208016799,64.961412049232));
#185646=CARTESIAN_POINT('Ctrl Pts',(123.616910763818,9.70826883189277,65.0773620752841));
#185647=CARTESIAN_POINT('Ctrl Pts',(125.379639856623,7.77153764746681,65.3885685191679));
#185648=CARTESIAN_POINT('Ctrl Pts',(126.286223890547,6.26842056998774,65.5428342292009));
#185649=CARTESIAN_POINT('Ctrl Pts',(127.183326724953,3.80455012558783,65.6859140196455));
#185650=CARTESIAN_POINT('Ctrl Pts',(127.403096581131,2.95846085195509,65.7182734354822));
#185651=CARTESIAN_POINT('Ctrl Pts',(127.637259599455,1.48709831544551,65.7454000803788));
#185652=CARTESIAN_POINT('Ctrl Pts',(127.691878872173,0.871913947897259,
65.7482971122607));
#185653=CARTESIAN_POINT('Ctrl Pts',(127.721704073428,-0.606022111551587,
65.7361311720197));
#185654=CARTESIAN_POINT('Ctrl Pts',(127.65734862261,-1.46774389326394,65.7133866238823));
#185655=CARTESIAN_POINT('Ctrl Pts',(127.218712115104,-4.04807163087889,
65.5966903809948));
#185656=CARTESIAN_POINT('Ctrl Pts',(126.594225323066,-5.69141216598206,
65.453722271121));
#185657=CARTESIAN_POINT('Ctrl Pts',(125.215914647381,-7.9075058974082,65.1542271548029));
#185658=CARTESIAN_POINT('Ctrl Pts',(124.6871438061,-8.59902863606933,65.040956822351));
#185659=CARTESIAN_POINT('Ctrl Pts',(123.809248021861,-9.53891006775381,
64.8544140425203));
#185660=CARTESIAN_POINT('Ctrl Pts',(123.508026186193,-9.83152877276116,
64.7906250911458));
#185661=CARTESIAN_POINT('Ctrl Pts',(122.019233236213,-11.144075489692,64.4766947679153));
#185662=CARTESIAN_POINT('Ctrl Pts',(120.663321346316,-11.9644757376867,
64.1941836778649));
#185663=CARTESIAN_POINT('Ctrl Pts',(118.479168800975,-12.7973455816125,
63.7406749481653));
#185664=CARTESIAN_POINT('Ctrl Pts',(117.727272371115,-13.006653057488,63.5848280374823));
#185665=CARTESIAN_POINT('Ctrl Pts',(116.19741872317,-13.287327677289,63.2681653310725));
#185666=CARTESIAN_POINT('Ctrl Pts',(115.419179639328,-13.3583908138007,
63.1072579646956));
#185667=CARTESIAN_POINT('Ctrl Pts',(114.640998168921,-13.3589088887046,
62.9463713323102));
#185668=CARTESIAN_POINT('',(107.485627742127,-11.3335893001804,62.6876626706917));
#185669=CARTESIAN_POINT('Ctrl Pts',(107.485561672623,-11.3337498925587,
62.6875423325866));
#185670=CARTESIAN_POINT('Ctrl Pts',(107.614804142611,-11.4160091339019,
62.7126646492232));
#185671=CARTESIAN_POINT('Ctrl Pts',(107.745249943893,-11.4958117911507,
62.7380208709361));
#185672=CARTESIAN_POINT('Ctrl Pts',(107.876899835385,-11.5731613609192,
62.763611145244));
#185673=CARTESIAN_POINT('Ctrl Pts',(108.061365151314,-11.6815421021619,
62.7994677493131));
#185674=CARTESIAN_POINT('Ctrl Pts',(108.24819346307,-11.78510864237,62.8357836755335));
#185675=CARTESIAN_POINT('Ctrl Pts',(108.437354282934,-11.8839349705715,
62.8725529976636));
#185676=CARTESIAN_POINT('Ctrl Pts',(108.6328913266,-11.9860925318822,62.9105617383324));
#185677=CARTESIAN_POINT('Ctrl Pts',(108.83092107342,-12.083185339433,62.9490550138287));
#185678=CARTESIAN_POINT('Ctrl Pts',(109.031436582887,-12.1752440931379,
62.9880314750483));
#185679=CARTESIAN_POINT('Ctrl Pts',(109.22430368395,-12.263791383079,63.0255212288587));
#185680=CARTESIAN_POINT('Ctrl Pts',(109.419468438602,-12.3476802430602,
63.0634576035127));
#185681=CARTESIAN_POINT('Ctrl Pts',(109.61695720614,-12.4268962909364,63.1018457227644));
#185682=CARTESIAN_POINT('Ctrl Pts',(109.771926507834,-12.4890570698777,
63.1319688538566));
#185683=CARTESIAN_POINT('Ctrl Pts',(109.928326637475,-12.5483393104261,
63.1623701111152));
#185684=CARTESIAN_POINT('Ctrl Pts',(110.086172426641,-12.6047129308209,
63.1930523775215));
#185685=CARTESIAN_POINT('Ctrl Pts',(110.130137395395,-12.6204147399875,
63.2015983443858));
#185686=CARTESIAN_POINT('Ctrl Pts',(110.174214539726,-12.635890784121,63.2101661160821));
#185687=CARTESIAN_POINT('Ctrl Pts',(110.218404225387,-12.6511401433646,
63.218755763706));
#185688=CARTESIAN_POINT('Ctrl Pts',(110.254123274814,-12.6634663821332,
63.2256988782237));
#185689=CARTESIAN_POINT('Ctrl Pts',(110.289911272532,-12.6756430115032,
63.2326553949984));
#185690=CARTESIAN_POINT('Ctrl Pts',(110.32579415179,-12.6876780033411,63.2396303549681));
#185691=CARTESIAN_POINT('Ctrl Pts',(110.473374762606,-12.7371760225445,
63.268317262876));
#185692=CARTESIAN_POINT('Ctrl Pts',(110.622478207417,-12.7842446063055,
63.2973001812039));
#185693=CARTESIAN_POINT('Ctrl Pts',(110.772679057295,-12.8286913645498,
63.3264964145326));
#185694=CARTESIAN_POINT('Ctrl Pts',(110.885625137274,-12.8621138592661,
63.3484510180337));
#185695=CARTESIAN_POINT('Ctrl Pts',(110.999191292185,-12.8940547885104,
63.3705261524935));
#185696=CARTESIAN_POINT('Ctrl Pts',(111.113190270013,-12.9244506654267,
63.3926854196253));
#185697=CARTESIAN_POINT('Ctrl Pts',(111.154854057468,-12.9355596014846,
63.400784079925));
#185698=CARTESIAN_POINT('Ctrl Pts',(111.196575611453,-12.9464623161029,
63.4088939689567));
#185699=CARTESIAN_POINT('Ctrl Pts',(111.238345640527,-12.9571562472333,
63.4170132806382));
#185700=CARTESIAN_POINT('Ctrl Pts',(111.266446655741,-12.9643506478132,
63.4224755919209));
#185701=CARTESIAN_POINT('Ctrl Pts',(111.294573102417,-12.9714513970515,
63.4279428466037));
#185702=CARTESIAN_POINT('Ctrl Pts',(111.322698384524,-12.9784519718767,
63.4334098749161));
#185703=CARTESIAN_POINT('Ctrl Pts',(111.536825921765,-13.0317497784859,
63.475032259506));
#185704=CARTESIAN_POINT('Ctrl Pts',(111.751164558969,-13.0793184605927,
63.5166956779769));
#185705=CARTESIAN_POINT('Ctrl Pts',(111.965659100288,-13.1212776219255,
63.5583894012888));
#185706=CARTESIAN_POINT('Ctrl Pts',(112.181521726303,-13.163504406323,63.6003490546542));
#185707=CARTESIAN_POINT('Ctrl Pts',(112.397542665596,-13.2000500000777,
63.642339481157));
#185708=CARTESIAN_POINT('Ctrl Pts',(112.613688198126,-13.2309885564611,
63.6843541262526));
#185709=CARTESIAN_POINT('Ctrl Pts',(112.830693324041,-13.2620501529929,
63.7265358602099));
#185710=CARTESIAN_POINT('Ctrl Pts',(113.047824453117,-13.2874601398532,
63.7687420868227));
#185711=CARTESIAN_POINT('Ctrl Pts',(113.265063829592,-13.3072438790148,
63.8109693547035));
#185712=CARTESIAN_POINT('Ctrl Pts',(113.350228480118,-13.3149997253955,
63.827523768411));
#185713=CARTESIAN_POINT('Ctrl Pts',(113.435409910131,-13.3218903354083,
63.8440814437367));
#185714=CARTESIAN_POINT('Ctrl Pts',(113.520607519528,-13.327915104691,63.8606422640318));
#185715=CARTESIAN_POINT('Ctrl Pts',(113.736958181362,-13.343214393379,63.9026967824238));
#185716=CARTESIAN_POINT('Ctrl Pts',(113.953412858971,-13.3529339642487,
63.9447715195353));
#185717=CARTESIAN_POINT('Ctrl Pts',(114.169957504393,-13.3571513294797,
63.9868637447053));
#185718=CARTESIAN_POINT('Ctrl Pts',(114.390268030086,-13.3614420379812,
64.0296879864995));
#185719=CARTESIAN_POINT('Ctrl Pts',(114.61067211477,-13.3600375840576,64.0725304144101));
#185720=CARTESIAN_POINT('Ctrl Pts',(114.831156415951,-13.3529648919269,
64.1153884349059));
#185721=CARTESIAN_POINT('Ctrl Pts',(114.927618297717,-13.3498705891197,
64.1341388188728));
#185722=CARTESIAN_POINT('Ctrl Pts',(115.024095512377,-13.345690645084,64.1528921832671));
#185723=CARTESIAN_POINT('Ctrl Pts',(115.120586694554,-13.3404240435081,
64.1716482626854));
#185724=CARTESIAN_POINT('Ctrl Pts',(115.172274692604,-13.337602852122,64.181695441863));
#185725=CARTESIAN_POINT('Ctrl Pts',(115.223966694672,-13.3344698120586,
64.1917433993467));
#185726=CARTESIAN_POINT('Ctrl Pts',(115.275662457027,-13.331024533966,64.2017920877599));
#185727=CARTESIAN_POINT('Ctrl Pts',(115.300632026009,-13.329360430274,64.2066457045184));
#185728=CARTESIAN_POINT('Ctrl Pts',(115.32560247186,-13.3276234794556,64.2114994917237));
#185729=CARTESIAN_POINT('Ctrl Pts',(115.350573764693,-13.3258136240892,
64.2163534435667));
#185730=CARTESIAN_POINT('Ctrl Pts',(115.369789998032,-13.3244208806993,
64.2200887195836));
#185731=CARTESIAN_POINT('Ctrl Pts',(115.389005122721,-13.3229850672834,
64.2238237800996));
#185732=CARTESIAN_POINT('Ctrl Pts',(115.408209864803,-13.3215069300936,
64.2275568224313));
#185733=CARTESIAN_POINT('Ctrl Pts',(115.620264914641,-13.3051856249646,
64.2687763542688));
#185734=CARTESIAN_POINT('Ctrl Pts',(115.831369254668,-13.2836859243608,
64.3098110859172));
#185735=CARTESIAN_POINT('Ctrl Pts',(116.041541009532,-13.2570867575058,
64.3506645404687));
#185736=CARTESIAN_POINT('Ctrl Pts',(116.252521508358,-13.2303852366707,
64.3916751997061));
#185737=CARTESIAN_POINT('Ctrl Pts',(116.462562646362,-13.1985448687571,
64.4325032647852));
#185738=CARTESIAN_POINT('Ctrl Pts',(116.671680915997,-13.1615929593013,
64.4731519415302));
#185739=CARTESIAN_POINT('Ctrl Pts',(116.880751147312,-13.1246495383798,
64.5137912805254));
#185740=CARTESIAN_POINT('Ctrl Pts',(117.088899348997,-13.0825968505039,
64.5542513942214));
#185741=CARTESIAN_POINT('Ctrl Pts',(117.296133937521,-13.0354108225876,
64.5945339186226));
#185742=CARTESIAN_POINT('Ctrl Pts',(117.501753324005,-12.9885925661379,
64.6345024779852));
#185743=CARTESIAN_POINT('Ctrl Pts',(117.70647367483,-12.9367205635069,64.6742962816465));
#185744=CARTESIAN_POINT('Ctrl Pts',(117.91028928519,-12.8797222224478,64.7139142206988));
#185745=CARTESIAN_POINT('Ctrl Pts',(118.031475045392,-12.8458318483036,
64.7374704637815));
#185746=CARTESIAN_POINT('Ctrl Pts',(118.152340658396,-12.8101282247323,
64.7609644762425));
#185747=CARTESIAN_POINT('Ctrl Pts',(118.272881693326,-12.7725879900098,
64.7843953968021));
#185748=CARTESIAN_POINT('Ctrl Pts',(118.303191203236,-12.7631486640822,
64.7902869981089));
#185749=CARTESIAN_POINT('Ctrl Pts',(118.33348017807,-12.7535931889409,64.7961746077812));
#185750=CARTESIAN_POINT('Ctrl Pts',(118.363748518854,-12.7439211333848,
64.8020582065804));
#185751=CARTESIAN_POINT('Ctrl Pts',(118.395124158262,-12.7338952476039,
64.8081570435028));
#185752=CARTESIAN_POINT('Ctrl Pts',(118.426470549753,-12.7237463489279,
64.8142501951775));
#185753=CARTESIAN_POINT('Ctrl Pts',(118.457784720862,-12.7134750686029,
64.8203370838131));
#185754=CARTESIAN_POINT('Ctrl Pts',(118.598547337112,-12.6673038866874,
64.8476987012161));
#185755=CARTESIAN_POINT('Ctrl Pts',(118.738697794193,-12.6186516797937,
64.874941326337));
#185756=CARTESIAN_POINT('Ctrl Pts',(118.878489383028,-12.5673757495857,
64.9021141941889));
#185757=CARTESIAN_POINT('Ctrl Pts',(118.956946557128,-12.5385974474216,
64.917364800049));
#185758=CARTESIAN_POINT('Ctrl Pts',(119.035290365746,-12.508991816977,64.9325933697815));
#185759=CARTESIAN_POINT('Ctrl Pts',(119.113562750043,-12.478526951352,64.9478080559632));
#185760=CARTESIAN_POINT('Ctrl Pts',(119.152698942191,-12.4632945185395,
64.955415399054));
#185761=CARTESIAN_POINT('Ctrl Pts',(119.191817243841,-12.4478472018354,
64.963019264567));
#185762=CARTESIAN_POINT('Ctrl Pts',(119.230922679739,-12.4321805612555,
64.9706206292184));
#185763=CARTESIAN_POINT('Ctrl Pts',(119.251451510466,-12.4239561851514,
64.9746110495946));
#185764=CARTESIAN_POINT('Ctrl Pts',(119.271976793086,-12.4156713618556,
64.9786007802852));
#185765=CARTESIAN_POINT('Ctrl Pts',(119.292499237416,-12.4073254157032,
64.9825899592652));
#185766=CARTESIAN_POINT('Ctrl Pts',(119.306734613276,-12.4015362573318,
64.9853570498342));
#185767=CARTESIAN_POINT('Ctrl Pts',(119.320968623249,-12.3957176892737,
64.9881238749001));
#185768=CARTESIAN_POINT('Ctrl Pts',(119.335201500787,-12.3898694795256,
64.9908904798418));
#185769=CARTESIAN_POINT('Ctrl Pts',(119.339536190148,-12.3880883799194,
64.9917330623046));
#185770=CARTESIAN_POINT('Ctrl Pts',(119.343870997956,-12.3863044387621,
64.9925756677911));
#185771=CARTESIAN_POINT('Ctrl Pts',(119.348205220554,-12.384517942185,64.9934181595239));
#185772=CARTESIAN_POINT('Ctrl Pts',(119.544789338538,-12.3034891426856,
65.031630431838));
#185773=CARTESIAN_POINT('Ctrl Pts',(119.738478069006,-12.2179058838895,
65.0692798950231));
#185774=CARTESIAN_POINT('Ctrl Pts',(119.929341495406,-12.1279359966252,
65.1063801719896));
#185775=CARTESIAN_POINT('Ctrl Pts',(120.122558815125,-12.0368565226763,
65.1439380017504));
#185776=CARTESIAN_POINT('Ctrl Pts',(120.31288104309,-11.9412813697266,65.1809330798728));
#185777=CARTESIAN_POINT('Ctrl Pts',(120.50036917076,-11.841332181931,65.2173772619545));
#185778=CARTESIAN_POINT('Ctrl Pts',(120.689606070474,-11.7404507305963,
65.2541613725831));
#185779=CARTESIAN_POINT('Ctrl Pts',(120.875956098769,-11.6351130659804,
65.2903843294525));
#185780=CARTESIAN_POINT('Ctrl Pts',(121.059464992335,-11.5253941026604,
65.3260550229191));
#185781=CARTESIAN_POINT('Ctrl Pts',(121.244274503297,-11.4148975073162,
65.3619785320589));
#185782=CARTESIAN_POINT('Ctrl Pts',(121.426202823407,-11.2999570785843,
65.3973419916353));
#185783=CARTESIAN_POINT('Ctrl Pts',(121.605274210285,-11.180601831691,65.4321501168758));
#185784=CARTESIAN_POINT('Ctrl Pts',(121.784368612727,-11.061231244389,65.4669627159108));
#185785=CARTESIAN_POINT('Ctrl Pts',(121.960605693043,-10.9374444567741,
65.5012199050162));
#185786=CARTESIAN_POINT('Ctrl Pts',(122.133982072171,-10.8092266649049,
65.5349210273653));
#185787=CARTESIAN_POINT('Ctrl Pts',(122.306425892347,-10.6816985324356,
65.5684408777125));
#185788=CARTESIAN_POINT('Ctrl Pts',(122.476040026031,-10.5497866711897,
65.6014106899798));
#185789=CARTESIAN_POINT('Ctrl Pts',(122.642788850821,-10.4134370267834,
65.6338235398391));
#185790=CARTESIAN_POINT('Ctrl Pts',(122.717000904232,-10.3527542177382,
65.6482489737095));
#185791=CARTESIAN_POINT('Ctrl Pts',(122.79064496167,-10.2911919068618,65.6625639997959));
#185792=CARTESIAN_POINT('Ctrl Pts',(122.863715547138,-10.2287429973371,
65.6767675536675));
#185793=CARTESIAN_POINT('',(107.470912577424,-11.3244123346074,62.6846948227235));
#185794=CARTESIAN_POINT('Ctrl Pts',(107.485627742145,-11.3335893001918,
62.6876626706956));
#185795=CARTESIAN_POINT('Ctrl Pts',(107.480720751801,-11.3305336178283,
62.6866730118255));
#185796=CARTESIAN_POINT('Ctrl Pts',(107.47581569552,-11.3274746283431,62.6856837289009));
#185797=CARTESIAN_POINT('Ctrl Pts',(107.470912577424,-11.3244123346074,
62.6846948227235));
#185798=CARTESIAN_POINT('Ctrl Pts',(107.470912577424,-11.3244123346074,
62.6846948227235));
#185799=CARTESIAN_POINT('Ctrl Pts',(106.274400038169,-10.558499336519,62.4344828152312));
#185800=CARTESIAN_POINT('Ctrl Pts',(105.20088303681,-9.59249959662681,62.2069325119651));
#185801=CARTESIAN_POINT('Ctrl Pts',(103.95853529321,-8.04858401858125,61.9426111970985));
#185802=CARTESIAN_POINT('Ctrl Pts',(103.639020846898,-7.5965992708658,61.8741089306158));
#185803=CARTESIAN_POINT('Ctrl Pts',(103.005157994299,-6.5665024217714,61.7357740944669));
#185804=CARTESIAN_POINT('Ctrl Pts',(102.70329262004,-5.98313165971164,61.6684239476137));
#185805=CARTESIAN_POINT('Ctrl Pts',(102.13470301904,-4.65742573741101,61.5397236763161));
#185806=CARTESIAN_POINT('Ctrl Pts',(101.886849244608,-3.90643332928001,
61.4825608413799));
#185807=CARTESIAN_POINT('Ctrl Pts',(101.606380445827,-2.71745730486092,
61.4139284022522));
#185808=CARTESIAN_POINT('Ctrl Pts',(101.527103418739,-2.29091550080621,
61.3934507827151));
#185809=CARTESIAN_POINT('Ctrl Pts',(101.369437898936,-1.12967719105034,
61.3483570289574));
#185810=CARTESIAN_POINT('Ctrl Pts',(101.330879433115,-0.389445079030975,
61.3310502435924));
#185811=CARTESIAN_POINT('Ctrl Pts',(101.381383843657,1.38471795578357,61.3191228559119));
#185812=CARTESIAN_POINT('Ctrl Pts',(101.528098343796,2.41736244468448,61.335856812152));
#185813=CARTESIAN_POINT('Ctrl Pts',(102.006775533799,4.24789039142094,61.4062133868773));
#185814=CARTESIAN_POINT('Ctrl Pts',(102.301591504679,5.04970934213961,61.4526635038114));
#185815=CARTESIAN_POINT('Ctrl Pts',(103.04391014446,6.60201841175238,61.5757503765786));
#185816=CARTESIAN_POINT('Ctrl Pts',(103.494532433191,7.35019918636513,61.6528035402932));
#185817=CARTESIAN_POINT('Ctrl Pts',(104.264830156951,8.38776329761607,61.7870168561449));
#185818=CARTESIAN_POINT('Ctrl Pts',(104.533803506792,8.71628340900593,61.8342336481498));
#185819=CARTESIAN_POINT('Ctrl Pts',(105.391433894827,9.66631592104284,61.9856619875418));
#185820=CARTESIAN_POINT('Ctrl Pts',(106.024476706078,10.2417873164856,62.0979956492993));
#185821=CARTESIAN_POINT('Ctrl Pts',(107.325363196647,11.2154249903307,62.3303691611087));
#185822=CARTESIAN_POINT('Ctrl Pts',(107.986739416363,11.6254157423024,62.4491993210171));
#185823=CARTESIAN_POINT('Ctrl Pts',(109.30206962946,12.288064782333,62.6875058937065));
#185824=CARTESIAN_POINT('Ctrl Pts',(109.94976826693,12.5517322071569,62.805433842119));
#185825=CARTESIAN_POINT('Ctrl Pts',(111.024128414873,12.8891408930617,63.0000736376732));
#185826=CARTESIAN_POINT('Ctrl Pts',(111.436116267895,12.9964564726427,63.0746275600137));
#185827=CARTESIAN_POINT('Ctrl Pts',(112.387345784475,13.1951971218302,63.2469597722259));
#185828=CARTESIAN_POINT('Ctrl Pts',(112.929322628392,13.2733025335376,63.3453035071527));
#185829=CARTESIAN_POINT('Ctrl Pts',(113.998736369994,13.3594764034328,63.5402847871116));
#185830=CARTESIAN_POINT('Ctrl Pts',(114.526067620634,13.3699725817027,63.636788996925));
#185831=CARTESIAN_POINT('Ctrl Pts',(115.589865537427,13.3258847307165,63.8310683835618));
#185832=CARTESIAN_POINT('Ctrl Pts',(116.123598056301,13.26996623454,63.9281991926313));
#185833=CARTESIAN_POINT('Ctrl Pts',(117.14090877311,13.0980526102477,64.1125799098966));
#185834=CARTESIAN_POINT('Ctrl Pts',(117.622521233663,12.9879604505935,64.1996577800957));
#185835=CARTESIAN_POINT('Ctrl Pts',(118.581644607567,12.7108171472874,64.3734971949168));
#185836=CARTESIAN_POINT('Ctrl Pts',(119.05885117347,12.5424808386177,64.4602302397172));
#185837=CARTESIAN_POINT('Ctrl Pts',(120.269595561566,12.0350375352245,64.6801119316231));
#185838=CARTESIAN_POINT('Ctrl Pts',(120.987439448018,11.653405886996,64.8102647342016));
#185839=CARTESIAN_POINT('Ctrl Pts',(122.178969727996,10.8671355693131,65.023761533422));
#185840=CARTESIAN_POINT('Ctrl Pts',(122.668385475051,10.4918447060699,65.1109046216195));
#185841=CARTESIAN_POINT('Ctrl Pts',(123.982720490917,9.33072838523825,65.3447478333531));
#185842=CARTESIAN_POINT('Ctrl Pts',(124.740910296221,8.46625703112186,65.4788130603719));
#185843=CARTESIAN_POINT('Ctrl Pts',(126.455173626972,5.91411760544508,65.774825677581));
#185844=CARTESIAN_POINT('Ctrl Pts',(127.079976237841,4.23004003854899,65.8738275446836));
#185845=CARTESIAN_POINT('Ctrl Pts',(127.521918605851,2.06461609064611,65.9335986559922));
#185846=CARTESIAN_POINT('Ctrl Pts',(127.604696841238,1.44096751722637,65.9425181099599));
#185847=CARTESIAN_POINT('Ctrl Pts',(127.69157796131,0.0271249438644891,
65.9420409839444));
#185848=CARTESIAN_POINT('Ctrl Pts',(127.671382588491,-0.761203590754172,
65.9279951415855));
#185849=CARTESIAN_POINT('Ctrl Pts',(127.536960431653,-1.96405359133338,
65.8868217647676));
#185850=CARTESIAN_POINT('Ctrl Pts',(127.470080944866,-2.38431013298785,
65.8686512888352));
#185851=CARTESIAN_POINT('Ctrl Pts',(127.250851352109,-3.44076794102639,
65.8134560522557));
#185852=CARTESIAN_POINT('Ctrl Pts',(127.071723489756,-4.07190745080252,
65.7713949622881));
#185853=CARTESIAN_POINT('Ctrl Pts',(126.695431475237,-5.10151277065501,
65.6849024742793));
#185854=CARTESIAN_POINT('Ctrl Pts',(126.523343650202,-5.50839992739275,
65.6457971789059));
#185855=CARTESIAN_POINT('Ctrl Pts',(125.975698112604,-6.64449929089201,
65.5231111714808));
#185856=CARTESIAN_POINT('Ctrl Pts',(125.552386113774,-7.34984794587801,
65.4305106531452));
#185857=CARTESIAN_POINT('Ctrl Pts',(124.692802634908,-8.5243484946755,65.2464636238839));
#185858=CARTESIAN_POINT('Ctrl Pts',(124.279879019018,-9.01139391102258,
65.158963056486));
#185859=CARTESIAN_POINT('Ctrl Pts',(123.504906080448,-9.80077588539326,
64.9947841549065));
#185860=CARTESIAN_POINT('Ctrl Pts',(123.158325467745,-10.1173084808118,
64.921297478286));
#185861=CARTESIAN_POINT('Ctrl Pts',(121.653507750894,-11.3509702814949,
64.6035100892289));
#185862=CARTESIAN_POINT('Ctrl Pts',(120.354661175151,-12.0919359407802,
64.3343530005754));
#185863=CARTESIAN_POINT('Ctrl Pts',(118.275599042184,-12.8452877574834,
63.9028610817256));
#185864=CARTESIAN_POINT('Ctrl Pts',(117.559956039398,-13.0353633222222,
63.7541248279207));
#185865=CARTESIAN_POINT('Ctrl Pts',(116.098077005825,-13.2928123808805,
63.4513742094034));
#185866=CARTESIAN_POINT('Ctrl Pts',(115.350465393516,-13.3584111921057,
63.2968556267763));
#185867=CARTESIAN_POINT('Ctrl Pts',(114.602892108729,-13.3589088885551,
63.1424102408455));
#185868=CARTESIAN_POINT('Ctrl Pts',(118.780288836585,-12.65925539485,64.0299347534317));
#185869=CARTESIAN_POINT('Ctrl Pts',(116.595886786058,-13.41168843809,63.5767576294984));
#185870=CARTESIAN_POINT('Ctrl Pts',(111.830850147376,-13.70841130529,62.5933831941367));
#185871=CARTESIAN_POINT('Ctrl Pts',(105.43801356551,-10.41179638488,61.2650246644536));
#185872=CARTESIAN_POINT('Ctrl Pts',(101.552926167766,-4.27236878269199,
60.4241256289558));
#185873=CARTESIAN_POINT('Ctrl Pts',(101.239769506549,3.03341342218001,60.277543059066));
#185874=CARTESIAN_POINT('Ctrl Pts',(104.588660551712,9.51104676477801,60.8427940066454));
#185875=CARTESIAN_POINT('Ctrl Pts',(110.689622481059,13.39202095622,61.9429960129963));
#185876=CARTESIAN_POINT('Ctrl Pts',(117.881403714159,13.61677928444,63.2552328709365));
#185877=CARTESIAN_POINT('Ctrl Pts',(124.204921450959,10.12395787573,64.3986955598227));
#185878=CARTESIAN_POINT('Ctrl Pts',(127.938147290484,3.86714835369002,65.0386539963514));
#185879=CARTESIAN_POINT('Ctrl Pts',(128.066238757101,-3.44544911201899,
64.977841801965));
#185880=CARTESIAN_POINT('Ctrl Pts',(124.558608071853,-9.81738869681499,
64.2103132850727));
#185881=CARTESIAN_POINT('Ctrl Pts',(118.37727253464,-13.50903793953,62.9230665989836));
#185882=CARTESIAN_POINT('Ctrl Pts',(111.214209907503,-13.51252273589,61.4449905453842));
#185883=CARTESIAN_POINT('Ctrl Pts',(105.029423762811,-9.82689168621099,
60.1570731257995));
#185884=CARTESIAN_POINT('Ctrl Pts',(101.515833922933,-3.45837583796399,
59.3883862608075));
#185885=CARTESIAN_POINT('Ctrl Pts',(101.637084647361,3.85432706958101,59.3262443542041));
#185886=CARTESIAN_POINT('Ctrl Pts',(105.364455691648,10.11474245491,59.9650647281479));
#185887=CARTESIAN_POINT('Ctrl Pts',(111.684703352911,13.6136855823,61.1078917755655));
#185888=CARTESIAN_POINT('Ctrl Pts',(118.876690783495,13.39589393048,62.4201687144387));
#185889=CARTESIAN_POINT('Ctrl Pts',(124.981283460208,9.52082779822401,63.5210764701047));
#185890=CARTESIAN_POINT('Ctrl Pts',(128.336221493489,3.04643677302001,64.0875028389717));
#185891=CARTESIAN_POINT('Ctrl Pts',(128.029940821833,-4.25967593268699,
63.9422568327185));
#185892=CARTESIAN_POINT('Ctrl Pts',(124.150443525087,-10.40283497821,63.102444408213));
#185893=CARTESIAN_POINT('Ctrl Pts',(117.761271878036,-13.70586824618,61.7747982732376));
#185894=CARTESIAN_POINT('Ctrl Pts',(110.611146146451,-13.266999738,60.2992369099465));
#185895=CARTESIAN_POINT('Ctrl Pts',(104.656537122664,-9.20604594134699,
59.0560616135515));
#185896=CARTESIAN_POINT('Ctrl Pts',(101.527525978629,-2.63171028823999,
58.3621296473937));
#185897=CARTESIAN_POINT('Ctrl Pts',(102.082749950975,4.66113184975601,58.3843440158345));
#185898=CARTESIAN_POINT('Ctrl Pts',(106.175050417972,10.68137526099,59.0940998377636));
#185899=CARTESIAN_POINT('Ctrl Pts',(112.691393445214,13.78560312531,60.275044153263));
#185900=CARTESIAN_POINT('Ctrl Pts',(119.857699338531,13.12557900619,61.5823290820643));
#185901=CARTESIAN_POINT('Ctrl Pts',(123.765651770777,10.29802594745,62.2848213563563));
#185902=CARTESIAN_POINT('Ctrl Pts',(125.237609274392,8.47864527230601,62.5423720795936));
#185903=CARTESIAN_POINT('Ctrl Pts',(118.79600886555,-12.65925539485,63.9490626188614));
#185904=CARTESIAN_POINT('Ctrl Pts',(116.611606815023,-13.41168843809,63.4958854949296));
#185905=CARTESIAN_POINT('Ctrl Pts',(111.846570176341,-13.70841130529,62.5125110595679));
#185906=CARTESIAN_POINT('Ctrl Pts',(105.453733594475,-10.41179638488,61.1841525298833));
#185907=CARTESIAN_POINT('Ctrl Pts',(101.568646196731,-4.27236878269199,
60.343253494387));
#185908=CARTESIAN_POINT('Ctrl Pts',(101.255489535514,3.03341342218001,60.1966709244958));
#185909=CARTESIAN_POINT('Ctrl Pts',(104.604380580679,9.51104676477801,60.7619218720702));
#185910=CARTESIAN_POINT('Ctrl Pts',(110.705342510024,13.39202095622,61.862123878426));
#185911=CARTESIAN_POINT('Ctrl Pts',(117.897123743125,13.61677928444,63.1743607363613));
#185912=CARTESIAN_POINT('Ctrl Pts',(124.220641479924,10.12395787573,64.3178234252538));
#185913=CARTESIAN_POINT('Ctrl Pts',(127.953867319451,3.86714835369002,64.9577818617762));
#185914=CARTESIAN_POINT('Ctrl Pts',(128.081958786066,-3.44544911201899,
64.8969696673961));
#185915=CARTESIAN_POINT('Ctrl Pts',(124.574328100819,-9.81738869681499,
64.1294411504975));
#185916=CARTESIAN_POINT('Ctrl Pts',(118.392992563605,-13.50903793953,62.8421944644147));
#185917=CARTESIAN_POINT('Ctrl Pts',(111.229929936469,-13.51252273589,61.364118410809));
#185918=CARTESIAN_POINT('Ctrl Pts',(105.045143791776,-9.82689168621099,
60.0762009912307));
#185919=CARTESIAN_POINT('Ctrl Pts',(101.531553951899,-3.45837583796399,
59.3075141262323));
#185920=CARTESIAN_POINT('Ctrl Pts',(101.652804676326,3.85432706958101,59.2453722196352));
#185921=CARTESIAN_POINT('Ctrl Pts',(105.380175720614,10.11474245491,59.8841925935776));
#185922=CARTESIAN_POINT('Ctrl Pts',(111.700423381876,13.6136855823,61.0270196409966));
#185923=CARTESIAN_POINT('Ctrl Pts',(118.89241081246,13.39589393048,62.3392965798684));
#185924=CARTESIAN_POINT('Ctrl Pts',(124.997003489173,9.52082779822401,63.4402043355359));
#185925=CARTESIAN_POINT('Ctrl Pts',(128.351941522455,3.04643677302001,64.0066307044015));
#185926=CARTESIAN_POINT('Ctrl Pts',(128.045660850798,-4.25967593268699,
63.8613846981497));
#185927=CARTESIAN_POINT('Ctrl Pts',(124.166163554053,-10.40283497821,63.0215722736427));
#185928=CARTESIAN_POINT('Ctrl Pts',(117.776991907001,-13.70586824618,61.6939261386688));
#185929=CARTESIAN_POINT('Ctrl Pts',(110.626866175417,-13.266999738,60.2183647753762));
#185930=CARTESIAN_POINT('Ctrl Pts',(104.672257151629,-9.20604594134699,
58.9751894789827));
#185931=CARTESIAN_POINT('Ctrl Pts',(101.543246007595,-2.63171028823999,
58.2812575128234));
#185932=CARTESIAN_POINT('Ctrl Pts',(102.09846997994,4.66113184975601,58.3034718812657));
#185933=CARTESIAN_POINT('Ctrl Pts',(106.190770446937,10.68137526099,59.0132277031934));
#185934=CARTESIAN_POINT('Ctrl Pts',(112.70711347418,13.78560312531,60.1941720186878));
#185935=CARTESIAN_POINT('Ctrl Pts',(119.873419367496,13.12557900619,61.501456947494));
#185936=CARTESIAN_POINT('Ctrl Pts',(123.781371799742,10.29802594745,62.203949221786));
#185937=CARTESIAN_POINT('Ctrl Pts',(125.253329303358,8.47864527230601,62.4614999450184));
#185938=CARTESIAN_POINT('Ctrl Pts',(118.811728894516,-12.65925539485,63.8681904842861));
#185939=CARTESIAN_POINT('Ctrl Pts',(116.627326843988,-13.41168843809,63.4150133603608));
#185940=CARTESIAN_POINT('Ctrl Pts',(111.862290205306,-13.70841130529,62.4316389249991));
#185941=CARTESIAN_POINT('Ctrl Pts',(105.469453623441,-10.41179638488,61.103280395308));
#185942=CARTESIAN_POINT('Ctrl Pts',(101.584366225696,-4.27236878269199,
60.2623813598182));
#185943=CARTESIAN_POINT('Ctrl Pts',(101.271209564481,3.03341342218001,60.1157987899205));
#185944=CARTESIAN_POINT('Ctrl Pts',(104.620100609644,9.51104676477801,60.6810497375008));
#185945=CARTESIAN_POINT('Ctrl Pts',(110.72106253899,13.39202095622,61.7812517438507));
#185946=CARTESIAN_POINT('Ctrl Pts',(117.91284377209,13.61677928444,63.0934886017919));
#185947=CARTESIAN_POINT('Ctrl Pts',(124.236361508889,10.12395787573,64.2369512906843));
#185948=CARTESIAN_POINT('Ctrl Pts',(127.969587348416,3.86714835369002,64.8769097272067));
#185949=CARTESIAN_POINT('Ctrl Pts',(128.097678815032,-3.44544911201899,
64.8160975328265));
#185950=CARTESIAN_POINT('Ctrl Pts',(124.590048129785,-9.81738869681499,
64.048569015928));
#185951=CARTESIAN_POINT('Ctrl Pts',(118.40871259257,-13.50903793953,62.7613223298451));
#185952=CARTESIAN_POINT('Ctrl Pts',(111.245649965435,-13.51252273589,61.2832462762396));
#185953=CARTESIAN_POINT('Ctrl Pts',(105.060863820742,-9.82689168621099,
59.9953288566611));
#185954=CARTESIAN_POINT('Ctrl Pts',(101.547273980864,-3.45837583796399,
59.2266419916628));
#185955=CARTESIAN_POINT('Ctrl Pts',(101.668524705291,3.85432706958101,59.1645000850656));
#185956=CARTESIAN_POINT('Ctrl Pts',(105.39589574958,10.11474245491,59.8033204590023));
#185957=CARTESIAN_POINT('Ctrl Pts',(111.716143410841,13.6136855823,60.9461475064271));
#185958=CARTESIAN_POINT('Ctrl Pts',(118.908130841426,13.39589393048,62.2584244452931));
#185959=CARTESIAN_POINT('Ctrl Pts',(125.012723518138,9.52082779822401,63.3593322009671));
#185960=CARTESIAN_POINT('Ctrl Pts',(128.367661551421,3.04643677302001,63.9257585698262));
#185961=CARTESIAN_POINT('Ctrl Pts',(128.061380879763,-4.25967593268699,
63.7805125635808));
#185962=CARTESIAN_POINT('Ctrl Pts',(124.181883583019,-10.40283497821,62.9407001390674));
#185963=CARTESIAN_POINT('Ctrl Pts',(117.792711935966,-13.70586824618,61.6130540041));
#185964=CARTESIAN_POINT('Ctrl Pts',(110.642586204383,-13.266999738,60.1374926408009));
#185965=CARTESIAN_POINT('Ctrl Pts',(104.687977180594,-9.20604594134699,
58.8943173444139));
#185966=CARTESIAN_POINT('Ctrl Pts',(101.558966036561,-2.63171028823999,
58.2003853782481));
#185967=CARTESIAN_POINT('Ctrl Pts',(102.114190008905,4.66113184975601,58.2225997466969));
#185968=CARTESIAN_POINT('Ctrl Pts',(106.206490475903,10.68137526099,58.9323555686181));
#185969=CARTESIAN_POINT('Ctrl Pts',(112.722833503145,13.78560312531,60.1132998841184));
#185970=CARTESIAN_POINT('Ctrl Pts',(119.889139396462,13.12557900619,61.4205848129187));
#185971=CARTESIAN_POINT('Ctrl Pts',(123.797091828709,10.29802594745,62.1230770872107));
#185972=CARTESIAN_POINT('Ctrl Pts',(125.269049332323,8.47864527230601,62.3806278104489));
#185973=CARTESIAN_POINT('Ctrl Pts',(118.827448923481,-12.65925539485,63.787318349716));
#185974=CARTESIAN_POINT('Ctrl Pts',(116.643046872953,-13.41168843809,63.334141225792));
#185975=CARTESIAN_POINT('Ctrl Pts',(111.878010234271,-13.70841130529,62.3507667904303));
#185976=CARTESIAN_POINT('Ctrl Pts',(105.485173652407,-10.41179638488,61.0224082607378));
#185977=CARTESIAN_POINT('Ctrl Pts',(101.600086254661,-4.27236878269199,
60.1815092252494));
#185978=CARTESIAN_POINT('Ctrl Pts',(101.286929593446,3.03341342218001,60.0349266553503));
#185979=CARTESIAN_POINT('Ctrl Pts',(104.635820638609,9.51104676477801,60.6001776029319));
#185980=CARTESIAN_POINT('Ctrl Pts',(110.736782567956,13.39202095622,61.7003796092806));
#185981=CARTESIAN_POINT('Ctrl Pts',(117.928563801055,13.61677928444,63.012616467223));
#185982=CARTESIAN_POINT('Ctrl Pts',(124.252081537856,10.12395787573,64.1560791561089));
#185983=CARTESIAN_POINT('Ctrl Pts',(127.985307377381,3.86714835369002,64.7960375926378));
#185984=CARTESIAN_POINT('Ctrl Pts',(128.113398843998,-3.44544911201899,
64.7352253982512));
#185985=CARTESIAN_POINT('Ctrl Pts',(124.60576815875,-9.81738869681499,63.9676968813591));
#185986=CARTESIAN_POINT('Ctrl Pts',(118.424432621537,-13.50903793953,62.6804501952698));
#185987=CARTESIAN_POINT('Ctrl Pts',(111.2613699944,-13.51252273589,61.2023741416707));
#185988=CARTESIAN_POINT('Ctrl Pts',(105.076583849708,-9.82689168621099,
59.9144567220858));
#185989=CARTESIAN_POINT('Ctrl Pts',(101.562994009829,-3.45837583796399,
59.145769857094));
#185990=CARTESIAN_POINT('Ctrl Pts',(101.684244734257,3.85432706958101,59.0836279504903));
#185991=CARTESIAN_POINT('Ctrl Pts',(105.411615778545,10.11474245491,59.7224483244321));
#185992=CARTESIAN_POINT('Ctrl Pts',(111.731863439807,13.6136855823,60.8652753718517));
#185993=CARTESIAN_POINT('Ctrl Pts',(118.923850870392,13.39589393048,62.177552310723));
#185994=CARTESIAN_POINT('Ctrl Pts',(125.028443547103,9.52082779822401,63.2784600663983));
#185995=CARTESIAN_POINT('Ctrl Pts',(128.383381580386,3.04643677302001,63.844886435256));
#185996=CARTESIAN_POINT('Ctrl Pts',(128.077100908728,-4.25967593268699,
63.699640429012));
#185997=CARTESIAN_POINT('Ctrl Pts',(124.197603611984,-10.40283497821,62.8598280044972));
#185998=CARTESIAN_POINT('Ctrl Pts',(117.808431964931,-13.70586824618,61.5321818695312));
#185999=CARTESIAN_POINT('Ctrl Pts',(110.658306233348,-13.266999738,60.0566205062307));
#186000=CARTESIAN_POINT('Ctrl Pts',(104.703697209559,-9.20604594134699,
58.8134452098451));
#186001=CARTESIAN_POINT('Ctrl Pts',(101.574686065526,-2.63171028823999,
58.119513243678));
#186002=CARTESIAN_POINT('Ctrl Pts',(102.12991003787,4.66113184975601,58.1417276121281));
#186003=CARTESIAN_POINT('Ctrl Pts',(106.222210504869,10.68137526099,58.8514834340479));
#186004=CARTESIAN_POINT('Ctrl Pts',(112.73855353211,13.78560312531,60.0324277495495));
#186005=CARTESIAN_POINT('Ctrl Pts',(119.904859425427,13.12557900619,61.3397126783486));
#186006=CARTESIAN_POINT('Ctrl Pts',(123.812811857674,10.29802594745,62.0422049526405));
#186007=CARTESIAN_POINT('Ctrl Pts',(125.284769361288,8.47864527230601,62.29975567588));
#186008=CARTESIAN_POINT('',(121.944453055693,11.3913829322761,61.9325710545576));
#186009=CARTESIAN_POINT('Ctrl Pts',(114.603093529674,-13.3575246836283,
63.1414291237798));
#186010=CARTESIAN_POINT('Ctrl Pts',(113.990399128991,-13.3579712225348,
63.0150807040448));
#186011=CARTESIAN_POINT('Ctrl Pts',(113.377598459867,-13.3149179937247,
62.8889596251551));
#186012=CARTESIAN_POINT('Ctrl Pts',(112.541949711885,-13.1951183779221,
62.7164706356709));
#186013=CARTESIAN_POINT('Ctrl Pts',(112.313896472985,-13.156046153819,62.6693449757331));
#186014=CARTESIAN_POINT('Ctrl Pts',(111.83368261156,-13.0600519108201,62.5699333560895));
#186015=CARTESIAN_POINT('Ctrl Pts',(111.582250764064,-13.0016394937268,
62.5177690092337));
#186016=CARTESIAN_POINT('Ctrl Pts',(110.736367646641,-12.7777826485591,
62.3420902766842));
#186017=CARTESIAN_POINT('Ctrl Pts',(110.150989524571,-12.5763566939195,
62.2201551227424));
#186018=CARTESIAN_POINT('Ctrl Pts',(109.257110310978,-12.1959211403354,
62.0338541239351));
#186019=CARTESIAN_POINT('Ctrl Pts',(108.9373775311,-12.0442498276864,61.9671938147611));
#186020=CARTESIAN_POINT('Ctrl Pts',(108.437323988917,-11.7818132071309,
61.8629873299671));
#186021=CARTESIAN_POINT('Ctrl Pts',(108.252845595734,-11.6792645761009,
61.8245546881921));
#186022=CARTESIAN_POINT('Ctrl Pts',(107.722356500847,-11.3674350300325,
61.7140987949494));
#186023=CARTESIAN_POINT('Ctrl Pts',(107.382965637735,-11.1463339682985,
61.643515121726));
#186024=CARTESIAN_POINT('Ctrl Pts',(106.761349151428,-10.6989278292122,
61.5139348992215));
#186025=CARTESIAN_POINT('Ctrl Pts',(106.476918491919,-10.4758011555531,
61.4545116996931));
#186026=CARTESIAN_POINT('Ctrl Pts',(106.087648063399,-10.1430954036906,
61.3727449161145));
#186027=CARTESIAN_POINT('Ctrl Pts',(105.974841627675,-10.0432137601379,
61.3489939526357));
#186028=CARTESIAN_POINT('Ctrl Pts',(105.72663775211,-9.81551201509332,61.2965812295366));
#186029=CARTESIAN_POINT('Ctrl Pts',(105.592182627668,-9.68665969691926,
61.2680810899966));
#186030=CARTESIAN_POINT('Ctrl Pts',(105.164012850198,-9.25828802477612,
61.1770676842786));
#186031=CARTESIAN_POINT('Ctrl Pts',(104.881607468134,-8.94702551784144,
61.1166754190157));
#186032=CARTESIAN_POINT('Ctrl Pts',(104.451172343227,-8.42494967512794,
61.0243126220469));
#186033=CARTESIAN_POINT('Ctrl Pts',(104.293679228789,-8.22228192446864,
60.9904257600904));
#186034=CARTESIAN_POINT('Ctrl Pts',(103.899979252224,-7.6845451033037,60.905480482773));
#186035=CARTESIAN_POINT('Ctrl Pts',(103.672797452591,-7.3425411504999,60.8562241236915));
#186036=CARTESIAN_POINT('Ctrl Pts',(103.288487906928,-6.70271984641751,
60.7724586431333));
#186037=CARTESIAN_POINT('Ctrl Pts',(103.126113862337,-6.40813787795307,
60.7368922019998));
#186038=CARTESIAN_POINT('Ctrl Pts',(102.736314164748,-5.63405145937279,
60.6510334912565));
#186039=CARTESIAN_POINT('Ctrl Pts',(102.525359677965,-5.1458644023358,60.604152712784));
#186040=CARTESIAN_POINT('Ctrl Pts',(102.284288680491,-4.48130736408789,
60.5491035341268));
#186041=CARTESIAN_POINT('Ctrl Pts',(102.227659467904,-4.31500044297743,
60.5360292504741));
#186042=CARTESIAN_POINT('Ctrl Pts',(102.133336072709,-4.0187047394526,60.5139403222276));
#186043=CARTESIAN_POINT('Ctrl Pts',(102.094324477853,-3.8892840859754,60.5046909968951));
#186044=CARTESIAN_POINT('Ctrl Pts',(101.940901963849,-3.35065271176429,
60.4678551803245));
#186045=CARTESIAN_POINT('Ctrl Pts',(101.844081773649,-2.93620937072642,
60.4434556038056));
#186046=CARTESIAN_POINT('Ctrl Pts',(101.714392725028,-2.23381695610262,
60.408965602747));
#186047=CARTESIAN_POINT('Ctrl Pts',(101.67096999485,-1.94792448789282,60.3968094589545));
#186048=CARTESIAN_POINT('Ctrl Pts',(101.598473111033,-1.34246095847658,
60.375049049133));
#186049=CARTESIAN_POINT('Ctrl Pts',(101.571488054667,-1.02260856995072,
60.3658534673498));
#186050=CARTESIAN_POINT('Ctrl Pts',(101.532822286821,-0.238679710083945,
60.3488377832787));
#186051=CARTESIAN_POINT('Ctrl Pts',(101.533348262028,0.226107876286849,
60.3434631935411));
#186052=CARTESIAN_POINT('Ctrl Pts',(101.581616641272,1.15641839581304,60.3420158780094));
#186053=CARTESIAN_POINT('Ctrl Pts',(101.629688549945,1.62196856350683,60.346019299718));
#186054=CARTESIAN_POINT('Ctrl Pts',(101.730287773067,2.26629813330814,60.3581004771507));
#186055=CARTESIAN_POINT('Ctrl Pts',(101.76255554724,2.44830131570257,60.3622439241077));
#186056=CARTESIAN_POINT('Ctrl Pts',(101.827890671572,2.77686456409949,60.3710068909742));
#186057=CARTESIAN_POINT('Ctrl Pts',(101.859650753442,2.92354205228318,60.3753860595442));
#186058=CARTESIAN_POINT('Ctrl Pts',(101.938522433542,3.25999282947182,60.3864959044332));
#186059=CARTESIAN_POINT('Ctrl Pts',(101.98728453623,3.44911749528315,60.3935302965536));
#186060=CARTESIAN_POINT('Ctrl Pts',(102.169929054132,4.09851524021271,60.4204630601464));
#186061=CARTESIAN_POINT('Ctrl Pts',(102.324406955099,4.55282166789539,60.4441827223226));
#186062=CARTESIAN_POINT('Ctrl Pts',(102.576490407172,5.18328923546371,60.4844168993197));
#186063=CARTESIAN_POINT('Ctrl Pts',(102.654850537588,5.36740702646428,60.4970871990457));
#186064=CARTESIAN_POINT('Ctrl Pts',(102.822598854042,5.73874769461095,60.5245706972002));
#186065=CARTESIAN_POINT('Ctrl Pts',(102.912291951358,5.92583453852271,60.5394502848693));
#186066=CARTESIAN_POINT('Ctrl Pts',(103.157878185703,6.40955926284171,60.5806142866393));
#186067=CARTESIAN_POINT('Ctrl Pts',(103.320515703495,6.70267873209368,60.6082769725156));
#186068=CARTESIAN_POINT('Ctrl Pts',(103.782695926849,7.46762915852709,60.6877061879545));
#186069=CARTESIAN_POINT('Ctrl Pts',(104.101032348795,7.92777487488369,60.7432166644688));
#186070=CARTESIAN_POINT('Ctrl Pts',(104.643581968534,8.61506328198171,60.838455772304));
#186071=CARTESIAN_POINT('Ctrl Pts',(104.849376098324,8.85730205307405,60.8747076682046));
#186072=CARTESIAN_POINT('Ctrl Pts',(105.211916819241,9.25360446151154,60.9386398140822));
#186073=CARTESIAN_POINT('Ctrl Pts',(105.364160067242,9.41176931881221,60.9654981659304));
#186074=CARTESIAN_POINT('Ctrl Pts',(105.914805879218,9.95582270744608,61.062741440476));
#186075=CARTESIAN_POINT('Ctrl Pts',(106.33373432711,10.3202241310802,61.1368991003599));
#186076=CARTESIAN_POINT('Ctrl Pts',(107.046553904861,10.8662092021664,61.2638464902885));
#186077=CARTESIAN_POINT('Ctrl Pts',(107.327877569277,11.0648492747695,61.3141227043485));
#186078=CARTESIAN_POINT('Ctrl Pts',(107.771210615629,11.3528471796474,61.393726947745));
#186079=CARTESIAN_POINT('Ctrl Pts',(107.928209517917,11.4502500553402,61.421988950572));
#186080=CARTESIAN_POINT('Ctrl Pts',(108.474337294025,11.7735030045097,61.5205427731455));
#186081=CARTESIAN_POINT('Ctrl Pts',(108.872912821115,11.9828420737496,61.5928613985386));
#186082=CARTESIAN_POINT('Ctrl Pts',(109.663541350441,12.3475323162289,61.7365354725881));
#186083=CARTESIAN_POINT('Ctrl Pts',(110.054473613383,12.5054328828345,61.8076726200996));
#186084=CARTESIAN_POINT('Ctrl Pts',(110.609223455065,12.6982886925242,61.9084425988955));
#186085=CARTESIAN_POINT('Ctrl Pts',(110.767469955839,12.7498663302499,61.9371682360402));
#186086=CARTESIAN_POINT('Ctrl Pts',(111.363249485869,12.9311309394018,62.04519857268));
#186087=CARTESIAN_POINT('Ctrl Pts',(111.806667237708,13.0403185425305,62.1254509820834));
#186088=CARTESIAN_POINT('Ctrl Pts',(112.862110238992,13.2418699389597,62.316686915616));
#186089=CARTESIAN_POINT('Ctrl Pts',(113.477839764735,13.3143197715914,62.4283409326716));
#186090=CARTESIAN_POINT('Ctrl Pts',(114.365275936587,13.3555827718125,62.5896880030508));
#186091=CARTESIAN_POINT('Ctrl Pts',(114.635529499474,13.3597800420865,62.6388792844762));
#186092=CARTESIAN_POINT('Ctrl Pts',(115.186965896953,13.3512644341853,62.7393961135737));
#186093=CARTESIAN_POINT('Ctrl Pts',(115.468148714922,13.337841615018,62.7907406314709));
#186094=CARTESIAN_POINT('Ctrl Pts',(116.121802857897,13.2853458171502,62.9102231332582));
#186095=CARTESIAN_POINT('Ctrl Pts',(116.493733483146,13.2392582619345,62.9782804683887));
#186096=CARTESIAN_POINT('Ctrl Pts',(117.082406931017,13.1400188510727,63.0857750469098));
#186097=CARTESIAN_POINT('Ctrl Pts',(117.300830280039,13.0973365343111,63.1256103648593));
#186098=CARTESIAN_POINT('Ctrl Pts',(117.647318249538,13.0201361057555,63.1886519774697));
#186099=CARTESIAN_POINT('Ctrl Pts',(117.776029707718,12.9893386278848,63.2120349993459));
#186100=CARTESIAN_POINT('Ctrl Pts',(118.260920770969,12.8652535870903,63.2999850507719));
#186101=CARTESIAN_POINT('Ctrl Pts',(118.613584209923,12.7585192387634,63.3636844776029));
#186102=CARTESIAN_POINT('Ctrl Pts',(119.474635456428,12.4573514852675,63.5190997726643));
#186103=CARTESIAN_POINT('Ctrl Pts',(119.977084610835,12.2453701443103,63.6097570810696));
#186104=CARTESIAN_POINT('Ctrl Pts',(120.806472734739,11.8333804996213,63.7593664832312));
#186105=CARTESIAN_POINT('Ctrl Pts',(121.140919423904,11.6488090164101,63.8196801823219));
#186106=CARTESIAN_POINT('Ctrl Pts',(121.838290784598,11.2236733904382,63.9453837087774));
#186107=CARTESIAN_POINT('Ctrl Pts',(122.198770165219,10.9788615259388,64.010324535685));
#186108=CARTESIAN_POINT('Ctrl Pts',(122.802348646447,10.5237137485963,64.1189457270106));
#186109=CARTESIAN_POINT('Ctrl Pts',(123.051293885605,10.3213649095711,64.163709649583));
#186110=CARTESIAN_POINT('Ctrl Pts',(123.439276718796,9.98155152818562,64.2331514937779));
#186111=CARTESIAN_POINT('Ctrl Pts',(123.583108545896,9.84978394265308,64.2588181818252));
#186112=CARTESIAN_POINT('Ctrl Pts',(123.821575857368,9.6212240690469,64.3011787757565));
#186113=CARTESIAN_POINT('Ctrl Pts',(123.917666763204,9.52619733132495,64.3181895209984));
#186114=CARTESIAN_POINT('Ctrl Pts',(124.324516419101,9.11117979478066,64.3899863887137));
#186115=CARTESIAN_POINT('Ctrl Pts',(124.620735406745,8.77640159922797,64.4416812578214));
#186116=CARTESIAN_POINT('Ctrl Pts',(125.129629014704,8.13966932052117,64.5299469177379));
#186117=CARTESIAN_POINT('Ctrl Pts',(125.347834048512,7.8422862133304,64.5676025306936));
#186118=CARTESIAN_POINT('Ctrl Pts',(125.713892906783,7.29809807681613,64.6305708973747));
#186119=CARTESIAN_POINT('Ctrl Pts',(125.866638509675,7.05465995084478,64.6567534501411));
#186120=CARTESIAN_POINT('Ctrl Pts',(126.269425035444,6.36511094393209,64.7254520590792));
#186121=CARTESIAN_POINT('Ctrl Pts',(126.502612962555,5.90876842958892,64.7648118599198));
#186122=CARTESIAN_POINT('Ctrl Pts',(126.884997982173,5.04273407190103,64.8281914697899));
#186123=CARTESIAN_POINT('Ctrl Pts',(127.041565807407,4.63636429983549,64.8536389038463));
#186124=CARTESIAN_POINT('Ctrl Pts',(127.226180793314,4.07732050402872,64.8826839013661));
#186125=CARTESIAN_POINT('Ctrl Pts',(127.27182798204,3.93066265157856,64.8897586781975));
#186126=CARTESIAN_POINT('Ctrl Pts',(127.358921359513,3.63274878555362,64.9029866170164));
#186127=CARTESIAN_POINT('Ctrl Pts',(127.400206249997,3.48163242963907,64.9091052687959));
#186128=CARTESIAN_POINT('Ctrl Pts',(127.586855709503,2.74799610622354,64.9360194697212));
#186129=CARTESIAN_POINT('Ctrl Pts',(127.69576976199,2.1559534205035,64.9493034547574));
#186130=CARTESIAN_POINT('Ctrl Pts',(127.802864054099,1.23846863873338,64.9582071320374));
#186131=CARTESIAN_POINT('Ctrl Pts',(127.828961547112,0.916315746228356,
64.9591552854305));
#186132=CARTESIAN_POINT('Ctrl Pts',(127.852757527575,0.394883279898758,
64.9573298409709));
#186133=CARTESIAN_POINT('Ctrl Pts',(127.85751236588,0.195904482082526,64.9558467078465));
#186134=CARTESIAN_POINT('Ctrl Pts',(127.859073009378,-0.513478792821087,
64.9477028540574));
#186135=CARTESIAN_POINT('Ctrl Pts',(127.831788820181,-1.02393759294173,
64.9365714982727));
#186136=CARTESIAN_POINT('Ctrl Pts',(127.725292970965,-1.99321268054657,
64.9047196082197));
#186137=CARTESIAN_POINT('Ctrl Pts',(127.650897750762,-2.45261458369212,
64.8849346109271));
#186138=CARTESIAN_POINT('Ctrl Pts',(127.506858377997,-3.11974815108727,
64.8488157552804));
#186139=CARTESIAN_POINT('Ctrl Pts',(127.455719142738,-3.331326615975,64.8362361394663));
#186140=CARTESIAN_POINT('Ctrl Pts',(127.230599950141,-4.17144759019554,
64.7817289946605));
#186141=CARTESIAN_POINT('Ctrl Pts',(127.015836385385,-4.7879106457032,64.7315324928152));
#186142=CARTESIAN_POINT('Ctrl Pts',(126.593301402418,-5.76812496720764,
64.635693285313));
#186143=CARTESIAN_POINT('Ctrl Pts',(126.410655559543,-6.14321701101547,
64.594877149254));
#186144=CARTESIAN_POINT('Ctrl Pts',(126.116202692636,-6.68329148997502,
64.5300454745718));
#186145=CARTESIAN_POINT('Ctrl Pts',(126.017270402795,-6.8556181497677,64.508400080519));
#186146=CARTESIAN_POINT('Ctrl Pts',(125.650352077731,-7.46331190321983,
64.4286298455308));
#186147=CARTESIAN_POINT('Ctrl Pts',(125.361457757297,-7.88560860618325,
64.3667151681209));
#186148=CARTESIAN_POINT('Ctrl Pts',(124.836072736936,-8.56612860916472,
64.2547677919321));
#186149=CARTESIAN_POINT('Ctrl Pts',(124.611730848969,-8.83414045673399,
64.2071328096745));
#186150=CARTESIAN_POINT('Ctrl Pts',(124.27609758154,-9.20389656957432,64.1358983363456));
#186151=CARTESIAN_POINT('Ctrl Pts',(124.173072262069,-9.31351948663113,
64.1140357286447));
#186152=CARTESIAN_POINT('Ctrl Pts',(123.78437624167,-9.71287015076297,64.0315317062448));
#186153=CARTESIAN_POINT('Ctrl Pts',(123.48720079234,-9.99065485180476,63.9684561583088));
#186154=CARTESIAN_POINT('Ctrl Pts',(122.675414468006,-10.6816878256984,
63.7968605506766));
#186155=CARTESIAN_POINT('Ctrl Pts',(122.141137842134,-11.0709225469987,
63.6844921281256));
#186156=CARTESIAN_POINT('Ctrl Pts',(121.31913387786,-11.5804619472397,63.5126042031283));
#186157=CARTESIAN_POINT('Ctrl Pts',(121.051033409447,-11.7338699920835,
63.4566841379968));
#186158=CARTESIAN_POINT('Ctrl Pts',(120.48833618688,-12.0300134240572,63.3396299291538));
#186159=CARTESIAN_POINT('Ctrl Pts',(120.193096662126,-12.171537845633,63.2783952214694));
#186160=CARTESIAN_POINT('Ctrl Pts',(119.588988333214,-12.4335413509648,
63.1533780556106));
#186161=CARTESIAN_POINT('Ctrl Pts',(119.279988086963,-12.5537086435395,
63.089547306203));
#186162=CARTESIAN_POINT('Ctrl Pts',(118.773320790979,-12.728412563179,62.9848087207607));
#186163=CARTESIAN_POINT('Ctrl Pts',(118.57815607602,-12.7904962382517,62.9444465084282));
#186164=CARTESIAN_POINT('Ctrl Pts',(118.257514733425,-12.8839711460315,
62.8780449302931));
#186165=CARTESIAN_POINT('Ctrl Pts',(118.133022492874,-12.9181922210399,
62.852239704963));
#186166=CARTESIAN_POINT('Ctrl Pts',(117.607496050715,-13.0539948854129,
62.7432115424693));
#186167=CARTESIAN_POINT('Ctrl Pts',(117.202250300468,-13.1377049950957,
62.6589251792515));
#186168=CARTESIAN_POINT('Ctrl Pts',(116.461094617542,-13.2538240182983,
62.5049356440482));
#186169=CARTESIAN_POINT('Ctrl Pts',(116.126187755109,-13.292848399882,62.4354379192552));
#186170=CARTESIAN_POINT('Ctrl Pts',(115.43101844711,-13.3464515712576,62.2913908971411));
#186171=CARTESIAN_POINT('Ctrl Pts',(115.07058717598,-13.3591407803865,62.2168100328529));
#186172=CARTESIAN_POINT('Ctrl Pts',(114.253503630022,-13.3538765372014,
62.0479170822489));
#186173=CARTESIAN_POINT('Ctrl Pts',(113.796836931941,-13.3268147639553,
61.9536501983375));
#186174=CARTESIAN_POINT('Ctrl Pts',(112.964062028573,-13.2329114512214,
61.7818653406047));
#186175=CARTESIAN_POINT('Ctrl Pts',(112.587127111227,-13.1734090120992,
61.7041812070377));
#186176=CARTESIAN_POINT('Ctrl Pts',(112.036675326882,-13.0609800384358,
61.5906465634742));
#186177=CARTESIAN_POINT('Ctrl Pts',(111.860603977884,-13.0211014353704,
61.5543083486569));
#186178=CARTESIAN_POINT('Ctrl Pts',(111.545434807673,-12.9425739328143,
61.4891650733484));
#186179=CARTESIAN_POINT('Ctrl Pts',(111.406031208211,-12.9052902859207,
61.4603151595134));
#186180=CARTESIAN_POINT('Ctrl Pts',(111.102252667029,-12.8183942533883,
61.3973426970148));
#186181=CARTESIAN_POINT('Ctrl Pts',(110.938332612829,-12.7678588459617,
61.3632998685479));
#186182=CARTESIAN_POINT('Ctrl Pts',(110.347535637555,-12.5725450063597,
61.240432705736));
#186183=CARTESIAN_POINT('Ctrl Pts',(109.926918022354,-12.4082541610369,
61.1526297606735));
#186184=CARTESIAN_POINT('Ctrl Pts',(109.329464262365,-12.138287729035,61.0278643889183));
#186185=CARTESIAN_POINT('Ctrl Pts',(109.145197258408,-12.0497436547561,
60.9893774315288));
#186186=CARTESIAN_POINT('Ctrl Pts',(108.759968061027,-11.8534066209237,
60.908960060838));
#186187=CARTESIAN_POINT('Ctrl Pts',(108.559508436871,-11.7445672318688,
60.8671377064275));
#186188=CARTESIAN_POINT('Ctrl Pts',(108.055610129353,-11.4537736453416,
60.7620247599346));
#186189=CARTESIAN_POINT('Ctrl Pts',(107.756174536728,-11.2645262356543,
60.699578638175));
#186190=CARTESIAN_POINT('Ctrl Pts',(106.954972154193,-10.7117862354286,
60.5323380063867));
#186191=CARTESIAN_POINT('Ctrl Pts',(106.469346848412,-10.3238003590776,
60.430794959707));
#186192=CARTESIAN_POINT('Ctrl Pts',(105.870541743564,-9.77082063875566,
60.3048069856716));
#186193=CARTESIAN_POINT('Ctrl Pts',(105.730755572468,-9.63581577841111,
60.2753387427463));
#186194=CARTESIAN_POINT('Ctrl Pts',(105.472453944849,-9.37481351423717,
60.2207164513879));
#186195=CARTESIAN_POINT('Ctrl Pts',(105.353510507324,-9.24968093933481,
60.1954818877547));
#186196=CARTESIAN_POINT('Ctrl Pts',(104.81733432664,-8.6625411529408,60.08134731658));
#186197=CARTESIAN_POINT('Ctrl Pts',(104.43019108471,-8.17220202521634,59.9978719182808));
#186198=CARTESIAN_POINT('Ctrl Pts',(103.885593824562,-7.3738994096418,59.8794922208696));
#186199=CARTESIAN_POINT('Ctrl Pts',(103.703348083998,-7.08354261682428,
59.839674168317));
#186200=CARTESIAN_POINT('Ctrl Pts',(103.439669756716,-6.62581518192857,
59.7818667741538));
#186201=CARTESIAN_POINT('Ctrl Pts',(103.35035870522,-6.46316754664296,59.7622509382567));
#186202=CARTESIAN_POINT('Ctrl Pts',(103.033510526149,-5.85706529756014,
59.692494099151));
#186203=CARTESIAN_POINT('Ctrl Pts',(102.826653077162,-5.40225905357714,
59.6466007045469));
#186204=CARTESIAN_POINT('Ctrl Pts',(102.487068323946,-4.53055175746746,
59.5699066853281));
#186205=CARTESIAN_POINT('Ctrl Pts',(102.348276674649,-4.11609423383822,
59.5379299371577));
#186206=CARTESIAN_POINT('Ctrl Pts',(102.180257084585,-3.51796211383271,
59.4978670558067));
#186207=CARTESIAN_POINT('Ctrl Pts',(102.134062417779,-3.33931372374463,
59.4866507402423));
#186208=CARTESIAN_POINT('Ctrl Pts',(101.971958078993,-2.65323768786973,
59.4464249527177));
#186209=CARTESIAN_POINT('Ctrl Pts',(101.882101016615,-2.13973237506003,
59.422296002869));
#186210=CARTESIAN_POINT('Ctrl Pts',(101.757857086493,-1.07291576295581,
59.3844126710314));
#186211=CARTESIAN_POINT('Ctrl Pts',(101.727303810479,-0.519109698192167,
59.371394102765));
#186212=CARTESIAN_POINT('Ctrl Pts',(101.731271809209,0.274346340597185,
59.3623652755867));
#186213=CARTESIAN_POINT('Ctrl Pts',(101.738722628582,0.514141584924893,
59.3608965589136));
#186214=CARTESIAN_POINT('Ctrl Pts',(101.768809432482,1.04017549387642,59.3604753263735));
#186215=CARTESIAN_POINT('Ctrl Pts',(101.794145457511,1.32626989230036,59.3620899828508));
#186216=CARTESIAN_POINT('Ctrl Pts',(101.874479959946,1.99401728511432,59.370063845904));
#186217=CARTESIAN_POINT('Ctrl Pts',(101.936676246456,2.37479690063633,59.377850930817));
#186218=CARTESIAN_POINT('Ctrl Pts',(102.050301619527,2.92186233280537,59.3935397502688));
#186219=CARTESIAN_POINT('Ctrl Pts',(102.088826290953,3.09089056309865,59.399021021663));
#186220=CARTESIAN_POINT('Ctrl Pts',(102.166564929235,3.40370280264371,59.4103262432364));
#186221=CARTESIAN_POINT('Ctrl Pts',(102.204929901869,3.54772295953015,59.4159951034999));
#186222=CARTESIAN_POINT('Ctrl Pts',(102.30030540256,3.88284706408452,59.4302602563008));
#186223=CARTESIAN_POINT('Ctrl Pts',(102.359217431612,4.07335890134234,59.4391968220913));
#186224=CARTESIAN_POINT('Ctrl Pts',(102.534693125102,4.59887196798283,59.4662316344382));
#186225=CARTESIAN_POINT('Ctrl Pts',(102.660388063998,4.93071944386864,59.4860603876968));
#186226=CARTESIAN_POINT('Ctrl Pts',(103.0150981765,5.76676162757953,59.5433859493828));
#186227=CARTESIAN_POINT('Ctrl Pts',(103.262488366159,6.26295389947851,59.5844864238727));
#186228=CARTESIAN_POINT('Ctrl Pts',(103.71339776416,7.04464691947722,59.6610255955423));
#186229=CARTESIAN_POINT('Ctrl Pts',(103.899616607257,7.34056394672016,59.692991585322));
#186230=CARTESIAN_POINT('Ctrl Pts',(104.339338176009,7.98291811571845,59.7692257793045));
#186231=CARTESIAN_POINT('Ctrl Pts',(104.598490075028,8.32538958658205,59.8146705297761));
#186232=CARTESIAN_POINT('Ctrl Pts',(105.105329222861,8.93206696220115,59.9042118354609));
#186233=CARTESIAN_POINT('Ctrl Pts',(105.348527623573,9.2001531104887,59.9473810850936));
#186234=CARTESIAN_POINT('Ctrl Pts',(105.694706448755,9.55122332925254,60.0088055477242));
#186235=CARTESIAN_POINT('Ctrl Pts',(105.788489308381,9.64348721462895,60.0254426646478));
#186236=CARTESIAN_POINT('Ctrl Pts',(106.015931419453,9.86050293142528,60.0657680598013));
#186237=CARTESIAN_POINT('Ctrl Pts',(106.150731784925,9.98377978897873,60.089654911538));
#186238=CARTESIAN_POINT('Ctrl Pts',(106.486688665688,10.2783280034598,60.1492089906058));
#186239=CARTESIAN_POINT('Ctrl Pts',(106.690552131011,10.4464005601864,60.1853657100624));
#186240=CARTESIAN_POINT('Ctrl Pts',(107.210323154609,10.849351275424,60.2777666053788));
#186241=CARTESIAN_POINT('Ctrl Pts',(107.532048619494,11.0764650379316,60.3351836812339));
#186242=CARTESIAN_POINT('Ctrl Pts',(108.13145529298,11.4609626719913,60.4427131326062));
#186243=CARTESIAN_POINT('Ctrl Pts',(108.406027674603,11.6234316216101,60.4921430409791));
#186244=CARTESIAN_POINT('Ctrl Pts',(109.181586494496,12.0454063103798,60.6321540848603));
#186245=CARTESIAN_POINT('Ctrl Pts',(109.694045300436,12.2832223442261,60.7251031530113));
#186246=CARTESIAN_POINT('Ctrl Pts',(110.656858173676,12.6565525849736,60.9001867589728));
#186247=CARTESIAN_POINT('Ctrl Pts',(111.103320675212,12.8025175224817,60.9816012342247));
#186248=CARTESIAN_POINT('Ctrl Pts',(111.702412603349,12.9624121663959,61.0906657332844));
#186249=CARTESIAN_POINT('Ctrl Pts',(111.849070138252,12.9987659994906,61.1173423283447));
#186250=CARTESIAN_POINT('Ctrl Pts',(112.182266698995,13.0750468217819,61.1778755177285));
#186251=CARTESIAN_POINT('Ctrl Pts',(112.368911696764,13.1133759068098,61.2117386811187));
#186252=CARTESIAN_POINT('Ctrl Pts',(113.270743147748,13.2777166253032,61.3752322029498));
#186253=CARTESIAN_POINT('Ctrl Pts',(113.995967849278,13.3471278131987,61.5063279130925));
#186254=CARTESIAN_POINT('Ctrl Pts',(114.931297617332,13.3587583818418,61.6763206603305));
#186255=CARTESIAN_POINT('Ctrl Pts',(115.140952460877,13.3563277685502,61.7144808472429));
#186256=CARTESIAN_POINT('Ctrl Pts',(115.865296282167,13.3305319188046,61.8464562028411));
#186257=CARTESIAN_POINT('Ctrl Pts',(116.379135200741,13.2818084306026,61.9403139337308));
#186258=CARTESIAN_POINT('Ctrl Pts',(117.438215883638,13.1174641702283,62.1336861666048));
#186259=CARTESIAN_POINT('Ctrl Pts',(117.982728905425,12.9968181043918,62.2330586948186));
#186260=CARTESIAN_POINT('Ctrl Pts',(118.711899683826,12.7842611624471,62.3655861347268));
#186261=CARTESIAN_POINT('Ctrl Pts',(118.904663692281,12.7230242617307,62.4005577440117));
#186262=CARTESIAN_POINT('Ctrl Pts',(119.490819433883,12.5213878339624,62.5066990972885));
#186263=CARTESIAN_POINT('Ctrl Pts',(119.879181565658,12.3661949774273,62.5767623580464));
#186264=CARTESIAN_POINT('Ctrl Pts',(120.689759635771,11.9963169906521,62.7227149854452));
#186265=CARTESIAN_POINT('Ctrl Pts',(121.109729522615,11.7764848283689,62.7981634508621));
#186266=CARTESIAN_POINT('Ctrl Pts',(121.693251830559,11.430033722902,62.9030226659486));
#186267=CARTESIAN_POINT('Ctrl Pts',(121.867128623607,11.3212721891398,62.9342721120155));
#186268=CARTESIAN_POINT('Ctrl Pts',(122.240682633842,11.0753959751299,63.0014485617585));
#186269=CARTESIAN_POINT('Ctrl Pts',(122.43936170471,10.9367007592207,63.0372046986133));
#186270=CARTESIAN_POINT('Ctrl Pts',(122.935071864527,10.5700890771558,63.1263830059613));
#186271=CARTESIAN_POINT('Ctrl Pts',(123.226772673359,10.334696351177,63.178827132535));
#186272=CARTESIAN_POINT('Ctrl Pts',(123.7207520185,9.90013447494156,63.2672995646437));
#186273=CARTESIAN_POINT('Ctrl Pts',(123.927459598736,9.70617552676832,63.3042067513528));
#186274=CARTESIAN_POINT('Ctrl Pts',(124.254676364109,9.37854786336352,63.3623258709278));
#186275=CARTESIAN_POINT('Ctrl Pts',(124.379001624991,9.2488473685348,63.3843308828263));
#186276=CARTESIAN_POINT('Ctrl Pts',(124.699904082089,8.89988778401403,63.4408761111308));
#186277=CARTESIAN_POINT('Ctrl Pts',(124.891816860741,8.67643052291237,63.4744247705943));
#186278=CARTESIAN_POINT('Ctrl Pts',(125.541904278356,7.8663041210362,63.5875186164069));
#186279=CARTESIAN_POINT('Ctrl Pts',(125.95941217609,7.24570641563249,63.6590240656914));
#186280=CARTESIAN_POINT('Ctrl Pts',(126.472481886112,6.32860285449774,63.7456313903176));
#186281=CARTESIAN_POINT('Ctrl Pts',(126.612395247932,6.05754829899803,63.7690772116149));
#186282=CARTESIAN_POINT('Ctrl Pts',(126.852014643002,5.55245517862468,63.8089334125459));
#186283=CARTESIAN_POINT('Ctrl Pts',(126.954540209441,5.31977410356813,63.8258684256751));
#186284=CARTESIAN_POINT('Ctrl Pts',(127.164228419731,4.80526949483151,63.8602328269393));
#186285=CARTESIAN_POINT('Ctrl Pts',(127.26873559346,4.5223202814057,63.8771599645833));
#186286=CARTESIAN_POINT('Ctrl Pts',(127.462351927687,3.93882141893424,63.9078548047792));
#186287=CARTESIAN_POINT('Ctrl Pts',(127.550706990229,3.63801922852502,63.9214742870542));
#186288=CARTESIAN_POINT('Ctrl Pts',(127.664862727722,3.19205124165761,63.9382519208259));
#186289=CARTESIAN_POINT('Ctrl Pts',(127.69896186235,3.04908434874342,63.9431242382031));
#186290=CARTESIAN_POINT('Ctrl Pts',(127.767163462692,2.74056520066485,63.9525216878805));
#186291=CARTESIAN_POINT('Ctrl Pts',(127.800499166874,2.57484993737074,63.9568853802017));
#186292=CARTESIAN_POINT('Ctrl Pts',(127.964565906962,1.67129687725773,63.9771156891775));
#186293=CARTESIAN_POINT('Ctrl Pts',(128.036688072689,0.922605975005862,
63.9812836524761));
#186294=CARTESIAN_POINT('Ctrl Pts',(128.053091050656,-0.218177777081743,
63.9702774680057));
#186295=CARTESIAN_POINT('Ctrl Pts',(128.041997650652,-0.609788606400816,
63.9633379770788));
#186296=CARTESIAN_POINT('Ctrl Pts',(127.983621303946,-1.43100647438174,
63.9421188950817));
#186297=CARTESIAN_POINT('Ctrl Pts',(127.932691422753,-1.86039262337457,
63.9271497778164));
#186298=CARTESIAN_POINT('Ctrl Pts',(127.782740837144,-2.75777645693293,
63.8875453859669));
#186299=CARTESIAN_POINT('Ctrl Pts',(127.679129178069,-3.22497637434037,
63.862097099584));
#186300=CARTESIAN_POINT('Ctrl Pts',(127.51060112987,-3.82953454489757,63.8220021106787));
#186301=CARTESIAN_POINT('Ctrl Pts',(127.467871035817,-3.97339419455098,
63.8119133852327));
#186302=CARTESIAN_POINT('Ctrl Pts',(127.37534701678,-4.26651999497137,63.7901883057961));
#186303=CARTESIAN_POINT('Ctrl Pts',(127.325352687751,-4.41560557477619,
63.7785128416517));
#186304=CARTESIAN_POINT('Ctrl Pts',(127.207009551048,-4.74884976880704,
63.7510372798475));
#186305=CARTESIAN_POINT('Ctrl Pts',(127.137197990067,-4.93245846603757,
63.7349359962479));
#186306=CARTESIAN_POINT('Ctrl Pts',(126.845763014017,-5.6510844006793,63.6682125453016));
#186307=CARTESIAN_POINT('Ctrl Pts',(126.593564354546,-6.1731528873397,63.6115520130025));
#186308=CARTESIAN_POINT('Ctrl Pts',(126.167987863232,-6.92690905571856,
63.5180417570039));
#186309=CARTESIAN_POINT('Ctrl Pts',(126.01864264227,-7.17275495149999,63.4855035475113));
#186310=CARTESIAN_POINT('Ctrl Pts',(125.514303532643,-7.94627078660459,
63.3763704607782));
#186311=CARTESIAN_POINT('Ctrl Pts',(125.129643765918,-8.45393733842158,
63.2942226989373));
#186312=CARTESIAN_POINT('Ctrl Pts',(124.41935384716,-9.26357998023273,63.1436351485535));
#186313=CARTESIAN_POINT('Ctrl Pts',(124.110988560638,-9.58136061805701,
63.078597795913));
#186314=CARTESIAN_POINT('Ctrl Pts',(123.67262068835,-9.98900230521898,62.9861548190844));
#186315=CARTESIAN_POINT('Ctrl Pts',(123.555961958387,-10.0935683813924,
62.9615455628932));
#186316=CARTESIAN_POINT('Ctrl Pts',(123.155247880156,-10.4398460019076,
62.8770102525141));
#186317=CARTESIAN_POINT('Ctrl Pts',(122.862685236626,-10.671328784282,62.8152862900541));
#186318=CARTESIAN_POINT('Ctrl Pts',(122.159797824742,-11.180264880214,62.6672746406744));
#186319=CARTESIAN_POINT('Ctrl Pts',(121.742468657624,-11.4476761776246,
62.5796037064665));
#186320=CARTESIAN_POINT('Ctrl Pts',(121.148562699661,-11.7826136804606,
62.4555314190495));
#186321=CARTESIAN_POINT('Ctrl Pts',(120.983377506188,-11.8711632738061,
62.4210970945461));
#186322=CARTESIAN_POINT('Ctrl Pts',(120.508991344542,-12.1125350242583,
62.3223919198141));
#186323=CARTESIAN_POINT('Ctrl Pts',(120.195543029721,-12.2567548452443,
62.2573852988289));
#186324=CARTESIAN_POINT('Ctrl Pts',(119.354447999188,-12.6040699377361,
62.0832447920378));
#186325=CARTESIAN_POINT('Ctrl Pts',(118.818218563734,-12.7856804477348,
61.972519341747));
#186326=CARTESIAN_POINT('Ctrl Pts',(118.052684370993,-12.9894033090308,
61.8142392204107));
#186327=CARTESIAN_POINT('Ctrl Pts',(117.831096009594,-13.0420435768363,
61.7684005408198));
#186328=CARTESIAN_POINT('Ctrl Pts',(117.309005986134,-13.1511373540155,
61.6602808060396));
#186329=CARTESIAN_POINT('Ctrl Pts',(117.007659058018,-13.2026988463473,
61.5978008101505));
#186330=CARTESIAN_POINT('Ctrl Pts',(116.214693322051,-13.3091861549093,
61.4333122961321));
#186331=CARTESIAN_POINT('Ctrl Pts',(115.720822048658,-13.3464251704356,
61.3307864325695));
#186332=CARTESIAN_POINT('Ctrl Pts',(114.888702387365,-13.361368067599,61.1582188651562));
#186333=CARTESIAN_POINT('Ctrl Pts',(114.550685094673,-13.3541943840866,
61.0881692756249));
#186334=CARTESIAN_POINT('Ctrl Pts',(114.016990026164,-13.3219977754822,
60.9777369926673));
#186335=CARTESIAN_POINT('Ctrl Pts',(113.820801172636,-13.3056779377818,
60.9371780810214));
#186336=CARTESIAN_POINT('Ctrl Pts',(113.44540351328,-13.2658306572991,60.8596592629578));
#186337=CARTESIAN_POINT('Ctrl Pts',(113.266119931918,-13.243005196364,60.8226742777998));
#186338=CARTESIAN_POINT('Ctrl Pts',(112.685274192186,-13.1566587477565,
60.7029039921763));
#186339=CARTESIAN_POINT('Ctrl Pts',(112.285854357962,-13.0779213233347,
60.6206285512193));
#186340=CARTESIAN_POINT('Ctrl Pts',(111.641850478772,-12.9187461343833,
60.4877295429215));
#186341=CARTESIAN_POINT('Ctrl Pts',(111.394559370389,-12.8496737090834,
60.4366376755461));
#186342=CARTESIAN_POINT('Ctrl Pts',(111.009641701352,-12.7294158528691,
60.3569250514861));
#186343=CARTESIAN_POINT('Ctrl Pts',(110.870468796284,-12.6832664974673,
60.3280639465654));
#186344=CARTESIAN_POINT('Ctrl Pts',(110.477781840778,-12.5453673215558,
60.2464941364024));
#186345=CARTESIAN_POINT('Ctrl Pts',(110.226382355776,-12.4479236444354,
60.1941216196114));
#186346=CARTESIAN_POINT('Ctrl Pts',(109.250792830405,-12.0339139003957,
59.9906797226233));
#186347=CARTESIAN_POINT('Ctrl Pts',(108.550967101069,-11.6575470229572,
59.8443399405338));
#186348=CARTESIAN_POINT('Ctrl Pts',(107.628519625626,-11.048776635446,59.6512194976542));
#186349=CARTESIAN_POINT('Ctrl Pts',(107.373529672581,-10.8671978593662,
59.5978079690161));
#186350=CARTESIAN_POINT('Ctrl Pts',(106.850294642191,-10.4658965124238,
59.4881725473388));
#186351=CARTESIAN_POINT('Ctrl Pts',(106.583500592508,-10.2441546883599,
59.4322671054812));
#186352=CARTESIAN_POINT('Ctrl Pts',(105.966221290747,-9.68851907553079,
59.3027759329984));
#186353=CARTESIAN_POINT('Ctrl Pts',(105.624189772017,-9.34486134790611,
59.2308502016745));
#186354=CARTESIAN_POINT('Ctrl Pts',(105.21524486331,-8.88506388942526,59.143984133459));
#186355=CARTESIAN_POINT('Ctrl Pts',(105.129875396587,-8.78610309430652,
59.1257962386369));
#186356=CARTESIAN_POINT('Ctrl Pts',(104.911838299881,-8.52544257103956,
59.0791880659478));
#186357=CARTESIAN_POINT('Ctrl Pts',(104.781603815473,-8.36186613787664,
59.0512003770977));
#186358=CARTESIAN_POINT('Ctrl Pts',(104.436161232675,-7.90606134668474,
58.9766487802347));
#186359=CARTESIAN_POINT('Ctrl Pts',(104.228840159586,-7.60763160336805,
58.9315488782535));
#186360=CARTESIAN_POINT('Ctrl Pts',(103.83041101936,-6.98127575743222,58.8445096536074));
#186361=CARTESIAN_POINT('Ctrl Pts',(103.640375514436,-6.65262136003278,
58.8027776458652));
#186362=CARTESIAN_POINT('Ctrl Pts',(103.287879427994,-5.97939108095663,
58.7248534295313));
#186363=CARTESIAN_POINT('Ctrl Pts',(103.125455760468,-5.63474501456723,
58.6886681631905));
#186364=CARTESIAN_POINT('Ctrl Pts',(102.754489486424,-4.75364716805687,
58.6051776592044));
#186365=CARTESIAN_POINT('Ctrl Pts',(102.564614963436,-4.20889762287071,
58.5616052014557));
#186366=CARTESIAN_POINT('Ctrl Pts',(102.317229074917,-3.31966234096533,
58.5029892298193));
#186367=CARTESIAN_POINT('Ctrl Pts',(102.237119228676,-2.98175700208736,
58.4834744150268));
#186368=CARTESIAN_POINT('Ctrl Pts',(102.143823970434,-2.50557116089143,
58.4595633350259));
#186369=CARTESIAN_POINT('Ctrl Pts',(102.119427593877,-2.36980130658472,
58.4531465691196));
#186370=CARTESIAN_POINT('Ctrl Pts',(102.057617438939,-1.99210732526352,
58.4364040758067));
#186371=CARTESIAN_POINT('Ctrl Pts',(102.024755348943,-1.74946093646282,
58.4269048771876));
#186372=CARTESIAN_POINT('Ctrl Pts',(101.951565432986,-1.07054042208053,
58.4038874117156));
#186373=CARTESIAN_POINT('Ctrl Pts',(101.92581646583,-0.632606724627165,
58.3931148720186));
#186374=CARTESIAN_POINT('Ctrl Pts',(101.918350216145,0.0517733804404306,
58.382898292293));
#186375=CARTESIAN_POINT('Ctrl Pts',(101.922279839217,0.298038649552079,
58.3805672237773));
#186376=CARTESIAN_POINT('Ctrl Pts',(101.944293541922,0.813131802559715,
58.378508659593));
#186377=CARTESIAN_POINT('Ctrl Pts',(101.963675680976,1.08191790442571,58.3790382325729));
#186378=CARTESIAN_POINT('Ctrl Pts',(102.024269068008,1.67818784857894,58.3837204401154));
#186379=CARTESIAN_POINT('Ctrl Pts',(102.06941541431,2.00528819897112,58.3886621852478));
#186380=CARTESIAN_POINT('Ctrl Pts',(102.252549109192,3.05167094571696,58.4119970789988));
#186381=CARTESIAN_POINT('Ctrl Pts',(102.436612856431,3.76271670958568,58.4395009374162));
#186382=CARTESIAN_POINT('Ctrl Pts',(102.740773885875,4.63307852635012,58.4875084157057));
#186383=CARTESIAN_POINT('Ctrl Pts',(102.807447662412,4.81138131478656,58.4981222182692));
#186384=CARTESIAN_POINT('Ctrl Pts',(102.962955648451,5.20157270975982,58.5230916109307));
#186385=CARTESIAN_POINT('Ctrl Pts',(103.053513781866,5.41274488839898,58.5377660429203));
#186386=CARTESIAN_POINT('Ctrl Pts',(103.372229421647,6.10639564721346,58.589905492546));
#186387=CARTESIAN_POINT('Ctrl Pts',(103.623788036266,6.57780657297239,58.6318163633313));
#186388=CARTESIAN_POINT('Ctrl Pts',(104.01468572894,7.21706777752638,58.6983130368445));
#186389=CARTESIAN_POINT('Ctrl Pts',(104.131951611141,7.39894151672453,58.7184069722934));
#186390=CARTESIAN_POINT('Ctrl Pts',(104.375829286261,7.75808924965383,58.7605178909363));
#186391=CARTESIAN_POINT('Ctrl Pts',(104.502509670978,7.93532551059293,58.7825480811276));
#186392=CARTESIAN_POINT('Ctrl Pts',(104.806069119068,8.33909106701811,58.8356272618875));
#186393=CARTESIAN_POINT('Ctrl Pts',(104.986036476691,8.56323146678516,58.8673059483869));
#186394=CARTESIAN_POINT('Ctrl Pts',(105.524614237572,9.19157060047395,58.9625122021844));
#186395=CARTESIAN_POINT('Ctrl Pts',(105.900780706283,9.58020194423673,59.0294844967148));
#186396=CARTESIAN_POINT('Ctrl Pts',(106.432416330796,10.0652659689011,59.1241819595329));
#186397=CARTESIAN_POINT('Ctrl Pts',(106.568062064155,10.1839519667814,59.1483446829909));
#186398=CARTESIAN_POINT('Ctrl Pts',(107.11332517056,10.6411825880818,59.2454578434561));
#186399=CARTESIAN_POINT('Ctrl Pts',(107.540906406993,10.9570240383061,59.3217094916449));
#186400=CARTESIAN_POINT('Ctrl Pts',(108.449380222038,11.5470377948677,59.4843150452172));
#186401=CARTESIAN_POINT('Ctrl Pts',(108.931802983704,11.8188256777415,59.570955894139));
#186402=CARTESIAN_POINT('Ctrl Pts',(109.640610281318,12.1617693850152,59.6989191194564));
#186403=CARTESIAN_POINT('Ctrl Pts',(109.855119747486,12.2585817559649,59.7377272239079));
#186404=CARTESIAN_POINT('Ctrl Pts',(110.401281311468,12.487708913009,59.8367735521387));
#186405=CARTESIAN_POINT('Ctrl Pts',(110.736014572361,12.6124110844187,59.8977177565918));
#186406=CARTESIAN_POINT('Ctrl Pts',(111.511137194225,12.8655114715568,60.0390407043567));
#186407=CARTESIAN_POINT('Ctrl Pts',(111.954399339892,12.9847903415047,60.119988526134));
#186408=CARTESIAN_POINT('Ctrl Pts',(112.542832544102,13.1095830730738,60.2271441174067));
#186409=CARTESIAN_POINT('Ctrl Pts',(112.683481461978,13.1369421209752,60.2527344594261));
#186410=CARTESIAN_POINT('Ctrl Pts',(113.020421265411,13.1965521251643,60.3139608042953));
#186411=CARTESIAN_POINT('Ctrl Pts',(113.21704746674,13.2265732737833,60.3496295521908));
#186412=CARTESIAN_POINT('Ctrl Pts',(113.770245336926,13.2978721680189,60.4499160475966));
#186413=CARTESIAN_POINT('Ctrl Pts',(114.128105727272,13.328749185719,60.5147370715045));
#186414=CARTESIAN_POINT('Ctrl Pts',(115.009487793307,13.3680815138604,60.6745963157342));
#186415=CARTESIAN_POINT('Ctrl Pts',(115.533764431818,13.3597628890784,60.7698056127025));
#186416=CARTESIAN_POINT('Ctrl Pts',(116.396792464626,13.2942870369107,60.9267630984186));
#186417=CARTESIAN_POINT('Ctrl Pts',(116.736951665917,13.2550401511003,60.988686797659));
#186418=CARTESIAN_POINT('Ctrl Pts',(117.530664211689,13.1317629284829,61.1333196159765));
#186419=CARTESIAN_POINT('Ctrl Pts',(117.982615037574,13.0369043089246,61.2158285959178));
#186420=CARTESIAN_POINT('Ctrl Pts',(118.753447251637,12.8315730227818,61.3565373467627));
#186421=CARTESIAN_POINT('Ctrl Pts',(119.075219000797,12.7322883896691,61.4152341570359));
#186422=CARTESIAN_POINT('Ctrl Pts',(119.517472589056,12.576433390397,61.4955966707724));
#186423=CARTESIAN_POINT('Ctrl Pts',(119.641491808641,12.5305504516168,61.5180962721938));
#186424=CARTESIAN_POINT('Ctrl Pts',(119.933687864695,12.4172323908981,61.5710059976784));
#186425=CARTESIAN_POINT('Ctrl Pts',(120.101077122722,12.3481859799875,61.6012415758661));
#186426=CARTESIAN_POINT('Ctrl Pts',(120.846030158616,12.0223757780061,61.735561964536));
#186427=CARTESIAN_POINT('Ctrl Pts',(121.406999501065,11.7263298088096,61.8361064899413));
#186428=CARTESIAN_POINT('Ctrl Pts',(121.944453055693,11.3913829322761,61.9325710545576));
#186429=CARTESIAN_POINT('',(106.661976927588,10.2288565995845,58.9614167108613));
#186430=CARTESIAN_POINT('Ctrl Pts',(106.661350930769,10.2295773178667,58.9618221141476));
#186431=CARTESIAN_POINT('Ctrl Pts',(106.825922779295,10.3703884207358,58.993811800576));
#186432=CARTESIAN_POINT('Ctrl Pts',(106.993951579293,10.506970800954,59.0264734536535));
#186433=CARTESIAN_POINT('Ctrl Pts',(107.16541057696,10.6393620137197,59.0598018729417));
#186434=CARTESIAN_POINT('Ctrl Pts',(107.336748834558,10.7716599976416,59.0931068226209));
#186435=CARTESIAN_POINT('Ctrl Pts',(107.51151194005,10.8997723090449,59.1270774986143));
#186436=CARTESIAN_POINT('Ctrl Pts',(107.689704886371,11.0236957681757,59.1617148714556));
#186437=CARTESIAN_POINT('Ctrl Pts',(107.732786344196,11.0536565684669,59.1700891003352));
#186438=CARTESIAN_POINT('Ctrl Pts',(107.776068430774,11.0833723346163,59.1785023276886));
#186439=CARTESIAN_POINT('Ctrl Pts',(107.819551448625,11.1128426273365,59.1869546123197));
#186440=CARTESIAN_POINT('Ctrl Pts',(107.837833222047,11.1252329636295,59.1905082468226));
#186441=CARTESIAN_POINT('Ctrl Pts',(107.856150514099,11.137579906738,59.1940687854823));
#186442=CARTESIAN_POINT('Ctrl Pts',(107.87450335123,11.1498834153761,59.1976362334398));
#186443=CARTESIAN_POINT('Ctrl Pts',(107.891038087995,11.1609680926477,59.2008502767225));
#186444=CARTESIAN_POINT('Ctrl Pts',(107.907599232881,11.17201591509,59.2040694532496));
#186445=CARTESIAN_POINT('Ctrl Pts',(107.924204326524,11.1830384116525,59.2072971725923));
#186446=CARTESIAN_POINT('Ctrl Pts',(108.004056796198,11.2360446512704,59.2228189977908));
#186447=CARTESIAN_POINT('Ctrl Pts',(108.084832644889,11.2883974214026,59.2385203105836));
#186448=CARTESIAN_POINT('Ctrl Pts',(108.166019887746,11.3397585101557,59.2543015907009));
#186449=CARTESIAN_POINT('Ctrl Pts',(108.210746221189,11.3680535119403,59.2629955526071));
#186450=CARTESIAN_POINT('Ctrl Pts',(108.255596909759,11.3960483115572,59.2717136868221));
#186451=CARTESIAN_POINT('Ctrl Pts',(108.30048285165,11.4236920848158,59.2804386736227));
#186452=CARTESIAN_POINT('Ctrl Pts',(108.312416977699,11.4310419199901,59.2827584443096));
#186453=CARTESIAN_POINT('Ctrl Pts',(108.324353582836,11.4383669634109,59.2850786968848));
#186454=CARTESIAN_POINT('Ctrl Pts',(108.336290964591,11.4456663086518,59.28739910042));
#186455=CARTESIAN_POINT('Ctrl Pts',(108.348094863653,11.4528840332931,59.2896935574187));
#186456=CARTESIAN_POINT('Ctrl Pts',(108.359907957709,11.4600817926637,59.291989801752));
#186457=CARTESIAN_POINT('Ctrl Pts',(108.371730890304,11.4672600077199,59.2942879585132));
#186458=CARTESIAN_POINT('Ctrl Pts',(108.544485776277,11.572146990161,59.3278682742278));
#186459=CARTESIAN_POINT('Ctrl Pts',(108.719293829397,11.6728372308274,59.3618476871988));
#186460=CARTESIAN_POINT('Ctrl Pts',(108.896190732468,11.769405294605,59.3962331334954));
#186461=CARTESIAN_POINT('Ctrl Pts',(109.073164318318,11.8660152195306,59.4306334854885));
#186462=CARTESIAN_POINT('Ctrl Pts',(109.252228929304,11.9584995635849,59.4654402936222));
#186463=CARTESIAN_POINT('Ctrl Pts',(109.43344545626,12.0468875256908,59.5006653939349));
#186464=CARTESIAN_POINT('Ctrl Pts',(109.567751674034,12.112395087758,59.5267720083435));
#186465=CARTESIAN_POINT('Ctrl Pts',(109.703240449451,12.1756516537283,59.5531084898193));
#186466=CARTESIAN_POINT('Ctrl Pts',(109.839943719786,12.2366521263733,59.579681046371));
#186467=CARTESIAN_POINT('Ctrl Pts',(109.913322473696,12.26939559081,59.5939445024184));
#186468=CARTESIAN_POINT('Ctrl Pts',(109.987051250195,12.3014887635243,59.6082759963045));
#186469=CARTESIAN_POINT('Ctrl Pts',(110.061135575156,12.3329290625992,59.6226766021551));
#186470=CARTESIAN_POINT('Ctrl Pts',(110.090300640985,12.3453062880477,59.6283457449576));
#186471=CARTESIAN_POINT('Ctrl Pts',(110.119520813447,12.3575823177664,59.6340255994577));
#186472=CARTESIAN_POINT('Ctrl Pts',(110.148796444678,12.3697569395208,59.6397162341043));
#186473=CARTESIAN_POINT('Ctrl Pts',(110.172247679429,12.3795094162652,59.6442747151128));
#186474=CARTESIAN_POINT('Ctrl Pts',(110.19573662675,12.3891976567719,59.6488405267389));
#186475=CARTESIAN_POINT('Ctrl Pts',(110.219242226367,12.3988129478252,59.6534095752596));
#186476=CARTESIAN_POINT('Ctrl Pts',(110.450827955009,12.4935462973671,59.6984255054258));
#186477=CARTESIAN_POINT('Ctrl Pts',(110.684462240573,12.5813844818697,59.7438396367068));
#186478=CARTESIAN_POINT('Ctrl Pts',(110.919958817175,12.6623105107267,59.7896157625019));
#186479=CARTESIAN_POINT('Ctrl Pts',(111.155664087698,12.7433082551496,59.8354324544883));
#186480=CARTESIAN_POINT('Ctrl Pts',(111.39323540817,12.8173817852037,59.8816118716509));
#186481=CARTESIAN_POINT('Ctrl Pts',(111.63250912853,12.8844674464811,59.9281222034812));
#186482=CARTESIAN_POINT('Ctrl Pts',(111.752135698328,12.9180073919844,59.9513753691388));
#186483=CARTESIAN_POINT('Ctrl Pts',(111.872188112893,12.9497999244005,59.9747113110469));
#186484=CARTESIAN_POINT('Ctrl Pts',(111.992647543251,12.9798324840516,59.9981263692054));
#186485=CARTESIAN_POINT('Ctrl Pts',(112.084399238805,13.0027077231394,60.0159611811513));
#186486=CARTESIAN_POINT('Ctrl Pts',(112.176392155673,13.0245628749281,60.0338428820048));
#186487=CARTESIAN_POINT('Ctrl Pts',(112.268589488635,13.045384961734,60.05176431752));
#186488=CARTESIAN_POINT('Ctrl Pts',(112.453592664605,13.0871665628464,60.0877254715117));
#186489=CARTESIAN_POINT('Ctrl Pts',(112.639442277684,13.1247970806182,60.1238511570314));
#186490=CARTESIAN_POINT('Ctrl Pts',(112.826148207148,13.1582277947365,60.1601432944253));
#186491=CARTESIAN_POINT('Ctrl Pts',(112.967943093299,13.1836169418084,60.1877055657722));
#186492=CARTESIAN_POINT('Ctrl Pts',(113.110232052057,13.2065831118267,60.2153638755844));
#186493=CARTESIAN_POINT('Ctrl Pts',(113.253013755355,13.2271344963784,60.2431179657105));
#186494=CARTESIAN_POINT('Ctrl Pts',(113.386871602196,13.2464014193957,60.2691374252037));
#186495=CARTESIAN_POINT('Ctrl Pts',(113.521162574455,13.2635458793658,60.2952410761696));
#186496=CARTESIAN_POINT('Ctrl Pts',(113.65588596443,13.2785663779232,60.3214287810442));
#186497=CARTESIAN_POINT('Ctrl Pts',(113.671894084392,13.2803511455337,60.3245404598793));
#186498=CARTESIAN_POINT('Ctrl Pts',(113.687917524092,13.2821069432664,60.3276551165844));
#186499=CARTESIAN_POINT('Ctrl Pts',(113.703955974844,13.2838336233231,60.3307726911571));
#186500=CARTESIAN_POINT('Ctrl Pts',(113.797462937436,13.2939004689287,60.3489486941553));
#186501=CARTESIAN_POINT('Ctrl Pts',(113.891450114483,13.3029699738907,60.3672180418533));
#186502=CARTESIAN_POINT('Ctrl Pts',(113.985307606065,13.3109824254935,60.3854621811247));
#186503=CARTESIAN_POINT('Ctrl Pts',(114.04762458284,13.3163023179392,60.3975754347829));
#186504=CARTESIAN_POINT('Ctrl Pts',(114.109884258143,13.3211573008145,60.4096775501077));
#186505=CARTESIAN_POINT('Ctrl Pts',(114.171907118068,13.3255425067845,60.4217336329563));
#186506=CARTESIAN_POINT('Ctrl Pts',(114.18402496701,13.3263992757821,60.4240891159344));
#186507=CARTESIAN_POINT('Ctrl Pts',(114.196142823531,13.32723878514,60.4264446003854));
#186508=CARTESIAN_POINT('Ctrl Pts',(114.20826199609,13.3280611378834,60.4288003406496));
#186509=CARTESIAN_POINT('Ctrl Pts',(114.445669580006,13.3441705526948,60.4749479304909));
#186510=CARTESIAN_POINT('Ctrl Pts',(114.683414492677,13.353688708566,60.5211610907271));
#186511=CARTESIAN_POINT('Ctrl Pts',(114.921378109398,13.3566581767227,60.5674167629362));
#186512=CARTESIAN_POINT('Ctrl Pts',(115.159173594614,13.3596255468228,60.6136397535285));
#186513=CARTESIAN_POINT('Ctrl Pts',(115.397187946768,13.3560534382267,60.6599052877561));
#186514=CARTESIAN_POINT('Ctrl Pts',(115.635301434022,13.3459323690487,60.7061900919911));
#186515=CARTESIAN_POINT('Ctrl Pts',(115.806511310614,13.3386550534085,60.739470086806));
#186516=CARTESIAN_POINT('Ctrl Pts',(115.977772432714,13.3279908526501,60.7727600427885));
#186517=CARTESIAN_POINT('Ctrl Pts',(116.149037779096,13.3139197681031,60.806050819892));
#186518=CARTESIAN_POINT('Ctrl Pts',(116.172635983815,13.3119809501182,60.810637869111));
#186519=CARTESIAN_POINT('Ctrl Pts',(116.196234263956,13.3099774298684,60.8152249329905));
#186520=CARTESIAN_POINT('Ctrl Pts',(116.219832491622,13.307909134588,60.8198119866698));
#186521=CARTESIAN_POINT('Ctrl Pts',(116.240170921855,13.3061265482066,60.8237653967545));
#186522=CARTESIAN_POINT('Ctrl Pts',(116.26050592698,13.3042961307879,60.8277181410621));
#186523=CARTESIAN_POINT('Ctrl Pts',(116.28082958516,13.3024186422104,60.8316686797361));
#186524=CARTESIAN_POINT('Ctrl Pts',(116.495305897586,13.282605436185,60.8733588596927));
#186525=CARTESIAN_POINT('Ctrl Pts',(116.708780448291,13.2575315963514,60.9148543159246));
#186526=CARTESIAN_POINT('Ctrl Pts',(116.921258479399,13.2272498512068,60.9561560674024));
#186527=CARTESIAN_POINT('Ctrl Pts',(116.979436757235,13.2189584538647,60.9674648354668));
#186528=CARTESIAN_POINT('Ctrl Pts',(117.037540322311,13.2102763125356,60.9787590807694));
#186529=CARTESIAN_POINT('Ctrl Pts',(117.095569257697,13.2012038297673,60.9900388194574));
#186530=CARTESIAN_POINT('Ctrl Pts',(117.137732860675,13.1946117984137,60.9982346345379));
#186531=CARTESIAN_POINT('Ctrl Pts',(117.179857063159,13.1878136833666,61.0064227908998));
#186532=CARTESIAN_POINT('Ctrl Pts',(117.221941887973,13.1808095430678,61.0146032929798));
#186533=CARTESIAN_POINT('Ctrl Pts',(117.250681779517,13.1760263882504,61.0201897898609));
#186534=CARTESIAN_POINT('Ctrl Pts',(117.279403577157,13.1711470762405,61.0257727696255));
#186535=CARTESIAN_POINT('Ctrl Pts',(117.308094681736,13.1661738703345,61.0313497832339));
#186536=CARTESIAN_POINT('Ctrl Pts',(117.448904624499,13.1417664155069,61.0587206000251));
#186537=CARTESIAN_POINT('Ctrl Pts',(117.58906394148,13.1150870864737,61.0859649473445));
#186538=CARTESIAN_POINT('Ctrl Pts',(117.728884739466,13.0860754292987,61.1131434929087));
#186539=CARTESIAN_POINT('Ctrl Pts',(117.868152999214,13.0571784192304,61.1402146353833));
#186540=CARTESIAN_POINT('Ctrl Pts',(118.007085685501,13.0259674344299,61.1672205486595));
#186541=CARTESIAN_POINT('Ctrl Pts',(118.14598009617,12.992332384803,61.1942190218719));
#186542=CARTESIAN_POINT('Ctrl Pts',(118.171469405761,12.9861598240143,61.1991736664749));
#186543=CARTESIAN_POINT('Ctrl Pts',(118.196957389447,12.9799054892575,61.2041280533467));
#186544=CARTESIAN_POINT('Ctrl Pts',(118.222445832201,12.9735685161642,61.2090825294528));
#186545=CARTESIAN_POINT('Ctrl Pts',(118.23754875077,12.9698136069482,61.212018254083));
#186546=CARTESIAN_POINT('Ctrl Pts',(118.252654100341,12.9660291080705,61.2149544512547));
#186547=CARTESIAN_POINT('Ctrl Pts',(118.267754790522,12.9622167157772,61.2178897427281));
#186548=CARTESIAN_POINT('Ctrl Pts',(118.477140301939,12.9093542505205,61.2585903662726));
#186549=CARTESIAN_POINT('Ctrl Pts',(118.684730096326,12.8513622271013,61.2989419360439));
#186550=CARTESIAN_POINT('Ctrl Pts',(118.890527441424,12.7882501539497,61.3389450872296));
#186551=CARTESIAN_POINT('Ctrl Pts',(118.954537756875,12.7686200478895,61.3513874942257));
#186552=CARTESIAN_POINT('Ctrl Pts',(119.018374602236,12.7484942377947,61.3637961818838));
#186553=CARTESIAN_POINT('Ctrl Pts',(119.082037874589,12.7278720011977,61.3761711301986));
#186554=CARTESIAN_POINT('Ctrl Pts',(119.128757185184,12.7127383669824,61.385252489553));
#186555=CARTESIAN_POINT('Ctrl Pts',(119.175383018273,12.6973373792244,61.3943156786303));
#186556=CARTESIAN_POINT('Ctrl Pts',(119.221915290494,12.6816685898537,61.4033606812262));
#186557=CARTESIAN_POINT('Ctrl Pts',(119.250628234944,12.6720000940479,61.4089419400966));
#186558=CARTESIAN_POINT('Ctrl Pts',(119.279305788299,12.6622295793524,61.4145163196007));
#186559=CARTESIAN_POINT('Ctrl Pts',(119.307959019654,12.6523529953859,61.4200859713631));
#186560=CARTESIAN_POINT('Ctrl Pts',(119.422699883056,12.6128025601217,61.442389447162));
#186561=CARTESIAN_POINT('Ctrl Pts',(119.536995525351,12.5715684555563,61.4646063803124));
#186562=CARTESIAN_POINT('Ctrl Pts',(119.650676763164,12.5286947613551,61.4867038847336));
#186563=CARTESIAN_POINT('Ctrl Pts',(119.750603748029,12.4910083403235,61.5061278198734));
#186564=CARTESIAN_POINT('Ctrl Pts',(119.850056043861,12.452055293347,61.5254594843514));
#186565=CARTESIAN_POINT('Ctrl Pts',(119.94892798088,12.4118901617296,61.5446783379412));
#186566=CARTESIAN_POINT('Ctrl Pts',(120.037512300966,12.3759042087613,61.561897471392));
#186567=CARTESIAN_POINT('Ctrl Pts',(120.125630778712,12.3389454038338,61.5790260538131));
#186568=CARTESIAN_POINT('Ctrl Pts',(120.213209775707,12.3010583961822,61.5960497712754));
#186569=CARTESIAN_POINT('Ctrl Pts',(120.237949446469,12.2903559203873,61.6008587001239));
#186570=CARTESIAN_POINT('Ctrl Pts',(120.262654935792,12.2795755831455,61.6056609847406));
#186571=CARTESIAN_POINT('Ctrl Pts',(120.287326902652,12.2687172406279,61.610456753218));
#186572=CARTESIAN_POINT('Ctrl Pts',(120.486416639678,12.1810961535618,61.6491560709665));
#186573=CARTESIAN_POINT('Ctrl Pts',(120.683311997193,12.0884052960903,61.6874288424188));
#186574=CARTESIAN_POINT('Ctrl Pts',(120.878023145789,11.9906823843153,61.7252770445476));
#186575=CARTESIAN_POINT('Ctrl Pts',(121.072799870817,11.89292656061,61.7631379935069));
#186576=CARTESIAN_POINT('Ctrl Pts',(121.265391273193,11.7901350574577,61.800574156654));
#186577=CARTESIAN_POINT('Ctrl Pts',(121.455782450768,11.6823003088381,61.8375826372896));
#186578=CARTESIAN_POINT('Ctrl Pts',(121.620325552598,11.5891055282344,61.8695667358985));
#186579=CARTESIAN_POINT('Ctrl Pts',(121.783225041274,11.4921431217687,61.9012313468801));
#186580=CARTESIAN_POINT('Ctrl Pts',(121.944453055693,11.3913829322761,61.9325710545575));
#186581=CARTESIAN_POINT('Ctrl Pts',(106.597794809764,10.1748376799211,58.949467993991));
#186582=CARTESIAN_POINT('Ctrl Pts',(106.619133959162,10.1929126322122,58.9534397950288));
#186583=CARTESIAN_POINT('Ctrl Pts',(106.640528384642,10.2109188565186,58.9574223407024));
#186584=CARTESIAN_POINT('Ctrl Pts',(106.661977627748,10.2288560234639,58.961415541896));
#186585=CARTESIAN_POINT('Origin',(121.630276337646,13.,49.6468984217139));
#186586=CARTESIAN_POINT('',(115.139466160418,13.,48.3852064367498));
#186587=CARTESIAN_POINT('Ctrl Pts',(113.04734486836,13.,48.4878956643013));
#186588=CARTESIAN_POINT('Ctrl Pts',(114.126636691851,13.,48.364665625098));
#186589=CARTESIAN_POINT('Ctrl Pts',(115.139466160442,13.,48.3852064363081));
#186590=CARTESIAN_POINT('',(121.057846598951,13.,52.591779437011));
#186591=CARTESIAN_POINT('',(119.633560001989,13.,49.2587741462908));
#186592=CARTESIAN_POINT('Ctrl Pts',(119.633560002146,13.,49.2587741458773));
#186593=CARTESIAN_POINT('Ctrl Pts',(120.58033318249,13.,49.6191434041911));
#186594=CARTESIAN_POINT('Ctrl Pts',(121.534871380993,13.,50.1377119246391));
#186595=CARTESIAN_POINT('',(119.633560001989,13.,49.2587741462908));
#186596=CARTESIAN_POINT('Origin',(117.338810602979,1.45439216225896E-14,
49.0673970427951));
#186597=CARTESIAN_POINT('',(115.139466160418,-13.,48.3852064367498));
#186598=CARTESIAN_POINT('Ctrl Pts',(115.139466160442,-13.,48.3852064363082));
#186599=CARTESIAN_POINT('Ctrl Pts',(114.126636691851,-13.,48.364665625098));
#186600=CARTESIAN_POINT('Ctrl Pts',(113.04734486836,-13.,48.4878956643013));
#186601=CARTESIAN_POINT('Origin',(117.386513081203,1.45439216225896E-14,
48.8219902915203));
#186602=CARTESIAN_POINT('Origin',(117.338810602979,1.45439216225896E-14,
49.0673970427951));
#186603=CARTESIAN_POINT('',(119.633560001989,-13.,49.2587741462908));
#186604=CARTESIAN_POINT('Ctrl Pts',(121.534871380993,-13.,50.1377119246392));
#186605=CARTESIAN_POINT('Ctrl Pts',(120.58033318249,-13.,49.6191434041912));
#186606=CARTESIAN_POINT('Ctrl Pts',(119.633560002146,-13.,49.2587741458774));
#186607=CARTESIAN_POINT('Origin',(117.386513081203,1.45439216225896E-14,
48.8219902915203));
#186608=CARTESIAN_POINT('Origin',(113.14274982476,-13.,47.9970821613267));
#186609=CARTESIAN_POINT('',(112.570320086065,-13.,50.9419631766238));
#186610=CARTESIAN_POINT('',(115.139466160418,-13.,48.3852064367498));
#186611=CARTESIAN_POINT('Origin',(116.814083342508,1.45439216225896E-14,
51.7668713068174));
#186612=CARTESIAN_POINT('Origin',(116.814083342508,1.45439216225896E-14,
51.7668713068174));
#186613=CARTESIAN_POINT('Origin',(115.383008995769,1.45439216225896E-14,
59.12907384506));
#186614=CARTESIAN_POINT('Origin',(115.096794126421,1.45439216225896E-14,
60.6015143527085));
#186615=CARTESIAN_POINT('',(122.039447043815,11.3329480580267,61.950331991012));
#186616=CARTESIAN_POINT('Ctrl Pts',(121.944453055789,11.3913829318325,61.9325710578547));
#186617=CARTESIAN_POINT('Ctrl Pts',(121.975991009671,11.3717006163854,61.9384667390898));
#186618=CARTESIAN_POINT('Ctrl Pts',(122.007448447719,11.3518837406497,61.9443467695542));
#186619=CARTESIAN_POINT('Ctrl Pts',(122.038824288318,11.3319330864622,61.9502109390019));
#186620=CARTESIAN_POINT('Ctrl Pts',(122.039928552843,11.333968991207,61.9511297038209));
#186621=CARTESIAN_POINT('Ctrl Pts',(123.16620920987,10.6501122569522,62.1700575786149));
#186622=CARTESIAN_POINT('Ctrl Pts',(124.187604468863,9.79818933144462,62.3685976955743));
#186623=CARTESIAN_POINT('Ctrl Pts',(125.955460550856,7.80211216460018,62.7122358221437));
#186624=CARTESIAN_POINT('Ctrl Pts',(126.689541950163,6.67413921942583,62.85492750354));
#186625=CARTESIAN_POINT('Ctrl Pts',(127.936628835462,3.93791384118314,63.0973378475144));
#186626=CARTESIAN_POINT('Ctrl Pts',(128.393441930735,2.20871226321621,63.1861337613069));
#186627=CARTESIAN_POINT('Ctrl Pts',(128.552284670311,-1.46551021789508,
63.2170098162093));
#186628=CARTESIAN_POINT('Ctrl Pts',(128.281605122352,-3.25174142720192,
63.164394779438));
#186629=CARTESIAN_POINT('Ctrl Pts',(127.241550546623,-6.18489950503424,
62.9622276406228));
#186630=CARTESIAN_POINT('Ctrl Pts',(126.617322374644,-7.36740292814777,
62.8408893700727));
#186631=CARTESIAN_POINT('Ctrl Pts',(125.059576412758,-9.51520023323271,
62.5380927174118));
#186632=CARTESIAN_POINT('Ctrl Pts',(124.124637298172,-10.4720112212054,
62.3563580563915));
#186633=CARTESIAN_POINT('Ctrl Pts',(123.077241409441,-11.2743970687384,
62.1527639037644));
#186634=CARTESIAN_POINT('Origin',(115.096794126421,1.45439216225896E-14,
60.6015143527085));
#186635=CARTESIAN_POINT('Ctrl Pts',(119.407391898135,-13.0301062068,64.4806209347011));
#186636=CARTESIAN_POINT('Ctrl Pts',(118.147720209373,-13.52088854622,64.2197588532859));
#186637=CARTESIAN_POINT('Ctrl Pts',(115.484843558882,-14.11864469328,63.6701345092559));
#186638=CARTESIAN_POINT('Ctrl Pts',(111.407779104958,-13.78606076252,62.8296130437921));
#186639=CARTESIAN_POINT('Ctrl Pts',(107.603918121139,-12.25314221515,62.042197218315));
#186640=CARTESIAN_POINT('Ctrl Pts',(104.405185821524,-9.65337632876199,
61.3724070805235));
#186641=CARTESIAN_POINT('Ctrl Pts',(102.090884786275,-6.21311314882798,
60.8745338232188));
#186642=CARTESIAN_POINT('Ctrl Pts',(100.863295028327,-2.23188950467599,
60.587896894062));
#186643=CARTESIAN_POINT('Ctrl Pts',(100.830083860925,1.94365945142001,60.5334248031237));
#186644=CARTESIAN_POINT('Ctrl Pts',(101.994925696463,5.94997864935902,60.7118317873852));
#186645=CARTESIAN_POINT('Ctrl Pts',(104.257183696659,9.43824757472701,61.1035559294922));
#186646=CARTESIAN_POINT('Ctrl Pts',(107.420671557756,12.10475106522,61.6704622847683));
#186647=CARTESIAN_POINT('Ctrl Pts',(111.210735091372,13.71732310055,62.3591632207526));
#186648=CARTESIAN_POINT('Ctrl Pts',(115.298165671407,14.13556092567,63.1056667435966));
#186649=CARTESIAN_POINT('Ctrl Pts',(119.327863642558,13.32304958287,63.8409481280871));
#186650=CARTESIAN_POINT('Ctrl Pts',(122.949755987961,11.35053247341,64.4969597333906));
#186651=CARTESIAN_POINT('Ctrl Pts',(125.849276342301,8.38975190055401,65.0125557470494));
#186652=CARTESIAN_POINT('Ctrl Pts',(127.774753525765,4.69849588175201,65.338816003207));
#186653=CARTESIAN_POINT('Ctrl Pts',(128.559323946183,0.598153168230215,
65.4433053433738));
#186654=CARTESIAN_POINT('Ctrl Pts',(128.135460009217,-3.55426929776699,
65.3128976673845));
#186655=CARTESIAN_POINT('Ctrl Pts',(126.540849582971,-7.39723011566199,
64.9549187912497));
#186656=CARTESIAN_POINT('Ctrl Pts',(123.915114606311,-10.59613196357,64.396508606043));
#186657=CARTESIAN_POINT('Ctrl Pts',(120.48765454368,-12.87245417943,63.6822580730997));
#186658=CARTESIAN_POINT('Ctrl Pts',(116.557673127465,-14.02800288271,62.8703267966466));
#186659=CARTESIAN_POINT('Ctrl Pts',(112.468127411276,-13.96216723722,62.0273792074582));
#186660=CARTESIAN_POINT('Ctrl Pts',(108.575867327145,-12.68067939367,61.2227802517869));
#186661=CARTESIAN_POINT('Ctrl Pts',(105.220565623354,-10.29511540522,60.5225559529361));
#186662=CARTESIAN_POINT('Ctrl Pts',(102.695143378168,-7.01318056982799,
59.9836446847886));
#186663=CARTESIAN_POINT('Ctrl Pts',(101.22026606865,-3.12062503134899,59.6489396850396));
#186664=CARTESIAN_POINT('Ctrl Pts',(100.925130760206,1.04363579573001,59.5435544445256));
#186665=CARTESIAN_POINT('Ctrl Pts',(101.836217230004,5.11702977330802,59.6726361362038));
#186666=CARTESIAN_POINT('Ctrl Pts',(103.874982436677,8.74489632052901,60.0209174632251));
#186667=CARTESIAN_POINT('Ctrl Pts',(106.864699073354,11.61136585444,60.5540459456192));
#186668=CARTESIAN_POINT('Ctrl Pts',(110.545842787632,13.46686179209,61.2215749077958));
#186669=CARTESIAN_POINT('Ctrl Pts',(114.598688340515,14.14983058118,61.9613557488326));
#186670=CARTESIAN_POINT('Ctrl Pts',(118.671147311171,13.60080777785,62.7049490710946));
#186671=CARTESIAN_POINT('Ctrl Pts',(122.409423585822,11.86759547232,63.3835835334376));
#186672=CARTESIAN_POINT('Ctrl Pts',(125.488817531349,9.10110027621301,63.9341436058365));
#186673=CARTESIAN_POINT('Ctrl Pts',(127.641996808559,5.54219424821201,64.3046648862414));
#186674=CARTESIAN_POINT('Ctrl Pts',(128.682272353622,1.50074274532801,64.4588585156218));
#186675=CARTESIAN_POINT('Ctrl Pts',(128.519852944246,-2.67137480574699,
64.3792707613319));
#186676=CARTESIAN_POINT('Ctrl Pts',(127.16966310462,-6.61090220091999,64.0688026714746));
#186677=CARTESIAN_POINT('Ctrl Pts',(124.750043663147,-9.97483429952299,
63.5504574876502));
#186678=CARTESIAN_POINT('Ctrl Pts',(121.472448102156,-12.47028165393,62.8653378082347));
#186679=CARTESIAN_POINT('Ctrl Pts',(117.623031813639,-13.87997168676,62.0690668843584));
#186680=CARTESIAN_POINT('Ctrl Pts',(113.537737240012,-14.0811660897,61.226945637699));
#186681=CARTESIAN_POINT('Ctrl Pts',(109.573044176586,-13.05634735175,60.4082670668599));
#186682=CARTESIAN_POINT('Ctrl Pts',(106.074931936307,-10.89474396662,59.6802830732504));
#186683=CARTESIAN_POINT('Ctrl Pts',(103.348755766122,-7.78456152314698,
59.1023490003672));
#186684=CARTESIAN_POINT('Ctrl Pts',(101.632660302733,-3.99659609901699,
58.720755707315));
#186685=CARTESIAN_POINT('Ctrl Pts',(101.076844893947,0.139343300067115,
58.5646991354477));
#186686=CARTESIAN_POINT('Ctrl Pts',(101.730486103999,4.26315041437501,58.6437382882256));
#186687=CARTESIAN_POINT('Ctrl Pts',(103.537456028837,8.01577531292601,58.946962951863));
#186688=CARTESIAN_POINT('Ctrl Pts',(106.34120921727,11.07048600428,59.4439436213124));
#186689=CARTESIAN_POINT('Ctrl Pts',(109.898412705345,13.16131620227,60.0873809237817));
#186690=CARTESIAN_POINT('Ctrl Pts',(113.900132430754,14.10622236873,60.8172238610665));
#186691=CARTESIAN_POINT('Ctrl Pts',(117.998731373649,13.82293380427,61.5658983045794));
#186692=CARTESIAN_POINT('Ctrl Pts',(121.838137481187,12.33611576178,62.2641905131989));
#186693=CARTESIAN_POINT('Ctrl Pts',(125.084845970359,9.77522189391502,62.847273400612));
#186694=CARTESIAN_POINT('Ctrl Pts',(127.456956901142,6.36322306770402,63.2603508958846));
#186695=CARTESIAN_POINT('Ctrl Pts',(128.748719088097,2.39719371119201,63.4634288204047));
#186696=CARTESIAN_POINT('Ctrl Pts',(128.848445985611,-1.77755329875599,
63.4347974005724));
#186697=CARTESIAN_POINT('Ctrl Pts',(127.748233896623,-5.79753384146799,
63.172920305643));
#186698=CARTESIAN_POINT('Ctrl Pts',(125.544672779088,-9.31273409308899,
62.6965728151966));
#186699=CARTESIAN_POINT('Ctrl Pts',(122.430351858199,-12.01710831635,62.0431906691766));
#186700=CARTESIAN_POINT('Ctrl Pts',(119.928388506017,-13.12246273504,61.524844857904));
#186701=CARTESIAN_POINT('Ctrl Pts',(118.625437907371,-13.47672248693,61.2555701666254));
#186702=CARTESIAN_POINT('Ctrl Pts',(119.35682826831,-12.83307257039,64.3467570107765));
#186703=CARTESIAN_POINT('Ctrl Pts',(118.11624992964,-13.31643358665,64.0896063191756));
#186704=CARTESIAN_POINT('Ctrl Pts',(115.493730405444,-13.90515081526,63.5478266449777));
#186705=CARTESIAN_POINT('Ctrl Pts',(111.47845293012,-13.57759602396,62.7193154114488));
#186706=CARTESIAN_POINT('Ctrl Pts',(107.732247701997,-12.06785737328,61.9431067855144));
#186707=CARTESIAN_POINT('Ctrl Pts',(104.582020756437,-9.50740362435499,
61.2827451804895));
#186708=CARTESIAN_POINT('Ctrl Pts',(102.302851223542,-6.11916208981799,
60.7917008295511));
#186709=CARTESIAN_POINT('Ctrl Pts',(101.093960356319,-2.19814017844699,
60.5086986147019));
#186710=CARTESIAN_POINT('Ctrl Pts',(101.061387385959,1.91426857128501,60.4543505773211));
#186711=CARTESIAN_POINT('Ctrl Pts',(102.208751162539,5.86000655617201,60.6293601541255));
#186712=CARTESIAN_POINT('Ctrl Pts',(104.436936619098,9.29552792137202,61.0144612316163));
#186713=CARTESIAN_POINT('Ctrl Pts',(107.552724066323,11.92171010742,61.5720955194281));
#186714=CARTESIAN_POINT('Ctrl Pts',(111.285612475627,13.50989777266,62.2496826816131));
#186715=CARTESIAN_POINT('Ctrl Pts',(115.311371320996,13.92181125028,62.9841983737852));
#186716=CARTESIAN_POINT('Ctrl Pts',(119.280270556188,13.12158622825,63.7076616221994));
#186717=CARTESIAN_POINT('Ctrl Pts',(122.847530763518,11.17889636753,64.3530537626213));
#186718=CARTESIAN_POINT('Ctrl Pts',(125.703342266057,8.26288698484901,64.8601535937572));
#186719=CARTESIAN_POINT('Ctrl Pts',(127.599839508207,4.62744797818601,65.1807806918523));
#186720=CARTESIAN_POINT('Ctrl Pts',(128.372682111344,0.589108246264615,
65.2829903638944));
#186721=CARTESIAN_POINT('Ctrl Pts',(127.955363593847,-3.50052371860999,
65.1538549949141));
#186722=CARTESIAN_POINT('Ctrl Pts',(126.385001929965,-7.28537353322399,
64.8005896242253));
#186723=CARTESIAN_POINT('Ctrl Pts',(123.799107777366,-10.43590346047,64.2499237493622));
#186724=CARTESIAN_POINT('Ctrl Pts',(120.423611756099,-12.67780446466,63.5457740532488));
#186725=CARTESIAN_POINT('Ctrl Pts',(116.553193214911,-13.81587963708,62.7454206846333));
#186726=CARTESIAN_POINT('Ctrl Pts',(112.525623211661,-13.75103951966,61.9145200138023));
#186727=CARTESIAN_POINT('Ctrl Pts',(108.692355602661,-12.48892958492,61.121388090907));
#186728=CARTESIAN_POINT('Ctrl Pts',(105.387926803782,-10.13943869826,60.4310525323871));
#186729=CARTESIAN_POINT('Ctrl Pts',(102.900828512264,-6.90713135975199,
59.8995907233755));
#186730=CARTESIAN_POINT('Ctrl Pts',(101.448389431029,-3.07343676687899,
59.569247295142));
#186731=CARTESIAN_POINT('Ctrl Pts',(101.157852983112,1.02785454631301,59.46475598703));
#186732=CARTESIAN_POINT('Ctrl Pts',(102.055298534003,5.03965304529702,59.5911861394423));
#186733=CARTESIAN_POINT('Ctrl Pts',(104.063370724214,8.61266111885201,59.9335013186626));
#186734=CARTESIAN_POINT('Ctrl Pts',(107.008014613714,11.4357855789,60.4578685028059));
#186735=CARTESIAN_POINT('Ctrl Pts',(110.633630225412,13.26322379345,61.1146038413743));
#186736=CARTESIAN_POINT('Ctrl Pts',(114.625327018159,13.93586512842,61.8424985081874));
#186737=CARTESIAN_POINT('Ctrl Pts',(118.636340646059,13.39514432645,62.5741480061266));
#186738=CARTESIAN_POINT('Ctrl Pts',(122.318224893007,11.68814064254,63.2418209139908));
#186739=CARTESIAN_POINT('Ctrl Pts',(125.351190043614,8.96347876689701,63.783356097844));
#186740=CARTESIAN_POINT('Ctrl Pts',(127.471946201774,5.45838843197201,64.1475749308939));
#186741=CARTESIAN_POINT('Ctrl Pts',(128.496627306379,1.47804939228401,64.2987372929904));
#186742=CARTESIAN_POINT('Ctrl Pts',(128.336799905422,-2.63097984012399,
64.2196533766126));
#186743=CARTESIAN_POINT('Ctrl Pts',(127.007162843178,-6.51093600877899,
63.9131803619128));
#186744=CARTESIAN_POINT('Ctrl Pts',(124.624267467324,-9.82400069590499,
63.4019736489391));
#186745=CARTESIAN_POINT('Ctrl Pts',(121.396369784457,-12.2817133566,62.7265143066441));
#186746=CARTESIAN_POINT('Ctrl Pts',(117.60529811228,-13.67008688219,61.9415844839235));
#186747=CARTESIAN_POINT('Ctrl Pts',(113.581914968302,-13.86823894118,61.1114976601534));
#186748=CARTESIAN_POINT('Ctrl Pts',(109.677309669108,-12.85891691211,60.3044990257867));
#186749=CARTESIAN_POINT('Ctrl Pts',(106.23222983105,-10.73000002767,59.5868235383575));
#186750=CARTESIAN_POINT('Ctrl Pts',(103.547413297838,-7.66684794197098,
59.0169290046143));
#186751=CARTESIAN_POINT('Ctrl Pts',(101.857403622416,-3.93616191297999,
58.6404063003945));
#186752=CARTESIAN_POINT('Ctrl Pts',(101.310128925989,0.137236232267715,
58.4860098831306));
#186753=CARTESIAN_POINT('Ctrl Pts',(101.954022153609,4.19868555004701,58.5631542106142));
#186754=CARTESIAN_POINT('Ctrl Pts',(103.733804134502,7.89456545219501,58.8610940469303));
#186755=CARTESIAN_POINT('Ctrl Pts',(106.495296606141,10.90308459713,59.3498600241915));
#186756=CARTESIAN_POINT('Ctrl Pts',(109.998846143165,12.96229848513,59.982868003024));
#186757=CARTESIAN_POINT('Ctrl Pts',(113.940190203264,13.89291633382,60.7009750412564));
#186758=CARTESIAN_POINT('Ctrl Pts',(117.97694853005,13.61391149316,61.4376288266965));
#186759=CARTESIAN_POINT('Ctrl Pts',(121.758433383767,12.14957624252,62.1246622279085));
#186760=CARTESIAN_POINT('Ctrl Pts',(124.956183045448,9.62740671222201,62.6982284358081));
#186761=CARTESIAN_POINT('Ctrl Pts',(127.292560300925,6.26700213440002,63.104359973566));
#186762=CARTESIAN_POINT('Ctrl Pts',(128.564925213674,2.36094475154901,63.3036674311141));
#186763=CARTESIAN_POINT('Ctrl Pts',(128.66328009665,-1.75067417859599,63.2747693173408));
#186764=CARTESIAN_POINT('Ctrl Pts',(127.579840767871,-5.70986692940099,
63.0161525329957));
#186765=CARTESIAN_POINT('Ctrl Pts',(125.409736608484,-9.17191238110799,
62.5463084488705));
#186766=CARTESIAN_POINT('Ctrl Pts',(122.342644622221,-11.83539264088,61.9021067235759));
#186767=CARTESIAN_POINT('Ctrl Pts',(119.87860515966,-12.92403253729,61.3911326064781));
#186768=CARTESIAN_POINT('Ctrl Pts',(118.595402349439,-13.27293538064,61.125696515574));
#186769=CARTESIAN_POINT('Ctrl Pts',(119.306264638481,-12.63603893397,64.2128930868616));
#186770=CARTESIAN_POINT('Ctrl Pts',(118.084779649904,-13.11197862707,63.959453785075));
#186771=CARTESIAN_POINT('Ctrl Pts',(115.502617252005,-13.69165693723,63.4255187807093));
#186772=CARTESIAN_POINT('Ctrl Pts',(111.549126755281,-13.3691312854,62.6090177791154));
#186773=CARTESIAN_POINT('Ctrl Pts',(107.860577282853,-11.8825725314,61.8440163527233));
#186774=CARTESIAN_POINT('Ctrl Pts',(104.758855691358,-9.36143091994799,
61.1930832804673));
#186775=CARTESIAN_POINT('Ctrl Pts',(102.514817660809,-6.02521103080599,
60.7088678358931));
#186776=CARTESIAN_POINT('Ctrl Pts',(101.324625684322,-2.16439085221699,
60.4295003353339));
#186777=CARTESIAN_POINT('Ctrl Pts',(101.292690910985,1.88487769115301,60.3752763515067));
#186778=CARTESIAN_POINT('Ctrl Pts',(102.422576628608,5.77003446298902,60.546888520854));
#186779=CARTESIAN_POINT('Ctrl Pts',(104.616689541549,9.15280826802001,60.9253665337324));
#186780=CARTESIAN_POINT('Ctrl Pts',(107.684776574895,11.73866914963,61.4737287540785));
#186781=CARTESIAN_POINT('Ctrl Pts',(111.36048985989,13.30247244478,62.1402021424649));
#186782=CARTESIAN_POINT('Ctrl Pts',(115.324576970593,13.7080615749,62.8627300039652));
#186783=CARTESIAN_POINT('Ctrl Pts',(119.232677469826,12.92012287364,63.574375116313));
#186784=CARTESIAN_POINT('Ctrl Pts',(122.745305539082,11.00726026166,64.2091477918536));
#186785=CARTESIAN_POINT('Ctrl Pts',(125.557408189824,8.13602206913601,64.7077514404668));
#186786=CARTESIAN_POINT('Ctrl Pts',(127.424925490658,4.55640007460902,65.0227453804995));
#186787=CARTESIAN_POINT('Ctrl Pts',(128.186040276495,0.580063324285615,
65.1226753844131));
#186788=CARTESIAN_POINT('Ctrl Pts',(127.775267178477,-3.44677813946799,
64.9948123224437));
#186789=CARTESIAN_POINT('Ctrl Pts',(126.229154276958,-7.17351695080098,
64.6462604572009));
#186790=CARTESIAN_POINT('Ctrl Pts',(123.683100948408,-10.27567495739,64.1033388926787));
#186791=CARTESIAN_POINT('Ctrl Pts',(120.359568968502,-12.4831547499,63.4092900333947));
#186792=CARTESIAN_POINT('Ctrl Pts',(116.548713302336,-13.60375639144,62.620514572626));
#186793=CARTESIAN_POINT('Ctrl Pts',(112.583119012022,-13.5399118021,61.8016608201517));
#186794=CARTESIAN_POINT('Ctrl Pts',(108.808843878152,-12.29717977616,61.0199959300326));
#186795=CARTESIAN_POINT('Ctrl Pts',(105.555287984189,-9.98376199129099,
60.3395491118441));
#186796=CARTESIAN_POINT('Ctrl Pts',(103.106513646349,-6.80108214965099,
59.8155367619703));
#186797=CARTESIAN_POINT('Ctrl Pts',(101.676512793396,-3.02624850238099,
59.4895549052523));
#186798=CARTESIAN_POINT('Ctrl Pts',(101.39057520603,1.01207329692701,59.3859575295266));
#186799=CARTESIAN_POINT('Ctrl Pts',(102.274379838014,4.96227631731602,59.5097361426729));
#186800=CARTESIAN_POINT('Ctrl Pts',(104.251759011771,8.48042591720101,59.8460851740942));
#186801=CARTESIAN_POINT('Ctrl Pts',(107.151330154106,11.26020530339,60.3616910599886));
#186802=CARTESIAN_POINT('Ctrl Pts',(110.721417663228,13.05958579483,61.0076327749495));
#186803=CARTESIAN_POINT('Ctrl Pts',(114.651965695841,13.72189967566,61.7236412675494));
#186804=CARTESIAN_POINT('Ctrl Pts',(118.601533980985,13.18948087504,62.443346941166));
#186805=CARTESIAN_POINT('Ctrl Pts',(122.227026200225,11.50868581274,63.1000582945505));
#186806=CARTESIAN_POINT('Ctrl Pts',(125.2135625559,8.82585725755001,63.6325685898554));
#186807=CARTESIAN_POINT('Ctrl Pts',(127.301895595,5.37458261569201,63.9904849755484));
#186808=CARTESIAN_POINT('Ctrl Pts',(128.310982259146,1.45535603919601,64.1386160703609));
#186809=CARTESIAN_POINT('Ctrl Pts',(128.153746866589,-2.59058487454599,
64.0600359918914));
#186810=CARTESIAN_POINT('Ctrl Pts',(126.844662581706,-6.41096981667798,
63.7575580523452));
#186811=CARTESIAN_POINT('Ctrl Pts',(124.498491271469,-9.67316709231899,
63.2534898102216));
#186812=CARTESIAN_POINT('Ctrl Pts',(121.320291466714,-12.0931450593,62.5876908050552));
#186813=CARTESIAN_POINT('Ctrl Pts',(117.587564410871,-13.46020207762,61.8141020834892));
#186814=CARTESIAN_POINT('Ctrl Pts',(113.626092696544,-13.65531179265,60.9960496826084));
#186815=CARTESIAN_POINT('Ctrl Pts',(109.781575161582,-12.66148647246,60.2007309847145));
#186816=CARTESIAN_POINT('Ctrl Pts',(106.389527725756,-10.56525608868,59.4933640034673));
#186817=CARTESIAN_POINT('Ctrl Pts',(103.746070829524,-7.54913436075398,
58.9315090088654));
#186818=CARTESIAN_POINT('Ctrl Pts',(102.082146942077,-3.87572772689699,
58.56005689348));
#186819=CARTESIAN_POINT('Ctrl Pts',(101.543412958033,0.135129164517415,
58.4073206308037));
#186820=CARTESIAN_POINT('Ctrl Pts',(102.17755820323,4.13422068576602,58.482570132995));
#186821=CARTESIAN_POINT('Ctrl Pts',(103.930152240199,7.77335559150302,58.7752251419934));
#186822=CARTESIAN_POINT('Ctrl Pts',(106.649383995051,10.73568319001,59.255776427068));
#186823=CARTESIAN_POINT('Ctrl Pts',(110.099279581029,12.76328076801,59.8783550822648));
#186824=CARTESIAN_POINT('Ctrl Pts',(113.98024797582,13.67961029892,60.584726221445));
#186825=CARTESIAN_POINT('Ctrl Pts',(117.955165686495,13.40488918204,61.309359348822));
#186826=CARTESIAN_POINT('Ctrl Pts',(121.678729286384,11.96303672324,61.9851339426251));
#186827=CARTESIAN_POINT('Ctrl Pts',(124.827520120575,9.47959153049801,62.5491834710116));
#186828=CARTESIAN_POINT('Ctrl Pts',(127.128163700718,6.17078120106001,62.9483690512494));
#186829=CARTESIAN_POINT('Ctrl Pts',(128.381131339262,2.32469579186801,63.1439060418254));
#186830=CARTESIAN_POINT('Ctrl Pts',(128.478114207689,-1.72379505847099,
63.1147412341091));
#186831=CARTESIAN_POINT('Ctrl Pts',(127.4114476391,-5.62220001736299,62.8593847603446));
#186832=CARTESIAN_POINT('Ctrl Pts',(125.27480043787,-9.03109066914899,62.3960440825424));
#186833=CARTESIAN_POINT('Ctrl Pts',(122.254937386221,-11.65367696543,61.7610227779709));
#186834=CARTESIAN_POINT('Ctrl Pts',(119.828821813277,-12.72560233954,61.2574203550473));
#186835=CARTESIAN_POINT('Ctrl Pts',(118.565366791485,-13.06914827436,60.9958228645183));
#186836=CARTESIAN_POINT('Ctrl Pts',(119.255701008655,-12.43900529756,64.079029162937));
#186837=CARTESIAN_POINT('Ctrl Pts',(118.053309370171,-12.90752366749,63.8293012509647));
#186838=CARTESIAN_POINT('Ctrl Pts',(115.511504098567,-13.47816305921,63.3032109164311));
#186839=CARTESIAN_POINT('Ctrl Pts',(111.619800580443,-13.16066654684,62.4987201467721));
#186840=CARTESIAN_POINT('Ctrl Pts',(107.988906863712,-11.69728768953,61.7449259199226));
#186841=CARTESIAN_POINT('Ctrl Pts',(104.935690626277,-9.21545821554099,
61.1034213804345));
#186842=CARTESIAN_POINT('Ctrl Pts',(102.726784098077,-5.93125997179498,
60.6260348422253));
#186843=CARTESIAN_POINT('Ctrl Pts',(101.555291012315,-2.13064152598699,
60.350302055964));
#186844=CARTESIAN_POINT('Ctrl Pts',(101.523994436021,1.85548681101801,60.2962021256943));
#186845=CARTESIAN_POINT('Ctrl Pts',(102.636402094677,5.68006236980302,60.4644168875825));
#186846=CARTESIAN_POINT('Ctrl Pts',(104.796442463989,9.01008861466501,60.8362718358466));
#186847=CARTESIAN_POINT('Ctrl Pts',(107.816829083463,11.55562819184,61.3753619887283));
#186848=CARTESIAN_POINT('Ctrl Pts',(111.435367244147,13.09504711689,62.0307216033153));
#186849=CARTESIAN_POINT('Ctrl Pts',(115.337782620183,13.49431189952,62.741261634144));
#186850=CARTESIAN_POINT('Ctrl Pts',(119.185084383457,12.71865951902,63.4410886104253));
#186851=CARTESIAN_POINT('Ctrl Pts',(122.643080314639,10.83562415578,64.0652418210844));
#186852=CARTESIAN_POINT('Ctrl Pts',(125.41147411357,8.00915715343101,64.5553492871726));
#186853=CARTESIAN_POINT('Ctrl Pts',(127.250011473088,4.48535217104401,64.8647100691527));
#186854=CARTESIAN_POINT('Ctrl Pts',(127.999398441644,0.571018402320115,
64.9623604049417));
#186855=CARTESIAN_POINT('Ctrl Pts',(127.595170763105,-3.39303256031199,
64.8357696499831));
#186856=CARTESIAN_POINT('Ctrl Pts',(126.07330662396,-7.06166036836299,64.4919312901882));
#186857=CARTESIAN_POINT('Ctrl Pts',(123.567094119461,-10.11544645429,63.9567540360075));
#186858=CARTESIAN_POINT('Ctrl Pts',(120.295526180919,-12.28850503513,63.2728060135536));
#186859=CARTESIAN_POINT('Ctrl Pts',(116.544233389782,-13.3916331458,62.4956084606127));
#186860=CARTESIAN_POINT('Ctrl Pts',(112.640614812408,-13.32878408455,61.6888016264958));
#186861=CARTESIAN_POINT('Ctrl Pts',(108.925332153668,-12.10542996742,60.9186037691525));
#186862=CARTESIAN_POINT('Ctrl Pts',(105.722649164617,-9.82808528433599,
60.2480456912948));
#186863=CARTESIAN_POINT('Ctrl Pts',(103.312198780435,-6.69503293957399,
59.7314828005553));
#186864=CARTESIAN_POINT('Ctrl Pts',(101.904636155775,-2.97906023791099,
59.4098625153547));
#186865=CARTESIAN_POINT('Ctrl Pts',(101.623297428938,0.996292047509815,
59.3071590720213));
#186866=CARTESIAN_POINT('Ctrl Pts',(102.493461142014,4.88489958930502,59.4282861459017));
#186867=CARTESIAN_POINT('Ctrl Pts',(104.4401472993,8.34819071552401,59.7586690295201));
#186868=CARTESIAN_POINT('Ctrl Pts',(107.294645694468,11.08462502785,60.2655136171655));
#186869=CARTESIAN_POINT('Ctrl Pts',(110.80920510101,12.85594779619,60.9006617085182));
#186870=CARTESIAN_POINT('Ctrl Pts',(114.678604373486,13.5079342229,61.6047840269042));
#186871=CARTESIAN_POINT('Ctrl Pts',(118.566727315873,12.98381742364,62.312545876198));
#186872=CARTESIAN_POINT('Ctrl Pts',(122.13582750741,11.32923098296,62.9582956751037));
#186873=CARTESIAN_POINT('Ctrl Pts',(125.075935068154,8.68823574823501,63.4817810818708));
#186874=CARTESIAN_POINT('Ctrl Pts',(127.131844988214,5.29077679945202,63.8333950202108));
#186875=CARTESIAN_POINT('Ctrl Pts',(128.125337211901,1.43266268615201,63.9784948477393));
#186876=CARTESIAN_POINT('Ctrl Pts',(127.970693827763,-2.55018990892399,
63.9004186071819));
#186877=CARTESIAN_POINT('Ctrl Pts',(126.682162320262,-6.31100362453699,
63.6019357427932));
#186878=CARTESIAN_POINT('Ctrl Pts',(124.372715075645,-9.52233348869999,
63.1050059715203));
#186879=CARTESIAN_POINT('Ctrl Pts',(121.244213149014,-11.90457676197,62.4488673034646));
#186880=CARTESIAN_POINT('Ctrl Pts',(117.569830709511,-13.25031727305,61.6866196830542));
#186881=CARTESIAN_POINT('Ctrl Pts',(113.670270424834,-13.44238464412,60.8806017050628));
#186882=CARTESIAN_POINT('Ctrl Pts',(109.885840654102,-12.46405603282,60.0969629436411));
#186883=CARTESIAN_POINT('Ctrl Pts',(106.5468256205,-10.40051214973,59.3999044685746));
#186884=CARTESIAN_POINT('Ctrl Pts',(103.944728361231,-7.43142077957798,
58.8460890131106));
#186885=CARTESIAN_POINT('Ctrl Pts',(102.306890261749,-3.81529354086099,
58.4797074865576));
#186886=CARTESIAN_POINT('Ctrl Pts',(101.776696990086,0.133022096717915,
58.3286313784788));
#186887=CARTESIAN_POINT('Ctrl Pts',(102.401094252842,4.06975582143802,58.4019860553738));
#186888=CARTESIAN_POINT('Ctrl Pts',(104.126500345876,7.65214573077102,58.6893562370528));
#186889=CARTESIAN_POINT('Ctrl Pts',(106.803471383925,10.56828178286,59.1616928299374));
#186890=CARTESIAN_POINT('Ctrl Pts',(110.199713018851,12.56426305087,59.7738421614973));
#186891=CARTESIAN_POINT('Ctrl Pts',(114.020305748331,13.46630426402,60.468477401625));
#186892=CARTESIAN_POINT('Ctrl Pts',(117.933382842896,13.19586687093,61.1810898709391));
#186893=CARTESIAN_POINT('Ctrl Pts',(121.599025188964,11.77649720398,61.8456056573345));
#186894=CARTESIAN_POINT('Ctrl Pts',(124.698857195672,9.33177634880501,62.4001385062092));
#186895=CARTESIAN_POINT('Ctrl Pts',(126.963767100501,6.07456026775601,62.7923781289308));
#186896=CARTESIAN_POINT('Ctrl Pts',(128.197337464837,2.28844683222602,62.9841446525445));
#186897=CARTESIAN_POINT('Ctrl Pts',(128.292948318726,-1.69691593830999,
62.9547131508873));
#186898=CARTESIAN_POINT('Ctrl Pts',(127.243054510346,-5.53453310529599,
62.7026169877071));
#186899=CARTESIAN_POINT('Ctrl Pts',(125.139864267274,-8.89026895716699,
62.2457797162281));
#186900=CARTESIAN_POINT('Ctrl Pts',(122.167230150241,-11.47196128996,61.61993883238));
#186901=CARTESIAN_POINT('Ctrl Pts',(119.779038466918,-12.52717214178,61.1237081036312));
#186902=CARTESIAN_POINT('Ctrl Pts',(118.535331233552,-12.86536116807,60.8659492134769));
#186903=CARTESIAN_POINT('',(114.54332401699,-13.8999637388745,63.4488532896085));
#186904=CARTESIAN_POINT('Origin',(114.28108174878,1.45439216225896E-14,
64.7979697995068));
#186905=CARTESIAN_POINT('Ctrl Pts',(125.314806796842,-7.34586304067299,
66.2271012509232));
#186906=CARTESIAN_POINT('Ctrl Pts',(124.206005057303,-9.06047151994499,
65.9865345966579));
#186907=CARTESIAN_POINT('Ctrl Pts',(121.195667841809,-11.9531828368,65.351308690418));
#186908=CARTESIAN_POINT('Ctrl Pts',(115.253048553756,-13.77380876573,64.1210656902771));
#186909=CARTESIAN_POINT('Ctrl Pts',(109.139940975145,-12.69068481913,62.8576829581376));
#186910=CARTESIAN_POINT('Ctrl Pts',(104.147645605334,-8.93253702461299,
61.8121651368307));
#186911=CARTESIAN_POINT('Ctrl Pts',(101.331541571415,-3.29144748217499,
61.1896581710675));
#186912=CARTESIAN_POINT('Ctrl Pts',(101.288190926181,3.04345072980601,61.1061225557624));
#186913=CARTESIAN_POINT('Ctrl Pts',(104.029702302623,8.73681175115401,61.5639119824844));
#186914=CARTESIAN_POINT('Ctrl Pts',(108.981147777474,12.58851139971,62.4512712260906));
#186915=CARTESIAN_POINT('Ctrl Pts',(115.101761761745,13.78663799238,63.5658949400986));
#186916=CARTESIAN_POINT('Ctrl Pts',(121.104326210735,12.07863428537,64.6575720344359));
#186917=CARTESIAN_POINT('Ctrl Pts',(125.72650412153,7.82453632784801,65.4809278277585));
#186918=CARTESIAN_POINT('Ctrl Pts',(127.996946293465,1.92107788542301,65.8471502199406));
#186919=CARTESIAN_POINT('Ctrl Pts',(127.439989976586,-4.38732683985899,
65.6637792772028));
#186920=CARTESIAN_POINT('Ctrl Pts',(124.176131537949,-9.77092748121999,
64.954237237506));
#186921=CARTESIAN_POINT('Ctrl Pts',(118.895857162348,-13.09482740292,63.8527416886753));
#186922=CARTESIAN_POINT('Ctrl Pts',(114.77659556862,-13.47069719745,63.0019616433146));
#186923=CARTESIAN_POINT('Ctrl Pts',(112.783656420258,-13.17864608329,62.5895352285786));
#186924=CARTESIAN_POINT('Ctrl Pts',(125.510689982049,-7.46222138870299,
66.141141974147));
#186925=CARTESIAN_POINT('Ctrl Pts',(124.384250561224,-9.20398923768399,
65.8971468848321));
#186926=CARTESIAN_POINT('Ctrl Pts',(121.326081093995,-12.14252105354,65.2526232843154));
#186927=CARTESIAN_POINT('Ctrl Pts',(115.289107974865,-13.99198566682,64.0040396657971));
#186928=CARTESIAN_POINT('Ctrl Pts',(109.078946033499,-12.89170505496,62.7217913824783));
#186929=CARTESIAN_POINT('Ctrl Pts',(104.007349947628,-9.07402826206999,
61.660858986546));
#186930=CARTESIAN_POINT('Ctrl Pts',(101.146416032104,-3.34358395537999,
61.0296379310526));
#186931=CARTESIAN_POINT('Ctrl Pts',(101.102155872688,3.09165893860202,60.9459255232173));
#186932=CARTESIAN_POINT('Ctrl Pts',(103.886869902922,8.87520270355401,61.4121127370459));
#186933=CARTESIAN_POINT('Ctrl Pts',(108.91652335081,12.78791321029,62.3146741464906));
#186934=CARTESIAN_POINT('Ctrl Pts',(115.133864917805,14.0050181082,63.4480998917577));
#186935=CARTESIAN_POINT('Ctrl Pts',(121.231287046849,12.26995965095,64.5582155432809));
#186936=CARTESIAN_POINT('Ctrl Pts',(125.926457337962,7.94847685275301,65.3957596888578));
#186937=CARTESIAN_POINT('Ctrl Pts',(128.232640435342,1.95150772707801,65.768929447846));
#186938=CARTESIAN_POINT('Ctrl Pts',(127.666639098998,-4.45682202381698,
65.5838003226546));
#186939=CARTESIAN_POINT('Ctrl Pts',(124.350858356457,-9.92569880953099,
64.8641655591087));
#186940=CARTESIAN_POINT('Ctrl Pts',(118.986721682142,-13.30224925054,63.7463687493917));
#186941=CARTESIAN_POINT('Ctrl Pts',(114.802062493028,-13.68407281635,62.8828766357867));
#186942=CARTESIAN_POINT('Ctrl Pts',(112.777480941574,-13.38739561741,62.4642995302622));
#186943=CARTESIAN_POINT('Ctrl Pts',(125.706573167286,-7.57857973669199,
66.0551826973766));
#186944=CARTESIAN_POINT('Ctrl Pts',(124.562496065176,-9.34750695538599,
65.8077591730122));
#186945=CARTESIAN_POINT('Ctrl Pts',(121.456494346225,-12.33185927026,65.1539378782213));
#186946=CARTESIAN_POINT('Ctrl Pts',(115.325167396024,-14.21016256789,63.8870136413267));
#186947=CARTESIAN_POINT('Ctrl Pts',(109.017951091899,-13.09272529082,62.5858998068277));
#186948=CARTESIAN_POINT('Ctrl Pts',(103.86705428995,-9.21551949956499,61.5095528362669));
#186949=CARTESIAN_POINT('Ctrl Pts',(100.961290492803,-3.39572042863199,
60.8696176910395));
#186950=CARTESIAN_POINT('Ctrl Pts',(100.916120819196,3.13986714735501,60.7857284906722));
#186951=CARTESIAN_POINT('Ctrl Pts',(103.744037503191,9.01359365592001,61.2603134916017));
#186952=CARTESIAN_POINT('Ctrl Pts',(108.851898924109,12.98731502086,62.1780770668837));
#186953=CARTESIAN_POINT('Ctrl Pts',(115.165968073829,14.22339822402,63.3303048434097));
#186954=CARTESIAN_POINT('Ctrl Pts',(121.358247882935,12.46128501656,64.4588590521206));
#186955=CARTESIAN_POINT('Ctrl Pts',(126.126410554373,8.07241737768201,65.3105915499533));
#186956=CARTESIAN_POINT('Ctrl Pts',(128.468334577209,1.98193756875801,65.6907086757495));
#186957=CARTESIAN_POINT('Ctrl Pts',(127.893288221429,-4.52631720775899,
65.5038213681102));
#186958=CARTESIAN_POINT('Ctrl Pts',(124.525585174978,-10.08047013783,64.7740938807138));
#186959=CARTESIAN_POINT('Ctrl Pts',(119.077586201943,-13.50967109816,63.6399958100993));
#186960=CARTESIAN_POINT('Ctrl Pts',(114.827529417439,-13.89744843525,62.763791628249));
#186961=CARTESIAN_POINT('Ctrl Pts',(112.771305462889,-13.59614515153,62.3390638319355));
#186962=CARTESIAN_POINT('Ctrl Pts',(125.902456352492,-7.69493808472198,
65.9692234206102));
#186963=CARTESIAN_POINT('Ctrl Pts',(124.740741569096,-9.49102467312499,
65.7183714611964));
#186964=CARTESIAN_POINT('Ctrl Pts',(121.58690759841,-12.521197487,65.0552524721285));
#186965=CARTESIAN_POINT('Ctrl Pts',(115.361226817132,-14.42833946898,63.7699876168566));
#186966=CARTESIAN_POINT('Ctrl Pts',(108.956956150252,-13.29374552665,62.4500082311784));
#186967=CARTESIAN_POINT('Ctrl Pts',(103.726758632241,-9.35701073702199,
61.358246685992));
#186968=CARTESIAN_POINT('Ctrl Pts',(100.776164953491,-3.44785690183699,
60.7095974510343));
#186969=CARTESIAN_POINT('Ctrl Pts',(100.730085765701,3.18807535615101,60.6255314581369));
#186970=CARTESIAN_POINT('Ctrl Pts',(103.601205103488,9.15198460832001,61.108514246173));
#186971=CARTESIAN_POINT('Ctrl Pts',(108.787274497443,13.18671683143,62.0414799872937));
#186972=CARTESIAN_POINT('Ctrl Pts',(115.198071229887,14.44177833984,63.2125097950786));
#186973=CARTESIAN_POINT('Ctrl Pts',(121.485208719049,12.65261038215,64.3595025609656));
#186974=CARTESIAN_POINT('Ctrl Pts',(126.326363770805,8.19635790258801,65.2254234110526));
#186975=CARTESIAN_POINT('Ctrl Pts',(128.704028719076,2.01236741041301,65.612487903653));
#186976=CARTESIAN_POINT('Ctrl Pts',(128.11993734384,-4.59581239171698,65.4238424135619));
#186977=CARTESIAN_POINT('Ctrl Pts',(124.700311993483,-10.23524146614,64.6840222023159));
#186978=CARTESIAN_POINT('Ctrl Pts',(119.16845072174,-13.71709294579,63.533622870806));
#186979=CARTESIAN_POINT('Ctrl Pts',(114.85299634185,-14.11082405414,62.6447066207113));
#186980=CARTESIAN_POINT('Ctrl Pts',(112.765129984206,-13.80489468565,62.2138281336091));
#186981=CARTESIAN_POINT('Ctrl Pts',(122.863511281691,-10.228475512234,65.6767278482884));
#186982=CARTESIAN_POINT('Ctrl Pts',(123.110780037318,-10.0253785434155,
65.7247922653008));
#186983=CARTESIAN_POINT('Ctrl Pts',(123.350863821086,-9.81319073816203,
65.7714600582926));
#186984=CARTESIAN_POINT('Ctrl Pts',(123.815499473612,-9.37175300744527,
65.8617765307689));
#186985=CARTESIAN_POINT('Ctrl Pts',(124.040059565785,-9.14248705860146,
65.9054268087314));
#186986=CARTESIAN_POINT('Ctrl Pts',(124.256220060446,-8.90528662689628,
65.9474443621852));
#186987=CARTESIAN_POINT('Ctrl Pts',(108.487103650414,-12.59742940801,63.245643627947));
#186988=CARTESIAN_POINT('Ctrl Pts',(106.956911188634,-11.85516766911,62.9280906814806));
#186989=CARTESIAN_POINT('Ctrl Pts',(104.171395799652,-9.78264817709099,
62.3464142802986));
#186990=CARTESIAN_POINT('Ctrl Pts',(101.389134172046,-5.33442980417999,
61.7452581710137));
#186991=CARTESIAN_POINT('Ctrl Pts',(100.385889140724,-0.155999799768285,
61.4899095833419));
#186992=CARTESIAN_POINT('Ctrl Pts',(101.300395977681,5.04380189940801,61.6073360569171));
#186993=CARTESIAN_POINT('Ctrl Pts',(104.00904923499,9.55311537764301,62.0735110066611));
#186994=CARTESIAN_POINT('Ctrl Pts',(108.142577067656,12.75463210302,62.8166548989901));
#186995=CARTESIAN_POINT('Ctrl Pts',(113.136659801733,14.21007092034,63.7270745538334));
#186996=CARTESIAN_POINT('Ctrl Pts',(118.309166198777,13.72018623447,64.6721764285147));
#186997=CARTESIAN_POINT('Ctrl Pts',(122.953540186654,11.35204195259,65.5146192499319));
#186998=CARTESIAN_POINT('Ctrl Pts',(126.435525741389,7.42983117316102,66.1311155208569));
#186999=CARTESIAN_POINT('Ctrl Pts',(128.279993910017,2.49049495110001,66.4293090676415));
#187000=CARTESIAN_POINT('Ctrl Pts',(128.235991923602,-2.78978417332599,
66.3604193700536));
#187001=CARTESIAN_POINT('Ctrl Pts',(126.31107853456,-7.68814761989499,65.925915708057));
#187002=CARTESIAN_POINT('Ctrl Pts',(122.770362013952,-11.53402684478,65.1773301664936));
#187003=CARTESIAN_POINT('Ctrl Pts',(118.099935873545,-13.80091069517,64.2091502239663));
#187004=CARTESIAN_POINT('Ctrl Pts',(114.660876983065,-14.05266506285,63.5004372009833));
#187005=CARTESIAN_POINT('Ctrl Pts',(112.977552505738,-13.85500477741,63.1531182574564));
#187006=CARTESIAN_POINT('Ctrl Pts',(108.599155925917,-12.4069384568,63.1433891917103));
#187007=CARTESIAN_POINT('Ctrl Pts',(107.092159102354,-11.67590076529,62.8303450430814));
#187008=CARTESIAN_POINT('Ctrl Pts',(104.348878573649,-9.63472069949199,
62.2568783080545));
#187009=CARTESIAN_POINT('Ctrl Pts',(101.608859568653,-5.25376568020898,
61.663933373787));
#187010=CARTESIAN_POINT('Ctrl Pts',(100.620955912659,-0.153640862146685,
61.4115668622755));
#187011=CARTESIAN_POINT('Ctrl Pts',(101.521805004111,4.96753248042701,61.526338525809));
#187012=CARTESIAN_POINT('Ctrl Pts',(104.189670484291,9.40865876062801,61.9845850952611));
#187013=CARTESIAN_POINT('Ctrl Pts',(108.260864420817,12.5617640247,62.715612445124));
#187014=CARTESIAN_POINT('Ctrl Pts',(113.179600451426,13.99519454845,63.6113861113676));
#187015=CARTESIAN_POINT('Ctrl Pts',(118.274062126846,13.51271761195,64.5413175532287));
#187016=CARTESIAN_POINT('Ctrl Pts',(122.848377502147,11.18038302126,65.3701422919282));
#187017=CARTESIAN_POINT('Ctrl Pts',(126.277881401572,7.31748161662602,65.9764371115622));
#187018=CARTESIAN_POINT('Ctrl Pts',(128.094629493962,2.45283514473701,66.2692423944695));
#187019=CARTESIAN_POINT('Ctrl Pts',(128.051463771229,-2.74759869058399,
66.2005152508861));
#187020=CARTESIAN_POINT('Ctrl Pts',(126.155828686743,-7.57189195330198,
65.7717027431803));
#187021=CARTESIAN_POINT('Ctrl Pts',(122.668823699534,-11.35961604446,65.0335577181838));
#187022=CARTESIAN_POINT('Ctrl Pts',(118.069191899904,-13.59222140462,64.0791388701734));
#187023=CARTESIAN_POINT('Ctrl Pts',(114.682250371862,-13.84016889016,63.380556486757));
#187024=CARTESIAN_POINT('Ctrl Pts',(113.024437105427,-13.64549750782,63.0381964450459));
#187025=CARTESIAN_POINT('Ctrl Pts',(108.711208201378,-12.21644750558,63.0411347554654));
#187026=CARTESIAN_POINT('Ctrl Pts',(107.227407016037,-11.49663386145,62.7325994046647));
#187027=CARTESIAN_POINT('Ctrl Pts',(104.526361347626,-9.48679322185798,
62.1673423358065));
#187028=CARTESIAN_POINT('Ctrl Pts',(101.82858496525,-5.17310155619299,61.5826085765585));
#187029=CARTESIAN_POINT('Ctrl Pts',(100.856022684594,-0.151281924479185,
61.3332241412091));
#187030=CARTESIAN_POINT('Ctrl Pts',(101.74321403056,4.89126306148702,61.4453409947047));
#187031=CARTESIAN_POINT('Ctrl Pts',(104.370291733622,9.26420214364402,61.8956591838669));
#187032=CARTESIAN_POINT('Ctrl Pts',(108.379151774013,12.3688959464,62.6145699912648));
#187033=CARTESIAN_POINT('Ctrl Pts',(113.222541101156,13.78031817656,63.4956976689091));
#187034=CARTESIAN_POINT('Ctrl Pts',(118.238958054948,13.30524898942,64.4104586779493));
#187035=CARTESIAN_POINT('Ctrl Pts',(122.743214817667,11.00872408991,65.2256653339196));
#187036=CARTESIAN_POINT('Ctrl Pts',(126.120237061767,7.20513206006702,65.8217587022596));
#187037=CARTESIAN_POINT('Ctrl Pts',(127.909265077919,2.41517533835002,66.1091757212896));
#187038=CARTESIAN_POINT('Ctrl Pts',(127.866935618859,-2.70541320786099,
66.0406111317087));
#187039=CARTESIAN_POINT('Ctrl Pts',(126.000578838919,-7.45563628672199,
65.6174897782919));
#187040=CARTESIAN_POINT('Ctrl Pts',(122.56728538511,-11.18520524415,64.8897852698628));
#187041=CARTESIAN_POINT('Ctrl Pts',(118.03844792626,-13.38353211408,63.9491275163697));
#187042=CARTESIAN_POINT('Ctrl Pts',(114.70362376066,-13.62767271748,63.2606757725306));
#187043=CARTESIAN_POINT('Ctrl Pts',(113.07132170512,-13.43599023824,62.923274632626));
#187044=CARTESIAN_POINT('Ctrl Pts',(108.82326047688,-12.02595655437,62.9388803192384));
#187045=CARTESIAN_POINT('Ctrl Pts',(107.36265492976,-11.31736695764,62.6348537662557));
#187046=CARTESIAN_POINT('Ctrl Pts',(104.703844121629,-9.33886574425999,
62.0778063635736));
#187047=CARTESIAN_POINT('Ctrl Pts',(102.048310361865,-5.09243743222199,
61.5012837793436));
#187048=CARTESIAN_POINT('Ctrl Pts',(101.091089456537,-0.148922986857685,
61.2548814201544));
#187049=CARTESIAN_POINT('Ctrl Pts',(101.964623056987,4.81499364250501,61.3643434636064));
#187050=CARTESIAN_POINT('Ctrl Pts',(104.550912982913,9.11974552662901,61.806733272465));
#187051=CARTESIAN_POINT('Ctrl Pts',(108.497439127174,12.17602786808,62.5135275373988));
#187052=CARTESIAN_POINT('Ctrl Pts',(113.26548175085,13.56544180466,63.3800092264433));
#187053=CARTESIAN_POINT('Ctrl Pts',(118.203853983017,13.0977803669,64.2795998026635));
#187054=CARTESIAN_POINT('Ctrl Pts',(122.638052133161,10.83706515858,65.081188375906));
#187055=CARTESIAN_POINT('Ctrl Pts',(125.962592721952,7.09278250353201,65.6670802929552));
#187056=CARTESIAN_POINT('Ctrl Pts',(127.723900661866,2.37751553198702,65.9491090481079));
#187057=CARTESIAN_POINT('Ctrl Pts',(127.682407466479,-2.66322772511999,
65.8807070125294));
#187058=CARTESIAN_POINT('Ctrl Pts',(125.845328991104,-7.33938062012898,
65.4632768134054));
#187059=CARTESIAN_POINT('Ctrl Pts',(122.465747070694,-11.01079444384,64.7460128215434));
#187060=CARTESIAN_POINT('Ctrl Pts',(118.007703952621,-13.17484282353,63.819116162567));
#187061=CARTESIAN_POINT('Ctrl Pts',(114.724997149458,-13.41517654479,63.1407950583042));
#187062=CARTESIAN_POINT('Ctrl Pts',(113.118206304812,-13.22648296865,62.8083528202057));
#187063=CARTESIAN_POINT('',(105.924484859737,-10.2222654049121,62.3840982248477));
#187064=CARTESIAN_POINT('Ctrl Pts',(105.924635027038,-10.2220806761209,
62.3841274145597));
#187065=CARTESIAN_POINT('Ctrl Pts',(106.171216296684,-10.4260967714227,
62.4320581971677));
#187066=CARTESIAN_POINT('Ctrl Pts',(106.425035137045,-10.6210421244567,
62.4813958280292));
#187067=CARTESIAN_POINT('Ctrl Pts',(106.941125769492,-10.9884663950073,
62.5817141853213));
#187068=CARTESIAN_POINT('Ctrl Pts',(107.203172821437,-11.1612912792639,
62.6326512264755));
#187069=CARTESIAN_POINT('Ctrl Pts',(107.470912577424,-11.3244123346074,
62.6846948227235));
#187070=CARTESIAN_POINT('Ctrl Pts',(105.924385870765,-10.2223568854093,
62.3842011440511));
#187071=CARTESIAN_POINT('Ctrl Pts',(105.918649582816,-10.2174500398891,
62.3830453968698));
#187072=CARTESIAN_POINT('Ctrl Pts',(105.91291738673,-10.2125381703083,62.3818904450698));
#187073=CARTESIAN_POINT('Ctrl Pts',(105.907189290968,-10.2076212837564,
62.3807362902962));
#187074=CARTESIAN_POINT('Origin',(114.428959431277,1.45439216225896E-14,
64.0372088705551));
#187075=CARTESIAN_POINT('Origin',(114.772417274494,1.45439216225896E-14,
62.2702802613769));
#187076=CARTESIAN_POINT('Origin',(117.386513081203,1.45439216225896E-14,
48.8219902915203));
#187077=CARTESIAN_POINT('Origin',(105.886046742854,0.700000000000015,61.8672681344988));
#187078=CARTESIAN_POINT('',(105.826348707759,0.200000000000015,62.1743863680917));
#187079=CARTESIAN_POINT('',(105.829634839229,0.700000000000015,62.1574807716032));
#187080=CARTESIAN_POINT('Origin',(108.32086073557,1.45439216225896E-14,
49.3412985381828));
#187081=CARTESIAN_POINT('',(105.886046742854,0.200000000000015,61.8672681344988));
#187082=CARTESIAN_POINT('',(105.886046742854,0.200000000000015,61.8672681344988));
#187083=CARTESIAN_POINT('',(105.886046742854,0.700000000000015,61.8672681344988));
#187084=CARTESIAN_POINT('',(105.886046742854,0.700000000000015,61.8672681344988));
#187085=CARTESIAN_POINT('',(105.886046742854,0.700000000000015,61.8672681344988));
#187086=CARTESIAN_POINT('Origin',(106.376860245404,0.700000000000015,61.962673090948));
#187087=CARTESIAN_POINT('',(105.983292743205,0.700000000000015,61.8861709364391));
#187088=CARTESIAN_POINT('',(105.983292743205,0.700000000000015,61.8861709364391));
#187089=CARTESIAN_POINT('',(106.326420107966,0.700000000000015,62.2221638076415));
#187090=CARTESIAN_POINT('Origin',(116.959178380441,0.700000000000015,51.0204257716897));
#187091=CARTESIAN_POINT('',(106.258735053168,0.700000000000015,62.570371490472));
#187092=CARTESIAN_POINT('',(106.326420107966,0.700000000000015,62.2221638076415));
#187093=CARTESIAN_POINT('Origin',(116.959178380441,0.700000000000015,51.0204257716897));
#187094=CARTESIAN_POINT('Origin',(106.376860245404,0.200000000000015,61.962673090948));
#187095=CARTESIAN_POINT('',(106.25552825787,0.200000000000015,62.5868689397725));
#187096=CARTESIAN_POINT('Origin',(108.811674238119,1.45439216225896E-14,
49.4367034946321));
#187097=CARTESIAN_POINT('',(106.323126090759,0.200000000000015,62.2391099725262));
#187098=CARTESIAN_POINT('Origin',(108.811674238119,1.45439216225896E-14,
49.4367034946321));
#187099=CARTESIAN_POINT('',(106.323126090759,0.200000000000015,62.2391099725262));
#187100=CARTESIAN_POINT('Origin',(105.886046742854,0.200000000000015,61.8672681344988));
#187101=CARTESIAN_POINT('Origin',(116.959178380441,0.200000000000015,51.0204257716897));
#187102=CARTESIAN_POINT('',(105.957946172011,0.200000000000015,61.8812440375083));
#187103=CARTESIAN_POINT('Origin',(116.959178380441,0.200000000000015,51.0204257716897));
#187104=CARTESIAN_POINT('',(105.886046742854,0.200000000000015,61.8672681344988));
#187105=CARTESIAN_POINT('Origin',(105.689721341835,1.45439216225896E-14,
61.8291061519191));
#187106=CARTESIAN_POINT('Origin',(114.524364387726,1.45439216225896E-14,
63.5463953680056));
#187107=CARTESIAN_POINT('Origin',(105.886046742854,1.7,61.8672681344988));
#187108=CARTESIAN_POINT('',(105.836586502542,1.2,62.121717742656));
#187109=CARTESIAN_POINT('',(105.847234601382,1.7,62.0669382963709));
#187110=CARTESIAN_POINT('Origin',(108.32086073557,1.45439216225896E-14,
49.3412985381828));
#187111=CARTESIAN_POINT('',(105.886046742854,1.2,61.8672681344988));
#187112=CARTESIAN_POINT('',(105.886046742854,1.2,61.8672681344988));
#187113=CARTESIAN_POINT('',(105.886046742854,1.7,61.8672681344988));
#187114=CARTESIAN_POINT('',(105.886046742854,1.7,61.8672681344988));
#187115=CARTESIAN_POINT('',(105.886046742854,1.7,61.8672681344988));
#187116=CARTESIAN_POINT('Origin',(106.376860245404,1.7,61.962673090948));
#187117=CARTESIAN_POINT('',(106.119765346029,1.7,61.9126986555448));
#187118=CARTESIAN_POINT('',(106.344062462215,1.7,62.1314022161617));
#187119=CARTESIAN_POINT('Origin',(116.959178380441,1.7,51.0204257716897));
#187120=CARTESIAN_POINT('',(106.27590645159,1.7,62.4820327445918));
#187121=CARTESIAN_POINT('',(106.344062462215,1.7,62.1314022161617));
#187122=CARTESIAN_POINT('Origin',(116.959178380441,1.7,51.0204257716897));
#187123=CARTESIAN_POINT('',(106.119765346029,1.7,61.9126986555448));
#187124=CARTESIAN_POINT('Origin',(106.376860245404,1.2,61.962673090948));
#187125=CARTESIAN_POINT('',(106.265518217696,1.2,62.5354753082978));
#187126=CARTESIAN_POINT('Origin',(108.811674238119,1.45439216225896E-14,
49.4367034946321));
#187127=CARTESIAN_POINT('',(106.333388522201,1.2,62.1863146031025));
#187128=CARTESIAN_POINT('Origin',(108.811674238119,1.45439216225896E-14,
49.4367034946321));
#187129=CARTESIAN_POINT('',(106.333388522201,1.2,62.1863146031025));
#187130=CARTESIAN_POINT('Origin',(105.886046742854,1.2,61.8672681344988));
#187131=CARTESIAN_POINT('Origin',(116.959178380441,1.2,51.0204257716897));
#187132=CARTESIAN_POINT('',(106.037050746853,1.2,61.8966204859526));
#187133=CARTESIAN_POINT('Origin',(116.959178380441,1.2,51.0204257716897));
#187134=CARTESIAN_POINT('',(105.886046742854,1.2,61.8672681344988));
#187135=CARTESIAN_POINT('Origin',(105.689721341835,1.,61.8291061519191));
#187136=CARTESIAN_POINT('Origin',(114.524364387726,1.45439216225896E-14,
63.5463953680056));
#187137=CARTESIAN_POINT('Origin',(106.376860245404,2.2,61.962673090948));
#187138=CARTESIAN_POINT('',(106.376375477714,2.70027257384477,61.9628795173321));
#187139=CARTESIAN_POINT('',(106.307693166583,2.7,62.3185050883679));
#187140=CARTESIAN_POINT('',(106.376860245404,2.7,61.962673090948));
#187141=CARTESIAN_POINT('',(106.35849029638,2.2,62.0571778143663));
#187142=CARTESIAN_POINT('Origin',(108.811674238119,1.45439216225896E-14,
49.4367034946321));
#187143=CARTESIAN_POINT('',(106.289944307572,2.2,62.4098145966144));
#187144=CARTESIAN_POINT('',(106.35849029638,2.2,62.0571778143663));
#187145=CARTESIAN_POINT('Origin',(108.811674238119,1.45439216225896E-14,
49.4367034946321));
#187146=CARTESIAN_POINT('Origin',(106.376860245404,2.7,61.962673090948));
#187147=CARTESIAN_POINT('',(105.886046742854,2.7,61.8672681344988));
#187148=CARTESIAN_POINT('',(105.879830381159,2.7,61.8992483834357));
#187149=CARTESIAN_POINT('',(105.886046742854,2.7,61.8672681344988));
#187150=CARTESIAN_POINT('',(105.689721341835,2.7,61.8291061519191));
#187151=CARTESIAN_POINT('Origin',(116.959178380441,2.7,51.0204257716897));
#187152=CARTESIAN_POINT('Origin',(105.886046742854,2.7,61.8672681344988));
#187153=CARTESIAN_POINT('',(105.886046742854,2.2,61.8672681344988));
#187154=CARTESIAN_POINT('',(105.861627150251,2.2,61.9928954207813));
#187155=CARTESIAN_POINT('',(105.886046742854,2.2,61.8672681344988));
#187156=CARTESIAN_POINT('',(105.886046742854,2.7,61.8672681344988));
#187157=CARTESIAN_POINT('Origin',(108.32086073557,1.45439216225896E-14,
49.3412985381828));
#187158=CARTESIAN_POINT('Origin',(105.886046742854,2.2,61.8672681344988));
#187159=CARTESIAN_POINT('',(106.232303035066,2.2,61.9345738754923));
#187160=CARTESIAN_POINT('Origin',(116.959178380441,2.2,51.0204257716897));
#187161=CARTESIAN_POINT('',(105.886046742854,2.2,61.8672681344988));
#187162=CARTESIAN_POINT('Origin',(116.959178380441,2.2,51.0204257716897));
#187163=CARTESIAN_POINT('Origin',(105.689721341835,2.,61.8291061519191));
#187164=CARTESIAN_POINT('Origin',(114.524364387726,1.45439216225896E-14,
63.5463953680056));
#187165=CARTESIAN_POINT('Origin',(106.867673747954,0.200000000000015,62.0580780473973));
#187166=CARTESIAN_POINT('',(107.193139079362,0.200000000000015,63.0041213568046));
#187167=CARTESIAN_POINT('',(107.12837091224,0.200000000000015,63.3373230283091));
#187168=CARTESIAN_POINT('',(107.193139079362,0.200000000000015,63.0041213568046));
#187169=CARTESIAN_POINT('',(106.755733004587,0.200000000000015,62.6339603744237));
#187170=CARTESIAN_POINT('Origin',(116.959178380441,0.200000000000015,51.0204257716897));
#187171=CARTESIAN_POINT('',(106.689640619927,0.200000000000015,62.9739745205872));
#187172=CARTESIAN_POINT('',(106.755733004587,0.200000000000015,62.6339603744237));
#187173=CARTESIAN_POINT('Origin',(116.959178380441,0.200000000000015,51.0204257716897));
#187174=CARTESIAN_POINT('Origin',(107.358487250503,0.200000000000015,62.1534830038465));
#187175=CARTESIAN_POINT('',(107.196291522778,0.700000000000015,62.9879035222976));
#187176=CARTESIAN_POINT('',(107.13144664939,0.700000000000015,63.3214998113625));
#187177=CARTESIAN_POINT('',(107.196291522778,0.700000000000015,62.9879035222976));
#187178=CARTESIAN_POINT('Origin',(109.793301243218,1.45439216225896E-14,
49.6275134075306));
#187179=CARTESIAN_POINT('Origin',(109.793301243218,1.45439216225896E-14,
49.6275134075306));
#187180=CARTESIAN_POINT('Origin',(107.358487250503,0.700000000000015,62.1534830038465));
#187181=CARTESIAN_POINT('',(106.758951639987,0.700000000000015,62.617402013381));
#187182=CARTESIAN_POINT('',(106.692777740288,0.700000000000015,62.9578355159706));
#187183=CARTESIAN_POINT('',(106.758951639987,0.700000000000015,62.617402013381));
#187184=CARTESIAN_POINT('Origin',(116.959178380441,0.700000000000015,51.0204257716897));
#187185=CARTESIAN_POINT('Origin',(116.959178380441,0.700000000000015,51.0204257716897));
#187186=CARTESIAN_POINT('Origin',(106.867673747954,0.700000000000015,62.0580780473973));
#187187=CARTESIAN_POINT('Origin',(109.302487740669,1.45439216225896E-14,
49.5321084510813));
#187188=CARTESIAN_POINT('Origin',(109.302487740669,1.45439216225896E-14,
49.5321084510813));
#187189=CARTESIAN_POINT('Origin',(106.867673747954,1.2,62.0580780473973));
#187190=CARTESIAN_POINT('',(107.202959280012,1.2,62.9536010562203));
#187191=CARTESIAN_POINT('',(107.1379515719,1.2,63.2880350531379));
#187192=CARTESIAN_POINT('',(107.202959280012,1.2,62.9536010562203));
#187193=CARTESIAN_POINT('',(106.765759948068,1.2,62.5823764794873));
#187194=CARTESIAN_POINT('Origin',(116.959178380441,1.2,51.0204257716897));
#187195=CARTESIAN_POINT('',(106.699412965644,1.2,62.9237004110643));
#187196=CARTESIAN_POINT('',(106.765759948068,1.2,62.5823764794873));
#187197=CARTESIAN_POINT('Origin',(116.959178380441,1.2,51.0204257716897));
#187198=CARTESIAN_POINT('Origin',(107.358487250503,1.2,62.1534830038465));
#187199=CARTESIAN_POINT('',(107.213169604484,1.7,62.9010737525815));
#187200=CARTESIAN_POINT('',(107.147910976393,1.7,63.2367986144447));
#187201=CARTESIAN_POINT('',(107.213169604484,1.7,62.9010737525815));
#187202=CARTESIAN_POINT('Origin',(109.793301243218,1.45439216225896E-14,
49.6275134075306));
#187203=CARTESIAN_POINT('Origin',(109.793301243218,1.45439216225896E-14,
49.6275134075306));
#187204=CARTESIAN_POINT('Origin',(107.358487250503,1.7,62.1534830038465));
#187205=CARTESIAN_POINT('',(106.776186950858,1.7,62.5287344680997));
#187206=CARTESIAN_POINT('',(106.709573150634,1.7,62.8714310514089));
#187207=CARTESIAN_POINT('',(106.776186950858,1.7,62.5287344680997));
#187208=CARTESIAN_POINT('Origin',(116.959178380441,1.7,51.0204257716897));
#187209=CARTESIAN_POINT('Origin',(116.959178380441,1.7,51.0204257716897));
#187210=CARTESIAN_POINT('Origin',(106.867673747954,1.7,62.0580780473973));
#187211=CARTESIAN_POINT('Origin',(109.302487740669,1.45439216225896E-14,
49.5321084510813));
#187212=CARTESIAN_POINT('Origin',(109.302487740669,1.45439216225896E-14,
49.5321084510813));
#187213=CARTESIAN_POINT('Origin',(106.867673747954,2.2,62.0580780473973));
#187214=CARTESIAN_POINT('',(107.226964778796,2.2,62.8301040873326));
#187215=CARTESIAN_POINT('',(107.16136407846,2.2,63.1675887495536));
#187216=CARTESIAN_POINT('',(107.226964778796,2.2,62.8301040873326));
#187217=CARTESIAN_POINT('',(106.790277706451,2.2,62.4562441765705));
#187218=CARTESIAN_POINT('Origin',(116.959178380441,2.2,51.0204257716897));
#187219=CARTESIAN_POINT('',(106.723299952499,2.2,62.80081313015));
#187220=CARTESIAN_POINT('',(106.790277706451,2.2,62.4562441765705));
#187221=CARTESIAN_POINT('Origin',(116.959178380441,2.2,51.0204257716897));
#187222=CARTESIAN_POINT('Origin',(107.358487250503,2.2,62.1534830038465));
#187223=CARTESIAN_POINT('',(107.244403008174,2.7,62.740392622037));
#187224=CARTESIAN_POINT('',(107.178364799778,2.7,63.0801280568769));
#187225=CARTESIAN_POINT('',(107.244403008174,2.7,62.740392622037));
#187226=CARTESIAN_POINT('Origin',(109.793301243218,1.45439216225896E-14,
49.6275134075306));
#187227=CARTESIAN_POINT('Origin',(109.793301243218,1.45439216225896E-14,
49.6275134075306));
#187228=CARTESIAN_POINT('Origin',(107.358487250503,2.7,62.1534830038465));
#187229=CARTESIAN_POINT('',(106.808094303375,2.7,62.3645861887142));
#187230=CARTESIAN_POINT('',(106.740650702402,2.7,62.7115517054976));
#187231=CARTESIAN_POINT('',(106.808094303375,2.7,62.3645861887142));
#187232=CARTESIAN_POINT('Origin',(116.959178380441,2.7,51.0204257716897));
#187233=CARTESIAN_POINT('Origin',(116.959178380441,2.7,51.0204257716897));
#187234=CARTESIAN_POINT('Origin',(106.867673747954,2.7,62.0580780473973));
#187235=CARTESIAN_POINT('Origin',(109.302487740669,1.45439216225896E-14,
49.5321084510813));
#187236=CARTESIAN_POINT('Origin',(109.302487740669,1.45439216225896E-14,
49.5321084510813));
#187237=CARTESIAN_POINT('Origin',(107.358487250503,3.2,62.1534830038465));
#187238=CARTESIAN_POINT('',(107.290529118892,3.7,62.5030955380819));
#187239=CARTESIAN_POINT('',(107.223305387788,3.7,62.8489299280895));
#187240=CARTESIAN_POINT('',(107.290529118892,3.7,62.5030955380819));
#187241=CARTESIAN_POINT('',(107.265559688949,3.2,62.631551478141));
#187242=CARTESIAN_POINT('Origin',(109.793301243218,1.45439216225896E-14,
49.6275134075306));
#187243=CARTESIAN_POINT('',(107.198982882686,3.2,62.9740577449709));
#187244=CARTESIAN_POINT('',(107.265559688949,3.2,62.631551478141));
#187245=CARTESIAN_POINT('Origin',(109.793301243218,1.45439216225896E-14,
49.6275134075306));
#187246=CARTESIAN_POINT('Origin',(107.358487250503,3.7,62.1534830038465));
#187247=CARTESIAN_POINT('',(106.85524751672,3.7,62.1220051461779));
#187248=CARTESIAN_POINT('',(106.786539588514,3.7,62.4754750302491));
#187249=CARTESIAN_POINT('',(106.85524751672,3.7,62.1220051461779));
#187250=CARTESIAN_POINT('Origin',(116.959178380441,3.7,51.0204257716897));
#187251=CARTESIAN_POINT('Origin',(116.959178380441,3.7,51.0204257716897));
#187252=CARTESIAN_POINT('Origin',(106.867673747954,3.7,62.0580780473973));
#187253=CARTESIAN_POINT('',(106.829717275668,3.2,62.2533461948846));
#187254=CARTESIAN_POINT('',(106.76169964183,3.2,62.6032648400092));
#187255=CARTESIAN_POINT('',(106.829717275668,3.2,62.2533461948846));
#187256=CARTESIAN_POINT('Origin',(109.302487740669,1.45439216225896E-14,
49.5321084510813));
#187257=CARTESIAN_POINT('Origin',(109.302487740669,1.45439216225896E-14,
49.5321084510813));
#187258=CARTESIAN_POINT('Origin',(106.867673747954,3.2,62.0580780473973));
#187259=CARTESIAN_POINT('Origin',(116.959178380441,3.2,51.0204257716897));
#187260=CARTESIAN_POINT('Origin',(116.959178380441,3.2,51.0204257716897));
#187261=CARTESIAN_POINT('Origin',(106.867673747954,4.7,62.0580780473973));
#187262=CARTESIAN_POINT('',(106.815284123344,4.2,62.327597956097));
#187263=CARTESIAN_POINT('',(106.848070426457,4.7,62.1589278904623));
#187264=CARTESIAN_POINT('Origin',(109.302487740669,1.45439216225896E-14,
49.5321084510813));
#187265=CARTESIAN_POINT('',(106.867673747954,4.2,62.0580780473973));
#187266=CARTESIAN_POINT('',(106.867673747954,4.2,62.0580780473973));
#187267=CARTESIAN_POINT('',(106.867673747954,4.7,62.0580780473973));
#187268=CARTESIAN_POINT('',(106.867673747954,4.7,62.0580780473973));
#187269=CARTESIAN_POINT('',(106.867673747954,4.7,62.0580780473973));
#187270=CARTESIAN_POINT('Origin',(107.358487250503,4.7,62.1534830038465));
#187271=CARTESIAN_POINT('',(107.30381546326,4.7,62.1428558319088));
#187272=CARTESIAN_POINT('',(107.352392077707,4.7,62.1848397930544));
#187273=CARTESIAN_POINT('Origin',(116.959178380441,4.7,51.0204257716897));
#187274=CARTESIAN_POINT('',(107.283510824698,4.7,62.5392013514836));
#187275=CARTESIAN_POINT('',(107.352392077707,4.7,62.1848397930544));
#187276=CARTESIAN_POINT('Origin',(116.959178380441,4.7,51.0204257716897));
#187277=CARTESIAN_POINT('',(107.30381546326,4.7,62.1428558319088));
#187278=CARTESIAN_POINT('Origin',(107.358487250503,4.2,62.1534830038465));
#187279=CARTESIAN_POINT('',(107.251438653183,4.2,62.7041975468769));
#187280=CARTESIAN_POINT('Origin',(109.793301243218,1.45439216225896E-14,
49.6275134075306));
#187281=CARTESIAN_POINT('',(107.319426744379,4.2,62.3544308847057));
#187282=CARTESIAN_POINT('Origin',(109.793301243218,1.45439216225896E-14,
49.6275134075306));
#187283=CARTESIAN_POINT('',(107.319426744379,4.2,62.3544308847057));
#187284=CARTESIAN_POINT('Origin',(106.867673747954,4.2,62.0580780473973));
#187285=CARTESIAN_POINT('Origin',(116.959178380441,4.2,51.0204257716897));
#187286=CARTESIAN_POINT('',(107.012752757131,4.2,62.0862786907789));
#187287=CARTESIAN_POINT('Origin',(116.959178380441,4.2,51.0204257716897));
#187288=CARTESIAN_POINT('',(106.867673747954,4.2,62.0580780473973));
#187289=CARTESIAN_POINT('Origin',(106.671348346934,4.,62.0199160648176));
#187290=CARTESIAN_POINT('Origin',(114.524364387726,1.45439216225896E-14,
63.5463953680056));
#187291=CARTESIAN_POINT('Origin',(111.775808773449,8.2,63.0121276118898));
#187292=CARTESIAN_POINT('',(112.23936365414,8.2,63.2477653210878));
#187293=CARTESIAN_POINT('',(112.171058441185,8.2,63.5991634251371));
#187294=CARTESIAN_POINT('',(112.23936365414,8.2,63.2477653210878));
#187295=CARTESIAN_POINT('',(111.767477236086,8.2,63.0549894419973));
#187296=CARTESIAN_POINT('Origin',(116.959178380441,8.2,51.0204257716897));
#187297=CARTESIAN_POINT('',(111.698657306259,8.2,63.4090355215762));
#187298=CARTESIAN_POINT('',(111.767477236086,8.2,63.0549894419973));
#187299=CARTESIAN_POINT('Origin',(116.959178380441,8.2,51.0204257716897));
#187300=CARTESIAN_POINT('Origin',(112.266622275998,8.2,63.107532568339));
#187301=CARTESIAN_POINT('',(112.266622275998,8.7,63.107532568339));
#187302=CARTESIAN_POINT('',(112.232598328127,8.7,63.2825697325142));
#187303=CARTESIAN_POINT('',(112.266622275998,8.7,63.107532568339));
#187304=CARTESIAN_POINT('',(112.266622275998,8.42058489655001,63.107532568339));
#187305=CARTESIAN_POINT('',(112.266622275998,8.42058489655001,63.107532568339));
#187306=CARTESIAN_POINT('Origin',(114.701436268713,1.45439216225896E-14,
50.5815629720231));
#187307=CARTESIAN_POINT('Origin',(114.701436268713,1.45439216225896E-14,
50.5815629720231));
#187308=CARTESIAN_POINT('Origin',(112.266622275998,8.7,63.107532568339));
#187309=CARTESIAN_POINT('',(111.775808773449,8.7,63.0121276118898));
#187310=CARTESIAN_POINT('',(111.760659644282,8.7,63.0900627362657));
#187311=CARTESIAN_POINT('',(111.775808773449,8.7,63.0121276118898));
#187312=CARTESIAN_POINT('',(112.266622275998,8.7,63.107532568339));
#187313=CARTESIAN_POINT('Origin',(116.959178380441,8.7,51.0204257716897));
#187314=CARTESIAN_POINT('Origin',(111.775808773449,8.7,63.0121276118898));
#187315=CARTESIAN_POINT('',(111.775808773449,8.26778386268001,63.0121276118898));
#187316=CARTESIAN_POINT('Origin',(114.210622766164,1.45439216225896E-14,
50.4861580155739));
#187317=CARTESIAN_POINT('',(111.775808773449,8.7,63.0121276118898));
#187318=CARTESIAN_POINT('Origin',(114.210622766164,1.45439216225896E-14,
50.4861580155739));
#187319=CARTESIAN_POINT('Origin',(111.579483372429,8.,62.9739656293101));
#187320=CARTESIAN_POINT('Origin',(114.524364387726,1.45439216225896E-14,
63.5463953680056));
#187321=CARTESIAN_POINT('Origin',(112.757435778548,8.2,63.2029375247883));
#187322=CARTESIAN_POINT('',(113.194515126452,8.2,63.5747793628157));
#187323=CARTESIAN_POINT('',(113.126917293563,8.2,63.922538330062));
#187324=CARTESIAN_POINT('',(113.194515126452,8.2,63.5747793628157));
#187325=CARTESIAN_POINT('',(112.715066123186,8.2,63.4209094176961));
#187326=CARTESIAN_POINT('Origin',(116.959178380441,8.2,51.0204257716897));
#187327=CARTESIAN_POINT('',(112.647166429423,8.2,63.7702213167638));
#187328=CARTESIAN_POINT('',(112.715066123186,8.2,63.4209094176961));
#187329=CARTESIAN_POINT('Origin',(116.959178380441,8.2,51.0204257716897));
#187330=CARTESIAN_POINT('Origin',(113.248249281097,8.2,63.2983424812375));
#187331=CARTESIAN_POINT('',(113.248249281097,8.7,63.2983424812375));
#187332=CARTESIAN_POINT('',(113.187821582277,8.7,63.6092144905408));
#187333=CARTESIAN_POINT('',(113.248249281097,8.7,63.2983424812375));
#187334=CARTESIAN_POINT('',(113.248249281097,8.63170029600201,63.2983424812375));
#187335=CARTESIAN_POINT('',(113.248249281097,8.63170029600201,63.2983424812375));
#187336=CARTESIAN_POINT('Origin',(115.683063273812,1.45439216225896E-14,
50.7723728849216));
#187337=CARTESIAN_POINT('Origin',(115.683063273812,1.45439216225896E-14,
50.7723728849216));
#187338=CARTESIAN_POINT('Origin',(113.248249281097,8.7,63.2983424812375));
#187339=CARTESIAN_POINT('',(112.757435778548,8.7,63.2029375247883));
#187340=CARTESIAN_POINT('',(112.708341954184,8.7,63.4555020957113));
#187341=CARTESIAN_POINT('',(112.757435778548,8.7,63.2029375247883));
#187342=CARTESIAN_POINT('',(113.248249281097,8.7,63.2983424812375));
#187343=CARTESIAN_POINT('Origin',(116.959178380441,8.7,51.0204257716897));
#187344=CARTESIAN_POINT('Origin',(112.757435778548,8.7,63.2029375247883));
#187345=CARTESIAN_POINT('',(112.757435778548,8.54144308650501,63.2029375247883));
#187346=CARTESIAN_POINT('Origin',(115.192249771263,1.45439216225896E-14,
50.6769679284724));
#187347=CARTESIAN_POINT('',(112.757435778548,8.7,63.2029375247883));
#187348=CARTESIAN_POINT('Origin',(115.192249771263,1.45439216225896E-14,
50.6769679284724));
#187349=CARTESIAN_POINT('Origin',(112.561110377528,8.,63.1647755422086));
#187350=CARTESIAN_POINT('Origin',(114.524364387726,1.45439216225896E-14,
63.5463953680056));
#187351=CARTESIAN_POINT('Origin',(113.739062783647,8.2,63.3937474376868));
#187352=CARTESIAN_POINT('',(114.164465217381,8.2,63.8256614916251));
#187353=CARTESIAN_POINT('',(114.097174797181,8.2,64.1718389655816));
#187354=CARTESIAN_POINT('',(114.164465217381,8.2,63.8256614916251));
#187355=CARTESIAN_POINT('',(113.677659493004,8.2,63.7096384067719));
#187356=CARTESIAN_POINT('Origin',(116.959178380441,8.2,51.0204257716897));
#187357=CARTESIAN_POINT('',(113.610263873378,8.2,64.0563570821562));
#187358=CARTESIAN_POINT('',(113.677659493004,8.2,63.7096384067719));
#187359=CARTESIAN_POINT('Origin',(116.959178380441,8.2,51.0204257716897));
#187360=CARTESIAN_POINT('Origin',(114.229876286196,8.2,63.489152394136));
#187361=CARTESIAN_POINT('',(114.226766123991,8.7,63.5051527117506));
#187362=CARTESIAN_POINT('',(114.157802851094,8.7,63.8599362238241));
#187363=CARTESIAN_POINT('',(114.226766123991,8.7,63.5051527117506));
#187364=CARTESIAN_POINT('Origin',(116.664690278911,1.45439216225896E-14,
50.9631827978201));
#187365=CARTESIAN_POINT('Origin',(116.664690278911,1.45439216225896E-14,
50.9631827978201));
#187366=CARTESIAN_POINT('Origin',(114.229876286196,8.7,63.489152394136));
#187367=CARTESIAN_POINT('',(113.739062783647,8.7,63.3937474376868));
#187368=CARTESIAN_POINT('',(113.670986458514,8.7,63.7439680218447));
#187369=CARTESIAN_POINT('',(113.739062783647,8.7,63.3937474376868));
#187370=CARTESIAN_POINT('',(113.825924529237,8.7,63.4106317349037));
#187371=CARTESIAN_POINT('',(113.825924529237,8.7,63.4106317349037));
#187372=CARTESIAN_POINT('Origin',(116.959178380441,8.7,51.0204257716897));
#187373=CARTESIAN_POINT('Origin',(116.959178380441,8.7,51.0204257716897));
#187374=CARTESIAN_POINT('Origin',(113.739062783647,8.7,63.3937474376868));
#187375=CARTESIAN_POINT('',(113.739062783647,8.69230981960501,63.3937474376868));
#187376=CARTESIAN_POINT('Origin',(116.173876776362,1.45439216225896E-14,
50.8677778413709));
#187377=CARTESIAN_POINT('',(113.739062783647,8.7,63.3937474376868));
#187378=CARTESIAN_POINT('Origin',(116.173876776362,1.45439216225896E-14,
50.8677778413709));
#187379=CARTESIAN_POINT('Origin',(113.542737382627,8.,63.3555854551071));
#187380=CARTESIAN_POINT('Origin',(114.524364387726,1.45439216225896E-14,
63.5463953680056));
#187381=CARTESIAN_POINT('Origin',(114.720689788746,8.2,63.5845573505853));
#187382=CARTESIAN_POINT('',(115.149006332374,8.2,64.0014796835762));
#187383=CARTESIAN_POINT('',(115.081639452434,8.2,64.3480505068311));
#187384=CARTESIAN_POINT('',(115.149006332374,8.2,64.0014796835762));
#187385=CARTESIAN_POINT('',(114.654914694975,8.2,63.9229391847761));
#187386=CARTESIAN_POINT('Origin',(116.959178380441,8.2,51.0204257716897));
#187387=CARTESIAN_POINT('',(114.587633813946,8.2,64.2690675841949));
#187388=CARTESIAN_POINT('',(114.654914694975,8.2,63.9229391847761));
#187389=CARTESIAN_POINT('Origin',(116.959178380441,8.2,51.0204257716897));
#187390=CARTESIAN_POINT('Origin',(115.211503291295,8.2,63.6799623070345));
#187391=CARTESIAN_POINT('',(115.211381799034,8.7,63.6805873274131));
#187392=CARTESIAN_POINT('',(115.142336212475,8.7,64.0357943044535));
#187393=CARTESIAN_POINT('',(115.211381799034,8.7,63.6805873274131));
#187394=CARTESIAN_POINT('Origin',(117.64631728401,1.45439216225896E-14,
51.1539927107186));
#187395=CARTESIAN_POINT('Origin',(117.64631728401,1.45439216225896E-14,
51.1539927107186));
#187396=CARTESIAN_POINT('Origin',(115.211503291295,8.7,63.6799623070345));
#187397=CARTESIAN_POINT('',(114.717206300373,8.7,63.6024782552524));
#187398=CARTESIAN_POINT('',(114.648253295989,8.7,63.9572089406661));
#187399=CARTESIAN_POINT('',(114.717206300373,8.7,63.6024782552524));
#187400=CARTESIAN_POINT('Origin',(116.959178380441,8.7,51.0204257716897));
#187401=CARTESIAN_POINT('Origin',(116.959178380441,8.7,51.0204257716897));
#187402=CARTESIAN_POINT('Origin',(114.720689788746,8.7,63.5845573505853));
#187403=CARTESIAN_POINT('Origin',(117.155503781461,1.45439216225896E-14,
51.0585877542694));
#187404=CARTESIAN_POINT('Origin',(117.155503781461,1.45439216225896E-14,
51.0585877542694));
#187405=CARTESIAN_POINT('Origin',(115.702316793845,8.2,63.7753672634838));
#187406=CARTESIAN_POINT('',(116.148189911293,8.2,64.1019693048485));
#187407=CARTESIAN_POINT('',(116.080358733155,8.2,64.4509287233428));
#187408=CARTESIAN_POINT('',(116.148189911293,8.2,64.1019693048485));
#187409=CARTESIAN_POINT('',(115.646754512291,8.2,64.0612089957596));
#187410=CARTESIAN_POINT('Origin',(116.959178380441,8.2,51.0204257716897));
#187411=CARTESIAN_POINT('',(115.579204990518,8.2,64.4087194251001));
#187412=CARTESIAN_POINT('',(115.646754512291,8.2,64.0612089957596));
#187413=CARTESIAN_POINT('Origin',(116.959178380441,8.2,51.0204257716897));
#187414=CARTESIAN_POINT('Origin',(116.193130296394,8.2,63.870772219933));
#187415=CARTESIAN_POINT('',(116.193130296394,8.7,63.870772219933));
#187416=CARTESIAN_POINT('',(116.141472694311,8.7,64.1365262180004));
#187417=CARTESIAN_POINT('',(116.193130296394,8.7,63.870772219933));
#187418=CARTESIAN_POINT('',(116.193130296394,8.56190691376601,63.870772219933));
#187419=CARTESIAN_POINT('',(116.193130296394,8.56190691376601,63.870772219933));
#187420=CARTESIAN_POINT('Origin',(118.62794428911,1.45439216225896E-14,
51.3448026236171));
#187421=CARTESIAN_POINT('Origin',(118.62794428911,1.45439216225896E-14,
51.3448026236171));
#187422=CARTESIAN_POINT('Origin',(116.193130296394,8.7,63.870772219933));
#187423=CARTESIAN_POINT('',(115.702316793845,8.7,63.7753672634838));
#187424=CARTESIAN_POINT('',(115.640065868523,8.7,64.0956189132026));
#187425=CARTESIAN_POINT('',(115.702316793845,8.7,63.7753672634838));
#187426=CARTESIAN_POINT('',(116.193130296394,8.7,63.870772219933));
#187427=CARTESIAN_POINT('Origin',(116.959178380441,8.7,51.0204257716897));
#187428=CARTESIAN_POINT('Origin',(115.702316793845,8.7,63.7753672634838));
#187429=CARTESIAN_POINT('',(115.702316793845,8.64616967217301,63.7753672634838));
#187430=CARTESIAN_POINT('Origin',(118.13713078656,1.45439216225896E-14,
51.2493976671679));
#187431=CARTESIAN_POINT('',(115.702316793845,8.7,63.7753672634838));
#187432=CARTESIAN_POINT('Origin',(118.13713078656,1.45439216225896E-14,
51.2493976671679));
#187433=CARTESIAN_POINT('Origin',(115.505991392825,8.,63.7372052809041));
#187434=CARTESIAN_POINT('Origin',(114.524364387726,1.45439216225896E-14,
63.5463953680056));
#187435=CARTESIAN_POINT('Origin',(116.683943798944,8.2,63.9661771763823));
#187436=CARTESIAN_POINT('',(117.16233107026,8.2,64.1255092316122));
#187437=CARTESIAN_POINT('',(117.093623142053,8.2,64.4789791156834));
#187438=CARTESIAN_POINT('',(117.16233107026,8.2,64.1255092316122));
#187439=CARTESIAN_POINT('',(116.653360186866,8.2,64.1235154355592));
#187440=CARTESIAN_POINT('Origin',(116.959178380441,8.2,51.0204257716897));
#187441=CARTESIAN_POINT('',(116.585144612751,8.2,64.4744523900495));
#187442=CARTESIAN_POINT('',(116.653360186866,8.2,64.1235154355592));
#187443=CARTESIAN_POINT('Origin',(116.959178380441,8.2,51.0204257716897));
#187444=CARTESIAN_POINT('Origin',(117.174757301493,8.2,64.0615821328315));
#187445=CARTESIAN_POINT('',(117.174757301493,8.7,64.0615821328315));
#187446=CARTESIAN_POINT('',(117.155524853906,8.7,64.1605240045573));
#187447=CARTESIAN_POINT('',(117.174757301493,8.7,64.0615821328315));
#187448=CARTESIAN_POINT('',(117.174757301493,8.30097885794202,64.0615821328315));
#187449=CARTESIAN_POINT('',(117.174757301493,8.30097885794202,64.0615821328315));
#187450=CARTESIAN_POINT('Origin',(119.609571294209,1.45439216225896E-14,
51.5356125365156));
#187451=CARTESIAN_POINT('Origin',(119.609571294209,1.45439216225896E-14,
51.5356125365156));
#187452=CARTESIAN_POINT('Origin',(117.174757301493,8.7,64.0615821328315));
#187453=CARTESIAN_POINT('',(116.683943798944,8.7,63.9661771763823));
#187454=CARTESIAN_POINT('',(116.646603960045,8.7,64.1582730359324));
#187455=CARTESIAN_POINT('',(116.683943798944,8.7,63.9661771763823));
#187456=CARTESIAN_POINT('',(117.174757301493,8.7,64.0615821328315));
#187457=CARTESIAN_POINT('Origin',(116.959178380441,8.7,51.0204257716897));
#187458=CARTESIAN_POINT('Origin',(116.683943798944,8.7,63.9661771763823));
#187459=CARTESIAN_POINT('',(116.683943798944,8.44726287030301,63.9661771763823));
#187460=CARTESIAN_POINT('Origin',(119.118757791659,1.45439216225896E-14,
51.4402075800664));
#187461=CARTESIAN_POINT('',(116.683943798944,8.7,63.9661771763823));
#187462=CARTESIAN_POINT('Origin',(119.118757791659,1.45439216225896E-14,
51.4402075800664));
#187463=CARTESIAN_POINT('Origin',(116.487618397924,8.,63.9280151938026));
#187464=CARTESIAN_POINT('Origin',(114.524364387726,1.45439216225896E-14,
63.5463953680056));
#187465=CARTESIAN_POINT('Origin',(122.573705829538,2.7,65.1110366537733));
#187466=CARTESIAN_POINT('',(122.54312221746,2.2,65.2683749129502));
#187467=CARTESIAN_POINT('',(122.474906643345,2.2,65.6193118674405));
#187468=CARTESIAN_POINT('',(122.54312221746,2.2,65.2683749129502));
#187469=CARTESIAN_POINT('',(122.561279598304,2.7,65.174963752554));
#187470=CARTESIAN_POINT('Origin',(125.008519822253,1.45439216225896E-14,
52.5850670574574));
#187471=CARTESIAN_POINT('',(122.492571670098,2.7,65.5284336366251));
#187472=CARTESIAN_POINT('',(122.561279598304,2.7,65.174963752554));
#187473=CARTESIAN_POINT('Origin',(125.008519822253,1.45439216225896E-14,
52.5850670574574));
#187474=CARTESIAN_POINT('Origin',(122.573705829538,2.2,65.1110366537733));
#187475=CARTESIAN_POINT('',(123.064519332087,2.2,65.2064416102226));
#187476=CARTESIAN_POINT('',(123.027179493189,2.2,65.3985374697727));
#187477=CARTESIAN_POINT('',(123.064519332087,2.2,65.2064416102226));
#187478=CARTESIAN_POINT('',(122.816425740386,2.2,65.1582168605189));
#187479=CARTESIAN_POINT('',(122.816425740386,2.2,65.1582168605189));
#187480=CARTESIAN_POINT('Origin',(116.959178380441,2.2,51.0204257716897));
#187481=CARTESIAN_POINT('Origin',(116.959178380441,2.2,51.0204257716897));
#187482=CARTESIAN_POINT('Origin',(123.064519332087,2.2,65.2064416102226));
#187483=CARTESIAN_POINT('',(123.064519332087,2.7,65.2064416102226));
#187484=CARTESIAN_POINT('',(123.0452868845,2.7,65.3053834819483));
#187485=CARTESIAN_POINT('',(123.064519332087,2.7,65.2064416102226));
#187486=CARTESIAN_POINT('',(123.064519332087,2.2,65.2064416102226));
#187487=CARTESIAN_POINT('Origin',(125.499333324803,1.45439216225896E-14,
52.6804720139067));
#187488=CARTESIAN_POINT('Origin',(123.064519332087,2.7,65.2064416102226));
#187489=CARTESIAN_POINT('',(122.672829403438,2.7,65.1303044208618));
#187490=CARTESIAN_POINT('Origin',(116.959178380441,2.7,51.0204257716897));
#187491=CARTESIAN_POINT('',(123.064519332087,2.7,65.2064416102226));
#187492=CARTESIAN_POINT('Origin',(116.959178380441,2.7,51.0204257716897));
#187493=CARTESIAN_POINT('Origin',(122.377380428518,2.,65.0728746711936));
#187494=CARTESIAN_POINT('Origin',(114.524364387726,1.45439216225896E-14,
63.5463953680056));
#187495=CARTESIAN_POINT('Origin',(122.573705829538,1.7,65.1110366537733));
#187496=CARTESIAN_POINT('',(122.518143547984,1.2,65.3968783860492));
#187497=CARTESIAN_POINT('',(122.450594026211,1.2,65.7443888153896));
#187498=CARTESIAN_POINT('',(122.518143547984,1.2,65.3968783860492));
#187499=CARTESIAN_POINT('',(122.528765444436,1.7,65.3422337386888));
#187500=CARTESIAN_POINT('Origin',(125.008519822253,1.45439216225896E-14,
52.5850670574574));
#187501=CARTESIAN_POINT('',(122.460934266298,1.7,65.6911931571831));
#187502=CARTESIAN_POINT('',(122.528765444436,1.7,65.3422337386888));
#187503=CARTESIAN_POINT('Origin',(125.008519822253,1.45439216225896E-14,
52.5850670574574));
#187504=CARTESIAN_POINT('Origin',(122.573705829538,1.2,65.1110366537733));
#187505=CARTESIAN_POINT('',(123.064519332087,1.2,65.2064416102226));
#187506=CARTESIAN_POINT('',(123.002268406765,1.2,65.5266932599413));
#187507=CARTESIAN_POINT('',(123.064519332087,1.2,65.2064416102226));
#187508=CARTESIAN_POINT('',(123.011678028599,1.2,65.1961702500586));
#187509=CARTESIAN_POINT('',(123.011678028599,1.2,65.1961702500586));
#187510=CARTESIAN_POINT('Origin',(116.959178380441,1.2,51.0204257716897));
#187511=CARTESIAN_POINT('Origin',(116.959178380441,1.2,51.0204257716897));
#187512=CARTESIAN_POINT('Origin',(123.064519332087,1.2,65.2064416102226));
#187513=CARTESIAN_POINT('',(123.064519332087,1.7,65.2064416102226));
#187514=CARTESIAN_POINT('',(123.012861730004,1.7,65.4721956082899));
#187515=CARTESIAN_POINT('',(123.064519332087,1.7,65.2064416102226));
#187516=CARTESIAN_POINT('',(123.064519332087,1.2,65.2064416102226));
#187517=CARTESIAN_POINT('Origin',(125.499333324803,1.45439216225896E-14,
52.6804720139067));
#187518=CARTESIAN_POINT('Origin',(123.064519332087,1.7,65.2064416102226));
#187519=CARTESIAN_POINT('',(122.928963429423,1.7,65.1800920804664));
#187520=CARTESIAN_POINT('Origin',(116.959178380441,1.7,51.0204257716897));
#187521=CARTESIAN_POINT('',(123.064519332087,1.7,65.2064416102226));
#187522=CARTESIAN_POINT('Origin',(116.959178380441,1.7,51.0204257716897));
#187523=CARTESIAN_POINT('Origin',(122.377380428518,1.,65.0728746711936));
#187524=CARTESIAN_POINT('Origin',(114.524364387726,1.45439216225896E-14,
63.5463953680056));
#187525=CARTESIAN_POINT('Origin',(122.573705829538,0.200000000000015,65.1110366537733));
#187526=CARTESIAN_POINT('',(123.061035843715,0.200000000000015,65.2243625148896));
#187527=CARTESIAN_POINT('',(122.99208283933,0.200000000000015,65.5790932003033));
#187528=CARTESIAN_POINT('',(123.061035843715,0.200000000000015,65.2243625148896));
#187529=CARTESIAN_POINT('',(122.507930735767,0.200000000000015,65.4494184879642));
#187530=CARTESIAN_POINT('Origin',(116.959178380441,0.200000000000015,51.0204257716897));
#187531=CARTESIAN_POINT('',(122.440649854738,0.200000000000015,65.7955468873829));
#187532=CARTESIAN_POINT('',(122.507930735767,0.200000000000015,65.4494184879642));
#187533=CARTESIAN_POINT('Origin',(116.959178380441,0.200000000000015,51.0204257716897));
#187534=CARTESIAN_POINT('Origin',(123.064519332087,0.200000000000015,65.2064416102226));
#187535=CARTESIAN_POINT('',(123.064397839827,0.700000000000015,65.2070666306011));
#187536=CARTESIAN_POINT('',(122.995352253267,0.700000000000015,65.5622736076416));
#187537=CARTESIAN_POINT('',(123.064397839827,0.700000000000015,65.2070666306011));
#187538=CARTESIAN_POINT('Origin',(125.499333324803,1.45439216225896E-14,
52.6804720139067));
#187539=CARTESIAN_POINT('Origin',(125.499333324803,1.45439216225896E-14,
52.6804720139067));
#187540=CARTESIAN_POINT('Origin',(123.064519332087,0.700000000000015,65.2064416102226));
#187541=CARTESIAN_POINT('',(122.511208870617,0.700000000000015,65.432554030315));
#187542=CARTESIAN_POINT('',(122.443841990677,0.700000000000015,65.7791248535699));
#187543=CARTESIAN_POINT('',(122.511208870617,0.700000000000015,65.432554030315));
#187544=CARTESIAN_POINT('Origin',(116.959178380441,0.700000000000015,51.0204257716897));
#187545=CARTESIAN_POINT('Origin',(116.959178380441,0.700000000000015,51.0204257716897));
#187546=CARTESIAN_POINT('Origin',(122.573705829538,0.700000000000015,65.1110366537733));
#187547=CARTESIAN_POINT('Origin',(125.008519822253,1.45439216225896E-14,
52.5850670574574));
#187548=CARTESIAN_POINT('Origin',(125.008519822253,1.45439216225896E-14,
52.5850670574574));
#187549=CARTESIAN_POINT('Origin',(107.849300753053,0.200000000000015,62.2488879602958));
#187550=CARTESIAN_POINT('',(108.081232306075,0.200000000000015,63.6761184436699));
#187551=CARTESIAN_POINT('',(108.018661167669,0.200000000000015,63.9980174386746));
#187552=CARTESIAN_POINT('',(108.081232306075,0.200000000000015,63.6761184436699));
#187553=CARTESIAN_POINT('',(107.635054033078,0.200000000000015,63.351086283674));
#187554=CARTESIAN_POINT('Origin',(116.959178380441,0.200000000000015,51.0204257716897));
#187555=CARTESIAN_POINT('',(107.571453128439,0.200000000000015,63.6782829402525));
#187556=CARTESIAN_POINT('',(107.635054033078,0.200000000000015,63.351086283674));
#187557=CARTESIAN_POINT('Origin',(116.959178380441,0.200000000000015,51.0204257716897));
#187558=CARTESIAN_POINT('Origin',(108.340114255602,0.200000000000015,62.344292916745));
#187559=CARTESIAN_POINT('',(108.084275160503,0.700000000000015,63.6604643928218));
#187560=CARTESIAN_POINT('',(108.021634869547,0.700000000000015,63.9827191450807));
#187561=CARTESIAN_POINT('',(108.084275160503,0.700000000000015,63.6604643928218));
#187562=CARTESIAN_POINT('Origin',(110.774928248317,1.45439216225896E-14,
49.8183233204291));
#187563=CARTESIAN_POINT('Origin',(110.774928248317,1.45439216225896E-14,
49.8183233204291));
#187564=CARTESIAN_POINT('Origin',(108.340114255602,0.700000000000015,62.344292916745));
#187565=CARTESIAN_POINT('',(107.638148217403,0.700000000000015,63.335168164717));
#187566=CARTESIAN_POINT('',(107.574474684828,0.700000000000015,63.6627384577665));
#187567=CARTESIAN_POINT('',(107.638148217403,0.700000000000015,63.335168164717));
#187568=CARTESIAN_POINT('Origin',(116.959178380441,0.700000000000015,51.0204257716897));
#187569=CARTESIAN_POINT('Origin',(116.959178380441,0.700000000000015,51.0204257716897));
#187570=CARTESIAN_POINT('Origin',(107.849300753053,0.700000000000015,62.2488879602958));
#187571=CARTESIAN_POINT('Origin',(110.284114745768,1.45439216225896E-14,
49.7229183639799));
#187572=CARTESIAN_POINT('Origin',(110.284114745768,1.45439216225896E-14,
49.7229183639799));
#187573=CARTESIAN_POINT('Origin',(107.849300753053,1.2,62.2488879602958));
#187574=CARTESIAN_POINT('',(108.090710291957,1.2,63.62735867666));
#187575=CARTESIAN_POINT('',(108.027923255991,1.2,63.9503683627822));
#187576=CARTESIAN_POINT('',(108.090710291957,1.2,63.62735867666));
#187577=CARTESIAN_POINT('',(107.644692296156,1.2,63.3015019660882));
#187578=CARTESIAN_POINT('Origin',(116.959178380441,1.2,51.0204257716897));
#187579=CARTESIAN_POINT('',(107.580864617103,1.2,63.6298652700673));
#187580=CARTESIAN_POINT('',(107.644692296156,1.2,63.3015019660882));
#187581=CARTESIAN_POINT('Origin',(116.959178380441,1.2,51.0204257716897));
#187582=CARTESIAN_POINT('Origin',(108.340114255602,1.2,62.344292916745));
#187583=CARTESIAN_POINT('',(108.100562188088,1.7,63.5766753177783));
#187584=CARTESIAN_POINT('',(108.037549170674,1.7,63.9008475718654));
#187585=CARTESIAN_POINT('',(108.100562188088,1.7,63.5766753177783));
#187586=CARTESIAN_POINT('Origin',(110.774928248317,1.45439216225896E-14,
49.8183233204291));
#187587=CARTESIAN_POINT('Origin',(110.774928248317,1.45439216225896E-14,
49.8183233204291));
#187588=CARTESIAN_POINT('Origin',(108.340114255602,1.7,62.344292916745));
#187589=CARTESIAN_POINT('',(107.654712027589,1.7,63.2499551737372));
#187590=CARTESIAN_POINT('',(107.590646898367,1.7,63.5795400468435));
#187591=CARTESIAN_POINT('',(107.654712027589,1.7,63.2499551737372));
#187592=CARTESIAN_POINT('Origin',(116.959178380441,1.7,51.0204257716897));
#187593=CARTESIAN_POINT('Origin',(116.959178380441,1.7,51.0204257716897));
#187594=CARTESIAN_POINT('Origin',(107.849300753053,1.7,62.2488879602958));
#187595=CARTESIAN_POINT('Origin',(110.284114745768,1.45439216225896E-14,
49.7229183639799));
#187596=CARTESIAN_POINT('Origin',(110.284114745768,1.45439216225896E-14,
49.7229183639799));
#187597=CARTESIAN_POINT('Origin',(107.849300753053,2.2,62.2488879602958));
#187598=CARTESIAN_POINT('',(108.113868797738,2.2,63.5082190872827));
#187599=CARTESIAN_POINT('',(108.050547990326,2.2,63.8339747757386));
#187600=CARTESIAN_POINT('',(108.113868797738,2.2,63.5082190872827));
#187601=CARTESIAN_POINT('',(107.668247350469,2.2,63.1803223215487));
#187602=CARTESIAN_POINT('Origin',(116.959178380441,2.2,51.0204257716897));
#187603=CARTESIAN_POINT('',(107.603858672105,2.2,63.5115717023834));
#187604=CARTESIAN_POINT('',(107.668247350469,2.2,63.1803223215487));
#187605=CARTESIAN_POINT('Origin',(116.959178380441,2.2,51.0204257716897));
#187606=CARTESIAN_POINT('Origin',(108.340114255602,2.2,62.344292916745));
#187607=CARTESIAN_POINT('',(108.130682275735,2.7,63.4217216731765));
#187608=CARTESIAN_POINT('',(108.066968286624,2.7,63.7495000960255));
#187609=CARTESIAN_POINT('',(108.130682275735,2.7,63.4217216731765));
#187610=CARTESIAN_POINT('Origin',(110.774928248317,1.45439216225896E-14,
49.8183233204291));
#187611=CARTESIAN_POINT('Origin',(110.774928248317,1.45439216225896E-14,
49.8183233204291));
#187612=CARTESIAN_POINT('Origin',(108.340114255602,2.7,62.344292916745));
#187613=CARTESIAN_POINT('',(107.685353195764,2.7,63.0923208155893));
#187614=CARTESIAN_POINT('',(107.620550970598,2.7,63.4256976996709));
#187615=CARTESIAN_POINT('',(107.685353195764,2.7,63.0923208155893));
#187616=CARTESIAN_POINT('Origin',(116.959178380441,2.7,51.0204257716897));
#187617=CARTESIAN_POINT('Origin',(116.959178380441,2.7,51.0204257716897));
#187618=CARTESIAN_POINT('Origin',(107.849300753053,2.7,62.2488879602958));
#187619=CARTESIAN_POINT('Origin',(110.284114745768,1.45439216225896E-14,
49.7229183639799));
#187620=CARTESIAN_POINT('Origin',(110.284114745768,1.45439216225896E-14,
49.7229183639799));
#187621=CARTESIAN_POINT('Origin',(107.849300753053,3.2,62.2488879602958));
#187622=CARTESIAN_POINT('',(108.151070036431,3.2,63.3168362604153));
#187623=CARTESIAN_POINT('',(108.086872760294,3.2,63.6471009670686));
#187624=CARTESIAN_POINT('',(108.151070036431,3.2,63.3168362604153));
#187625=CARTESIAN_POINT('',(107.706100636741,3.2,62.9855850174297));
#187626=CARTESIAN_POINT('Origin',(116.959178380441,3.2,51.0204257716897));
#187627=CARTESIAN_POINT('',(107.640789730382,3.2,63.3215788263236));
#187628=CARTESIAN_POINT('',(107.706100636741,3.2,62.9855850174297));
#187629=CARTESIAN_POINT('Origin',(116.959178380441,3.2,51.0204257716897));
#187630=CARTESIAN_POINT('Origin',(108.340114255602,3.2,62.344292916745));
#187631=CARTESIAN_POINT('',(108.175116167184,3.7,63.1931302592104));
#187632=CARTESIAN_POINT('',(108.110339490587,3.7,63.5263757079516));
#187633=CARTESIAN_POINT('',(108.175116167184,3.7,63.1931302592104));
#187634=CARTESIAN_POINT('Origin',(110.774928248317,1.45439216225896E-14,
49.8183233204291));
#187635=CARTESIAN_POINT('Origin',(110.774928248317,1.45439216225896E-14,
49.8183233204291));
#187636=CARTESIAN_POINT('Origin',(108.340114255602,3.7,62.344292916745));
#187637=CARTESIAN_POINT('',(107.730578435575,3.7,62.859658287547));
#187638=CARTESIAN_POINT('',(107.664657153423,3.7,63.1987921920089));
#187639=CARTESIAN_POINT('',(107.730578435575,3.7,62.859658287547));
#187640=CARTESIAN_POINT('Origin',(116.959178380441,3.7,51.0204257716897));
#187641=CARTESIAN_POINT('Origin',(116.959178380441,3.7,51.0204257716897));
#187642=CARTESIAN_POINT('Origin',(107.849300753053,3.7,62.2488879602958));
#187643=CARTESIAN_POINT('Origin',(110.284114745768,1.45439216225896E-14,
49.7229183639799));
#187644=CARTESIAN_POINT('Origin',(110.284114745768,1.45439216225896E-14,
49.7229183639799));
#187645=CARTESIAN_POINT('Origin',(107.849300753053,4.2,62.2488879602958));
#187646=CARTESIAN_POINT('',(108.202923274195,4.2,63.0500758090438));
#187647=CARTESIAN_POINT('',(108.137463560871,4.2,63.3868351595864));
#187648=CARTESIAN_POINT('',(108.202923274195,4.2,63.0500758090438));
#187649=CARTESIAN_POINT('',(107.758895068754,4.2,62.7139825655704));
#187650=CARTESIAN_POINT('Origin',(116.959178380441,4.2,51.0204257716897));
#187651=CARTESIAN_POINT('',(107.692253482546,4.2,63.0568220946606));
#187652=CARTESIAN_POINT('',(107.758895068754,4.2,62.7139825655704));
#187653=CARTESIAN_POINT('Origin',(116.959178380441,4.2,51.0204257716897));
#187654=CARTESIAN_POINT('Origin',(108.340114255602,4.2,62.344292916745));
#187655=CARTESIAN_POINT('',(108.234614861118,4.7,62.8870375418728));
#187656=CARTESIAN_POINT('',(108.168359143959,4.7,63.2278919567083));
#187657=CARTESIAN_POINT('',(108.234614861118,4.7,62.8870375418728));
#187658=CARTESIAN_POINT('Origin',(110.774928248317,1.45439216225896E-14,
49.8183233204291));
#187659=CARTESIAN_POINT('Origin',(110.774928248317,1.45439216225896E-14,
49.8183233204291));
#187660=CARTESIAN_POINT('Origin',(108.340114255602,4.7,62.344292916745));
#187661=CARTESIAN_POINT('',(107.791181346046,4.7,62.5478848969395));
#187662=CARTESIAN_POINT('',(107.723699286108,4.7,62.8950482669577));
#187663=CARTESIAN_POINT('',(107.791181346046,4.7,62.5478848969395));
#187664=CARTESIAN_POINT('Origin',(116.959178380441,4.7,51.0204257716897));
#187665=CARTESIAN_POINT('Origin',(116.959178380441,4.7,51.0204257716897));
#187666=CARTESIAN_POINT('Origin',(107.849300753053,4.7,62.2488879602958));
#187667=CARTESIAN_POINT('Origin',(110.284114745768,1.45439216225896E-14,
49.7229183639799));
#187668=CARTESIAN_POINT('Origin',(110.284114745768,1.45439216225896E-14,
49.7229183639799));
#187669=CARTESIAN_POINT('Origin',(107.849300753053,5.2,62.2488879602958));
#187670=CARTESIAN_POINT('',(108.203162162018,5.2,63.0488468438676));
#187671=CARTESIAN_POINT('',(107.759138382928,5.2,62.7127308289054));
#187672=CARTESIAN_POINT('Origin',(116.959178380441,5.2,51.0204257716897));
#187673=CARTESIAN_POINT('',(108.270338379292,5.2,62.703256890106));
#187674=CARTESIAN_POINT('',(108.270338379292,5.2,62.703256890106));
#187675=CARTESIAN_POINT('',(107.827593782639,5.2,62.3605600848366));
#187676=CARTESIAN_POINT('Origin',(116.959178380441,5.2,51.0204257716897));
#187677=CARTESIAN_POINT('',(107.827593782639,5.2,62.3605600848366));
#187678=CARTESIAN_POINT('Origin',(108.340114255602,5.2,62.344292916745));
#187679=CARTESIAN_POINT('',(108.242033679243,5.7,62.848871221758));
#187680=CARTESIAN_POINT('Origin',(110.774928248317,1.45439216225896E-14,
49.8183233204291));
#187681=CARTESIAN_POINT('',(108.310269142593,5.7,62.4978319465326));
#187682=CARTESIAN_POINT('',(108.310269142593,5.7,62.4978319465326));
#187683=CARTESIAN_POINT('Origin',(110.774928248317,1.45439216225896E-14,
49.8183233204291));
#187684=CARTESIAN_POINT('Origin',(108.340114255602,5.7,62.344292916745));
#187685=CARTESIAN_POINT('',(108.034759286615,5.7,62.2849376272788));
#187686=CARTESIAN_POINT('',(107.849300753053,5.7,62.2488879602958));
#187687=CARTESIAN_POINT('',(108.034759286615,5.7,62.2849376272788));
#187688=CARTESIAN_POINT('Origin',(116.959178380441,5.7,51.0204257716897));
#187689=CARTESIAN_POINT('',(107.798741589013,5.7,62.5089910127149));
#187690=CARTESIAN_POINT('Origin',(116.959178380441,5.7,51.0204257716897));
#187691=CARTESIAN_POINT('',(107.849300753053,5.7,62.2488879602958));
#187692=CARTESIAN_POINT('Origin',(107.849300753053,5.7,62.2488879602958));
#187693=CARTESIAN_POINT('Origin',(110.284114745768,1.45439216225896E-14,
49.7229183639799));
#187694=CARTESIAN_POINT('',(107.849300753053,5.47323030759702,62.2488879602958));
#187695=CARTESIAN_POINT('Origin',(110.284114745768,1.45439216225896E-14,
49.7229183639799));
#187696=CARTESIAN_POINT('',(107.849300753053,5.7,62.2488879602958));
#187697=CARTESIAN_POINT('Origin',(107.652975352033,5.,62.2107259777161));
#187698=CARTESIAN_POINT('Origin',(114.524364387726,1.45439216225896E-14,
63.5463953680056));
#187699=CARTESIAN_POINT('Origin',(109.812554763251,7.2,62.6305077860928));
#187700=CARTESIAN_POINT('',(110.259896542597,7.2,62.9495542546965));
#187701=CARTESIAN_POINT('',(110.192026238092,7.2,63.2987149598918));
#187702=CARTESIAN_POINT('',(110.259896542597,7.2,62.9495542546965));
#187703=CARTESIAN_POINT('',(109.802733452754,7.2,62.6810337963105));
#187704=CARTESIAN_POINT('Origin',(116.959178380441,7.2,51.0204257716897));
#187705=CARTESIAN_POINT('',(109.733954314151,7.2,63.0348700242867));
#187706=CARTESIAN_POINT('',(109.802733452754,7.2,62.6810337963105));
#187707=CARTESIAN_POINT('Origin',(116.959178380441,7.2,51.0204257716897));
#187708=CARTESIAN_POINT('Origin',(110.3033682658,7.2,62.725912742542));
#187709=CARTESIAN_POINT('',(110.3033682658,7.7,62.725912742542));
#187710=CARTESIAN_POINT('',(110.245860503599,7.7,63.0217630551504));
#187711=CARTESIAN_POINT('',(110.3033682658,7.7,62.725912742542));
#187712=CARTESIAN_POINT('',(110.3033682658,7.59646299273501,62.725912742542));
#187713=CARTESIAN_POINT('',(110.3033682658,7.59646299273501,62.725912742542));
#187714=CARTESIAN_POINT('Origin',(112.738182258515,1.45439216225896E-14,
50.1999431462261));
#187715=CARTESIAN_POINT('Origin',(112.738182258515,1.45439216225896E-14,
50.1999431462261));
#187716=CARTESIAN_POINT('Origin',(110.3033682658,7.7,62.725912742542));
#187717=CARTESIAN_POINT('',(109.812554763251,7.7,62.6305077860928));
#187718=CARTESIAN_POINT('',(109.788505318111,7.7,62.7542308382569));
#187719=CARTESIAN_POINT('',(109.812554763251,7.7,62.6305077860928));
#187720=CARTESIAN_POINT('',(110.3033682658,7.7,62.725912742542));
#187721=CARTESIAN_POINT('Origin',(116.959178380441,7.7,51.0204257716897));
#187722=CARTESIAN_POINT('Origin',(109.812554763251,7.7,62.6305077860928));
#187723=CARTESIAN_POINT('',(109.812554763251,7.29083328570901,62.6305077860928));
#187724=CARTESIAN_POINT('Origin',(112.247368755966,1.45439216225896E-14,
50.1045381897769));
#187725=CARTESIAN_POINT('',(109.812554763251,7.7,62.6305077860928));
#187726=CARTESIAN_POINT('Origin',(112.247368755966,1.45439216225896E-14,
50.1045381897769));
#187727=CARTESIAN_POINT('Origin',(109.616229362231,7.,62.5923458035131));
#187728=CARTESIAN_POINT('Origin',(114.524364387726,1.45439216225896E-14,
63.5463953680056));
#187729=CARTESIAN_POINT('Origin',(110.79418176835,7.2,62.8213176989913));
#187730=CARTESIAN_POINT('',(111.186312844935,7.2,63.424397192804));
#187731=CARTESIAN_POINT('',(111.119883400425,7.2,63.7661453529164));
#187732=CARTESIAN_POINT('',(111.186312844935,7.2,63.424397192804));
#187733=CARTESIAN_POINT('',(110.721137271773,7.2,63.1970971819562));
#187734=CARTESIAN_POINT('Origin',(116.959178380441,7.2,51.0204257716897));
#187735=CARTESIAN_POINT('',(110.654046326041,7.2,63.5422484538535));
#187736=CARTESIAN_POINT('',(110.721137271773,7.2,63.1970971819562));
#187737=CARTESIAN_POINT('Origin',(116.959178380441,7.2,51.0204257716897));
#187738=CARTESIAN_POINT('Origin',(111.284995270899,7.2,62.9167226554405));
#187739=CARTESIAN_POINT('',(111.240421969713,7.7,63.1460312667499));
#187740=CARTESIAN_POINT('',(111.172581016328,7.7,63.4950409742804));
#187741=CARTESIAN_POINT('',(111.240421969713,7.7,63.1460312667499));
#187742=CARTESIAN_POINT('Origin',(113.719809263614,1.45439216225896E-14,
50.3907530591246));
#187743=CARTESIAN_POINT('Origin',(113.719809263614,1.45439216225896E-14,
50.3907530591246));
#187744=CARTESIAN_POINT('Origin',(111.284995270899,7.7,62.9167226554405));
#187745=CARTESIAN_POINT('',(110.775811819326,7.7,62.9158224224096));
#187746=CARTESIAN_POINT('',(110.707265830517,7.7,63.2684592046577));
#187747=CARTESIAN_POINT('',(110.775811819326,7.7,62.9158224224096));
#187748=CARTESIAN_POINT('Origin',(116.959178380441,7.7,51.0204257716897));
#187749=CARTESIAN_POINT('Origin',(116.959178380441,7.7,51.0204257716897));
#187750=CARTESIAN_POINT('Origin',(110.79418176835,7.7,62.8213176989913));
#187751=CARTESIAN_POINT('Origin',(113.228995761065,1.45439216225896E-14,
50.2953481026754));
#187752=CARTESIAN_POINT('Origin',(113.228995761065,1.45439216225896E-14,
50.2953481026754));
#187753=CARTESIAN_POINT('Origin',(111.775808773449,7.2,63.0121276118898));
#187754=CARTESIAN_POINT('',(112.12801611812,7.2,63.8205958761048));
#187755=CARTESIAN_POINT('',(112.062591509714,7.2,64.1571746284032));
#187756=CARTESIAN_POINT('',(112.12801611812,7.2,63.8205958761048));
#187757=CARTESIAN_POINT('',(111.655304822504,7.2,63.6320636030099));
#187758=CARTESIAN_POINT('Origin',(116.959178380441,7.2,51.0204257716897));
#187759=CARTESIAN_POINT('',(111.589428346857,7.2,63.9709669991386));
#187760=CARTESIAN_POINT('',(111.655304822504,7.2,63.6320636030099));
#187761=CARTESIAN_POINT('Origin',(116.959178380441,7.2,51.0204257716897));
#187762=CARTESIAN_POINT('Origin',(112.266622275998,7.2,63.107532568339));
#187763=CARTESIAN_POINT('',(112.18126791696,7.7,63.5466404876378));
#187764=CARTESIAN_POINT('',(112.114496201417,7.7,63.8901494707866));
#187765=CARTESIAN_POINT('',(112.18126791696,7.7,63.5466404876378));
#187766=CARTESIAN_POINT('Origin',(114.701436268713,1.45439216225896E-14,
50.5815629720231));
#187767=CARTESIAN_POINT('Origin',(114.701436268713,1.45439216225896E-14,
50.5815629720231));
#187768=CARTESIAN_POINT('Origin',(112.266622275998,7.7,63.107532568339));
#187769=CARTESIAN_POINT('',(111.708941922635,7.7,63.3561260211292));
#187770=CARTESIAN_POINT('',(111.641689634785,7.7,63.7021073221314));
#187771=CARTESIAN_POINT('',(111.708941922635,7.7,63.3561260211292));
#187772=CARTESIAN_POINT('Origin',(116.959178380441,7.7,51.0204257716897));
#187773=CARTESIAN_POINT('Origin',(116.959178380441,7.7,51.0204257716897));
#187774=CARTESIAN_POINT('Origin',(111.775808773449,7.7,63.0121276118898));
#187775=CARTESIAN_POINT('Origin',(114.210622766164,1.45439216225896E-14,
50.4861580155739));
#187776=CARTESIAN_POINT('Origin',(114.210622766164,1.45439216225896E-14,
50.4861580155739));
#187777=CARTESIAN_POINT('Origin',(112.757435778548,7.2,63.2029375247883));
#187778=CARTESIAN_POINT('',(113.084301723809,7.2,64.141775336531));
#187779=CARTESIAN_POINT('',(113.019499498642,7.2,64.4751522206127));
#187780=CARTESIAN_POINT('',(113.084301723809,7.2,64.141775336531));
#187781=CARTESIAN_POINT('',(112.604368680805,7.2,63.9903955475575));
#187782=CARTESIAN_POINT('Origin',(116.959178380441,7.2,51.0204257716897));
#187783=CARTESIAN_POINT('',(112.539300670928,7.2,64.325139768617));
#187784=CARTESIAN_POINT('',(112.604368680805,7.2,63.9903955475575));
#187785=CARTESIAN_POINT('Origin',(116.959178380441,7.2,51.0204257716897));
#187786=CARTESIAN_POINT('Origin',(113.248249281097,7.2,63.2983424812375));
#187787=CARTESIAN_POINT('',(113.137023438408,7.7,63.8705469814669));
#187788=CARTESIAN_POINT('',(113.070912965334,7.7,64.2106541839858));
#187789=CARTESIAN_POINT('',(113.137023438408,7.7,63.8705469814669));
#187790=CARTESIAN_POINT('Origin',(115.683063273812,1.45439216225896E-14,
50.7723728849216));
#187791=CARTESIAN_POINT('Origin',(115.683063273812,1.45439216225896E-14,
50.7723728849216));
#187792=CARTESIAN_POINT('Origin',(113.248249281097,7.7,63.2983424812375));
#187793=CARTESIAN_POINT('',(112.657316677859,7.7,63.7180030759923));
#187794=CARTESIAN_POINT('',(112.590923921114,7.7,64.059562494862));
#187795=CARTESIAN_POINT('',(112.657316677859,7.7,63.7180030759923));
#187796=CARTESIAN_POINT('Origin',(116.959178380441,7.7,51.0204257716897));
#187797=CARTESIAN_POINT('Origin',(116.959178380441,7.7,51.0204257716897));
#187798=CARTESIAN_POINT('Origin',(112.757435778548,7.7,63.2029375247883));
#187799=CARTESIAN_POINT('Origin',(115.192249771263,1.45439216225896E-14,
50.6769679284724));
#187800=CARTESIAN_POINT('Origin',(115.192249771263,1.45439216225896E-14,
50.6769679284724));
#187801=CARTESIAN_POINT('Origin',(113.739062783647,7.2,63.3937474376868));
#187802=CARTESIAN_POINT('',(114.054744863706,7.2,64.3901209609489));
#187803=CARTESIAN_POINT('',(113.990213608426,7.2,64.7221038327708));
#187804=CARTESIAN_POINT('',(114.054744863706,7.2,64.3901209609489));
#187805=CARTESIAN_POINT('',(113.567770401368,7.2,64.2749659533184));
#187806=CARTESIAN_POINT('Origin',(116.959178380441,7.2,51.0204257716897));
#187807=CARTESIAN_POINT('',(113.503146384053,7.2,64.6074260420585));
#187808=CARTESIAN_POINT('',(113.567770401368,7.2,64.2749659533184));
#187809=CARTESIAN_POINT('Origin',(116.959178380441,7.2,51.0204257716897));
#187810=CARTESIAN_POINT('Origin',(114.229876286196,7.2,63.489152394136));
#187811=CARTESIAN_POINT('',(114.107236013427,7.7,64.1200787534334));
#187812=CARTESIAN_POINT('',(114.041413185149,7.7,64.4587061591514));
#187813=CARTESIAN_POINT('',(114.107236013427,7.7,64.1200787534334));
#187814=CARTESIAN_POINT('Origin',(116.664690278911,1.45439216225896E-14,
50.9631827978201));
#187815=CARTESIAN_POINT('Origin',(116.664690278911,1.45439216225896E-14,
50.9631827978201));
#187816=CARTESIAN_POINT('Origin',(114.229876286196,7.7,63.489152394136));
#187817=CARTESIAN_POINT('',(113.620340466169,7.7,64.0045177649381));
#187818=CARTESIAN_POINT('',(113.554419184017,7.7,64.3436516693999));
#187819=CARTESIAN_POINT('',(113.620340466169,7.7,64.0045177649381));
#187820=CARTESIAN_POINT('Origin',(116.959178380441,7.7,51.0204257716897));
#187821=CARTESIAN_POINT('Origin',(116.959178380441,7.7,51.0204257716897));
#187822=CARTESIAN_POINT('Origin',(113.739062783647,7.7,63.3937474376868));
#187823=CARTESIAN_POINT('Origin',(116.173876776362,1.45439216225896E-14,
50.8677778413709));
#187824=CARTESIAN_POINT('Origin',(116.173876776362,1.45439216225896E-14,
50.8677778413709));
#187825=CARTESIAN_POINT('Origin',(114.720689788746,7.2,63.5845573505853));
#187826=CARTESIAN_POINT('',(115.039163337421,7.2,64.5665700844302));
#187827=CARTESIAN_POINT('',(114.974564658518,7.2,64.8988998189938));
#187828=CARTESIAN_POINT('',(115.039163337421,7.2,64.5665700844302));
#187829=CARTESIAN_POINT('',(114.545209642576,7.2,64.4873199362524));
#187830=CARTESIAN_POINT('Origin',(116.959178380441,7.2,51.0204257716897));
#187831=CARTESIAN_POINT('',(114.48068680041,7.2,64.8192595265691));
#187832=CARTESIAN_POINT('',(114.545209642576,7.2,64.4873199362524));
#187833=CARTESIAN_POINT('Origin',(116.959178380441,7.2,51.0204257716897));
#187834=CARTESIAN_POINT('Origin',(115.211503291295,7.2,63.6799623070345));
#187835=CARTESIAN_POINT('',(115.091711844631,7.7,64.2962327996897));
#187836=CARTESIAN_POINT('',(115.025817457352,7.7,64.635228342716));
#187837=CARTESIAN_POINT('',(115.091711844631,7.7,64.2962327996897));
#187838=CARTESIAN_POINT('Origin',(117.64631728401,1.45439216225896E-14,
51.1539927107186));
#187839=CARTESIAN_POINT('Origin',(117.64631728401,1.45439216225896E-14,
51.1539927107186));
#187840=CARTESIAN_POINT('Origin',(115.211503291295,7.7,63.6799623070345));
#187841=CARTESIAN_POINT('',(114.597693635811,7.7,64.2173145454823));
#187842=CARTESIAN_POINT('',(114.531879736022,7.7,64.5558960183304));
#187843=CARTESIAN_POINT('',(114.597693635811,7.7,64.2173145454823));
#187844=CARTESIAN_POINT('Origin',(116.959178380441,7.7,51.0204257716897));
#187845=CARTESIAN_POINT('Origin',(116.959178380441,7.7,51.0204257716897));
#187846=CARTESIAN_POINT('Origin',(114.720689788746,7.7,63.5845573505853));
#187847=CARTESIAN_POINT('Origin',(117.155503781461,1.45439216225896E-14,
51.0585877542694));
#187848=CARTESIAN_POINT('Origin',(117.155503781461,1.45439216225896E-14,
51.0585877542694));
#187849=CARTESIAN_POINT('Origin',(115.702316793845,7.2,63.7753672634838));
#187850=CARTESIAN_POINT('',(116.037602325903,7.2,64.6708902723069));
#187851=CARTESIAN_POINT('',(115.972594617792,7.2,65.0053242692244));
#187852=CARTESIAN_POINT('',(116.037602325903,7.2,64.6708902723069));
#187853=CARTESIAN_POINT('',(115.536618587108,7.2,64.6278063844825));
#187854=CARTESIAN_POINT('Origin',(116.959178380441,7.2,51.0204257716897));
#187855=CARTESIAN_POINT('',(115.471858926109,7.2,64.9609642959974));
#187856=CARTESIAN_POINT('',(115.536618587108,7.2,64.6278063844825));
#187857=CARTESIAN_POINT('Origin',(116.959178380441,7.2,51.0204257716897));
#187858=CARTESIAN_POINT('Origin',(116.193130296394,7.2,63.870772219933));
#187859=CARTESIAN_POINT('',(116.090498972252,7.7,64.398761975897));
#187860=CARTESIAN_POINT('',(116.02417027306,7.7,64.7399918488676));
#187861=CARTESIAN_POINT('',(116.090498972252,7.7,64.398761975897));
#187862=CARTESIAN_POINT('Origin',(118.62794428911,1.45439216225896E-14,
51.3448026236171));
#187863=CARTESIAN_POINT('Origin',(118.62794428911,1.45439216225896E-14,
51.3448026236171));
#187864=CARTESIAN_POINT('Origin',(116.193130296394,7.7,63.870772219933));
#187865=CARTESIAN_POINT('',(115.589304075579,7.7,64.3567643957619));
#187866=CARTESIAN_POINT('',(115.523238795715,7.7,64.6966391005331));
#187867=CARTESIAN_POINT('',(115.589304075579,7.7,64.3567643957619));
#187868=CARTESIAN_POINT('Origin',(116.959178380441,7.7,51.0204257716897));
#187869=CARTESIAN_POINT('Origin',(116.959178380441,7.7,51.0204257716897));
#187870=CARTESIAN_POINT('Origin',(115.702316793845,7.7,63.7753672634838));
#187871=CARTESIAN_POINT('Origin',(118.13713078656,1.45439216225896E-14,
51.2493976671679));
#187872=CARTESIAN_POINT('Origin',(118.13713078656,1.45439216225896E-14,
51.2493976671679));
#187873=CARTESIAN_POINT('Origin',(116.683943798944,7.2,63.9661771763823));
#187874=CARTESIAN_POINT('',(117.050338122776,7.2,64.7016601241992));
#187875=CARTESIAN_POINT('',(116.984559900636,7.2,65.040058052371));
#187876=CARTESIAN_POINT('',(117.050338122776,7.2,64.7016601241992));
#187877=CARTESIAN_POINT('',(116.54215633591,7.2,64.695606798692));
#187878=CARTESIAN_POINT('Origin',(116.959178380441,7.2,51.0204257716897));
#187879=CARTESIAN_POINT('',(116.476810507479,7.2,65.0317802651764));
#187880=CARTESIAN_POINT('',(116.54215633591,7.2,64.695606798692));
#187881=CARTESIAN_POINT('Origin',(116.959178380441,7.2,51.0204257716897));
#187882=CARTESIAN_POINT('Origin',(117.174757301493,7.2,64.0615821328315));
#187883=CARTESIAN_POINT('',(117.103891411332,7.7,64.4261537133422));
#187884=CARTESIAN_POINT('',(117.036743654029,7.7,64.7715972539806));
#187885=CARTESIAN_POINT('',(117.103891411332,7.7,64.4261537133422));
#187886=CARTESIAN_POINT('Origin',(119.609571294209,1.45439216225896E-14,
51.5356125365156));
#187887=CARTESIAN_POINT('Origin',(119.609571294209,1.45439216225896E-14,
51.5356125365156));
#187888=CARTESIAN_POINT('Origin',(117.174757301493,7.7,64.0615821328315));
#187889=CARTESIAN_POINT('',(116.595340998606,7.7,64.421996794018));
#187890=CARTESIAN_POINT('',(116.528653025038,7.7,64.7650749642014));
#187891=CARTESIAN_POINT('',(116.595340998606,7.7,64.421996794018));
#187892=CARTESIAN_POINT('Origin',(116.959178380441,7.7,51.0204257716897));
#187893=CARTESIAN_POINT('Origin',(116.959178380441,7.7,51.0204257716897));
#187894=CARTESIAN_POINT('Origin',(116.683943798944,7.7,63.9661771763823));
#187895=CARTESIAN_POINT('Origin',(119.118757791659,1.45439216225896E-14,
51.4402075800664));
#187896=CARTESIAN_POINT('Origin',(119.118757791659,1.45439216225896E-14,
51.4402075800664));
#187897=CARTESIAN_POINT('Origin',(117.665570804043,7.2,64.1569870892808));
#187898=CARTESIAN_POINT('',(118.077901556091,7.2,64.6561487801456));
#187899=CARTESIAN_POINT('',(118.010952010662,7.2,65.0005726141802));
#187900=CARTESIAN_POINT('',(118.077901556091,7.2,64.6561487801456));
#187901=CARTESIAN_POINT('',(117.562222158485,7.2,64.6886671256));
#187902=CARTESIAN_POINT('Origin',(116.959178380441,7.2,51.0204257716897));
#187903=CARTESIAN_POINT('',(117.495911727413,7.2,65.0298030177092));
#187904=CARTESIAN_POINT('',(117.562222158485,7.2,64.6886671256));
#187905=CARTESIAN_POINT('Origin',(116.959178380441,7.2,51.0204257716897));
#187906=CARTESIAN_POINT('Origin',(118.156384306592,7.2,64.25239204573));
#187907=CARTESIAN_POINT('',(118.132455171377,7.7,64.375496160079));
#187908=CARTESIAN_POINT('',(118.06405996519,7.7,64.7273572368534));
#187909=CARTESIAN_POINT('',(118.132455171377,7.7,64.375496160079));
#187910=CARTESIAN_POINT('Origin',(120.591198299308,1.45439216225896E-14,
51.7264224494141));
#187911=CARTESIAN_POINT('Origin',(120.591198299308,1.45439216225896E-14,
51.7264224494141));
#187912=CARTESIAN_POINT('Origin',(118.156384306592,7.7,64.25239204573));
#187913=CARTESIAN_POINT('',(117.616229642986,7.7,64.4108240908324));
#187914=CARTESIAN_POINT('',(117.548515439084,7.7,64.7591817320498));
#187915=CARTESIAN_POINT('',(117.616229642986,7.7,64.4108240908324));
#187916=CARTESIAN_POINT('Origin',(116.959178380441,7.7,51.0204257716897));
#187917=CARTESIAN_POINT('Origin',(116.959178380441,7.7,51.0204257716897));
#187918=CARTESIAN_POINT('Origin',(117.665570804043,7.7,64.1569870892808));
#187919=CARTESIAN_POINT('Origin',(120.100384796758,1.45439216225896E-14,
51.6310174929649));
#187920=CARTESIAN_POINT('Origin',(120.100384796758,1.45439216225896E-14,
51.6310174929649));
#187921=CARTESIAN_POINT('Origin',(118.647197809142,7.2,64.3477970021793));
#187922=CARTESIAN_POINT('',(119.121125941224,7.2,64.5300692255833));
#187923=CARTESIAN_POINT('',(119.05253957496,7.2,64.8829137307956));
#187924=CARTESIAN_POINT('',(119.121125941224,7.2,64.5300692255833));
#187925=CARTESIAN_POINT('',(118.597490268611,7.2,64.6035188533173));
#187926=CARTESIAN_POINT('Origin',(116.959178380441,7.2,51.0204257716897));
#187927=CARTESIAN_POINT('',(118.529785785263,7.2,64.9518264868721));
#187928=CARTESIAN_POINT('',(118.597490268611,7.2,64.6035188533173));
#187929=CARTESIAN_POINT('Origin',(116.959178380441,7.2,51.0204257716897));
#187930=CARTESIAN_POINT('Origin',(119.138011311691,7.2,64.4432019586286));
#187931=CARTESIAN_POINT('',(119.138011311691,7.7,64.4432019586286));
#187932=CARTESIAN_POINT('',(119.10693856578,7.7,64.6030565806735));
#187933=CARTESIAN_POINT('',(119.138011311691,7.7,64.4432019586286));
#187934=CARTESIAN_POINT('',(119.138011311691,7.35569507252702,64.4432019586286));
#187935=CARTESIAN_POINT('',(119.138011311691,7.35569507252702,64.4432019586286));
#187936=CARTESIAN_POINT('Origin',(121.572825304407,1.45439216225896E-14,
51.9172323623126));
#187937=CARTESIAN_POINT('Origin',(121.572825304407,1.45439216225896E-14,
51.9172323623126));
#187938=CARTESIAN_POINT('Origin',(119.138011311691,7.7,64.4432019586286));
#187939=CARTESIAN_POINT('',(118.647197809142,7.7,64.3477970021793));
#187940=CARTESIAN_POINT('',(118.58348926054,7.7,64.6755474361724));
#187941=CARTESIAN_POINT('',(118.647197809142,7.7,64.3477970021793));
#187942=CARTESIAN_POINT('',(119.138011311691,7.7,64.4432019586286));
#187943=CARTESIAN_POINT('Origin',(116.959178380441,7.7,51.0204257716897));
#187944=CARTESIAN_POINT('Origin',(118.647197809142,7.7,64.3477970021793));
#187945=CARTESIAN_POINT('',(118.647197809142,7.65220556441102,64.3477970021793));
#187946=CARTESIAN_POINT('Origin',(121.082011801857,1.45439216225896E-14,
51.8218274058634));
#187947=CARTESIAN_POINT('',(118.647197809142,7.7,64.3477970021793));
#187948=CARTESIAN_POINT('Origin',(121.082011801857,1.45439216225896E-14,
51.8218274058634));
#187949=CARTESIAN_POINT('Origin',(118.450872408122,7.,64.3096350195996));
#187950=CARTESIAN_POINT('Origin',(114.524364387726,1.45439216225896E-14,
63.5463953680056));
#187951=CARTESIAN_POINT('Origin',(121.592078824439,4.7,64.9202267408748));
#187952=CARTESIAN_POINT('',(121.542371283908,4.2,65.1759485920128));
#187953=CARTESIAN_POINT('',(121.47466680056,4.2,65.5242562255676));
#187954=CARTESIAN_POINT('',(121.542371283908,4.2,65.1759485920128));
#187955=CARTESIAN_POINT('',(121.575193453972,4.7,65.0070940078296));
#187956=CARTESIAN_POINT('Origin',(124.026892817154,1.45439216225896E-14,
52.3942571445589));
#187957=CARTESIAN_POINT('',(121.506607087708,4.7,65.3599385130419));
#187958=CARTESIAN_POINT('',(121.575193453972,4.7,65.0070940078296));
#187959=CARTESIAN_POINT('Origin',(124.026892817154,1.45439216225896E-14,
52.3942571445589));
#187960=CARTESIAN_POINT('Origin',(121.592078824439,4.2,64.9202267408748));
#187961=CARTESIAN_POINT('',(122.082892326988,4.2,65.0156316973241));
#187962=CARTESIAN_POINT('',(122.019183778387,4.2,65.3433821313171));
#187963=CARTESIAN_POINT('',(122.082892326988,4.2,65.0156316973241));
#187964=CARTESIAN_POINT('',(122.035976018321,4.2,65.0065120452323));
#187965=CARTESIAN_POINT('',(122.035976018321,4.2,65.0065120452323));
#187966=CARTESIAN_POINT('Origin',(116.959178380441,4.2,51.0204257716897));
#187967=CARTESIAN_POINT('Origin',(116.959178380441,4.2,51.0204257716897));
#187968=CARTESIAN_POINT('Origin',(122.082892326988,4.2,65.0156316973241));
#187969=CARTESIAN_POINT('',(122.082892326988,4.7,65.0156316973241));
#187970=CARTESIAN_POINT('',(122.051819581077,4.7,65.175486319369));
#187971=CARTESIAN_POINT('',(122.082892326988,4.7,65.0156316973241));
#187972=CARTESIAN_POINT('',(122.082892326988,4.2,65.0156316973241));
#187973=CARTESIAN_POINT('Origin',(124.517706319704,1.45439216225896E-14,
52.4896621010082));
#187974=CARTESIAN_POINT('Origin',(122.082892326988,4.7,65.0156316973241));
#187975=CARTESIAN_POINT('',(121.744913312192,4.7,64.9499349041024));
#187976=CARTESIAN_POINT('Origin',(116.959178380441,4.7,51.0204257716897));
#187977=CARTESIAN_POINT('',(122.082892326988,4.7,65.0156316973241));
#187978=CARTESIAN_POINT('Origin',(116.959178380441,4.7,51.0204257716897));
#187979=CARTESIAN_POINT('Origin',(121.395753423419,4.,64.8820647582951));
#187980=CARTESIAN_POINT('Origin',(114.524364387726,1.45439216225896E-14,
63.5463953680056));
#187981=CARTESIAN_POINT('Origin',(121.592078824439,3.2,64.9202267408748));
#187982=CARTESIAN_POINT('',(122.033551165931,3.2,65.2694686988757));
#187983=CARTESIAN_POINT('',(121.96583696203,3.2,65.6178263400931));
#187984=CARTESIAN_POINT('',(122.033551165931,3.2,65.2694686988757));
#187985=CARTESIAN_POINT('',(121.488730178881,3.2,65.451906777194));
#187986=CARTESIAN_POINT('Origin',(116.959178380441,3.2,51.0204257716897));
#187987=CARTESIAN_POINT('',(121.422419747809,3.2,65.7930426693032));
#187988=CARTESIAN_POINT('',(121.488730178881,3.2,65.451906777194));
#187989=CARTESIAN_POINT('Origin',(116.959178380441,3.2,51.0204257716897));
#187990=CARTESIAN_POINT('Origin',(122.082892326988,3.2,65.0156316973241));
#187991=CARTESIAN_POINT('',(122.058963191773,3.7,65.138735811673));
#187992=CARTESIAN_POINT('',(121.990567985586,3.7,65.4905968884474));
#187993=CARTESIAN_POINT('',(122.058963191773,3.7,65.138735811673));
#187994=CARTESIAN_POINT('Origin',(124.517706319704,1.45439216225896E-14,
52.4896621010082));
#187995=CARTESIAN_POINT('Origin',(124.517706319704,1.45439216225896E-14,
52.4896621010082));
#187996=CARTESIAN_POINT('Origin',(122.082892326988,3.7,65.0156316973241));
#187997=CARTESIAN_POINT('',(121.513596073938,3.7,65.3239834752904));
#187998=CARTESIAN_POINT('',(121.446646528509,3.7,65.6684073093249));
#187999=CARTESIAN_POINT('',(121.513596073938,3.7,65.3239834752904));
#188000=CARTESIAN_POINT('Origin',(116.959178380441,3.7,51.0204257716897));
#188001=CARTESIAN_POINT('Origin',(116.959178380441,3.7,51.0204257716897));
#188002=CARTESIAN_POINT('Origin',(121.592078824439,3.7,64.9202267408748));
#188003=CARTESIAN_POINT('Origin',(124.026892817154,1.45439216225896E-14,
52.3942571445589));
#188004=CARTESIAN_POINT('Origin',(124.026892817154,1.45439216225896E-14,
52.3942571445589));
#188005=CARTESIAN_POINT('Origin',(121.592078824439,2.2,64.9202267408748));
#188006=CARTESIAN_POINT('',(121.994289526651,2.2,65.4714513149597));
#188007=CARTESIAN_POINT('',(121.927601553083,2.2,65.8145294851432));
#188008=CARTESIAN_POINT('',(121.994289526651,2.2,65.4714513149597));
#188009=CARTESIAN_POINT('',(121.450291361405,2.2,65.6496563631845));
#188010=CARTESIAN_POINT('Origin',(116.959178380441,2.2,51.0204257716897));
#188011=CARTESIAN_POINT('',(121.384945532974,2.2,65.9858298296689));
#188012=CARTESIAN_POINT('',(121.450291361405,2.2,65.6496563631845));
#188013=CARTESIAN_POINT('Origin',(116.959178380441,2.2,51.0204257716897));
#188014=CARTESIAN_POINT('Origin',(122.082892326988,2.2,65.0156316973241));
#188015=CARTESIAN_POINT('',(122.012026436827,2.7,65.3802032778347));
#188016=CARTESIAN_POINT('',(121.944878679524,2.7,65.7256468184731));
#188017=CARTESIAN_POINT('',(122.012026436827,2.7,65.3802032778347));
#188018=CARTESIAN_POINT('Origin',(124.517706319704,1.45439216225896E-14,
52.4896621010082));
#188019=CARTESIAN_POINT('Origin',(124.517706319704,1.45439216225896E-14,
52.4896621010082));
#188020=CARTESIAN_POINT('Origin',(122.082892326988,2.7,65.0156316973241));
#188021=CARTESIAN_POINT('',(121.467659645721,2.7,65.5603047322425));
#188022=CARTESIAN_POINT('',(121.401881423582,2.7,65.8987026604143));
#188023=CARTESIAN_POINT('',(121.467659645721,2.7,65.5603047322425));
#188024=CARTESIAN_POINT('Origin',(116.959178380441,2.7,51.0204257716897));
#188025=CARTESIAN_POINT('Origin',(116.959178380441,2.7,51.0204257716897));
#188026=CARTESIAN_POINT('Origin',(121.592078824439,2.7,64.9202267408748));
#188027=CARTESIAN_POINT('Origin',(124.026892817154,1.45439216225896E-14,
52.3942571445589));
#188028=CARTESIAN_POINT('Origin',(124.026892817154,1.45439216225896E-14,
52.3942571445589));
#188029=CARTESIAN_POINT('Origin',(121.592078824439,1.2,64.9202267408748));
#188030=CARTESIAN_POINT('',(121.969879608722,1.2,65.5970288296021));
#188031=CARTESIAN_POINT('',(121.903814328859,1.2,65.9369035343734));
#188032=CARTESIAN_POINT('',(121.969879608722,1.2,65.5970288296021));
#188033=CARTESIAN_POINT('',(121.426380617702,1.2,65.7726658618735));
#188034=CARTESIAN_POINT('Origin',(116.959178380441,1.2,51.0204257716897));
#188035=CARTESIAN_POINT('',(121.361620956703,1.2,66.1058237733884));
#188036=CARTESIAN_POINT('',(121.426380617702,1.2,65.7726658618735));
#188037=CARTESIAN_POINT('Origin',(116.959178380441,1.2,51.0204257716897));
#188038=CARTESIAN_POINT('Origin',(122.082892326988,1.2,65.0156316973241));
#188039=CARTESIAN_POINT('',(121.980261002846,1.7,65.543621453288));
#188040=CARTESIAN_POINT('',(121.913932303654,1.7,65.8848513262587));
#188041=CARTESIAN_POINT('',(121.980261002846,1.7,65.543621453288));
#188042=CARTESIAN_POINT('Origin',(124.517706319704,1.45439216225896E-14,
52.4896621010082));
#188043=CARTESIAN_POINT('Origin',(124.517706319704,1.45439216225896E-14,
52.4896621010082));
#188044=CARTESIAN_POINT('Origin',(122.082892326988,1.7,65.0156316973241));
#188045=CARTESIAN_POINT('',(121.436550853948,1.7,65.7203447932486));
#188046=CARTESIAN_POINT('',(121.371543145836,1.7,66.0547787901662));
#188047=CARTESIAN_POINT('',(121.436550853948,1.7,65.7203447932486));
#188048=CARTESIAN_POINT('Origin',(116.959178380441,1.7,51.0204257716897));
#188049=CARTESIAN_POINT('Origin',(116.959178380441,1.7,51.0204257716897));
#188050=CARTESIAN_POINT('Origin',(121.592078824439,1.7,64.9202267408748));
#188051=CARTESIAN_POINT('Origin',(124.026892817154,1.45439216225896E-14,
52.3942571445589));
#188052=CARTESIAN_POINT('Origin',(124.026892817154,1.45439216225896E-14,
52.3942571445589));
#188053=CARTESIAN_POINT('Origin',(121.592078824439,0.200000000000015,64.9202267408748));
#188054=CARTESIAN_POINT('',(121.959896174053,0.200000000000015,65.6483888922211));
#188055=CARTESIAN_POINT('',(121.894082274265,0.200000000000015,65.9869703650692));
#188056=CARTESIAN_POINT('',(121.959896174053,0.200000000000015,65.6483888922211));
#188057=CARTESIAN_POINT('',(121.416598678269,0.200000000000015,65.822989326542));
#188058=CARTESIAN_POINT('Origin',(116.959178380441,0.200000000000015,51.0204257716897));
#188059=CARTESIAN_POINT('',(121.352075836103,0.200000000000015,66.1549289168586));
#188060=CARTESIAN_POINT('',(121.416598678269,0.200000000000015,65.822989326542));
#188061=CARTESIAN_POINT('Origin',(116.959178380441,0.200000000000015,51.0204257716897));
#188062=CARTESIAN_POINT('Origin',(122.082892326988,0.200000000000015,65.0156316973241));
#188063=CARTESIAN_POINT('',(121.963100880324,0.700000000000015,65.6319021899793));
#188064=CARTESIAN_POINT('',(121.897206493045,0.700000000000015,65.9708977330055));
#188065=CARTESIAN_POINT('',(121.963100880324,0.700000000000015,65.6319021899793));
#188066=CARTESIAN_POINT('Origin',(124.517706319704,1.45439216225896E-14,
52.4896621010082));
#188067=CARTESIAN_POINT('Origin',(124.517706319704,1.45439216225896E-14,
52.4896621010082));
#188068=CARTESIAN_POINT('Origin',(122.082892326988,0.700000000000015,65.0156316973241));
#188069=CARTESIAN_POINT('',(121.419738870565,0.700000000000015,65.8068345182705));
#188070=CARTESIAN_POINT('',(121.355140191661,0.700000000000015,66.1391642528341));
#188071=CARTESIAN_POINT('',(121.419738870565,0.700000000000015,65.8068345182705));
#188072=CARTESIAN_POINT('Origin',(116.959178380441,0.700000000000015,51.0204257716897));
#188073=CARTESIAN_POINT('Origin',(116.959178380441,0.700000000000015,51.0204257716897));
#188074=CARTESIAN_POINT('Origin',(121.592078824439,0.700000000000015,64.9202267408748));
#188075=CARTESIAN_POINT('Origin',(124.026892817154,1.45439216225896E-14,
52.3942571445589));
#188076=CARTESIAN_POINT('Origin',(124.026892817154,1.45439216225896E-14,
52.3942571445589));
#188077=CARTESIAN_POINT('Origin',(108.830927758152,0.200000000000015,62.4396978731943));
#188078=CARTESIAN_POINT('',(108.985574283718,0.200000000000015,64.264523370831));
#188079=CARTESIAN_POINT('',(108.924710285017,0.200000000000015,64.5776399372382));
#188080=CARTESIAN_POINT('',(108.985574283718,0.200000000000015,64.264523370831));
#188081=CARTESIAN_POINT('',(108.53146510291,0.200000000000015,63.9802919908596));
#188082=CARTESIAN_POINT('Origin',(116.959178380441,0.200000000000015,51.0204257716897));
#188083=CARTESIAN_POINT('',(108.469801984318,0.200000000000015,64.2975196521962));
#188084=CARTESIAN_POINT('',(108.53146510291,0.200000000000015,63.9802919908596));
#188085=CARTESIAN_POINT('Origin',(116.959178380441,0.200000000000015,51.0204257716897));
#188086=CARTESIAN_POINT('Origin',(109.321741260701,0.200000000000015,62.5351028296435));
#188087=CARTESIAN_POINT('',(108.988532178342,0.700000000000015,64.2493063981041));
#188088=CARTESIAN_POINT('',(108.927604540738,0.700000000000015,64.5627503566519));
#188089=CARTESIAN_POINT('',(108.988532178342,0.700000000000015,64.2493063981041));
#188090=CARTESIAN_POINT('Origin',(111.756555253416,1.45439216225896E-14,
50.0091332333276));
#188091=CARTESIAN_POINT('Origin',(111.756555253416,1.45439216225896E-14,
50.0091332333276));
#188092=CARTESIAN_POINT('Origin',(109.321741260701,0.700000000000015,62.5351028296435));
#188093=CARTESIAN_POINT('',(108.534462746944,0.700000000000015,63.9648705261644));
#188094=CARTESIAN_POINT('',(108.472733446567,0.700000000000015,64.2824386615687));
#188095=CARTESIAN_POINT('',(108.534462746944,0.700000000000015,63.9648705261644));
#188096=CARTESIAN_POINT('Origin',(116.959178380441,0.700000000000015,51.0204257716897));
#188097=CARTESIAN_POINT('Origin',(116.959178380441,0.700000000000015,51.0204257716897));
#188098=CARTESIAN_POINT('Origin',(108.830927758152,0.700000000000015,62.4396978731943));
#188099=CARTESIAN_POINT('Origin',(111.265741750867,1.45439216225896E-14,
49.9137282768784));
#188100=CARTESIAN_POINT('Origin',(111.265741750867,1.45439216225896E-14,
49.9137282768784));
#188101=CARTESIAN_POINT('Origin',(108.830927758152,1.2,62.4396978731943));
#188102=CARTESIAN_POINT('',(108.994787025916,1.2,64.217128157474));
#188103=CARTESIAN_POINT('',(108.933724381216,1.2,64.5312666638533));
#188104=CARTESIAN_POINT('',(108.994787025916,1.2,64.217128157474));
#188105=CARTESIAN_POINT('',(108.540801935833,1.2,63.932258389249));
#188106=CARTESIAN_POINT('Origin',(116.959178380441,1.2,51.0204257716897));
#188107=CARTESIAN_POINT('',(108.478932215543,1.2,64.2505489188773));
#188108=CARTESIAN_POINT('',(108.540801935833,1.2,63.932258389249));
#188109=CARTESIAN_POINT('Origin',(116.959178380441,1.2,51.0204257716897));
#188110=CARTESIAN_POINT('Origin',(109.321741260701,1.2,62.5351028296435));
#188111=CARTESIAN_POINT('',(109.004361305076,1.7,64.1678730069675));
#188112=CARTESIAN_POINT('',(108.943090855225,1.7,64.4830805728385));
#188113=CARTESIAN_POINT('',(109.004361305076,1.7,64.1678730069675));
#188114=CARTESIAN_POINT('Origin',(111.756555253416,1.45439216225896E-14,
50.0091332333276));
#188115=CARTESIAN_POINT('Origin',(111.756555253416,1.45439216225896E-14,
50.0091332333276));
#188116=CARTESIAN_POINT('Origin',(109.321741260701,1.7,62.5351028296435));
#188117=CARTESIAN_POINT('',(108.550506073729,1.7,63.8823351767978));
#188118=CARTESIAN_POINT('',(108.488420168295,1.7,64.2017378770224));
#188119=CARTESIAN_POINT('',(108.550506073729,1.7,63.8823351767978));
#188120=CARTESIAN_POINT('Origin',(116.959178380441,1.7,51.0204257716897));
#188121=CARTESIAN_POINT('Origin',(116.959178380441,1.7,51.0204257716897));
#188122=CARTESIAN_POINT('Origin',(108.830927758152,1.7,62.4396978731943));
#188123=CARTESIAN_POINT('Origin',(111.265741750867,1.45439216225896E-14,
49.9137282768784));
#188124=CARTESIAN_POINT('Origin',(111.265741750867,1.45439216225896E-14,
49.9137282768784));
#188125=CARTESIAN_POINT('Origin',(108.830927758152,2.2,62.4396978731943));
#188126=CARTESIAN_POINT('',(109.017289821827,2.2,64.1013618861081));
#188127=CARTESIAN_POINT('',(108.955736534662,2.2,64.4180245165501));
#188128=CARTESIAN_POINT('',(109.017289821827,2.2,64.1013618861081));
#188129=CARTESIAN_POINT('',(108.563611413924,2.2,63.814914382713));
#188130=CARTESIAN_POINT('Origin',(116.959178380441,2.2,51.0204257716897));
#188131=CARTESIAN_POINT('',(108.501231170594,2.2,64.1358313125929));
#188132=CARTESIAN_POINT('',(108.563611413924,2.2,63.814914382713));
#188133=CARTESIAN_POINT('Origin',(116.959178380441,2.2,51.0204257716897));
#188134=CARTESIAN_POINT('Origin',(109.321741260701,2.2,62.5351028296435));
#188135=CARTESIAN_POINT('',(109.03362035359,2.7,64.0173490025909));
#188136=CARTESIAN_POINT('',(108.971706090658,2.7,64.3358686830996));
#188137=CARTESIAN_POINT('',(109.03362035359,2.7,64.0173490025909));
#188138=CARTESIAN_POINT('Origin',(111.756555253416,1.45439216225896E-14,
50.0091332333276));
#188139=CARTESIAN_POINT('Origin',(111.756555253416,1.45439216225896E-14,
50.0091332333276));
#188140=CARTESIAN_POINT('Origin',(109.321741260701,2.7,62.5351028296435));
#188141=CARTESIAN_POINT('',(108.580167748568,2.7,63.7297398498768));
#188142=CARTESIAN_POINT('',(108.517411692007,2.7,64.0525901615711));
#188143=CARTESIAN_POINT('',(108.580167748568,2.7,63.7297398498768));
#188144=CARTESIAN_POINT('Origin',(116.959178380441,2.7,51.0204257716897));
#188145=CARTESIAN_POINT('Origin',(116.959178380441,2.7,51.0204257716897));
#188146=CARTESIAN_POINT('Origin',(108.830927758152,2.7,62.4396978731943));
#188147=CARTESIAN_POINT('Origin',(111.265741750867,1.45439216225896E-14,
49.9137282768784));
#188148=CARTESIAN_POINT('Origin',(111.265741750867,1.45439216225896E-14,
49.9137282768784));
#188149=CARTESIAN_POINT('Origin',(108.830927758152,3.2,62.4396978731943));
#188150=CARTESIAN_POINT('',(109.053414557622,3.2,63.9155171589135));
#188151=CARTESIAN_POINT('',(108.991057104461,3.2,64.2363168441179));
#188152=CARTESIAN_POINT('',(109.053414557622,3.2,63.9155171589135));
#188153=CARTESIAN_POINT('',(108.60023938276,3.2,63.6264807588764));
#188154=CARTESIAN_POINT('Origin',(116.959178380441,3.2,51.0204257716897));
#188155=CARTESIAN_POINT('',(108.537021672699,3.2,63.9517060600868));
#188156=CARTESIAN_POINT('',(108.60023938276,3.2,63.6264807588764));
#188157=CARTESIAN_POINT('Origin',(116.959178380441,3.2,51.0204257716897));
#188158=CARTESIAN_POINT('Origin',(109.321741260701,3.2,62.5351028296435));
#188159=CARTESIAN_POINT('',(109.076749185361,3.7,63.7954715051251));
#188160=CARTESIAN_POINT('',(109.013861148526,3.7,64.1190007930822));
#188161=CARTESIAN_POINT('',(109.076749185361,3.7,63.7954715051251));
#188162=CARTESIAN_POINT('Origin',(111.756555253416,1.45439216225896E-14,
50.0091332333276));
#188163=CARTESIAN_POINT('Origin',(111.756555253416,1.45439216225896E-14,
50.0091332333276));
#188164=CARTESIAN_POINT('Origin',(109.321741260701,3.7,62.5351028296435));
#188165=CARTESIAN_POINT('',(108.623906438908,3.7,63.5047249177198));
#188166=CARTESIAN_POINT('',(108.560135680847,3.7,63.8327953900438));
#188167=CARTESIAN_POINT('',(108.623906438908,3.7,63.5047249177198));
#188168=CARTESIAN_POINT('Origin',(116.959178380441,3.7,51.0204257716897));
#188169=CARTESIAN_POINT('Origin',(116.959178380441,3.7,51.0204257716897));
#188170=CARTESIAN_POINT('Origin',(108.830927758152,3.7,62.4396978731943));
#188171=CARTESIAN_POINT('Origin',(111.265741750867,1.45439216225896E-14,
49.9137282768784));
#188172=CARTESIAN_POINT('Origin',(111.265741750867,1.45439216225896E-14,
49.9137282768784));
#188173=CARTESIAN_POINT('Origin',(108.830927758152,4.2,62.4396978731943));
#188174=CARTESIAN_POINT('',(109.103717660933,4.2,63.6567314181698));
#188175=CARTESIAN_POINT('',(109.040205187114,4.2,63.9834731398894));
#188176=CARTESIAN_POINT('',(109.103717660933,4.2,63.6567314181698));
#188177=CARTESIAN_POINT('',(108.651266555877,4.2,63.3639700204965));
#188178=CARTESIAN_POINT('Origin',(116.959178380441,4.2,51.0204257716897));
#188179=CARTESIAN_POINT('',(108.586844415053,4.2,63.695391549907));
#188180=CARTESIAN_POINT('',(108.651266555877,4.2,63.3639700204965));
#188181=CARTESIAN_POINT('Origin',(116.959178380441,4.2,51.0204257716897));
#188182=CARTESIAN_POINT('Origin',(109.321741260701,4.2,62.5351028296435));
#188183=CARTESIAN_POINT('',(109.134432104066,4.7,63.4987200949224));
#188184=CARTESIAN_POINT('',(109.070193363986,4.7,63.8291981140025));
#188185=CARTESIAN_POINT('',(109.134432104066,4.7,63.4987200949224));
#188186=CARTESIAN_POINT('Origin',(111.756555253416,1.45439216225896E-14,
50.0091332333276));
#188187=CARTESIAN_POINT('Origin',(111.756555253416,1.45439216225896E-14,
50.0091332333276));
#188188=CARTESIAN_POINT('Origin',(109.321741260701,4.7,62.5351028296435));
#188189=CARTESIAN_POINT('',(108.682437072072,4.7,63.2036124164553));
#188190=CARTESIAN_POINT('',(108.617256626478,4.7,63.5389350662436));
#188191=CARTESIAN_POINT('',(108.682437072072,4.7,63.2036124164553));
#188192=CARTESIAN_POINT('Origin',(116.959178380441,4.7,51.0204257716897));
#188193=CARTESIAN_POINT('Origin',(116.959178380441,4.7,51.0204257716897));
#188194=CARTESIAN_POINT('Origin',(108.830927758152,4.7,62.4396978731943));
#188195=CARTESIAN_POINT('Origin',(111.265741750867,1.45439216225896E-14,
49.9137282768784));
#188196=CARTESIAN_POINT('Origin',(111.265741750867,1.45439216225896E-14,
49.9137282768784));
#188197=CARTESIAN_POINT('Origin',(108.830927758152,5.2,62.4396978731943));
#188198=CARTESIAN_POINT('',(109.169025907263,5.2,63.3207512938729));
#188199=CARTESIAN_POINT('',(109.10394926914,5.2,63.6555399031828));
#188200=CARTESIAN_POINT('',(109.169025907263,5.2,63.3207512938729));
#188201=CARTESIAN_POINT('',(108.717557815134,5.2,63.0229327583325));
#188202=CARTESIAN_POINT('Origin',(116.959178380441,5.2,51.0204257716897));
#188203=CARTESIAN_POINT('',(108.651501562792,5.2,63.3627610207596));
#188204=CARTESIAN_POINT('',(108.717557815134,5.2,63.0229327583325));
#188205=CARTESIAN_POINT('Origin',(116.959178380441,5.2,51.0204257716897));
#188206=CARTESIAN_POINT('Origin',(109.321741260701,5.2,62.5351028296435));
#188207=CARTESIAN_POINT('',(109.207657018372,5.7,63.122012447834));
#188208=CARTESIAN_POINT('',(109.141618809976,5.7,63.4617478826739));
#188209=CARTESIAN_POINT('',(109.207657018372,5.7,63.122012447834));
#188210=CARTESIAN_POINT('Origin',(111.756555253416,1.45439216225896E-14,
50.0091332333276));
#188211=CARTESIAN_POINT('Origin',(111.756555253416,1.45439216225896E-14,
50.0091332333276));
#188212=CARTESIAN_POINT('Origin',(109.321741260701,5.7,62.5351028296435));
#188213=CARTESIAN_POINT('',(108.756794667777,5.7,62.821077657805));
#188214=CARTESIAN_POINT('',(108.689732073798,5.7,63.166083073309));
#188215=CARTESIAN_POINT('',(108.756794667777,5.7,62.821077657805));
#188216=CARTESIAN_POINT('Origin',(116.959178380441,5.7,51.0204257716897));
#188217=CARTESIAN_POINT('Origin',(116.959178380441,5.7,51.0204257716897));
#188218=CARTESIAN_POINT('Origin',(108.830927758152,5.7,62.4396978731943));
#188219=CARTESIAN_POINT('Origin',(111.265741750867,1.45439216225896E-14,
49.9137282768784));
#188220=CARTESIAN_POINT('Origin',(111.265741750867,1.45439216225896E-14,
49.9137282768784));
#188221=CARTESIAN_POINT('Origin',(108.634602357132,6.,62.4015358906146));
#188222=CARTESIAN_POINT('',(109.031966112671,6.7,62.4787759657038));
#188223=CARTESIAN_POINT('',(108.830927758152,6.7,62.4396978731943));
#188224=CARTESIAN_POINT('',(109.031966112671,6.7,62.4787759657038));
#188225=CARTESIAN_POINT('',(108.830927758152,6.52351515672301,62.4396978731943));
#188226=CARTESIAN_POINT('',(108.830927758152,6.7,62.4396978731943));
#188227=CARTESIAN_POINT('Origin',(114.524364387726,1.45439216225896E-14,
63.5463953680056));
#188228=CARTESIAN_POINT('Origin',(108.830927758152,6.2,62.4396978731943));
#188229=CARTESIAN_POINT('',(109.250512137945,6.2,62.901543070532));
#188230=CARTESIAN_POINT('',(109.183373859264,6.2,63.2469378481324));
#188231=CARTESIAN_POINT('',(109.250512137945,6.2,62.901543070532));
#188232=CARTESIAN_POINT('',(108.800344146074,6.2,62.5970361323712));
#188233=CARTESIAN_POINT('Origin',(116.959178380441,6.2,51.0204257716897));
#188234=CARTESIAN_POINT('',(108.732128571959,6.2,62.9479730868615));
#188235=CARTESIAN_POINT('',(108.800344146074,6.2,62.5970361323712));
#188236=CARTESIAN_POINT('Origin',(116.959178380441,6.2,51.0204257716897));
#188237=CARTESIAN_POINT('Origin',(109.321741260701,6.2,62.5351028296435));
#188238=CARTESIAN_POINT('',(109.297812125485,6.7,62.6582069439925));
#188239=CARTESIAN_POINT('',(109.229416919299,6.7,63.0100680207669));
#188240=CARTESIAN_POINT('',(109.297812125485,6.7,62.6582069439925));
#188241=CARTESIAN_POINT('Origin',(111.756555253416,1.45439216225896E-14,
50.0091332333276));
#188242=CARTESIAN_POINT('Origin',(111.756555253416,1.45439216225896E-14,
50.0091332333276));
#188243=CARTESIAN_POINT('Origin',(109.321741260701,6.7,62.5351028296435));
#188244=CARTESIAN_POINT('',(108.77890411787,6.7,62.7073349651492));
#188245=CARTESIAN_POINT('',(108.830927758152,6.7,62.4396978731943));
#188246=CARTESIAN_POINT('Origin',(116.959178380441,6.7,51.0204257716897));
#188247=CARTESIAN_POINT('Origin',(116.959178380441,6.7,51.0204257716897));
#188248=CARTESIAN_POINT('Origin',(108.830927758152,6.7,62.4396978731943));
#188249=CARTESIAN_POINT('Origin',(111.265741750867,1.45439216225896E-14,
49.9137282768784));
#188250=CARTESIAN_POINT('Origin',(111.265741750867,1.45439216225896E-14,
49.9137282768784));
#188251=CARTESIAN_POINT('Origin',(109.812554763251,6.2,62.6305077860928));
#188252=CARTESIAN_POINT('',(110.163347709257,6.2,63.4462524643294));
#188253=CARTESIAN_POINT('',(110.09795814934,6.2,63.78265090868));
#188254=CARTESIAN_POINT('',(110.163347709257,6.2,63.4462524643294));
#188255=CARTESIAN_POINT('',(109.704906439227,6.2,63.1843076401468));
#188256=CARTESIAN_POINT('Origin',(116.959178380441,6.2,51.0204257716897));
#188257=CARTESIAN_POINT('',(109.638705300736,6.2,63.5248812734762));
#188258=CARTESIAN_POINT('',(109.704906439227,6.2,63.1843076401468));
#188259=CARTESIAN_POINT('Origin',(116.959178380441,6.2,51.0204257716897));
#188260=CARTESIAN_POINT('Origin',(110.3033682658,6.2,62.725912742542));
#188261=CARTESIAN_POINT('',(110.209360669591,6.7,63.2095374857282));
#188262=CARTESIAN_POINT('',(110.142811568378,6.7,63.5519012231441));
#188263=CARTESIAN_POINT('',(110.209360669591,6.7,63.2095374857282));
#188264=CARTESIAN_POINT('Origin',(112.738182258515,1.45439216225896E-14,
50.1999431462261));
#188265=CARTESIAN_POINT('Origin',(112.738182258515,1.45439216225896E-14,
50.1999431462261));
#188266=CARTESIAN_POINT('Origin',(110.3033682658,6.7,62.725912742542));
#188267=CARTESIAN_POINT('',(109.751516135199,6.7,62.9445227381437));
#188268=CARTESIAN_POINT('',(109.684110927497,6.7,63.2912907396567));
#188269=CARTESIAN_POINT('',(109.751516135199,6.7,62.9445227381437));
#188270=CARTESIAN_POINT('Origin',(116.959178380441,6.7,51.0204257716897));
#188271=CARTESIAN_POINT('Origin',(116.959178380441,6.7,51.0204257716897));
#188272=CARTESIAN_POINT('Origin',(109.812554763251,6.7,62.6305077860928));
#188273=CARTESIAN_POINT('Origin',(112.247368755966,1.45439216225896E-14,
50.1045381897769));
#188274=CARTESIAN_POINT('Origin',(112.247368755966,1.45439216225896E-14,
50.1045381897769));
#188275=CARTESIAN_POINT('Origin',(110.79418176835,6.2,62.8213176989913));
#188276=CARTESIAN_POINT('',(111.091791575357,6.2,63.9106645431981));
#188277=CARTESIAN_POINT('',(111.027693485939,6.2,64.2404189809629));
#188278=CARTESIAN_POINT('',(111.091791575357,6.2,63.9106645431981));
#188279=CARTESIAN_POINT('',(110.625684971198,6.2,63.6881542477025));
#188280=CARTESIAN_POINT('Origin',(116.959178380441,6.2,51.0204257716897));
#188281=CARTESIAN_POINT('',(110.560993238717,6.2,64.0209626990318));
#188282=CARTESIAN_POINT('',(110.625684971198,6.2,63.6881542477025));
#188283=CARTESIAN_POINT('Origin',(116.959178380441,6.2,51.0204257716897));
#188284=CARTESIAN_POINT('Origin',(111.284995270899,6.2,62.9167226554405));
#188285=CARTESIAN_POINT('',(111.136856952335,6.7,63.6788244340304));
#188286=CARTESIAN_POINT('',(111.071667833675,6.7,64.0141917026534));
#188287=CARTESIAN_POINT('',(111.136856952335,6.7,63.6788244340304));
#188288=CARTESIAN_POINT('Origin',(113.719809263614,1.45439216225896E-14,
50.3907530591246));
#188289=CARTESIAN_POINT('Origin',(113.719809263614,1.45439216225896E-14,
50.3907530591246));
#188290=CARTESIAN_POINT('Origin',(111.284995270899,6.7,62.9167226554405));
#188291=CARTESIAN_POINT('',(110.671185615415,6.7,63.4540748938883));
#188292=CARTESIAN_POINT('',(110.605371715626,6.7,63.7926563667364));
#188293=CARTESIAN_POINT('',(110.671185615415,6.7,63.4540748938883));
#188294=CARTESIAN_POINT('Origin',(116.959178380441,6.7,51.0204257716897));
#188295=CARTESIAN_POINT('Origin',(116.959178380441,6.7,51.0204257716897));
#188296=CARTESIAN_POINT('Origin',(110.79418176835,6.7,62.8213176989913));
#188297=CARTESIAN_POINT('Origin',(113.228995761065,1.45439216225896E-14,
50.2953481026754));
#188298=CARTESIAN_POINT('Origin',(113.228995761065,1.45439216225896E-14,
50.2953481026754));
#188299=CARTESIAN_POINT('Origin',(111.775808773449,6.2,63.0121276118898));
#188300=CARTESIAN_POINT('',(112.034909663219,6.2,64.2995846722948));
#188301=CARTESIAN_POINT('',(111.97171567341,6.2,64.6246879439969));
#188302=CARTESIAN_POINT('',(112.034909663219,6.2,64.2995846722948));
#188303=CARTESIAN_POINT('',(111.561562053474,6.2,64.114325935268));
#188304=CARTESIAN_POINT('Origin',(116.959178380441,6.2,51.0204257716897));
#188305=CARTESIAN_POINT('',(111.497961148835,6.2,64.4415225918465));
#188306=CARTESIAN_POINT('',(111.561562053474,6.2,64.114325935268));
#188307=CARTESIAN_POINT('Origin',(116.959178380441,6.2,51.0204257716897));
#188308=CARTESIAN_POINT('Origin',(112.266622275998,6.2,63.107532568339));
#188309=CARTESIAN_POINT('',(112.079313119363,6.7,64.0711498336179));
#188310=CARTESIAN_POINT('',(112.015074379284,6.7,64.401627852698));
#188311=CARTESIAN_POINT('',(112.079313119363,6.7,64.0711498336179));
#188312=CARTESIAN_POINT('Origin',(114.701436268713,1.45439216225896E-14,
50.5815629720231));
#188313=CARTESIAN_POINT('Origin',(114.701436268713,1.45439216225896E-14,
50.5815629720231));
#188314=CARTESIAN_POINT('Origin',(112.266622275998,6.7,63.107532568339));
#188315=CARTESIAN_POINT('',(111.606263280211,6.7,63.8843592073384));
#188316=CARTESIAN_POINT('',(111.54159696586,6.7,64.2170368943773));
#188317=CARTESIAN_POINT('',(111.606263280211,6.7,63.8843592073384));
#188318=CARTESIAN_POINT('Origin',(116.959178380441,6.7,51.0204257716897));
#188319=CARTESIAN_POINT('Origin',(116.959178380441,6.7,51.0204257716897));
#188320=CARTESIAN_POINT('Origin',(111.775808773449,6.7,63.0121276118898));
#188321=CARTESIAN_POINT('Origin',(114.210622766164,1.45439216225896E-14,
50.4861580155739));
#188322=CARTESIAN_POINT('Origin',(114.210622766164,1.45439216225896E-14,
50.4861580155739));
#188323=CARTESIAN_POINT('Origin',(112.757435778548,6.2,63.2029375247883));
#188324=CARTESIAN_POINT('',(112.992071921149,6.2,64.6162541704145));
#188325=CARTESIAN_POINT('',(112.929439325135,6.2,64.9384693358256));
#188326=CARTESIAN_POINT('',(112.992071921149,6.2,64.6162541704145));
#188327=CARTESIAN_POINT('',(112.511764478508,6.2,64.4668004909896));
#188328=CARTESIAN_POINT('Origin',(116.959178380441,6.2,51.0204257716897));
#188329=CARTESIAN_POINT('',(112.448892012004,6.2,64.7902496769364));
#188330=CARTESIAN_POINT('',(112.511764478508,6.2,64.4668004909896));
#188331=CARTESIAN_POINT('Origin',(116.959178380441,6.2,51.0204257716897));
#188332=CARTESIAN_POINT('Origin',(113.248249281097,6.2,63.2983424812375));
#188333=CARTESIAN_POINT('',(113.036064948792,6.7,64.3899307927943));
#188334=CARTESIAN_POINT('',(112.972415653174,6.7,64.7173763981386));
#188335=CARTESIAN_POINT('',(113.036064948792,6.7,64.3899307927943));
#188336=CARTESIAN_POINT('Origin',(115.683063273812,1.45439216225896E-14,
50.7723728849216));
#188337=CARTESIAN_POINT('Origin',(115.683063273812,1.45439216225896E-14,
50.7723728849216));
#188338=CARTESIAN_POINT('Origin',(113.248249281097,6.7,63.2983424812375));
#188339=CARTESIAN_POINT('',(112.555932818159,6.7,64.2395752157784));
#188340=CARTESIAN_POINT('',(112.492031730466,6.7,64.5683161725848));
#188341=CARTESIAN_POINT('',(112.555932818159,6.7,64.2395752157784));
#188342=CARTESIAN_POINT('Origin',(116.959178380441,6.7,51.0204257716897));
#188343=CARTESIAN_POINT('Origin',(116.959178380441,6.7,51.0204257716897));
#188344=CARTESIAN_POINT('Origin',(112.757435778548,6.7,63.2029375247883));
#188345=CARTESIAN_POINT('Origin',(115.192249771263,1.45439216225896E-14,
50.6769679284724));
#188346=CARTESIAN_POINT('Origin',(115.192249771263,1.45439216225896E-14,
50.6769679284724));
#188347=CARTESIAN_POINT('Origin',(113.739062783647,6.2,63.3937474376868));
#188348=CARTESIAN_POINT('',(113.962896812214,6.2,64.862635865129));
#188349=CARTESIAN_POINT('',(113.900508966606,6.2,65.1835919051392));
#188350=CARTESIAN_POINT('',(113.962896812214,6.2,64.862635865129));
#188351=CARTESIAN_POINT('',(113.475791658336,6.2,64.7481532038329));
#188352=CARTESIAN_POINT('Origin',(116.959178380441,6.2,51.0204257716897));
#188353=CARTESIAN_POINT('',(113.413320003765,6.2,65.0695404014283));
#188354=CARTESIAN_POINT('',(113.475791658336,6.2,64.7481532038329));
#188355=CARTESIAN_POINT('Origin',(116.959178380441,6.2,51.0204257716897));
#188356=CARTESIAN_POINT('Origin',(114.229876286196,6.2,63.489152394136));
#188357=CARTESIAN_POINT('',(114.006711044749,6.7,64.6372323040136));
#188358=CARTESIAN_POINT('',(113.943318565996,6.7,64.9633567077106));
#188359=CARTESIAN_POINT('',(114.006711044749,6.7,64.6372323040136));
#188360=CARTESIAN_POINT('Origin',(116.664690278911,1.45439216225896E-14,
50.9631827978201));
#188361=CARTESIAN_POINT('Origin',(116.664690278911,1.45439216225896E-14,
50.9631827978201));
#188362=CARTESIAN_POINT('Origin',(114.229876286196,6.7,63.489152394136));
#188363=CARTESIAN_POINT('',(113.519667105543,6.7,64.5224347220989));
#188364=CARTESIAN_POINT('',(113.456186697034,6.7,64.8490114829219));
#188365=CARTESIAN_POINT('',(113.519667105543,6.7,64.5224347220989));
#188366=CARTESIAN_POINT('Origin',(116.959178380441,6.7,51.0204257716897));
#188367=CARTESIAN_POINT('Origin',(116.959178380441,6.7,51.0204257716897));
#188368=CARTESIAN_POINT('Origin',(113.739062783647,6.7,63.3937474376868));
#188369=CARTESIAN_POINT('Origin',(116.173876776362,1.45439216225896E-14,
50.8677778413709));
#188370=CARTESIAN_POINT('Origin',(116.173876776362,1.45439216225896E-14,
50.8677778413709));
#188371=CARTESIAN_POINT('Origin',(114.720689788746,6.2,63.5845573505853));
#188372=CARTESIAN_POINT('',(114.947220292879,6.2,65.0395736830551));
#188373=CARTESIAN_POINT('',(114.884771528794,6.2,65.3608431198944));
#188374=CARTESIAN_POINT('',(114.947220292879,6.2,65.0395736830551));
#188375=CARTESIAN_POINT('',(114.453373444518,6.2,64.9597738601041));
#188376=CARTESIAN_POINT('Origin',(116.959178380441,6.2,51.0204257716897));
#188377=CARTESIAN_POINT('',(114.390993201188,6.2,65.2806907899839));
#188378=CARTESIAN_POINT('',(114.453373444518,6.2,64.9597738601041));
#188379=CARTESIAN_POINT('Origin',(116.959178380441,6.2,51.0204257716897));
#188380=CARTESIAN_POINT('Origin',(115.211503291295,6.2,63.6799623070345));
#188381=CARTESIAN_POINT('',(114.991079019732,6.7,64.8139412196562));
#188382=CARTESIAN_POINT('',(114.927622628352,6.7,65.140394423677));
#188383=CARTESIAN_POINT('',(114.991079019732,6.7,64.8139412196562));
#188384=CARTESIAN_POINT('Origin',(117.64631728401,1.45439216225896E-14,
51.1539927107186));
#188385=CARTESIAN_POINT('Origin',(117.64631728401,1.45439216225896E-14,
51.1539927107186));
#188386=CARTESIAN_POINT('Origin',(115.211503291295,6.7,63.6799623070345));
#188387=CARTESIAN_POINT('',(114.49718212478,6.7,64.734398862813));
#188388=CARTESIAN_POINT('',(114.433797621533,6.7,65.0604822362976));
#188389=CARTESIAN_POINT('',(114.49718212478,6.7,64.734398862813));
#188390=CARTESIAN_POINT('Origin',(116.959178380441,6.7,51.0204257716897));
#188391=CARTESIAN_POINT('Origin',(116.959178380441,6.7,51.0204257716897));
#188392=CARTESIAN_POINT('Origin',(114.720689788746,6.7,63.5845573505853));
#188393=CARTESIAN_POINT('Origin',(117.155503781461,1.45439216225896E-14,
51.0585877542694));
#188394=CARTESIAN_POINT('Origin',(117.155503781461,1.45439216225896E-14,
51.0585877542694));
#188395=CARTESIAN_POINT('Origin',(115.702316793845,6.2,63.7753672634838));
#188396=CARTESIAN_POINT('',(115.945083064097,6.2,65.146858236978));
#188397=CARTESIAN_POINT('',(115.882265002796,6.2,65.4700275338157));
#188398=CARTESIAN_POINT('',(115.945083064097,6.2,65.146858236978));
#188399=CARTESIAN_POINT('',(115.444448747065,6.2,65.1019767389875));
#188400=CARTESIAN_POINT('Origin',(116.959178380441,6.2,51.0204257716897));
#188401=CARTESIAN_POINT('',(115.381854583266,6.2,65.4239941887781));
#188402=CARTESIAN_POINT('',(115.444448747065,6.2,65.1019767389875));
#188403=CARTESIAN_POINT('Origin',(116.959178380441,6.2,51.0204257716897));
#188404=CARTESIAN_POINT('Origin',(116.193130296394,6.2,63.870772219933));
#188405=CARTESIAN_POINT('',(115.989211633983,6.7,64.9198375584453));
#188406=CARTESIAN_POINT('',(115.925367663769,6.7,65.2482846727662));
#188407=CARTESIAN_POINT('',(115.989211633983,6.7,64.9198375584453));
#188408=CARTESIAN_POINT('Origin',(118.62794428911,1.45439216225896E-14,
51.3448026236171));
#188409=CARTESIAN_POINT('Origin',(118.62794428911,1.45439216225896E-14,
51.3448026236171));
#188410=CARTESIAN_POINT('Origin',(116.193130296394,6.7,63.870772219933));
#188411=CARTESIAN_POINT('',(115.488413693631,6.7,64.8757978252638));
#188412=CARTESIAN_POINT('',(115.424804731494,6.7,65.2030359338696));
#188413=CARTESIAN_POINT('',(115.488413693631,6.7,64.8757978252638));
#188414=CARTESIAN_POINT('Origin',(116.959178380441,6.7,51.0204257716897));
#188415=CARTESIAN_POINT('Origin',(116.959178380441,6.7,51.0204257716897));
#188416=CARTESIAN_POINT('Origin',(115.702316793845,6.7,63.7753672634838));
#188417=CARTESIAN_POINT('Origin',(118.13713078656,1.45439216225896E-14,
51.2493976671679));
#188418=CARTESIAN_POINT('Origin',(118.13713078656,1.45439216225896E-14,
51.2493976671679));
#188419=CARTESIAN_POINT('Origin',(116.683943798944,6.2,63.9661771763823));
#188420=CARTESIAN_POINT('',(116.956733701725,6.2,65.1832107213578));
#188421=CARTESIAN_POINT('',(116.893221227906,6.2,65.5099524430775));
#188422=CARTESIAN_POINT('',(116.956733701725,6.2,65.1832107213578));
#188423=CARTESIAN_POINT('',(116.449160831798,6.2,65.1740248054003));
#188424=CARTESIAN_POINT('Origin',(116.959178380441,6.2,51.0204257716897));
#188425=CARTESIAN_POINT('',(116.386037842833,6.2,65.4987628112495));
#188426=CARTESIAN_POINT('',(116.449160831798,6.2,65.1740248054003));
#188427=CARTESIAN_POINT('Origin',(116.959178380441,6.2,51.0204257716897));
#188428=CARTESIAN_POINT('Origin',(117.174757301493,6.2,64.0615821328315));
#188429=CARTESIAN_POINT('',(117.001370196777,6.7,64.9535770074154));
#188430=CARTESIAN_POINT('',(116.936796826496,6.7,65.2857765410541));
#188431=CARTESIAN_POINT('',(117.001370196777,6.7,64.9535770074154));
#188432=CARTESIAN_POINT('Origin',(119.609571294209,1.45439216225896E-14,
51.5356125365156));
#188433=CARTESIAN_POINT('Origin',(119.609571294209,1.45439216225896E-14,
51.5356125365156));
#188434=CARTESIAN_POINT('Origin',(117.174757301493,6.7,64.0615821328315));
#188435=CARTESIAN_POINT('',(116.493512355389,6.7,64.9458571352127));
#188436=CARTESIAN_POINT('',(116.429348192645,6.7,65.2759514890787));
#188437=CARTESIAN_POINT('',(116.493512355389,6.7,64.9458571352127));
#188438=CARTESIAN_POINT('Origin',(116.959178380441,6.7,51.0204257716897));
#188439=CARTESIAN_POINT('Origin',(116.959178380441,6.7,51.0204257716897));
#188440=CARTESIAN_POINT('Origin',(116.683943798944,6.7,63.9661771763823));
#188441=CARTESIAN_POINT('Origin',(119.118757791659,1.45439216225896E-14,
51.4402075800664));
#188442=CARTESIAN_POINT('Origin',(119.118757791659,1.45439216225896E-14,
51.4402075800664));
#188443=CARTESIAN_POINT('Origin',(117.665570804043,6.2,64.1569870892808));
#188444=CARTESIAN_POINT('',(117.982648245008,6.2,65.1461821388146));
#188445=CARTESIAN_POINT('',(117.918083304325,6.2,65.4783383061452));
#188446=CARTESIAN_POINT('',(117.982648245008,6.2,65.1461821388146));
#188447=CARTESIAN_POINT('',(117.467868425555,6.2,65.1740725789575));
#188448=CARTESIAN_POINT('Origin',(116.959178380441,6.2,51.0204257716897));
#188449=CARTESIAN_POINT('',(117.403877271222,6.2,65.5032768861503));
#188450=CARTESIAN_POINT('',(117.467868425555,6.2,65.1740725789575));
#188451=CARTESIAN_POINT('Origin',(116.959178380441,6.2,51.0204257716897));
#188452=CARTESIAN_POINT('Origin',(118.156384306592,6.2,64.25239204573));
#188453=CARTESIAN_POINT('',(118.028055880648,6.7,64.9125812702591));
#188454=CARTESIAN_POINT('',(117.962375473602,6.7,65.2504759859093));
#188455=CARTESIAN_POINT('',(118.028055880648,6.7,64.9125812702591));
#188456=CARTESIAN_POINT('Origin',(120.591198299308,1.45439216225896E-14,
51.7264224494141));
#188457=CARTESIAN_POINT('Origin',(120.591198299308,1.45439216225896E-14,
51.7264224494141));
#188458=CARTESIAN_POINT('Origin',(118.156384306592,6.7,64.25239204573));
#188459=CARTESIAN_POINT('',(117.512855450604,6.7,64.9426355535102));
#188460=CARTESIAN_POINT('',(117.447778812482,6.7,65.2774241628201));
#188461=CARTESIAN_POINT('',(117.512855450604,6.7,64.9426355535102));
#188462=CARTESIAN_POINT('Origin',(116.959178380441,6.7,51.0204257716897));
#188463=CARTESIAN_POINT('Origin',(116.959178380441,6.7,51.0204257716897));
#188464=CARTESIAN_POINT('Origin',(117.665570804043,6.7,64.1569870892808));
#188465=CARTESIAN_POINT('Origin',(120.100384796758,1.45439216225896E-14,
51.6310174929649));
#188466=CARTESIAN_POINT('Origin',(120.100384796758,1.45439216225896E-14,
51.6310174929649));
#188467=CARTESIAN_POINT('Origin',(118.647197809142,6.2,64.3477970021793));
#188468=CARTESIAN_POINT('',(119.023569994761,6.2,65.0319485572271));
#188469=CARTESIAN_POINT('',(118.957540802795,6.2,65.3716376067848));
#188470=CARTESIAN_POINT('',(119.023569994761,6.2,65.0319485572271));
#188471=CARTESIAN_POINT('',(118.501174705973,6.2,65.0990169952141));
#188472=CARTESIAN_POINT('Origin',(116.959178380441,6.2,51.0204257716897));
#188473=CARTESIAN_POINT('',(118.435933476088,6.2,65.4346523515122));
#188474=CARTESIAN_POINT('',(118.501174705973,6.2,65.0990169952141));
#188475=CARTESIAN_POINT('Origin',(116.959178380441,6.2,51.0204257716897));
#188476=CARTESIAN_POINT('Origin',(119.138011311691,6.2,64.4432019586286));
#188477=CARTESIAN_POINT('',(119.07005318008,6.7,64.7928144928639));
#188478=CARTESIAN_POINT('',(119.002829448977,6.7,65.1386488828715));
#188479=CARTESIAN_POINT('',(119.07005318008,6.7,64.7928144928639));
#188480=CARTESIAN_POINT('Origin',(121.572825304407,1.45439216225896E-14,
51.9172323623126));
#188481=CARTESIAN_POINT('Origin',(121.572825304407,1.45439216225896E-14,
51.9172323623126));
#188482=CARTESIAN_POINT('Origin',(119.138011311691,6.7,64.4432019586286));
#188483=CARTESIAN_POINT('',(118.547078708453,6.7,64.8628625533834));
#188484=CARTESIAN_POINT('',(118.480685951708,6.7,65.204421972253));
#188485=CARTESIAN_POINT('',(118.547078708453,6.7,64.8628625533834));
#188486=CARTESIAN_POINT('Origin',(116.959178380441,6.7,51.0204257716897));
#188487=CARTESIAN_POINT('Origin',(116.959178380441,6.7,51.0204257716897));
#188488=CARTESIAN_POINT('Origin',(118.647197809142,6.7,64.3477970021793));
#188489=CARTESIAN_POINT('Origin',(121.082011801857,1.45439216225896E-14,
51.8218274058634));
#188490=CARTESIAN_POINT('Origin',(121.082011801857,1.45439216225896E-14,
51.8218274058634));
#188491=CARTESIAN_POINT('Origin',(119.628824814241,6.7,64.5386069150778));
#188492=CARTESIAN_POINT('',(119.549979931809,6.2,64.9442266474737));
#188493=CARTESIAN_POINT('',(119.4830397813,6.2,65.2886021490805));
#188494=CARTESIAN_POINT('',(119.549979931809,6.2,64.9442266474737));
#188495=CARTESIAN_POINT('',(119.597133868151,6.7,64.7016418854643));
#188496=CARTESIAN_POINT('Origin',(122.063638806956,1.45439216225896E-14,
52.0126373187619));
#188497=CARTESIAN_POINT('',(119.528948095297,6.7,65.0524255265237));
#188498=CARTESIAN_POINT('',(119.597133868151,6.7,64.7016418854643));
#188499=CARTESIAN_POINT('Origin',(122.063638806956,1.45439216225896E-14,
52.0126373187619));
#188500=CARTESIAN_POINT('Origin',(119.628824814241,6.2,64.5386069150778));
#188501=CARTESIAN_POINT('',(120.080577810667,6.2,64.8349597523862));
#188502=CARTESIAN_POINT('',(120.01258971947,6.2,65.1847264145575));
#188503=CARTESIAN_POINT('',(120.080577810667,6.2,64.8349597523862));
#188504=CARTESIAN_POINT('Origin',(116.959178380441,6.2,51.0204257716897));
#188505=CARTESIAN_POINT('Origin',(116.959178380441,6.2,51.0204257716897));
#188506=CARTESIAN_POINT('Origin',(120.11963831679,6.2,64.6340118715271));
#188507=CARTESIAN_POINT('',(120.11963831679,6.7,64.6340118715271));
#188508=CARTESIAN_POINT('',(120.05921061797,6.7,64.9448838808303));
#188509=CARTESIAN_POINT('',(120.11963831679,6.7,64.6340118715271));
#188510=CARTESIAN_POINT('',(120.11963831679,6.61107026131202,64.6340118715271));
#188511=CARTESIAN_POINT('',(120.11963831679,6.61107026131202,64.6340118715271));
#188512=CARTESIAN_POINT('Origin',(122.554452309506,1.45439216225896E-14,
52.1080422752111));
#188513=CARTESIAN_POINT('Origin',(122.554452309506,1.45439216225896E-14,
52.1080422752111));
#188514=CARTESIAN_POINT('Origin',(120.11963831679,6.7,64.6340118715271));
#188515=CARTESIAN_POINT('',(120.016762662781,6.7,64.6140147703074));
#188516=CARTESIAN_POINT('Origin',(116.959178380441,6.7,51.0204257716897));
#188517=CARTESIAN_POINT('',(120.11963831679,6.7,64.6340118715271));
#188518=CARTESIAN_POINT('Origin',(116.959178380441,6.7,51.0204257716897));
#188519=CARTESIAN_POINT('Origin',(119.432499413221,6.,64.5004449324981));
#188520=CARTESIAN_POINT('Origin',(114.524364387726,1.45439216225896E-14,
63.5463953680056));
#188521=CARTESIAN_POINT('Origin',(120.61045181934,5.7,64.7294168279763));
#188522=CARTESIAN_POINT('',(120.531606936909,5.2,65.1350365603722));
#188523=CARTESIAN_POINT('',(120.464666786399,5.2,65.479412061979));
#188524=CARTESIAN_POINT('',(120.531606936909,5.2,65.1350365603722));
#188525=CARTESIAN_POINT('',(120.571391313216,5.7,64.9303647088355));
#188526=CARTESIAN_POINT('Origin',(123.045265812055,1.45439216225896E-14,
52.2034472316604));
#188527=CARTESIAN_POINT('',(120.503403222019,5.7,65.2801313710067));
#188528=CARTESIAN_POINT('',(120.571391313216,5.7,64.9303647088355));
#188529=CARTESIAN_POINT('Origin',(123.045265812055,1.45439216225896E-14,
52.2034472316604));
#188530=CARTESIAN_POINT('Origin',(120.61045181934,5.2,64.7294168279763));
#188531=CARTESIAN_POINT('',(121.069574375799,5.2,64.9878567548121));
#188532=CARTESIAN_POINT('',(121.001388602946,5.2,65.3386403958715));
#188533=CARTESIAN_POINT('',(121.069574375799,5.2,64.9878567548121));
#188534=CARTESIAN_POINT('Origin',(116.959178380441,5.2,51.0204257716897));
#188535=CARTESIAN_POINT('Origin',(116.959178380441,5.2,51.0204257716897));
#188536=CARTESIAN_POINT('Origin',(121.101265321889,5.2,64.8248217844256));
#188537=CARTESIAN_POINT('',(121.101265321889,5.7,64.8248217844256));
#188538=CARTESIAN_POINT('',(121.040837623069,5.7,65.1356937937288));
#188539=CARTESIAN_POINT('',(121.101265321889,5.7,64.8248217844256));
#188540=CARTESIAN_POINT('',(121.101265321889,5.59519883471502,64.8248217844256));
#188541=CARTESIAN_POINT('',(121.101265321889,5.59519883471502,64.8248217844256));
#188542=CARTESIAN_POINT('Origin',(123.536079314605,1.45439216225896E-14,
52.2988521881097));
#188543=CARTESIAN_POINT('Origin',(123.536079314605,1.45439216225896E-14,
52.2988521881097));
#188544=CARTESIAN_POINT('Origin',(121.101265321889,5.7,64.8248217844256));
#188545=CARTESIAN_POINT('',(121.013969488837,5.7,64.8078531087324));
#188546=CARTESIAN_POINT('Origin',(116.959178380441,5.7,51.0204257716897));
#188547=CARTESIAN_POINT('',(121.101265321889,5.7,64.8248217844256));
#188548=CARTESIAN_POINT('Origin',(116.959178380441,5.7,51.0204257716897));
#188549=CARTESIAN_POINT('Origin',(120.41412641832,5.,64.6912548453966));
#188550=CARTESIAN_POINT('Origin',(114.524364387726,1.45439216225896E-14,
63.5463953680056));
#188551=CARTESIAN_POINT('Origin',(120.61045181934,4.2,64.7294168279763));
#188552=CARTESIAN_POINT('',(121.001146221201,4.2,65.3398873356296));
#188553=CARTESIAN_POINT('',(120.934753464455,4.2,65.6814467544992));
#188554=CARTESIAN_POINT('',(121.001146221201,4.2,65.3398873356296));
#188555=CARTESIAN_POINT('',(120.464428716171,4.2,65.4806368210111));
#188556=CARTESIAN_POINT('Origin',(116.959178380441,4.2,51.0204257716897));
#188557=CARTESIAN_POINT('',(120.399187486286,4.2,65.8162721773092));
#188558=CARTESIAN_POINT('',(120.464428716171,4.2,65.4806368210111));
#188559=CARTESIAN_POINT('Origin',(116.959178380441,4.2,51.0204257716897));
#188560=CARTESIAN_POINT('Origin',(121.101265321889,4.2,64.8248217844256));
#188561=CARTESIAN_POINT('',(121.033307190278,4.7,65.1744343186609));
#188562=CARTESIAN_POINT('',(120.966083459175,4.7,65.5202687086685));
#188563=CARTESIAN_POINT('',(121.033307190278,4.7,65.1744343186609));
#188564=CARTESIAN_POINT('Origin',(123.536079314605,1.45439216225896E-14,
52.2988521881097));
#188565=CARTESIAN_POINT('Origin',(123.536079314605,1.45439216225896E-14,
52.2988521881097));
#188566=CARTESIAN_POINT('Origin',(121.101265321889,4.7,64.8248217844256));
#188567=CARTESIAN_POINT('',(120.496010502409,4.7,65.3181634265749));
#188568=CARTESIAN_POINT('',(120.429981310443,4.7,65.6578524761325));
#188569=CARTESIAN_POINT('',(120.496010502409,4.7,65.3181634265749));
#188570=CARTESIAN_POINT('Origin',(116.959178380441,4.7,51.0204257716897));
#188571=CARTESIAN_POINT('Origin',(116.959178380441,4.7,51.0204257716897));
#188572=CARTESIAN_POINT('Origin',(120.61045181934,4.7,64.7294168279763));
#188573=CARTESIAN_POINT('Origin',(123.045265812055,1.45439216225896E-14,
52.2034472316604));
#188574=CARTESIAN_POINT('Origin',(123.045265812055,1.45439216225896E-14,
52.2034472316604));
#188575=CARTESIAN_POINT('Origin',(120.61045181934,3.2,64.7294168279763));
#188576=CARTESIAN_POINT('',(120.948549968451,3.2,65.6104702486549));
#188577=CARTESIAN_POINT('',(120.883473330329,3.2,65.9452588579649));
#188578=CARTESIAN_POINT('',(120.948549968451,3.2,65.6104702486549));
#188579=CARTESIAN_POINT('',(120.412749440852,3.2,65.746502317653));
#188580=CARTESIAN_POINT('Origin',(116.959178380441,3.2,51.0204257716897));
#188581=CARTESIAN_POINT('',(120.348758286519,3.2,66.0757066248458));
#188582=CARTESIAN_POINT('',(120.412749440852,3.2,65.746502317653));
#188583=CARTESIAN_POINT('Origin',(116.959178380441,3.2,51.0204257716897));
#188584=CARTESIAN_POINT('Origin',(121.101265321889,3.2,64.8248217844256));
#188585=CARTESIAN_POINT('',(120.972936895945,3.7,65.4850110089547));
#188586=CARTESIAN_POINT('',(120.907256488899,3.7,65.8229057246048));
#188587=CARTESIAN_POINT('',(120.972936895945,3.7,65.4850110089547));
#188588=CARTESIAN_POINT('Origin',(123.536079314605,1.45439216225896E-14,
52.2988521881097));
#188589=CARTESIAN_POINT('Origin',(123.536079314605,1.45439216225896E-14,
52.2988521881097));
#188590=CARTESIAN_POINT('Origin',(121.101265321889,3.7,64.8248217844256));
#188591=CARTESIAN_POINT('',(120.436715757755,3.7,65.6232069210608));
#188592=CARTESIAN_POINT('',(120.372150817072,3.7,65.9553630883915));
#188593=CARTESIAN_POINT('',(120.436715757755,3.7,65.6232069210608));
#188594=CARTESIAN_POINT('Origin',(116.959178380441,3.7,51.0204257716897));
#188595=CARTESIAN_POINT('Origin',(116.959178380441,3.7,51.0204257716897));
#188596=CARTESIAN_POINT('Origin',(120.61045181934,3.7,64.7294168279763));
#188597=CARTESIAN_POINT('Origin',(123.045265812055,1.45439216225896E-14,
52.2034472316604));
#188598=CARTESIAN_POINT('Origin',(123.045265812055,1.45439216225896E-14,
52.2034472316604));
#188599=CARTESIAN_POINT('Origin',(120.61045181934,2.2,64.7294168279763));
#188600=CARTESIAN_POINT('',(120.910833878335,2.2,65.804501743256));
#188601=CARTESIAN_POINT('',(120.846669715591,2.2,66.134596097122));
#188602=CARTESIAN_POINT('',(120.910833878335,2.2,65.804501743256));
#188603=CARTESIAN_POINT('',(120.375668852194,2.2,65.9372644569943));
#188604=CARTESIAN_POINT('Origin',(116.959178380441,2.2,51.0204257716897));
#188605=CARTESIAN_POINT('',(120.312545863229,2.2,66.2620024628435));
#188606=CARTESIAN_POINT('',(120.375668852194,2.2,65.9372644569943));
#188607=CARTESIAN_POINT('Origin',(116.959178380441,2.2,51.0204257716897));
#188608=CARTESIAN_POINT('Origin',(121.101265321889,2.2,64.8248217844256));
#188609=CARTESIAN_POINT('',(120.927878217173,2.7,65.7168166590094));
#188610=CARTESIAN_POINT('',(120.863304846892,2.7,66.0490161926481));
#188611=CARTESIAN_POINT('',(120.927878217173,2.7,65.7168166590094));
#188612=CARTESIAN_POINT('Origin',(123.536079314605,1.45439216225896E-14,
52.2988521881097));
#188613=CARTESIAN_POINT('Origin',(123.536079314605,1.45439216225896E-14,
52.2988521881097));
#188614=CARTESIAN_POINT('Origin',(121.101265321889,2.7,64.8248217844256));
#188615=CARTESIAN_POINT('',(120.392428219572,2.7,65.8510454165026));
#188616=CARTESIAN_POINT('',(120.328915745752,2.7,66.1777871382222));
#188617=CARTESIAN_POINT('',(120.392428219572,2.7,65.8510454165026));
#188618=CARTESIAN_POINT('Origin',(116.959178380441,2.7,51.0204257716897));
#188619=CARTESIAN_POINT('Origin',(116.959178380441,2.7,51.0204257716897));
#188620=CARTESIAN_POINT('Origin',(120.61045181934,2.7,64.7294168279763));
#188621=CARTESIAN_POINT('Origin',(123.045265812055,1.45439216225896E-14,
52.2034472316604));
#188622=CARTESIAN_POINT('Origin',(123.045265812055,1.45439216225896E-14,
52.2034472316604));
#188623=CARTESIAN_POINT('Origin',(120.61045181934,1.2,64.7294168279763));
#188624=CARTESIAN_POINT('',(120.887362221676,1.2,65.9252523462056));
#188625=CARTESIAN_POINT('',(120.823753259538,1.2,66.2524904548114));
#188626=CARTESIAN_POINT('',(120.887362221676,1.2,65.9252523462056));
#188627=CARTESIAN_POINT('',(120.35258377256,1.2,66.05602630348));
#188628=CARTESIAN_POINT('Origin',(116.959178380441,1.2,51.0204257716897));
#188629=CARTESIAN_POINT('',(120.289989608761,1.2,66.3780437532706));
#188630=CARTESIAN_POINT('',(120.35258377256,1.2,66.05602630348));
#188631=CARTESIAN_POINT('Origin',(116.959178380441,1.2,51.0204257716897));
#188632=CARTESIAN_POINT('Origin',(121.101265321889,1.2,64.8248217844256));
#188633=CARTESIAN_POINT('',(120.897346659478,1.7,65.8738871229378));
#188634=CARTESIAN_POINT('',(120.833502689264,1.7,66.2023342372587));
#188635=CARTESIAN_POINT('',(120.897346659478,1.7,65.8738871229378));
#188636=CARTESIAN_POINT('Origin',(123.536079314605,1.45439216225896E-14,
52.2988521881097));
#188637=CARTESIAN_POINT('Origin',(123.536079314605,1.45439216225896E-14,
52.2988521881097));
#188638=CARTESIAN_POINT('Origin',(121.101265321889,1.7,64.8248217844256));
#188639=CARTESIAN_POINT('',(120.362404587042,1.7,66.0055028450213));
#188640=CARTESIAN_POINT('',(120.299586525741,1.7,66.3286721418589));
#188641=CARTESIAN_POINT('',(120.362404587042,1.7,66.0055028450213));
#188642=CARTESIAN_POINT('Origin',(116.959178380441,1.7,51.0204257716897));
#188643=CARTESIAN_POINT('Origin',(116.959178380441,1.7,51.0204257716897));
#188644=CARTESIAN_POINT('Origin',(120.61045181934,1.7,64.7294168279763));
#188645=CARTESIAN_POINT('Origin',(123.045265812055,1.45439216225896E-14,
52.2034472316604));
#188646=CARTESIAN_POINT('Origin',(123.045265812055,1.45439216225896E-14,
52.2034472316604));
#188647=CARTESIAN_POINT('Origin',(120.61045181934,0.200000000000015,64.7294168279763));
#188648=CARTESIAN_POINT('',(120.877757657924,0.200000000000015,65.9746632966532));
#188649=CARTESIAN_POINT('',(120.814373154676,0.200000000000015,66.3007466701378));
#188650=CARTESIAN_POINT('',(120.877757657924,0.200000000000015,65.9746632966532));
#188651=CARTESIAN_POINT('',(120.343135475112,0.200000000000015,66.1046333374951));
#188652=CARTESIAN_POINT('Origin',(116.959178380441,0.200000000000015,51.0204257716897));
#188653=CARTESIAN_POINT('',(120.280755231782,0.200000000000015,66.4255502673749));
#188654=CARTESIAN_POINT('',(120.343135475112,0.200000000000015,66.1046333374951));
#188655=CARTESIAN_POINT('Origin',(116.959178380441,0.200000000000015,51.0204257716897));
#188656=CARTESIAN_POINT('Origin',(121.101265321889,0.200000000000015,64.8248217844256));
#188657=CARTESIAN_POINT('',(120.880841050326,0.700000000000015,65.9588006970472));
#188658=CARTESIAN_POINT('',(120.817384658946,0.700000000000015,66.285253901068));
#188659=CARTESIAN_POINT('',(120.880841050326,0.700000000000015,65.9588006970472));
#188660=CARTESIAN_POINT('Origin',(123.536079314605,1.45439216225896E-14,
52.2988521881097));
#188661=CARTESIAN_POINT('Origin',(123.536079314605,1.45439216225896E-14,
52.2988521881097));
#188662=CARTESIAN_POINT('Origin',(121.101265321889,0.700000000000015,64.8248217844256));
#188663=CARTESIAN_POINT('',(120.346168820923,0.700000000000015,66.0890282039968));
#188664=CARTESIAN_POINT('',(120.283720056839,0.700000000000015,66.4102976408361));
#188665=CARTESIAN_POINT('',(120.346168820923,0.700000000000015,66.0890282039968));
#188666=CARTESIAN_POINT('Origin',(116.959178380441,0.700000000000015,51.0204257716897));
#188667=CARTESIAN_POINT('Origin',(116.959178380441,0.700000000000015,51.0204257716897));
#188668=CARTESIAN_POINT('Origin',(120.61045181934,0.700000000000015,64.7294168279763));
#188669=CARTESIAN_POINT('Origin',(123.045265812055,1.45439216225896E-14,
52.2034472316604));
#188670=CARTESIAN_POINT('Origin',(123.045265812055,1.45439216225896E-14,
52.2034472316604));
#188671=CARTESIAN_POINT('Origin',(109.812554763251,0.200000000000015,62.6305077860928));
#188672=CARTESIAN_POINT('',(109.904835051783,0.200000000000015,64.7761781578189));
#188673=CARTESIAN_POINT('',(109.845282885134,0.200000000000015,65.0825459670545));
#188674=CARTESIAN_POINT('',(109.904835051783,0.200000000000015,64.7761781578189));
#188675=CARTESIAN_POINT('',(109.443407616813,0.200000000000015,64.5295957438079));
#188676=CARTESIAN_POINT('Origin',(116.959178380441,0.200000000000015,51.0204257716897));
#188677=CARTESIAN_POINT('',(109.383244376598,0.200000000000015,64.8391072383233));
#188678=CARTESIAN_POINT('',(109.443407616813,0.200000000000015,64.5295957438079));
#188679=CARTESIAN_POINT('Origin',(116.959178380441,0.200000000000015,51.0204257716897));
#188680=CARTESIAN_POINT('Origin',(110.3033682658,0.200000000000015,62.725912742542));
#188681=CARTESIAN_POINT('',(109.907727771406,0.700000000000015,64.7612964797325));
#188682=CARTESIAN_POINT('',(109.848115997298,0.700000000000015,65.0679709412246));
#188683=CARTESIAN_POINT('',(109.907727771406,0.700000000000015,64.7612964797325));
#188684=CARTESIAN_POINT('Origin',(112.738182258515,1.45439216225896E-14,
50.1999431462261));
#188685=CARTESIAN_POINT('Origin',(112.738182258515,1.45439216225896E-14,
50.1999431462261));
#188686=CARTESIAN_POINT('Origin',(110.3033682658,0.700000000000015,62.725912742542));
#188687=CARTESIAN_POINT('',(109.446330684182,0.700000000000015,64.5145579408814));
#188688=CARTESIAN_POINT('',(109.38610598051,0.700000000000015,64.8243856358901));
#188689=CARTESIAN_POINT('',(109.446330684182,0.700000000000015,64.5145579408814));
#188690=CARTESIAN_POINT('Origin',(116.959178380441,0.700000000000015,51.0204257716897));
#188691=CARTESIAN_POINT('Origin',(116.959178380441,0.700000000000015,51.0204257716897));
#188692=CARTESIAN_POINT('Origin',(109.812554763251,0.700000000000015,62.6305077860928));
#188693=CARTESIAN_POINT('Origin',(112.247368755966,1.45439216225896E-14,
50.1045381897769));
#188694=CARTESIAN_POINT('Origin',(112.247368755966,1.45439216225896E-14,
50.1045381897769));
#188695=CARTESIAN_POINT('Origin',(109.812554763251,1.2,62.6305077860928));
#188696=CARTESIAN_POINT('',(109.913844353467,1.2,64.7298295499524));
#188697=CARTESIAN_POINT('',(109.854106151249,1.2,65.0371544244425));
#188698=CARTESIAN_POINT('',(109.913844353467,1.2,64.7298295499524));
#188699=CARTESIAN_POINT('',(109.45251164372,1.2,64.4827598193477));
#188700=CARTESIAN_POINT('Origin',(116.959178380441,1.2,51.0204257716897));
#188701=CARTESIAN_POINT('',(109.392156562714,1.2,64.7932582442455));
#188702=CARTESIAN_POINT('',(109.45251164372,1.2,64.4827598193477));
#188703=CARTESIAN_POINT('Origin',(116.959178380441,1.2,51.0204257716897));
#188704=CARTESIAN_POINT('Origin',(110.3033682658,1.2,62.725912742542));
#188705=CARTESIAN_POINT('',(109.923205813012,1.7,64.6816692559874));
#188706=CARTESIAN_POINT('',(109.863273080932,1.7,64.9899948948704));
#188707=CARTESIAN_POINT('',(109.923205813012,1.7,64.6816692559874));
#188708=CARTESIAN_POINT('Origin',(112.738182258515,1.45439216225896E-14,
50.1999431462261));
#188709=CARTESIAN_POINT('Origin',(112.738182258515,1.45439216225896E-14,
50.1999431462261));
#188710=CARTESIAN_POINT('Origin',(110.3033682658,1.7,62.725912742542));
#188711=CARTESIAN_POINT('',(109.461972183711,1.7,64.4340898032213));
#188712=CARTESIAN_POINT('',(109.401416462735,1.7,64.7456204261326));
#188713=CARTESIAN_POINT('',(109.461972183711,1.7,64.4340898032213));
#188714=CARTESIAN_POINT('Origin',(116.959178380441,1.7,51.0204257716897));
#188715=CARTESIAN_POINT('Origin',(116.959178380441,1.7,51.0204257716897));
#188716=CARTESIAN_POINT('Origin',(109.812554763251,1.7,62.6305077860928));
#188717=CARTESIAN_POINT('Origin',(112.247368755966,1.45439216225896E-14,
50.1045381897769));
#188718=CARTESIAN_POINT('Origin',(112.247368755966,1.45439216225896E-14,
50.1045381897769));
#188719=CARTESIAN_POINT('Origin',(109.812554763251,2.2,62.6305077860928));
#188720=CARTESIAN_POINT('',(109.935844669259,2.2,64.6166483017972));
#188721=CARTESIAN_POINT('',(109.875647305929,2.2,64.9263353436442));
#188722=CARTESIAN_POINT('',(109.935844669259,2.2,64.6166483017972));
#188723=CARTESIAN_POINT('',(109.474745874983,2.2,64.3683751864209));
#188724=CARTESIAN_POINT('Origin',(116.959178380441,2.2,51.0204257716897));
#188725=CARTESIAN_POINT('',(109.413917145163,2.2,64.6813103110717));
#188726=CARTESIAN_POINT('',(109.474745874983,2.2,64.3683751864209));
#188727=CARTESIAN_POINT('Origin',(116.959178380441,2.2,51.0204257716897));
#188728=CARTESIAN_POINT('Origin',(110.3033682658,2.2,62.725912742542));
#188729=CARTESIAN_POINT('',(109.95180552014,2.7,64.5345372520554));
#188730=CARTESIAN_POINT('',(109.89127064788,2.7,64.8459606181596));
#188731=CARTESIAN_POINT('',(109.95180552014,2.7,64.5345372520554));
#188732=CARTESIAN_POINT('Origin',(112.738182258515,1.45439216225896E-14,
50.1999431462261));
#188733=CARTESIAN_POINT('Origin',(112.738182258515,1.45439216225896E-14,
50.1999431462261));
#188734=CARTESIAN_POINT('Origin',(110.3033682658,2.7,62.725912742542));
#188735=CARTESIAN_POINT('',(109.490878776999,2.7,64.2853790147403));
#188736=CARTESIAN_POINT('',(109.429701743214,2.7,64.6001059990095));
#188737=CARTESIAN_POINT('',(109.490878776999,2.7,64.2853790147403));
#188738=CARTESIAN_POINT('Origin',(116.959178380441,2.7,51.0204257716897));
#188739=CARTESIAN_POINT('Origin',(116.959178380441,2.7,51.0204257716897));
#188740=CARTESIAN_POINT('Origin',(109.812554763251,2.7,62.6305077860928));
#188741=CARTESIAN_POINT('Origin',(112.247368755966,1.45439216225896E-14,
50.1045381897769));
#188742=CARTESIAN_POINT('Origin',(112.247368755966,1.45439216225896E-14,
50.1045381897769));
#188743=CARTESIAN_POINT('Origin',(109.812554763251,3.2,62.6305077860928));
#188744=CARTESIAN_POINT('',(109.971145850964,3.2,64.4350403719647));
#188745=CARTESIAN_POINT('',(109.910196955985,3.2,64.7485936896801));
#188746=CARTESIAN_POINT('',(109.971145850964,3.2,64.4350403719647));
#188747=CARTESIAN_POINT('',(109.510430291786,3.2,64.184795692762));
#188748=CARTESIAN_POINT('Origin',(116.959178380441,3.2,51.0204257716897));
#188749=CARTESIAN_POINT('',(109.448825823059,3.2,64.5017216282059));
#188750=CARTESIAN_POINT('',(109.510430291786,3.2,64.184795692762));
#188751=CARTESIAN_POINT('Origin',(116.959178380441,3.2,51.0204257716897));
#188752=CARTESIAN_POINT('Origin',(110.3033682658,3.2,62.725912742542));
#188753=CARTESIAN_POINT('',(109.993937112423,3.7,64.317790081408));
#188754=CARTESIAN_POINT('',(109.932493071797,3.7,64.6338906899368));
#188755=CARTESIAN_POINT('',(109.993937112423,3.7,64.317790081408));
#188756=CARTESIAN_POINT('Origin',(112.738182258515,1.45439216225896E-14,
50.1999431462261));
#188757=CARTESIAN_POINT('Origin',(112.738182258515,1.45439216225896E-14,
50.1999431462261));
#188758=CARTESIAN_POINT('Origin',(110.3033682658,3.7,62.725912742542));
#188759=CARTESIAN_POINT('',(109.533474303738,3.7,64.066245120129));
#188760=CARTESIAN_POINT('',(109.471358401437,3.7,64.3858021400896));
#188761=CARTESIAN_POINT('',(109.533474303738,3.7,64.066245120129));
#188762=CARTESIAN_POINT('Origin',(116.959178380441,3.7,51.0204257716897));
#188763=CARTESIAN_POINT('Origin',(116.959178380441,3.7,51.0204257716897));
#188764=CARTESIAN_POINT('Origin',(109.812554763251,3.7,62.6305077860928));
#188765=CARTESIAN_POINT('Origin',(112.247368755966,1.45439216225896E-14,
50.1045381897769));
#188766=CARTESIAN_POINT('Origin',(112.247368755966,1.45439216225896E-14,
50.1045381897769));
#188767=CARTESIAN_POINT('Origin',(109.812554763251,4.2,62.6305077860928));
#188768=CARTESIAN_POINT('',(110.020266117139,4.2,64.182339770391));
#188769=CARTESIAN_POINT('',(109.958240075275,4.2,64.5014345007899));
#188770=CARTESIAN_POINT('',(110.020266117139,4.2,64.182339770391));
#188771=CARTESIAN_POINT('',(109.560100658523,4.2,63.9292650832573));
#188772=CARTESIAN_POINT('Origin',(116.959178380441,4.2,51.0204257716897));
#188773=CARTESIAN_POINT('',(109.497383261795,4.2,64.2519165083483));
#188774=CARTESIAN_POINT('',(109.560100658523,4.2,63.9292650832573));
#188775=CARTESIAN_POINT('Origin',(116.959178380441,4.2,51.0204257716897));
#188776=CARTESIAN_POINT('Origin',(110.3033682658,4.2,62.725912742542));
#188777=CARTESIAN_POINT('',(110.050236821974,4.7,64.0281546298999));
#188778=CARTESIAN_POINT('',(109.987534869184,4.7,64.3507266032104));
#188779=CARTESIAN_POINT('',(110.050236821974,4.7,64.0281546298999));
#188780=CARTESIAN_POINT('Origin',(112.738182258515,1.45439216225896E-14,
50.1999431462261));
#188781=CARTESIAN_POINT('Origin',(112.738182258515,1.45439216225896E-14,
50.1999431462261));
#188782=CARTESIAN_POINT('Origin',(110.3033682658,4.7,62.725912742542));
#188783=CARTESIAN_POINT('',(109.590417054145,4.7,63.7733015267161));
#188784=CARTESIAN_POINT('',(109.527000630799,4.7,64.0995491140498));
#188785=CARTESIAN_POINT('',(109.590417054145,4.7,63.7733015267161));
#188786=CARTESIAN_POINT('Origin',(116.959178380441,4.7,51.0204257716897));
#188787=CARTESIAN_POINT('Origin',(116.959178380441,4.7,51.0204257716897));
#188788=CARTESIAN_POINT('Origin',(109.812554763251,4.7,62.6305077860928));
#188789=CARTESIAN_POINT('Origin',(112.247368755966,1.45439216225896E-14,
50.1045381897769));
#188790=CARTESIAN_POINT('Origin',(112.247368755966,1.45439216225896E-14,
50.1045381897769));
#188791=CARTESIAN_POINT('Origin',(109.812554763251,5.2,62.6305077860928));
#188792=CARTESIAN_POINT('',(110.083972587697,5.2,63.8546000269541));
#188793=CARTESIAN_POINT('',(110.020492179188,5.2,64.1811767877771));
#188794=CARTESIAN_POINT('',(110.083972587697,5.2,63.8546000269541));
#188795=CARTESIAN_POINT('',(109.624551443867,5.2,63.5976961913039));
#188796=CARTESIAN_POINT('Origin',(116.959178380441,5.2,51.0204257716897));
#188797=CARTESIAN_POINT('',(109.560329299005,5.2,63.9280888358195));
#188798=CARTESIAN_POINT('',(109.624551443867,5.2,63.5976961913039));
#188799=CARTESIAN_POINT('Origin',(116.959178380441,5.2,51.0204257716897));
#188800=CARTESIAN_POINT('Origin',(110.3033682658,5.2,62.725912742542));
#188801=CARTESIAN_POINT('',(110.121619040844,5.7,63.6609267817127));
#188802=CARTESIAN_POINT('',(110.057247074165,5.7,63.9920901888077));
#188803=CARTESIAN_POINT('',(110.121619040844,5.7,63.6609267817127));
#188804=CARTESIAN_POINT('Origin',(112.738182258515,1.45439216225896E-14,
50.1999431462261));
#188805=CARTESIAN_POINT('Origin',(112.738182258515,1.45439216225896E-14,
50.1999431462261));
#188806=CARTESIAN_POINT('Origin',(110.3033682658,5.7,62.725912742542));
#188807=CARTESIAN_POINT('',(109.66265508748,5.7,63.401670916753));
#188808=CARTESIAN_POINT('',(109.597509299565,5.7,63.7368152691325));
#188809=CARTESIAN_POINT('',(109.66265508748,5.7,63.401670916753));
#188810=CARTESIAN_POINT('Origin',(116.959178380441,5.7,51.0204257716897));
#188811=CARTESIAN_POINT('Origin',(116.959178380441,5.7,51.0204257716897));
#188812=CARTESIAN_POINT('Origin',(109.812554763251,5.7,62.6305077860928));
#188813=CARTESIAN_POINT('Origin',(112.247368755966,1.45439216225896E-14,
50.1045381897769));
#188814=CARTESIAN_POINT('Origin',(112.247368755966,1.45439216225896E-14,
50.1045381897769));
#188815=CARTESIAN_POINT('Origin',(110.79418176835,5.2,62.8213176989913));
#188816=CARTESIAN_POINT('',(111.013976121973,5.2,64.3109883486827));
#188817=CARTESIAN_POINT('',(110.951679320672,5.2,64.6314760086754));
#188818=CARTESIAN_POINT('',(111.013976121973,5.2,64.3109883486827));
#188819=CARTESIAN_POINT('',(110.54715253499,5.2,64.0921665916452));
#188820=CARTESIAN_POINT('Origin',(116.959178380441,5.2,51.0204257716897));
#188821=CARTESIAN_POINT('',(110.484311174475,5.2,64.4154557519527));
#188822=CARTESIAN_POINT('',(110.54715253499,5.2,64.0921665916452));
#188823=CARTESIAN_POINT('Origin',(116.959178380441,5.2,51.0204257716897));
#188824=CARTESIAN_POINT('Origin',(111.284995270899,5.2,62.9167226554405));
#188825=CARTESIAN_POINT('',(111.050894299475,5.7,64.1210617381391));
#188826=CARTESIAN_POINT('',(110.98775555323,5.7,64.4458808077575));
#188827=CARTESIAN_POINT('',(111.050894299475,5.7,64.1210617381391));
#188828=CARTESIAN_POINT('Origin',(113.719809263614,1.45439216225896E-14,
50.3907530591246));
#188829=CARTESIAN_POINT('Origin',(113.719809263614,1.45439216225896E-14,
50.3907530591246));
#188830=CARTESIAN_POINT('Origin',(111.284995270899,5.7,62.9167226554405));
#188831=CARTESIAN_POINT('',(110.584405587776,5.7,63.900517205712));
#188832=CARTESIAN_POINT('',(110.520699696142,5.7,64.2282539708631));
#188833=CARTESIAN_POINT('',(110.584405587776,5.7,63.900517205712));
#188834=CARTESIAN_POINT('Origin',(116.959178380441,5.7,51.0204257716897));
#188835=CARTESIAN_POINT('Origin',(116.959178380441,5.7,51.0204257716897));
#188836=CARTESIAN_POINT('Origin',(110.79418176835,5.7,62.8213176989913));
#188837=CARTESIAN_POINT('Origin',(113.228995761065,1.45439216225896E-14,
50.2953481026754));
#188838=CARTESIAN_POINT('Origin',(113.228995761065,1.45439216225896E-14,
50.2953481026754));
#188839=CARTESIAN_POINT('Origin',(111.775808773449,5.2,63.0121276118898));
#188840=CARTESIAN_POINT('',(111.958186342362,5.2,64.6942899710361));
#188841=CARTESIAN_POINT('',(111.896720498972,5.2,65.0105027445071));
#188842=CARTESIAN_POINT('',(111.958186342362,5.2,64.6942899710361));
#188843=CARTESIAN_POINT('',(111.484347160118,5.2,64.5115601426693));
#188844=CARTESIAN_POINT('Origin',(116.959178380441,5.2,51.0204257716897));
#188845=CARTESIAN_POINT('',(111.422507081558,5.2,64.8296981795755));
#188846=CARTESIAN_POINT('',(111.484347160118,5.2,64.5115601426693));
#188847=CARTESIAN_POINT('Origin',(116.959178380441,5.2,51.0204257716897));
#188848=CARTESIAN_POINT('Origin',(112.266622275998,5.2,63.107532568339));
#188849=CARTESIAN_POINT('',(111.994594150334,5.7,64.5069889710055));
#188850=CARTESIAN_POINT('',(111.932320047887,5.7,64.8273598561001));
#188851=CARTESIAN_POINT('',(111.994594150334,5.7,64.5069889710055));
#188852=CARTESIAN_POINT('Origin',(114.701436268713,1.45439216225896E-14,
50.5815629720231));
#188853=CARTESIAN_POINT('Origin',(114.701436268713,1.45439216225896E-14,
50.5815629720231));
#188854=CARTESIAN_POINT('Origin',(112.266622275998,5.7,63.107532568339));
#188855=CARTESIAN_POINT('',(111.520984728148,5.7,64.3230771355044));
#188856=CARTESIAN_POINT('',(111.458321335333,5.7,64.6454507359363));
#188857=CARTESIAN_POINT('',(111.520984728148,5.7,64.3230771355044));
#188858=CARTESIAN_POINT('Origin',(116.959178380441,5.7,51.0204257716897));
#188859=CARTESIAN_POINT('Origin',(116.959178380441,5.7,51.0204257716897));
#188860=CARTESIAN_POINT('Origin',(111.775808773449,5.7,63.0121276118898));
#188861=CARTESIAN_POINT('Origin',(114.210622766164,1.45439216225896E-14,
50.4861580155739));
#188862=CARTESIAN_POINT('Origin',(114.210622766164,1.45439216225896E-14,
50.4861580155739));
#188863=CARTESIAN_POINT('Origin',(112.757435778548,5.2,63.2029375247883));
#188864=CARTESIAN_POINT('',(112.916026866261,5.2,65.0074701106602));
#188865=CARTESIAN_POINT('',(112.855077971282,5.2,65.3210234283756));
#188866=CARTESIAN_POINT('',(112.916026866261,5.2,65.0074701106602));
#188867=CARTESIAN_POINT('',(112.435429605694,5.2,64.8595074077664));
#188868=CARTESIAN_POINT('Origin',(116.959178380441,5.2,51.0204257716897));
#188869=CARTESIAN_POINT('',(112.374259740071,5.2,65.1741975152246));
#188870=CARTESIAN_POINT('',(112.435429605694,5.2,64.8595074077664));
#188871=CARTESIAN_POINT('Origin',(116.959178380441,5.2,51.0204257716897));
#188872=CARTESIAN_POINT('Origin',(113.248249281097,5.2,63.2983424812375));
#188873=CARTESIAN_POINT('',(112.952117544559,5.7,64.8218005932256));
#188874=CARTESIAN_POINT('',(112.890380877488,5.7,65.1394066267945));
#188875=CARTESIAN_POINT('',(112.952117544559,5.7,64.8218005932256));
#188876=CARTESIAN_POINT('Origin',(115.683063273812,1.45439216225896E-14,
50.7723728849216));
#188877=CARTESIAN_POINT('Origin',(115.683063273812,1.45439216225896E-14,
50.7723728849216));
#188878=CARTESIAN_POINT('Origin',(113.248249281097,5.7,63.2983424812375));
#188879=CARTESIAN_POINT('',(112.471655806575,5.7,64.6731406905662));
#188880=CARTESIAN_POINT('',(112.409689455418,5.7,64.9919283404247));
#188881=CARTESIAN_POINT('',(112.471655806575,5.7,64.6731406905662));
#188882=CARTESIAN_POINT('Origin',(116.959178380441,5.7,51.0204257716897));
#188883=CARTESIAN_POINT('Origin',(116.959178380441,5.7,51.0204257716897));
#188884=CARTESIAN_POINT('Origin',(112.757435778548,5.7,63.2029375247883));
#188885=CARTESIAN_POINT('Origin',(115.192249771263,1.45439216225896E-14,
50.6769679284724));
#188886=CARTESIAN_POINT('Origin',(115.192249771263,1.45439216225896E-14,
50.6769679284724));
#188887=CARTESIAN_POINT('Origin',(113.739062783647,5.2,63.3937474376868));
#188888=CARTESIAN_POINT('',(113.887147487649,5.2,65.2523304123455));
#188889=CARTESIAN_POINT('',(113.826424197673,5.2,65.5647230987283));
#188890=CARTESIAN_POINT('',(113.887147487649,5.2,65.2523304123455));
#188891=CARTESIAN_POINT('',(113.39994106609,5.2,65.138368725503));
#188892=CARTESIAN_POINT('Origin',(116.959178380441,5.2,51.0204257716897));
#188893=CARTESIAN_POINT('',(113.339140507264,5.2,65.4511589236753));
#188894=CARTESIAN_POINT('',(113.39994106609,5.2,65.138368725503));
#188895=CARTESIAN_POINT('Origin',(116.959178380441,5.2,51.0204257716897));
#188896=CARTESIAN_POINT('Origin',(114.229876286196,5.2,63.489152394136));
#188897=CARTESIAN_POINT('',(113.92309985496,5.7,65.0673724397024));
#188898=CARTESIAN_POINT('',(113.861597621984,5.7,65.3837724204277));
#188899=CARTESIAN_POINT('',(113.92309985496,5.7,65.0673724397024));
#188900=CARTESIAN_POINT('Origin',(116.664690278911,1.45439216225896E-14,
50.9631827978201));
#188901=CARTESIAN_POINT('Origin',(116.664690278911,1.45439216225896E-14,
50.9631827978201));
#188902=CARTESIAN_POINT('Origin',(114.229876286196,5.7,63.489152394136));
#188903=CARTESIAN_POINT('',(113.43594079827,5.7,64.9531670829504));
#188904=CARTESIAN_POINT('',(113.37435828013,5.7,65.2699800929758));
#188905=CARTESIAN_POINT('',(113.43594079827,5.7,64.9531670829504));
#188906=CARTESIAN_POINT('Origin',(116.959178380441,5.7,51.0204257716897));
#188907=CARTESIAN_POINT('Origin',(116.959178380441,5.7,51.0204257716897));
#188908=CARTESIAN_POINT('Origin',(113.739062783647,5.7,63.3937474376868));
#188909=CARTESIAN_POINT('Origin',(116.173876776362,1.45439216225896E-14,
50.8677778413709));
#188910=CARTESIAN_POINT('Origin',(116.173876776362,1.45439216225896E-14,
50.8677778413709));
#188911=CARTESIAN_POINT('Origin',(114.720689788746,5.2,63.5845573505853));
#188912=CARTESIAN_POINT('',(114.871397359373,5.2,65.429646913552));
#188913=CARTESIAN_POINT('',(114.810617903123,5.2,65.7423285489213));
#188914=CARTESIAN_POINT('',(114.871397359373,5.2,65.429646913552));
#188915=CARTESIAN_POINT('',(114.377633306,5.2,65.3494211494406));
#188916=CARTESIAN_POINT('Origin',(116.959178380441,5.2,51.0204257716897));
#188917=CARTESIAN_POINT('',(114.316917025863,5.2,65.6617777735075));
#188918=CARTESIAN_POINT('',(114.377633306,5.2,65.3494211494406));
#188919=CARTESIAN_POINT('Origin',(116.959178380441,5.2,51.0204257716897));
#188920=CARTESIAN_POINT('Origin',(115.211503291295,5.2,63.6799623070345));
#188921=CARTESIAN_POINT('',(114.907384155297,5.7,65.2445118219335));
#188922=CARTESIAN_POINT('',(114.845823564294,5.7,65.5612120271824));
#188923=CARTESIAN_POINT('',(114.907384155297,5.7,65.2445118219335));
#188924=CARTESIAN_POINT('Origin',(117.64631728401,1.45439216225896E-14,
51.1539927107186));
#188925=CARTESIAN_POINT('Origin',(117.64631728401,1.45439216225896E-14,
51.1539927107186));
#188926=CARTESIAN_POINT('Origin',(115.211503291295,5.7,63.6799623070345));
#188927=CARTESIAN_POINT('',(114.413581376678,5.7,65.1644852809468));
#188928=CARTESIAN_POINT('',(114.352086426791,5.7,65.4808477936172));
#188929=CARTESIAN_POINT('',(114.413581376678,5.7,65.1644852809468));
#188930=CARTESIAN_POINT('Origin',(116.959178380441,5.7,51.0204257716897));
#188931=CARTESIAN_POINT('Origin',(116.959178380441,5.7,51.0204257716897));
#188932=CARTESIAN_POINT('Origin',(114.720689788746,5.7,63.5845573505853));
#188933=CARTESIAN_POINT('Origin',(117.155503781461,1.45439216225896E-14,
51.0585877542694));
#188934=CARTESIAN_POINT('Origin',(117.155503781461,1.45439216225896E-14,
51.0585877542694));
#188935=CARTESIAN_POINT('Origin',(115.702316793845,5.2,63.7753672634838));
#188936=CARTESIAN_POINT('',(115.868813923706,5.2,65.5392269914383));
#188937=CARTESIAN_POINT('',(115.807694164759,5.2,65.8536593236842));
#188938=CARTESIAN_POINT('',(115.868813923706,5.2,65.5392269914383));
#188939=CARTESIAN_POINT('',(115.368450128478,5.2,65.4929537863623));
#188940=CARTESIAN_POINT('Origin',(116.959178380441,5.2,51.0204257716897));
#188941=CARTESIAN_POINT('',(115.307536650107,5.2,65.8063249023359));
#188942=CARTESIAN_POINT('',(115.368450128478,5.2,65.4929537863623));
#188943=CARTESIAN_POINT('Origin',(116.959178380441,5.2,51.0204257716897));
#188944=CARTESIAN_POINT('Origin',(116.193130296394,5.2,63.870772219933));
#188945=CARTESIAN_POINT('',(115.905009389283,5.7,65.3530183928804));
#188946=CARTESIAN_POINT('',(115.843095126351,5.7,65.6715380733892));
#188947=CARTESIAN_POINT('',(115.905009389283,5.7,65.3530183928804));
#188948=CARTESIAN_POINT('Origin',(118.62794428911,1.45439216225896E-14,
51.3448026236171));
#188949=CARTESIAN_POINT('Origin',(118.62794428911,1.45439216225896E-14,
51.3448026236171));
#188950=CARTESIAN_POINT('Origin',(116.193130296394,5.7,63.870772219933));
#188951=CARTESIAN_POINT('',(115.404519090427,5.7,65.3073959893009));
#188952=CARTESIAN_POINT('',(115.342819230478,5.7,65.6248126675899));
#188953=CARTESIAN_POINT('',(115.404519090427,5.7,65.3073959893009));
#188954=CARTESIAN_POINT('Origin',(116.959178380441,5.7,51.0204257716897));
#188955=CARTESIAN_POINT('Origin',(116.959178380441,5.7,51.0204257716897));
#188956=CARTESIAN_POINT('Origin',(115.702316793845,5.7,63.7753672634838));
#188957=CARTESIAN_POINT('Origin',(118.13713078656,1.45439216225896E-14,
51.2493976671679));
#188958=CARTESIAN_POINT('Origin',(118.13713078656,1.45439216225896E-14,
51.2493976671679));
#188959=CARTESIAN_POINT('Origin',(116.683943798944,5.2,63.9661771763823));
#188960=CARTESIAN_POINT('',(116.879625633083,5.2,65.5798953659895));
#188961=CARTESIAN_POINT('',(116.81786685009,5.2,65.8976151755468));
#188962=CARTESIAN_POINT('',(116.879625633083,5.2,65.5798953659895));
#188963=CARTESIAN_POINT('',(116.372523288069,5.2,65.5682888212799));
#188964=CARTESIAN_POINT('Origin',(116.959178380441,5.2,51.0204257716897));
#188965=CARTESIAN_POINT('',(116.311122783449,5.2,65.8841654575899));
#188966=CARTESIAN_POINT('',(116.372523288069,5.2,65.5682888212799));
#188967=CARTESIAN_POINT('Origin',(116.959178380441,5.2,51.0204257716897));
#188968=CARTESIAN_POINT('Origin',(117.174757301493,5.2,64.0615821328315));
#188969=CARTESIAN_POINT('',(116.91621327714,5.7,65.3916691941193));
#188970=CARTESIAN_POINT('',(116.853634466426,5.7,65.7136076595311));
#188971=CARTESIAN_POINT('',(116.91621327714,5.7,65.3916691941193));
#188972=CARTESIAN_POINT('Origin',(119.609571294209,1.45439216225896E-14,
51.5356125365156));
#188973=CARTESIAN_POINT('Origin',(119.609571294209,1.45439216225896E-14,
51.5356125365156));
#188974=CARTESIAN_POINT('Origin',(117.174757301493,5.7,64.0615821328315));
#188975=CARTESIAN_POINT('',(116.408890997126,5.7,65.3811941112541));
#188976=CARTESIAN_POINT('',(116.346684842631,5.7,65.7012154361843));
#188977=CARTESIAN_POINT('',(116.408890997126,5.7,65.3811941112541));
#188978=CARTESIAN_POINT('Origin',(116.959178380441,5.7,51.0204257716897));
#188979=CARTESIAN_POINT('Origin',(116.959178380441,5.7,51.0204257716897));
#188980=CARTESIAN_POINT('Origin',(116.683943798944,5.7,63.9661771763823));
#188981=CARTESIAN_POINT('Origin',(119.118757791659,1.45439216225896E-14,
51.4402075800664));
#188982=CARTESIAN_POINT('Origin',(119.118757791659,1.45439216225896E-14,
51.4402075800664));
#188983=CARTESIAN_POINT('Origin',(117.665570804043,5.2,64.1569870892808));
#188984=CARTESIAN_POINT('',(117.904268935444,5.2,65.5494067183983));
#188985=CARTESIAN_POINT('',(117.841543812465,5.2,65.8720978914024));
#188986=CARTESIAN_POINT('',(117.904268935444,5.2,65.5494067183983));
#188987=CARTESIAN_POINT('',(117.390182135468,5.2,65.5737319002038));
#188988=CARTESIAN_POINT('Origin',(116.959178380441,5.2,51.0204257716897));
#188989=CARTESIAN_POINT('',(117.327983517023,5.2,65.8937144557068));
#188990=CARTESIAN_POINT('',(117.390182135468,5.2,65.5737319002038));
#188991=CARTESIAN_POINT('Origin',(116.959178380441,5.2,51.0204257716897));
#188992=CARTESIAN_POINT('Origin',(118.156384306592,5.2,64.25239204573));
#188993=CARTESIAN_POINT('',(117.941450480778,5.7,65.3581252045768));
#188994=CARTESIAN_POINT('',(117.87786568195,5.7,65.6852390043561));
#188995=CARTESIAN_POINT('',(117.941450480778,5.7,65.3581252045768));
#188996=CARTESIAN_POINT('Origin',(120.591198299308,1.45439216225896E-14,
51.7264224494141));
#188997=CARTESIAN_POINT('Origin',(120.591198299308,1.45439216225896E-14,
51.7264224494141));
#188998=CARTESIAN_POINT('Origin',(118.156384306592,5.7,64.25239204573));
#188999=CARTESIAN_POINT('',(117.42703997039,5.7,65.3841157237722));
#189000=CARTESIAN_POINT('',(117.364003436039,5.7,65.7084089614048));
#189001=CARTESIAN_POINT('',(117.42703997039,5.7,65.3841157237722));
#189002=CARTESIAN_POINT('Origin',(116.959178380441,5.7,51.0204257716897));
#189003=CARTESIAN_POINT('Origin',(116.959178380441,5.7,51.0204257716897));
#189004=CARTESIAN_POINT('Origin',(117.665570804043,5.7,64.1569870892808));
#189005=CARTESIAN_POINT('Origin',(120.100384796758,1.45439216225896E-14,
51.6310174929649));
#189006=CARTESIAN_POINT('Origin',(120.100384796758,1.45439216225896E-14,
51.6310174929649));
#189007=CARTESIAN_POINT('Origin',(118.647197809142,5.2,64.3477970021793));
#189008=CARTESIAN_POINT('',(118.943422586228,5.2,65.44426917207));
#189009=CARTESIAN_POINT('',(118.879357457006,5.2,65.7738540451763));
#189010=CARTESIAN_POINT('',(118.943422586228,5.2,65.44426917207));
#189011=CARTESIAN_POINT('',(118.421978693774,5.2,65.5064431246532));
#189012=CARTESIAN_POINT('Origin',(116.959178380441,5.2,51.0204257716897));
#189013=CARTESIAN_POINT('',(118.358634022938,5.2,65.8323215791715));
#189014=CARTESIAN_POINT('',(118.421978693774,5.2,65.5064431246532));
#189015=CARTESIAN_POINT('Origin',(116.959178380441,5.2,51.0204257716897));
#189016=CARTESIAN_POINT('Origin',(119.138011311691,5.2,64.4432019586286));
#189017=CARTESIAN_POINT('',(118.981429396835,5.7,65.2487420576654));
#189018=CARTESIAN_POINT('',(118.916447481056,5.7,65.5830433651943));
#189019=CARTESIAN_POINT('',(118.981429396835,5.7,65.2487420576654));
#189020=CARTESIAN_POINT('Origin',(121.572825304407,1.45439216225896E-14,
51.9172323623126));
#189021=CARTESIAN_POINT('Origin',(121.572825304407,1.45439216225896E-14,
51.9172323623126));
#189022=CARTESIAN_POINT('Origin',(119.138011311691,5.7,64.4432019586286));
#189023=CARTESIAN_POINT('',(118.459541548164,5.7,65.3131999555876));
#189024=CARTESIAN_POINT('',(118.395311107302,5.7,65.6436352791055));
#189025=CARTESIAN_POINT('',(118.459541548164,5.7,65.3131999555876));
#189026=CARTESIAN_POINT('Origin',(116.959178380441,5.7,51.0204257716897));
#189027=CARTESIAN_POINT('Origin',(116.959178380441,5.7,51.0204257716897));
#189028=CARTESIAN_POINT('Origin',(118.647197809142,5.7,64.3477970021793));
#189029=CARTESIAN_POINT('Origin',(121.082011801857,1.45439216225896E-14,
51.8218274058634));
#189030=CARTESIAN_POINT('Origin',(121.082011801857,1.45439216225896E-14,
51.8218274058634));
#189031=CARTESIAN_POINT('Origin',(119.628824814241,5.2,64.5386069150778));
#189032=CARTESIAN_POINT('',(119.998065981774,5.2,65.2594441947878));
#189033=CARTESIAN_POINT('',(119.932216346204,5.2,65.5982095113747));
#189034=CARTESIAN_POINT('',(119.998065981774,5.2,65.2594441947878));
#189035=CARTESIAN_POINT('',(119.468732843108,5.2,65.3622045981111));
#189036=CARTESIAN_POINT('Origin',(116.959178380441,5.2,51.0204257716897));
#189037=CARTESIAN_POINT('',(119.403836680514,5.2,65.696064745953));
#189038=CARTESIAN_POINT('',(119.468732843108,5.2,65.3622045981111));
#189039=CARTESIAN_POINT('Origin',(116.959178380441,5.2,51.0204257716897));
#189040=CARTESIAN_POINT('Origin',(120.11963831679,5.2,64.6340118715271));
#189041=CARTESIAN_POINT('',(120.037174980321,5.7,65.0582468432809));
#189042=CARTESIAN_POINT('',(119.970328561956,5.7,65.4021401372109));
#189043=CARTESIAN_POINT('',(120.037174980321,5.7,65.0582468432809));
#189044=CARTESIAN_POINT('Origin',(122.554452309506,1.45439216225896E-14,
52.1080422752111));
#189045=CARTESIAN_POINT('Origin',(122.554452309506,1.45439216225896E-14,
52.1080422752111));
#189046=CARTESIAN_POINT('Origin',(120.11963831679,5.7,64.6340118715271));
#189047=CARTESIAN_POINT('',(119.507252479224,5.7,65.1640392383386));
#189048=CARTESIAN_POINT('',(119.441402843655,5.7,65.5028045549254));
#189049=CARTESIAN_POINT('',(119.507252479224,5.7,65.1640392383386));
#189050=CARTESIAN_POINT('Origin',(116.959178380441,5.7,51.0204257716897));
#189051=CARTESIAN_POINT('Origin',(116.959178380441,5.7,51.0204257716897));
#189052=CARTESIAN_POINT('Origin',(119.628824814241,5.7,64.5386069150778));
#189053=CARTESIAN_POINT('Origin',(122.063638806956,1.45439216225896E-14,
52.0126373187619));
#189054=CARTESIAN_POINT('Origin',(122.063638806956,1.45439216225896E-14,
52.0126373187619));
#189055=CARTESIAN_POINT('Origin',(119.628824814241,4.2,64.5386069150778));
#189056=CARTESIAN_POINT('',(119.931982055812,4.2,65.5994148249354));
#189057=CARTESIAN_POINT('',(119.867751614951,4.2,65.9298501484533));
#189058=CARTESIAN_POINT('',(119.931982055812,4.2,65.5994148249354));
#189059=CARTESIAN_POINT('',(119.403605698873,4.2,65.6972530375517));
#189060=CARTESIAN_POINT('Origin',(116.959178380441,4.2,51.0204257716897));
#189061=CARTESIAN_POINT('',(119.340261028037,4.2,66.02313149207));
#189062=CARTESIAN_POINT('',(119.403605698873,4.2,65.6972530375517));
#189063=CARTESIAN_POINT('Origin',(116.959178380441,4.2,51.0204257716897));
#189064=CARTESIAN_POINT('Origin',(120.11963831679,4.2,64.6340118715271));
#189065=CARTESIAN_POINT('',(119.963056401934,4.7,65.4395519705639));
#189066=CARTESIAN_POINT('',(119.898074486155,4.7,65.7738532780928));
#189067=CARTESIAN_POINT('',(119.963056401934,4.7,65.4395519705639));
#189068=CARTESIAN_POINT('Origin',(122.554452309506,1.45439216225896E-14,
52.1080422752111));
#189069=CARTESIAN_POINT('Origin',(122.554452309506,1.45439216225896E-14,
52.1080422752111));
#189070=CARTESIAN_POINT('Origin',(120.11963831679,4.7,64.6340118715271));
#189071=CARTESIAN_POINT('',(119.434236088778,4.7,65.5396741285193));
#189072=CARTESIAN_POINT('',(119.370170959555,4.7,65.8692590016255));
#189073=CARTESIAN_POINT('',(119.434236088778,4.7,65.5396741285193));
#189074=CARTESIAN_POINT('Origin',(116.959178380441,4.7,51.0204257716897));
#189075=CARTESIAN_POINT('Origin',(116.959178380441,4.7,51.0204257716897));
#189076=CARTESIAN_POINT('Origin',(119.628824814241,4.7,64.5386069150778));
#189077=CARTESIAN_POINT('Origin',(122.063638806956,1.45439216225896E-14,
52.0126373187619));
#189078=CARTESIAN_POINT('Origin',(122.063638806956,1.45439216225896E-14,
52.0126373187619));
#189079=CARTESIAN_POINT('Origin',(119.628824814241,3.2,64.5386069150778));
#189080=CARTESIAN_POINT('',(119.881107483137,3.2,65.8611405060185));
#189081=CARTESIAN_POINT('',(119.818070948787,3.2,66.1854337436511));
#189082=CARTESIAN_POINT('',(119.881107483137,3.2,65.8611405060185));
#189083=CARTESIAN_POINT('',(119.353436145666,3.2,65.9553517260008));
#189084=CARTESIAN_POINT('Origin',(116.959178380441,3.2,51.0204257716897));
#189085=CARTESIAN_POINT('',(119.291237527222,3.2,66.2753342815038));
#189086=CARTESIAN_POINT('',(119.353436145666,3.2,65.9553517260008));
#189087=CARTESIAN_POINT('Origin',(116.959178380441,3.2,51.0204257716897));
#189088=CARTESIAN_POINT('Origin',(120.11963831679,3.2,64.6340118715271));
#189089=CARTESIAN_POINT('',(119.904704490976,3.7,65.7397450303738));
#189090=CARTESIAN_POINT('',(119.841119692148,3.7,66.0668588301531));
#189091=CARTESIAN_POINT('',(119.904704490976,3.7,65.7397450303738));
#189092=CARTESIAN_POINT('Origin',(122.554452309506,1.45439216225896E-14,
52.1080422752111));
#189093=CARTESIAN_POINT('Origin',(122.554452309506,1.45439216225896E-14,
52.1080422752111));
#189094=CARTESIAN_POINT('Origin',(120.11963831679,3.7,64.6340118715271));
#189095=CARTESIAN_POINT('',(119.376709443092,3.7,65.835621587746));
#189096=CARTESIAN_POINT('',(119.313984320114,3.7,66.1583127607501));
#189097=CARTESIAN_POINT('',(119.376709443092,3.7,65.835621587746));
#189098=CARTESIAN_POINT('Origin',(116.959178380441,3.7,51.0204257716897));
#189099=CARTESIAN_POINT('Origin',(116.959178380441,3.7,51.0204257716897));
#189100=CARTESIAN_POINT('Origin',(119.628824814241,3.7,64.5386069150778));
#189101=CARTESIAN_POINT('Origin',(122.063638806956,1.45439216225896E-14,
52.0126373187619));
#189102=CARTESIAN_POINT('Origin',(122.063638806956,1.45439216225896E-14,
52.0126373187619));
#189103=CARTESIAN_POINT('Origin',(119.628824814241,2.2,64.5386069150778));
#189104=CARTESIAN_POINT('',(119.844585514972,2.2,66.0490288063989));
#189105=CARTESIAN_POINT('',(119.782379360477,2.2,66.3690501313291));
#189106=CARTESIAN_POINT('',(119.844585514972,2.2,66.0490288063989));
#189107=CARTESIAN_POINT('',(119.317404303366,2.2,66.1407185599755));
#189108=CARTESIAN_POINT('Origin',(116.959178380441,2.2,51.0204257716897));
#189109=CARTESIAN_POINT('',(119.256003798747,2.2,66.4565951962854));
#189110=CARTESIAN_POINT('',(119.317404303366,2.2,66.1407185599755));
#189111=CARTESIAN_POINT('Origin',(116.959178380441,2.2,51.0204257716897));
#189112=CARTESIAN_POINT('Origin',(120.11963831679,2.2,64.6340118715271));
#189113=CARTESIAN_POINT('',(119.861094292437,2.7,65.9640989328148));
#189114=CARTESIAN_POINT('',(119.798515481723,2.7,66.2860373982266));
#189115=CARTESIAN_POINT('',(119.861094292437,2.7,65.9640989328148));
#189116=CARTESIAN_POINT('Origin',(122.554452309506,1.45439216225896E-14,
52.1080422752111));
#189117=CARTESIAN_POINT('Origin',(122.554452309506,1.45439216225896E-14,
52.1080422752111));
#189118=CARTESIAN_POINT('Origin',(120.11963831679,2.7,64.6340118715271));
#189119=CARTESIAN_POINT('',(119.33369314583,2.7,66.0569201482357));
#189120=CARTESIAN_POINT('',(119.271934362838,2.7,66.3746399577931));
#189121=CARTESIAN_POINT('',(119.33369314583,2.7,66.0569201482357));
#189122=CARTESIAN_POINT('Origin',(116.959178380441,2.7,51.0204257716897));
#189123=CARTESIAN_POINT('Origin',(116.959178380441,2.7,51.0204257716897));
#189124=CARTESIAN_POINT('Origin',(119.628824814241,2.7,64.5386069150778));
#189125=CARTESIAN_POINT('Origin',(122.063638806956,1.45439216225896E-14,
52.0126373187619));
#189126=CARTESIAN_POINT('Origin',(122.063638806956,1.45439216225896E-14,
52.0126373187619));
#189127=CARTESIAN_POINT('Origin',(119.628824814241,1.2,64.5386069150778));
#189128=CARTESIAN_POINT('',(119.821840613373,1.2,66.1660405973442));
#189129=CARTESIAN_POINT('',(119.760140753424,1.2,66.4834572756331));
#189130=CARTESIAN_POINT('',(119.821840613373,1.2,66.1660405973442));
#189131=CARTESIAN_POINT('',(119.294958148874,1.2,66.2561934379564));
#189132=CARTESIAN_POINT('Origin',(116.959178380441,1.2,51.0204257716897));
#189133=CARTESIAN_POINT('',(119.234044670503,1.2,66.5695645539299));
#189134=CARTESIAN_POINT('',(119.294958148874,1.2,66.2561934379564));
#189135=CARTESIAN_POINT('Origin',(116.959178380441,1.2,51.0204257716897));
#189136=CARTESIAN_POINT('Origin',(120.11963831679,1.2,64.6340118715271));
#189137=CARTESIAN_POINT('',(119.831517409679,1.7,66.1162580444744));
#189138=CARTESIAN_POINT('',(119.769603146747,1.7,66.4347777249832));
#189139=CARTESIAN_POINT('',(119.831517409679,1.7,66.1162580444744));
#189140=CARTESIAN_POINT('Origin',(122.554452309506,1.45439216225896E-14,
52.1080422752111));
#189141=CARTESIAN_POINT('Origin',(122.554452309506,1.45439216225896E-14,
52.1080422752111));
#189142=CARTESIAN_POINT('Origin',(120.11963831679,1.7,64.6340118715271));
#189143=CARTESIAN_POINT('',(119.304508441553,1.7,66.2070616865831));
#189144=CARTESIAN_POINT('',(119.243388682605,1.7,66.5214940188289));
#189145=CARTESIAN_POINT('',(119.304508441553,1.7,66.2070616865831));
#189146=CARTESIAN_POINT('Origin',(116.959178380441,1.7,51.0204257716897));
#189147=CARTESIAN_POINT('Origin',(116.959178380441,1.7,51.0204257716897));
#189148=CARTESIAN_POINT('Origin',(119.628824814241,1.7,64.5386069150778));
#189149=CARTESIAN_POINT('Origin',(122.063638806956,1.45439216225896E-14,
52.0126373187619));
#189150=CARTESIAN_POINT('Origin',(122.063638806956,1.45439216225896E-14,
52.0126373187619));
#189151=CARTESIAN_POINT('Origin',(119.628824814241,0.200000000000015,64.5386069150778));
#189152=CARTESIAN_POINT('',(119.812529904723,0.200000000000015,66.2139398018886));
#189153=CARTESIAN_POINT('',(119.751034954835,0.200000000000015,66.530302314559));
#189154=CARTESIAN_POINT('',(119.812529904723,0.200000000000015,66.2139398018886));
#189155=CARTESIAN_POINT('',(119.285768331495,0.200000000000015,66.3034707139332));
#189156=CARTESIAN_POINT('Origin',(116.959178380441,0.200000000000015,51.0204257716897));
#189157=CARTESIAN_POINT('',(119.225052051358,0.200000000000015,66.615827338));
#189158=CARTESIAN_POINT('',(119.285768331495,0.200000000000015,66.3034707139332));
#189159=CARTESIAN_POINT('Origin',(116.959178380441,0.200000000000015,51.0204257716897));
#189160=CARTESIAN_POINT('Origin',(120.11963831679,0.200000000000015,64.6340118715271));
#189161=CARTESIAN_POINT('',(119.815519180792,0.700000000000015,66.1985613864261));
#189162=CARTESIAN_POINT('',(119.753958589789,0.700000000000015,66.5152615916749));
#189163=CARTESIAN_POINT('',(119.815519180792,0.700000000000015,66.1985613864261));
#189164=CARTESIAN_POINT('Origin',(122.554452309506,1.45439216225896E-14,
52.1080422752111));
#189165=CARTESIAN_POINT('Origin',(122.554452309506,1.45439216225896E-14,
52.1080422752111));
#189166=CARTESIAN_POINT('Origin',(120.11963831679,0.700000000000015,64.6340118715271));
#189167=CARTESIAN_POINT('',(119.288718882318,0.700000000000015,66.2882915215953));
#189168=CARTESIAN_POINT('',(119.227939426069,0.700000000000015,66.6009731569646));
#189169=CARTESIAN_POINT('',(119.288718882318,0.700000000000015,66.2882915215953));
#189170=CARTESIAN_POINT('Origin',(116.959178380441,0.700000000000015,51.0204257716897));
#189171=CARTESIAN_POINT('Origin',(116.959178380441,0.700000000000015,51.0204257716897));
#189172=CARTESIAN_POINT('Origin',(119.628824814241,0.700000000000015,64.5386069150778));
#189173=CARTESIAN_POINT('Origin',(122.063638806956,1.45439216225896E-14,
52.0126373187619));
#189174=CARTESIAN_POINT('Origin',(122.063638806956,1.45439216225896E-14,
52.0126373187619));
#189175=CARTESIAN_POINT('Origin',(111.284995270899,0.200000000000015,62.9167226554405));
#189176=CARTESIAN_POINT('',(110.840889914737,0.700000000000015,65.2014352476504));
#189177=CARTESIAN_POINT('',(110.782261475414,0.700000000000015,65.5030509154767));
#189178=CARTESIAN_POINT('',(110.840889914737,0.700000000000015,65.2014352476504));
#189179=CARTESIAN_POINT('',(110.838045843825,0.200000000000015,65.2160666510678));
#189180=CARTESIAN_POINT('Origin',(113.719809263614,1.45439216225896E-14,
50.3907530591246));
#189181=CARTESIAN_POINT('',(110.779474112948,0.200000000000015,65.5173905806832));
#189182=CARTESIAN_POINT('',(110.838045843825,0.200000000000015,65.2160666510678));
#189183=CARTESIAN_POINT('Origin',(113.719809263614,1.45439216225896E-14,
50.3907530591246));
#189184=CARTESIAN_POINT('Origin',(111.284995270899,0.700000000000015,62.9167226554405));
#189185=CARTESIAN_POINT('',(110.372612258069,0.700000000000015,64.9900939933211));
#189186=CARTESIAN_POINT('',(110.313530599756,0.700000000000015,65.2940412590885));
#189187=CARTESIAN_POINT('',(110.372612258069,0.700000000000015,64.9900939933211));
#189188=CARTESIAN_POINT('Origin',(116.959178380441,0.700000000000015,51.0204257716897));
#189189=CARTESIAN_POINT('Origin',(116.959178380441,0.700000000000015,51.0204257716897));
#189190=CARTESIAN_POINT('Origin',(110.79418176835,0.700000000000015,62.8213176989913));
#189191=CARTESIAN_POINT('',(110.369745770862,0.200000000000015,65.0048407180042));
#189192=CARTESIAN_POINT('',(110.310722145193,0.200000000000015,65.3084894331871));
#189193=CARTESIAN_POINT('',(110.369745770862,0.200000000000015,65.0048407180042));
#189194=CARTESIAN_POINT('Origin',(113.228995761065,1.45439216225896E-14,
50.2953481026754));
#189195=CARTESIAN_POINT('Origin',(113.228995761065,1.45439216225896E-14,
50.2953481026754));
#189196=CARTESIAN_POINT('Origin',(110.79418176835,0.200000000000015,62.8213176989913));
#189197=CARTESIAN_POINT('Origin',(116.959178380441,0.200000000000015,51.0204257716897));
#189198=CARTESIAN_POINT('Origin',(116.959178380441,0.200000000000015,51.0204257716897));
#189199=CARTESIAN_POINT('Origin',(110.79418176835,1.2,62.8213176989913));
#189200=CARTESIAN_POINT('',(110.846903310467,1.2,65.1704991628781));
#189201=CARTESIAN_POINT('',(110.788154610309,1.2,65.4727335159764));
#189202=CARTESIAN_POINT('',(110.846903310467,1.2,65.1704991628781));
#189203=CARTESIAN_POINT('',(110.378673197833,1.2,64.958913316921));
#189204=CARTESIAN_POINT('Origin',(116.959178380441,1.2,51.0204257716897));
#189205=CARTESIAN_POINT('',(110.319468461813,1.2,65.2634937594351));
#189206=CARTESIAN_POINT('',(110.378673197833,1.2,64.958913316921));
#189207=CARTESIAN_POINT('Origin',(116.959178380441,1.2,51.0204257716897));
#189208=CARTESIAN_POINT('Origin',(111.284995270899,1.2,62.9167226554405));
#189209=CARTESIAN_POINT('',(110.856105996431,1.7,65.1231556841011));
#189210=CARTESIAN_POINT('',(110.797172304788,1.7,65.4263417311382));
#189211=CARTESIAN_POINT('',(110.856105996431,1.7,65.1231556841011));
#189212=CARTESIAN_POINT('Origin',(113.719809263614,1.45439216225896E-14,
50.3907530591246));
#189213=CARTESIAN_POINT('Origin',(113.719809263614,1.45439216225896E-14,
50.3907530591246));
#189214=CARTESIAN_POINT('Origin',(111.284995270899,1.7,62.9167226554405));
#189215=CARTESIAN_POINT('',(110.387949034711,1.7,64.9111935111905));
#189216=CARTESIAN_POINT('',(110.328554951129,1.7,65.2167480576087));
#189217=CARTESIAN_POINT('',(110.387949034711,1.7,64.9111935111905));
#189218=CARTESIAN_POINT('Origin',(116.959178380441,1.7,51.0204257716897));
#189219=CARTESIAN_POINT('Origin',(116.959178380441,1.7,51.0204257716897));
#189220=CARTESIAN_POINT('Origin',(110.79418176835,1.7,62.8213176989913));
#189221=CARTESIAN_POINT('Origin',(113.228995761065,1.45439216225896E-14,
50.2953481026754));
#189222=CARTESIAN_POINT('Origin',(113.228995761065,1.45439216225896E-14,
50.2953481026754));
#189223=CARTESIAN_POINT('Origin',(110.79418176835,2.2,62.8213176989913));
#189224=CARTESIAN_POINT('',(110.868528853359,2.2,65.0592459445302));
#189225=CARTESIAN_POINT('',(110.809343601815,2.2,65.3637261486052));
#189226=CARTESIAN_POINT('',(110.868528853359,2.2,65.0592459445302));
#189227=CARTESIAN_POINT('',(110.40047139724,2.2,64.8467718622361));
#189228=CARTESIAN_POINT('Origin',(116.959178380441,2.2,51.0204257716897));
#189229=CARTESIAN_POINT('',(110.340819785234,2.2,65.1536512709261));
#189230=CARTESIAN_POINT('',(110.40047139724,2.2,64.8467718622361));
#189231=CARTESIAN_POINT('Origin',(116.959178380441,2.2,51.0204257716897));
#189232=CARTESIAN_POINT('Origin',(111.284995270899,2.2,62.9167226554405));
#189233=CARTESIAN_POINT('',(110.884214204038,2.7,64.9785522133862));
#189234=CARTESIAN_POINT('',(110.824708275305,2.7,65.2846821503487));
#189235=CARTESIAN_POINT('',(110.884214204038,2.7,64.9785522133862));
#189236=CARTESIAN_POINT('Origin',(113.719809263614,1.45439216225896E-14,
50.3907530591246));
#189237=CARTESIAN_POINT('Origin',(113.719809263614,1.45439216225896E-14,
50.3907530591246));
#189238=CARTESIAN_POINT('Origin',(111.284995270899,2.7,62.9167226554405));
#189239=CARTESIAN_POINT('',(110.416283646265,2.7,64.7654252989529));
#189240=CARTESIAN_POINT('',(110.356303673257,2.7,65.0739939701296));
#189241=CARTESIAN_POINT('',(110.416283646265,2.7,64.7654252989529));
#189242=CARTESIAN_POINT('Origin',(116.959178380441,2.7,51.0204257716897));
#189243=CARTESIAN_POINT('Origin',(116.959178380441,2.7,51.0204257716897));
#189244=CARTESIAN_POINT('Origin',(110.79418176835,2.7,62.8213176989913));
#189245=CARTESIAN_POINT('Origin',(113.228995761065,1.45439216225896E-14,
50.2953481026754));
#189246=CARTESIAN_POINT('Origin',(113.228995761065,1.45439216225896E-14,
50.2953481026754));
#189247=CARTESIAN_POINT('Origin',(110.79418176835,3.2,62.8213176989913));
#189248=CARTESIAN_POINT('',(110.903216553537,3.2,64.8807940877961));
#189249=CARTESIAN_POINT('',(110.84331749671,3.2,65.188946483383));
#189250=CARTESIAN_POINT('',(110.903216553537,3.2,64.8807940877961));
#189251=CARTESIAN_POINT('',(110.435441646089,3.2,64.6668664258578));
#189252=CARTESIAN_POINT('Origin',(116.959178380441,3.2,51.0204257716897));
#189253=CARTESIAN_POINT('',(110.375059009152,3.2,64.9775066130281));
#189254=CARTESIAN_POINT('',(110.435441646089,3.2,64.6668664258578));
#189255=CARTESIAN_POINT('Origin',(116.959178380441,3.2,51.0204257716897));
#189256=CARTESIAN_POINT('Origin',(111.284995270899,3.2,62.9167226554405));
#189257=CARTESIAN_POINT('',(110.925603574051,3.7,64.7656234262428));
#189258=CARTESIAN_POINT('',(110.865234719798,3.7,65.0761927080012));
#189259=CARTESIAN_POINT('',(110.925603574051,3.7,64.7656234262428));
#189260=CARTESIAN_POINT('Origin',(113.719809263614,1.45439216225896E-14,
50.3907530591246));
#189261=CARTESIAN_POINT('Origin',(113.719809263614,1.45439216225896E-14,
50.3907530591246));
#189262=CARTESIAN_POINT('Origin',(111.284995270899,3.7,62.9167226554405));
#189263=CARTESIAN_POINT('',(110.458014791367,3.7,64.5507382401787));
#189264=CARTESIAN_POINT('',(110.397150792666,3.7,64.8638548065859));
#189265=CARTESIAN_POINT('',(110.458014791367,3.7,64.5507382401787));
#189266=CARTESIAN_POINT('Origin',(116.959178380441,3.7,51.0204257716897));
#189267=CARTESIAN_POINT('Origin',(116.959178380441,3.7,51.0204257716897));
#189268=CARTESIAN_POINT('Origin',(110.79418176835,3.7,62.8213176989913));
#189269=CARTESIAN_POINT('Origin',(113.228995761065,1.45439216225896E-14,
50.2953481026754));
#189270=CARTESIAN_POINT('Origin',(113.228995761065,1.45439216225896E-14,
50.2953481026754));
#189271=CARTESIAN_POINT('Origin',(110.79418176835,4.2,62.8213176989913));
#189272=CARTESIAN_POINT('',(110.951457377512,4.2,64.6326178015551));
#189273=CARTESIAN_POINT('',(110.890536820758,4.2,64.9460253324646));
#189274=CARTESIAN_POINT('',(110.951457377512,4.2,64.6326178015551));
#189275=CARTESIAN_POINT('',(110.48408733561,4.2,64.4166072973359));
#189276=CARTESIAN_POINT('Origin',(116.959178380441,4.2,51.0204257716897));
#189277=CARTESIAN_POINT('',(110.422657817275,4.2,64.7326331955291));
#189278=CARTESIAN_POINT('',(110.48408733561,4.2,64.4166072973359));
#189279=CARTESIAN_POINT('Origin',(116.959178380441,4.2,51.0204257716897));
#189280=CARTESIAN_POINT('Origin',(111.284995270899,4.2,62.9167226554405));
#189281=CARTESIAN_POINT('',(110.980876134901,4.7,64.4812721703395));
#189282=CARTESIAN_POINT('',(110.919315543898,4.7,64.7979723755884));
#189283=CARTESIAN_POINT('',(110.980876134901,4.7,64.4812721703395));
#189284=CARTESIAN_POINT('Origin',(113.719809263614,1.45439216225896E-14,
50.3907530591246));
#189285=CARTESIAN_POINT('Origin',(113.719809263614,1.45439216225896E-14,
50.3907530591246));
#189286=CARTESIAN_POINT('Origin',(111.284995270899,4.7,62.9167226554405));
#189287=CARTESIAN_POINT('',(110.513760083927,4.7,64.2639550025948));
#189288=CARTESIAN_POINT('',(110.451674178493,4.7,64.5833577028194));
#189289=CARTESIAN_POINT('',(110.513760083927,4.7,64.2639550025948));
#189290=CARTESIAN_POINT('Origin',(116.959178380441,4.7,51.0204257716897));
#189291=CARTESIAN_POINT('Origin',(116.959178380441,4.7,51.0204257716897));
#189292=CARTESIAN_POINT('Origin',(110.79418176835,4.7,62.8213176989913));
#189293=CARTESIAN_POINT('Origin',(113.228995761065,1.45439216225896E-14,
50.2953481026754));
#189294=CARTESIAN_POINT('Origin',(113.228995761065,1.45439216225896E-14,
50.2953481026754));
#189295=CARTESIAN_POINT('Origin',(111.775808773449,4.2,63.0121276118898));
#189296=CARTESIAN_POINT('',(111.896501450699,4.2,65.0116296445541));
#189297=CARTESIAN_POINT('',(111.836358656514,4.2,65.3210359538879));
#189298=CARTESIAN_POINT('',(111.896501450699,4.2,65.0116296445541));
#189299=CARTESIAN_POINT('',(111.422286729203,4.2,64.830831788513));
#189300=CARTESIAN_POINT('Origin',(116.959178380441,4.2,51.0204257716897));
#189301=CARTESIAN_POINT('',(111.361793489841,4.2,65.142040972989));
#189302=CARTESIAN_POINT('',(111.422286729203,4.2,64.830831788513));
#189303=CARTESIAN_POINT('Origin',(116.959178380441,4.2,51.0204257716897));
#189304=CARTESIAN_POINT('Origin',(112.266622275998,4.2,63.107532568339));
#189305=CARTESIAN_POINT('',(111.925532478671,4.7,64.862278698319));
#189306=CARTESIAN_POINT('',(111.864774103035,4.7,65.1748518838705));
#189307=CARTESIAN_POINT('',(111.925532478671,4.7,64.862278698319));
#189308=CARTESIAN_POINT('Origin',(114.701436268713,1.45439216225896E-14,
50.5815629720231));
#189309=CARTESIAN_POINT('Origin',(114.701436268713,1.45439216225896E-14,
50.5815629720231));
#189310=CARTESIAN_POINT('Origin',(112.266622275998,4.7,63.107532568339));
#189311=CARTESIAN_POINT('',(111.451492400761,4.7,64.6805823833951));
#189312=CARTESIAN_POINT('',(111.390372641813,4.7,64.9950147156409));
#189313=CARTESIAN_POINT('',(111.451492400761,4.7,64.6805823833951));
#189314=CARTESIAN_POINT('Origin',(116.959178380441,4.7,51.0204257716897));
#189315=CARTESIAN_POINT('Origin',(116.959178380441,4.7,51.0204257716897));
#189316=CARTESIAN_POINT('Origin',(111.775808773449,4.7,63.0121276118898));
#189317=CARTESIAN_POINT('Origin',(114.210622766164,1.45439216225896E-14,
50.4861580155739));
#189318=CARTESIAN_POINT('Origin',(114.210622766164,1.45439216225896E-14,
50.4861580155739));
#189319=CARTESIAN_POINT('Origin',(112.757435778548,4.2,63.2029375247883));
#189320=CARTESIAN_POINT('',(112.854860725266,4.2,65.322141056661));
#189321=CARTESIAN_POINT('',(112.79520246584,4.2,65.6290546631941));
#189322=CARTESIAN_POINT('',(112.854860725266,4.2,65.322141056661));
#189323=CARTESIAN_POINT('',(112.374041723553,4.2,65.1753191073788));
#189324=CARTESIAN_POINT('Origin',(116.959178380441,4.2,51.0204257716897));
#189325=CARTESIAN_POINT('',(112.314176285267,4.2,65.4832985514289));
#189326=CARTESIAN_POINT('',(112.374041723553,4.2,65.1753191073788));
#189327=CARTESIAN_POINT('Origin',(116.959178380441,4.2,51.0204257716897));
#189328=CARTESIAN_POINT('Origin',(113.248249281097,4.2,63.2983424812375));
#189329=CARTESIAN_POINT('',(112.883650447187,4.7,65.1740315162422));
#189330=CARTESIAN_POINT('',(112.82339151564,4.7,65.4840352975252));
#189331=CARTESIAN_POINT('',(112.883650447187,4.7,65.1740315162422));
#189332=CARTESIAN_POINT('Origin',(115.683063273812,1.45439216225896E-14,
50.7723728849216));
#189333=CARTESIAN_POINT('Origin',(115.683063273812,1.45439216225896E-14,
50.7723728849216));
#189334=CARTESIAN_POINT('Origin',(113.248249281097,4.7,63.2983424812375));
#189335=CARTESIAN_POINT('',(112.40293460111,4.7,65.0266788798666));
#189336=CARTESIAN_POINT('',(112.342462146009,4.7,65.337781139129));
#189337=CARTESIAN_POINT('',(112.40293460111,4.7,65.0266788798666));
#189338=CARTESIAN_POINT('Origin',(116.959178380441,4.7,51.0204257716897));
#189339=CARTESIAN_POINT('Origin',(116.959178380441,4.7,51.0204257716897));
#189340=CARTESIAN_POINT('Origin',(112.757435778548,4.7,63.2029375247883));
#189341=CARTESIAN_POINT('Origin',(115.192249771263,1.45439216225896E-14,
50.6769679284724));
#189342=CARTESIAN_POINT('Origin',(115.192249771263,1.45439216225896E-14,
50.6769679284724));
#189343=CARTESIAN_POINT('Origin',(113.739062783647,4.2,63.3937474376868));
#189344=CARTESIAN_POINT('',(113.826207738508,4.2,65.5658366790392));
#189345=CARTESIAN_POINT('',(113.76676110055,4.2,65.8716615929319));
#189346=CARTESIAN_POINT('',(113.826207738508,4.2,65.5658366790392));
#189347=CARTESIAN_POINT('',(113.338923778585,4.2,65.4522738905049));
#189348=CARTESIAN_POINT('Origin',(116.959178380441,4.2,51.0204257716897));
#189349=CARTESIAN_POINT('',(113.27940465001,4.2,65.7584717344309));
#189350=CARTESIAN_POINT('',(113.338923778585,4.2,65.4522738905049));
#189351=CARTESIAN_POINT('Origin',(116.959178380441,4.2,51.0204257716897));
#189352=CARTESIAN_POINT('Origin',(114.229876286196,4.2,63.489152394136));
#189353=CARTESIAN_POINT('',(113.854892127718,4.7,65.4182690257343));
#189354=CARTESIAN_POINT('',(113.794851251881,4.7,65.7271510132369));
#189355=CARTESIAN_POINT('',(113.854892127718,4.7,65.4182690257343));
#189356=CARTESIAN_POINT('Origin',(116.664690278911,1.45439216225896E-14,
50.9631827978201));
#189357=CARTESIAN_POINT('Origin',(116.664690278911,1.45439216225896E-14,
50.9631827978201));
#189358=CARTESIAN_POINT('Origin',(114.229876286196,4.7,63.489152394136));
#189359=CARTESIAN_POINT('',(113.367644245392,4.7,65.3045206349844));
#189360=CARTESIAN_POINT('',(113.307528680178,4.7,65.6137868641028));
#189361=CARTESIAN_POINT('',(113.367644245392,4.7,65.3045206349844));
#189362=CARTESIAN_POINT('Origin',(116.959178380441,4.7,51.0204257716897));
#189363=CARTESIAN_POINT('Origin',(116.959178380441,4.7,51.0204257716897));
#189364=CARTESIAN_POINT('Origin',(113.739062783647,4.7,63.3937474376868));
#189365=CARTESIAN_POINT('Origin',(116.173876776362,1.45439216225896E-14,
50.8677778413709));
#189366=CARTESIAN_POINT('Origin',(116.173876776362,1.45439216225896E-14,
50.8677778413709));
#189367=CARTESIAN_POINT('Origin',(114.720689788746,4.2,63.5845573505853));
#189368=CARTESIAN_POINT('',(114.810401248048,4.2,65.7434431370981));
#189369=CARTESIAN_POINT('',(114.750901915942,4.2,66.0495391375266));
#189370=CARTESIAN_POINT('',(114.810401248048,4.2,65.7434431370981));
#189371=CARTESIAN_POINT('',(114.31670059115,4.2,65.6628912280229));
#189372=CARTESIAN_POINT('Origin',(116.959178380441,4.2,51.0204257716897));
#189373=CARTESIAN_POINT('',(114.25726053012,4.2,65.9686823067247));
#189374=CARTESIAN_POINT('',(114.31670059115,4.2,65.6628912280229));
#189375=CARTESIAN_POINT('Origin',(116.959178380441,4.2,51.0204257716897));
#189376=CARTESIAN_POINT('Origin',(115.211503291295,4.2,63.6799623070345));
#189377=CARTESIAN_POINT('',(114.83911186201,4.7,65.595740569812));
#189378=CARTESIAN_POINT('',(114.779016694271,4.7,65.9049018635434));
#189379=CARTESIAN_POINT('',(114.83911186201,4.7,65.595740569812));
#189380=CARTESIAN_POINT('Origin',(117.64631728401,1.45439216225896E-14,
51.1539927107186));
#189381=CARTESIAN_POINT('Origin',(117.64631728401,1.45439216225896E-14,
51.1539927107186));
#189382=CARTESIAN_POINT('Origin',(115.211503291295,4.7,63.6799623070345));
#189383=CARTESIAN_POINT('',(114.345381707316,4.7,65.5153404129881));
#189384=CARTESIAN_POINT('',(114.285347607624,4.7,65.8241875404224));
#189385=CARTESIAN_POINT('',(114.345381707316,4.7,65.5153404129881));
#189386=CARTESIAN_POINT('Origin',(116.959178380441,4.7,51.0204257716897));
#189387=CARTESIAN_POINT('Origin',(116.959178380441,4.7,51.0204257716897));
#189388=CARTESIAN_POINT('Origin',(114.720689788746,4.7,63.5845573505853));
#189389=CARTESIAN_POINT('Origin',(117.155503781461,1.45439216225896E-14,
51.0585877542694));
#189390=CARTESIAN_POINT('Origin',(117.155503781461,1.45439216225896E-14,
51.0585877542694));
#189391=CARTESIAN_POINT('Origin',(115.702316793845,4.2,63.7753672634838));
#189392=CARTESIAN_POINT('',(115.807476322943,4.2,65.8547800170803));
#189393=CARTESIAN_POINT('',(115.747657855648,4.2,66.1625178175346));
#189394=CARTESIAN_POINT('',(115.807476322943,4.2,65.8547800170803));
#189395=CARTESIAN_POINT('',(115.307319527602,4.2,65.8074418952141));
#189396=CARTESIAN_POINT('Origin',(116.959178380441,4.2,51.0204257716897));
#189397=CARTESIAN_POINT('',(115.247694483068,4.2,66.1141846267932));
#189398=CARTESIAN_POINT('',(115.307319527602,4.2,65.8074418952141));
#189399=CARTESIAN_POINT('Origin',(116.959178380441,4.2,51.0204257716897));
#189400=CARTESIAN_POINT('Origin',(116.193130296394,4.2,63.870772219933));
#189401=CARTESIAN_POINT('',(115.836345810381,4.7,65.7062601206949));
#189402=CARTESIAN_POINT('',(115.775921768676,4.7,66.01711331587));
#189403=CARTESIAN_POINT('',(115.836345810381,4.7,65.7062601206949));
#189404=CARTESIAN_POINT('Origin',(118.62794428911,1.45439216225896E-14,
51.3448026236171));
#189405=CARTESIAN_POINT('Origin',(118.62794428911,1.45439216225896E-14,
51.3448026236171));
#189406=CARTESIAN_POINT('Origin',(116.193130296394,4.7,63.870772219933));
#189407=CARTESIAN_POINT('',(115.336092714776,4.7,65.6594174182724));
#189408=CARTESIAN_POINT('',(115.275868011104,4.7,65.9692451132811));
#189409=CARTESIAN_POINT('',(115.336092714776,4.7,65.6594174182724));
#189410=CARTESIAN_POINT('Origin',(116.959178380441,4.7,51.0204257716897));
#189411=CARTESIAN_POINT('Origin',(116.959178380441,4.7,51.0204257716897));
#189412=CARTESIAN_POINT('Origin',(115.702316793845,4.7,63.7753672634838));
#189413=CARTESIAN_POINT('Origin',(118.13713078656,1.45439216225896E-14,
51.2493976671679));
#189414=CARTESIAN_POINT('Origin',(118.13713078656,1.45439216225896E-14,
51.2493976671679));
#189415=CARTESIAN_POINT('Origin',(116.683943798944,4.2,63.9661771763823));
#189416=CARTESIAN_POINT('',(116.817646780977,4.2,65.8987473273376));
#189417=CARTESIAN_POINT('',(116.757229645983,4.2,66.2095649907366));
#189418=CARTESIAN_POINT('',(116.817646780977,4.2,65.8987473273376));
#189419=CARTESIAN_POINT('',(116.310903962914,4.2,65.8852911860356));
#189420=CARTESIAN_POINT('Origin',(116.959178380441,4.2,51.0204257716897));
#189421=CARTESIAN_POINT('',(116.250822381959,4.2,66.1943825821719));
#189422=CARTESIAN_POINT('',(116.310903962914,4.2,65.8852911860356));
#189423=CARTESIAN_POINT('Origin',(116.959178380441,4.2,51.0204257716897));
#189424=CARTESIAN_POINT('Origin',(117.174757301493,4.2,64.0615821328315));
#189425=CARTESIAN_POINT('',(116.846814517752,4.7,65.7486930787876));
#189426=CARTESIAN_POINT('',(116.785773249647,4.7,66.062721612669));
#189427=CARTESIAN_POINT('',(116.846814517752,4.7,65.7486930787876));
#189428=CARTESIAN_POINT('Origin',(119.609571294209,1.45439216225896E-14,
51.5356125365156));
#189429=CARTESIAN_POINT('Origin',(119.609571294209,1.45439216225896E-14,
51.5356125365156));
#189430=CARTESIAN_POINT('Origin',(117.174757301493,4.7,64.0615821328315));
#189431=CARTESIAN_POINT('',(116.339904495447,4.7,65.7360971244494));
#189432=CARTESIAN_POINT('',(116.27920923027,4.7,66.0483456364567));
#189433=CARTESIAN_POINT('',(116.339904495447,4.7,65.7360971244494));
#189434=CARTESIAN_POINT('Origin',(116.959178380441,4.7,51.0204257716897));
#189435=CARTESIAN_POINT('Origin',(116.959178380441,4.7,51.0204257716897));
#189436=CARTESIAN_POINT('Origin',(116.683943798944,4.7,63.9661771763823));
#189437=CARTESIAN_POINT('Origin',(119.118757791659,1.45439216225896E-14,
51.4402075800664));
#189438=CARTESIAN_POINT('Origin',(119.118757791659,1.45439216225896E-14,
51.4402075800664));
#189439=CARTESIAN_POINT('Origin',(117.665570804043,4.2,64.1569870892808));
#189440=CARTESIAN_POINT('',(117.841320378148,4.2,65.8732473555792));
#189441=CARTESIAN_POINT('',(117.779999449725,4.2,66.1887146098929));
#189442=CARTESIAN_POINT('',(117.841320378148,4.2,65.8732473555792));
#189443=CARTESIAN_POINT('',(117.327761915775,4.2,65.894854489609));
#189444=CARTESIAN_POINT('Origin',(116.959178380441,4.2,51.0204257716897));
#189445=CARTESIAN_POINT('',(117.266933185955,4.2,66.2077896142598));
#189446=CARTESIAN_POINT('',(117.327761915775,4.2,65.894854489609));
#189447=CARTESIAN_POINT('Origin',(116.959178380441,4.2,51.0204257716897));
#189448=CARTESIAN_POINT('Origin',(118.156384306592,4.2,64.25239204573));
#189449=CARTESIAN_POINT('',(117.870938918374,4.7,65.7208739358971));
#189450=CARTESIAN_POINT('',(117.808965115304,4.7,66.0396999223345));
#189451=CARTESIAN_POINT('',(117.870938918374,4.7,65.7208739358971));
#189452=CARTESIAN_POINT('Origin',(120.591198299308,1.45439216225896E-14,
51.7264224494141));
#189453=CARTESIAN_POINT('Origin',(120.591198299308,1.45439216225896E-14,
51.7264224494141));
#189454=CARTESIAN_POINT('Origin',(118.156384306592,4.7,64.25239204573));
#189455=CARTESIAN_POINT('',(117.357134870407,4.7,65.7437444919779));
#189456=CARTESIAN_POINT('',(117.295669027016,4.7,66.0599572654489));
#189457=CARTESIAN_POINT('',(117.357134870407,4.7,65.7437444919779));
#189458=CARTESIAN_POINT('Origin',(116.959178380441,4.7,51.0204257716897));
#189459=CARTESIAN_POINT('Origin',(116.959178380441,4.7,51.0204257716897));
#189460=CARTESIAN_POINT('Origin',(117.665570804043,4.7,64.1569870892808));
#189461=CARTESIAN_POINT('Origin',(120.100384796758,1.45439216225896E-14,
51.6310174929649));
#189462=CARTESIAN_POINT('Origin',(120.100384796758,1.45439216225896E-14,
51.6310174929649));
#189463=CARTESIAN_POINT('Origin',(118.647197809142,4.2,64.3477970021793));
#189464=CARTESIAN_POINT('',(118.879129362164,4.2,65.7750274855535));
#189465=CARTESIAN_POINT('',(118.816558223758,4.2,66.0969264805582));
#189466=CARTESIAN_POINT('',(118.879129362164,4.2,65.7750274855535));
#189467=CARTESIAN_POINT('',(118.358408432976,4.2,65.8334821331224));
#189468=CARTESIAN_POINT('Origin',(116.959178380441,4.2,51.0204257716897));
#189469=CARTESIAN_POINT('',(118.296509028281,4.2,66.1519253750136));
#189470=CARTESIAN_POINT('',(118.358408432976,4.2,65.8334821331224));
#189471=CARTESIAN_POINT('Origin',(116.959178380441,4.2,51.0204257716897));
#189472=CARTESIAN_POINT('Origin',(119.138011311691,4.2,64.4432019586286));
#189473=CARTESIAN_POINT('',(118.909372592695,4.7,65.6194403288909));
#189474=CARTESIAN_POINT('',(118.846107361872,4.7,65.9449101020099));
#189475=CARTESIAN_POINT('',(118.909372592695,4.7,65.6194403288909));
#189476=CARTESIAN_POINT('Origin',(121.572825304407,1.45439216225896E-14,
51.9172323623126));
#189477=CARTESIAN_POINT('Origin',(121.572825304407,1.45439216225896E-14,
51.9172323623126));
#189478=CARTESIAN_POINT('Origin',(119.138011311691,4.7,64.4432019586286));
#189479=CARTESIAN_POINT('',(118.388315859615,4.7,65.6796225291042));
#189480=CARTESIAN_POINT('',(118.325744721209,4.7,66.0015215241089));
#189481=CARTESIAN_POINT('',(118.388315859615,4.7,65.6796225291042));
#189482=CARTESIAN_POINT('Origin',(116.959178380441,4.7,51.0204257716897));
#189483=CARTESIAN_POINT('Origin',(116.959178380441,4.7,51.0204257716897));
#189484=CARTESIAN_POINT('Origin',(118.647197809142,4.7,64.3477970021793));
#189485=CARTESIAN_POINT('Origin',(121.082011801857,1.45439216225896E-14,
51.8218274058634));
#189486=CARTESIAN_POINT('Origin',(121.082011801857,1.45439216225896E-14,
51.8218274058634));
#189487=CARTESIAN_POINT('Origin',(118.647197809142,3.2,64.3477970021793));
#189488=CARTESIAN_POINT('',(118.829575378056,3.2,66.0299593613256));
#189489=CARTESIAN_POINT('',(118.768109534665,3.2,66.3461721347966));
#189490=CARTESIAN_POINT('',(118.829575378056,3.2,66.0299593613256));
#189491=CARTESIAN_POINT('',(118.309388920874,3.2,66.0856644025075));
#189492=CARTESIAN_POINT('Origin',(116.959178380441,3.2,51.0204257716897));
#189493=CARTESIAN_POINT('',(118.248560191054,3.2,66.3985995271583));
#189494=CARTESIAN_POINT('',(118.309388920874,3.2,66.0856644025075));
#189495=CARTESIAN_POINT('Origin',(116.959178380441,3.2,51.0204257716897));
#189496=CARTESIAN_POINT('Origin',(119.138011311691,3.2,64.4432019586286));
#189497=CARTESIAN_POINT('',(118.852565923473,3.7,65.9116838487956));
#189498=CARTESIAN_POINT('',(118.790592120403,3.7,66.230509835233));
#189499=CARTESIAN_POINT('',(118.852565923473,3.7,65.9116838487956));
#189500=CARTESIAN_POINT('Origin',(121.572825304407,1.45439216225896E-14,
51.9172323623126));
#189501=CARTESIAN_POINT('Origin',(121.572825304407,1.45439216225896E-14,
51.9172323623126));
#189502=CARTESIAN_POINT('Origin',(119.138011311691,3.7,64.4432019586286));
#189503=CARTESIAN_POINT('',(118.332133880698,3.7,65.9686523120285));
#189504=CARTESIAN_POINT('',(118.270812952274,3.7,66.2841195663421));
#189505=CARTESIAN_POINT('',(118.332133880698,3.7,65.9686523120285));
#189506=CARTESIAN_POINT('Origin',(116.959178380441,3.7,51.0204257716897));
#189507=CARTESIAN_POINT('Origin',(116.959178380441,3.7,51.0204257716897));
#189508=CARTESIAN_POINT('Origin',(118.647197809142,3.7,64.3477970021793));
#189509=CARTESIAN_POINT('Origin',(121.082011801857,1.45439216225896E-14,
51.8218274058634));
#189510=CARTESIAN_POINT('Origin',(121.082011801857,1.45439216225896E-14,
51.8218274058634));
#189511=CARTESIAN_POINT('Origin',(118.647197809142,2.2,64.3477970021793));
#189512=CARTESIAN_POINT('',(118.793972008194,2.2,66.2131219066956));
#189513=CARTESIAN_POINT('',(118.733276743018,2.2,66.5253704187029));
#189514=CARTESIAN_POINT('',(118.793972008194,2.2,66.2131219066956));
#189515=CARTESIAN_POINT('',(118.274157973112,2.2,66.2669110118326));
#189516=CARTESIAN_POINT('Origin',(116.959178380441,2.2,51.0204257716897));
#189517=CARTESIAN_POINT('',(118.214076392157,2.2,66.5760024079689));
#189518=CARTESIAN_POINT('',(118.274157973112,2.2,66.2669110118326));
#189519=CARTESIAN_POINT('Origin',(116.959178380441,2.2,51.0204257716897));
#189520=CARTESIAN_POINT('Origin',(119.138011311691,2.2,64.4432019586286));
#189521=CARTESIAN_POINT('',(118.81006852795,2.7,66.1303129045846));
#189522=CARTESIAN_POINT('',(118.749027259845,2.7,66.444341438466));
#189523=CARTESIAN_POINT('',(118.81006852795,2.7,66.1303129045846));
#189524=CARTESIAN_POINT('Origin',(121.572825304407,1.45439216225896E-14,
51.9172323623126));
#189525=CARTESIAN_POINT('Origin',(121.572825304407,1.45439216225896E-14,
51.9172323623126));
#189526=CARTESIAN_POINT('Origin',(119.138011311691,2.7,64.4432019586286));
#189527=CARTESIAN_POINT('',(118.290087288625,2.7,66.1849621966853));
#189528=CARTESIAN_POINT('',(118.229670153632,2.7,66.4957798600844));
#189529=CARTESIAN_POINT('',(118.290087288625,2.7,66.1849621966853));
#189530=CARTESIAN_POINT('Origin',(116.959178380441,2.7,51.0204257716897));
#189531=CARTESIAN_POINT('Origin',(116.959178380441,2.7,51.0204257716897));
#189532=CARTESIAN_POINT('Origin',(118.647197809142,2.7,64.3477970021793));
#189533=CARTESIAN_POINT('Origin',(121.082011801857,1.45439216225896E-14,
51.8218274058634));
#189534=CARTESIAN_POINT('Origin',(121.082011801857,1.45439216225896E-14,
51.8218274058634));
#189535=CARTESIAN_POINT('Origin',(118.647197809142,1.2,64.3477970021793));
#189536=CARTESIAN_POINT('',(118.771787232622,1.2,66.3272521134172));
#189537=CARTESIAN_POINT('',(118.711562528951,1.2,66.6370798084259));
#189538=CARTESIAN_POINT('',(118.771787232622,1.2,66.3272521134172));
#189539=CARTESIAN_POINT('',(118.252200542899,1.2,66.3798716339097));
#189540=CARTESIAN_POINT('Origin',(116.959178380441,1.2,51.0204257716897));
#189541=CARTESIAN_POINT('',(118.192575498365,1.2,66.6866143654888));
#189542=CARTESIAN_POINT('',(118.252200542899,1.2,66.3798716339097));
#189543=CARTESIAN_POINT('Origin',(116.959178380441,1.2,51.0204257716897));
#189544=CARTESIAN_POINT('Origin',(119.138011311691,1.2,64.4432019586286));
#189545=CARTESIAN_POINT('',(118.781226825678,1.7,66.2786898593904));
#189546=CARTESIAN_POINT('',(118.720802783973,1.7,66.5895430545655));
#189547=CARTESIAN_POINT('',(118.781226825678,1.7,66.2786898593904));
#189548=CARTESIAN_POINT('Origin',(121.572825304407,1.45439216225896E-14,
51.9172323623126));
#189549=CARTESIAN_POINT('Origin',(121.572825304407,1.45439216225896E-14,
51.9172323623126));
#189550=CARTESIAN_POINT('Origin',(119.138011311691,1.7,64.4432019586286));
#189551=CARTESIAN_POINT('',(118.26154383569,1.7,66.3318047993266));
#189552=CARTESIAN_POINT('',(118.201725368395,1.7,66.6395425997809));
#189553=CARTESIAN_POINT('',(118.26154383569,1.7,66.3318047993266));
#189554=CARTESIAN_POINT('Origin',(116.959178380441,1.7,51.0204257716897));
#189555=CARTESIAN_POINT('Origin',(116.959178380441,1.7,51.0204257716897));
#189556=CARTESIAN_POINT('Origin',(118.647197809142,1.7,64.3477970021793));
#189557=CARTESIAN_POINT('Origin',(121.082011801857,1.45439216225896E-14,
51.8218274058634));
#189558=CARTESIAN_POINT('Origin',(121.082011801857,1.45439216225896E-14,
51.8218274058634));
#189559=CARTESIAN_POINT('Origin',(118.647197809142,0.200000000000015,64.3477970021793));
#189560=CARTESIAN_POINT('',(118.762703230262,0.200000000000015,66.3739850210313));
#189561=CARTESIAN_POINT('',(118.70266913057,0.200000000000015,66.6828321484657));
#189562=CARTESIAN_POINT('',(118.762703230262,0.200000000000015,66.3739850210313));
#189563=CARTESIAN_POINT('',(118.243208611546,0.200000000000015,66.4261308796169));
#189564=CARTESIAN_POINT('Origin',(116.959178380441,0.200000000000015,51.0204257716897));
#189565=CARTESIAN_POINT('',(118.183768550516,0.200000000000015,66.7319219583188));
#189566=CARTESIAN_POINT('',(118.243208611546,0.200000000000015,66.4261308796169));
#189567=CARTESIAN_POINT('Origin',(116.959178380441,0.200000000000015,51.0204257716897));
#189568=CARTESIAN_POINT('Origin',(119.138011311691,0.200000000000015,64.4432019586286));
#189569=CARTESIAN_POINT('',(118.765619882406,0.700000000000015,66.358980221406));
#189570=CARTESIAN_POINT('',(118.705524714667,0.700000000000015,66.6681415151374));
#189571=CARTESIAN_POINT('',(118.765619882406,0.700000000000015,66.358980221406));
#189572=CARTESIAN_POINT('Origin',(121.572825304407,1.45439216225896E-14,
51.9172323623126));
#189573=CARTESIAN_POINT('Origin',(121.572825304407,1.45439216225896E-14,
51.9172323623126));
#189574=CARTESIAN_POINT('Origin',(119.138011311691,0.700000000000015,64.4432019586286));
#189575=CARTESIAN_POINT('',(118.246095765894,0.700000000000015,66.4112778322429));
#189576=CARTESIAN_POINT('',(118.186596433788,0.700000000000015,66.7173738326713));
#189577=CARTESIAN_POINT('',(118.246095765894,0.700000000000015,66.4112778322429));
#189578=CARTESIAN_POINT('Origin',(116.959178380441,0.700000000000015,51.0204257716897));
#189579=CARTESIAN_POINT('Origin',(116.959178380441,0.700000000000015,51.0204257716897));
#189580=CARTESIAN_POINT('Origin',(118.647197809142,0.700000000000015,64.3477970021793));
#189581=CARTESIAN_POINT('Origin',(121.082011801857,1.45439216225896E-14,
51.8218274058634));
#189582=CARTESIAN_POINT('Origin',(121.082011801857,1.45439216225896E-14,
51.8218274058634));
#189583=CARTESIAN_POINT('Origin',(111.775808773449,0.200000000000015,63.0121276118898));
#189584=CARTESIAN_POINT('',(111.784511933794,0.200000000000015,65.58776288843));
#189585=CARTESIAN_POINT('',(111.726632415304,0.200000000000015,65.8855257118037));
#189586=CARTESIAN_POINT('',(111.784511933794,0.200000000000015,65.58776288843));
#189587=CARTESIAN_POINT('',(111.30965635868,0.200000000000015,65.4102619219916));
#189588=CARTESIAN_POINT('Origin',(116.959178380441,0.200000000000015,51.0204257716897));
#189589=CARTESIAN_POINT('',(111.251464695365,0.200000000000015,65.7096305832602));
#189590=CARTESIAN_POINT('',(111.30965635868,0.200000000000015,65.4102619219916));
#189591=CARTESIAN_POINT('Origin',(116.959178380441,0.200000000000015,51.0204257716897));
#189592=CARTESIAN_POINT('Origin',(112.266622275998,0.200000000000015,63.107532568339));
#189593=CARTESIAN_POINT('',(111.787321688715,0.700000000000015,65.5733080246022));
#189594=CARTESIAN_POINT('',(111.729387450815,0.700000000000015,65.8713523535303));
#189595=CARTESIAN_POINT('',(111.787321688715,0.700000000000015,65.5733080246022));
#189596=CARTESIAN_POINT('Origin',(114.701436268713,1.45439216225896E-14,
50.5815629720231));
#189597=CARTESIAN_POINT('Origin',(114.701436268713,1.45439216225896E-14,
50.5815629720231));
#189598=CARTESIAN_POINT('Origin',(112.266622275998,0.700000000000015,63.107532568339));
#189599=CARTESIAN_POINT('',(111.31248158481,0.700000000000015,65.3957274660892));
#189600=CARTESIAN_POINT('',(111.254234311024,0.700000000000015,65.6953822170022));
#189601=CARTESIAN_POINT('',(111.31248158481,0.700000000000015,65.3957274660892));
#189602=CARTESIAN_POINT('Origin',(116.959178380441,0.700000000000015,51.0204257716897));
#189603=CARTESIAN_POINT('Origin',(116.959178380441,0.700000000000015,51.0204257716897));
#189604=CARTESIAN_POINT('Origin',(111.775808773449,0.700000000000015,63.0121276118898));
#189605=CARTESIAN_POINT('Origin',(114.210622766164,1.45439216225896E-14,
50.4861580155739));
#189606=CARTESIAN_POINT('Origin',(114.210622766164,1.45439216225896E-14,
50.4861580155739));
#189607=CARTESIAN_POINT('Origin',(111.775808773449,1.2,63.0121276118898));
#189608=CARTESIAN_POINT('',(111.793262308365,1.2,65.5427463384361));
#189609=CARTESIAN_POINT('',(111.735212040126,1.2,65.8413875887286));
#189610=CARTESIAN_POINT('',(111.793262308365,1.2,65.5427463384361));
#189611=CARTESIAN_POINT('',(111.318455014226,1.2,65.3649969891498));
#189612=CARTESIAN_POINT('Origin',(116.959178380441,1.2,51.0204257716897));
#189613=CARTESIAN_POINT('',(111.260089814989,1.2,65.6652584108877));
#189614=CARTESIAN_POINT('',(111.318455014226,1.2,65.3649969891498));
#189615=CARTESIAN_POINT('Origin',(116.959178380441,1.2,51.0204257716897));
#189616=CARTESIAN_POINT('Origin',(112.266622275998,1.2,63.107532568339));
#189617=CARTESIAN_POINT('',(111.802353039398,1.7,65.4959788149727));
#189618=CARTESIAN_POINT('',(111.74412432015,1.7,65.7955381115431));
#189619=CARTESIAN_POINT('',(111.802353039398,1.7,65.4959788149727));
#189620=CARTESIAN_POINT('Origin',(114.701436268713,1.45439216225896E-14,
50.5815629720231));
#189621=CARTESIAN_POINT('Origin',(114.701436268713,1.45439216225896E-14,
50.5815629720231));
#189622=CARTESIAN_POINT('Origin',(112.266622275998,1.7,63.107532568339));
#189623=CARTESIAN_POINT('',(111.327596215435,1.7,65.3179698204353));
#189624=CARTESIAN_POINT('',(111.269049635537,1.7,65.6191643601265));
#189625=CARTESIAN_POINT('',(111.327596215435,1.7,65.3179698204353));
#189626=CARTESIAN_POINT('Origin',(116.959178380441,1.7,51.0204257716897));
#189627=CARTESIAN_POINT('Origin',(116.959178380441,1.7,51.0204257716897));
#189628=CARTESIAN_POINT('Origin',(111.775808773449,1.7,63.0121276118898));
#189629=CARTESIAN_POINT('Origin',(114.210622766164,1.45439216225896E-14,
50.4861580155739));
#189630=CARTESIAN_POINT('Origin',(114.210622766164,1.45439216225896E-14,
50.4861580155739));
#189631=CARTESIAN_POINT('Origin',(111.775808773449,2.2,63.0121276118898));
#189632=CARTESIAN_POINT('',(111.814623641277,2.2,65.4328523558162));
#189633=CARTESIAN_POINT('',(111.756152320341,2.2,65.7336597236466));
#189634=CARTESIAN_POINT('',(111.814623641277,2.2,65.4328523558162));
#189635=CARTESIAN_POINT('',(111.339935449923,2.2,65.2544902788798));
#189636=CARTESIAN_POINT('Origin',(116.959178380441,2.2,51.0204257716897));
#189637=CARTESIAN_POINT('',(111.281142256204,2.2,65.5569535303645));
#189638=CARTESIAN_POINT('',(111.339935449923,2.2,65.2544902788798));
#189639=CARTESIAN_POINT('Origin',(116.959178380441,2.2,51.0204257716897));
#189640=CARTESIAN_POINT('Origin',(112.266622275998,2.2,63.107532568339));
#189641=CARTESIAN_POINT('',(111.830114881284,2.7,65.3531572325288));
#189642=CARTESIAN_POINT('',(111.771334410325,2.7,65.6555550314119));
#189643=CARTESIAN_POINT('',(111.830114881284,2.7,65.3531572325288));
#189644=CARTESIAN_POINT('Origin',(114.701436268713,1.45439216225896E-14,
50.5815629720231));
#189645=CARTESIAN_POINT('Origin',(114.701436268713,1.45439216225896E-14,
50.5815629720231));
#189646=CARTESIAN_POINT('Origin',(112.266622275998,2.7,63.107532568339));
#189647=CARTESIAN_POINT('',(111.355514181256,2.7,65.1743450539802));
#189648=CARTESIAN_POINT('',(111.296406675647,2.7,65.4784252918939));
#189649=CARTESIAN_POINT('',(111.355514181256,2.7,65.1743450539802));
#189650=CARTESIAN_POINT('Origin',(116.959178380441,2.7,51.0204257716897));
#189651=CARTESIAN_POINT('Origin',(116.959178380441,2.7,51.0204257716897));
#189652=CARTESIAN_POINT('Origin',(111.775808773449,2.7,63.0121276118898));
#189653=CARTESIAN_POINT('Origin',(114.210622766164,1.45439216225896E-14,
50.4861580155739));
#189654=CARTESIAN_POINT('Origin',(114.210622766164,1.45439216225896E-14,
50.4861580155739));
#189655=CARTESIAN_POINT('Origin',(111.775808773449,3.2,63.0121276118898));
#189656=CARTESIAN_POINT('',(111.848879229412,3.2,65.2566235117408));
#189657=CARTESIAN_POINT('',(111.789719927259,3.2,65.5609702184402));
#189658=CARTESIAN_POINT('',(111.848879229412,3.2,65.2566235117408));
#189659=CARTESIAN_POINT('',(111.374385790137,3.2,65.0772595272087));
#189660=CARTESIAN_POINT('Origin',(116.959178380441,3.2,51.0204257716897));
#189661=CARTESIAN_POINT('',(111.314893052466,3.2,65.3833216023821));
#189662=CARTESIAN_POINT('',(111.374385790137,3.2,65.0772595272087));
#189663=CARTESIAN_POINT('Origin',(116.959178380441,3.2,51.0204257716897));
#189664=CARTESIAN_POINT('Origin',(112.266622275998,3.2,63.107532568339));
#189665=CARTESIAN_POINT('',(111.870981781604,3.7,65.1429163055294));
#189666=CARTESIAN_POINT('',(111.811370007496,3.7,65.4495907670216));
#189667=CARTESIAN_POINT('',(111.870981781604,3.7,65.1429163055294));
#189668=CARTESIAN_POINT('Origin',(114.701436268713,1.45439216225896E-14,
50.5815629720231));
#189669=CARTESIAN_POINT('Origin',(114.701436268713,1.45439216225896E-14,
50.5815629720231));
#189670=CARTESIAN_POINT('Origin',(112.266622275998,3.7,63.107532568339));
#189671=CARTESIAN_POINT('',(111.396616525,3.7,64.9628928816151));
#189672=CARTESIAN_POINT('',(111.336663560482,3.7,65.2713226068464));
#189673=CARTESIAN_POINT('',(111.396616525,3.7,64.9628928816151));
#189674=CARTESIAN_POINT('Origin',(116.959178380441,3.7,51.0204257716897));
#189675=CARTESIAN_POINT('Origin',(116.959178380441,3.7,51.0204257716897));
#189676=CARTESIAN_POINT('Origin',(111.775808773449,3.7,63.0121276118898));
#189677=CARTESIAN_POINT('Origin',(114.210622766164,1.45439216225896E-14,
50.4861580155739));
#189678=CARTESIAN_POINT('Origin',(114.210622766164,1.45439216225896E-14,
50.4861580155739));
#189679=CARTESIAN_POINT('Origin',(112.757435778548,3.2,63.2029375247883));
#189680=CARTESIAN_POINT('',(112.807623831785,3.2,65.5651525940272));
#189681=CARTESIAN_POINT('',(112.748925857912,3.2,65.8671259843151));
#189682=CARTESIAN_POINT('',(112.807623831785,3.2,65.5651525940272));
#189683=CARTESIAN_POINT('',(112.326640075344,3.2,65.4191782301113));
#189684=CARTESIAN_POINT('Origin',(116.959178380441,3.2,51.0204257716897));
#189685=CARTESIAN_POINT('',(112.267744801195,3.2,65.7221666372604));
#189686=CARTESIAN_POINT('',(112.326640075344,3.2,65.4191782301113));
#189687=CARTESIAN_POINT('Origin',(116.959178380441,3.2,51.0204257716897));
#189688=CARTESIAN_POINT('Origin',(113.248249281097,3.2,63.2983424812375));
#189689=CARTESIAN_POINT('',(112.82954913754,3.7,65.4523572371316));
#189690=CARTESIAN_POINT('',(112.770409275048,3.7,65.7566039359465));
#189691=CARTESIAN_POINT('',(112.82954913754,3.7,65.4523572371316));
#189692=CARTESIAN_POINT('Origin',(115.683063273812,1.45439216225896E-14,
50.7723728849216));
#189693=CARTESIAN_POINT('Origin',(115.683063273812,1.45439216225896E-14,
50.7723728849216));
#189694=CARTESIAN_POINT('Origin',(113.248249281097,3.7,63.2983424812375));
#189695=CARTESIAN_POINT('',(112.348641171179,3.7,65.305992969006));
#189696=CARTESIAN_POINT('',(112.289299502814,3.7,65.6112778638504));
#189697=CARTESIAN_POINT('',(112.348641171179,3.7,65.305992969006));
#189698=CARTESIAN_POINT('Origin',(116.959178380441,3.7,51.0204257716897));
#189699=CARTESIAN_POINT('Origin',(116.959178380441,3.7,51.0204257716897));
#189700=CARTESIAN_POINT('Origin',(112.757435778548,3.7,63.2029375247883));
#189701=CARTESIAN_POINT('Origin',(115.192249771263,1.45439216225896E-14,
50.6769679284724));
#189702=CARTESIAN_POINT('Origin',(115.192249771263,1.45439216225896E-14,
50.6769679284724));
#189703=CARTESIAN_POINT('Origin',(113.739062783647,3.2,63.3937474376868));
#189704=CARTESIAN_POINT('',(113.779139125086,3.2,65.8079824948715));
#189705=CARTESIAN_POINT('',(113.72064275009,3.2,66.1089187540186));
#189706=CARTESIAN_POINT('',(113.779139125086,3.2,65.8079824948715));
#189707=CARTESIAN_POINT('',(113.291797521939,3.2,65.6947162535388));
#189708=CARTESIAN_POINT('Origin',(116.959178380441,3.2,51.0204257716897));
#189709=CARTESIAN_POINT('',(113.233232081845,3.2,65.9960078200407));
#189710=CARTESIAN_POINT('',(113.291797521939,3.2,65.6947162535388));
#189711=CARTESIAN_POINT('Origin',(116.959178380441,3.2,51.0204257716897));
#189712=CARTESIAN_POINT('Origin',(114.229876286196,3.2,63.489152394136));
#189713=CARTESIAN_POINT('',(113.800987011728,3.7,65.6955854227966));
#189714=CARTESIAN_POINT('',(113.742053320085,3.7,65.9987714698337));
#189715=CARTESIAN_POINT('',(113.800987011728,3.7,65.6955854227966));
#189716=CARTESIAN_POINT('Origin',(116.664690278911,1.45439216225896E-14,
50.9631827978201));
#189717=CARTESIAN_POINT('Origin',(116.664690278911,1.45439216225896E-14,
50.9631827978201));
#189718=CARTESIAN_POINT('Origin',(114.229876286196,3.7,63.489152394136));
#189719=CARTESIAN_POINT('',(113.31367192882,3.7,65.582182747345));
#189720=CARTESIAN_POINT('',(113.254667609391,3.7,65.8857321410265));
#189721=CARTESIAN_POINT('',(113.31367192882,3.7,65.582182747345));
#189722=CARTESIAN_POINT('Origin',(116.959178380441,3.7,51.0204257716897));
#189723=CARTESIAN_POINT('Origin',(116.959178380441,3.7,51.0204257716897));
#189724=CARTESIAN_POINT('Origin',(113.739062783647,3.7,63.3937474376868));
#189725=CARTESIAN_POINT('Origin',(116.173876776362,1.45439216225896E-14,
50.8677778413709));
#189726=CARTESIAN_POINT('Origin',(116.173876776362,1.45439216225896E-14,
50.8677778413709));
#189727=CARTESIAN_POINT('Origin',(114.720689788746,3.2,63.5845573505853));
#189728=CARTESIAN_POINT('',(114.763290733282,3.2,65.9858045155801));
#189729=CARTESIAN_POINT('',(114.704744153384,3.2,66.2869990552712));
#189730=CARTESIAN_POINT('',(114.763290733282,3.2,65.9858045155801));
#189731=CARTESIAN_POINT('',(114.269637207538,3.2,65.905010138951));
#189732=CARTESIAN_POINT('Origin',(116.959178380441,3.2,51.0204257716897));
#189733=CARTESIAN_POINT('',(114.211147099076,3.2,66.2059141597396));
#189734=CARTESIAN_POINT('',(114.269637207538,3.2,65.905010138951));
#189735=CARTESIAN_POINT('Origin',(116.959178380441,3.2,51.0204257716897));
#189736=CARTESIAN_POINT('Origin',(115.211503291295,3.2,63.6799623070345));
#189737=CARTESIAN_POINT('',(114.785157897793,3.7,65.873308267962));
#189738=CARTESIAN_POINT('',(114.726172865673,3.7,66.1767584375391));
#189739=CARTESIAN_POINT('',(114.785157897793,3.7,65.873308267962));
#189740=CARTESIAN_POINT('Origin',(117.64631728401,1.45439216225896E-14,
51.1539927107186));
#189741=CARTESIAN_POINT('Origin',(117.64631728401,1.45439216225896E-14,
51.1539927107186));
#189742=CARTESIAN_POINT('Origin',(115.211503291295,3.7,63.6799623070345));
#189743=CARTESIAN_POINT('',(114.291482688029,3.7,65.792625445389));
#189744=CARTESIAN_POINT('',(114.232555404523,3.7,66.0957785255825));
#189745=CARTESIAN_POINT('',(114.291482688029,3.7,65.792625445389));
#189746=CARTESIAN_POINT('Origin',(116.959178380441,3.7,51.0204257716897));
#189747=CARTESIAN_POINT('Origin',(116.959178380441,3.7,51.0204257716897));
#189748=CARTESIAN_POINT('Origin',(114.720689788746,3.7,63.5845573505853));
#189749=CARTESIAN_POINT('Origin',(117.155503781461,1.45439216225896E-14,
51.0585877542694));
#189750=CARTESIAN_POINT('Origin',(117.155503781461,1.45439216225896E-14,
51.0585877542694));
#189751=CARTESIAN_POINT('Origin',(115.702316793845,3.2,63.7753672634838));
#189752=CARTESIAN_POINT('',(115.760112028091,3.2,66.0984469744097));
#189753=CARTESIAN_POINT('',(115.701261479518,3.2,66.401205289563));
#189754=CARTESIAN_POINT('',(115.760112028091,3.2,66.0984469744097));
#189755=CARTESIAN_POINT('',(115.260109046897,3.2,66.0503175513039));
#189756=CARTESIAN_POINT('Origin',(116.959178380441,3.2,51.0204257716897));
#189757=CARTESIAN_POINT('',(115.201442710298,3.2,66.3521281827397));
#189758=CARTESIAN_POINT('',(115.260109046897,3.2,66.0503175513039));
#189759=CARTESIAN_POINT('Origin',(116.959178380441,3.2,51.0204257716897));
#189760=CARTESIAN_POINT('Origin',(116.193130296394,3.2,63.870772219933));
#189761=CARTESIAN_POINT('',(115.782095941346,3.7,65.985350109572));
#189762=CARTESIAN_POINT('',(115.722800022625,3.7,66.2903996440776));
#189763=CARTESIAN_POINT('',(115.782095941346,3.7,65.985350109572));
#189764=CARTESIAN_POINT('Origin',(118.62794428911,1.45439216225896E-14,
51.3448026236171));
#189765=CARTESIAN_POINT('Origin',(118.62794428911,1.45439216225896E-14,
51.3448026236171));
#189766=CARTESIAN_POINT('Origin',(116.193130296394,3.7,63.870772219933));
#189767=CARTESIAN_POINT('',(115.282022201653,3.7,65.9375847055742));
#189768=CARTESIAN_POINT('',(115.222914696043,3.7,66.2416649434879));
#189769=CARTESIAN_POINT('',(115.282022201653,3.7,65.9375847055742));
#189770=CARTESIAN_POINT('Origin',(116.959178380441,3.7,51.0204257716897));
#189771=CARTESIAN_POINT('Origin',(116.959178380441,3.7,51.0204257716897));
#189772=CARTESIAN_POINT('Origin',(115.702316793845,3.7,63.7753672634838));
#189773=CARTESIAN_POINT('Origin',(118.13713078656,1.45439216225896E-14,
51.2493976671679));
#189774=CARTESIAN_POINT('Origin',(118.13713078656,1.45439216225896E-14,
51.2493976671679));
#189775=CARTESIAN_POINT('Origin',(116.683943798944,3.2,63.9661771763823));
#189776=CARTESIAN_POINT('',(116.76980637141,3.2,66.1448636703097));
#189777=CARTESIAN_POINT('',(116.710386028075,3.2,66.4505533107689));
#189778=CARTESIAN_POINT('',(116.76980637141,3.2,66.1448636703097));
#189779=CARTESIAN_POINT('',(116.263330423862,3.2,66.1300346060814));
#189780=CARTESIAN_POINT('Origin',(116.959178380441,3.2,51.0204257716897));
#189781=CARTESIAN_POINT('',(116.204229383259,3.2,66.4340815845874));
#189782=CARTESIAN_POINT('',(116.263330423862,3.2,66.1300346060814));
#189783=CARTESIAN_POINT('Origin',(116.959178380441,3.2,51.0204257716897));
#189784=CARTESIAN_POINT('Origin',(117.174757301493,3.2,64.0615821328315));
#189785=CARTESIAN_POINT('',(116.792009270423,3.7,66.0306402270355));
#189786=CARTESIAN_POINT('',(116.732130391513,3.7,66.3386888167544));
#189787=CARTESIAN_POINT('',(116.792009270423,3.7,66.0306402270355));
#189788=CARTESIAN_POINT('Origin',(119.609571294209,1.45439216225896E-14,
51.5356125365156));
#189789=CARTESIAN_POINT('Origin',(119.609571294209,1.45439216225896E-14,
51.5356125365156));
#189790=CARTESIAN_POINT('Origin',(117.174757301493,3.7,64.0615821328315));
#189791=CARTESIAN_POINT('',(116.285410584927,3.7,66.0164425916591));
#189792=CARTESIAN_POINT('',(116.225858418278,3.7,66.3228104008948));
#189793=CARTESIAN_POINT('',(116.285410584927,3.7,66.0164425916591));
#189794=CARTESIAN_POINT('Origin',(116.959178380441,3.7,51.0204257716897));
#189795=CARTESIAN_POINT('Origin',(116.959178380441,3.7,51.0204257716897));
#189796=CARTESIAN_POINT('Origin',(116.683943798944,3.7,63.9661771763823));
#189797=CARTESIAN_POINT('Origin',(119.118757791659,1.45439216225896E-14,
51.4402075800664));
#189798=CARTESIAN_POINT('Origin',(119.118757791659,1.45439216225896E-14,
51.4402075800664));
#189799=CARTESIAN_POINT('Origin',(117.665570804043,3.2,64.1569870892808));
#189800=CARTESIAN_POINT('',(117.792761072847,3.2,66.1230620780361));
#189801=CARTESIAN_POINT('',(117.732481576534,3.2,66.4331716553377));
#189802=CARTESIAN_POINT('',(117.792761072847,3.2,66.1230620780361));
#189803=CARTESIAN_POINT('',(117.279594132899,3.2,66.1426550138522));
#189804=CARTESIAN_POINT('Origin',(116.959178380441,3.2,51.0204257716897));
#189805=CARTESIAN_POINT('',(117.219782366722,3.2,66.450358340214));
#189806=CARTESIAN_POINT('',(117.279594132899,3.2,66.1426550138522));
#189807=CARTESIAN_POINT('Origin',(116.959178380441,3.2,51.0204257716897));
#189808=CARTESIAN_POINT('Origin',(118.156384306592,3.2,64.25239204573));
#189809=CARTESIAN_POINT('',(117.815294509265,3.7,66.0071381757101));
#189810=CARTESIAN_POINT('',(117.754536133629,3.7,66.3197113612616));
#189811=CARTESIAN_POINT('',(117.815294509265,3.7,66.0071381757101));
#189812=CARTESIAN_POINT('Origin',(120.591198299308,1.45439216225896E-14,
51.7264224494141));
#189813=CARTESIAN_POINT('Origin',(120.591198299308,1.45439216225896E-14,
51.7264224494141));
#189814=CARTESIAN_POINT('Origin',(118.156384306592,3.7,64.25239204573));
#189815=CARTESIAN_POINT('',(117.301947570297,3.7,66.0276571215869));
#189816=CARTESIAN_POINT('',(117.241668073985,3.7,66.3377666988885));
#189817=CARTESIAN_POINT('',(117.301947570297,3.7,66.0276571215869));
#189818=CARTESIAN_POINT('Origin',(116.959178380441,3.7,51.0204257716897));
#189819=CARTESIAN_POINT('Origin',(116.959178380441,3.7,51.0204257716897));
#189820=CARTESIAN_POINT('Origin',(117.665570804043,3.7,64.1569870892808));
#189821=CARTESIAN_POINT('Origin',(120.100384796758,1.45439216225896E-14,
51.6310174929649));
#189822=CARTESIAN_POINT('Origin',(120.100384796758,1.45439216225896E-14,
51.6310174929649));
#189823=CARTESIAN_POINT('Origin',(117.665570804043,2.2,64.1569870892808));
#189824=CARTESIAN_POINT('',(117.757851092575,2.2,66.3026574610069));
#189825=CARTESIAN_POINT('',(117.698298925926,2.2,66.6090252702425));
#189826=CARTESIAN_POINT('',(117.757851092575,2.2,66.3026574610069));
#189827=CARTESIAN_POINT('',(117.244957428961,2.2,66.3208445189799));
#189828=CARTESIAN_POINT('Origin',(116.959178380441,2.2,51.0204257716897));
#189829=CARTESIAN_POINT('',(117.185856388358,2.2,66.6248914974859));
#189830=CARTESIAN_POINT('',(117.244957428961,2.2,66.3208445189799));
#189831=CARTESIAN_POINT('Origin',(116.959178380441,2.2,51.0204257716897));
#189832=CARTESIAN_POINT('Origin',(118.156384306592,2.2,64.25239204573));
#189833=CARTESIAN_POINT('',(117.773636275522,2.7,66.221450139934));
#189834=CARTESIAN_POINT('',(117.713757396612,2.7,66.5294987296529));
#189835=CARTESIAN_POINT('',(117.773636275522,2.7,66.221450139934));
#189836=CARTESIAN_POINT('Origin',(120.591198299308,1.45439216225896E-14,
51.7264224494141));
#189837=CARTESIAN_POINT('Origin',(120.591198299308,1.45439216225896E-14,
51.7264224494141));
#189838=CARTESIAN_POINT('Origin',(118.156384306592,2.7,64.25239204573));
#189839=CARTESIAN_POINT('',(117.26061987396,2.7,66.2402686267589));
#189840=CARTESIAN_POINT('',(117.201199530625,2.7,66.5459582672182));
#189841=CARTESIAN_POINT('',(117.26061987396,2.7,66.2402686267589));
#189842=CARTESIAN_POINT('Origin',(116.959178380441,2.7,51.0204257716897));
#189843=CARTESIAN_POINT('Origin',(116.959178380441,2.7,51.0204257716897));
#189844=CARTESIAN_POINT('Origin',(117.665570804043,2.7,64.1569870892808));
#189845=CARTESIAN_POINT('Origin',(120.100384796758,1.45439216225896E-14,
51.6310174929649));
#189846=CARTESIAN_POINT('Origin',(120.100384796758,1.45439216225896E-14,
51.6310174929649));
#189847=CARTESIAN_POINT('Origin',(117.665570804043,1.2,64.1569870892808));
#189848=CARTESIAN_POINT('',(117.7360897144,1.2,66.4146094878205));
#189849=CARTESIAN_POINT('',(117.67698220879,1.2,66.7186897257342));
#189850=CARTESIAN_POINT('',(117.7360897144,1.2,66.4146094878205));
#189851=CARTESIAN_POINT('',(117.223363057096,1.2,66.4319373771009));
#189852=CARTESIAN_POINT('Origin',(116.959178380441,1.2,51.0204257716897));
#189853=CARTESIAN_POINT('',(117.164696720496,1.2,66.7337480085367));
#189854=CARTESIAN_POINT('',(117.223363057096,1.2,66.4319373771009));
#189855=CARTESIAN_POINT('Origin',(116.959178380441,1.2,51.0204257716897));
#189856=CARTESIAN_POINT('Origin',(118.156384306592,1.2,64.25239204573));
#189857=CARTESIAN_POINT('',(117.745349951544,1.7,66.366969935369));
#189858=CARTESIAN_POINT('',(117.686054032823,1.7,66.6720194698746));
#189859=CARTESIAN_POINT('',(117.745349951544,1.7,66.366969935369));
#189860=CARTESIAN_POINT('Origin',(120.591198299308,1.45439216225896E-14,
51.7264224494141));
#189861=CARTESIAN_POINT('Origin',(120.591198299308,1.45439216225896E-14,
51.7264224494141));
#189862=CARTESIAN_POINT('Origin',(118.156384306592,1.7,64.25239204573));
#189863=CARTESIAN_POINT('',(117.232552535739,1.7,66.3846618437574));
#189864=CARTESIAN_POINT('',(117.173701987167,1.7,66.6874201589108));
#189865=CARTESIAN_POINT('',(117.232552535739,1.7,66.3846618437574));
#189866=CARTESIAN_POINT('Origin',(116.959178380441,1.7,51.0204257716897));
#189867=CARTESIAN_POINT('Origin',(116.959178380441,1.7,51.0204257716897));
#189868=CARTESIAN_POINT('Origin',(117.665570804043,1.7,64.1569870892808));
#189869=CARTESIAN_POINT('Origin',(120.100384796758,1.45439216225896E-14,
51.6310174929649));
#189870=CARTESIAN_POINT('Origin',(120.100384796758,1.45439216225896E-14,
51.6310174929649));
#189871=CARTESIAN_POINT('Origin',(117.665570804043,0.200000000000015,64.1569870892808));
#189872=CARTESIAN_POINT('',(117.727177205876,0.200000000000015,66.4604601405338));
#189873=CARTESIAN_POINT('',(117.668249922372,0.200000000000015,66.7636132207175));
#189874=CARTESIAN_POINT('',(117.727177205876,0.200000000000015,66.4604601405338));
#189875=CARTESIAN_POINT('',(117.214518222835,0.200000000000015,66.4774398776465));
#189876=CARTESIAN_POINT('Origin',(116.959178380441,0.200000000000015,51.0204257716897));
#189877=CARTESIAN_POINT('',(117.156028114373,0.200000000000015,66.7783438984351));
#189878=CARTESIAN_POINT('',(117.214518222835,0.200000000000015,66.4774398776465));
#189879=CARTESIAN_POINT('Origin',(116.959178380441,0.200000000000015,51.0204257716897));
#189880=CARTESIAN_POINT('Origin',(118.156384306592,0.200000000000015,64.25239204573));
#189881=CARTESIAN_POINT('',(117.73003891309,0.700000000000015,66.4457380066575));
#189882=CARTESIAN_POINT('',(117.67105388097,0.700000000000015,66.7491881762347));
#189883=CARTESIAN_POINT('',(117.73003891309,0.700000000000015,66.4457380066575));
#189884=CARTESIAN_POINT('Origin',(120.591198299308,1.45439216225896E-14,
51.7264224494141));
#189885=CARTESIAN_POINT('Origin',(120.591198299308,1.45439216225896E-14,
51.7264224494141));
#189886=CARTESIAN_POINT('Origin',(118.156384306592,0.700000000000015,64.25239204573));
#189887=CARTESIAN_POINT('',(117.217358246029,0.700000000000015,66.4628292978264));
#189888=CARTESIAN_POINT('',(117.158811666132,0.700000000000015,66.7640238375175));
#189889=CARTESIAN_POINT('',(117.217358246029,0.700000000000015,66.4628292978264));
#189890=CARTESIAN_POINT('Origin',(116.959178380441,0.700000000000015,51.0204257716897));
#189891=CARTESIAN_POINT('Origin',(116.959178380441,0.700000000000015,51.0204257716897));
#189892=CARTESIAN_POINT('Origin',(117.665570804043,0.700000000000015,64.1569870892808));
#189893=CARTESIAN_POINT('Origin',(120.100384796758,1.45439216225896E-14,
51.6310174929649));
#189894=CARTESIAN_POINT('Origin',(120.100384796758,1.45439216225896E-14,
51.6310174929649));
#189895=CARTESIAN_POINT('Origin',(112.757435778548,0.200000000000015,63.2029375247883));
#189896=CARTESIAN_POINT('',(112.743757590842,0.200000000000015,65.8937142807404));
#189897=CARTESIAN_POINT('',(112.686310316266,0.200000000000015,66.1892534130432));
#189898=CARTESIAN_POINT('',(112.743757590842,0.200000000000015,65.8937142807404));
#189899=CARTESIAN_POINT('',(112.262559541475,0.200000000000015,65.7488423528614));
#189900=CARTESIAN_POINT('Origin',(116.959178380441,0.200000000000015,51.0204257716897));
#189901=CARTESIAN_POINT('',(112.204927352587,0.200000000000015,66.0453327820839));
#189902=CARTESIAN_POINT('',(112.262559541475,0.200000000000015,65.7488423528614));
#189903=CARTESIAN_POINT('Origin',(116.959178380441,0.200000000000015,51.0204257716897));
#189904=CARTESIAN_POINT('Origin',(113.248249281097,0.200000000000015,63.2983424812375));
#189905=CARTESIAN_POINT('',(112.746545930485,0.700000000000015,65.8793695884159));
#189906=CARTESIAN_POINT('',(112.689045154583,0.700000000000015,66.1751839598116));
#189907=CARTESIAN_POINT('',(112.746545930485,0.700000000000015,65.8793695884159));
#189908=CARTESIAN_POINT('Origin',(115.683063273812,1.45439216225896E-14,
50.7723728849216));
#189909=CARTESIAN_POINT('Origin',(115.683063273812,1.45439216225896E-14,
50.7723728849216));
#189910=CARTESIAN_POINT('Origin',(113.248249281097,0.700000000000015,63.2983424812375));
#189911=CARTESIAN_POINT('',(112.265357041383,0.700000000000015,65.7344505352944));
#189912=CARTESIAN_POINT('',(112.20767083231,0.700000000000015,66.0312188728892));
#189913=CARTESIAN_POINT('',(112.265357041383,0.700000000000015,65.7344505352944));
#189914=CARTESIAN_POINT('Origin',(116.959178380441,0.700000000000015,51.0204257716897));
#189915=CARTESIAN_POINT('Origin',(116.959178380441,0.700000000000015,51.0204257716897));
#189916=CARTESIAN_POINT('Origin',(112.757435778548,0.700000000000015,63.2029375247883));
#189917=CARTESIAN_POINT('Origin',(115.192249771263,1.45439216225896E-14,
50.6769679284724));
#189918=CARTESIAN_POINT('Origin',(115.192249771263,1.45439216225896E-14,
50.6769679284724));
#189919=CARTESIAN_POINT('Origin',(112.757435778548,1.2,63.2029375247883));
#189920=CARTESIAN_POINT('',(112.752441137483,1.2,65.8490415289272));
#189921=CARTESIAN_POINT('',(112.694826921622,1.2,66.1454394954038));
#189922=CARTESIAN_POINT('',(112.752441137483,1.2,65.8490415289272));
#189923=CARTESIAN_POINT('',(112.271271673005,1.2,65.7040225452736));
#189924=CARTESIAN_POINT('Origin',(116.959178380441,1.2,51.0204257716897));
#189925=CARTESIAN_POINT('',(112.213470920606,1.2,66.0013801542565));
#189926=CARTESIAN_POINT('',(112.271271673005,1.2,65.7040225452736));
#189927=CARTESIAN_POINT('Origin',(116.959178380441,1.2,51.0204257716897));
#189928=CARTESIAN_POINT('Origin',(113.248249281097,1.2,63.2983424812375));
#189929=CARTESIAN_POINT('',(112.761462018886,1.7,65.8026333488664));
#189930=CARTESIAN_POINT('',(112.703673355823,1.7,66.0999287639157));
#189931=CARTESIAN_POINT('',(112.761462018886,1.7,65.8026333488664));
#189932=CARTESIAN_POINT('Origin',(115.683063273812,1.45439216225896E-14,
50.7723728849216));
#189933=CARTESIAN_POINT('Origin',(115.683063273812,1.45439216225896E-14,
50.7723728849216));
#189934=CARTESIAN_POINT('Origin',(113.248249281097,1.7,63.2983424812375));
#189935=CARTESIAN_POINT('',(112.28032243059,1.7,65.657460666346));
#189936=CARTESIAN_POINT('',(112.222345525672,1.7,65.9557244969574));
#189937=CARTESIAN_POINT('',(112.28032243059,1.7,65.657460666346));
#189938=CARTESIAN_POINT('Origin',(116.959178380441,1.7,51.0204257716897));
#189939=CARTESIAN_POINT('Origin',(116.959178380441,1.7,51.0204257716897));
#189940=CARTESIAN_POINT('Origin',(112.757435778548,1.7,63.2029375247883));
#189941=CARTESIAN_POINT('Origin',(115.192249771263,1.45439216225896E-14,
50.6769679284724));
#189942=CARTESIAN_POINT('Origin',(115.192249771263,1.45439216225896E-14,
50.6769679284724));
#189943=CARTESIAN_POINT('Origin',(112.757435778548,2.2,63.2029375247883));
#189944=CARTESIAN_POINT('',(112.773637648674,2.2,65.7399954763229));
#189945=CARTESIAN_POINT('',(112.715611865814,2.2,66.0385107608908));
#189946=CARTESIAN_POINT('',(112.773637648674,2.2,65.7399954763229));
#189947=CARTESIAN_POINT('',(112.292538680002,2.2,65.5946138249966));
#189948=CARTESIAN_POINT('Origin',(116.959178380441,2.2,51.0204257716897));
#189949=CARTESIAN_POINT('',(112.234322320598,2.2,65.8941095360005));
#189950=CARTESIAN_POINT('',(112.292538680002,2.2,65.5946138249966));
#189951=CARTESIAN_POINT('Origin',(116.959178380441,2.2,51.0204257716897));
#189952=CARTESIAN_POINT('Origin',(113.248249281097,2.2,63.2983424812375));
#189953=CARTESIAN_POINT('',(112.78900784376,2.7,65.6609230720582));
#189954=CARTESIAN_POINT('',(112.730679961499,2.7,65.9609925155598));
#189955=CARTESIAN_POINT('',(112.78900784376,2.7,65.6609230720582));
#189956=CARTESIAN_POINT('Origin',(115.683063273812,1.45439216225896E-14,
50.7723728849216));
#189957=CARTESIAN_POINT('Origin',(115.683063273812,1.45439216225896E-14,
50.7723728849216));
#189958=CARTESIAN_POINT('Origin',(113.248249281097,2.7,63.2983424812375));
#189959=CARTESIAN_POINT('',(112.307960642765,2.7,65.5152751004566));
#189960=CARTESIAN_POINT('',(112.249439181471,2.7,65.816340416776));
#189961=CARTESIAN_POINT('',(112.307960642765,2.7,65.5152751004566));
#189962=CARTESIAN_POINT('Origin',(116.959178380441,2.7,51.0204257716897));
#189963=CARTESIAN_POINT('Origin',(116.959178380441,2.7,51.0204257716897));
#189964=CARTESIAN_POINT('Origin',(112.757435778548,2.7,63.2029375247883));
#189965=CARTESIAN_POINT('Origin',(115.192249771263,1.45439216225896E-14,
50.6769679284724));
#189966=CARTESIAN_POINT('Origin',(115.192249771263,1.45439216225896E-14,
50.6769679284724));
#189967=CARTESIAN_POINT('Origin',(113.739062783647,2.2,63.3937474376868));
#189968=CARTESIAN_POINT('',(113.745270654261,2.2,65.9822198029767));
#189969=CARTESIAN_POINT('',(113.687439645288,2.2,66.2797330677587));
#189970=CARTESIAN_POINT('',(113.745270654261,2.2,65.9822198029767));
#189971=CARTESIAN_POINT('',(113.257888725595,2.2,65.8691610174192));
#189972=CARTESIAN_POINT('Origin',(116.959178380441,2.2,51.0204257716897));
#189973=CARTESIAN_POINT('',(113.199990984535,2.2,66.1670175873205));
#189974=CARTESIAN_POINT('',(113.257888725595,2.2,65.8691610174192));
#189975=CARTESIAN_POINT('Origin',(116.959178380441,2.2,51.0204257716897));
#189976=CARTESIAN_POINT('Origin',(114.229876286196,2.2,63.489152394136));
#189977=CARTESIAN_POINT('',(113.760587954822,2.7,65.9034195160936));
#189978=CARTESIAN_POINT('',(113.702457894475,2.7,66.2024712591523));
#189979=CARTESIAN_POINT('',(113.760587954822,2.7,65.9034195160936));
#189980=CARTESIAN_POINT('Origin',(116.664690278911,1.45439216225896E-14,
50.9631827978201));
#189981=CARTESIAN_POINT('Origin',(116.664690278911,1.45439216225896E-14,
50.9631827978201));
#189982=CARTESIAN_POINT('Origin',(114.229876286196,2.7,63.489152394136));
#189983=CARTESIAN_POINT('',(113.273224147002,2.7,65.7902675073336));
#189984=CARTESIAN_POINT('',(113.215026312613,2.7,66.0896679158723));
#189985=CARTESIAN_POINT('',(113.273224147002,2.7,65.7902675073336));
#189986=CARTESIAN_POINT('Origin',(116.959178380441,2.7,51.0204257716897));
#189987=CARTESIAN_POINT('Origin',(116.959178380441,2.7,51.0204257716897));
#189988=CARTESIAN_POINT('Origin',(113.739062783647,2.7,63.3937474376868));
#189989=CARTESIAN_POINT('Origin',(116.173876776362,1.45439216225896E-14,
50.8677778413709));
#189990=CARTESIAN_POINT('Origin',(116.173876776362,1.45439216225896E-14,
50.8677778413709));
#189991=CARTESIAN_POINT('Origin',(114.720689788746,2.2,63.5845573505853));
#189992=CARTESIAN_POINT('',(114.729392949091,2.2,66.1601926271255));
#189993=CARTESIAN_POINT('',(114.671513430601,2.2,66.4579554504992));
#189994=CARTESIAN_POINT('',(114.729392949091,2.2,66.1601926271255));
#189995=CARTESIAN_POINT('',(114.235772395539,2.2,66.0792286241228));
#189996=CARTESIAN_POINT('Origin',(116.959178380441,2.2,51.0204257716897));
#189997=CARTESIAN_POINT('',(114.177947441683,2.2,66.3767107381891));
#189998=CARTESIAN_POINT('',(114.235772395539,2.2,66.0792286241228));
#189999=CARTESIAN_POINT('Origin',(116.959178380441,2.2,51.0204257716897));
#190000=CARTESIAN_POINT('Origin',(115.211503291295,2.2,63.6799623070345));
#190001=CARTESIAN_POINT('',(114.744723422072,2.7,66.0813245743583));
#190002=CARTESIAN_POINT('',(114.686544095021,2.7,66.3806297713697));
#190003=CARTESIAN_POINT('',(114.744723422072,2.7,66.0813245743583));
#190004=CARTESIAN_POINT('Origin',(117.64631728401,1.45439216225896E-14,
51.1539927107186));
#190005=CARTESIAN_POINT('Origin',(117.64631728401,1.45439216225896E-14,
51.1539927107186));
#190006=CARTESIAN_POINT('Origin',(115.211503291295,2.7,63.6799623070345));
#190007=CARTESIAN_POINT('',(114.251088051933,2.7,66.0004367957037));
#190008=CARTESIAN_POINT('',(114.192964141128,2.7,66.2994569022688));
#190009=CARTESIAN_POINT('',(114.251088051933,2.7,66.0004367957037));
#190010=CARTESIAN_POINT('Origin',(116.959178380441,2.7,51.0204257716897));
#190011=CARTESIAN_POINT('Origin',(116.959178380441,2.7,51.0204257716897));
#190012=CARTESIAN_POINT('Origin',(114.720689788746,2.7,63.5845573505853));
#190013=CARTESIAN_POINT('Origin',(117.155503781461,1.45439216225896E-14,
51.0585877542694));
#190014=CARTESIAN_POINT('Origin',(117.155503781461,1.45439216225896E-14,
51.0585877542694));
#190015=CARTESIAN_POINT('Origin',(115.702316793845,2.2,63.7753672634838));
#190016=CARTESIAN_POINT('',(115.726036750819,2.2,66.2737482041414));
#190017=CARTESIAN_POINT('',(115.66786358896,2.2,66.5730216841463));
#190018=CARTESIAN_POINT('',(115.726036750819,2.2,66.2737482041414));
#190019=CARTESIAN_POINT('',(115.22614133726,2.2,66.2250653962915));
#190020=CARTESIAN_POINT('Origin',(116.959178380441,2.2,51.0204257716897));
#190021=CARTESIAN_POINT('',(115.168146117596,2.2,66.5234234476348));
#190022=CARTESIAN_POINT('',(115.22614133726,2.2,66.2250653962915));
#190023=CARTESIAN_POINT('Origin',(116.959178380441,2.2,51.0204257716897));
#190024=CARTESIAN_POINT('Origin',(116.193130296394,2.2,63.870772219933));
#190025=CARTESIAN_POINT('',(115.741446978392,2.7,66.1944698516157));
#190026=CARTESIAN_POINT('',(115.682969396959,2.7,66.4953094267459));
#190027=CARTESIAN_POINT('',(115.741446978392,2.7,66.1944698516157));
#190028=CARTESIAN_POINT('Origin',(118.62794428911,1.45439216225896E-14,
51.3448026236171));
#190029=CARTESIAN_POINT('Origin',(118.62794428911,1.45439216225896E-14,
51.3448026236171));
#190030=CARTESIAN_POINT('Origin',(116.193130296394,2.7,63.870772219933));
#190031=CARTESIAN_POINT('',(115.241503231448,2.7,66.1460356962372));
#190032=CARTESIAN_POINT('',(115.183206392039,2.7,66.4459454389002));
#190033=CARTESIAN_POINT('',(115.241503231448,2.7,66.1460356962372));
#190034=CARTESIAN_POINT('Origin',(116.959178380441,2.7,51.0204257716897));
#190035=CARTESIAN_POINT('Origin',(116.959178380441,2.7,51.0204257716897));
#190036=CARTESIAN_POINT('Origin',(115.702316793845,2.7,63.7753672634838));
#190037=CARTESIAN_POINT('Origin',(118.13713078656,1.45439216225896E-14,
51.2493976671679));
#190038=CARTESIAN_POINT('Origin',(118.13713078656,1.45439216225896E-14,
51.2493976671679));
#190039=CARTESIAN_POINT('Origin',(116.683943798944,2.2,63.9661771763823));
#190040=CARTESIAN_POINT('',(116.735398317472,2.2,66.321876879036));
#190041=CARTESIAN_POINT('',(116.676674996893,2.2,66.6239806661718));
#190042=CARTESIAN_POINT('',(116.735398317472,2.2,66.321876879036));
#190043=CARTESIAN_POINT('',(116.229108862081,2.2,66.306088400618));
#190044=CARTESIAN_POINT('Origin',(116.959178380441,2.2,51.0204257716897));
#190045=CARTESIAN_POINT('',(116.170693795267,2.2,66.6066063675209));
#190046=CARTESIAN_POINT('',(116.229108862081,2.2,66.306088400618));
#190047=CARTESIAN_POINT('Origin',(116.959178380441,2.2,51.0204257716897));
#190048=CARTESIAN_POINT('Origin',(117.174757301493,2.2,64.0615821328315));
#190049=CARTESIAN_POINT('',(116.750958052759,2.7,66.2418293798362));
#190050=CARTESIAN_POINT('',(116.691921545728,2.7,66.5455443635489));
#190051=CARTESIAN_POINT('',(116.750958052759,2.7,66.2418293798362));
#190052=CARTESIAN_POINT('Origin',(119.609571294209,1.45439216225896E-14,
51.5356125365156));
#190053=CARTESIAN_POINT('Origin',(119.609571294209,1.45439216225896E-14,
51.5356125365156));
#190054=CARTESIAN_POINT('Origin',(117.174757301493,2.7,64.0615821328315));
#190055=CARTESIAN_POINT('',(116.244584814922,2.7,66.2264719225867));
#190056=CARTESIAN_POINT('',(116.185861494343,2.7,66.5285757097225));
#190057=CARTESIAN_POINT('',(116.244584814922,2.7,66.2264719225867));
#190058=CARTESIAN_POINT('Origin',(116.959178380441,2.7,51.0204257716897));
#190059=CARTESIAN_POINT('Origin',(116.959178380441,2.7,51.0204257716897));
#190060=CARTESIAN_POINT('Origin',(116.683943798944,2.7,63.9661771763823));
#190061=CARTESIAN_POINT('Origin',(119.118757791659,1.45439216225896E-14,
51.4402075800664));
#190062=CARTESIAN_POINT('Origin',(119.118757791659,1.45439216225896E-14,
51.4402075800664));
#190063=CARTESIAN_POINT('Origin',(116.683943798944,1.2,63.9661771763823));
#190064=CARTESIAN_POINT('',(116.713943739096,1.2,66.432250565585));
#190065=CARTESIAN_POINT('',(116.655646899688,1.2,66.732160308248));
#190066=CARTESIAN_POINT('',(116.713943739096,1.2,66.432250565585));
#190067=CARTESIAN_POINT('',(116.207768342359,1.2,66.41587530919));
#190068=CARTESIAN_POINT('Origin',(116.959178380441,1.2,51.0204257716897));
#190069=CARTESIAN_POINT('',(116.149773122695,1.2,66.7142333605333));
#190070=CARTESIAN_POINT('',(116.207768342359,1.2,66.41587530919));
#190071=CARTESIAN_POINT('Origin',(116.959178380441,1.2,51.0204257716897));
#190072=CARTESIAN_POINT('Origin',(117.174757301493,1.2,64.0615821328315));
#190073=CARTESIAN_POINT('',(116.723073983491,1.7,66.3852797645142));
#190074=CARTESIAN_POINT('',(116.664596402058,1.7,66.6861193396444));
#190075=CARTESIAN_POINT('',(116.723073983491,1.7,66.3852797645142));
#190076=CARTESIAN_POINT('Origin',(119.609571294209,1.45439216225896E-14,
51.5356125365156));
#190077=CARTESIAN_POINT('Origin',(119.609571294209,1.45439216225896E-14,
51.5356125365156));
#190078=CARTESIAN_POINT('Origin',(117.174757301493,1.7,64.0615821328315));
#190079=CARTESIAN_POINT('',(116.216850253369,1.7,66.3691531605907));
#190080=CARTESIAN_POINT('',(116.15867709151,1.7,66.6684266405955));
#190081=CARTESIAN_POINT('',(116.216850253369,1.7,66.3691531605907));
#190082=CARTESIAN_POINT('Origin',(116.959178380441,1.7,51.0204257716897));
#190083=CARTESIAN_POINT('Origin',(116.959178380441,1.7,51.0204257716897));
#190084=CARTESIAN_POINT('Origin',(116.683943798944,1.7,63.9661771763823));
#190085=CARTESIAN_POINT('Origin',(119.118757791659,1.45439216225896E-14,
51.4402075800664));
#190086=CARTESIAN_POINT('Origin',(119.118757791659,1.45439216225896E-14,
51.4402075800664));
#190087=CARTESIAN_POINT('Origin',(116.683943798944,0.200000000000015,63.9661771763823));
#190088=CARTESIAN_POINT('',(116.705155564681,0.200000000000015,66.47746157795));
#190089=CARTESIAN_POINT('',(116.647031653875,0.200000000000015,66.7764816845151));
#190090=CARTESIAN_POINT('',(116.705155564681,0.200000000000015,66.47746157795));
#190091=CARTESIAN_POINT('',(116.199026405737,0.200000000000015,66.4608484499199));
#190092=CARTESIAN_POINT('Origin',(116.959178380441,0.200000000000015,51.0204257716897));
#190093=CARTESIAN_POINT('',(116.141201451881,0.200000000000015,66.7583305639861));
#190094=CARTESIAN_POINT('',(116.199026405737,0.200000000000015,66.4608484499199));
#190095=CARTESIAN_POINT('Origin',(116.959178380441,0.200000000000015,51.0204257716897));
#190096=CARTESIAN_POINT('Origin',(117.174757301493,0.200000000000015,64.0615821328315));
#190097=CARTESIAN_POINT('',(116.70797743227,0.700000000000015,66.4629444001553));
#190098=CARTESIAN_POINT('',(116.649798105219,0.700000000000015,66.7622495971667));
#190099=CARTESIAN_POINT('',(116.70797743227,0.700000000000015,66.4629444001553));
#190100=CARTESIAN_POINT('Origin',(119.609571294209,1.45439216225896E-14,
51.5356125365156));
#190101=CARTESIAN_POINT('Origin',(119.609571294209,1.45439216225896E-14,
51.5356125365156));
#190102=CARTESIAN_POINT('Origin',(117.174757301493,0.700000000000015,64.0615821328315));
#190103=CARTESIAN_POINT('',(116.20183345674,0.700000000000015,66.4464074964732));
#190104=CARTESIAN_POINT('',(116.143953938249,0.700000000000015,66.744170319847));
#190105=CARTESIAN_POINT('',(116.20183345674,0.700000000000015,66.4464074964732));
#190106=CARTESIAN_POINT('Origin',(116.959178380441,0.700000000000015,51.0204257716897));
#190107=CARTESIAN_POINT('Origin',(116.959178380441,0.700000000000015,51.0204257716897));
#190108=CARTESIAN_POINT('Origin',(116.683943798944,0.700000000000015,63.9661771763823));
#190109=CARTESIAN_POINT('Origin',(119.118757791659,1.45439216225896E-14,
51.4402075800664));
#190110=CARTESIAN_POINT('Origin',(119.118757791659,1.45439216225896E-14,
51.4402075800664));
#190111=CARTESIAN_POINT('Origin',(113.739062783647,0.200000000000015,63.3937474376868));
#190112=CARTESIAN_POINT('',(113.715491849759,0.200000000000015,66.1354177067687));
#190113=CARTESIAN_POINT('',(113.658233599506,0.200000000000015,66.4299843980828));
#190114=CARTESIAN_POINT('',(113.715491849759,0.200000000000015,66.1354177067687));
#190115=CARTESIAN_POINT('',(113.22807523146,0.200000000000015,66.022537383013));
#190116=CARTESIAN_POINT('Origin',(116.959178380441,0.200000000000015,51.0204257716897));
#190117=CARTESIAN_POINT('',(113.170752214749,0.200000000000015,66.317437267206));
#190118=CARTESIAN_POINT('',(113.22807523146,0.200000000000015,66.022537383013));
#190119=CARTESIAN_POINT('Origin',(116.959178380441,0.200000000000015,51.0204257716897));
#190120=CARTESIAN_POINT('Origin',(114.229876286196,0.200000000000015,63.489152394136));
#190121=CARTESIAN_POINT('',(113.718270827401,0.700000000000015,66.1211211775216));
#190122=CARTESIAN_POINT('',(113.66095960276,0.700000000000015,66.4159603970774));
#190123=CARTESIAN_POINT('',(113.718270827401,0.700000000000015,66.1211211775216));
#190124=CARTESIAN_POINT('Origin',(116.664690278911,1.45439216225896E-14,
50.9631827978201));
#190125=CARTESIAN_POINT('Origin',(116.664690278911,1.45439216225896E-14,
50.9631827978201));
#190126=CARTESIAN_POINT('Origin',(114.229876286196,0.700000000000015,63.489152394136));
#190127=CARTESIAN_POINT('',(113.230857416645,0.700000000000015,66.0082243524688));
#190128=CARTESIAN_POINT('',(113.17348124539,0.700000000000015,66.3033976917261));
#190129=CARTESIAN_POINT('',(113.230857416645,0.700000000000015,66.0082243524688));
#190130=CARTESIAN_POINT('Origin',(116.959178380441,0.700000000000015,51.0204257716897));
#190131=CARTESIAN_POINT('Origin',(116.959178380441,0.700000000000015,51.0204257716897));
#190132=CARTESIAN_POINT('Origin',(113.739062783647,0.700000000000015,63.3937474376868));
#190133=CARTESIAN_POINT('Origin',(116.173876776362,1.45439216225896E-14,
50.8677778413709));
#190134=CARTESIAN_POINT('Origin',(116.173876776362,1.45439216225896E-14,
50.8677778413709));
#190135=CARTESIAN_POINT('Origin',(113.739062783647,1.2,63.3937474376868));
#190136=CARTESIAN_POINT('',(113.724146182571,1.2,66.0908952463201));
#190137=CARTESIAN_POINT('',(113.666722638469,1.2,66.3863122965288));
#190138=CARTESIAN_POINT('',(113.724146182571,1.2,66.0908952463201));
#190139=CARTESIAN_POINT('',(113.236739573243,1.2,65.9779634311333));
#190140=CARTESIAN_POINT('Origin',(116.959178380441,1.2,51.0204257716897));
#190141=CARTESIAN_POINT('',(113.179250699444,1.2,66.273716571817));
#190142=CARTESIAN_POINT('',(113.236739573243,1.2,65.9779634311333));
#190143=CARTESIAN_POINT('Origin',(116.959178380441,1.2,51.0204257716897));
#190144=CARTESIAN_POINT('Origin',(114.229876286196,1.2,63.489152394136));
#190145=CARTESIAN_POINT('',(113.733136532284,1.7,66.0446441374075));
#190146=CARTESIAN_POINT('',(113.675540272641,1.7,66.3409497276097));
#190147=CARTESIAN_POINT('',(113.733136532284,1.7,66.0446441374075));
#190148=CARTESIAN_POINT('Origin',(116.664690278911,1.45439216225896E-14,
50.9631827978201));
#190149=CARTESIAN_POINT('Origin',(116.664690278911,1.45439216225896E-14,
50.9631827978201));
#190150=CARTESIAN_POINT('Origin',(114.229876286196,1.7,63.489152394136));
#190151=CARTESIAN_POINT('',(113.245740383227,1.7,65.9316585090553));
#190152=CARTESIAN_POINT('',(113.188078201874,1.7,66.2283032353676));
#190153=CARTESIAN_POINT('',(113.245740383227,1.7,65.9316585090553));
#190154=CARTESIAN_POINT('Origin',(116.959178380441,1.7,51.0204257716897));
#190155=CARTESIAN_POINT('Origin',(116.959178380441,1.7,51.0204257716897));
#190156=CARTESIAN_POINT('Origin',(113.739062783647,1.7,63.3937474376868));
#190157=CARTESIAN_POINT('Origin',(116.173876776362,1.45439216225896E-14,
50.8677778413709));
#190158=CARTESIAN_POINT('Origin',(116.173876776362,1.45439216225896E-14,
50.8677778413709));
#190159=CARTESIAN_POINT('Origin',(114.720689788746,1.2,63.5845573505853));
#190160=CARTESIAN_POINT('',(114.708250536407,1.2,66.268960368429));
#190161=CARTESIAN_POINT('',(114.65077950191,1.2,66.5646217343204));
#190162=CARTESIAN_POINT('',(114.708250536407,1.2,66.268960368429));
#190163=CARTESIAN_POINT('',(114.214650163263,1.2,66.1878925467383));
#190164=CARTESIAN_POINT('Origin',(116.959178380441,1.2,51.0204257716897));
#190165=CARTESIAN_POINT('',(114.157232547186,1.2,66.4832791000537));
#190166=CARTESIAN_POINT('',(114.214650163263,1.2,66.1878925467383));
#190167=CARTESIAN_POINT('Origin',(116.959178380441,1.2,51.0204257716897));
#190168=CARTESIAN_POINT('Origin',(115.211503291295,1.2,63.6799623070345));
#190169=CARTESIAN_POINT('',(114.717248489969,1.7,66.2226701412973));
#190170=CARTESIAN_POINT('',(114.659604309712,1.7,66.5192222604567));
#190171=CARTESIAN_POINT('',(114.717248489969,1.7,66.2226701412973));
#190172=CARTESIAN_POINT('Origin',(117.64631728401,1.45439216225896E-14,
51.1539927107186));
#190173=CARTESIAN_POINT('Origin',(117.64631728401,1.45439216225896E-14,
51.1539927107186));
#190174=CARTESIAN_POINT('Origin',(115.211503291295,1.7,63.6799623070345));
#190175=CARTESIAN_POINT('',(114.223639563849,1.7,66.1416463206347));
#190176=CARTESIAN_POINT('',(114.166049285884,1.7,66.4379211379298));
#190177=CARTESIAN_POINT('',(114.223639563849,1.7,66.1416463206347));
#190178=CARTESIAN_POINT('Origin',(116.959178380441,1.7,51.0204257716897));
#190179=CARTESIAN_POINT('Origin',(116.959178380441,1.7,51.0204257716897));
#190180=CARTESIAN_POINT('Origin',(114.720689788746,1.7,63.5845573505853));
#190181=CARTESIAN_POINT('Origin',(117.155503781461,1.45439216225896E-14,
51.0585877542694));
#190182=CARTESIAN_POINT('Origin',(117.155503781461,1.45439216225896E-14,
51.0585877542694));
#190183=CARTESIAN_POINT('Origin',(115.702316793845,1.2,63.7753672634838));
#190184=CARTESIAN_POINT('',(115.704785723703,1.2,66.3830747154636));
#190185=CARTESIAN_POINT('',(115.647027250828,1.2,66.6802148162415));
#190186=CARTESIAN_POINT('',(115.704785723703,1.2,66.3830747154636));
#190187=CARTESIAN_POINT('',(115.204956130839,1.2,66.3340532911867));
#190188=CARTESIAN_POINT('Origin',(116.959178380441,1.2,51.0204257716897));
#190189=CARTESIAN_POINT('',(115.147371832686,1.2,66.630297345165));
#190190=CARTESIAN_POINT('',(115.204956130839,1.2,66.3340532911867));
#190191=CARTESIAN_POINT('Origin',(116.959178380441,1.2,51.0204257716897));
#190192=CARTESIAN_POINT('Origin',(116.193130296394,1.2,63.870772219933));
#190193=CARTESIAN_POINT('',(115.713829709111,1.7,66.3365476761963));
#190194=CARTESIAN_POINT('',(115.655895471211,1.7,66.6345920051243));
#190195=CARTESIAN_POINT('',(115.713829709111,1.7,66.3365476761963));
#190196=CARTESIAN_POINT('Origin',(118.62794428911,1.45439216225896E-14,
51.3448026236171));
#190197=CARTESIAN_POINT('Origin',(118.62794428911,1.45439216225896E-14,
51.3448026236171));
#190198=CARTESIAN_POINT('Origin',(116.193130296394,1.7,63.870772219933));
#190199=CARTESIAN_POINT('',(115.213972221154,1.7,66.2876697590143));
#190200=CARTESIAN_POINT('',(115.156213748278,1.7,66.5848098597922));
#190201=CARTESIAN_POINT('',(115.213972221154,1.7,66.2876697590143));
#190202=CARTESIAN_POINT('Origin',(116.959178380441,1.7,51.0204257716897));
#190203=CARTESIAN_POINT('Origin',(116.959178380441,1.7,51.0204257716897));
#190204=CARTESIAN_POINT('Origin',(115.702316793845,1.7,63.7753672634838));
#190205=CARTESIAN_POINT('Origin',(118.13713078656,1.45439216225896E-14,
51.2493976671679));
#190206=CARTESIAN_POINT('Origin',(118.13713078656,1.45439216225896E-14,
51.2493976671679));
#190207=CARTESIAN_POINT('Origin',(115.702316793845,0.200000000000015,63.7753672634838));
#190208=CARTESIAN_POINT('',(115.696080071498,0.200000000000015,66.4278611899825));
#190209=CARTESIAN_POINT('',(115.638489793532,0.200000000000015,66.7241360072775));
#190210=CARTESIAN_POINT('',(115.696080071498,0.200000000000015,66.4278611899825));
#190211=CARTESIAN_POINT('',(115.196277168362,0.200000000000015,66.3787024596368));
#190212=CARTESIAN_POINT('Origin',(116.959178380441,0.200000000000015,51.0204257716897));
#190213=CARTESIAN_POINT('',(115.138859552286,0.200000000000015,66.6740890129522));
#190214=CARTESIAN_POINT('',(115.196277168362,0.200000000000015,66.3787024596368));
#190215=CARTESIAN_POINT('Origin',(116.959178380441,0.200000000000015,51.0204257716897));
#190216=CARTESIAN_POINT('Origin',(116.193130296394,0.200000000000015,63.870772219933));
#190217=CARTESIAN_POINT('',(115.698875495068,0.700000000000015,66.4134800541959));
#190218=CARTESIAN_POINT('',(115.641231314811,0.700000000000015,66.7100321733552));
#190219=CARTESIAN_POINT('',(115.698875495068,0.700000000000015,66.4134800541959));
#190220=CARTESIAN_POINT('Origin',(118.62794428911,1.45439216225896E-14,
51.3448026236171));
#190221=CARTESIAN_POINT('Origin',(118.62794428911,1.45439216225896E-14,
51.3448026236171));
#190222=CARTESIAN_POINT('Origin',(116.193130296394,0.700000000000015,63.870772219933));
#190223=CARTESIAN_POINT('',(115.199064038956,0.700000000000015,66.3643653248782));
#190224=CARTESIAN_POINT('',(115.141593004459,0.700000000000015,66.6600266907696));
#190225=CARTESIAN_POINT('',(115.199064038956,0.700000000000015,66.3643653248782));
#190226=CARTESIAN_POINT('Origin',(116.959178380441,0.700000000000015,51.0204257716897));
#190227=CARTESIAN_POINT('Origin',(116.959178380441,0.700000000000015,51.0204257716897));
#190228=CARTESIAN_POINT('Origin',(115.702316793845,0.700000000000015,63.7753672634838));
#190229=CARTESIAN_POINT('Origin',(118.13713078656,1.45439216225896E-14,
51.2493976671679));
#190230=CARTESIAN_POINT('Origin',(118.13713078656,1.45439216225896E-14,
51.2493976671679));
#190231=CARTESIAN_POINT('Origin',(117.174757301493,-8.3,64.0615821328315));
#190232=CARTESIAN_POINT('',(116.66557384992,-8.3,64.0606818998006));
#190233=CARTESIAN_POINT('',(116.597027861112,-8.3,64.4133186820487));
#190234=CARTESIAN_POINT('',(116.66557384992,-8.3,64.0606818998006));
#190235=CARTESIAN_POINT('',(117.174968553192,-8.30043647285503,64.0619238523546));
#190236=CARTESIAN_POINT('Origin',(116.959178380441,-8.3,51.0204257716897));
#190237=CARTESIAN_POINT('',(117.105590222673,-8.3,64.4174141302515));
#190238=CARTESIAN_POINT('',(117.174757301493,-8.3,64.0615821328315));
#190239=CARTESIAN_POINT('Origin',(116.959178380441,-8.3,51.0204257716897));
#190240=CARTESIAN_POINT('Origin',(116.683943798944,-8.3,63.9661771763823));
#190241=CARTESIAN_POINT('',(116.683943798944,-8.8,63.9661771763823));
#190242=CARTESIAN_POINT('',(116.65952420634,-8.8,64.0918044626649));
#190243=CARTESIAN_POINT('',(116.683943798944,-8.8,63.9661771763823));
#190244=CARTESIAN_POINT('',(116.683943798944,-8.44726287030299,63.9661771763823));
#190245=CARTESIAN_POINT('',(116.683943798944,-8.44726287030299,63.9661771763823));
#190246=CARTESIAN_POINT('Origin',(119.118757791659,1.45439216225896E-14,
51.4402075800664));
#190247=CARTESIAN_POINT('Origin',(119.118757791659,1.45439216225896E-14,
51.4402075800664));
#190248=CARTESIAN_POINT('Origin',(116.683943798944,-8.8,63.9661771763823));
#190249=CARTESIAN_POINT('',(117.174757301493,-8.8,64.0615821328315));
#190250=CARTESIAN_POINT('',(117.168540939797,-8.8,64.0935623817685));
#190251=CARTESIAN_POINT('',(117.174757301493,-8.8,64.0615821328315));
#190252=CARTESIAN_POINT('',(116.683943798944,-8.8,63.9661771763823));
#190253=CARTESIAN_POINT('Origin',(116.959178380441,-8.8,51.0204257716897));
#190254=CARTESIAN_POINT('Origin',(117.174757301493,-8.8,64.0615821328315));
#190255=CARTESIAN_POINT('',(117.174757301493,-9.,64.0615821328315));
#190256=CARTESIAN_POINT('Origin',(119.609571294209,1.45439216225896E-14,
51.5356125365156));
#190257=CARTESIAN_POINT('Origin',(116.487618397924,-9.,63.9280151938026));
#190258=CARTESIAN_POINT('Origin',(114.524364387726,1.45439216225896E-14,
63.5463953680056));
#190259=CARTESIAN_POINT('Origin',(116.193130296394,-8.3,63.870772219933));
#190260=CARTESIAN_POINT('',(115.658845070641,-8.3,63.9990087756383));
#190261=CARTESIAN_POINT('',(115.590974766137,-8.3,64.3481694808335));
#190262=CARTESIAN_POINT('',(115.658845070641,-8.3,63.9990087756383));
#190263=CARTESIAN_POINT('',(116.160332513205,-8.3,64.0395013451467));
#190264=CARTESIAN_POINT('Origin',(116.959178380441,-8.3,51.0204257716897));
#190265=CARTESIAN_POINT('',(116.09217650258,-8.3,64.3901318735768));
#190266=CARTESIAN_POINT('',(116.160332513205,-8.3,64.0395013451467));
#190267=CARTESIAN_POINT('Origin',(116.959178380441,-8.3,51.0204257716897));
#190268=CARTESIAN_POINT('Origin',(115.702316793845,-8.3,63.7753672634838));
#190269=CARTESIAN_POINT('',(115.702316793845,-8.8,63.7753672634838));
#190270=CARTESIAN_POINT('',(115.652856553532,-8.8,64.029816871641));
#190271=CARTESIAN_POINT('',(115.702316793845,-8.8,63.7753672634838));
#190272=CARTESIAN_POINT('',(115.702316793845,-8.64616967217299,63.7753672634838));
#190273=CARTESIAN_POINT('',(115.702316793845,-8.64616967217299,63.7753672634838));
#190274=CARTESIAN_POINT('Origin',(118.13713078656,1.45439216225896E-14,
51.2493976671679));
#190275=CARTESIAN_POINT('Origin',(118.13713078656,1.45439216225896E-14,
51.2493976671679));
#190276=CARTESIAN_POINT('Origin',(115.702316793845,-8.8,63.7753672634838));
#190277=CARTESIAN_POINT('',(116.193130296394,-8.8,63.870772219933));
#190278=CARTESIAN_POINT('',(116.154318154922,-8.8,64.0704423818052));
#190279=CARTESIAN_POINT('',(116.193130296394,-8.8,63.870772219933));
#190280=CARTESIAN_POINT('',(115.702316793845,-8.8,63.7753672634838));
#190281=CARTESIAN_POINT('Origin',(116.959178380441,-8.8,51.0204257716897));
#190282=CARTESIAN_POINT('Origin',(116.193130296394,-8.8,63.870772219933));
#190283=CARTESIAN_POINT('',(116.193130296394,-8.56190691376599,63.870772219933));
#190284=CARTESIAN_POINT('Origin',(118.62794428911,1.45439216225896E-14,
51.3448026236171));
#190285=CARTESIAN_POINT('',(116.193130296394,-8.8,63.870772219933));
#190286=CARTESIAN_POINT('Origin',(118.62794428911,1.45439216225896E-14,
51.3448026236171));
#190287=CARTESIAN_POINT('Origin',(115.505991392825,-9.,63.7372052809041));
#190288=CARTESIAN_POINT('Origin',(114.524364387726,1.45439216225896E-14,
63.5463953680056));
#190289=CARTESIAN_POINT('Origin',(115.211503291295,-8.3,63.6799623070345));
#190290=CARTESIAN_POINT('',(114.6669556341,-8.3,63.8609942321634));
#190291=CARTESIAN_POINT('',(114.599357801212,-8.3,64.2087531994098));
#190292=CARTESIAN_POINT('',(114.6669556341,-8.3,63.8609942321634));
#190293=CARTESIAN_POINT('',(115.161063153857,-8.3,63.939453023728));
#190294=CARTESIAN_POINT('Origin',(116.959178380441,-8.3,51.0204257716897));
#190295=CARTESIAN_POINT('',(115.093378099059,-8.3,64.2876607065586));
#190296=CARTESIAN_POINT('',(115.161063153857,-8.3,63.939453023728));
#190297=CARTESIAN_POINT('Origin',(116.959178380441,-8.3,51.0204257716897));
#190298=CARTESIAN_POINT('Origin',(114.720689788746,-8.3,63.5845573505853));
#190299=CARTESIAN_POINT('',(114.720689788746,-8.8,63.5845573505853));
#190300=CARTESIAN_POINT('',(114.66099175365,-8.8,63.8916755841782));
#190301=CARTESIAN_POINT('',(114.720689788746,-8.8,63.5845573505853));
#190302=CARTESIAN_POINT('',(114.720689788746,-8.72675483785299,63.5845573505853));
#190303=CARTESIAN_POINT('',(114.720689788746,-8.72675483785299,63.5845573505853));
#190304=CARTESIAN_POINT('Origin',(117.155503781461,1.45439216225896E-14,
51.0585877542694));
#190305=CARTESIAN_POINT('Origin',(117.155503781461,1.45439216225896E-14,
51.0585877542694));
#190306=CARTESIAN_POINT('Origin',(114.720689788746,-8.8,63.5845573505853));
#190307=CARTESIAN_POINT('',(115.211503291295,-8.8,63.6799623070345));
#190308=CARTESIAN_POINT('',(115.15509138767,-8.8,63.970174944139));
#190309=CARTESIAN_POINT('',(115.211503291295,-8.8,63.6799623070345));
#190310=CARTESIAN_POINT('',(114.720689788746,-8.8,63.5845573505853));
#190311=CARTESIAN_POINT('Origin',(116.959178380441,-8.8,51.0204257716897));
#190312=CARTESIAN_POINT('Origin',(115.211503291295,-8.8,63.6799623070345));
#190313=CARTESIAN_POINT('',(115.211503291295,-8.70093385792599,63.6799623070345));
#190314=CARTESIAN_POINT('Origin',(117.64631728401,1.45439216225896E-14,
51.1539927107186));
#190315=CARTESIAN_POINT('',(115.211503291295,-8.8,63.6799623070345));
#190316=CARTESIAN_POINT('Origin',(117.64631728401,1.45439216225896E-14,
51.1539927107186));
#190317=CARTESIAN_POINT('Origin',(114.524364387726,-9.,63.5463953680056));
#190318=CARTESIAN_POINT('Origin',(114.524364387726,1.45439216225896E-14,
63.5463953680056));
#190319=CARTESIAN_POINT('Origin',(114.229876286196,-8.3,63.489152394136));
#190320=CARTESIAN_POINT('',(113.68972162259,-8.3,63.6475844392384));
#190321=CARTESIAN_POINT('',(113.622007418688,-8.3,63.9959420804558));
#190322=CARTESIAN_POINT('',(113.68972162259,-8.3,63.6475844392384));
#190323=CARTESIAN_POINT('',(114.176507918113,-8.3,63.7637074763767));
#190324=CARTESIAN_POINT('Origin',(116.959178380441,-8.3,51.0204257716897));
#190325=CARTESIAN_POINT('',(114.108900410553,-8.3,64.1115162152435));
#190326=CARTESIAN_POINT('',(114.176507918113,-8.3,63.7637074763767));
#190327=CARTESIAN_POINT('Origin',(116.959178380441,-8.3,51.0204257716897));
#190328=CARTESIAN_POINT('Origin',(113.739062783647,-8.3,63.3937474376868));
#190329=CARTESIAN_POINT('',(113.739062783647,-8.8,63.3937474376868));
#190330=CARTESIAN_POINT('',(113.683747220861,-8.8,63.6783199182644));
#190331=CARTESIAN_POINT('',(113.739062783647,-8.8,63.3937474376868));
#190332=CARTESIAN_POINT('',(113.739062783647,-8.69230981960499,63.3937474376868));
#190333=CARTESIAN_POINT('',(113.739062783647,-8.69230981960499,63.3937474376868));
#190334=CARTESIAN_POINT('Origin',(116.173876776362,1.45439216225896E-14,
50.8677778413709));
#190335=CARTESIAN_POINT('Origin',(116.173876776362,1.45439216225896E-14,
50.8677778413709));
#190336=CARTESIAN_POINT('Origin',(113.739062783647,-8.8,63.3937474376868));
#190337=CARTESIAN_POINT('',(114.229876286196,-8.8,63.489152394136));
#190338=CARTESIAN_POINT('',(114.170543163013,-8.8,63.7943933280519));
#190339=CARTESIAN_POINT('',(114.229876286196,-8.8,63.489152394136));
#190340=CARTESIAN_POINT('',(113.739062783647,-8.8,63.3937474376868));
#190341=CARTESIAN_POINT('Origin',(116.959178380441,-8.8,51.0204257716897));
#190342=CARTESIAN_POINT('Origin',(114.229876286196,-8.8,63.489152394136));
#190343=CARTESIAN_POINT('',(114.229876286196,-8.72388961415699,63.489152394136));
#190344=CARTESIAN_POINT('Origin',(116.664690278911,1.45439216225896E-14,
50.9631827978201));
#190345=CARTESIAN_POINT('',(114.229876286196,-8.8,63.489152394136));
#190346=CARTESIAN_POINT('Origin',(116.664690278911,1.45439216225896E-14,
50.9631827978201));
#190347=CARTESIAN_POINT('Origin',(113.542737382627,-9.,63.3555854551071));
#190348=CARTESIAN_POINT('Origin',(114.524364387726,1.45439216225896E-14,
63.5463953680056));
#190349=CARTESIAN_POINT('Origin',(113.248249281097,-8.3,63.2983424812375));
#190350=CARTESIAN_POINT('',(112.727221388347,-8.3,63.3583763115525));
#190351=CARTESIAN_POINT('',(112.65899587179,-8.3,63.7093644152198));
#190352=CARTESIAN_POINT('',(112.727221388347,-8.3,63.3583763115525));
#190353=CARTESIAN_POINT('',(113.206614610098,-8.3,63.5125332262568));
#190354=CARTESIAN_POINT('Origin',(116.959178380441,-8.3,51.0204257716897));
#190355=CARTESIAN_POINT('',(113.138695302267,-8.3,63.8619460304553));
#190356=CARTESIAN_POINT('',(113.206614610098,-8.3,63.5125332262568));
#190357=CARTESIAN_POINT('Origin',(116.959178380441,-8.3,51.0204257716897));
#190358=CARTESIAN_POINT('Origin',(112.757435778548,-8.3,63.2029375247883));
#190359=CARTESIAN_POINT('',(112.757435778548,-8.8,63.2029375247883));
#190360=CARTESIAN_POINT('',(112.72120074226,-8.8,63.3893496959914));
#190361=CARTESIAN_POINT('',(112.757435778548,-8.8,63.2029375247883));
#190362=CARTESIAN_POINT('',(112.757435778548,-8.54144308650499,63.2029375247883));
#190363=CARTESIAN_POINT('',(112.757435778548,-8.54144308650499,63.2029375247883));
#190364=CARTESIAN_POINT('Origin',(115.192249771263,1.45439216225896E-14,
50.6769679284724));
#190365=CARTESIAN_POINT('Origin',(115.192249771263,1.45439216225896E-14,
50.6769679284724));
#190366=CARTESIAN_POINT('Origin',(112.757435778548,-8.8,63.2029375247883));
#190367=CARTESIAN_POINT('',(113.248249281097,-8.8,63.2983424812375));
#190368=CARTESIAN_POINT('',(113.200621661374,-8.8,63.5433641208314));
#190369=CARTESIAN_POINT('',(113.248249281097,-8.8,63.2983424812375));
#190370=CARTESIAN_POINT('',(112.757435778548,-8.8,63.2029375247883));
#190371=CARTESIAN_POINT('Origin',(116.959178380441,-8.8,51.0204257716897));
#190372=CARTESIAN_POINT('Origin',(113.248249281097,-8.8,63.2983424812375));
#190373=CARTESIAN_POINT('',(113.248249281097,-8.63170029600199,63.2983424812375));
#190374=CARTESIAN_POINT('Origin',(115.683063273812,1.45439216225896E-14,
50.7723728849216));
#190375=CARTESIAN_POINT('',(113.248249281097,-8.8,63.2983424812375));
#190376=CARTESIAN_POINT('Origin',(115.683063273812,1.45439216225896E-14,
50.7723728849216));
#190377=CARTESIAN_POINT('Origin',(112.561110377528,-9.,63.1647755422086));
#190378=CARTESIAN_POINT('Origin',(114.524364387726,1.45439216225896E-14,
63.5463953680056));
#190379=CARTESIAN_POINT('Origin',(112.266622275998,-8.3,63.107532568339));
#190380=CARTESIAN_POINT('',(111.775808773449,-8.3,63.0121276118898));
#190381=CARTESIAN_POINT('',(111.710643451443,-8.3,63.3473724579512));
#190382=CARTESIAN_POINT('',(111.775808773449,-8.3,63.0121276118898));
#190383=CARTESIAN_POINT('',(111.871019148132,-8.3,63.030634726309));
#190384=CARTESIAN_POINT('',(111.871019148132,-8.3,63.030634726309));
#190385=CARTESIAN_POINT('',(112.251593893842,-8.3,63.1848465062967));
#190386=CARTESIAN_POINT('Origin',(116.959178380441,-8.3,51.0204257716897));
#190387=CARTESIAN_POINT('',(112.182956955252,-8.3,63.5379511822739));
#190388=CARTESIAN_POINT('',(112.251593893842,-8.3,63.1848465062967));
#190389=CARTESIAN_POINT('Origin',(116.959178380441,-8.3,51.0204257716897));
#190390=CARTESIAN_POINT('Origin',(111.775808773449,-8.3,63.0121276118898));
#190391=CARTESIAN_POINT('',(111.775808773449,-8.8,63.0121276118898));
#190392=CARTESIAN_POINT('',(111.773697539863,-8.8,63.0229889129114));
#190393=CARTESIAN_POINT('',(111.775808773449,-8.8,63.0121276118898));
#190394=CARTESIAN_POINT('',(111.775808773449,-8.3,63.0121276118898));
#190395=CARTESIAN_POINT('Origin',(114.210622766164,1.45439216225896E-14,
50.4861580155739));
#190396=CARTESIAN_POINT('Origin',(111.775808773449,-8.8,63.0121276118898));
#190397=CARTESIAN_POINT('',(112.266622275998,-8.8,63.107532568339));
#190398=CARTESIAN_POINT('',(112.245536018932,-8.8,63.2160114154701));
#190399=CARTESIAN_POINT('',(112.266622275998,-8.8,63.107532568339));
#190400=CARTESIAN_POINT('',(111.775808773449,-8.8,63.0121276118898));
#190401=CARTESIAN_POINT('Origin',(116.959178380441,-8.8,51.0204257716897));
#190402=CARTESIAN_POINT('Origin',(112.266622275998,-8.8,63.107532568339));
#190403=CARTESIAN_POINT('',(112.266622275998,-8.42058489654999,63.107532568339));
#190404=CARTESIAN_POINT('Origin',(114.701436268713,1.45439216225896E-14,
50.5815629720231));
#190405=CARTESIAN_POINT('',(112.266622275998,-8.8,63.107532568339));
#190406=CARTESIAN_POINT('Origin',(114.701436268713,1.45439216225896E-14,
50.5815629720231));
#190407=CARTESIAN_POINT('Origin',(111.579483372429,-9.,62.9739656293101));
#190408=CARTESIAN_POINT('Origin',(114.524364387726,1.45439216225896E-14,
63.5463953680056));
#190409=CARTESIAN_POINT('Origin',(106.376860245404,-2.3,61.962673090948));
#190410=CARTESIAN_POINT('',(105.886046742854,-2.3,61.8672681344988));
#190411=CARTESIAN_POINT('',(105.864960485789,-2.3,61.9757469816299));
#190412=CARTESIAN_POINT('',(105.886046742854,-2.3,61.8672681344988));
#190413=CARTESIAN_POINT('',(106.258490854543,-2.3,61.9396642973404));
#190414=CARTESIAN_POINT('',(106.258490854543,-2.3,61.9396642973404));
#190415=CARTESIAN_POINT('',(106.361831863248,-2.3,62.0399870289056));
#190416=CARTESIAN_POINT('Origin',(116.959178380441,-2.3,51.0204257716897));
#190417=CARTESIAN_POINT('',(106.293194924658,-2.3,62.3930917048829));
#190418=CARTESIAN_POINT('',(106.361831863248,-2.3,62.0399870289056));
#190419=CARTESIAN_POINT('Origin',(116.959178380441,-2.3,51.0204257716897));
#190420=CARTESIAN_POINT('Origin',(105.886046742854,-2.3,61.8672681344988));
#190421=CARTESIAN_POINT('',(105.886046742854,-2.8,61.8672681344988));
#190422=CARTESIAN_POINT('',(105.883935509269,-2.8,61.8781294355204));
#190423=CARTESIAN_POINT('',(105.886046742854,-2.8,61.8672681344988));
#190424=CARTESIAN_POINT('',(105.886046742854,-2.3,61.8672681344988));
#190425=CARTESIAN_POINT('Origin',(108.32086073557,1.45439216225896E-14,
49.3412985381828));
#190426=CARTESIAN_POINT('Origin',(105.886046742854,-2.8,61.8672681344988));
#190427=CARTESIAN_POINT('',(106.376860245404,-2.8,61.962673090948));
#190428=CARTESIAN_POINT('',(106.311694923398,-2.8,62.2979179370094));
#190429=CARTESIAN_POINT('',(106.376860245404,-2.8,61.962673090948));
#190430=CARTESIAN_POINT('',(105.886046742854,-2.8,61.8672681344988));
#190431=CARTESIAN_POINT('Origin',(116.959178380441,-2.8,51.0204257716897));
#190432=CARTESIAN_POINT('Origin',(106.376860245404,-2.8,61.962673090948));
#190433=CARTESIAN_POINT('',(106.376860245404,-2.70300758415499,61.962673090948));
#190434=CARTESIAN_POINT('Origin',(108.811674238119,1.45439216225896E-14,
49.4367034946321));
#190435=CARTESIAN_POINT('',(106.376860245404,-2.8,61.962673090948));
#190436=CARTESIAN_POINT('Origin',(108.811674238119,1.45439216225896E-14,
49.4367034946321));
#190437=CARTESIAN_POINT('Origin',(105.689721341835,-3.,61.8291061519191));
#190438=CARTESIAN_POINT('Origin',(114.524364387726,1.45439216225896E-14,
63.5463953680056));
#190439=CARTESIAN_POINT('Origin',(106.376860245404,-1.8,61.962673090948));
#190440=CARTESIAN_POINT('',(106.335225574405,-1.3,62.1768638359673));
#190441=CARTESIAN_POINT('',(106.267306266574,-1.3,62.5262766401657));
#190442=CARTESIAN_POINT('',(106.335225574405,-1.3,62.1768638359673));
#190443=CARTESIAN_POINT('',(106.346645855203,-1.8,62.1181118777122));
#190444=CARTESIAN_POINT('Origin',(108.811674238119,1.45439216225896E-14,
49.4367034946321));
#190445=CARTESIAN_POINT('',(106.278420338646,-1.8,62.4690999813795));
#190446=CARTESIAN_POINT('',(106.346645855203,-1.8,62.1181118777122));
#190447=CARTESIAN_POINT('Origin',(108.811674238119,1.45439216225896E-14,
49.4367034946321));
#190448=CARTESIAN_POINT('Origin',(106.376860245404,-1.3,61.962673090948));
#190449=CARTESIAN_POINT('',(105.886046742854,-1.3,61.8672681344988));
#190450=CARTESIAN_POINT('',(105.838419123131,-1.3,62.1122897740926));
#190451=CARTESIAN_POINT('',(105.886046742854,-1.3,61.8672681344988));
#190452=CARTESIAN_POINT('',(106.051254277249,-1.3,61.8993813863595));
#190453=CARTESIAN_POINT('',(106.051254277249,-1.3,61.8993813863595));
#190454=CARTESIAN_POINT('Origin',(116.959178380441,-1.3,51.0204257716897));
#190455=CARTESIAN_POINT('Origin',(116.959178380441,-1.3,51.0204257716897));
#190456=CARTESIAN_POINT('Origin',(105.886046742854,-1.3,61.8672681344988));
#190457=CARTESIAN_POINT('',(105.886046742854,-1.8,61.8672681344988));
#190458=CARTESIAN_POINT('',(105.849811706567,-1.8,62.0536803057019));
#190459=CARTESIAN_POINT('',(105.886046742854,-1.8,61.8672681344988));
#190460=CARTESIAN_POINT('',(105.886046742854,-1.3,61.8672681344988));
#190461=CARTESIAN_POINT('Origin',(108.32086073557,1.45439216225896E-14,
49.3412985381828));
#190462=CARTESIAN_POINT('Origin',(105.886046742854,-1.8,61.8672681344988));
#190463=CARTESIAN_POINT('',(106.139853191496,-1.8,61.916603356642));
#190464=CARTESIAN_POINT('Origin',(116.959178380441,-1.8,51.0204257716897));
#190465=CARTESIAN_POINT('',(105.886046742854,-1.8,61.8672681344988));
#190466=CARTESIAN_POINT('Origin',(116.959178380441,-1.8,51.0204257716897));
#190467=CARTESIAN_POINT('Origin',(105.689721341835,-2.,61.8291061519191));
#190468=CARTESIAN_POINT('Origin',(114.524364387726,1.45439216225896E-14,
63.5463953680056));
#190469=CARTESIAN_POINT('Origin',(106.376860245404,-0.799999999999986,61.962673090948));
#190470=CARTESIAN_POINT('',(106.323491877321,-0.299999999999985,62.2372281731886));
#190471=CARTESIAN_POINT('',(106.255884369761,-0.299999999999985,62.5850369120555));
#190472=CARTESIAN_POINT('',(106.323491877321,-0.299999999999985,62.2372281731886));
#190473=CARTESIAN_POINT('',(106.327519084347,-0.799999999999986,62.2165100924996));
#190474=CARTESIAN_POINT('Origin',(108.811674238119,1.45439216225896E-14,
49.4367034946321));
#190475=CARTESIAN_POINT('',(106.259804880446,-0.799999999999986,62.564867733717));
#190476=CARTESIAN_POINT('',(106.327519084347,-0.799999999999986,62.2165100924996));
#190477=CARTESIAN_POINT('Origin',(108.811674238119,1.45439216225896E-14,
49.4367034946321));
#190478=CARTESIAN_POINT('Origin',(106.376860245404,-0.299999999999985,61.962673090948));
#190479=CARTESIAN_POINT('',(105.886046742854,-0.299999999999985,61.8672681344988));
#190480=CARTESIAN_POINT('',(105.826713619671,-0.299999999999985,62.1725090684146));
#190481=CARTESIAN_POINT('',(105.886046742854,-0.299999999999985,61.8672681344988));
#190482=CARTESIAN_POINT('',(105.960758752966,-0.299999999999985,61.8817907505921));
#190483=CARTESIAN_POINT('',(105.960758752966,-0.299999999999985,61.8817907505921));
#190484=CARTESIAN_POINT('Origin',(116.959178380441,-0.299999999999985,51.0204257716897));
#190485=CARTESIAN_POINT('Origin',(116.959178380441,-0.299999999999985,51.0204257716897));
#190486=CARTESIAN_POINT('Origin',(105.886046742854,-0.299999999999985,61.8672681344988));
#190487=CARTESIAN_POINT('',(105.886046742854,-0.799999999999986,61.8672681344988));
#190488=CARTESIAN_POINT('',(105.830731180069,-0.799999999999986,62.1518406150764));
#190489=CARTESIAN_POINT('',(105.886046742854,-0.799999999999986,61.8672681344988));
#190490=CARTESIAN_POINT('',(105.886046742854,-0.299999999999985,61.8672681344988));
#190491=CARTESIAN_POINT('Origin',(108.32086073557,1.45439216225896E-14,
49.3412985381828));
#190492=CARTESIAN_POINT('Origin',(105.886046742854,-0.799999999999986,61.8672681344988));
#190493=CARTESIAN_POINT('',(105.991758332114,-0.799999999999986,61.88781648844));
#190494=CARTESIAN_POINT('Origin',(116.959178380441,-0.799999999999986,51.0204257716897));
#190495=CARTESIAN_POINT('',(105.886046742854,-0.799999999999986,61.8672681344988));
#190496=CARTESIAN_POINT('Origin',(116.959178380441,-0.799999999999986,51.0204257716897));
#190497=CARTESIAN_POINT('Origin',(105.689721341835,-0.999999999999985,61.8291061519191));
#190498=CARTESIAN_POINT('Origin',(114.524364387726,1.45439216225896E-14,
63.5463953680056));
#190499=CARTESIAN_POINT('Origin',(119.138011311691,-7.3,64.4432019586286));
#190500=CARTESIAN_POINT('',(118.608137303018,-7.3,64.5487448830385));
#190501=CARTESIAN_POINT('',(118.540149211821,-7.3,64.8985115452097));
#190502=CARTESIAN_POINT('',(118.608137303018,-7.3,64.5487448830385));
#190503=CARTESIAN_POINT('',(119.131916138895,-7.3,64.4745587478364));
#190504=CARTESIAN_POINT('Origin',(116.959178380441,-7.3,51.0204257716897));
#190505=CARTESIAN_POINT('',(119.063034885886,-7.3,64.8289203062656));
#190506=CARTESIAN_POINT('',(119.131916138895,-7.3,64.4745587478364));
#190507=CARTESIAN_POINT('Origin',(116.959178380441,-7.3,51.0204257716897));
#190508=CARTESIAN_POINT('Origin',(118.647197809142,-7.3,64.3477970021793));
#190509=CARTESIAN_POINT('',(118.647197809142,-7.8,64.3477970021793));
#190510=CARTESIAN_POINT('',(118.594808184532,-7.8,64.6173169108791));
#190511=CARTESIAN_POINT('',(118.647197809142,-7.8,64.3477970021793));
#190512=CARTESIAN_POINT('',(118.647197809142,-7.65220556441099,64.3477970021793));
#190513=CARTESIAN_POINT('',(118.647197809142,-7.65220556441099,64.3477970021793));
#190514=CARTESIAN_POINT('Origin',(121.082011801857,1.45439216225896E-14,
51.8218274058634));
#190515=CARTESIAN_POINT('Origin',(121.082011801857,1.45439216225896E-14,
51.8218274058634));
#190516=CARTESIAN_POINT('Origin',(118.647197809142,-7.8,64.3477970021793));
#190517=CARTESIAN_POINT('',(119.138011311691,-7.8,64.4432019586286));
#190518=CARTESIAN_POINT('',(119.118407990194,-7.8,64.5440518016936));
#190519=CARTESIAN_POINT('',(119.138011311691,-7.8,64.4432019586286));
#190520=CARTESIAN_POINT('',(118.647197809142,-7.8,64.3477970021793));
#190521=CARTESIAN_POINT('Origin',(116.959178380441,-7.8,51.0204257716897));
#190522=CARTESIAN_POINT('Origin',(119.138011311691,-7.8,64.4432019586286));
#190523=CARTESIAN_POINT('',(119.138011311691,-7.35569507252699,64.4432019586286));
#190524=CARTESIAN_POINT('Origin',(121.572825304407,1.45439216225896E-14,
51.9172323623126));
#190525=CARTESIAN_POINT('',(119.138011311691,-7.8,64.4432019586286));
#190526=CARTESIAN_POINT('Origin',(121.572825304407,1.45439216225896E-14,
51.9172323623126));
#190527=CARTESIAN_POINT('Origin',(118.450872408122,-8.,64.3096350195996));
#190528=CARTESIAN_POINT('Origin',(114.524364387726,1.45439216225896E-14,
63.5463953680056));
#190529=CARTESIAN_POINT('Origin',(117.665570804043,-7.8,64.1569870892808));
#190530=CARTESIAN_POINT('',(118.143958075359,-7.8,64.3163191445107));
#190531=CARTESIAN_POINT('',(118.075250147152,-7.8,64.6697890285819));
#190532=CARTESIAN_POINT('',(118.143958075359,-7.8,64.3163191445107));
#190533=CARTESIAN_POINT('',(117.627614331757,-7.8,64.3522552367681));
#190534=CARTESIAN_POINT('Origin',(116.959178380441,-7.8,51.0204257716897));
#190535=CARTESIAN_POINT('',(117.55959669792,-7.8,64.7021738818927));
#190536=CARTESIAN_POINT('',(117.627614331757,-7.8,64.3522552367681));
#190537=CARTESIAN_POINT('Origin',(116.959178380441,-7.8,51.0204257716897));
#190538=CARTESIAN_POINT('Origin',(118.156384306592,-7.8,64.25239204573));
#190539=CARTESIAN_POINT('',(118.088426174981,-7.3,64.6020045799654));
#190540=CARTESIAN_POINT('',(118.021202443878,-7.3,64.947838969973));
#190541=CARTESIAN_POINT('',(118.088426174981,-7.3,64.6020045799654));
#190542=CARTESIAN_POINT('Origin',(120.591198299308,1.45439216225896E-14,
51.7264224494141));
#190543=CARTESIAN_POINT('Origin',(120.591198299308,1.45439216225896E-14,
51.7264224494141));
#190544=CARTESIAN_POINT('Origin',(118.156384306592,-7.3,64.25239204573));
#190545=CARTESIAN_POINT('',(117.572643242488,-7.3,64.6350555635753));
#190546=CARTESIAN_POINT('',(117.506066436225,-7.3,64.9775618304052));
#190547=CARTESIAN_POINT('',(117.572643242488,-7.3,64.6350555635753));
#190548=CARTESIAN_POINT('Origin',(116.959178380441,-7.3,51.0204257716897));
#190549=CARTESIAN_POINT('Origin',(116.959178380441,-7.3,51.0204257716897));
#190550=CARTESIAN_POINT('Origin',(117.665570804043,-7.3,64.1569870892808));
#190551=CARTESIAN_POINT('Origin',(120.100384796758,1.45439216225896E-14,
51.6310174929649));
#190552=CARTESIAN_POINT('Origin',(120.100384796758,1.45439216225896E-14,
51.6310174929649));
#190553=CARTESIAN_POINT('Origin',(116.683943798944,-7.8,63.9661771763823));
#190554=CARTESIAN_POINT('',(117.115177856914,-7.8,64.3680902741484));
#190555=CARTESIAN_POINT('',(117.047734255941,-7.8,64.7150557909319));
#190556=CARTESIAN_POINT('',(117.115177856914,-7.8,64.3680902741484));
#190557=CARTESIAN_POINT('',(116.606547757441,-7.8,64.3643433055556));
#190558=CARTESIAN_POINT('Origin',(116.959178380441,-7.8,51.0204257716897));
#190559=CARTESIAN_POINT('',(116.539570003489,-7.8,64.708912259135));
#190560=CARTESIAN_POINT('',(116.606547757441,-7.8,64.3643433055556));
#190561=CARTESIAN_POINT('Origin',(116.959178380441,-7.8,51.0204257716897));
#190562=CARTESIAN_POINT('Origin',(117.174757301493,-7.8,64.0615821328315));
#190563=CARTESIAN_POINT('',(117.060673059164,-7.3,64.6484917510221));
#190564=CARTESIAN_POINT('',(116.994634850768,-7.3,64.9882271858619));
#190565=CARTESIAN_POINT('',(117.060673059164,-7.3,64.6484917510221));
#190566=CARTESIAN_POINT('Origin',(119.609571294209,1.45439216225896E-14,
51.5356125365156));
#190567=CARTESIAN_POINT('Origin',(119.609571294209,1.45439216225896E-14,
51.5356125365156));
#190568=CARTESIAN_POINT('Origin',(117.174757301493,-7.3,64.0615821328315));
#190569=CARTESIAN_POINT('',(116.552421327236,-7.3,64.6427982598684));
#190570=CARTESIAN_POINT('',(116.486820626901,-7.3,64.9802829220894));
#190571=CARTESIAN_POINT('',(116.552421327236,-7.3,64.6427982598684));
#190572=CARTESIAN_POINT('Origin',(116.959178380441,-7.3,51.0204257716897));
#190573=CARTESIAN_POINT('Origin',(116.959178380441,-7.3,51.0204257716897));
#190574=CARTESIAN_POINT('Origin',(116.683943798944,-7.3,63.9661771763823));
#190575=CARTESIAN_POINT('Origin',(119.118757791659,1.45439216225896E-14,
51.4402075800664));
#190576=CARTESIAN_POINT('Origin',(119.118757791659,1.45439216225896E-14,
51.4402075800664));
#190577=CARTESIAN_POINT('Origin',(115.702316793845,-7.8,63.7753672634838));
#190578=CARTESIAN_POINT('',(116.101643499298,-7.8,64.3414286406355));
#190579=CARTESIAN_POINT('',(116.035029699075,-7.8,64.6841252239447));
#190580=CARTESIAN_POINT('',(116.101643499298,-7.8,64.3414286406355));
#190581=CARTESIAN_POINT('',(115.600402993959,-7.8,64.2996656955739));
#190582=CARTESIAN_POINT('Origin',(116.959178380441,-7.8,51.0204257716897));
#190583=CARTESIAN_POINT('',(115.534056011535,-7.8,64.6409896271509));
#190584=CARTESIAN_POINT('',(115.600402993959,-7.8,64.2996656955739));
#190585=CARTESIAN_POINT('Origin',(116.959178380441,-7.8,51.0204257716897));
#190586=CARTESIAN_POINT('Origin',(116.193130296394,-7.8,63.870772219933));
#190587=CARTESIAN_POINT('',(116.047812650375,-7.3,64.618362968668));
#190588=CARTESIAN_POINT('',(115.982554022284,-7.3,64.9540878305312));
#190589=CARTESIAN_POINT('',(116.047812650375,-7.3,64.618362968668));
#190590=CARTESIAN_POINT('Origin',(118.62794428911,1.45439216225896E-14,
51.3448026236171));
#190591=CARTESIAN_POINT('Origin',(118.62794428911,1.45439216225896E-14,
51.3448026236171));
#190592=CARTESIAN_POINT('Origin',(116.193130296394,-7.3,63.870772219933));
#190593=CARTESIAN_POINT('',(115.546788823354,-7.3,64.5754853158576));
#190594=CARTESIAN_POINT('',(115.481781115242,-7.3,64.9099193127751));
#190595=CARTESIAN_POINT('',(115.546788823354,-7.3,64.5754853158576));
#190596=CARTESIAN_POINT('Origin',(116.959178380441,-7.3,51.0204257716897));
#190597=CARTESIAN_POINT('Origin',(116.959178380441,-7.3,51.0204257716897));
#190598=CARTESIAN_POINT('Origin',(115.702316793845,-7.3,63.7753672634838));
#190599=CARTESIAN_POINT('Origin',(118.13713078656,1.45439216225896E-14,
51.2493976671679));
#190600=CARTESIAN_POINT('Origin',(118.13713078656,1.45439216225896E-14,
51.2493976671679));
#190601=CARTESIAN_POINT('Origin',(114.720689788746,-7.8,63.5845573505853));
#190602=CARTESIAN_POINT('',(115.102781183328,-7.8,64.2392862730183));
#190603=CARTESIAN_POINT('',(115.03660728363,-7.8,64.5797197756079));
#190604=CARTESIAN_POINT('',(115.102781183328,-7.8,64.2392862730183));
#190605=CARTESIAN_POINT('',(114.608749045379,-7.8,64.1604396776117));
#190606=CARTESIAN_POINT('Origin',(116.959178380441,-7.8,51.0204257716897));
#190607=CARTESIAN_POINT('',(114.542656660719,-7.8,64.5004538237752));
#190608=CARTESIAN_POINT('',(114.608749045379,-7.8,64.1604396776117));
#190609=CARTESIAN_POINT('Origin',(116.959178380441,-7.8,51.0204257716897));
#190610=CARTESIAN_POINT('Origin',(115.211503291295,-7.8,63.6799623070345));
#190611=CARTESIAN_POINT('',(115.04930756357,-7.3,64.5143828254856));
#190612=CARTESIAN_POINT('',(114.984462690182,-7.3,64.8479791145506));
#190613=CARTESIAN_POINT('',(115.04930756357,-7.3,64.5143828254856));
#190614=CARTESIAN_POINT('Origin',(117.64631728401,1.45439216225896E-14,
51.1539927107186));
#190615=CARTESIAN_POINT('Origin',(117.64631728401,1.45439216225896E-14,
51.1539927107186));
#190616=CARTESIAN_POINT('Origin',(115.211503291295,-7.3,63.6799623070345));
#190617=CARTESIAN_POINT('',(114.555341617604,-7.3,64.4351957035434));
#190618=CARTESIAN_POINT('',(114.490573450483,-7.3,64.7683973750478));
#190619=CARTESIAN_POINT('',(114.555341617604,-7.3,64.4351957035434));
#190620=CARTESIAN_POINT('Origin',(116.959178380441,-7.3,51.0204257716897));
#190621=CARTESIAN_POINT('Origin',(116.959178380441,-7.3,51.0204257716897));
#190622=CARTESIAN_POINT('Origin',(114.720689788746,-7.3,63.5845573505853));
#190623=CARTESIAN_POINT('Origin',(117.155503781461,1.45439216225896E-14,
51.0585877542694));
#190624=CARTESIAN_POINT('Origin',(117.155503781461,1.45439216225896E-14,
51.0585877542694));
#190625=CARTESIAN_POINT('Origin',(113.739062783647,-7.8,63.3937474376868));
#190626=CARTESIAN_POINT('',(114.118292968078,-7.8,64.0631959368381));
#190627=CARTESIAN_POINT('',(114.052191541068,-7.8,64.403256601628));
#190628=CARTESIAN_POINT('',(114.118292968078,-7.8,64.0631959368381));
#190629=CARTESIAN_POINT('',(113.631414459623,-7.8,63.9475472917409));
#190630=CARTESIAN_POINT('Origin',(116.959178380441,-7.8,51.0204257716897));
#190631=CARTESIAN_POINT('',(113.565213321132,-7.8,64.2881209250702));
#190632=CARTESIAN_POINT('',(113.631414459623,-7.8,63.9475472917409));
#190633=CARTESIAN_POINT('Origin',(116.959178380441,-7.8,51.0204257716897));
#190634=CARTESIAN_POINT('Origin',(114.229876286196,-7.8,63.489152394136));
#190635=CARTESIAN_POINT('',(114.064878197778,-7.3,64.3379897366015));
#190636=CARTESIAN_POINT('',(114.000101521181,-7.3,64.6712351853426));
#190637=CARTESIAN_POINT('',(114.064878197778,-7.3,64.3379897366015));
#190638=CARTESIAN_POINT('Origin',(116.664690278911,1.45439216225896E-14,
50.9631827978201));
#190639=CARTESIAN_POINT('Origin',(116.664690278911,1.45439216225896E-14,
50.9631827978201));
#190640=CARTESIAN_POINT('Origin',(114.229876286196,-7.3,63.489152394136));
#190641=CARTESIAN_POINT('',(113.577918721109,-7.3,64.2227576347738));
#190642=CARTESIAN_POINT('',(113.513048218327,-7.3,64.5564857749867));
#190643=CARTESIAN_POINT('',(113.577918721109,-7.3,64.2227576347738));
#190644=CARTESIAN_POINT('Origin',(116.959178380441,-7.3,51.0204257716897));
#190645=CARTESIAN_POINT('Origin',(116.959178380441,-7.3,51.0204257716897));
#190646=CARTESIAN_POINT('Origin',(113.739062783647,-7.3,63.3937474376868));
#190647=CARTESIAN_POINT('Origin',(116.173876776362,1.45439216225896E-14,
50.8677778413709));
#190648=CARTESIAN_POINT('Origin',(116.173876776362,1.45439216225896E-14,
50.8677778413709));
#190649=CARTESIAN_POINT('Origin',(112.757435778548,-7.8,63.2029375247883));
#190650=CARTESIAN_POINT('',(113.148130180408,-7.8,63.8134080324416));
#190651=CARTESIAN_POINT('',(113.081737423663,-7.8,64.1549674513112));
#190652=CARTESIAN_POINT('',(113.148130180408,-7.8,63.8134080324416));
#190653=CARTESIAN_POINT('',(112.668472298385,-7.8,63.6606126700068));
#190654=CARTESIAN_POINT('Origin',(116.959178380441,-7.8,51.0204257716897));
#190655=CARTESIAN_POINT('',(112.601793610039,-7.8,64.0036430720998));
#190656=CARTESIAN_POINT('',(112.668472298385,-7.8,63.6606126700068));
#190657=CARTESIAN_POINT('Origin',(116.959178380441,-7.8,51.0204257716897));
#190658=CARTESIAN_POINT('Origin',(113.248249281097,-7.8,63.2983424812375));
#190659=CARTESIAN_POINT('',(113.094478838136,-7.3,64.0894188834233));
#190660=CARTESIAN_POINT('',(113.02942807446,-7.3,64.4240743809113));
#190661=CARTESIAN_POINT('',(113.094478838136,-7.3,64.0894188834233));
#190662=CARTESIAN_POINT('Origin',(115.683063273812,1.45439216225896E-14,
50.7723728849216));
#190663=CARTESIAN_POINT('Origin',(115.683063273812,1.45439216225896E-14,
50.7723728849216));
#190664=CARTESIAN_POINT('Origin',(113.248249281097,-7.3,63.2983424812375));
#190665=CARTESIAN_POINT('',(112.614588752975,-7.3,63.9378180966099));
#190666=CARTESIAN_POINT('',(112.54926912135,-7.3,64.2738567928821));
#190667=CARTESIAN_POINT('',(112.614588752975,-7.3,63.9378180966099));
#190668=CARTESIAN_POINT('Origin',(116.959178380441,-7.3,51.0204257716897));
#190669=CARTESIAN_POINT('Origin',(116.959178380441,-7.3,51.0204257716897));
#190670=CARTESIAN_POINT('Origin',(112.757435778548,-7.3,63.2029375247883));
#190671=CARTESIAN_POINT('Origin',(115.192249771263,1.45439216225896E-14,
50.6769679284724));
#190672=CARTESIAN_POINT('Origin',(115.192249771263,1.45439216225896E-14,
50.6769679284724));
#190673=CARTESIAN_POINT('Origin',(111.775808773449,-7.8,63.0121276118898));
#190674=CARTESIAN_POINT('',(112.192489185624,-7.8,63.4889123529498));
#190675=CARTESIAN_POINT('',(112.125426591645,-7.8,63.8339177684538));
#190676=CARTESIAN_POINT('',(112.192489185624,-7.8,63.4889123529498));
#190677=CARTESIAN_POINT('',(111.720246491895,-7.8,63.2979693441656));
#190678=CARTESIAN_POINT('Origin',(116.959178380441,-7.8,51.0204257716897));
#190679=CARTESIAN_POINT('',(111.652696970122,-7.8,63.6454797735061));
#190680=CARTESIAN_POINT('',(111.720246491895,-7.8,63.2979693441656));
#190681=CARTESIAN_POINT('Origin',(116.959178380441,-7.8,51.0204257716897));
#190682=CARTESIAN_POINT('Origin',(112.266622275998,-7.8,63.107532568339));
#190683=CARTESIAN_POINT('',(112.138293850054,-7.3,63.7677217928681));
#190684=CARTESIAN_POINT('',(112.072613443008,-7.3,64.1056165085183));
#190685=CARTESIAN_POINT('',(112.138293850054,-7.3,63.7677217928681));
#190686=CARTESIAN_POINT('Origin',(114.701436268713,1.45439216225896E-14,
50.5815629720231));
#190687=CARTESIAN_POINT('Origin',(114.701436268713,1.45439216225896E-14,
50.5815629720231));
#190688=CARTESIAN_POINT('Origin',(112.266622275998,-7.3,63.107532568339));
#190689=CARTESIAN_POINT('',(111.665655658314,-7.3,63.5788134348104));
#190690=CARTESIAN_POINT('',(111.599518024745,-7.3,63.9190603652681));
#190691=CARTESIAN_POINT('',(111.665655658314,-7.3,63.5788134348104));
#190692=CARTESIAN_POINT('Origin',(116.959178380441,-7.3,51.0204257716897));
#190693=CARTESIAN_POINT('Origin',(116.959178380441,-7.3,51.0204257716897));
#190694=CARTESIAN_POINT('Origin',(111.775808773449,-7.3,63.0121276118898));
#190695=CARTESIAN_POINT('Origin',(114.210622766164,1.45439216225896E-14,
50.4861580155739));
#190696=CARTESIAN_POINT('Origin',(114.210622766164,1.45439216225896E-14,
50.4861580155739));
#190697=CARTESIAN_POINT('Origin',(110.79418176835,-7.8,62.8213176989913));
#190698=CARTESIAN_POINT('',(111.25182865232,-7.8,63.0873492647716));
#190699=CARTESIAN_POINT('',(111.18368255378,-7.8,63.4379288002016));
#190700=CARTESIAN_POINT('',(111.25182865232,-7.8,63.0873492647716));
#190701=CARTESIAN_POINT('',(110.787340913104,-7.8,62.8565106726941));
#190702=CARTESIAN_POINT('Origin',(116.959178380441,-7.8,51.0204257716897));
#190703=CARTESIAN_POINT('',(110.718480119372,-7.8,63.2107669777972));
#190704=CARTESIAN_POINT('',(110.787340913104,-7.8,62.8565106726941));
#190705=CARTESIAN_POINT('Origin',(116.959178380441,-7.8,51.0204257716897));
#190706=CARTESIAN_POINT('Origin',(111.284995270899,-7.8,62.9167226554405));
#190707=CARTESIAN_POINT('',(111.196753201947,-7.3,63.3706864802381));
#190708=CARTESIAN_POINT('',(111.130055939274,-7.3,63.7138124384881));
#190709=CARTESIAN_POINT('',(111.196753201947,-7.3,63.3706864802381));
#190710=CARTESIAN_POINT('Origin',(113.719809263614,1.45439216225896E-14,
50.3907530591246));
#190711=CARTESIAN_POINT('Origin',(113.719809263614,1.45439216225896E-14,
50.3907530591246));
#190712=CARTESIAN_POINT('Origin',(111.284995270899,-7.3,62.9167226554405));
#190713=CARTESIAN_POINT('',(110.731684809429,-7.3,63.142835075533));
#190714=CARTESIAN_POINT('',(110.664317929489,-7.3,63.4894058987878));
#190715=CARTESIAN_POINT('',(110.731684809429,-7.3,63.142835075533));
#190716=CARTESIAN_POINT('Origin',(116.959178380441,-7.3,51.0204257716897));
#190717=CARTESIAN_POINT('Origin',(116.959178380441,-7.3,51.0204257716897));
#190718=CARTESIAN_POINT('Origin',(110.79418176835,-7.3,62.8213176989913));
#190719=CARTESIAN_POINT('Origin',(113.228995761065,1.45439216225896E-14,
50.2953481026754));
#190720=CARTESIAN_POINT('Origin',(113.228995761065,1.45439216225896E-14,
50.2953481026754));
#190721=CARTESIAN_POINT('Origin',(110.3033682658,-7.3,62.725912742542));
#190722=CARTESIAN_POINT('',(109.812554763251,-7.3,62.6305077860928));
#190723=CARTESIAN_POINT('',(109.744478438118,-7.3,62.9807283702507));
#190724=CARTESIAN_POINT('',(109.812554763251,-7.3,62.6305077860928));
#190725=CARTESIAN_POINT('',(109.82625098298,-7.3,62.6331700748033));
#190726=CARTESIAN_POINT('',(109.82625098298,-7.3,62.6331700748033));
#190727=CARTESIAN_POINT('',(110.270570482611,-7.3,62.8946418677557));
#190728=CARTESIAN_POINT('Origin',(116.959178380441,-7.3,51.0204257716897));
#190729=CARTESIAN_POINT('',(110.202414471986,-7.3,63.2452723961858));
#190730=CARTESIAN_POINT('',(110.270570482611,-7.3,62.8946418677557));
#190731=CARTESIAN_POINT('Origin',(116.959178380441,-7.3,51.0204257716897));
#190732=CARTESIAN_POINT('Origin',(109.812554763251,-7.3,62.6305077860928));
#190733=CARTESIAN_POINT('',(109.812554763251,-7.8,62.6305077860928));
#190734=CARTESIAN_POINT('',(109.800007656622,-7.8,62.6950567317697));
#190735=CARTESIAN_POINT('',(109.812554763251,-7.8,62.6305077860928));
#190736=CARTESIAN_POINT('',(109.812554763251,-7.3,62.6305077860928));
#190737=CARTESIAN_POINT('Origin',(112.247368755966,1.45439216225896E-14,
50.1045381897769));
#190738=CARTESIAN_POINT('Origin',(109.812554763251,-7.8,62.6305077860928));
#190739=CARTESIAN_POINT('',(110.3033682658,-7.8,62.725912742542));
#190740=CARTESIAN_POINT('',(110.257207717211,-7.8,62.9633869931011));
#190741=CARTESIAN_POINT('',(110.3033682658,-7.8,62.725912742542));
#190742=CARTESIAN_POINT('',(109.812554763251,-7.8,62.6305077860928));
#190743=CARTESIAN_POINT('Origin',(116.959178380441,-7.8,51.0204257716897));
#190744=CARTESIAN_POINT('Origin',(110.3033682658,-7.8,62.725912742542));
#190745=CARTESIAN_POINT('',(110.3033682658,-7.59646299273499,62.725912742542));
#190746=CARTESIAN_POINT('Origin',(112.738182258515,1.45439216225896E-14,
50.1999431462261));
#190747=CARTESIAN_POINT('',(110.3033682658,-7.8,62.725912742542));
#190748=CARTESIAN_POINT('Origin',(112.738182258515,1.45439216225896E-14,
50.1999431462261));
#190749=CARTESIAN_POINT('Origin',(109.616229362231,-8.,62.5923458035131));
#190750=CARTESIAN_POINT('Origin',(114.524364387726,1.45439216225896E-14,
63.5463953680056));
#190751=CARTESIAN_POINT('Origin',(107.358487250503,-4.3,62.1534830038465));
#190752=CARTESIAN_POINT('',(106.867673747954,-4.3,62.0580780473973));
#190753=CARTESIAN_POINT('',(106.821513199365,-4.3,62.2955522979563));
#190754=CARTESIAN_POINT('',(106.867673747954,-4.3,62.0580780473973));
#190755=CARTESIAN_POINT('',(107.067471170822,-4.3,62.0969149260251));
#190756=CARTESIAN_POINT('',(107.067471170822,-4.3,62.0969149260251));
#190757=CARTESIAN_POINT('',(107.325689467314,-4.3,62.3222121290602));
#190758=CARTESIAN_POINT('Origin',(116.959178380441,-4.3,51.0204257716897));
#190759=CARTESIAN_POINT('',(107.257533456689,-4.3,62.6728426574903));
#190760=CARTESIAN_POINT('',(107.325689467314,-4.3,62.3222121290602));
#190761=CARTESIAN_POINT('Origin',(116.959178380441,-4.3,51.0204257716897));
#190762=CARTESIAN_POINT('Origin',(106.867673747954,-4.3,62.0580780473973));
#190763=CARTESIAN_POINT('',(106.867673747954,-4.8,62.0580780473973));
#190764=CARTESIAN_POINT('',(106.855126641325,-4.8,62.1226269930741));
#190765=CARTESIAN_POINT('',(106.867673747954,-4.8,62.0580780473973));
#190766=CARTESIAN_POINT('',(106.867673747954,-4.3,62.0580780473973));
#190767=CARTESIAN_POINT('Origin',(109.302487740669,1.45439216225896E-14,
49.5321084510813));
#190768=CARTESIAN_POINT('Origin',(106.867673747954,-4.8,62.0580780473973));
#190769=CARTESIAN_POINT('',(107.358487250503,-4.8,62.1534830038465));
#190770=CARTESIAN_POINT('',(107.29041092537,-4.8,62.5037035880044));
#190771=CARTESIAN_POINT('',(107.358487250503,-4.8,62.1534830038465));
#190772=CARTESIAN_POINT('',(106.867673747954,-4.8,62.0580780473973));
#190773=CARTESIAN_POINT('Origin',(116.959178380441,-4.8,51.0204257716897));
#190774=CARTESIAN_POINT('Origin',(107.358487250503,-4.8,62.1534830038465));
#190775=CARTESIAN_POINT('',(107.358487250503,-4.78604742976898,62.1534830038465));
#190776=CARTESIAN_POINT('Origin',(109.793301243218,1.45439216225896E-14,
49.6275134075306));
#190777=CARTESIAN_POINT('',(107.358487250503,-4.8,62.1534830038465));
#190778=CARTESIAN_POINT('Origin',(109.793301243218,1.45439216225896E-14,
49.6275134075306));
#190779=CARTESIAN_POINT('Origin',(106.671348346934,-5.,62.0199160648176));
#190780=CARTESIAN_POINT('Origin',(114.524364387726,1.45439216225896E-14,
63.5463953680056));
#190781=CARTESIAN_POINT('Origin',(107.358487250503,-3.8,62.1534830038465));
#190782=CARTESIAN_POINT('',(107.270245181551,-3.3,62.6074468286441));
#190783=CARTESIAN_POINT('',(107.203547918878,-3.3,62.9505727868941));
#190784=CARTESIAN_POINT('',(107.270245181551,-3.3,62.6074468286441));
#190785=CARTESIAN_POINT('',(107.295990291582,-3.8,62.4750003803882));
#190786=CARTESIAN_POINT('Origin',(109.793301243218,1.45439216225896E-14,
49.6275134075306));
#190787=CARTESIAN_POINT('',(107.228623411642,-3.8,62.8215712036431));
#190788=CARTESIAN_POINT('',(107.295990291582,-3.8,62.4750003803882));
#190789=CARTESIAN_POINT('Origin',(109.793301243218,1.45439216225896E-14,
49.6275134075306));
#190790=CARTESIAN_POINT('Origin',(107.358487250503,-3.3,62.1534830038465));
#190791=CARTESIAN_POINT('',(106.834507129375,-3.3,62.2287046567283));
#190792=CARTESIAN_POINT('',(106.766361030834,-3.3,62.5792841921583));
#190793=CARTESIAN_POINT('',(106.834507129375,-3.3,62.2287046567283));
#190794=CARTESIAN_POINT('Origin',(116.959178380441,-3.3,51.0204257716897));
#190795=CARTESIAN_POINT('Origin',(116.959178380441,-3.3,51.0204257716897));
#190796=CARTESIAN_POINT('Origin',(106.867673747954,-3.3,62.0580780473973));
#190797=CARTESIAN_POINT('',(106.860832892708,-3.8,62.0932710211001));
#190798=CARTESIAN_POINT('',(106.791972098975,-3.8,62.4475273262032));
#190799=CARTESIAN_POINT('',(106.860832892708,-3.8,62.0932710211001));
#190800=CARTESIAN_POINT('Origin',(109.302487740669,1.45439216225896E-14,
49.5321084510813));
#190801=CARTESIAN_POINT('Origin',(109.302487740669,1.45439216225896E-14,
49.5321084510813));
#190802=CARTESIAN_POINT('Origin',(106.867673747954,-3.8,62.0580780473973));
#190803=CARTESIAN_POINT('Origin',(116.959178380441,-3.8,51.0204257716897));
#190804=CARTESIAN_POINT('Origin',(116.959178380441,-3.8,51.0204257716897));
#190805=CARTESIAN_POINT('Origin',(106.867673747954,-2.8,62.0580780473973));
#190806=CARTESIAN_POINT('',(107.248334135368,-2.8,62.7201688267671));
#190807=CARTESIAN_POINT('',(107.182196501799,-2.8,63.0604157572248));
#190808=CARTESIAN_POINT('',(107.248334135368,-2.8,62.7201688267671));
#190809=CARTESIAN_POINT('',(106.8121114664,-2.8,62.3439197796731));
#190810=CARTESIAN_POINT('Origin',(116.959178380441,-2.8,51.0204257716897));
#190811=CARTESIAN_POINT('',(106.744561944627,-2.8,62.6914302090136));
#190812=CARTESIAN_POINT('',(106.8121114664,-2.8,62.3439197796731));
#190813=CARTESIAN_POINT('Origin',(116.959178380441,-2.8,51.0204257716897));
#190814=CARTESIAN_POINT('Origin',(107.358487250503,-2.8,62.1534830038465));
#190815=CARTESIAN_POINT('',(107.230158824559,-2.3,62.8136722283756));
#190816=CARTESIAN_POINT('',(107.164478417513,-2.3,63.1515669440258));
#190817=CARTESIAN_POINT('',(107.230158824559,-2.3,62.8136722283756));
#190818=CARTESIAN_POINT('Origin',(109.793301243218,1.45439216225896E-14,
49.6275134075306));
#190819=CARTESIAN_POINT('Origin',(109.793301243218,1.45439216225896E-14,
49.6275134075306));
#190820=CARTESIAN_POINT('Origin',(107.358487250503,-2.3,62.1534830038465));
#190821=CARTESIAN_POINT('',(106.793540657579,-2.3,62.439457832008));
#190822=CARTESIAN_POINT('',(106.7264780636,-2.3,62.784463247512));
#190823=CARTESIAN_POINT('',(106.793540657579,-2.3,62.439457832008));
#190824=CARTESIAN_POINT('Origin',(116.959178380441,-2.3,51.0204257716897));
#190825=CARTESIAN_POINT('Origin',(116.959178380441,-2.3,51.0204257716897));
#190826=CARTESIAN_POINT('Origin',(106.867673747954,-2.3,62.0580780473973));
#190827=CARTESIAN_POINT('Origin',(109.302487740669,1.45439216225896E-14,
49.5321084510813));
#190828=CARTESIAN_POINT('Origin',(109.302487740669,1.45439216225896E-14,
49.5321084510813));
#190829=CARTESIAN_POINT('Origin',(106.867673747954,-1.8,62.0580780473973));
#190830=CARTESIAN_POINT('',(107.21564022493,-1.8,62.8883635756681));
#190831=CARTESIAN_POINT('',(107.150320593305,-1.8,63.2244022719403));
#190832=CARTESIAN_POINT('',(107.21564022493,-1.8,62.8883635756681));
#190833=CARTESIAN_POINT('',(106.778710267791,-1.8,62.5157531926157));
#190834=CARTESIAN_POINT('Origin',(116.959178380441,-1.8,51.0204257716897));
#190835=CARTESIAN_POINT('',(106.712031579445,-1.8,62.8587835947088));
#190836=CARTESIAN_POINT('',(106.778710267791,-1.8,62.5157531926157));
#190837=CARTESIAN_POINT('Origin',(116.959178380441,-1.8,51.0204257716897));
#190838=CARTESIAN_POINT('Origin',(107.358487250503,-1.8,62.1534830038465));
#190839=CARTESIAN_POINT('',(107.204716807541,-1.3,62.9445594060323));
#190840=CARTESIAN_POINT('',(107.139666043865,-1.3,63.2792149035202));
#190841=CARTESIAN_POINT('',(107.204716807541,-1.3,62.9445594060323));
#190842=CARTESIAN_POINT('Origin',(109.793301243218,1.45439216225896E-14,
49.6275134075306));
#190843=CARTESIAN_POINT('Origin',(109.793301243218,1.45439216225896E-14,
49.6275134075306));
#190844=CARTESIAN_POINT('Origin',(107.358487250503,-1.3,62.1534830038465));
#190845=CARTESIAN_POINT('',(106.767554647265,-1.3,62.5731435986013));
#190846=CARTESIAN_POINT('',(106.701161890519,-1.3,62.9147030174709));
#190847=CARTESIAN_POINT('',(106.767554647265,-1.3,62.5731435986013));
#190848=CARTESIAN_POINT('Origin',(116.959178380441,-1.3,51.0204257716897));
#190849=CARTESIAN_POINT('Origin',(116.959178380441,-1.3,51.0204257716897));
#190850=CARTESIAN_POINT('Origin',(106.867673747954,-1.3,62.0580780473973));
#190851=CARTESIAN_POINT('Origin',(109.302487740669,1.45439216225896E-14,
49.5321084510813));
#190852=CARTESIAN_POINT('Origin',(109.302487740669,1.45439216225896E-14,
49.5321084510813));
#190853=CARTESIAN_POINT('Origin',(106.867673747954,-0.799999999999986,62.0580780473973));
#190854=CARTESIAN_POINT('',(107.197343187966,-0.799999999999986,62.9824932009336));
#190855=CARTESIAN_POINT('',(107.132472685183,-0.799999999999986,63.3162213411464));
#190856=CARTESIAN_POINT('',(107.197343187966,-0.799999999999986,62.9824932009336));
#190857=CARTESIAN_POINT('',(106.76002542393,-0.799999999999986,62.6118779014513));
#190858=CARTESIAN_POINT('Origin',(116.959178380441,-0.799999999999986,51.0204257716897));
#190859=CARTESIAN_POINT('',(106.693824285439,-0.799999999999986,62.9524515347807));
#190860=CARTESIAN_POINT('',(106.76002542393,-0.799999999999986,62.6118779014513));
#190861=CARTESIAN_POINT('Origin',(116.959178380441,-0.799999999999986,51.0204257716897));
#190862=CARTESIAN_POINT('Origin',(107.358487250503,-0.799999999999986,62.1534830038465));
#190863=CARTESIAN_POINT('',(107.193489162085,-0.299999999999985,63.0023203463119));
#190864=CARTESIAN_POINT('',(107.128712485488,-0.299999999999985,63.3355657950531));
#190865=CARTESIAN_POINT('',(107.193489162085,-0.299999999999985,63.0023203463119));
#190866=CARTESIAN_POINT('Origin',(109.793301243218,1.45439216225896E-14,
49.6275134075306));
#190867=CARTESIAN_POINT('Origin',(109.793301243218,1.45439216225896E-14,
49.6275134075306));
#190868=CARTESIAN_POINT('Origin',(107.358487250503,-0.299999999999985,62.1534830038465));
#190869=CARTESIAN_POINT('',(106.756090429836,-0.299999999999985,62.6321215900993));
#190870=CARTESIAN_POINT('',(106.689989002826,-0.299999999999985,62.9721822548892));
#190871=CARTESIAN_POINT('',(106.756090429836,-0.299999999999985,62.6321215900993));
#190872=CARTESIAN_POINT('Origin',(116.959178380441,-0.299999999999985,51.0204257716897));
#190873=CARTESIAN_POINT('Origin',(116.959178380441,-0.299999999999985,51.0204257716897));
#190874=CARTESIAN_POINT('Origin',(106.867673747954,-0.299999999999985,62.0580780473973));
#190875=CARTESIAN_POINT('Origin',(109.302487740669,1.45439216225896E-14,
49.5321084510813));
#190876=CARTESIAN_POINT('Origin',(109.302487740669,1.45439216225896E-14,
49.5321084510813));
#190877=CARTESIAN_POINT('Origin',(123.064519332087,-0.299999999999985,65.2064416102226));
#190878=CARTESIAN_POINT('',(122.508294760723,-0.299999999999985,65.4475457512624));
#190879=CARTESIAN_POINT('',(122.441004340522,-0.299999999999985,65.7937232252189));
#190880=CARTESIAN_POINT('',(122.508294760723,-0.299999999999985,65.4475457512624));
#190881=CARTESIAN_POINT('',(123.061409169883,-0.299999999999985,65.2224419278371));
#190882=CARTESIAN_POINT('Origin',(116.959178380441,-0.299999999999985,51.0204257716897));
#190883=CARTESIAN_POINT('',(122.992445896985,-0.299999999999985,65.5772254399106));
#190884=CARTESIAN_POINT('',(123.061409169883,-0.299999999999985,65.2224419278371));
#190885=CARTESIAN_POINT('Origin',(116.959178380441,-0.299999999999985,51.0204257716897));
#190886=CARTESIAN_POINT('Origin',(122.573705829538,-0.299999999999985,65.1110366537733));
#190887=CARTESIAN_POINT('',(122.512302538895,-0.799999999999986,65.4269276228584));
#190888=CARTESIAN_POINT('',(122.444906919269,-0.799999999999986,65.7736462982427));
#190889=CARTESIAN_POINT('',(122.512302538895,-0.799999999999986,65.4269276228584));
#190890=CARTESIAN_POINT('Origin',(125.008519822253,1.45439216225896E-14,
52.5850670574574));
#190891=CARTESIAN_POINT('Origin',(125.008519822253,1.45439216225896E-14,
52.5850670574574));
#190892=CARTESIAN_POINT('Origin',(122.573705829538,-0.799999999999986,65.1110366537733));
#190893=CARTESIAN_POINT('',(123.064519332087,-0.799999999999986,65.2064416102226));
#190894=CARTESIAN_POINT('',(122.996443006954,-0.799999999999986,65.5566621943805));
#190895=CARTESIAN_POINT('',(123.064519332087,-0.799999999999986,65.2064416102226));
#190896=CARTESIAN_POINT('',(123.056970443337,-0.799999999999986,65.2049742475712));
#190897=CARTESIAN_POINT('',(123.056970443337,-0.799999999999986,65.2049742475712));
#190898=CARTESIAN_POINT('Origin',(116.959178380441,-0.799999999999986,51.0204257716897));
#190899=CARTESIAN_POINT('Origin',(116.959178380441,-0.799999999999986,51.0204257716897));
#190900=CARTESIAN_POINT('Origin',(123.064519332087,-0.799999999999986,65.2064416102226));
#190901=CARTESIAN_POINT('',(123.064519332087,-0.711512473537285,65.2064416102226));
#190902=CARTESIAN_POINT('Origin',(125.499333324803,1.45439216225896E-14,
52.6804720139067));
#190903=CARTESIAN_POINT('',(123.064519332087,-0.799999999999986,65.2064416102226));
#190904=CARTESIAN_POINT('Origin',(125.499333324803,1.45439216225896E-14,
52.6804720139067));
#190905=CARTESIAN_POINT('Origin',(122.377380428518,-0.999999999999985,65.0728746711936));
#190906=CARTESIAN_POINT('Origin',(114.524364387726,1.45439216225896E-14,
63.5463953680056));
#190907=CARTESIAN_POINT('Origin',(122.573705829538,-1.3,65.1110366537733));
#190908=CARTESIAN_POINT('',(122.531336174176,-1.8,65.3290085466811));
#190909=CARTESIAN_POINT('',(122.463436480413,-1.8,65.6783204457488));
#190910=CARTESIAN_POINT('',(122.531336174176,-1.8,65.3290085466811));
#190911=CARTESIAN_POINT('',(122.519971674893,-1.3,65.3874735353515));
#190912=CARTESIAN_POINT('Origin',(125.008519822253,1.45439216225896E-14,
52.5850670574574));
#190913=CARTESIAN_POINT('',(122.452373842004,-1.3,65.7352325025978));
#190914=CARTESIAN_POINT('',(122.519971674893,-1.3,65.3874735353515));
#190915=CARTESIAN_POINT('Origin',(125.008519822253,1.45439216225896E-14,
52.5850670574574));
#190916=CARTESIAN_POINT('Origin',(122.573705829538,-1.8,65.1110366537733));
#190917=CARTESIAN_POINT('',(123.064519332087,-1.8,65.2064416102226));
#190918=CARTESIAN_POINT('',(123.015425507724,-1.8,65.4590061811456));
#190919=CARTESIAN_POINT('',(123.064519332087,-1.8,65.2064416102226));
#190920=CARTESIAN_POINT('',(122.908875583955,-1.8,65.1761873793691));
#190921=CARTESIAN_POINT('',(122.908875583955,-1.8,65.1761873793691));
#190922=CARTESIAN_POINT('Origin',(116.959178380441,-1.8,51.0204257716897));
#190923=CARTESIAN_POINT('Origin',(116.959178380441,-1.8,51.0204257716897));
#190924=CARTESIAN_POINT('Origin',(123.064519332087,-1.8,65.2064416102226));
#190925=CARTESIAN_POINT('',(123.064519332087,-1.3,65.2064416102226));
#190926=CARTESIAN_POINT('',(123.004091633267,-1.3,65.5173136195258));
#190927=CARTESIAN_POINT('',(123.064519332087,-1.3,65.2064416102226));
#190928=CARTESIAN_POINT('',(123.064519332087,-1.8,65.2064416102226));
#190929=CARTESIAN_POINT('Origin',(125.499333324803,1.45439216225896E-14,
52.6804720139067));
#190930=CARTESIAN_POINT('Origin',(123.064519332087,-1.3,65.2064416102226));
#190931=CARTESIAN_POINT('',(122.997474498203,-1.3,65.1934093496517));
#190932=CARTESIAN_POINT('Origin',(116.959178380441,-1.3,51.0204257716897));
#190933=CARTESIAN_POINT('',(123.064519332087,-1.3,65.2064416102226));
#190934=CARTESIAN_POINT('Origin',(116.959178380441,-1.3,51.0204257716897));
#190935=CARTESIAN_POINT('Origin',(122.377380428518,-2.,65.0728746711936));
#190936=CARTESIAN_POINT('Origin',(114.524364387726,1.45439216225896E-14,
63.5463953680056));
#190937=CARTESIAN_POINT('Origin',(122.573705829538,-2.3,65.1110366537733));
#190938=CARTESIAN_POINT('',(122.565374292175,-2.8,65.1538984838808));
#190939=CARTESIAN_POINT('',(122.496554362349,-2.8,65.5079445634598));
#190940=CARTESIAN_POINT('',(122.565374292175,-2.8,65.1538984838808));
#190941=CARTESIAN_POINT('',(122.54644720768,-2.3,65.2512694065221));
#190942=CARTESIAN_POINT('Origin',(125.008519822253,1.45439216225896E-14,
52.5850670574574));
#190943=CARTESIAN_POINT('',(122.478141994724,-2.3,65.6026675105714));
#190944=CARTESIAN_POINT('',(122.54644720768,-2.3,65.2512694065221));
#190945=CARTESIAN_POINT('Origin',(125.008519822253,1.45439216225896E-14,
52.5850670574574));
#190946=CARTESIAN_POINT('Origin',(122.573705829538,-2.8,65.1110366537733));
#190947=CARTESIAN_POINT('',(123.064519332087,-2.8,65.2064416102226));
#190948=CARTESIAN_POINT('',(123.04937020292,-2.8,65.2843767345985));
#190949=CARTESIAN_POINT('',(123.064519332087,-2.8,65.2064416102226));
#190950=CARTESIAN_POINT('',(122.640244299654,-2.8,65.1239704867072));
#190951=CARTESIAN_POINT('',(122.640244299654,-2.8,65.1239704867072));
#190952=CARTESIAN_POINT('Origin',(116.959178380441,-2.8,51.0204257716897));
#190953=CARTESIAN_POINT('Origin',(116.959178380441,-2.8,51.0204257716897));
#190954=CARTESIAN_POINT('Origin',(123.064519332087,-2.8,65.2064416102226));
#190955=CARTESIAN_POINT('',(123.064519332087,-2.3,65.2064416102226));
#190956=CARTESIAN_POINT('',(123.030495384216,-2.3,65.3814787743977));
#190957=CARTESIAN_POINT('',(123.064519332087,-2.3,65.2064416102226));
#190958=CARTESIAN_POINT('',(123.064519332087,-2.8,65.2064416102226));
#190959=CARTESIAN_POINT('Origin',(125.499333324803,1.45439216225896E-14,
52.6804720139067));
#190960=CARTESIAN_POINT('Origin',(123.064519332087,-2.3,65.2064416102226));
#190961=CARTESIAN_POINT('',(122.790237920908,-2.3,65.1531264386707));
#190962=CARTESIAN_POINT('Origin',(116.959178380441,-2.3,51.0204257716897));
#190963=CARTESIAN_POINT('',(123.064519332087,-2.3,65.2064416102226));
#190964=CARTESIAN_POINT('Origin',(116.959178380441,-2.3,51.0204257716897));
#190965=CARTESIAN_POINT('Origin',(122.377380428518,-3.,65.0728746711936));
#190966=CARTESIAN_POINT('Origin',(114.524364387726,1.45439216225896E-14,
63.5463953680056));
#190967=CARTESIAN_POINT('Origin',(120.11963831679,-6.3,64.6340118715271));
#190968=CARTESIAN_POINT('',(119.55904893793,-6.3,64.8975708884388));
#190969=CARTESIAN_POINT('',(119.491872720657,-6.3,65.2431608422003));
#190970=CARTESIAN_POINT('',(119.55904893793,-6.3,64.8975708884388));
#190971=CARTESIAN_POINT('',(120.089793203781,-6.3,64.7875509013147));
#190972=CARTESIAN_POINT('Origin',(116.959178380441,-6.3,51.0204257716897));
#190973=CARTESIAN_POINT('',(120.021557740431,-6.3,65.13859017654));
#190974=CARTESIAN_POINT('',(120.089793203781,-6.3,64.7875509013147));
#190975=CARTESIAN_POINT('Origin',(116.959178380441,-6.3,51.0204257716897));
#190976=CARTESIAN_POINT('Origin',(119.628824814241,-6.3,64.5386069150778));
#190977=CARTESIAN_POINT('',(119.607117843827,-6.8,64.6502790396187));
#190978=CARTESIAN_POINT('',(119.538662444116,-6.8,65.0024497836874));
#190979=CARTESIAN_POINT('',(119.607117843827,-6.8,64.6502790396187));
#190980=CARTESIAN_POINT('Origin',(122.063638806956,1.45439216225896E-14,
52.0126373187619));
#190981=CARTESIAN_POINT('Origin',(122.063638806956,1.45439216225896E-14,
52.0126373187619));
#190982=CARTESIAN_POINT('Origin',(119.628824814241,-6.8,64.5386069150778));
#190983=CARTESIAN_POINT('',(120.11963831679,-6.8,64.6340118715271));
#190984=CARTESIAN_POINT('',(120.06907915275,-6.8,64.8941149239462));
#190985=CARTESIAN_POINT('',(120.11963831679,-6.8,64.6340118715271));
#190986=CARTESIAN_POINT('',(119.897035062789,-6.8,64.5907419662716));
#190987=CARTESIAN_POINT('',(119.897035062789,-6.8,64.5907419662716));
#190988=CARTESIAN_POINT('Origin',(116.959178380441,-6.8,51.0204257716897));
#190989=CARTESIAN_POINT('Origin',(116.959178380441,-6.8,51.0204257716897));
#190990=CARTESIAN_POINT('Origin',(120.11963831679,-6.8,64.6340118715271));
#190991=CARTESIAN_POINT('',(120.11963831679,-6.61107026131199,64.6340118715271));
#190992=CARTESIAN_POINT('Origin',(122.554452309506,1.45439216225896E-14,
52.1080422752111));
#190993=CARTESIAN_POINT('',(120.11963831679,-6.8,64.6340118715271));
#190994=CARTESIAN_POINT('Origin',(122.554452309506,1.45439216225896E-14,
52.1080422752111));
#190995=CARTESIAN_POINT('Origin',(119.432499413221,-7.,64.5004449324981));
#190996=CARTESIAN_POINT('Origin',(114.524364387726,1.45439216225896E-14,
63.5463953680056));
#190997=CARTESIAN_POINT('Origin',(118.647197809142,-6.8,64.3477970021793));
#190998=CARTESIAN_POINT('',(119.079891904685,-6.8,64.7421988952723));
#190999=CARTESIAN_POINT('',(119.012409844747,-6.8,65.0893622652905));
#191000=CARTESIAN_POINT('',(119.079891904685,-6.8,64.7421988952723));
#191001=CARTESIAN_POINT('',(118.556792124843,-6.8,64.8128916074539));
#191002=CARTESIAN_POINT('Origin',(116.959178380441,-6.8,51.0204257716897));
#191003=CARTESIAN_POINT('',(118.490150538636,-6.8,65.1557311365441));
#191004=CARTESIAN_POINT('',(118.556792124843,-6.8,64.8128916074539));
#191005=CARTESIAN_POINT('Origin',(116.959178380441,-6.8,51.0204257716897));
#191006=CARTESIAN_POINT('Origin',(119.138011311691,-6.8,64.4432019586286));
#191007=CARTESIAN_POINT('',(119.032511917208,-6.3,64.9859465837563));
#191008=CARTESIAN_POINT('',(118.966256200048,-6.3,65.3268009985918));
#191009=CARTESIAN_POINT('',(119.032511917208,-6.3,64.9859465837563));
#191010=CARTESIAN_POINT('Origin',(121.572825304407,1.45439216225896E-14,
51.9172323623126));
#191011=CARTESIAN_POINT('Origin',(121.572825304407,1.45439216225896E-14,
51.9172323623126));
#191012=CARTESIAN_POINT('Origin',(119.138011311691,-6.3,64.4432019586286));
#191013=CARTESIAN_POINT('',(118.510006827735,-6.3,65.053579894478));
#191014=CARTESIAN_POINT('',(118.444547114411,-6.3,65.3903392450207));
#191015=CARTESIAN_POINT('',(118.510006827735,-6.3,65.053579894478));
#191016=CARTESIAN_POINT('Origin',(116.959178380441,-6.3,51.0204257716897));
#191017=CARTESIAN_POINT('Origin',(116.959178380441,-6.3,51.0204257716897));
#191018=CARTESIAN_POINT('Origin',(118.647197809142,-6.3,64.3477970021793));
#191019=CARTESIAN_POINT('Origin',(121.082011801857,1.45439216225896E-14,
51.8218274058634));
#191020=CARTESIAN_POINT('Origin',(121.082011801857,1.45439216225896E-14,
51.8218274058634));
#191021=CARTESIAN_POINT('Origin',(117.665570804043,-6.8,64.1569870892808));
#191022=CARTESIAN_POINT('',(118.037661989115,-6.8,64.8631623729813));
#191023=CARTESIAN_POINT('',(117.971740706963,-6.8,65.2022962774431));
#191024=CARTESIAN_POINT('',(118.037661989115,-6.8,64.8631623729813));
#191025=CARTESIAN_POINT('',(117.522370687732,-6.8,64.8936841464147));
#191026=CARTESIAN_POINT('Origin',(116.959178380441,-6.8,51.0204257716897));
#191027=CARTESIAN_POINT('',(117.457059781373,-6.8,65.2296779553086));
#191028=CARTESIAN_POINT('',(117.522370687732,-6.8,64.8936841464147));
#191029=CARTESIAN_POINT('Origin',(116.959178380441,-6.8,51.0204257716897));
#191030=CARTESIAN_POINT('Origin',(118.156384306592,-6.8,64.25239204573));
#191031=CARTESIAN_POINT('',(117.991386218174,-6.3,65.1012293881955));
#191032=CARTESIAN_POINT('',(117.926609541577,-6.3,65.4344748369367));
#191033=CARTESIAN_POINT('',(117.991386218174,-6.3,65.1012293881955));
#191034=CARTESIAN_POINT('Origin',(120.591198299308,1.45439216225896E-14,
51.7264224494141));
#191035=CARTESIAN_POINT('Origin',(120.591198299308,1.45439216225896E-14,
51.7264224494141));
#191036=CARTESIAN_POINT('Origin',(118.156384306592,-6.3,64.25239204573));
#191037=CARTESIAN_POINT('',(117.476526584872,-6.3,65.1295304329511));
#191038=CARTESIAN_POINT('',(117.412329308735,-6.3,65.4597951396044));
#191039=CARTESIAN_POINT('',(117.476526584872,-6.3,65.1295304329511));
#191040=CARTESIAN_POINT('Origin',(116.959178380441,-6.3,51.0204257716897));
#191041=CARTESIAN_POINT('Origin',(116.959178380441,-6.3,51.0204257716897));
#191042=CARTESIAN_POINT('Origin',(117.665570804043,-6.3,64.1569870892808));
#191043=CARTESIAN_POINT('Origin',(120.100384796758,1.45439216225896E-14,
51.6310174929649));
#191044=CARTESIAN_POINT('Origin',(120.100384796758,1.45439216225896E-14,
51.6310174929649));
#191045=CARTESIAN_POINT('Origin',(116.683943798944,-6.8,63.9661771763823));
#191046=CARTESIAN_POINT('',(117.010809744205,-6.8,64.9050149881251));
#191047=CARTESIAN_POINT('',(116.946007519038,-6.8,65.2383918722067));
#191048=CARTESIAN_POINT('',(117.010809744205,-6.8,64.9050149881251));
#191049=CARTESIAN_POINT('',(116.50289039636,-6.8,64.8976115376352));
#191050=CARTESIAN_POINT('Origin',(116.959178380441,-6.8,51.0204257716897));
#191051=CARTESIAN_POINT('',(116.438501717996,-6.8,65.2288609184699));
#191052=CARTESIAN_POINT('',(116.50289039636,-6.8,64.8976115376352));
#191053=CARTESIAN_POINT('Origin',(116.959178380441,-6.8,51.0204257716897));
#191054=CARTESIAN_POINT('Origin',(117.174757301493,-6.8,64.0615821328315));
#191055=CARTESIAN_POINT('',(116.965325321626,-6.3,65.139010889263));
#191056=CARTESIAN_POINT('',(116.901611332515,-6.3,65.466789312112));
#191057=CARTESIAN_POINT('',(116.965325321626,-6.3,65.139010889263));
#191058=CARTESIAN_POINT('Origin',(119.609571294209,1.45439216225896E-14,
51.5356125365156));
#191059=CARTESIAN_POINT('Origin',(119.609571294209,1.45439216225896E-14,
51.5356125365156));
#191060=CARTESIAN_POINT('Origin',(117.174757301493,-6.3,64.0615821328315));
#191061=CARTESIAN_POINT('',(116.457698341079,-6.3,65.1301033469199));
#191062=CARTESIAN_POINT('',(116.394377533667,-6.3,65.4558590353759));
#191063=CARTESIAN_POINT('',(116.457698341079,-6.3,65.1301033469199));
#191064=CARTESIAN_POINT('Origin',(116.959178380441,-6.3,51.0204257716897));
#191065=CARTESIAN_POINT('Origin',(116.959178380441,-6.3,51.0204257716897));
#191066=CARTESIAN_POINT('Origin',(116.683943798944,-6.3,63.9661771763823));
#191067=CARTESIAN_POINT('Origin',(119.118757791659,1.45439216225896E-14,
51.4402075800664));
#191068=CARTESIAN_POINT('Origin',(119.118757791659,1.45439216225896E-14,
51.4402075800664));
#191069=CARTESIAN_POINT('Origin',(115.702316793845,-6.8,63.7753672634838));
#191070=CARTESIAN_POINT('',(115.998541570931,-6.8,64.8718394333745));
#191071=CARTESIAN_POINT('',(115.934476441709,-6.8,65.2014243064807));
#191072=CARTESIAN_POINT('',(115.998541570931,-6.8,64.8718394333745));
#191073=CARTESIAN_POINT('',(115.497708336948,-6.8,64.8279812692763));
#191074=CARTESIAN_POINT('Origin',(116.959178380441,-6.8,51.0204257716897));
#191075=CARTESIAN_POINT('',(115.433880657895,-6.8,65.1563445732553));
#191076=CARTESIAN_POINT('',(115.497708336948,-6.8,64.8279812692763));
#191077=CARTESIAN_POINT('Origin',(116.959178380441,-6.8,51.0204257716897));
#191078=CARTESIAN_POINT('Origin',(116.193130296394,-6.8,63.870772219933));
#191079=CARTESIAN_POINT('',(115.95357822888,-6.3,65.1031546209663));
#191080=CARTESIAN_POINT('',(115.890565211466,-6.3,65.4273268750535));
#191081=CARTESIAN_POINT('',(115.95357822888,-6.3,65.1031546209663));
#191082=CARTESIAN_POINT('Origin',(118.62794428911,1.45439216225896E-14,
51.3448026236171));
#191083=CARTESIAN_POINT('Origin',(118.62794428911,1.45439216225896E-14,
51.3448026236171));
#191084=CARTESIAN_POINT('Origin',(116.193130296394,-6.3,63.870772219933));
#191085=CARTESIAN_POINT('',(115.4529128302,-6.3,65.0584330233987));
#191086=CARTESIAN_POINT('',(115.390125794234,-6.3,65.381442709521));
#191087=CARTESIAN_POINT('',(115.4529128302,-6.3,65.0584330233987));
#191088=CARTESIAN_POINT('Origin',(116.959178380441,-6.3,51.0204257716897));
#191089=CARTESIAN_POINT('Origin',(116.959178380441,-6.3,51.0204257716897));
#191090=CARTESIAN_POINT('Origin',(115.702316793845,-6.3,63.7753672634838));
#191091=CARTESIAN_POINT('Origin',(118.13713078656,1.45439216225896E-14,
51.2493976671679));
#191092=CARTESIAN_POINT('Origin',(118.13713078656,1.45439216225896E-14,
51.2493976671679));
#191093=CARTESIAN_POINT('Origin',(114.720689788746,-6.8,63.5845573505853));
#191094=CARTESIAN_POINT('',(115.000350755645,-6.8,64.7662425114558));
#191095=CARTESIAN_POINT('',(114.936677223071,-6.8,65.0938128045052));
#191096=CARTESIAN_POINT('',(115.000350755645,-6.8,64.7662425114558));
#191097=CARTESIAN_POINT('',(114.506443068771,-6.8,64.6867556739635));
#191098=CARTESIAN_POINT('Origin',(116.959178380441,-6.8,51.0204257716897));
#191099=CARTESIAN_POINT('',(114.442842164132,-6.8,65.013952330542));
#191100=CARTESIAN_POINT('',(114.506443068771,-6.8,64.6867556739635));
#191101=CARTESIAN_POINT('Origin',(116.959178380441,-6.8,51.0204257716897));
#191102=CARTESIAN_POINT('Origin',(115.211503291295,-6.8,63.6799623070345));
#191103=CARTESIAN_POINT('',(114.955664196196,-6.3,64.9961337831114));
#191104=CARTESIAN_POINT('',(114.89302390524,-6.3,65.3183885353702));
#191105=CARTESIAN_POINT('',(114.955664196196,-6.3,64.9961337831114));
#191106=CARTESIAN_POINT('Origin',(117.64631728401,1.45439216225896E-14,
51.1539927107186));
#191107=CARTESIAN_POINT('Origin',(117.64631728401,1.45439216225896E-14,
51.1539927107186));
#191108=CARTESIAN_POINT('Origin',(115.211503291295,-6.3,63.6799623070345));
#191109=CARTESIAN_POINT('',(114.461807839218,-6.3,64.9163828775102));
#191110=CARTESIAN_POINT('',(114.399236700813,-6.3,65.2382818725149));
#191111=CARTESIAN_POINT('',(114.461807839218,-6.3,64.9163828775102));
#191112=CARTESIAN_POINT('Origin',(116.959178380441,-6.3,51.0204257716897));
#191113=CARTESIAN_POINT('Origin',(116.959178380441,-6.3,51.0204257716897));
#191114=CARTESIAN_POINT('Origin',(114.720689788746,-6.3,63.5845573505853));
#191115=CARTESIAN_POINT('Origin',(117.155503781461,1.45439216225896E-14,
51.0585877542694));
#191116=CARTESIAN_POINT('Origin',(117.155503781461,1.45439216225896E-14,
51.0585877542694));
#191117=CARTESIAN_POINT('Origin',(113.739062783647,-6.8,63.3937474376868));
#191118=CARTESIAN_POINT('',(114.015973185983,-6.8,64.589582955916));
#191119=CARTESIAN_POINT('',(113.952364223845,-6.8,64.9168210645219));
#191120=CARTESIAN_POINT('',(114.015973185983,-6.8,64.589582955916));
#191121=CARTESIAN_POINT('',(113.528942447158,-6.8,64.4747174642696));
#191122=CARTESIAN_POINT('Origin',(116.959178380441,-6.8,51.0204257716897));
#191123=CARTESIAN_POINT('',(113.465244649916,-6.8,64.802412587586));
#191124=CARTESIAN_POINT('',(113.528942447158,-6.8,64.4747174642696));
#191125=CARTESIAN_POINT('Origin',(116.959178380441,-6.8,51.0204257716897));
#191126=CARTESIAN_POINT('Origin',(114.229876286196,-6.8,63.489152394136));
#191127=CARTESIAN_POINT('',(113.971332261843,-6.3,64.8192394554237));
#191128=CARTESIAN_POINT('',(113.908753451129,-6.3,65.1411779208355));
#191129=CARTESIAN_POINT('',(113.971332261843,-6.3,64.8192394554237));
#191130=CARTESIAN_POINT('Origin',(116.664690278911,1.45439216225896E-14,
50.9631827978201));
#191131=CARTESIAN_POINT('Origin',(116.664690278911,1.45439216225896E-14,
50.9631827978201));
#191132=CARTESIAN_POINT('Origin',(114.229876286196,-6.3,63.489152394136));
#191133=CARTESIAN_POINT('',(113.484238738346,-6.3,64.7046969613014));
#191134=CARTESIAN_POINT('',(113.421575345531,-6.3,65.0270705617333));
#191135=CARTESIAN_POINT('',(113.484238738346,-6.3,64.7046969613014));
#191136=CARTESIAN_POINT('Origin',(116.959178380441,-6.3,51.0204257716897));
#191137=CARTESIAN_POINT('Origin',(116.959178380441,-6.3,51.0204257716897));
#191138=CARTESIAN_POINT('Origin',(113.739062783647,-6.3,63.3937474376868));
#191139=CARTESIAN_POINT('Origin',(116.173876776362,1.45439216225896E-14,
50.8677778413709));
#191140=CARTESIAN_POINT('Origin',(116.173876776362,1.45439216225896E-14,
50.8677778413709));
#191141=CARTESIAN_POINT('Origin',(112.757435778548,-6.8,63.2029375247883));
#191142=CARTESIAN_POINT('',(113.045365648647,-6.8,64.3420830787778));
#191143=CARTESIAN_POINT('',(112.981497218279,-6.8,64.6706560290523));
#191144=CARTESIAN_POINT('',(113.045365648647,-6.8,64.3420830787778));
#191145=CARTESIAN_POINT('',(112.565271334663,-6.8,64.191532952939));
#191146=CARTESIAN_POINT('Origin',(116.959178380441,-6.8,51.0204257716897));
#191147=CARTESIAN_POINT('',(112.501148491679,-6.8,64.5214147361248));
#191148=CARTESIAN_POINT('',(112.565271334663,-6.8,64.191532952939));
#191149=CARTESIAN_POINT('Origin',(116.959178380441,-6.8,51.0204257716897));
#191150=CARTESIAN_POINT('Origin',(113.248249281097,-6.8,63.2983424812375));
#191151=CARTESIAN_POINT('',(113.000541338854,-6.3,64.572683010979));
#191152=CARTESIAN_POINT('',(112.937715514028,-6.3,64.8958922474905));
#191153=CARTESIAN_POINT('',(113.000541338854,-6.3,64.572683010979));
#191154=CARTESIAN_POINT('Origin',(115.683063273812,1.45439216225896E-14,
50.7723728849216));
#191155=CARTESIAN_POINT('Origin',(115.683063273812,1.45439216225896E-14,
50.7723728849216));
#191156=CARTESIAN_POINT('Origin',(113.248249281097,-6.3,63.2983424812375));
#191157=CARTESIAN_POINT('',(112.520267197199,-6.3,64.42305801369));
#191158=CARTESIAN_POINT('',(112.457199265932,-6.3,64.7475127736486));
#191159=CARTESIAN_POINT('',(112.520267197199,-6.3,64.42305801369));
#191160=CARTESIAN_POINT('Origin',(116.959178380441,-6.3,51.0204257716897));
#191161=CARTESIAN_POINT('Origin',(116.959178380441,-6.3,51.0204257716897));
#191162=CARTESIAN_POINT('Origin',(112.757435778548,-6.3,63.2029375247883));
#191163=CARTESIAN_POINT('Origin',(115.192249771263,1.45439216225896E-14,
50.6769679284724));
#191164=CARTESIAN_POINT('Origin',(115.192249771263,1.45439216225896E-14,
50.6769679284724));
#191165=CARTESIAN_POINT('Origin',(111.775808773449,-6.8,63.0121276118898));
#191166=CARTESIAN_POINT('',(112.088702367317,-6.8,64.0228465813954));
#191167=CARTESIAN_POINT('',(112.024238324945,-6.8,64.354483674506));
#191168=CARTESIAN_POINT('',(112.088702367317,-6.8,64.0228465813954));
#191169=CARTESIAN_POINT('',(111.615716802316,-6.8,63.8357252949231));
#191170=CARTESIAN_POINT('Origin',(116.959178380441,-6.8,51.0204257716897));
#191171=CARTESIAN_POINT('',(111.550820639722,-6.8,64.169585442765));
#191172=CARTESIAN_POINT('',(111.615716802316,-6.8,63.8357252949231));
#191173=CARTESIAN_POINT('Origin',(116.959178380441,-6.8,51.0204257716897));
#191174=CARTESIAN_POINT('Origin',(112.266622275998,-6.8,63.107532568339));
#191175=CARTESIAN_POINT('',(112.043457034551,-6.3,64.2556124782166));
#191176=CARTESIAN_POINT('',(111.980064555798,-6.3,64.5817368819136));
#191177=CARTESIAN_POINT('',(112.043457034551,-6.3,64.2556124782166));
#191178=CARTESIAN_POINT('Origin',(114.701436268713,1.45439216225896E-14,
50.5815629720231));
#191179=CARTESIAN_POINT('Origin',(114.701436268713,1.45439216225896E-14,
50.5815629720231));
#191180=CARTESIAN_POINT('Origin',(112.266622275998,-6.3,63.107532568339));
#191181=CARTESIAN_POINT('',(111.570165962703,-6.3,64.0700628803767));
#191182=CARTESIAN_POINT('',(111.506362697021,-6.3,64.3983005890775));
#191183=CARTESIAN_POINT('',(111.570165962703,-6.3,64.0700628803767));
#191184=CARTESIAN_POINT('Origin',(116.959178380441,-6.3,51.0204257716897));
#191185=CARTESIAN_POINT('Origin',(116.959178380441,-6.3,51.0204257716897));
#191186=CARTESIAN_POINT('Origin',(111.775808773449,-6.3,63.0121276118898));
#191187=CARTESIAN_POINT('Origin',(114.210622766164,1.45439216225896E-14,
50.4861580155739));
#191188=CARTESIAN_POINT('Origin',(114.210622766164,1.45439216225896E-14,
50.4861580155739));
#191189=CARTESIAN_POINT('Origin',(110.79418176835,-6.8,62.8213176989913));
#191190=CARTESIAN_POINT('',(111.146389113021,-6.8,63.6297859632063));
#191191=CARTESIAN_POINT('',(111.080964504615,-6.8,63.9663647155047));
#191192=CARTESIAN_POINT('',(111.146389113021,-6.8,63.6297859632063));
#191193=CARTESIAN_POINT('',(110.680811825332,-6.8,63.4045525841295));
#191194=CARTESIAN_POINT('Origin',(116.959178380441,-6.8,51.0204257716897));
#191195=CARTESIAN_POINT('',(110.61475557299,-6.8,63.7443808465566));
#191196=CARTESIAN_POINT('',(110.680811825332,-6.8,63.4045525841295));
#191197=CARTESIAN_POINT('Origin',(116.959178380441,-6.8,51.0204257716897));
#191198=CARTESIAN_POINT('Origin',(111.284995270899,-6.8,62.9167226554405));
#191199=CARTESIAN_POINT('',(111.100464604885,-6.3,63.8660458969672));
#191200=CARTESIAN_POINT('',(111.036159355032,-6.3,64.1968660774633));
#191201=CARTESIAN_POINT('',(111.100464604885,-6.3,63.8660458969672));
#191202=CARTESIAN_POINT('Origin',(113.719809263614,1.45439216225896E-14,
50.3907530591246));
#191203=CARTESIAN_POINT('Origin',(113.719809263614,1.45439216225896E-14,
50.3907530591246));
#191204=CARTESIAN_POINT('Origin',(111.284995270899,-6.3,62.9167226554405));
#191205=CARTESIAN_POINT('',(110.634440589158,-6.3,63.6431107229422));
#191206=CARTESIAN_POINT('',(110.569535866522,-6.3,63.9770149081617));
#191207=CARTESIAN_POINT('',(110.634440589158,-6.3,63.6431107229422));
#191208=CARTESIAN_POINT('Origin',(116.959178380441,-6.3,51.0204257716897));
#191209=CARTESIAN_POINT('Origin',(116.959178380441,-6.3,51.0204257716897));
#191210=CARTESIAN_POINT('Origin',(110.79418176835,-6.3,62.8213176989913));
#191211=CARTESIAN_POINT('Origin',(113.228995761065,1.45439216225896E-14,
50.2953481026754));
#191212=CARTESIAN_POINT('Origin',(113.228995761065,1.45439216225896E-14,
50.2953481026754));
#191213=CARTESIAN_POINT('Origin',(109.812554763251,-6.8,62.6305077860928));
#191214=CARTESIAN_POINT('',(110.219097651412,-6.8,63.1594453067728));
#191215=CARTESIAN_POINT('',(110.152297951675,-6.8,63.5030982553971));
#191216=CARTESIAN_POINT('',(110.219097651412,-6.8,63.1594453067728));
#191217=CARTESIAN_POINT('',(109.761382244793,-6.8,62.8937662576995));
#191218=CARTESIAN_POINT('Origin',(116.959178380441,-6.8,51.0204257716897));
#191219=CARTESIAN_POINT('',(109.693716601825,-6.8,63.241874075816));
#191220=CARTESIAN_POINT('',(109.761382244793,-6.8,62.8937662576995));
#191221=CARTESIAN_POINT('Origin',(116.959178380441,-6.8,51.0204257716897));
#191222=CARTESIAN_POINT('Origin',(110.3033682658,-6.8,62.725912742542));
#191223=CARTESIAN_POINT('',(110.172200491729,-6.3,63.4007090739833));
#191224=CARTESIAN_POINT('',(110.106590949423,-6.3,63.7382392239751));
#191225=CARTESIAN_POINT('',(110.172200491729,-6.3,63.4007090739833));
#191226=CARTESIAN_POINT('Origin',(112.738182258515,1.45439216225896E-14,
50.1999431462261));
#191227=CARTESIAN_POINT('Origin',(112.738182258515,1.45439216225896E-14,
50.1999431462261));
#191228=CARTESIAN_POINT('Origin',(110.3033682658,-6.3,62.725912742542));
#191229=CARTESIAN_POINT('',(109.713872337286,-6.3,63.1381823234563));
#191230=CARTESIAN_POINT('',(109.647442892777,-6.3,63.4799304835687));
#191231=CARTESIAN_POINT('',(109.713872337286,-6.3,63.1381823234563));
#191232=CARTESIAN_POINT('Origin',(116.959178380441,-6.3,51.0204257716897));
#191233=CARTESIAN_POINT('Origin',(116.959178380441,-6.3,51.0204257716897));
#191234=CARTESIAN_POINT('Origin',(109.812554763251,-6.3,62.6305077860928));
#191235=CARTESIAN_POINT('Origin',(112.247368755966,1.45439216225896E-14,
50.1045381897769));
#191236=CARTESIAN_POINT('Origin',(112.247368755966,1.45439216225896E-14,
50.1045381897769));
#191237=CARTESIAN_POINT('Origin',(109.321741260701,-6.8,62.5351028296435));
#191238=CARTESIAN_POINT('',(109.259608804648,-6.3,62.8547450108513));
#191239=CARTESIAN_POINT('',(109.192232348899,-6.3,63.2013650971262));
#191240=CARTESIAN_POINT('',(109.259608804648,-6.3,62.8547450108513));
#191241=CARTESIAN_POINT('',(109.307827747489,-6.8,62.6066812927165));
#191242=CARTESIAN_POINT('Origin',(111.756555253416,1.45439216225896E-14,
50.0091332333276));
#191243=CARTESIAN_POINT('',(109.239160411739,-6.8,62.9599423477459));
#191244=CARTESIAN_POINT('',(109.307827747489,-6.8,62.6066812927165));
#191245=CARTESIAN_POINT('Origin',(111.756555253416,1.45439216225896E-14,
50.0091332333276));
#191246=CARTESIAN_POINT('Origin',(109.321741260701,-6.3,62.5351028296435));
#191247=CARTESIAN_POINT('',(108.809591344001,-6.3,62.5494636605398));
#191248=CARTESIAN_POINT('',(108.741125896572,-6.3,62.9016860953786));
#191249=CARTESIAN_POINT('',(108.809591344001,-6.3,62.5494636605398));
#191250=CARTESIAN_POINT('Origin',(116.959178380441,-6.3,51.0204257716897));
#191251=CARTESIAN_POINT('Origin',(116.959178380441,-6.3,51.0204257716897));
#191252=CARTESIAN_POINT('Origin',(108.830927758152,-6.3,62.4396978731943));
#191253=CARTESIAN_POINT('',(108.830927758152,-6.8,62.4396978731943));
#191254=CARTESIAN_POINT('',(108.78880613563,-6.8,62.6563937541252));
#191255=CARTESIAN_POINT('',(108.830927758152,-6.8,62.4396978731943));
#191256=CARTESIAN_POINT('',(108.830927758152,-6.52351515672298,62.4396978731943));
#191257=CARTESIAN_POINT('',(108.830927758152,-6.52351515672298,62.4396978731943));
#191258=CARTESIAN_POINT('Origin',(111.265741750867,1.45439216225896E-14,
49.9137282768784));
#191259=CARTESIAN_POINT('Origin',(111.265741750867,1.45439216225896E-14,
49.9137282768784));
#191260=CARTESIAN_POINT('Origin',(108.830927758152,-6.8,62.4396978731943));
#191261=CARTESIAN_POINT('',(109.151693712662,-6.8,62.5020487697396));
#191262=CARTESIAN_POINT('Origin',(116.959178380441,-6.8,51.0204257716897));
#191263=CARTESIAN_POINT('',(108.830927758152,-6.8,62.4396978731943));
#191264=CARTESIAN_POINT('Origin',(116.959178380441,-6.8,51.0204257716897));
#191265=CARTESIAN_POINT('Origin',(108.634602357132,-7.,62.4015358906146));
#191266=CARTESIAN_POINT('Origin',(114.524364387726,1.45439216225896E-14,
63.5463953680056));
#191267=CARTESIAN_POINT('Origin',(108.340114255602,-5.8,62.344292916745));
#191268=CARTESIAN_POINT('',(108.277981799549,-5.3,62.6639350979528));
#191269=CARTESIAN_POINT('',(108.2106053438,-5.3,63.0105551842277));
#191270=CARTESIAN_POINT('',(108.277981799549,-5.3,62.6639350979528));
#191271=CARTESIAN_POINT('',(108.318777841451,-5.8,62.4540587040905));
#191272=CARTESIAN_POINT('Origin',(110.774928248317,1.45439216225896E-14,
49.8183233204291));
#191273=CARTESIAN_POINT('',(108.250312394022,-5.8,62.8062811389293));
#191274=CARTESIAN_POINT('',(108.318777841451,-5.8,62.4540587040905));
#191275=CARTESIAN_POINT('Origin',(110.774928248317,1.45439216225896E-14,
49.8183233204291));
#191276=CARTESIAN_POINT('Origin',(108.340114255602,-5.3,62.344292916745));
#191277=CARTESIAN_POINT('',(107.835387239841,-5.3,62.3204664233688));
#191278=CARTESIAN_POINT('',(107.766719904091,-5.3,62.6737274783981));
#191279=CARTESIAN_POINT('',(107.835387239841,-5.3,62.3204664233688));
#191280=CARTESIAN_POINT('Origin',(116.959178380441,-5.3,51.0204257716897));
#191281=CARTESIAN_POINT('Origin',(116.959178380441,-5.3,51.0204257716897));
#191282=CARTESIAN_POINT('Origin',(107.849300753053,-5.3,62.2488879602958));
#191283=CARTESIAN_POINT('',(107.849300753053,-5.8,62.2488879602958));
#191284=CARTESIAN_POINT('',(107.807179130531,-5.8,62.4655838412267));
#191285=CARTESIAN_POINT('',(107.849300753053,-5.8,62.2488879602958));
#191286=CARTESIAN_POINT('',(107.849300753053,-5.47323030759699,62.2488879602958));
#191287=CARTESIAN_POINT('',(107.849300753053,-5.47323030759699,62.2488879602958));
#191288=CARTESIAN_POINT('Origin',(110.284114745768,1.45439216225896E-14,
49.7229183639799));
#191289=CARTESIAN_POINT('Origin',(110.284114745768,1.45439216225896E-14,
49.7229183639799));
#191290=CARTESIAN_POINT('Origin',(107.849300753053,-5.8,62.2488879602958));
#191291=CARTESIAN_POINT('',(108.120705741714,-5.8,62.3016440091592));
#191292=CARTESIAN_POINT('Origin',(116.959178380441,-5.8,51.0204257716897));
#191293=CARTESIAN_POINT('',(107.849300753053,-5.8,62.2488879602958));
#191294=CARTESIAN_POINT('Origin',(116.959178380441,-5.8,51.0204257716897));
#191295=CARTESIAN_POINT('Origin',(107.652975352033,-6.,62.2107259777161));
#191296=CARTESIAN_POINT('Origin',(114.524364387726,1.45439216225896E-14,
63.5463953680056));
#191297=CARTESIAN_POINT('Origin',(107.849300753053,-4.8,62.2488879602958));
#191298=CARTESIAN_POINT('',(108.241431829638,-4.8,62.8519674541085));
#191299=CARTESIAN_POINT('',(108.175002385128,-4.8,63.1937156142209));
#191300=CARTESIAN_POINT('',(108.241431829638,-4.8,62.8519674541085));
#191301=CARTESIAN_POINT('',(107.798128234595,-4.8,62.5121464319025));
#191302=CARTESIAN_POINT('Origin',(116.959178380441,-4.8,51.0204257716897));
#191303=CARTESIAN_POINT('',(107.730462591627,-4.8,62.8602542500189));
#191304=CARTESIAN_POINT('',(107.798128234595,-4.8,62.5121464319025));
#191305=CARTESIAN_POINT('Origin',(116.959178380441,-4.8,51.0204257716897));
#191306=CARTESIAN_POINT('Origin',(108.340114255602,-4.8,62.344292916745));
#191307=CARTESIAN_POINT('',(108.208946481531,-4.3,63.0190892481863));
#191308=CARTESIAN_POINT('',(108.143336939225,-4.3,63.3566193981781));
#191309=CARTESIAN_POINT('',(108.208946481531,-4.3,63.0190892481863));
#191310=CARTESIAN_POINT('Origin',(110.774928248317,1.45439216225896E-14,
49.8183233204291));
#191311=CARTESIAN_POINT('Origin',(110.774928248317,1.45439216225896E-14,
49.8183233204291));
#191312=CARTESIAN_POINT('Origin',(108.340114255602,-4.3,62.344292916745));
#191313=CARTESIAN_POINT('',(107.765030138665,-4.3,62.6824205245265));
#191314=CARTESIAN_POINT('',(107.698230438928,-4.3,63.0260734731508));
#191315=CARTESIAN_POINT('',(107.765030138665,-4.3,62.6824205245265));
#191316=CARTESIAN_POINT('Origin',(116.959178380441,-4.3,51.0204257716897));
#191317=CARTESIAN_POINT('Origin',(116.959178380441,-4.3,51.0204257716897));
#191318=CARTESIAN_POINT('Origin',(107.849300753053,-4.3,62.2488879602958));
#191319=CARTESIAN_POINT('Origin',(110.284114745768,1.45439216225896E-14,
49.7229183639799));
#191320=CARTESIAN_POINT('Origin',(110.284114745768,1.45439216225896E-14,
49.7229183639799));
#191321=CARTESIAN_POINT('Origin',(107.849300753053,-3.8,62.2488879602958));
#191322=CARTESIAN_POINT('',(108.180373076411,-3.8,63.1660859406959));
#191323=CARTESIAN_POINT('',(108.115468353774,-3.8,63.4999901259154));
#191324=CARTESIAN_POINT('',(108.180373076411,-3.8,63.1660859406959));
#191325=CARTESIAN_POINT('',(107.735930810035,-3.8,62.832122845434));
#191326=CARTESIAN_POINT('Origin',(116.959178380441,-3.8,51.0204257716897));
#191327=CARTESIAN_POINT('',(107.669874557693,-3.8,63.1719511078611));
#191328=CARTESIAN_POINT('',(107.735930810035,-3.8,62.832122845434));
#191329=CARTESIAN_POINT('Origin',(116.959178380441,-3.8,51.0204257716897));
#191330=CARTESIAN_POINT('Origin',(108.340114255602,-3.8,62.344292916745));
#191331=CARTESIAN_POINT('',(108.155583589588,-3.3,63.2936161582717));
#191332=CARTESIAN_POINT('',(108.091278339735,-3.3,63.6244363387677));
#191333=CARTESIAN_POINT('',(108.155583589588,-3.3,63.2936161582717));
#191334=CARTESIAN_POINT('Origin',(110.774928248317,1.45439216225896E-14,
49.8183233204291));
#191335=CARTESIAN_POINT('Origin',(110.774928248317,1.45439216225896E-14,
49.8183233204291));
#191336=CARTESIAN_POINT('Origin',(108.340114255602,-3.3,62.344292916745));
#191337=CARTESIAN_POINT('',(107.710694595175,-3.3,62.9619512680616));
#191338=CARTESIAN_POINT('',(107.645269986769,-3.3,63.2985300203599));
#191339=CARTESIAN_POINT('',(107.710694595175,-3.3,62.9619512680616));
#191340=CARTESIAN_POINT('Origin',(116.959178380441,-3.3,51.0204257716897));
#191341=CARTESIAN_POINT('Origin',(116.959178380441,-3.3,51.0204257716897));
#191342=CARTESIAN_POINT('Origin',(107.849300753053,-3.3,62.2488879602958));
#191343=CARTESIAN_POINT('Origin',(110.284114745768,1.45439216225896E-14,
49.7229183639799));
#191344=CARTESIAN_POINT('Origin',(110.284114745768,1.45439216225896E-14,
49.7229183639799));
#191345=CARTESIAN_POINT('Origin',(107.849300753053,-2.8,62.2488879602958));
#191346=CARTESIAN_POINT('',(108.134471444857,-2.8,63.4022281852319));
#191347=CARTESIAN_POINT('',(108.070668179174,-2.8,63.7304658939327));
#191348=CARTESIAN_POINT('',(108.134471444857,-2.8,63.4022281852319));
#191349=CARTESIAN_POINT('',(107.68920878192,-2.8,63.0724856433291));
#191350=CARTESIAN_POINT('Origin',(116.959178380441,-2.8,51.0204257716897));
#191351=CARTESIAN_POINT('',(107.624312619326,-2.8,63.4063457911709));
#191352=CARTESIAN_POINT('',(107.68920878192,-2.8,63.0724856433291));
#191353=CARTESIAN_POINT('Origin',(116.959178380441,-2.8,51.0204257716897));
#191354=CARTESIAN_POINT('Origin',(108.340114255602,-2.8,62.344292916745));
#191355=CARTESIAN_POINT('',(108.116949014155,-2.3,63.4923728266226));
#191356=CARTESIAN_POINT('',(108.053556535402,-2.3,63.8184972303196));
#191357=CARTESIAN_POINT('',(108.116949014155,-2.3,63.4923728266226));
#191358=CARTESIAN_POINT('Origin',(110.774928248317,1.45439216225896E-14,
49.8183233204291));
#191359=CARTESIAN_POINT('Origin',(110.774928248317,1.45439216225896E-14,
49.8183233204291));
#191360=CARTESIAN_POINT('Origin',(108.340114255602,-2.3,62.344292916745));
#191361=CARTESIAN_POINT('',(107.671380844371,-2.3,63.1642019733521));
#191362=CARTESIAN_POINT('',(107.606916801999,-2.3,63.4958390664627));
#191363=CARTESIAN_POINT('',(107.671380844371,-2.3,63.1642019733521));
#191364=CARTESIAN_POINT('Origin',(116.959178380441,-2.3,51.0204257716897));
#191365=CARTESIAN_POINT('Origin',(116.959178380441,-2.3,51.0204257716897));
#191366=CARTESIAN_POINT('Origin',(107.849300753053,-2.3,62.2488879602958));
#191367=CARTESIAN_POINT('Origin',(110.284114745768,1.45439216225896E-14,
49.7229183639799));
#191368=CARTESIAN_POINT('Origin',(110.284114745768,1.45439216225896E-14,
49.7229183639799));
#191369=CARTESIAN_POINT('Origin',(107.849300753053,-1.8,62.2488879602958));
#191370=CARTESIAN_POINT('',(108.102945674253,-1.8,63.5644134056468));
#191371=CARTESIAN_POINT('',(108.039877742986,-1.8,63.8888681656054));
#191372=CARTESIAN_POINT('',(108.102945674253,-1.8,63.5644134056468));
#191373=CARTESIAN_POINT('',(107.657136309168,-1.8,63.2374833884464));
#191374=CARTESIAN_POINT('Origin',(116.959178380441,-1.8,51.0204257716897));
#191375=CARTESIAN_POINT('',(107.593013466184,-1.8,63.5673651716323));
#191376=CARTESIAN_POINT('',(107.657136309168,-1.8,63.2374833884464));
#191377=CARTESIAN_POINT('Origin',(116.959178380441,-1.8,51.0204257716897));
#191378=CARTESIAN_POINT('Origin',(108.340114255602,-1.8,62.344292916745));
#191379=CARTESIAN_POINT('',(108.092406313359,-1.3,63.6186334464865));
#191380=CARTESIAN_POINT('',(108.029580488533,-1.3,63.941842682998));
#191381=CARTESIAN_POINT('',(108.092406313359,-1.3,63.6186334464865));
#191382=CARTESIAN_POINT('Origin',(110.774928248317,1.45439216225896E-14,
49.8183233204291));
#191383=CARTESIAN_POINT('Origin',(110.774928248317,1.45439216225896E-14,
49.8183233204291));
#191384=CARTESIAN_POINT('Origin',(108.340114255602,-1.3,62.344292916745));
#191385=CARTESIAN_POINT('',(107.646417120603,-1.3,63.292628557836));
#191386=CARTESIAN_POINT('',(107.582548690235,-1.3,63.6212015081105));
#191387=CARTESIAN_POINT('',(107.646417120603,-1.3,63.292628557836));
#191388=CARTESIAN_POINT('Origin',(116.959178380441,-1.3,51.0204257716897));
#191389=CARTESIAN_POINT('Origin',(116.959178380441,-1.3,51.0204257716897));
#191390=CARTESIAN_POINT('Origin',(107.849300753053,-1.3,62.2488879602958));
#191391=CARTESIAN_POINT('Origin',(110.284114745768,1.45439216225896E-14,
49.7229183639799));
#191392=CARTESIAN_POINT('Origin',(110.284114745768,1.45439216225896E-14,
49.7229183639799));
#191393=CARTESIAN_POINT('Origin',(107.849300753053,-0.799999999999986,62.2488879602958));
#191394=CARTESIAN_POINT('',(108.085290210302,-0.799999999999986,63.6552424403597));
#191395=CARTESIAN_POINT('',(108.022626817486,-0.799999999999986,63.9776160407915));
#191396=CARTESIAN_POINT('',(108.085290210302,-0.799999999999986,63.6552424403597));
#191397=CARTESIAN_POINT('',(107.639180416563,-0.799999999999986,63.3298579868786));
#191398=CARTESIAN_POINT('Origin',(116.959178380441,-0.799999999999986,51.0204257716897));
#191399=CARTESIAN_POINT('',(107.575482619322,-0.799999999999986,63.657553110195));
#191400=CARTESIAN_POINT('',(107.639180416563,-0.799999999999986,63.3298579868786));
#191401=CARTESIAN_POINT('Origin',(116.959178380441,-0.799999999999986,51.0204257716897));
#191402=CARTESIAN_POINT('Origin',(108.340114255602,-0.799999999999986,62.344292916745));
#191403=CARTESIAN_POINT('',(108.081570231249,-0.299999999999985,63.6743799780327));
#191404=CARTESIAN_POINT('',(108.018991420535,-0.299999999999985,63.9963184434445));
#191405=CARTESIAN_POINT('',(108.081570231249,-0.299999999999985,63.6743799780327));
#191406=CARTESIAN_POINT('Origin',(110.774928248317,1.45439216225896E-14,
49.8183233204291));
#191407=CARTESIAN_POINT('Origin',(110.774928248317,1.45439216225896E-14,
49.8183233204291));
#191408=CARTESIAN_POINT('Origin',(108.340114255602,-0.299999999999985,62.344292916745));
#191409=CARTESIAN_POINT('',(107.635397652839,-0.299999999999985,63.3493185220758));
#191410=CARTESIAN_POINT('',(107.571788690702,-0.299999999999985,63.6765566306816));
#191411=CARTESIAN_POINT('',(107.635397652839,-0.299999999999985,63.3493185220758));
#191412=CARTESIAN_POINT('Origin',(116.959178380441,-0.299999999999985,51.0204257716897));
#191413=CARTESIAN_POINT('Origin',(116.959178380441,-0.299999999999985,51.0204257716897));
#191414=CARTESIAN_POINT('Origin',(107.849300753053,-0.299999999999985,62.2488879602958));
#191415=CARTESIAN_POINT('Origin',(110.284114745768,1.45439216225896E-14,
49.7229183639799));
#191416=CARTESIAN_POINT('Origin',(110.284114745768,1.45439216225896E-14,
49.7229183639799));
#191417=CARTESIAN_POINT('Origin',(121.592078824439,-0.799999999999986,64.9202267408748));
#191418=CARTESIAN_POINT('',(121.964170009511,-0.799999999999986,65.6264020245753));
#191419=CARTESIAN_POINT('',(121.898248727359,-0.799999999999986,65.9655359290372));
#191420=CARTESIAN_POINT('',(121.964170009511,-0.799999999999986,65.6264020245753));
#191421=CARTESIAN_POINT('',(121.42078644216,-0.799999999999986,65.8014452565064));
#191422=CARTESIAN_POINT('Origin',(116.959178380441,-0.799999999999986,51.0204257716897));
#191423=CARTESIAN_POINT('',(121.356162424845,-0.799999999999986,66.1339053452465));
#191424=CARTESIAN_POINT('',(121.42078644216,-0.799999999999986,65.8014452565064));
#191425=CARTESIAN_POINT('Origin',(116.959178380441,-0.799999999999986,51.0204257716897));
#191426=CARTESIAN_POINT('Origin',(122.082892326988,-0.799999999999986,65.0156316973241));
#191427=CARTESIAN_POINT('',(121.960252054219,-0.299999999999985,65.6465580566214));
#191428=CARTESIAN_POINT('',(121.894429225941,-0.299999999999985,65.9851854623394));
#191429=CARTESIAN_POINT('',(121.960252054219,-0.299999999999985,65.6465580566214));
#191430=CARTESIAN_POINT('Origin',(124.517706319704,1.45439216225896E-14,
52.4896621010082));
#191431=CARTESIAN_POINT('Origin',(124.517706319704,1.45439216225896E-14,
52.4896621010082));
#191432=CARTESIAN_POINT('Origin',(122.082892326988,-0.299999999999985,65.0156316973241));
#191433=CARTESIAN_POINT('',(121.416947401949,-0.299999999999985,65.8211953076876));
#191434=CARTESIAN_POINT('',(121.352416146668,-0.299999999999985,66.1531781795096));
#191435=CARTESIAN_POINT('',(121.416947401949,-0.299999999999985,65.8211953076876));
#191436=CARTESIAN_POINT('Origin',(116.959178380441,-0.299999999999985,51.0204257716897));
#191437=CARTESIAN_POINT('Origin',(116.959178380441,-0.299999999999985,51.0204257716897));
#191438=CARTESIAN_POINT('Origin',(121.592078824439,-0.299999999999985,64.9202267408748));
#191439=CARTESIAN_POINT('Origin',(124.026892817154,1.45439216225896E-14,
52.3942571445589));
#191440=CARTESIAN_POINT('Origin',(124.026892817154,1.45439216225896E-14,
52.3942571445589));
#191441=CARTESIAN_POINT('Origin',(121.592078824439,-1.8,64.9202267408748));
#191442=CARTESIAN_POINT('',(121.9827732263,-1.8,65.5306972485281));
#191443=CARTESIAN_POINT('',(121.916380469554,-1.8,65.8722566673977));
#191444=CARTESIAN_POINT('',(121.9827732263,-1.8,65.5306972485281));
#191445=CARTESIAN_POINT('',(121.439011726697,-1.8,65.7076847636441));
#191446=CARTESIAN_POINT('Origin',(116.959178380441,-1.8,51.0204257716897));
#191447=CARTESIAN_POINT('',(121.373943716819,-1.8,66.0424289847036));
#191448=CARTESIAN_POINT('',(121.439011726697,-1.8,65.7076847636441));
#191449=CARTESIAN_POINT('Origin',(116.959178380441,-1.8,51.0204257716897));
#191450=CARTESIAN_POINT('Origin',(122.082892326988,-1.8,65.0156316973241));
#191451=CARTESIAN_POINT('',(121.971666484299,-1.3,65.5878361975535));
#191452=CARTESIAN_POINT('',(121.905556011225,-1.3,65.9279434000723));
#191453=CARTESIAN_POINT('',(121.971666484299,-1.3,65.5878361975535));
#191454=CARTESIAN_POINT('Origin',(124.517706319704,1.45439216225896E-14,
52.4896621010082));
#191455=CARTESIAN_POINT('Origin',(124.517706319704,1.45439216225896E-14,
52.4896621010082));
#191456=CARTESIAN_POINT('Origin',(122.082892326988,-1.3,65.0156316973241));
#191457=CARTESIAN_POINT('',(121.42813126715,-1.3,65.7636595961683));
#191458=CARTESIAN_POINT('',(121.363329041984,-1.3,66.09703648025));
#191459=CARTESIAN_POINT('',(121.42813126715,-1.3,65.7636595961683));
#191460=CARTESIAN_POINT('Origin',(116.959178380441,-1.3,51.0204257716897));
#191461=CARTESIAN_POINT('Origin',(116.959178380441,-1.3,51.0204257716897));
#191462=CARTESIAN_POINT('Origin',(121.592078824439,-1.3,64.9202267408748));
#191463=CARTESIAN_POINT('Origin',(124.026892817154,1.45439216225896E-14,
52.3942571445589));
#191464=CARTESIAN_POINT('Origin',(124.026892817154,1.45439216225896E-14,
52.3942571445589));
#191465=CARTESIAN_POINT('Origin',(121.592078824439,-2.8,64.9202267408748));
#191466=CARTESIAN_POINT('',(122.016025476175,-2.8,65.3596301065635));
#191467=CARTESIAN_POINT('',(121.948773188325,-2.8,65.7056114075657));
#191468=CARTESIAN_POINT('',(122.016025476175,-2.8,65.3596301065635));
#191469=CARTESIAN_POINT('',(121.471574873494,-2.8,65.540162731995));
#191470=CARTESIAN_POINT('Origin',(116.959178380441,-2.8,51.0204257716897));
#191471=CARTESIAN_POINT('',(121.405698397847,-2.8,65.8790661281236));
#191472=CARTESIAN_POINT('',(121.471574873494,-2.8,65.540162731995));
#191473=CARTESIAN_POINT('Origin',(116.959178380441,-2.8,51.0204257716897));
#191474=CARTESIAN_POINT('Origin',(122.082892326988,-2.8,65.0156316973241));
#191475=CARTESIAN_POINT('',(121.99753796795,-2.3,65.4547396166228));
#191476=CARTESIAN_POINT('',(121.930766252407,-2.3,65.7982485997717));
#191477=CARTESIAN_POINT('',(121.99753796795,-2.3,65.4547396166228));
#191478=CARTESIAN_POINT('Origin',(124.517706319704,1.45439216225896E-14,
52.4896621010082));
#191479=CARTESIAN_POINT('Origin',(124.517706319704,1.45439216225896E-14,
52.4896621010082));
#191480=CARTESIAN_POINT('Origin',(122.082892326988,-2.3,65.0156316973241));
#191481=CARTESIAN_POINT('',(121.453472666561,-2.3,65.6332900486406));
#191482=CARTESIAN_POINT('',(121.388048058155,-2.3,65.969868800939));
#191483=CARTESIAN_POINT('',(121.453472666561,-2.3,65.6332900486406));
#191484=CARTESIAN_POINT('Origin',(116.959178380441,-2.3,51.0204257716897));
#191485=CARTESIAN_POINT('Origin',(116.959178380441,-2.3,51.0204257716897));
#191486=CARTESIAN_POINT('Origin',(121.592078824439,-2.3,64.9202267408748));
#191487=CARTESIAN_POINT('Origin',(124.026892817154,1.45439216225896E-14,
52.3942571445589));
#191488=CARTESIAN_POINT('Origin',(124.026892817154,1.45439216225896E-14,
52.3942571445589));
#191489=CARTESIAN_POINT('Origin',(121.592078824439,-3.8,64.9202267408748));
#191490=CARTESIAN_POINT('',(122.064522377965,-3.8,65.1101364207424));
#191491=CARTESIAN_POINT('',(121.995976389156,-3.8,65.4627732029904));
#191492=CARTESIAN_POINT('',(122.064522377965,-3.8,65.1101364207424));
#191493=CARTESIAN_POINT('',(121.519034327862,-3.8,65.2960062238397));
#191494=CARTESIAN_POINT('Origin',(116.959178380441,-3.8,51.0204257716897));
#191495=CARTESIAN_POINT('',(121.451943382131,-3.8,65.641157495737));
#191496=CARTESIAN_POINT('',(121.519034327862,-3.8,65.2960062238397));
#191497=CARTESIAN_POINT('Origin',(116.959178380441,-3.8,51.0204257716897));
#191498=CARTESIAN_POINT('Origin',(122.082892326988,-3.8,65.0156316973241));
#191499=CARTESIAN_POINT('',(122.038319025802,-3.3,65.2449403086335));
#191500=CARTESIAN_POINT('',(121.970478072417,-3.3,65.5939500161639));
#191501=CARTESIAN_POINT('',(122.038319025802,-3.3,65.2449403086335));
#191502=CARTESIAN_POINT('Origin',(124.517706319704,1.45439216225896E-14,
52.4896621010082));
#191503=CARTESIAN_POINT('Origin',(124.517706319704,1.45439216225896E-14,
52.4896621010082));
#191504=CARTESIAN_POINT('Origin',(122.082892326988,-3.3,65.0156316973241));
#191505=CARTESIAN_POINT('',(121.493396398475,-3.3,65.4279012782383));
#191506=CARTESIAN_POINT('',(121.426966953965,-3.3,65.7696494383507));
#191507=CARTESIAN_POINT('',(121.493396398475,-3.3,65.4279012782383));
#191508=CARTESIAN_POINT('Origin',(116.959178380441,-3.3,51.0204257716897));
#191509=CARTESIAN_POINT('Origin',(116.959178380441,-3.3,51.0204257716897));
#191510=CARTESIAN_POINT('Origin',(121.592078824439,-3.3,64.9202267408748));
#191511=CARTESIAN_POINT('Origin',(124.026892817154,1.45439216225896E-14,
52.3942571445589));
#191512=CARTESIAN_POINT('Origin',(124.026892817154,1.45439216225896E-14,
52.3942571445589));
#191513=CARTESIAN_POINT('Origin',(121.592078824439,-4.3,64.9202267408748));
#191514=CARTESIAN_POINT('',(121.582257513942,-4.8,64.9707527510925));
#191515=CARTESIAN_POINT('',(121.513478375339,-4.8,65.3245889790688));
#191516=CARTESIAN_POINT('',(121.582257513942,-4.8,64.9707527510925));
#191517=CARTESIAN_POINT('',(121.548607101235,-4.3,65.1438682530293));
#191518=CARTESIAN_POINT('Origin',(124.026892817154,1.45439216225896E-14,
52.3942571445589));
#191519=CARTESIAN_POINT('',(121.480736796731,-4.3,65.4930289582246));
#191520=CARTESIAN_POINT('',(121.548607101235,-4.3,65.1438682530293));
#191521=CARTESIAN_POINT('Origin',(124.026892817154,1.45439216225896E-14,
52.3942571445589));
#191522=CARTESIAN_POINT('Origin',(121.592078824439,-4.8,64.9202267408748));
#191523=CARTESIAN_POINT('',(122.082892326988,-4.8,65.0156316973241));
#191524=CARTESIAN_POINT('',(122.058842881848,-4.8,65.1393547494882));
#191525=CARTESIAN_POINT('',(122.082892326988,-4.8,65.0156316973241));
#191526=CARTESIAN_POINT('',(121.681243230653,-4.8,64.9375586322092));
#191527=CARTESIAN_POINT('',(121.681243230653,-4.8,64.9375586322092));
#191528=CARTESIAN_POINT('Origin',(116.959178380441,-4.8,51.0204257716897));
#191529=CARTESIAN_POINT('Origin',(116.959178380441,-4.8,51.0204257716897));
#191530=CARTESIAN_POINT('Origin',(122.082892326988,-4.8,65.0156316973241));
#191531=CARTESIAN_POINT('',(122.082892326988,-4.3,65.0156316973241));
#191532=CARTESIAN_POINT('',(122.025384564787,-4.3,65.3114820099324));
#191533=CARTESIAN_POINT('',(122.082892326988,-4.3,65.0156316973241));
#191534=CARTESIAN_POINT('',(122.082892326988,-4.8,65.0156316973241));
#191535=CARTESIAN_POINT('Origin',(124.517706319704,1.45439216225896E-14,
52.4896621010082));
#191536=CARTESIAN_POINT('Origin',(122.082892326988,-4.3,65.0156316973241));
#191537=CARTESIAN_POINT('',(121.98125760463,-4.3,64.9958758099861));
#191538=CARTESIAN_POINT('Origin',(116.959178380441,-4.3,51.0204257716897));
#191539=CARTESIAN_POINT('',(122.082892326988,-4.3,65.0156316973241));
#191540=CARTESIAN_POINT('Origin',(116.959178380441,-4.3,51.0204257716897));
#191541=CARTESIAN_POINT('Origin',(121.395753423419,-5.,64.8820647582951));
#191542=CARTESIAN_POINT('Origin',(114.524364387726,1.45439216225896E-14,
63.5463953680056));
#191543=CARTESIAN_POINT('Origin',(121.101265321889,-5.3,64.8248217844256));
#191544=CARTESIAN_POINT('',(120.539222696584,-5.3,65.0958570688648));
#191545=CARTESIAN_POINT('',(120.472084417903,-5.3,65.4412518464652));
#191546=CARTESIAN_POINT('',(120.539222696584,-5.3,65.0958570688648));
#191547=CARTESIAN_POINT('',(121.077336186674,-5.3,64.9479258987745));
#191548=CARTESIAN_POINT('Origin',(116.959178380441,-5.3,51.0204257716897));
#191549=CARTESIAN_POINT('',(121.008940980487,-5.3,65.2997869755489));
#191550=CARTESIAN_POINT('',(121.077336186674,-5.3,64.9479258987745));
#191551=CARTESIAN_POINT('Origin',(116.959178380441,-5.3,51.0204257716897));
#191552=CARTESIAN_POINT('Origin',(120.61045181934,-5.3,64.7294168279763));
#191553=CARTESIAN_POINT('',(120.579868207262,-5.8,64.8867550871532));
#191554=CARTESIAN_POINT('',(120.511652633147,-5.8,65.2376920416435));
#191555=CARTESIAN_POINT('',(120.579868207262,-5.8,64.8867550871532));
#191556=CARTESIAN_POINT('Origin',(123.045265812055,1.45439216225896E-14,
52.2034472316604));
#191557=CARTESIAN_POINT('Origin',(123.045265812055,1.45439216225896E-14,
52.2034472316604));
#191558=CARTESIAN_POINT('Origin',(120.61045181934,-5.8,64.7294168279763));
#191559=CARTESIAN_POINT('',(121.101265321889,-5.8,64.8248217844256));
#191560=CARTESIAN_POINT('',(121.049241681607,-5.8,65.0924588763805));
#191561=CARTESIAN_POINT('',(121.101265321889,-5.8,64.8248217844256));
#191562=CARTESIAN_POINT('',(120.928023033738,-5.8,64.791146726852));
#191563=CARTESIAN_POINT('',(120.928023033738,-5.8,64.791146726852));
#191564=CARTESIAN_POINT('Origin',(116.959178380441,-5.8,51.0204257716897));
#191565=CARTESIAN_POINT('Origin',(116.959178380441,-5.8,51.0204257716897));
#191566=CARTESIAN_POINT('Origin',(121.101265321889,-5.8,64.8248217844256));
#191567=CARTESIAN_POINT('',(121.101265321889,-5.59519883471499,64.8248217844256));
#191568=CARTESIAN_POINT('Origin',(123.536079314605,1.45439216225896E-14,
52.2988521881097));
#191569=CARTESIAN_POINT('',(121.101265321889,-5.8,64.8248217844256));
#191570=CARTESIAN_POINT('Origin',(123.536079314605,1.45439216225896E-14,
52.2988521881097));
#191571=CARTESIAN_POINT('Origin',(120.41412641832,-6.,64.6912548453966));
#191572=CARTESIAN_POINT('Origin',(114.524364387726,1.45439216225896E-14,
63.5463953680056));
#191573=CARTESIAN_POINT('Origin',(119.628824814241,-5.8,64.5386069150778));
#191574=CARTESIAN_POINT('',(120.045505226416,-5.8,65.0153916561379));
#191575=CARTESIAN_POINT('',(119.978442632437,-5.8,65.3603970716418));
#191576=CARTESIAN_POINT('',(120.045505226416,-5.8,65.0153916561379));
#191577=CARTESIAN_POINT('',(119.515454871223,-5.8,65.121841800216));
#191578=CARTESIAN_POINT('Origin',(116.959178380441,-5.8,51.0204257716897));
#191579=CARTESIAN_POINT('',(119.449398618882,-5.8,65.4616700626431));
#191580=CARTESIAN_POINT('',(119.515454871223,-5.8,65.121841800216));
#191581=CARTESIAN_POINT('Origin',(116.959178380441,-5.8,51.0204257716897));
#191582=CARTESIAN_POINT('Origin',(120.11963831679,-5.8,64.6340118715271));
#191583=CARTESIAN_POINT('',(120.005554074461,-5.3,65.2209214897176));
#191584=CARTESIAN_POINT('',(119.939515866065,-5.3,65.5606569245574));
#191585=CARTESIAN_POINT('',(120.005554074461,-5.3,65.2209214897176));
#191586=CARTESIAN_POINT('Origin',(122.554452309506,1.45439216225896E-14,
52.1080422752111));
#191587=CARTESIAN_POINT('Origin',(122.554452309506,1.45439216225896E-14,
52.1080422752111));
#191588=CARTESIAN_POINT('Origin',(120.11963831679,-5.3,64.6340118715271));
#191589=CARTESIAN_POINT('',(119.476109460802,-5.3,65.3242553793072));
#191590=CARTESIAN_POINT('',(119.41103282268,-5.3,65.6590439886171));
#191591=CARTESIAN_POINT('',(119.476109460802,-5.3,65.3242553793072));
#191592=CARTESIAN_POINT('Origin',(116.959178380441,-5.3,51.0204257716897));
#191593=CARTESIAN_POINT('Origin',(116.959178380441,-5.3,51.0204257716897));
#191594=CARTESIAN_POINT('Origin',(119.628824814241,-5.3,64.5386069150778));
#191595=CARTESIAN_POINT('Origin',(122.063638806956,1.45439216225896E-14,
52.0126373187619));
#191596=CARTESIAN_POINT('Origin',(122.063638806956,1.45439216225896E-14,
52.0126373187619));
#191597=CARTESIAN_POINT('Origin',(118.647197809142,-5.8,64.3477970021793));
#191598=CARTESIAN_POINT('',(118.989520625611,-5.8,65.2071165018896));
#191599=CARTESIAN_POINT('',(118.924340180018,-5.8,65.5424391516779));
#191600=CARTESIAN_POINT('',(118.989520625611,-5.8,65.2071165018896));
#191601=CARTESIAN_POINT('',(118.467536606867,-5.8,65.2720691494816));
#191602=CARTESIAN_POINT('Origin',(116.959178380441,-5.8,51.0204257716897));
#191603=CARTESIAN_POINT('',(118.403114466043,-5.8,65.6034906788921));
#191604=CARTESIAN_POINT('',(118.467536606867,-5.8,65.2720691494816));
#191605=CARTESIAN_POINT('Origin',(116.959178380441,-5.8,51.0204257716897));
#191606=CARTESIAN_POINT('Origin',(119.138011311691,-5.8,64.4432019586286));
#191607=CARTESIAN_POINT('',(118.950702155056,-5.3,65.4068192239074));
#191608=CARTESIAN_POINT('',(118.886463414977,-5.3,65.7372972429876));
#191609=CARTESIAN_POINT('',(118.950702155056,-5.3,65.4068192239074));
#191610=CARTESIAN_POINT('Origin',(121.572825304407,1.45439216225896E-14,
51.9172323623126));
#191611=CARTESIAN_POINT('Origin',(121.572825304407,1.45439216225896E-14,
51.9172323623126));
#191612=CARTESIAN_POINT('Origin',(119.138011311691,-5.3,64.4432019586286));
#191613=CARTESIAN_POINT('',(118.429174209374,-5.3,65.4694255907055));
#191614=CARTESIAN_POINT('',(118.365661735554,-5.3,65.7961673124252));
#191615=CARTESIAN_POINT('',(118.429174209374,-5.3,65.4694255907055));
#191616=CARTESIAN_POINT('Origin',(116.959178380441,-5.3,51.0204257716897));
#191617=CARTESIAN_POINT('Origin',(116.959178380441,-5.3,51.0204257716897));
#191618=CARTESIAN_POINT('Origin',(118.647197809142,-5.3,64.3477970021793));
#191619=CARTESIAN_POINT('Origin',(121.082011801857,1.45439216225896E-14,
51.8218274058634));
#191620=CARTESIAN_POINT('Origin',(121.082011801857,1.45439216225896E-14,
51.8218274058634));
#191621=CARTESIAN_POINT('Origin',(117.665570804043,-5.8,64.1569870892808));
#191622=CARTESIAN_POINT('',(117.949362987349,-5.8,65.3174190902556));
#191623=CARTESIAN_POINT('',(117.885592229287,-5.8,65.6454895625796));
#191624=CARTESIAN_POINT('',(117.949362987349,-5.8,65.3174190902556));
#191625=CARTESIAN_POINT('',(117.434882428651,-5.8,65.3437699749629));
#191626=CARTESIAN_POINT('Origin',(116.959178380441,-5.8,51.0204257716897));
#191627=CARTESIAN_POINT('',(117.371664718591,-5.8,65.6689952761733));
#191628=CARTESIAN_POINT('',(117.434882428651,-5.8,65.3437699749629));
#191629=CARTESIAN_POINT('Origin',(116.959178380441,-5.8,51.0204257716897));
#191630=CARTESIAN_POINT('Origin',(118.156384306592,-5.8,64.25239204573));
#191631=CARTESIAN_POINT('',(117.911392231253,-5.3,65.5127607212116));
#191632=CARTESIAN_POINT('',(117.848504194417,-5.3,65.8362900091687));
#191633=CARTESIAN_POINT('',(117.911392231253,-5.3,65.5127607212116));
#191634=CARTESIAN_POINT('Origin',(120.591198299308,1.45439216225896E-14,
51.7264224494141));
#191635=CARTESIAN_POINT('Origin',(120.591198299308,1.45439216225896E-14,
51.7264224494141));
#191636=CARTESIAN_POINT('Origin',(118.156384306592,-5.3,64.25239204573));
#191637=CARTESIAN_POINT('',(117.397244100963,-5.3,65.5374014185508));
#191638=CARTESIAN_POINT('',(117.334886647803,-5.3,65.8582011037552));
#191639=CARTESIAN_POINT('',(117.397244100963,-5.3,65.5374014185508));
#191640=CARTESIAN_POINT('Origin',(116.959178380441,-5.3,51.0204257716897));
#191641=CARTESIAN_POINT('Origin',(116.959178380441,-5.3,51.0204257716897));
#191642=CARTESIAN_POINT('Origin',(117.665570804043,-5.3,64.1569870892808));
#191643=CARTESIAN_POINT('Origin',(120.100384796758,1.45439216225896E-14,
51.6310174929649));
#191644=CARTESIAN_POINT('Origin',(120.100384796758,1.45439216225896E-14,
51.6310174929649));
#191645=CARTESIAN_POINT('Origin',(116.683943798944,-5.8,63.9661771763823));
#191646=CARTESIAN_POINT('',(116.92399729191,-5.8,65.3516241095141));
#191647=CARTESIAN_POINT('',(116.861241235349,-5.8,65.6744744212084));
#191648=CARTESIAN_POINT('',(116.92399729191,-5.8,65.3516241095141));
#191649=CARTESIAN_POINT('',(116.416627454716,-5.8,65.3413936859011));
#191650=CARTESIAN_POINT('Origin',(116.959178380441,-5.8,51.0204257716897));
#191651=CARTESIAN_POINT('',(116.354247211386,-5.8,65.6623106157809));
#191652=CARTESIAN_POINT('',(116.416627454716,-5.8,65.3413936859011));
#191653=CARTESIAN_POINT('Origin',(116.959178380441,-5.8,51.0204257716897));
#191654=CARTESIAN_POINT('Origin',(117.174757301493,-5.8,64.0615821328315));
#191655=CARTESIAN_POINT('',(116.886636394382,-5.3,65.5438283057789));
#191656=CARTESIAN_POINT('',(116.82472213145,-5.3,65.8623479862876));
#191657=CARTESIAN_POINT('',(116.886636394382,-5.3,65.5438283057789));
#191658=CARTESIAN_POINT('Origin',(119.609571294209,1.45439216225896E-14,
51.5356125365156));
#191659=CARTESIAN_POINT('Origin',(119.609571294209,1.45439216225896E-14,
51.5356125365156));
#191660=CARTESIAN_POINT('Origin',(117.174757301493,-5.3,64.0615821328315));
#191661=CARTESIAN_POINT('',(116.379492360069,-5.3,65.5324362328468));
#191662=CARTESIAN_POINT('',(116.317939072905,-5.3,65.8490988632889));
#191663=CARTESIAN_POINT('',(116.379492360069,-5.3,65.5324362328468));
#191664=CARTESIAN_POINT('Origin',(116.959178380441,-5.3,51.0204257716897));
#191665=CARTESIAN_POINT('Origin',(116.959178380441,-5.3,51.0204257716897));
#191666=CARTESIAN_POINT('Origin',(116.683943798944,-5.3,63.9661771763823));
#191667=CARTESIAN_POINT('Origin',(119.118757791659,1.45439216225896E-14,
51.4402075800664));
#191668=CARTESIAN_POINT('Origin',(119.118757791659,1.45439216225896E-14,
51.4402075800664));
#191669=CARTESIAN_POINT('Origin',(115.702316793845,-5.8,63.7753672634838));
#191670=CARTESIAN_POINT('',(115.912708611971,-5.8,65.3134095235366));
#191671=CARTESIAN_POINT('',(115.850622706538,-5.8,65.6328122237612));
#191672=CARTESIAN_POINT('',(115.912708611971,-5.8,65.3134095235366));
#191673=CARTESIAN_POINT('',(115.412190971526,-5.8,65.2679277795385));
#191674=CARTESIAN_POINT('Origin',(116.959178380441,-5.8,51.0204257716897));
#191675=CARTESIAN_POINT('',(115.350321251236,-5.8,65.5862183091668));
#191676=CARTESIAN_POINT('',(115.412190971526,-5.8,65.2679277795385));
#191677=CARTESIAN_POINT('Origin',(116.959178380441,-5.8,51.0204257716897));
#191678=CARTESIAN_POINT('Origin',(116.193130296394,-5.8,63.870772219933));
#191679=CARTESIAN_POINT('',(115.875750340769,-5.3,65.503542397257));
#191680=CARTESIAN_POINT('',(115.814479890918,-5.3,65.8187499631281));
#191681=CARTESIAN_POINT('',(115.875750340769,-5.3,65.503542397257));
#191682=CARTESIAN_POINT('Origin',(118.62794428911,1.45439216225896E-14,
51.3448026236171));
#191683=CARTESIAN_POINT('Origin',(118.62794428911,1.45439216225896E-14,
51.3448026236171));
#191684=CARTESIAN_POINT('Origin',(116.193130296394,-5.3,63.870772219933));
#191685=CARTESIAN_POINT('',(115.37536255906,-5.3,65.4573925913142));
#191686=CARTESIAN_POINT('',(115.31429991436,-5.3,65.7715310976936));
#191687=CARTESIAN_POINT('',(115.37536255906,-5.3,65.4573925913142));
#191688=CARTESIAN_POINT('Origin',(116.959178380441,-5.3,51.0204257716897));
#191689=CARTESIAN_POINT('Origin',(116.959178380441,-5.3,51.0204257716897));
#191690=CARTESIAN_POINT('Origin',(115.702316793845,-5.3,63.7753672634838));
#191691=CARTESIAN_POINT('Origin',(118.13713078656,1.45439216225896E-14,
51.2493976671679));
#191692=CARTESIAN_POINT('Origin',(118.13713078656,1.45439216225896E-14,
51.2493976671679));
#191693=CARTESIAN_POINT('Origin',(114.720689788746,-5.8,63.5845573505853));
#191694=CARTESIAN_POINT('',(114.915038280088,-5.8,65.2051349600047));
#191695=CARTESIAN_POINT('',(114.853308979711,-5.8,65.522703095409));
#191696=CARTESIAN_POINT('',(114.915038280088,-5.8,65.2051349600047));
#191697=CARTESIAN_POINT('',(114.421227133504,-5.8,65.1251514682507));
#191698=CARTESIAN_POINT('Origin',(116.959178380441,-5.8,51.0204257716897));
#191699=CARTESIAN_POINT('',(114.359564014912,-5.8,65.4423791295872));
#191700=CARTESIAN_POINT('',(114.421227133504,-5.8,65.1251514682507));
#191701=CARTESIAN_POINT('Origin',(116.959178380441,-5.8,51.0204257716897));
#191702=CARTESIAN_POINT('Origin',(115.211503291295,-5.8,63.6799623070345));
#191703=CARTESIAN_POINT('',(114.878294208936,-5.3,65.3941658754951));
#191704=CARTESIAN_POINT('',(114.817366571332,-5.3,65.7076098340429));
#191705=CARTESIAN_POINT('',(114.878294208936,-5.3,65.3941658754951));
#191706=CARTESIAN_POINT('Origin',(117.64631728401,1.45439216225896E-14,
51.1539927107186));
#191707=CARTESIAN_POINT('Origin',(117.64631728401,1.45439216225896E-14,
51.1539927107186));
#191708=CARTESIAN_POINT('Origin',(115.211503291295,-5.3,63.6799623070345));
#191709=CARTESIAN_POINT('',(114.384522811763,-5.3,65.3139778917727));
#191710=CARTESIAN_POINT('',(114.323658813062,-5.3,65.6270944581799));
#191711=CARTESIAN_POINT('',(114.384522811763,-5.3,65.3139778917727));
#191712=CARTESIAN_POINT('Origin',(116.959178380441,-5.3,51.0204257716897));
#191713=CARTESIAN_POINT('Origin',(116.959178380441,-5.3,51.0204257716897));
#191714=CARTESIAN_POINT('Origin',(114.720689788746,-5.3,63.5845573505853));
#191715=CARTESIAN_POINT('Origin',(117.155503781461,1.45439216225896E-14,
51.0585877542694));
#191716=CARTESIAN_POINT('Origin',(117.155503781461,1.45439216225896E-14,
51.0585877542694));
#191717=CARTESIAN_POINT('Origin',(113.739062783647,-5.8,63.3937474376868));
#191718=CARTESIAN_POINT('',(113.930746540204,-5.8,65.0280338507332));
#191719=CARTESIAN_POINT('',(113.869076078592,-5.8,65.3452992884439));
#191720=CARTESIAN_POINT('',(113.930746540204,-5.8,65.0280338507332));
#191721=CARTESIAN_POINT('',(113.443597718493,-5.8,64.9137758398423));
#191722=CARTESIAN_POINT('Origin',(116.959178380441,-5.8,51.0204257716897));
#191723=CARTESIAN_POINT('',(113.381846310114,-5.8,65.2314577104878));
#191724=CARTESIAN_POINT('',(113.443597718493,-5.8,64.9137758398423));
#191725=CARTESIAN_POINT('Origin',(116.959178380441,-5.8,51.0204257716897));
#191726=CARTESIAN_POINT('Origin',(114.229876286196,-5.8,63.489152394136));
#191727=CARTESIAN_POINT('',(113.894037808231,-5.3,65.2168829628162));
#191728=CARTESIAN_POINT('',(113.833166748388,-5.3,65.5300358554694));
#191729=CARTESIAN_POINT('',(113.894037808231,-5.3,65.2168829628162));
#191730=CARTESIAN_POINT('Origin',(116.664690278911,1.45439216225896E-14,
50.9631827978201));
#191731=CARTESIAN_POINT('Origin',(116.664690278911,1.45439216225896E-14,
50.9631827978201));
#191732=CARTESIAN_POINT('Origin',(114.229876286196,-5.3,63.489152394136));
#191733=CARTESIAN_POINT('',(113.40684036881,-5.3,65.1028750671095));
#191734=CARTESIAN_POINT('',(113.345891473831,-5.3,65.4164283848248));
#191735=CARTESIAN_POINT('',(113.40684036881,-5.3,65.1028750671095));
#191736=CARTESIAN_POINT('Origin',(116.959178380441,-5.3,51.0204257716897));
#191737=CARTESIAN_POINT('Origin',(116.959178380441,-5.3,51.0204257716897));
#191738=CARTESIAN_POINT('Origin',(113.739062783647,-5.3,63.3937474376868));
#191739=CARTESIAN_POINT('Origin',(116.173876776362,1.45439216225896E-14,
50.8677778413709));
#191740=CARTESIAN_POINT('Origin',(116.173876776362,1.45439216225896E-14,
50.8677778413709));
#191741=CARTESIAN_POINT('Origin',(112.757435778548,-5.8,63.2029375247883));
#191742=CARTESIAN_POINT('',(112.959794118948,-5.8,64.7823082386979));
#191743=CARTESIAN_POINT('',(112.897887286472,-5.8,65.1007896930215));
#191744=CARTESIAN_POINT('',(112.959794118948,-5.8,64.7823082386979));
#191745=CARTESIAN_POINT('',(112.479361672869,-5.8,64.633497643002));
#191746=CARTESIAN_POINT('Origin',(116.959178380441,-5.8,51.0204257716897));
#191747=CARTESIAN_POINT('',(112.417223244359,-5.8,64.9531705496847));
#191748=CARTESIAN_POINT('',(112.479361672869,-5.8,64.633497643002));
#191749=CARTESIAN_POINT('Origin',(116.959178380441,-5.8,51.0204257716897));
#191750=CARTESIAN_POINT('Origin',(113.248249281097,-5.8,63.2983424812375));
#191751=CARTESIAN_POINT('',(112.922943414692,-5.3,64.9718877312178));
#191752=CARTESIAN_POINT('',(112.861845092366,-5.3,65.2862097821557));
#191753=CARTESIAN_POINT('',(112.922943414692,-5.3,64.9718877312178));
#191754=CARTESIAN_POINT('Origin',(115.683063273812,1.45439216225896E-14,
50.7723728849216));
#191755=CARTESIAN_POINT('Origin',(115.683063273812,1.45439216225896E-14,
50.7723728849216));
#191756=CARTESIAN_POINT('Origin',(113.248249281097,-5.3,63.2983424812375));
#191757=CARTESIAN_POINT('',(112.442371850103,-5.3,64.8237928346375));
#191758=CARTESIAN_POINT('',(112.38105092168,-5.3,65.1392600889511));
#191759=CARTESIAN_POINT('',(112.442371850103,-5.3,64.8237928346375));
#191760=CARTESIAN_POINT('Origin',(116.959178380441,-5.3,51.0204257716897));
#191761=CARTESIAN_POINT('Origin',(116.959178380441,-5.3,51.0204257716897));
#191762=CARTESIAN_POINT('Origin',(112.757435778548,-5.3,63.2029375247883));
#191763=CARTESIAN_POINT('Origin',(115.192249771263,1.45439216225896E-14,
50.6769679284724));
#191764=CARTESIAN_POINT('Origin',(115.192249771263,1.45439216225896E-14,
50.6769679284724));
#191765=CARTESIAN_POINT('Origin',(111.775808773449,-5.8,63.0121276118898));
#191766=CARTESIAN_POINT('',(112.002339277582,-5.8,64.4671439443595));
#191767=CARTESIAN_POINT('',(111.939890513497,-5.8,64.7884133811989));
#191768=CARTESIAN_POINT('',(112.002339277582,-5.8,64.4671439443595));
#191769=CARTESIAN_POINT('',(111.528779540089,-5.8,64.2829765045437));
#191770=CARTESIAN_POINT('Origin',(116.959178380441,-5.8,51.0204257716897));
#191771=CARTESIAN_POINT('',(111.465938179574,-5.8,64.6062656648512));
#191772=CARTESIAN_POINT('',(111.528779540089,-5.8,64.2829765045437));
#191773=CARTESIAN_POINT('Origin',(116.959178380441,-5.8,51.0204257716897));
#191774=CARTESIAN_POINT('Origin',(112.266622275998,-5.8,63.107532568339));
#191775=CARTESIAN_POINT('',(111.965163015835,-5.3,64.6583982766151));
#191776=CARTESIAN_POINT('',(111.903543900335,-5.3,64.9753995627983));
#191777=CARTESIAN_POINT('',(111.965163015835,-5.3,64.6583982766151));
#191778=CARTESIAN_POINT('Origin',(114.701436268713,1.45439216225896E-14,
50.5815629720231));
#191779=CARTESIAN_POINT('Origin',(114.701436268713,1.45439216225896E-14,
50.5815629720231));
#191780=CARTESIAN_POINT('Origin',(112.266622275998,-5.3,63.107532568339));
#191781=CARTESIAN_POINT('',(111.491367383505,-5.3,64.4754444044786));
#191782=CARTESIAN_POINT('',(111.429371208549,-5.3,64.7943854837179));
#191783=CARTESIAN_POINT('',(111.491367383505,-5.3,64.4754444044786));
#191784=CARTESIAN_POINT('Origin',(116.959178380441,-5.3,51.0204257716897));
#191785=CARTESIAN_POINT('Origin',(116.959178380441,-5.3,51.0204257716897));
#191786=CARTESIAN_POINT('Origin',(111.775808773449,-5.3,63.0121276118898));
#191787=CARTESIAN_POINT('Origin',(114.210622766164,1.45439216225896E-14,
50.4861580155739));
#191788=CARTESIAN_POINT('Origin',(114.210622766164,1.45439216225896E-14,
50.4861580155739));
#191789=CARTESIAN_POINT('Origin',(110.79418176835,-5.8,62.8213176989913));
#191790=CARTESIAN_POINT('',(111.058749813035,-5.8,64.0806488259782));
#191791=CARTESIAN_POINT('',(110.995429005623,-5.8,64.4064045144342));
#191792=CARTESIAN_POINT('',(111.058749813035,-5.8,64.0806488259782));
#191793=CARTESIAN_POINT('',(110.592333572166,-5.8,63.8597314653125));
#191794=CARTESIAN_POINT('Origin',(116.959178380441,-5.8,51.0204257716897));
#191795=CARTESIAN_POINT('',(110.528440653502,-5.8,64.1884303963207));
#191796=CARTESIAN_POINT('',(110.592333572166,-5.8,63.8597314653125));
#191797=CARTESIAN_POINT('Origin',(116.959178380441,-5.8,51.0204257716897));
#191798=CARTESIAN_POINT('Origin',(111.284995270899,-5.8,62.9167226554405));
#191799=CARTESIAN_POINT('',(111.021049521363,-5.3,64.2745990450339));
#191800=CARTESIAN_POINT('',(110.958593129912,-5.3,64.5959077210777));
#191801=CARTESIAN_POINT('',(111.021049521363,-5.3,64.2745990450339));
#191802=CARTESIAN_POINT('Origin',(113.719809263614,1.45439216225896E-14,
50.3907530591246));
#191803=CARTESIAN_POINT('Origin',(113.719809263614,1.45439216225896E-14,
50.3907530591246));
#191804=CARTESIAN_POINT('Origin',(111.284995270899,-5.3,62.9167226554405));
#191805=CARTESIAN_POINT('',(110.554289376198,-5.3,64.0554509097686));
#191806=CARTESIAN_POINT('',(110.491284191915,-5.3,64.3795828660941));
#191807=CARTESIAN_POINT('',(110.554289376198,-5.3,64.0554509097686));
#191808=CARTESIAN_POINT('Origin',(116.959178380441,-5.3,51.0204257716897));
#191809=CARTESIAN_POINT('Origin',(116.959178380441,-5.3,51.0204257716897));
#191810=CARTESIAN_POINT('Origin',(110.79418176835,-5.3,62.8213176989913));
#191811=CARTESIAN_POINT('Origin',(113.228995761065,1.45439216225896E-14,
50.2953481026754));
#191812=CARTESIAN_POINT('Origin',(113.228995761065,1.45439216225896E-14,
50.2953481026754));
#191813=CARTESIAN_POINT('Origin',(109.812554763251,-5.8,62.6305077860928));
#191814=CARTESIAN_POINT('',(110.129632204215,-5.8,63.6197028356265));
#191815=CARTESIAN_POINT('',(110.065067263532,-5.8,63.9518590029572));
#191816=CARTESIAN_POINT('',(110.129632204215,-5.8,63.6197028356265));
#191817=CARTESIAN_POINT('',(109.670767300217,-5.8,63.3599374084025));
#191818=CARTESIAN_POINT('Origin',(116.959178380441,-5.8,51.0204257716897));
#191819=CARTESIAN_POINT('',(109.605421471785,-5.8,63.6961108748868));
#191820=CARTESIAN_POINT('',(109.670767300217,-5.8,63.3599374084025));
#191821=CARTESIAN_POINT('Origin',(116.959178380441,-5.8,51.0204257716897));
#191822=CARTESIAN_POINT('Origin',(110.3033682658,-5.8,62.725912742542));
#191823=CARTESIAN_POINT('',(110.091183933495,-5.3,63.8175010540987));
#191824=CARTESIAN_POINT('',(110.027534637877,-5.3,64.1449466594431));
#191825=CARTESIAN_POINT('',(110.091183933495,-5.3,63.8175010540987));
#191826=CARTESIAN_POINT('Origin',(112.738182258515,1.45439216225896E-14,
50.1999431462261));
#191827=CARTESIAN_POINT('Origin',(112.738182258515,1.45439216225896E-14,
50.1999431462261));
#191828=CARTESIAN_POINT('Origin',(110.3033682658,-5.3,62.725912742542));
#191829=CARTESIAN_POINT('',(109.631849341272,-5.3,63.560151951261));
#191830=CARTESIAN_POINT('',(109.567452302182,-5.3,63.8914443440855));
#191831=CARTESIAN_POINT('',(109.631849341272,-5.3,63.560151951261));
#191832=CARTESIAN_POINT('Origin',(116.959178380441,-5.3,51.0204257716897));
#191833=CARTESIAN_POINT('Origin',(116.959178380441,-5.3,51.0204257716897));
#191834=CARTESIAN_POINT('Origin',(109.812554763251,-5.3,62.6305077860928));
#191835=CARTESIAN_POINT('Origin',(112.247368755966,1.45439216225896E-14,
50.1045381897769));
#191836=CARTESIAN_POINT('Origin',(112.247368755966,1.45439216225896E-14,
50.1045381897769));
#191837=CARTESIAN_POINT('Origin',(108.830927758152,-5.8,62.4396978731943));
#191838=CARTESIAN_POINT('',(109.215883585073,-5.8,63.0796906422719));
#191839=CARTESIAN_POINT('',(109.149636973735,-5.8,63.4204982119526));
#191840=CARTESIAN_POINT('',(109.215883585073,-5.8,63.0796906422719));
#191841=CARTESIAN_POINT('',(108.765152664381,-5.8,62.7780797073851));
#191842=CARTESIAN_POINT('Origin',(116.959178380441,-5.8,51.0204257716897));
#191843=CARTESIAN_POINT('',(108.697871783352,-5.8,63.1242081068039));
#191844=CARTESIAN_POINT('',(108.765152664381,-5.8,62.7780797073851));
#191845=CARTESIAN_POINT('Origin',(116.959178380441,-5.8,51.0204257716897));
#191846=CARTESIAN_POINT('Origin',(109.321741260701,-5.8,62.5351028296435));
#191847=CARTESIAN_POINT('',(109.176423614682,-5.3,63.2826935783785));
#191848=CARTESIAN_POINT('',(109.111164986591,-5.3,63.6184184402417));
#191849=CARTESIAN_POINT('',(109.176423614682,-5.3,63.2826935783785));
#191850=CARTESIAN_POINT('Origin',(111.756555253416,1.45439216225896E-14,
50.0091332333276));
#191851=CARTESIAN_POINT('Origin',(111.756555253416,1.45439216225896E-14,
50.0091332333276));
#191852=CARTESIAN_POINT('Origin',(109.321741260701,-5.3,62.5351028296435));
#191853=CARTESIAN_POINT('',(108.725070082524,-5.3,62.9842856858227));
#191854=CARTESIAN_POINT('',(108.658823471186,-5.3,63.3250932555033));
#191855=CARTESIAN_POINT('',(108.725070082524,-5.3,62.9842856858227));
#191856=CARTESIAN_POINT('Origin',(116.959178380441,-5.3,51.0204257716897));
#191857=CARTESIAN_POINT('Origin',(116.959178380441,-5.3,51.0204257716897));
#191858=CARTESIAN_POINT('Origin',(108.830927758152,-5.3,62.4396978731943));
#191859=CARTESIAN_POINT('Origin',(111.265741750867,1.45439216225896E-14,
49.9137282768784));
#191860=CARTESIAN_POINT('Origin',(111.265741750867,1.45439216225896E-14,
49.9137282768784));
#191861=CARTESIAN_POINT('Origin',(108.830927758152,-4.8,62.4396978731943));
#191862=CARTESIAN_POINT('',(109.141035838722,-4.8,63.4647469948118));
#191863=CARTESIAN_POINT('',(109.076638799632,-4.8,63.7960393876363));
#191864=CARTESIAN_POINT('',(109.141035838722,-4.8,63.4647469948118));
#191865=CARTESIAN_POINT('',(108.689140295118,-4.8,63.169127495504));
#191866=CARTESIAN_POINT('Origin',(116.959178380441,-4.8,51.0204257716897));
#191867=CARTESIAN_POINT('',(108.623794466686,-4.8,63.5053009619883));
#191868=CARTESIAN_POINT('',(108.689140295118,-4.8,63.169127495504));
#191869=CARTESIAN_POINT('Origin',(116.959178380441,-4.8,51.0204257716897));
#191870=CARTESIAN_POINT('Origin',(109.321741260701,-4.8,62.5351028296435));
#191871=CARTESIAN_POINT('',(109.109556928396,-4.3,63.6266911412002));
#191872=CARTESIAN_POINT('',(109.045907632778,-4.3,63.9541367465445));
#191873=CARTESIAN_POINT('',(109.109556928396,-4.3,63.6266911412002));
#191874=CARTESIAN_POINT('Origin',(111.756555253416,1.45439216225896E-14,
50.0091332333276));
#191875=CARTESIAN_POINT('Origin',(111.756555253416,1.45439216225896E-14,
50.0091332333276));
#191876=CARTESIAN_POINT('Origin',(109.321741260701,-4.3,62.5351028296435));
#191877=CARTESIAN_POINT('',(108.657191696567,-4.3,63.3334879662788));
#191878=CARTESIAN_POINT('',(108.592626755884,-4.3,63.6656441336094));
#191879=CARTESIAN_POINT('',(108.657191696567,-4.3,63.3334879662788));
#191880=CARTESIAN_POINT('Origin',(116.959178380441,-4.3,51.0204257716897));
#191881=CARTESIAN_POINT('Origin',(116.959178380441,-4.3,51.0204257716897));
#191882=CARTESIAN_POINT('Origin',(108.830927758152,-4.3,62.4396978731943));
#191883=CARTESIAN_POINT('Origin',(111.265741750867,1.45439216225896E-14,
49.9137282768784));
#191884=CARTESIAN_POINT('Origin',(111.265741750867,1.45439216225896E-14,
49.9137282768784));
#191885=CARTESIAN_POINT('Origin',(108.830927758152,-3.8,62.4396978731943));
#191886=CARTESIAN_POINT('',(109.08184886855,-3.8,63.7692360404209));
#191887=CARTESIAN_POINT('',(109.018843684266,-3.8,64.0933679967464));
#191888=CARTESIAN_POINT('',(109.08184886855,-3.8,63.7692360404209));
#191889=CARTESIAN_POINT('',(108.629079561968,-3.8,63.4781116395155));
#191890=CARTESIAN_POINT('Origin',(116.959178380441,-3.8,51.0204257716897));
#191891=CARTESIAN_POINT('',(108.565186643304,-3.8,63.8068105705237));
#191892=CARTESIAN_POINT('',(108.629079561968,-3.8,63.4781116395155));
#191893=CARTESIAN_POINT('Origin',(116.959178380441,-3.8,51.0204257716897));
#191894=CARTESIAN_POINT('Origin',(109.321741260701,-3.8,62.5351028296435));
#191895=CARTESIAN_POINT('',(109.057795511165,-3.3,63.8929792192369));
#191896=CARTESIAN_POINT('',(108.995339119714,-3.3,64.2142878952807));
#191897=CARTESIAN_POINT('',(109.057795511165,-3.3,63.8929792192369));
#191898=CARTESIAN_POINT('Origin',(111.756555253416,1.45439216225896E-14,
50.0091332333276));
#191899=CARTESIAN_POINT('Origin',(111.756555253416,1.45439216225896E-14,
50.0091332333276));
#191900=CARTESIAN_POINT('Origin',(109.321741260701,-3.3,62.5351028296435));
#191901=CARTESIAN_POINT('',(108.604682300287,-3.3,63.6036240437319));
#191902=CARTESIAN_POINT('',(108.541361492875,-3.3,63.9293797321879));
#191903=CARTESIAN_POINT('',(108.604682300287,-3.3,63.6036240437319));
#191904=CARTESIAN_POINT('Origin',(116.959178380441,-3.3,51.0204257716897));
#191905=CARTESIAN_POINT('Origin',(116.959178380441,-3.3,51.0204257716897));
#191906=CARTESIAN_POINT('Origin',(108.830927758152,-3.3,62.4396978731943));
#191907=CARTESIAN_POINT('Origin',(111.265741750867,1.45439216225896E-14,
49.9137282768784));
#191908=CARTESIAN_POINT('Origin',(111.265741750867,1.45439216225896E-14,
49.9137282768784));
#191909=CARTESIAN_POINT('Origin',(108.830927758152,-2.8,62.4396978731943));
#191910=CARTESIAN_POINT('',(109.037299870757,-2.8,63.9984196222324));
#191911=CARTESIAN_POINT('',(108.975303695801,-2.8,64.3173607014716));
#191912=CARTESIAN_POINT('',(109.037299870757,-2.8,63.9984196222324));
#191913=CARTESIAN_POINT('',(108.583898524792,-2.8,63.7105467658482));
#191914=CARTESIAN_POINT('Origin',(116.959178380441,-2.8,51.0204257716897));
#191915=CARTESIAN_POINT('',(108.521057164277,-2.8,64.0338359261557));
#191916=CARTESIAN_POINT('',(108.583898524792,-2.8,63.7105467658482));
#191917=CARTESIAN_POINT('Origin',(116.959178380441,-2.8,51.0204257716897));
#191918=CARTESIAN_POINT('Origin',(109.321741260701,-2.8,62.5351028296435));
#191919=CARTESIAN_POINT('',(109.020282000538,-2.3,64.0859685379196));
#191920=CARTESIAN_POINT('',(108.958662885038,-2.3,64.4029698241028));
#191921=CARTESIAN_POINT('',(109.020282000538,-2.3,64.0859685379196));
#191922=CARTESIAN_POINT('Origin',(111.756555253416,1.45439216225896E-14,
50.0091332333276));
#191923=CARTESIAN_POINT('Origin',(111.756555253416,1.45439216225896E-14,
50.0091332333276));
#191924=CARTESIAN_POINT('Origin',(109.321741260701,-2.3,62.5351028296435));
#191925=CARTESIAN_POINT('',(108.566644759735,-2.3,63.7993092492148));
#191926=CARTESIAN_POINT('',(108.504195995651,-2.3,64.1205786860541));
#191927=CARTESIAN_POINT('',(108.566644759735,-2.3,63.7993092492148));
#191928=CARTESIAN_POINT('Origin',(116.959178380441,-2.3,51.0204257716897));
#191929=CARTESIAN_POINT('Origin',(116.959178380441,-2.3,51.0204257716897));
#191930=CARTESIAN_POINT('Origin',(108.830927758152,-2.3,62.4396978731943));
#191931=CARTESIAN_POINT('Origin',(111.265741750867,1.45439216225896E-14,
49.9137282768784));
#191932=CARTESIAN_POINT('Origin',(111.265741750867,1.45439216225896E-14,
49.9137282768784));
#191933=CARTESIAN_POINT('Origin',(108.830927758152,-1.8,62.4396978731943));
#191934=CARTESIAN_POINT('',(109.006677332257,-1.8,64.1559581394927));
#191935=CARTESIAN_POINT('',(108.945356403834,-1.8,64.4714253938064));
#191936=CARTESIAN_POINT('',(109.006677332257,-1.8,64.1559581394927));
#191937=CARTESIAN_POINT('',(108.552853652473,-1.8,63.870257991408));
#191938=CARTESIAN_POINT('Origin',(116.959178380441,-1.8,51.0204257716897));
#191939=CARTESIAN_POINT('',(108.490715223963,-1.8,64.1899308980908));
#191940=CARTESIAN_POINT('',(108.552853652473,-1.8,63.870257991408));
#191941=CARTESIAN_POINT('Origin',(116.959178380441,-1.8,51.0204257716897));
#191942=CARTESIAN_POINT('Origin',(109.321741260701,-1.8,62.5351028296435));
#191943=CARTESIAN_POINT('',(108.996435394296,-1.3,64.2086480796238));
#191944=CARTESIAN_POINT('',(108.93533707197,-1.3,64.5229701305617));
#191945=CARTESIAN_POINT('',(108.996435394296,-1.3,64.2086480796238));
#191946=CARTESIAN_POINT('Origin',(111.756555253416,1.45439216225896E-14,
50.0091332333276));
#191947=CARTESIAN_POINT('Origin',(111.756555253416,1.45439216225896E-14,
50.0091332333276));
#191948=CARTESIAN_POINT('Origin',(109.321741260701,-1.3,62.5351028296435));
#191949=CARTESIAN_POINT('',(108.542472596003,-1.3,63.9236636306546));
#191950=CARTESIAN_POINT('',(108.480565763526,-1.3,64.2421450849782));
#191951=CARTESIAN_POINT('',(108.542472596003,-1.3,63.9236636306546));
#191952=CARTESIAN_POINT('Origin',(116.959178380441,-1.3,51.0204257716897));
#191953=CARTESIAN_POINT('Origin',(116.959178380441,-1.3,51.0204257716897));
#191954=CARTESIAN_POINT('Origin',(108.830927758152,-1.3,62.4396978731943));
#191955=CARTESIAN_POINT('Origin',(111.265741750867,1.45439216225896E-14,
49.9137282768784));
#191956=CARTESIAN_POINT('Origin',(111.265741750867,1.45439216225896E-14,
49.9137282768784));
#191957=CARTESIAN_POINT('Origin',(108.830927758152,-0.799999999999986,62.4396978731943));
#191958=CARTESIAN_POINT('',(108.989518845865,-0.799999999999986,64.2442304590662));
#191959=CARTESIAN_POINT('',(108.928569950886,-0.799999999999986,64.5577837767815));
#191960=CARTESIAN_POINT('',(108.989518845865,-0.799999999999986,64.2442304590662));
#191961=CARTESIAN_POINT('',(108.535462692998,-0.799999999999986,63.9597262753498));
#191962=CARTESIAN_POINT('Origin',(116.959178380441,-0.799999999999986,51.0204257716897));
#191963=CARTESIAN_POINT('',(108.473711284619,-0.799999999999986,64.2774081459953));
#191964=CARTESIAN_POINT('',(108.535462692998,-0.799999999999986,63.9597262753498));
#191965=CARTESIAN_POINT('Origin',(116.959178380441,-0.799999999999986,51.0204257716897));
#191966=CARTESIAN_POINT('Origin',(109.321741260701,-0.799999999999986,62.5351028296435));
#191967=CARTESIAN_POINT('',(108.985902782736,-0.299999999999985,64.2628333983237));
#191968=CARTESIAN_POINT('',(108.925031722893,-0.299999999999985,64.5759862909769));
#191969=CARTESIAN_POINT('',(108.985902782736,-0.299999999999985,64.2628333983237));
#191970=CARTESIAN_POINT('Origin',(111.756555253416,1.45439216225896E-14,
50.0091332333276));
#191971=CARTESIAN_POINT('Origin',(111.756555253416,1.45439216225896E-14,
50.0091332333276));
#191972=CARTESIAN_POINT('Origin',(109.321741260701,-0.299999999999985,62.5351028296435));
#191973=CARTESIAN_POINT('',(108.531798012159,-0.299999999999985,63.9785793297914));
#191974=CARTESIAN_POINT('',(108.470127550547,-0.299999999999985,64.2958447675021));
#191975=CARTESIAN_POINT('',(108.531798012159,-0.299999999999985,63.9785793297914));
#191976=CARTESIAN_POINT('Origin',(116.959178380441,-0.299999999999985,51.0204257716897));
#191977=CARTESIAN_POINT('Origin',(116.959178380441,-0.299999999999985,51.0204257716897));
#191978=CARTESIAN_POINT('Origin',(108.830927758152,-0.299999999999985,62.4396978731943));
#191979=CARTESIAN_POINT('Origin',(111.265741750867,1.45439216225896E-14,
49.9137282768784));
#191980=CARTESIAN_POINT('Origin',(111.265741750867,1.45439216225896E-14,
49.9137282768784));
#191981=CARTESIAN_POINT('Origin',(120.61045181934,-0.799999999999986,64.7294168279763));
#191982=CARTESIAN_POINT('',(120.881869643786,-0.799999999999986,65.9535090688376));
#191983=CARTESIAN_POINT('',(120.818389235277,-0.799999999999986,66.2800858296606));
#191984=CARTESIAN_POINT('',(120.881869643786,-0.799999999999986,65.9535090688376));
#191985=CARTESIAN_POINT('',(120.347180694029,-0.799999999999986,66.0838225941224));
#191986=CARTESIAN_POINT('Origin',(116.959178380441,-0.799999999999986,51.0204257716897));
#191987=CARTESIAN_POINT('',(120.284709039459,-0.799999999999986,66.4052097917178));
#191988=CARTESIAN_POINT('',(120.347180694029,-0.799999999999986,66.0838225941224));
#191989=CARTESIAN_POINT('Origin',(116.959178380441,-0.799999999999986,51.0204257716897));
#191990=CARTESIAN_POINT('Origin',(121.101265321889,-0.799999999999986,64.8248217844256));
#191991=CARTESIAN_POINT('',(120.878100080442,-0.299999999999985,65.9729016943031));
#191992=CARTESIAN_POINT('',(120.814707601689,-0.299999999999985,66.2990260980001));
#191993=CARTESIAN_POINT('',(120.878100080442,-0.299999999999985,65.9729016943031));
#191994=CARTESIAN_POINT('Origin',(123.536079314605,1.45439216225896E-14,
52.2988521881097));
#191995=CARTESIAN_POINT('Origin',(123.536079314605,1.45439216225896E-14,
52.2988521881097));
#191996=CARTESIAN_POINT('Origin',(121.101265321889,-0.299999999999985,64.8248217844256));
#191997=CARTESIAN_POINT('',(120.343472345358,-0.299999999999985,66.1029002989693));
#191998=CARTESIAN_POINT('',(120.28108449975,-0.299999999999985,66.4238563389795));
#191999=CARTESIAN_POINT('',(120.343472345358,-0.299999999999985,66.1029002989693));
#192000=CARTESIAN_POINT('Origin',(116.959178380441,-0.299999999999985,51.0204257716897));
#192001=CARTESIAN_POINT('Origin',(116.959178380441,-0.299999999999985,51.0204257716897));
#192002=CARTESIAN_POINT('Origin',(120.61045181934,-0.299999999999985,64.7294168279763));
#192003=CARTESIAN_POINT('Origin',(123.045265812055,1.45439216225896E-14,
52.2034472316604));
#192004=CARTESIAN_POINT('Origin',(123.045265812055,1.45439216225896E-14,
52.2034472316604));
#192005=CARTESIAN_POINT('Origin',(120.61045181934,-1.8,64.7294168279763));
#192006=CARTESIAN_POINT('',(120.8997623615,-1.8,65.8614594754157));
#192007=CARTESIAN_POINT('',(120.835861273808,-1.8,66.1902004322221));
#192008=CARTESIAN_POINT('',(120.8997623615,-1.8,65.8614594754157));
#192009=CARTESIAN_POINT('',(120.3647805193,-1.8,65.9932797941777));
#192010=CARTESIAN_POINT('Origin',(116.959178380441,-1.8,51.0204257716897));
#192011=CARTESIAN_POINT('',(120.301908052796,-1.8,66.3167289801245));
#192012=CARTESIAN_POINT('',(120.3647805193,-1.8,65.9932797941777));
#192013=CARTESIAN_POINT('Origin',(116.959178380441,-1.8,51.0204257716897));
#192014=CARTESIAN_POINT('Origin',(121.101265321889,-1.8,64.8248217844256));
#192015=CARTESIAN_POINT('',(120.889080989585,-1.3,65.9164100959823));
#192016=CARTESIAN_POINT('',(120.825431693966,-1.3,66.2438557013266));
#192017=CARTESIAN_POINT('',(120.889080989585,-1.3,65.9164100959823));
#192018=CARTESIAN_POINT('Origin',(123.536079314605,1.45439216225896E-14,
52.2988521881097));
#192019=CARTESIAN_POINT('Origin',(123.536079314605,1.45439216225896E-14,
52.2988521881097));
#192020=CARTESIAN_POINT('Origin',(121.101265321889,-1.3,64.8248217844256));
#192021=CARTESIAN_POINT('',(120.354274459392,-1.3,66.0473285171533));
#192022=CARTESIAN_POINT('',(120.291641863378,-1.3,66.3695436825644));
#192023=CARTESIAN_POINT('',(120.354274459392,-1.3,66.0473285171533));
#192024=CARTESIAN_POINT('Origin',(116.959178380441,-1.3,51.0204257716897));
#192025=CARTESIAN_POINT('Origin',(116.959178380441,-1.3,51.0204257716897));
#192026=CARTESIAN_POINT('Origin',(120.61045181934,-1.3,64.7294168279763));
#192027=CARTESIAN_POINT('Origin',(123.045265812055,1.45439216225896E-14,
52.2034472316604));
#192028=CARTESIAN_POINT('Origin',(123.045265812055,1.45439216225896E-14,
52.2034472316604));
#192029=CARTESIAN_POINT('Origin',(120.61045181934,-2.8,64.7294168279763));
#192030=CARTESIAN_POINT('',(120.931719828652,-2.8,65.6970533798742));
#192031=CARTESIAN_POINT('',(120.867053514301,-2.8,66.0297310669131));
#192032=CARTESIAN_POINT('',(120.931719828652,-2.8,65.6970533798742));
#192033=CARTESIAN_POINT('',(120.396205099365,-2.8,65.8316151513545));
#192034=CARTESIAN_POINT('Origin',(116.959178380441,-2.8,51.0204257716897));
#192035=CARTESIAN_POINT('',(120.332604194726,-2.8,66.158811807933));
#192036=CARTESIAN_POINT('',(120.396205099365,-2.8,65.8316151513545));
#192037=CARTESIAN_POINT('Origin',(116.959178380441,-2.8,51.0204257716897));
#192038=CARTESIAN_POINT('Origin',(121.101265321889,-2.8,64.8248217844256));
#192039=CARTESIAN_POINT('',(120.913956165254,-2.3,65.7884390497044));
#192040=CARTESIAN_POINT('',(120.849717425175,-2.3,66.1189170687846));
#192041=CARTESIAN_POINT('',(120.913956165254,-2.3,65.7884390497044));
#192042=CARTESIAN_POINT('Origin',(123.536079314605,1.45439216225896E-14,
52.2988521881097));
#192043=CARTESIAN_POINT('Origin',(123.536079314605,1.45439216225896E-14,
52.2988521881097));
#192044=CARTESIAN_POINT('Origin',(121.101265321889,-2.3,64.8248217844256));
#192045=CARTESIAN_POINT('',(120.37873920656,-2.3,65.9214689319321));
#192046=CARTESIAN_POINT('',(120.315545216751,-2.3,66.2465722036342));
#192047=CARTESIAN_POINT('',(120.37873920656,-2.3,65.9214689319321));
#192048=CARTESIAN_POINT('Origin',(116.959178380441,-2.3,51.0204257716897));
#192049=CARTESIAN_POINT('Origin',(116.959178380441,-2.3,51.0204257716897));
#192050=CARTESIAN_POINT('Origin',(120.61045181934,-2.3,64.7294168279763));
#192051=CARTESIAN_POINT('Origin',(123.045265812055,1.45439216225896E-14,
52.2034472316604));
#192052=CARTESIAN_POINT('Origin',(123.045265812055,1.45439216225896E-14,
52.2034472316604));
#192053=CARTESIAN_POINT('Origin',(120.61045181934,-3.8,64.7294168279763));
#192054=CARTESIAN_POINT('',(120.978269168954,-3.8,65.4575789793226));
#192055=CARTESIAN_POINT('',(120.912455269166,-3.8,65.7961604521707));
#192056=CARTESIAN_POINT('',(120.978269168954,-3.8,65.4575789793226));
#192057=CARTESIAN_POINT('',(120.441955022188,-3.8,65.5962533766876));
#192058=CARTESIAN_POINT('Origin',(116.959178380441,-3.8,51.0204257716897));
#192059=CARTESIAN_POINT('',(120.377263289707,-3.8,65.9290618280169));
#192060=CARTESIAN_POINT('',(120.441955022188,-3.8,65.5962533766876));
#192061=CARTESIAN_POINT('Origin',(116.959178380441,-3.8,51.0204257716897));
#192062=CARTESIAN_POINT('Origin',(121.101265321889,-3.8,64.8248217844256));
#192063=CARTESIAN_POINT('',(120.953127003325,-3.3,65.5869235630155));
#192064=CARTESIAN_POINT('',(120.887937884665,-3.3,65.9222908316384));
#192065=CARTESIAN_POINT('',(120.953127003325,-3.3,65.5869235630155));
#192066=CARTESIAN_POINT('Origin',(123.536079314605,1.45439216225896E-14,
52.2988521881097));
#192067=CARTESIAN_POINT('Origin',(123.536079314605,1.45439216225896E-14,
52.2988521881097));
#192068=CARTESIAN_POINT('Origin',(121.101265321889,-3.3,64.8248217844256));
#192069=CARTESIAN_POINT('',(120.417248123798,-3.3,65.7233587157339));
#192070=CARTESIAN_POINT('',(120.35315003438,-3.3,66.0531131534987));
#192071=CARTESIAN_POINT('',(120.417248123798,-3.3,65.7233587157339));
#192072=CARTESIAN_POINT('Origin',(116.959178380441,-3.3,51.0204257716897));
#192073=CARTESIAN_POINT('Origin',(116.959178380441,-3.3,51.0204257716897));
#192074=CARTESIAN_POINT('Origin',(120.61045181934,-3.3,64.7294168279763));
#192075=CARTESIAN_POINT('Origin',(123.045265812055,1.45439216225896E-14,
52.2034472316604));
#192076=CARTESIAN_POINT('Origin',(123.045265812055,1.45439216225896E-14,
52.2034472316604));
#192077=CARTESIAN_POINT('Origin',(120.61045181934,-4.8,64.7294168279763));
#192078=CARTESIAN_POINT('',(121.040226693838,-4.8,65.1388367364764));
#192079=CARTESIAN_POINT('',(120.972821486136,-4.8,65.4856047379895));
#192080=CARTESIAN_POINT('',(121.040226693838,-4.8,65.1388367364764));
#192081=CARTESIAN_POINT('',(120.502803495316,-4.8,65.2832166820304));
#192082=CARTESIAN_POINT('Origin',(116.959178380441,-4.8,51.0204257716897));
#192083=CARTESIAN_POINT('',(120.436602356825,-4.8,65.6237903153597));
#192084=CARTESIAN_POINT('',(120.502803495316,-4.8,65.2832166820304));
#192085=CARTESIAN_POINT('Origin',(116.959178380441,-4.8,51.0204257716897));
#192086=CARTESIAN_POINT('Origin',(121.101265321889,-4.8,64.8248217844256));
#192087=CARTESIAN_POINT('',(121.007257725681,-4.3,65.3084465276117));
#192088=CARTESIAN_POINT('',(120.940708624467,-4.3,65.6508102650276));
#192089=CARTESIAN_POINT('',(121.007257725681,-4.3,65.3084465276117));
#192090=CARTESIAN_POINT('Origin',(123.536079314605,1.45439216225896E-14,
52.2988521881097));
#192091=CARTESIAN_POINT('Origin',(123.536079314605,1.45439216225896E-14,
52.2988521881097));
#192092=CARTESIAN_POINT('Origin',(121.101265321889,-4.3,64.8248217844256));
#192093=CARTESIAN_POINT('',(120.470431262797,-4.3,65.4497565497637));
#192094=CARTESIAN_POINT('',(120.40504170288,-4.3,65.7861549941143));
#192095=CARTESIAN_POINT('',(120.470431262797,-4.3,65.4497565497637));
#192096=CARTESIAN_POINT('Origin',(116.959178380441,-4.3,51.0204257716897));
#192097=CARTESIAN_POINT('Origin',(116.959178380441,-4.3,51.0204257716897));
#192098=CARTESIAN_POINT('Origin',(120.61045181934,-4.3,64.7294168279763));
#192099=CARTESIAN_POINT('Origin',(123.045265812055,1.45439216225896E-14,
52.2034472316604));
#192100=CARTESIAN_POINT('Origin',(123.045265812055,1.45439216225896E-14,
52.2034472316604));
#192101=CARTESIAN_POINT('Origin',(119.628824814241,-4.8,64.5386069150778));
#192102=CARTESIAN_POINT('',(119.96973864102,-4.8,65.4051750021872));
#192103=CARTESIAN_POINT('',(119.904592853105,-4.8,65.7403193545668));
#192104=CARTESIAN_POINT('',(119.96973864102,-4.8,65.4051750021872));
#192105=CARTESIAN_POINT('',(119.440821494858,-4.8,65.5057953202889));
#192106=CARTESIAN_POINT('Origin',(116.959178380441,-4.8,51.0204257716897));
#192107=CARTESIAN_POINT('',(119.376599349995,-4.8,65.8361879648046));
#192108=CARTESIAN_POINT('',(119.440821494858,-4.8,65.5057953202889));
#192109=CARTESIAN_POINT('Origin',(116.959178380441,-4.8,51.0204257716897));
#192110=CARTESIAN_POINT('Origin',(120.11963831679,-4.8,64.6340118715271));
#192111=CARTESIAN_POINT('',(119.937889091834,-4.3,65.5690259106978));
#192112=CARTESIAN_POINT('',(119.873517125155,-4.3,65.9001893177927));
#192113=CARTESIAN_POINT('',(119.937889091834,-4.3,65.5690259106978));
#192114=CARTESIAN_POINT('Origin',(122.554452309506,1.45439216225896E-14,
52.1080422752111));
#192115=CARTESIAN_POINT('Origin',(122.554452309506,1.45439216225896E-14,
52.1080422752111));
#192116=CARTESIAN_POINT('Origin',(120.11963831679,-4.3,64.6340118715271));
#192117=CARTESIAN_POINT('',(119.409429136137,-4.3,65.6672941994899));
#192118=CARTESIAN_POINT('',(119.345948727628,-4.3,65.9938709603129));
#192119=CARTESIAN_POINT('',(119.409429136137,-4.3,65.6672941994899));
#192120=CARTESIAN_POINT('Origin',(116.959178380441,-4.3,51.0204257716897));
#192121=CARTESIAN_POINT('Origin',(116.959178380441,-4.3,51.0204257716897));
#192122=CARTESIAN_POINT('Origin',(119.628824814241,-4.3,64.5386069150778));
#192123=CARTESIAN_POINT('Origin',(122.063638806956,1.45439216225896E-14,
52.0126373187619));
#192124=CARTESIAN_POINT('Origin',(122.063638806956,1.45439216225896E-14,
52.0126373187619));
#192125=CARTESIAN_POINT('Origin',(118.647197809142,-4.8,64.3477970021793));
#192126=CARTESIAN_POINT('',(118.915873602585,-4.8,65.5859956992519));
#192127=CARTESIAN_POINT('',(118.85245717924,-4.8,65.9122432865856));
#192128=CARTESIAN_POINT('',(118.915873602585,-4.8,65.5859956992519));
#192129=CARTESIAN_POINT('',(118.394743704415,-4.8,65.6465542993439));
#192130=CARTESIAN_POINT('Origin',(116.959178380441,-4.8,51.0204257716897));
#192131=CARTESIAN_POINT('',(118.332026307686,-4.8,65.9692057244349));
#192132=CARTESIAN_POINT('',(118.394743704415,-4.8,65.6465542993439));
#192133=CARTESIAN_POINT('Origin',(116.959178380441,-4.8,51.0204257716897));
#192134=CARTESIAN_POINT('Origin',(119.138011311691,-4.8,64.4432019586286));
#192135=CARTESIAN_POINT('',(118.884879867865,-4.3,65.7454438459865));
#192136=CARTESIAN_POINT('',(118.822177915075,-4.3,66.0680158192969));
#192137=CARTESIAN_POINT('',(118.884879867865,-4.3,65.7454438459865));
#192138=CARTESIAN_POINT('Origin',(121.572825304407,1.45439216225896E-14,
51.9172323623126));
#192139=CARTESIAN_POINT('Origin',(121.572825304407,1.45439216225896E-14,
51.9172323623126));
#192140=CARTESIAN_POINT('Origin',(119.138011311691,-4.3,64.4432019586286));
#192141=CARTESIAN_POINT('',(118.364095660481,-4.3,65.8042240300283));
#192142=CARTESIAN_POINT('',(118.302069618616,-4.3,66.1233187604272));
#192143=CARTESIAN_POINT('',(118.364095660481,-4.3,65.8042240300283));
#192144=CARTESIAN_POINT('Origin',(116.959178380441,-4.3,51.0204257716897));
#192145=CARTESIAN_POINT('Origin',(116.959178380441,-4.3,51.0204257716897));
#192146=CARTESIAN_POINT('Origin',(118.647197809142,-4.3,64.3477970021793));
#192147=CARTESIAN_POINT('Origin',(121.082011801857,1.45439216225896E-14,
51.8218274058634));
#192148=CARTESIAN_POINT('Origin',(121.082011801857,1.45439216225896E-14,
51.8218274058634));
#192149=CARTESIAN_POINT('Origin',(117.665570804043,-4.8,64.1569870892808));
#192150=CARTESIAN_POINT('',(117.87730384708,-4.8,65.6881293797663));
#192151=CARTESIAN_POINT('',(117.815187944779,-4.8,66.0076863997269));
#192152=CARTESIAN_POINT('',(117.87730384708,-4.8,65.6881293797663));
#192153=CARTESIAN_POINT('',(117.363446332578,-4.8,65.7112749959501));
#192154=CARTESIAN_POINT('Origin',(116.959178380441,-4.8,51.0204257716897));
#192155=CARTESIAN_POINT('',(117.301841863851,-4.8,66.028200931394));
#192156=CARTESIAN_POINT('',(117.363446332578,-4.8,65.7112749959501));
#192157=CARTESIAN_POINT('Origin',(116.959178380441,-4.8,51.0204257716897));
#192158=CARTESIAN_POINT('Origin',(118.156384306592,-4.8,64.25239204573));
#192159=CARTESIAN_POINT('',(117.846953153215,-4.3,65.844269384596));
#192160=CARTESIAN_POINT('',(117.785509112589,-4.3,66.1603699931248));
#192161=CARTESIAN_POINT('',(117.846953153215,-4.3,65.844269384596));
#192162=CARTESIAN_POINT('Origin',(120.591198299308,1.45439216225896E-14,
51.7264224494141));
#192163=CARTESIAN_POINT('Origin',(120.591198299308,1.45439216225896E-14,
51.7264224494141));
#192164=CARTESIAN_POINT('Origin',(118.156384306592,-4.3,64.25239204573));
#192165=CARTESIAN_POINT('',(117.333348389206,-4.3,65.8661147187035));
#192166=CARTESIAN_POINT('',(117.272399494227,-4.3,66.1796680364188));
#192167=CARTESIAN_POINT('',(117.333348389206,-4.3,65.8661147187035));
#192168=CARTESIAN_POINT('Origin',(116.959178380441,-4.3,51.0204257716897));
#192169=CARTESIAN_POINT('Origin',(116.959178380441,-4.3,51.0204257716897));
#192170=CARTESIAN_POINT('Origin',(117.665570804043,-4.3,64.1569870892808));
#192171=CARTESIAN_POINT('Origin',(120.100384796758,1.45439216225896E-14,
51.6310174929649));
#192172=CARTESIAN_POINT('Origin',(120.100384796758,1.45439216225896E-14,
51.6310174929649));
#192173=CARTESIAN_POINT('Origin',(116.683943798944,-4.8,63.9661771763823));
#192174=CARTESIAN_POINT('',(116.853081315242,-4.8,65.7164533614791));
#192175=CARTESIAN_POINT('',(116.791904281457,-4.8,66.0311803457483));
#192176=CARTESIAN_POINT('',(116.853081315242,-4.8,65.7164533614791));
#192177=CARTESIAN_POINT('',(116.346134910676,-4.8,65.7040445767105));
#192178=CARTESIAN_POINT('Origin',(116.959178380441,-4.8,51.0204257716897));
#192179=CARTESIAN_POINT('',(116.285306180856,-4.8,66.0169797013613));
#192180=CARTESIAN_POINT('',(116.346134910676,-4.8,65.7040445767105));
#192181=CARTESIAN_POINT('Origin',(116.959178380441,-4.8,51.0204257716897));
#192182=CARTESIAN_POINT('Origin',(117.174757301493,-4.8,64.0615821328315));
#192183=CARTESIAN_POINT('',(116.823194555833,-4.3,65.8702066423449));
#192184=CARTESIAN_POINT('',(116.762659683573,-4.3,66.1816300084491));
#192185=CARTESIAN_POINT('',(116.823194555833,-4.3,65.8702066423449));
#192186=CARTESIAN_POINT('Origin',(119.609571294209,1.45439216225896E-14,
51.5356125365156));
#192187=CARTESIAN_POINT('Origin',(119.609571294209,1.45439216225896E-14,
51.5356125365156));
#192188=CARTESIAN_POINT('Origin',(117.174757301493,-4.3,64.0615821328315));
#192189=CARTESIAN_POINT('',(116.316420202403,-4.3,65.8569127356375));
#192190=CARTESIAN_POINT('',(116.256222839073,-4.3,66.1665997774845));
#192191=CARTESIAN_POINT('',(116.316420202403,-4.3,65.8569127356375));
#192192=CARTESIAN_POINT('Origin',(116.959178380441,-4.3,51.0204257716897));
#192193=CARTESIAN_POINT('Origin',(116.959178380441,-4.3,51.0204257716897));
#192194=CARTESIAN_POINT('Origin',(116.683943798944,-4.3,63.9661771763823));
#192195=CARTESIAN_POINT('Origin',(119.118757791659,1.45439216225896E-14,
51.4402075800664));
#192196=CARTESIAN_POINT('Origin',(119.118757791659,1.45439216225896E-14,
51.4402075800664));
#192197=CARTESIAN_POINT('Origin',(115.702316793845,-4.8,63.7753672634838));
#192198=CARTESIAN_POINT('',(115.842547716854,-4.8,65.6743542370615));
#192199=CARTESIAN_POINT('',(115.781991995879,-4.8,65.9858848599729));
#192200=CARTESIAN_POINT('',(115.842547716854,-4.8,65.6743542370615));
#192201=CARTESIAN_POINT('',(115.342273674314,-4.8,65.6276192967388));
#192202=CARTESIAN_POINT('Origin',(116.959178380441,-4.8,51.0204257716897));
#192203=CARTESIAN_POINT('',(115.281918593308,-4.8,65.9381177216365));
#192204=CARTESIAN_POINT('',(115.342273674314,-4.8,65.6276192967388));
#192205=CARTESIAN_POINT('Origin',(116.959178380441,-4.8,51.0204257716897));
#192206=CARTESIAN_POINT('Origin',(116.193130296394,-4.8,63.870772219933));
#192207=CARTESIAN_POINT('',(115.812967843606,-4.3,65.8265287333784));
#192208=CARTESIAN_POINT('',(115.753035111526,-4.3,66.1348543722614));
#192209=CARTESIAN_POINT('',(115.812967843606,-4.3,65.8265287333784));
#192210=CARTESIAN_POINT('Origin',(118.62794428911,1.45439216225896E-14,
51.3448026236171));
#192211=CARTESIAN_POINT('Origin',(118.62794428911,1.45439216225896E-14,
51.3448026236171));
#192212=CARTESIAN_POINT('Origin',(116.193130296394,-4.3,63.870772219933));
#192213=CARTESIAN_POINT('',(115.312792881512,-4.3,65.7792840708942));
#192214=CARTESIAN_POINT('',(115.253054679294,-4.3,66.0866089453843));
#192215=CARTESIAN_POINT('',(115.312792881512,-4.3,65.7792840708942));
#192216=CARTESIAN_POINT('Origin',(116.959178380441,-4.3,51.0204257716897));
#192217=CARTESIAN_POINT('Origin',(116.959178380441,-4.3,51.0204257716897));
#192218=CARTESIAN_POINT('Origin',(115.702316793845,-4.3,63.7753672634838));
#192219=CARTESIAN_POINT('Origin',(118.13713078656,1.45439216225896E-14,
51.2493976671679));
#192220=CARTESIAN_POINT('Origin',(118.13713078656,1.45439216225896E-14,
51.2493976671679));
#192221=CARTESIAN_POINT('Origin',(114.720689788746,-4.8,63.5845573505853));
#192222=CARTESIAN_POINT('',(114.845279212226,-4.8,65.5640124618232));
#192223=CARTESIAN_POINT('',(114.785054508555,-4.8,65.8738401568318));
#192224=CARTESIAN_POINT('',(114.845279212226,-4.8,65.5640124618232));
#192225=CARTESIAN_POINT('',(114.351542642308,-4.8,65.4836453083005));
#192226=CARTESIAN_POINT('Origin',(116.959178380441,-4.8,51.0204257716897));
#192227=CARTESIAN_POINT('',(114.291379402093,-4.8,65.7931568028158));
#192228=CARTESIAN_POINT('',(114.351542642308,-4.8,65.4836453083005));
#192229=CARTESIAN_POINT('Origin',(116.959178380441,-4.8,51.0204257716897));
#192230=CARTESIAN_POINT('Origin',(115.211503291295,-4.8,63.6799623070345));
#192231=CARTESIAN_POINT('',(114.815862796901,-4.3,65.7153460442249));
#192232=CARTESIAN_POINT('',(114.756251022793,-4.3,66.0220205057171));
#192233=CARTESIAN_POINT('',(114.815862796901,-4.3,65.7153460442249));
#192234=CARTESIAN_POINT('Origin',(117.64631728401,1.45439216225896E-14,
51.1539927107186));
#192235=CARTESIAN_POINT('Origin',(117.64631728401,1.45439216225896E-14,
51.1539927107186));
#192236=CARTESIAN_POINT('Origin',(115.211503291295,-4.3,63.6799623070345));
#192237=CARTESIAN_POINT('',(114.322156574729,-4.3,65.6348227658621));
#192238=CARTESIAN_POINT('',(114.26260440808,-4.3,65.9411905750978));
#192239=CARTESIAN_POINT('',(114.322156574729,-4.3,65.6348227658621));
#192240=CARTESIAN_POINT('Origin',(116.959178380441,-4.3,51.0204257716897));
#192241=CARTESIAN_POINT('Origin',(116.959178380441,-4.3,51.0204257716897));
#192242=CARTESIAN_POINT('Origin',(114.720689788746,-4.3,63.5845573505853));
#192243=CARTESIAN_POINT('Origin',(117.155503781461,1.45439216225896E-14,
51.0585877542694));
#192244=CARTESIAN_POINT('Origin',(117.155503781461,1.45439216225896E-14,
51.0585877542694));
#192245=CARTESIAN_POINT('Origin',(113.739062783647,-4.8,63.3937474376868));
#192246=CARTESIAN_POINT('',(113.861053774525,-4.8,65.3865702590969));
#192247=CARTESIAN_POINT('',(113.800883714328,-4.8,65.6961168391996));
#192248=CARTESIAN_POINT('',(113.861053774525,-4.8,65.3865702590969));
#192249=CARTESIAN_POINT('',(113.373813738472,-4.8,65.272781502971));
#192250=CARTESIAN_POINT('Origin',(116.959178380441,-4.8,51.0204257716897));
#192251=CARTESIAN_POINT('',(113.313568505077,-4.8,65.5827148137224));
#192252=CARTESIAN_POINT('',(113.373813738472,-4.8,65.272781502971));
#192253=CARTESIAN_POINT('Origin',(116.959178380441,-4.8,51.0204257716897));
#192254=CARTESIAN_POINT('Origin',(114.229876286196,-4.8,63.489152394136));
#192255=CARTESIAN_POINT('',(113.83166433961,-4.3,65.5377650400095));
#192256=CARTESIAN_POINT('',(113.772105558741,-4.3,65.8441668762851));
#192257=CARTESIAN_POINT('',(113.83166433961,-4.3,65.5377650400095));
#192258=CARTESIAN_POINT('Origin',(116.664690278911,1.45439216225896E-14,
50.9631827978201));
#192259=CARTESIAN_POINT('Origin',(116.664690278911,1.45439216225896E-14,
50.9631827978201));
#192260=CARTESIAN_POINT('Origin',(114.229876286196,-4.3,63.489152394136));
#192261=CARTESIAN_POINT('',(113.344387186316,-4.3,65.4241672345822));
#192262=CARTESIAN_POINT('',(113.284755503242,-4.3,65.7309441183195));
#192263=CARTESIAN_POINT('',(113.344387186316,-4.3,65.4241672345822));
#192264=CARTESIAN_POINT('Origin',(116.959178380441,-4.3,51.0204257716897));
#192265=CARTESIAN_POINT('Origin',(116.959178380441,-4.3,51.0204257716897));
#192266=CARTESIAN_POINT('Origin',(113.739062783647,-4.3,63.3937474376868));
#192267=CARTESIAN_POINT('Origin',(116.173876776362,1.45439216225896E-14,
50.8677778413709));
#192268=CARTESIAN_POINT('Origin',(116.173876776362,1.45439216225896E-14,
50.8677778413709));
#192269=CARTESIAN_POINT('Origin',(112.757435778548,-4.8,63.2029375247883));
#192270=CARTESIAN_POINT('',(112.889835003128,-4.8,65.1422148929144));
#192271=CARTESIAN_POINT('',(112.829445471306,-4.8,65.4528905510097));
#192272=CARTESIAN_POINT('',(112.889835003128,-4.8,65.1422148929144));
#192273=CARTESIAN_POINT('',(112.409141595728,-4.8,64.9947468201283));
#192274=CARTESIAN_POINT('Origin',(116.959178380441,-4.8,51.0204257716897));
#192275=CARTESIAN_POINT('',(112.348537143845,-4.8,65.3065281405739));
#192276=CARTESIAN_POINT('',(112.409141595728,-4.8,64.9947468201283));
#192277=CARTESIAN_POINT('Origin',(116.959178380441,-4.8,51.0204257716897));
#192278=CARTESIAN_POINT('Origin',(113.248249281097,-4.8,63.2983424812375));
#192279=CARTESIAN_POINT('',(112.860337198513,-4.3,65.2939671848206));
#192280=CARTESIAN_POINT('',(112.800565591803,-4.3,65.6014639096681));
#192281=CARTESIAN_POINT('',(112.860337198513,-4.3,65.2939671848206));
#192282=CARTESIAN_POINT('Origin',(115.683063273812,1.45439216225896E-14,
50.7723728849216));
#192283=CARTESIAN_POINT('Origin',(115.683063273812,1.45439216225896E-14,
50.7723728849216));
#192284=CARTESIAN_POINT('Origin',(113.248249281097,-4.3,63.2983424812375));
#192285=CARTESIAN_POINT('',(112.379537656463,-4.3,65.14704512475));
#192286=CARTESIAN_POINT('',(112.319557683455,-4.3,65.4556137959266));
#192287=CARTESIAN_POINT('',(112.379537656463,-4.3,65.14704512475));
#192288=CARTESIAN_POINT('Origin',(116.959178380441,-4.3,51.0204257716897));
#192289=CARTESIAN_POINT('Origin',(116.959178380441,-4.3,51.0204257716897));
#192290=CARTESIAN_POINT('Origin',(112.757435778548,-4.3,63.2029375247883));
#192291=CARTESIAN_POINT('Origin',(115.192249771263,1.45439216225896E-14,
50.6769679284724));
#192292=CARTESIAN_POINT('Origin',(115.192249771263,1.45439216225896E-14,
50.6769679284724));
#192293=CARTESIAN_POINT('Origin',(111.775808773449,-4.8,63.0121276118898));
#192294=CARTESIAN_POINT('',(111.931769528859,-4.8,64.8301920168471));
#192295=CARTESIAN_POINT('',(111.870877270834,-4.8,65.1434539641476));
#192296=CARTESIAN_POINT('',(111.931769528859,-4.8,64.8301920168471));
#192297=CARTESIAN_POINT('',(111.457767453663,-4.8,64.6483001958862));
#192298=CARTESIAN_POINT('Origin',(116.959178380441,-4.8,51.0204257716897));
#192299=CARTESIAN_POINT('',(111.396511403375,-4.8,64.9634336827943));
#192300=CARTESIAN_POINT('',(111.457767453663,-4.8,64.6483001958862));
#192301=CARTESIAN_POINT('Origin',(116.959178380441,-4.8,51.0204257716897));
#192302=CARTESIAN_POINT('Origin',(112.266622275998,-4.8,63.107532568339));
#192303=CARTESIAN_POINT('',(111.902023442088,-4.3,64.9832216033437));
#192304=CARTESIAN_POINT('',(111.841764510541,-4.3,65.2932253846267));
#192305=CARTESIAN_POINT('',(111.902023442088,-4.3,64.9832216033437));
#192306=CARTESIAN_POINT('Origin',(114.701436268713,1.45439216225896E-14,
50.5815629720231));
#192307=CARTESIAN_POINT('Origin',(114.701436268713,1.45439216225896E-14,
50.5815629720231));
#192308=CARTESIAN_POINT('Origin',(112.266622275998,-4.3,63.107532568339));
#192309=CARTESIAN_POINT('',(111.427841658067,-4.3,64.8022542995263));
#192310=CARTESIAN_POINT('',(111.367230235014,-4.3,65.1140714833514));
#192311=CARTESIAN_POINT('',(111.427841658067,-4.3,64.8022542995263));
#192312=CARTESIAN_POINT('Origin',(116.959178380441,-4.3,51.0204257716897));
#192313=CARTESIAN_POINT('Origin',(116.959178380441,-4.3,51.0204257716897));
#192314=CARTESIAN_POINT('Origin',(111.775808773449,-4.3,63.0121276118898));
#192315=CARTESIAN_POINT('Origin',(114.210622766164,1.45439216225896E-14,
50.4861580155739));
#192316=CARTESIAN_POINT('Origin',(114.210622766164,1.45439216225896E-14,
50.4861580155739));
#192317=CARTESIAN_POINT('Origin',(110.79418176835,-4.8,62.8213176989913));
#192318=CARTESIAN_POINT('',(110.987197567482,-4.8,64.4487513812576));
#192319=CARTESIAN_POINT('',(110.925497707532,-4.8,64.7661680595466));
#192320=CARTESIAN_POINT('',(110.987197567482,-4.8,64.4487513812576));
#192321=CARTESIAN_POINT('',(110.520136816659,-4.8,64.2311497203179));
#192322=CARTESIAN_POINT('Origin',(116.959178380441,-4.8,51.0204257716897));
#192323=CARTESIAN_POINT('',(110.457908037569,-4.8,64.5512874381168));
#192324=CARTESIAN_POINT('',(110.520136816659,-4.8,64.2311497203179));
#192325=CARTESIAN_POINT('Origin',(116.959178380441,-4.8,51.0204257716897));
#192326=CARTESIAN_POINT('Origin',(111.284995270899,-4.8,62.9167226554405));
#192327=CARTESIAN_POINT('',(110.957052487158,-4.3,64.6038336013966));
#192328=CARTESIAN_POINT('',(110.896011219052,-4.3,64.917862135278));
#192329=CARTESIAN_POINT('',(110.957052487158,-4.3,64.6038336013966));
#192330=CARTESIAN_POINT('Origin',(113.719809263614,1.45439216225896E-14,
50.3907530591246));
#192331=CARTESIAN_POINT('Origin',(113.719809263614,1.45439216225896E-14,
50.3907530591246));
#192332=CARTESIAN_POINT('Origin',(111.284995270899,-4.3,62.9167226554405));
#192333=CARTESIAN_POINT('',(110.489730329475,-4.3,64.3875767554558));
#192334=CARTESIAN_POINT('',(110.428177042311,-4.3,64.7042393858979));
#192335=CARTESIAN_POINT('',(110.489730329475,-4.3,64.3875767554558));
#192336=CARTESIAN_POINT('Origin',(116.959178380441,-4.3,51.0204257716897));
#192337=CARTESIAN_POINT('Origin',(116.959178380441,-4.3,51.0204257716897));
#192338=CARTESIAN_POINT('Origin',(110.79418176835,-4.3,62.8213176989913));
#192339=CARTESIAN_POINT('Origin',(113.228995761065,1.45439216225896E-14,
50.2953481026754));
#192340=CARTESIAN_POINT('Origin',(113.228995761065,1.45439216225896E-14,
50.2953481026754));
#192341=CARTESIAN_POINT('Origin',(109.812554763251,-4.8,62.6305077860928));
#192342=CARTESIAN_POINT('',(110.056678451302,-4.8,63.9950154852452));
#192343=CARTESIAN_POINT('',(109.993829318619,-4.8,64.3183446296844));
#192344=CARTESIAN_POINT('',(110.056678451302,-4.8,63.9950154852452));
#192345=CARTESIAN_POINT('',(109.596934009723,-4.8,63.7397748640298));
#192346=CARTESIAN_POINT('Origin',(116.959178380441,-4.8,51.0204257716897));
#192347=CARTESIAN_POINT('',(109.533365304474,-4.8,64.0668058699322));
#192348=CARTESIAN_POINT('',(109.596934009723,-4.8,63.7397748640298));
#192349=CARTESIAN_POINT('Origin',(116.959178380441,-4.8,51.0204257716897));
#192350=CARTESIAN_POINT('Origin',(110.3033682658,-4.8,62.725912742542));
#192351=CARTESIAN_POINT('',(110.025965270125,-4.3,64.1530203163257));
#192352=CARTESIAN_POINT('',(109.963811810516,-4.3,64.4727705509212));
#192353=CARTESIAN_POINT('',(110.025965270125,-4.3,64.1530203163257));
#192354=CARTESIAN_POINT('Origin',(112.738182258515,1.45439216225896E-14,
50.1999431462261));
#192355=CARTESIAN_POINT('Origin',(112.738182258515,1.45439216225896E-14,
50.1999431462261));
#192356=CARTESIAN_POINT('Origin',(110.3033682658,-4.3,62.725912742542));
#192357=CARTESIAN_POINT('',(109.565864948752,-4.3,63.8996105287959));
#192358=CARTESIAN_POINT('',(109.50301581607,-4.3,64.2229396732352));
#192359=CARTESIAN_POINT('',(109.565864948752,-4.3,63.8996105287959));
#192360=CARTESIAN_POINT('Origin',(116.959178380441,-4.3,51.0204257716897));
#192361=CARTESIAN_POINT('Origin',(116.959178380441,-4.3,51.0204257716897));
#192362=CARTESIAN_POINT('Origin',(109.812554763251,-4.3,62.6305077860928));
#192363=CARTESIAN_POINT('Origin',(112.247368755966,1.45439216225896E-14,
50.1045381897769));
#192364=CARTESIAN_POINT('Origin',(112.247368755966,1.45439216225896E-14,
50.1045381897769));
#192365=CARTESIAN_POINT('Origin',(109.812554763251,-3.8,62.6305077860928));
#192366=CARTESIAN_POINT('',(109.998916826926,-3.8,64.2921717990066));
#192367=CARTESIAN_POINT('',(109.937363539761,-3.8,64.6088344294486));
#192368=CARTESIAN_POINT('',(109.998916826926,-3.8,64.2921717990066));
#192369=CARTESIAN_POINT('',(109.53850981156,-3.8,64.0403398074194));
#192370=CARTESIAN_POINT('Origin',(116.959178380441,-3.8,51.0204257716897));
#192371=CARTESIAN_POINT('',(109.47628103247,-3.8,64.3604775252183));
#192372=CARTESIAN_POINT('',(109.53850981156,-3.8,64.0403398074194));
#192373=CARTESIAN_POINT('Origin',(116.959178380441,-3.8,51.0204257716897));
#192374=CARTESIAN_POINT('Origin',(110.3033682658,-3.8,62.725912742542));
#192375=CARTESIAN_POINT('',(109.975425482059,-3.3,64.4130236884981));
#192376=CARTESIAN_POINT('',(109.914384213953,-3.3,64.7270522223795));
#192377=CARTESIAN_POINT('',(109.975425482059,-3.3,64.4130236884981));
#192378=CARTESIAN_POINT('Origin',(112.738182258515,1.45439216225896E-14,
50.1999431462261));
#192379=CARTESIAN_POINT('Origin',(112.738182258515,1.45439216225896E-14,
50.1999431462261));
#192380=CARTESIAN_POINT('Origin',(110.3033682658,-3.3,62.725912742542));
#192381=CARTESIAN_POINT('',(109.514757059833,-3.3,64.1625365119099));
#192382=CARTESIAN_POINT('',(109.453057199884,-3.3,64.4799531901988));
#192383=CARTESIAN_POINT('',(109.514757059833,-3.3,64.1625365119099));
#192384=CARTESIAN_POINT('Origin',(116.959178380441,-3.3,51.0204257716897));
#192385=CARTESIAN_POINT('Origin',(116.959178380441,-3.3,51.0204257716897));
#192386=CARTESIAN_POINT('Origin',(109.812554763251,-3.3,62.6305077860928));
#192387=CARTESIAN_POINT('Origin',(112.247368755966,1.45439216225896E-14,
50.1045381897769));
#192388=CARTESIAN_POINT('Origin',(112.247368755966,1.45439216225896E-14,
50.1045381897769));
#192389=CARTESIAN_POINT('Origin',(109.812554763251,-2.8,62.6305077860928));
#192390=CARTESIAN_POINT('',(109.955401150418,-2.8,64.5160394301785));
#192391=CARTESIAN_POINT('',(109.894789727366,-2.8,64.8278566140037));
#192392=CARTESIAN_POINT('',(109.955401150418,-2.8,64.5160394301785));
#192393=CARTESIAN_POINT('',(109.494513443465,-2.8,64.2666803700892));
#192394=CARTESIAN_POINT('Origin',(116.959178380441,-2.8,51.0204257716897));
#192395=CARTESIAN_POINT('',(109.433257393177,-2.8,64.5818138569973));
#192396=CARTESIAN_POINT('',(109.494513443465,-2.8,64.2666803700892));
#192397=CARTESIAN_POINT('Origin',(116.959178380441,-2.8,51.0204257716897));
#192398=CARTESIAN_POINT('Origin',(110.3033682658,-2.8,62.725912742542));
#192399=CARTESIAN_POINT('',(109.93876943189,-2.3,64.6016017775467));
#192400=CARTESIAN_POINT('',(109.878510500343,-2.3,64.9116055588297));
#192401=CARTESIAN_POINT('',(109.93876943189,-2.3,64.6016017775467));
#192402=CARTESIAN_POINT('Origin',(112.738182258515,1.45439216225896E-14,
50.1999431462261));
#192403=CARTESIAN_POINT('Origin',(112.738182258515,1.45439216225896E-14,
50.1999431462261));
#192404=CARTESIAN_POINT('Origin',(110.3033682658,-2.3,62.725912742542));
#192405=CARTESIAN_POINT('',(109.477702016111,-2.3,64.3531672346009));
#192406=CARTESIAN_POINT('',(109.416809758086,-2.3,64.6664291819013));
#192407=CARTESIAN_POINT('',(109.477702016111,-2.3,64.3531672346009));
#192408=CARTESIAN_POINT('Origin',(116.959178380441,-2.3,51.0204257716897));
#192409=CARTESIAN_POINT('Origin',(116.959178380441,-2.3,51.0204257716897));
#192410=CARTESIAN_POINT('Origin',(109.812554763251,-2.3,62.6305077860928));
#192411=CARTESIAN_POINT('Origin',(112.247368755966,1.45439216225896E-14,
50.1045381897769));
#192412=CARTESIAN_POINT('Origin',(112.247368755966,1.45439216225896E-14,
50.1045381897769));
#192413=CARTESIAN_POINT('Origin',(109.812554763251,-1.8,62.6305077860928));
#192414=CARTESIAN_POINT('',(109.925470143716,-1.8,64.6700203425037));
#192415=CARTESIAN_POINT('',(109.865490170707,-1.8,64.9785890136804));
#192416=CARTESIAN_POINT('',(109.925470143716,-1.8,64.6700203425037));
#192417=CARTESIAN_POINT('',(109.464260580431,-1.8,64.4223170814327));
#192418=CARTESIAN_POINT('Origin',(116.959178380441,-1.8,51.0204257716897));
#192419=CARTESIAN_POINT('',(109.403656128548,-1.8,64.7340984018784));
#192420=CARTESIAN_POINT('',(109.464260580431,-1.8,64.4223170814327));
#192421=CARTESIAN_POINT('Origin',(116.959178380441,-1.8,51.0204257716897));
#192422=CARTESIAN_POINT('Origin',(110.3033682658,-1.8,62.725912742542));
#192423=CARTESIAN_POINT('',(109.915456183216,-1.3,64.7215374461251));
#192424=CARTESIAN_POINT('',(109.855684576506,-1.3,65.0290341709726));
#192425=CARTESIAN_POINT('',(109.915456183216,-1.3,64.7215374461251));
#192426=CARTESIAN_POINT('Origin',(112.738182258515,1.45439216225896E-14,
50.1999431462261));
#192427=CARTESIAN_POINT('Origin',(112.738182258515,1.45439216225896E-14,
50.1999431462261));
#192428=CARTESIAN_POINT('Origin',(110.3033682658,-1.3,62.725912742542));
#192429=CARTESIAN_POINT('',(109.454140485281,-1.3,64.4743801977696));
#192430=CARTESIAN_POINT('',(109.39375095346,-1.3,64.7850558558649));
#192431=CARTESIAN_POINT('',(109.454140485281,-1.3,64.4743801977696));
#192432=CARTESIAN_POINT('Origin',(116.959178380441,-1.3,51.0204257716897));
#192433=CARTESIAN_POINT('Origin',(116.959178380441,-1.3,51.0204257716897));
#192434=CARTESIAN_POINT('Origin',(109.812554763251,-1.3,62.6305077860928));
#192435=CARTESIAN_POINT('Origin',(112.247368755966,1.45439216225896E-14,
50.1045381897769));
#192436=CARTESIAN_POINT('Origin',(112.247368755966,1.45439216225896E-14,
50.1045381897769));
#192437=CARTESIAN_POINT('Origin',(109.812554763251,-0.799999999999986,62.6305077860928));
#192438=CARTESIAN_POINT('',(109.90869266847,-0.799999999999986,64.7563325394375));
#192439=CARTESIAN_POINT('',(109.849060985396,-0.799999999999986,65.0631094231747));
#192440=CARTESIAN_POINT('',(109.90869266847,-0.799999999999986,64.7563325394375));
#192441=CARTESIAN_POINT('',(109.447305718076,-0.799999999999986,64.509541851377));
#192442=CARTESIAN_POINT('Origin',(116.959178380441,-0.799999999999986,51.0204257716897));
#192443=CARTESIAN_POINT('',(109.387060484681,-0.799999999999986,64.8194751621284));
#192444=CARTESIAN_POINT('',(109.447305718076,-0.799999999999986,64.509541851377));
#192445=CARTESIAN_POINT('Origin',(116.959178380441,-0.799999999999986,51.0204257716897));
#192446=CARTESIAN_POINT('Origin',(110.3033682658,-0.799999999999986,62.725912742542));
#192447=CARTESIAN_POINT('',(109.905156319214,-0.299999999999985,64.7745253884155));
#192448=CARTESIAN_POINT('',(109.845597538345,-0.299999999999985,65.0809272246911));
#192449=CARTESIAN_POINT('',(109.905156319214,-0.299999999999985,64.7745253884155));
#192450=CARTESIAN_POINT('Origin',(112.738182258515,1.45439216225896E-14,
50.1999431462261));
#192451=CARTESIAN_POINT('Origin',(112.738182258515,1.45439216225896E-14,
50.1999431462261));
#192452=CARTESIAN_POINT('Origin',(110.3033682658,-0.299999999999985,62.725912742542));
#192453=CARTESIAN_POINT('',(109.443732251579,-0.299999999999985,64.5279256510537));
#192454=CARTESIAN_POINT('',(109.383562191382,-0.299999999999985,64.8374722311563));
#192455=CARTESIAN_POINT('',(109.443732251579,-0.299999999999985,64.5279256510537));
#192456=CARTESIAN_POINT('Origin',(116.959178380441,-0.299999999999985,51.0204257716897));
#192457=CARTESIAN_POINT('Origin',(116.959178380441,-0.299999999999985,51.0204257716897));
#192458=CARTESIAN_POINT('Origin',(109.812554763251,-0.299999999999985,62.6305077860928));
#192459=CARTESIAN_POINT('Origin',(112.247368755966,1.45439216225896E-14,
50.1045381897769));
#192460=CARTESIAN_POINT('Origin',(112.247368755966,1.45439216225896E-14,
50.1045381897769));
#192461=CARTESIAN_POINT('Origin',(119.628824814241,-0.799999999999986,64.5386069150778));
#192462=CARTESIAN_POINT('',(119.816516331414,-0.799999999999986,66.1934315167906));
#192463=CARTESIAN_POINT('',(119.754933813274,-0.799999999999986,66.5102445268161));
#192464=CARTESIAN_POINT('',(119.816516331414,-0.799999999999986,66.1934315167906));
#192465=CARTESIAN_POINT('',(119.289703096684,-0.799999999999986,66.283228202894));
#192466=CARTESIAN_POINT('Origin',(116.959178380441,-0.799999999999986,51.0204257716897));
#192467=CARTESIAN_POINT('',(119.228902537858,-0.799999999999986,66.5960184010664));
#192468=CARTESIAN_POINT('',(119.289703096684,-0.799999999999986,66.283228202894));
#192469=CARTESIAN_POINT('Origin',(116.959178380441,-0.799999999999986,51.0204257716897));
#192470=CARTESIAN_POINT('Origin',(120.11963831679,-0.799999999999986,64.6340118715271));
#192471=CARTESIAN_POINT('',(119.812861885554,-0.299999999999985,66.2122319170934));
#192472=CARTESIAN_POINT('',(119.751359652578,-0.299999999999985,66.5286318978187));
#192473=CARTESIAN_POINT('',(119.812861885554,-0.299999999999985,66.2122319170934));
#192474=CARTESIAN_POINT('Origin',(122.554452309506,1.45439216225896E-14,
52.1080422752111));
#192475=CARTESIAN_POINT('Origin',(122.554452309506,1.45439216225896E-14,
52.1080422752111));
#192476=CARTESIAN_POINT('Origin',(120.11963831679,-0.299999999999985,64.6340118715271));
#192477=CARTESIAN_POINT('',(119.286096015694,-0.299999999999985,66.3017849332873));
#192478=CARTESIAN_POINT('',(119.225372725718,-0.299999999999985,66.6141776196701));
#192479=CARTESIAN_POINT('',(119.286096015694,-0.299999999999985,66.3017849332873));
#192480=CARTESIAN_POINT('Origin',(116.959178380441,-0.299999999999985,51.0204257716897));
#192481=CARTESIAN_POINT('Origin',(116.959178380441,-0.299999999999985,51.0204257716897));
#192482=CARTESIAN_POINT('Origin',(119.628824814241,-0.299999999999985,64.5386069150778));
#192483=CARTESIAN_POINT('Origin',(122.063638806956,1.45439216225896E-14,
52.0126373187619));
#192484=CARTESIAN_POINT('Origin',(122.063638806956,1.45439216225896E-14,
52.0126373187619));
#192485=CARTESIAN_POINT('Origin',(119.628824814241,-1.8,64.5386069150778));
#192486=CARTESIAN_POINT('',(119.833858344817,-1.8,66.104215037305));
#192487=CARTESIAN_POINT('',(119.771891993661,-1.8,66.4230026871635));
#192488=CARTESIAN_POINT('',(119.833858344817,-1.8,66.104215037305));
#192489=CARTESIAN_POINT('',(119.306818641387,-1.8,66.195176798056));
#192490=CARTESIAN_POINT('Origin',(116.959178380441,-1.8,51.0204257716897));
#192491=CARTESIAN_POINT('',(119.245648775764,-1.8,66.5098669055141));
#192492=CARTESIAN_POINT('',(119.306818641387,-1.8,66.195176798056));
#192493=CARTESIAN_POINT('Origin',(116.959178380441,-1.8,51.0204257716897));
#192494=CARTESIAN_POINT('Origin',(120.11963831679,-1.8,64.6340118715271));
#192495=CARTESIAN_POINT('',(119.823506580252,-1.3,66.1574699835151));
#192496=CARTESIAN_POINT('',(119.761769913181,-1.3,66.475076017084));
#192497=CARTESIAN_POINT('',(119.823506580252,-1.3,66.1574699835151));
#192498=CARTESIAN_POINT('Origin',(122.554452309506,1.45439216225896E-14,
52.1080422752111));
#192499=CARTESIAN_POINT('Origin',(122.554452309506,1.45439216225896E-14,
52.1080422752111));
#192500=CARTESIAN_POINT('Origin',(120.11963831679,-1.3,64.6340118715271));
#192501=CARTESIAN_POINT('',(119.296602399404,-1.3,66.2477345445005));
#192502=CARTESIAN_POINT('',(119.235653504425,-1.3,66.5612878622158));
#192503=CARTESIAN_POINT('',(119.296602399404,-1.3,66.2477345445005));
#192504=CARTESIAN_POINT('Origin',(116.959178380441,-1.3,51.0204257716897));
#192505=CARTESIAN_POINT('Origin',(116.959178380441,-1.3,51.0204257716897));
#192506=CARTESIAN_POINT('Origin',(119.628824814241,-1.3,64.5386069150778));
#192507=CARTESIAN_POINT('Origin',(122.063638806956,1.45439216225896E-14,
52.0126373187619));
#192508=CARTESIAN_POINT('Origin',(122.063638806956,1.45439216225896E-14,
52.0126373187619));
#192509=CARTESIAN_POINT('Origin',(119.628824814241,-2.8,64.5386069150778));
#192510=CARTESIAN_POINT('',(119.86481427149,-2.8,65.9449613951417));
#192511=CARTESIAN_POINT('',(119.802150878674,-2.8,66.2673349955735));
#192512=CARTESIAN_POINT('',(119.86481427149,-2.8,65.9449613951417));
#192513=CARTESIAN_POINT('',(119.33736320091,-2.8,66.0380394458573));
#192514=CARTESIAN_POINT('Origin',(116.959178380441,-2.8,51.0204257716897));
#192515=CARTESIAN_POINT('',(119.27552312235,-2.8,66.3561774827635));
#192516=CARTESIAN_POINT('',(119.33736320091,-2.8,66.0380394458573));
#192517=CARTESIAN_POINT('Origin',(116.959178380441,-2.8,51.0204257716897));
#192518=CARTESIAN_POINT('Origin',(120.11963831679,-2.8,64.6340118715271));
#192519=CARTESIAN_POINT('',(119.847610191126,-2.3,66.0334682741935));
#192520=CARTESIAN_POINT('',(119.78533608868,-2.3,66.3538391592881));
#192521=CARTESIAN_POINT('',(119.847610191126,-2.3,66.0334682741935));
#192522=CARTESIAN_POINT('Origin',(122.554452309506,1.45439216225896E-14,
52.1080422752111));
#192523=CARTESIAN_POINT('Origin',(122.554452309506,1.45439216225896E-14,
52.1080422752111));
#192524=CARTESIAN_POINT('Origin',(120.11963831679,-2.3,64.6340118715271));
#192525=CARTESIAN_POINT('',(119.320388880605,-2.3,66.1253643177749));
#192526=CARTESIAN_POINT('',(119.258923037214,-2.3,66.4415770912459));
#192527=CARTESIAN_POINT('',(119.320388880605,-2.3,66.1253643177749));
#192528=CARTESIAN_POINT('Origin',(116.959178380441,-2.3,51.0204257716897));
#192529=CARTESIAN_POINT('Origin',(116.959178380441,-2.3,51.0204257716897));
#192530=CARTESIAN_POINT('Origin',(119.628824814241,-2.3,64.5386069150778));
#192531=CARTESIAN_POINT('Origin',(122.063638806956,1.45439216225896E-14,
52.0126373187619));
#192532=CARTESIAN_POINT('Origin',(122.063638806956,1.45439216225896E-14,
52.0126373187619));
#192533=CARTESIAN_POINT('Origin',(119.628824814241,-3.8,64.5386069150778));
#192534=CARTESIAN_POINT('',(119.909862136217,-3.8,65.7132113782478));
#192535=CARTESIAN_POINT('',(119.846156244582,-3.8,66.0409481433989));
#192536=CARTESIAN_POINT('',(119.909862136217,-3.8,65.7132113782478));
#192537=CARTESIAN_POINT('',(119.381795580881,-3.8,65.8094558077318));
#192538=CARTESIAN_POINT('Origin',(116.959178380441,-3.8,51.0204257716897));
#192539=CARTESIAN_POINT('',(119.318954220366,-3.8,66.1327449680392));
#192540=CARTESIAN_POINT('',(119.381795580881,-3.8,65.8094558077318));
#192541=CARTESIAN_POINT('Origin',(116.959178380441,-3.8,51.0204257716897));
#192542=CARTESIAN_POINT('Origin',(120.11963831679,-3.8,64.6340118715271));
#192543=CARTESIAN_POINT('',(119.885537345366,-3.3,65.8383509542256));
#192544=CARTESIAN_POINT('',(119.822398599122,-3.3,66.163170023844));
#192545=CARTESIAN_POINT('',(119.885537345366,-3.3,65.8383509542256));
#192546=CARTESIAN_POINT('Origin',(122.554452309506,1.45439216225896E-14,
52.1080422752111));
#192547=CARTESIAN_POINT('Origin',(122.554452309506,1.45439216225896E-14,
52.1080422752111));
#192548=CARTESIAN_POINT('Origin',(120.11963831679,-3.3,64.6340118715271));
#192549=CARTESIAN_POINT('',(119.357805665315,-3.3,65.9328726083199));
#192550=CARTESIAN_POINT('',(119.295508864014,-3.3,66.2533602683127));
#192551=CARTESIAN_POINT('',(119.357805665315,-3.3,65.9328726083199));
#192552=CARTESIAN_POINT('Origin',(116.959178380441,-3.3,51.0204257716897));
#192553=CARTESIAN_POINT('Origin',(116.959178380441,-3.3,51.0204257716897));
#192554=CARTESIAN_POINT('Origin',(119.628824814241,-3.3,64.5386069150778));
#192555=CARTESIAN_POINT('Origin',(122.063638806956,1.45439216225896E-14,
52.0126373187619));
#192556=CARTESIAN_POINT('Origin',(122.063638806956,1.45439216225896E-14,
52.0126373187619));
#192557=CARTESIAN_POINT('Origin',(118.647197809142,-3.8,64.3477970021793));
#192558=CARTESIAN_POINT('',(118.857589627268,-3.8,65.8858392622321));
#192559=CARTESIAN_POINT('',(118.795503721835,-3.8,66.2052419624567));
#192560=CARTESIAN_POINT('',(118.857589627268,-3.8,65.8858392622321));
#192561=CARTESIAN_POINT('',(118.337103376402,-3.8,65.9430866005239));
#192562=CARTESIAN_POINT('Origin',(116.959178380441,-3.8,51.0204257716897));
#192563=CARTESIAN_POINT('',(118.275673858067,-3.8,66.2591124987171));
#192564=CARTESIAN_POINT('',(118.337103376402,-3.8,65.9430866005239));
#192565=CARTESIAN_POINT('Origin',(116.959178380441,-3.8,51.0204257716897));
#192566=CARTESIAN_POINT('Origin',(119.138011311691,-3.8,64.4432019586286));
#192567=CARTESIAN_POINT('',(118.833892175693,-3.3,66.0077514735275));
#192568=CARTESIAN_POINT('',(118.77233158469,-3.3,66.3244516787764));
#192569=CARTESIAN_POINT('',(118.833892175693,-3.3,66.0077514735275));
#192570=CARTESIAN_POINT('Origin',(121.572825304407,1.45439216225896E-14,
51.9172323623126));
#192571=CARTESIAN_POINT('Origin',(121.572825304407,1.45439216225896E-14,
51.9172323623126));
#192572=CARTESIAN_POINT('Origin',(119.138011311691,-3.3,64.4432019586286));
#192573=CARTESIAN_POINT('',(118.313659915754,-3.3,66.0636921482939));
#192574=CARTESIAN_POINT('',(118.252739359001,-3.3,66.3770996792034));
#192575=CARTESIAN_POINT('',(118.313659915754,-3.3,66.0636921482939));
#192576=CARTESIAN_POINT('Origin',(116.959178380441,-3.3,51.0204257716897));
#192577=CARTESIAN_POINT('Origin',(116.959178380441,-3.3,51.0204257716897));
#192578=CARTESIAN_POINT('Origin',(118.647197809142,-3.3,64.3477970021793));
#192579=CARTESIAN_POINT('Origin',(121.082011801857,1.45439216225896E-14,
51.8218274058634));
#192580=CARTESIAN_POINT('Origin',(121.082011801857,1.45439216225896E-14,
51.8218274058634));
#192581=CARTESIAN_POINT('Origin',(117.665570804043,-3.8,64.1569870892808));
#192582=CARTESIAN_POINT('',(117.820217329609,-3.8,65.9818125869175));
#192583=CARTESIAN_POINT('',(117.759353330908,-3.8,66.2949291533247));
#192584=CARTESIAN_POINT('',(117.820217329609,-3.8,65.9818125869175));
#192585=CARTESIAN_POINT('',(117.306830681782,-3.8,66.0025358161473));
#192586=CARTESIAN_POINT('Origin',(116.959178380441,-3.8,51.0204257716897));
#192587=CARTESIAN_POINT('',(117.246448044845,-3.8,66.3131760033177));
#192588=CARTESIAN_POINT('',(117.306830681782,-3.8,66.0025358161473));
#192589=CARTESIAN_POINT('Origin',(116.959178380441,-3.8,51.0204257716897));
#192590=CARTESIAN_POINT('Origin',(118.156384306592,-3.8,64.25239204573));
#192591=CARTESIAN_POINT('',(117.796992609744,-3.3,66.1012928165323));
#192592=CARTESIAN_POINT('',(117.736623755491,-3.3,66.4118620982908));
#192593=CARTESIAN_POINT('',(117.796992609744,-3.3,66.1012928165323));
#192594=CARTESIAN_POINT('Origin',(120.591198299308,1.45439216225896E-14,
51.7264224494141));
#192595=CARTESIAN_POINT('Origin',(120.591198299308,1.45439216225896E-14,
51.7264224494141));
#192596=CARTESIAN_POINT('Origin',(118.156384306592,-3.3,64.25239204573));
#192597=CARTESIAN_POINT('',(117.283792086681,-3.3,66.1210585216364));
#192598=CARTESIAN_POINT('',(117.223893029854,-3.3,66.4292109172233));
#192599=CARTESIAN_POINT('',(117.283792086681,-3.3,66.1210585216364));
#192600=CARTESIAN_POINT('Origin',(116.959178380441,-3.3,51.0204257716897));
#192601=CARTESIAN_POINT('Origin',(116.959178380441,-3.3,51.0204257716897));
#192602=CARTESIAN_POINT('Origin',(117.665570804043,-3.3,64.1569870892808));
#192603=CARTESIAN_POINT('Origin',(120.100384796758,1.45439216225896E-14,
51.6310174929649));
#192604=CARTESIAN_POINT('Origin',(120.100384796758,1.45439216225896E-14,
51.6310174929649));
#192605=CARTESIAN_POINT('Origin',(116.683943798944,-3.8,63.9661771763823));
#192606=CARTESIAN_POINT('',(116.796859179409,-3.8,66.0056897327932));
#192607=CARTESIAN_POINT('',(116.7368792064,-3.8,66.3142584039699));
#192608=CARTESIAN_POINT('',(116.796859179409,-3.8,66.0056897327932));
#192609=CARTESIAN_POINT('',(116.290233427834,-3.8,65.9916313396271));
#192610=CARTESIAN_POINT('Origin',(116.959178380441,-3.8,51.0204257716897));
#192611=CARTESIAN_POINT('',(116.230581815828,-3.8,66.2985107483171));
#192612=CARTESIAN_POINT('',(116.290233427834,-3.8,65.9916313396271));
#192613=CARTESIAN_POINT('Origin',(116.959178380441,-3.8,51.0204257716897));
#192614=CARTESIAN_POINT('Origin',(117.174757301493,-3.8,64.0615821328315));
#192615=CARTESIAN_POINT('',(116.773976234632,-3.3,66.1234116907773));
#192616=CARTESIAN_POINT('',(116.7144703059,-3.3,66.4295416277397));
#192617=CARTESIAN_POINT('',(116.773976234632,-3.3,66.1234116907773));
#192618=CARTESIAN_POINT('Origin',(119.609571294209,1.45439216225896E-14,
51.5356125365156));
#192619=CARTESIAN_POINT('Origin',(119.609571294209,1.45439216225896E-14,
51.5356125365156));
#192620=CARTESIAN_POINT('Origin',(117.174757301493,-3.3,64.0615821328315));
#192621=CARTESIAN_POINT('',(116.267477381404,-3.3,66.108700465472));
#192622=CARTESIAN_POINT('',(116.20829212986,-3.3,66.413180669547));
#192623=CARTESIAN_POINT('',(116.267477381404,-3.3,66.108700465472));
#192624=CARTESIAN_POINT('Origin',(116.959178380441,-3.3,51.0204257716897));
#192625=CARTESIAN_POINT('Origin',(116.959178380441,-3.3,51.0204257716897));
#192626=CARTESIAN_POINT('Origin',(116.683943798944,-3.3,63.9661771763823));
#192627=CARTESIAN_POINT('Origin',(119.118757791659,1.45439216225896E-14,
51.4402075800664));
#192628=CARTESIAN_POINT('Origin',(119.118757791659,1.45439216225896E-14,
51.4402075800664));
#192629=CARTESIAN_POINT('Origin',(115.702316793845,-3.8,63.7753672634838));
#192630=CARTESIAN_POINT('',(115.786897562756,-3.8,65.9606480321323));
#192631=CARTESIAN_POINT('',(115.727503479173,-3.8,66.2662025785505));
#192632=CARTESIAN_POINT('',(115.786897562756,-3.8,65.9606480321323));
#192633=CARTESIAN_POINT('',(115.286808223328,-3.8,65.9129628814135));
#192634=CARTESIAN_POINT('Origin',(116.959178380441,-3.8,51.0204257716897));
#192635=CARTESIAN_POINT('',(115.227603487308,-3.8,66.2175433239276));
#192636=CARTESIAN_POINT('',(115.286808223328,-3.8,65.9129628814135));
#192637=CARTESIAN_POINT('Origin',(116.959178380441,-3.8,51.0204257716897));
#192638=CARTESIAN_POINT('Origin',(116.193130296394,-3.8,63.870772219933));
#192639=CARTESIAN_POINT('',(115.764241021926,-3.3,66.0772052485936));
#192640=CARTESIAN_POINT('',(115.705307330283,-3.3,66.3803912956307));
#192641=CARTESIAN_POINT('',(115.764241021926,-3.3,66.0772052485936));
#192642=CARTESIAN_POINT('Origin',(118.62794428911,1.45439216225896E-14,
51.3448026236171));
#192643=CARTESIAN_POINT('Origin',(118.62794428911,1.45439216225896E-14,
51.3448026236171));
#192644=CARTESIAN_POINT('Origin',(116.193130296394,-3.3,63.870772219933));
#192645=CARTESIAN_POINT('',(115.264224833413,-3.3,66.0291437709213));
#192646=CARTESIAN_POINT('',(115.205476133255,-3.3,66.3313781240196));
#192647=CARTESIAN_POINT('',(115.264224833413,-3.3,66.0291437709213));
#192648=CARTESIAN_POINT('Origin',(116.959178380441,-3.3,51.0204257716897));
#192649=CARTESIAN_POINT('Origin',(116.959178380441,-3.3,51.0204257716897));
#192650=CARTESIAN_POINT('Origin',(115.702316793845,-3.3,63.7753672634838));
#192651=CARTESIAN_POINT('Origin',(118.13713078656,1.45439216225896E-14,
51.2493976671679));
#192652=CARTESIAN_POINT('Origin',(118.13713078656,1.45439216225896E-14,
51.2493976671679));
#192653=CARTESIAN_POINT('Origin',(114.720689788746,-3.8,63.5845573505853));
#192654=CARTESIAN_POINT('',(114.789933781015,-3.8,65.8487386013644));
#192655=CARTESIAN_POINT('',(114.730852122701,-3.8,66.1526858671318));
#192656=CARTESIAN_POINT('',(114.789933781015,-3.8,65.8487386013644));
#192657=CARTESIAN_POINT('',(114.296253791258,-3.8,65.7680803695982));
#192658=CARTESIAN_POINT('Origin',(116.959178380441,-3.8,51.0204257716897));
#192659=CARTESIAN_POINT('',(114.237230165589,-3.8,66.0717290847811));
#192660=CARTESIAN_POINT('',(114.296253791258,-3.8,65.7680803695982));
#192661=CARTESIAN_POINT('Origin',(116.959178380441,-3.8,51.0204257716897));
#192662=CARTESIAN_POINT('Origin',(115.211503291295,-3.8,63.6799623070345));
#192663=CARTESIAN_POINT('',(114.767397935133,-3.3,65.9646748992444));
#192664=CARTESIAN_POINT('',(114.70876949581,-3.3,66.2662905670707));
#192665=CARTESIAN_POINT('',(114.767397935133,-3.3,65.9646748992444));
#192666=CARTESIAN_POINT('Origin',(117.64631728401,1.45439216225896E-14,
51.1539927107186));
#192667=CARTESIAN_POINT('Origin',(117.64631728401,1.45439216225896E-14,
51.1539927107186));
#192668=CARTESIAN_POINT('Origin',(115.211503291295,-3.3,63.6799623070345));
#192669=CARTESIAN_POINT('',(114.273740361672,-3.3,65.8839013462125));
#192670=CARTESIAN_POINT('',(114.215168630795,-3.3,66.185225275828));
#192671=CARTESIAN_POINT('',(114.273740361672,-3.3,65.8839013462125));
#192672=CARTESIAN_POINT('Origin',(116.959178380441,-3.3,51.0204257716897));
#192673=CARTESIAN_POINT('Origin',(116.959178380441,-3.3,51.0204257716897));
#192674=CARTESIAN_POINT('Origin',(114.720689788746,-3.3,63.5845573505853));
#192675=CARTESIAN_POINT('Origin',(117.155503781461,1.45439216225896E-14,
51.0585877542694));
#192676=CARTESIAN_POINT('Origin',(117.155503781461,1.45439216225896E-14,
51.0585877542694));
#192677=CARTESIAN_POINT('Origin',(113.739062783647,-3.8,63.3937474376868));
#192678=CARTESIAN_POINT('',(113.805758645357,-3.8,65.6710376183478));
#192679=CARTESIAN_POINT('',(113.746728580063,-3.8,65.9747194623623));
#192680=CARTESIAN_POINT('',(113.805758645357,-3.8,65.6710376183478));
#192681=CARTESIAN_POINT('',(113.318449408565,-3.8,65.5576048673859));
#192682=CARTESIAN_POINT('Origin',(116.959178380441,-3.8,51.0204257716897));
#192683=CARTESIAN_POINT('',(113.259348367962,-3.8,65.8616518458919));
#192684=CARTESIAN_POINT('',(113.318449408565,-3.8,65.5576048673859));
#192685=CARTESIAN_POINT('Origin',(116.959178380441,-3.8,51.0204257716897));
#192686=CARTESIAN_POINT('Origin',(114.229876286196,-3.8,63.489152394136));
#192687=CARTESIAN_POINT('',(113.783242728376,-3.3,65.7868713914321));
#192688=CARTESIAN_POINT('',(113.724664704686,-3.3,66.0882276946056));
#192689=CARTESIAN_POINT('',(113.783242728376,-3.3,65.7868713914321));
#192690=CARTESIAN_POINT('Origin',(116.664690278911,1.45439216225896E-14,
50.9631827978201));
#192691=CARTESIAN_POINT('Origin',(116.664690278911,1.45439216225896E-14,
50.9631827978201));
#192692=CARTESIAN_POINT('Origin',(114.229876286196,-3.3,63.489152394136));
#192693=CARTESIAN_POINT('',(113.295906075692,-3.3,65.6735796823071));
#192694=CARTESIAN_POINT('',(113.237258696916,-3.3,65.9752927846826));
#192695=CARTESIAN_POINT('',(113.295906075692,-3.3,65.6735796823071));
#192696=CARTESIAN_POINT('Origin',(116.959178380441,-3.3,51.0204257716897));
#192697=CARTESIAN_POINT('Origin',(116.959178380441,-3.3,51.0204257716897));
#192698=CARTESIAN_POINT('Origin',(113.739062783647,-3.3,63.3937474376868));
#192699=CARTESIAN_POINT('Origin',(116.173876776362,1.45439216225896E-14,
50.8677778413709));
#192700=CARTESIAN_POINT('Origin',(116.173876776362,1.45439216225896E-14,
50.8677778413709));
#192701=CARTESIAN_POINT('Origin',(112.757435778548,-3.8,63.2029375247883));
#192702=CARTESIAN_POINT('',(112.834337837981,-3.8,65.4277216319878));
#192703=CARTESIAN_POINT('',(112.775100585027,-3.8,65.732469358792));
#192704=CARTESIAN_POINT('',(112.834337837981,-3.8,65.4277216319878));
#192705=CARTESIAN_POINT('',(112.353446580952,-3.8,65.2812714022259));
#192706=CARTESIAN_POINT('Origin',(116.959178380441,-3.8,51.0204257716897));
#192707=CARTESIAN_POINT('',(112.294006519922,-3.8,65.5870624809277));
#192708=CARTESIAN_POINT('',(112.353446580952,-3.8,65.2812714022259));
#192709=CARTESIAN_POINT('Origin',(116.959178380441,-3.8,51.0204257716897));
#192710=CARTESIAN_POINT('Origin',(113.248249281097,-3.8,63.2983424812375));
#192711=CARTESIAN_POINT('',(112.811741886383,-3.3,65.5439671454273));
#192712=CARTESIAN_POINT('',(112.752961415424,-3.3,65.8463649443104));
#192713=CARTESIAN_POINT('',(112.811741886383,-3.3,65.5439671454273));
#192714=CARTESIAN_POINT('Origin',(115.683063273812,1.45439216225896E-14,
50.7723728849216));
#192715=CARTESIAN_POINT('Origin',(115.683063273812,1.45439216225896E-14,
50.7723728849216));
#192716=CARTESIAN_POINT('Origin',(113.248249281097,-3.3,63.2983424812375));
#192717=CARTESIAN_POINT('',(112.330772276248,-3.3,65.3979200054423));
#192718=CARTESIAN_POINT('',(112.271793669026,-3.3,65.7013371219498));
#192719=CARTESIAN_POINT('',(112.330772276248,-3.3,65.3979200054423));
#192720=CARTESIAN_POINT('Origin',(116.959178380441,-3.3,51.0204257716897));
#192721=CARTESIAN_POINT('Origin',(116.959178380441,-3.3,51.0204257716897));
#192722=CARTESIAN_POINT('Origin',(112.757435778548,-3.3,63.2029375247883));
#192723=CARTESIAN_POINT('Origin',(115.192249771263,1.45439216225896E-14,
50.6769679284724));
#192724=CARTESIAN_POINT('Origin',(115.192249771263,1.45439216225896E-14,
50.6769679284724));
#192725=CARTESIAN_POINT('Origin',(111.775808773449,-3.8,63.0121276118898));
#192726=CARTESIAN_POINT('',(111.875809561864,-3.8,65.1180796531428));
#192727=CARTESIAN_POINT('',(111.816098042946,-3.8,65.425267254645));
#192728=CARTESIAN_POINT('',(111.875809561864,-3.8,65.1180796531428));
#192729=CARTESIAN_POINT('',(111.401472572927,-3.8,64.9379108054185));
#192730=CARTESIAN_POINT('Origin',(116.959178380441,-3.8,51.0204257716897));
#192731=CARTESIAN_POINT('',(111.341418137912,-3.8,65.2468625484944));
#192732=CARTESIAN_POINT('',(111.401472572927,-3.8,64.9379108054185));
#192733=CARTESIAN_POINT('Origin',(116.959178380441,-3.8,51.0204257716897));
#192734=CARTESIAN_POINT('Origin',(112.266622275998,-3.8,63.107532568339));
#192735=CARTESIAN_POINT('',(111.853030365824,-3.3,65.2352678728129));
#192736=CARTESIAN_POINT('',(111.79378660305,-3.3,65.5400490895696));
#192737=CARTESIAN_POINT('',(111.853030365824,-3.3,65.2352678728129));
#192738=CARTESIAN_POINT('Origin',(114.701436268713,1.45439216225896E-14,
50.5815629720231));
#192739=CARTESIAN_POINT('Origin',(114.701436268713,1.45439216225896E-14,
50.5815629720231));
#192740=CARTESIAN_POINT('Origin',(112.266622275998,-3.3,63.107532568339));
#192741=CARTESIAN_POINT('',(111.378560847823,-3.3,65.0557808246087));
#192742=CARTESIAN_POINT('',(111.318982211057,-3.3,65.3622848101095));
#192743=CARTESIAN_POINT('',(111.378560847823,-3.3,65.0557808246087));
#192744=CARTESIAN_POINT('Origin',(116.959178380441,-3.3,51.0204257716897));
#192745=CARTESIAN_POINT('Origin',(116.959178380441,-3.3,51.0204257716897));
#192746=CARTESIAN_POINT('Origin',(111.775808773449,-3.3,63.0121276118898));
#192747=CARTESIAN_POINT('Origin',(114.210622766164,1.45439216225896E-14,
50.4861580155739));
#192748=CARTESIAN_POINT('Origin',(114.210622766164,1.45439216225896E-14,
50.4861580155739));
#192749=CARTESIAN_POINT('Origin',(110.79418176835,-3.8,62.8213176989913));
#192750=CARTESIAN_POINT('',(110.930494093462,-3.8,64.7404640105189));
#192751=CARTESIAN_POINT('',(110.87002163836,-3.8,65.0515662697813));
#192752=CARTESIAN_POINT('',(110.930494093462,-3.8,64.7404640105189));
#192753=CARTESIAN_POINT('',(110.462946372987,-3.8,64.5253675787552));
#192754=CARTESIAN_POINT('Origin',(116.959178380441,-3.8,51.0204257716897));
#192755=CARTESIAN_POINT('',(110.401976198362,-3.8,64.8390303702136));
#192756=CARTESIAN_POINT('',(110.462946372987,-3.8,64.5253675787552));
#192757=CARTESIAN_POINT('Origin',(116.959178380441,-3.8,51.0204257716897));
#192758=CARTESIAN_POINT('Origin',(111.284995270899,-3.8,62.9167226554405));
#192759=CARTESIAN_POINT('',(110.907420773452,-3.3,64.8591653592831));
#192760=CARTESIAN_POINT('',(110.847434042615,-3.3,65.1677687963017));
#192761=CARTESIAN_POINT('',(110.907420773452,-3.3,64.8591653592831));
#192762=CARTESIAN_POINT('Origin',(113.719809263614,1.45439216225896E-14,
50.3907530591246));
#192763=CARTESIAN_POINT('Origin',(113.719809263614,1.45439216225896E-14,
50.3907530591246));
#192764=CARTESIAN_POINT('Origin',(111.284995270899,-3.3,62.9167226554405));
#192765=CARTESIAN_POINT('',(110.439680590912,-3.3,64.6450590540696));
#192766=CARTESIAN_POINT('',(110.379208135811,-3.3,64.956161313332));
#192767=CARTESIAN_POINT('',(110.439680590912,-3.3,64.6450590540696));
#192768=CARTESIAN_POINT('Origin',(116.959178380441,-3.3,51.0204257716897));
#192769=CARTESIAN_POINT('Origin',(116.959178380441,-3.3,51.0204257716897));
#192770=CARTESIAN_POINT('Origin',(110.79418176835,-3.3,62.8213176989913));
#192771=CARTESIAN_POINT('Origin',(113.228995761065,1.45439216225896E-14,
50.2953481026754));
#192772=CARTESIAN_POINT('Origin',(113.228995761065,1.45439216225896E-14,
50.2953481026754));
#192773=CARTESIAN_POINT('Origin',(110.79418176835,-2.8,62.8213176989913));
#192774=CARTESIAN_POINT('',(110.887747345274,-2.8,64.9603758681595));
#192775=CARTESIAN_POINT('',(110.828168708508,-2.8,65.2668798536603));
#192776=CARTESIAN_POINT('',(110.887747345274,-2.8,64.9603758681595));
#192777=CARTESIAN_POINT('',(110.419845567828,-2.8,64.74710089252));
#192778=CARTESIAN_POINT('Origin',(116.959178380441,-2.8,51.0204257716897));
#192779=CARTESIAN_POINT('',(110.359791132813,-2.8,65.0560526355959));
#192780=CARTESIAN_POINT('',(110.419845567828,-2.8,64.74710089252));
#192781=CARTESIAN_POINT('Origin',(116.959178380441,-2.8,51.0204257716897));
#192782=CARTESIAN_POINT('Origin',(111.284995270899,-2.8,62.9167226554405));
#192783=CARTESIAN_POINT('',(110.871403360725,-2.3,65.0444579599144));
#192784=CARTESIAN_POINT('',(110.812159597951,-2.3,65.3492391766711));
#192785=CARTESIAN_POINT('',(110.871403360725,-2.3,65.0444579599144));
#192786=CARTESIAN_POINT('Origin',(113.719809263614,1.45439216225896E-14,
50.3907530591246));
#192787=CARTESIAN_POINT('Origin',(113.719809263614,1.45439216225896E-14,
50.3907530591246));
#192788=CARTESIAN_POINT('Origin',(111.284995270899,-2.3,62.9167226554405));
#192789=CARTESIAN_POINT('',(110.403369054216,-2.3,64.8318647837951));
#192790=CARTESIAN_POINT('',(110.343657535297,-2.3,65.1390523852972));
#192791=CARTESIAN_POINT('',(110.403369054216,-2.3,64.8318647837951));
#192792=CARTESIAN_POINT('Origin',(116.959178380441,-2.3,51.0204257716897));
#192793=CARTESIAN_POINT('Origin',(116.959178380441,-2.3,51.0204257716897));
#192794=CARTESIAN_POINT('Origin',(110.79418176835,-2.3,62.8213176989913));
#192795=CARTESIAN_POINT('Origin',(113.228995761065,1.45439216225896E-14,
50.2953481026754));
#192796=CARTESIAN_POINT('Origin',(113.228995761065,1.45439216225896E-14,
50.2953481026754));
#192797=CARTESIAN_POINT('Origin',(110.79418176835,-1.8,62.8213176989913));
#192798=CARTESIAN_POINT('',(110.8583317686,-1.8,65.1117051360946));
#192799=CARTESIAN_POINT('',(110.799353161377,-1.8,65.4151222526021));
#192800=CARTESIAN_POINT('',(110.8583317686,-1.8,65.1117051360946));
#192801=CARTESIAN_POINT('',(110.390192570754,-1.8,64.8996515764289));
#192802=CARTESIAN_POINT('Origin',(116.959178380441,-1.8,51.0204257716897));
#192803=CARTESIAN_POINT('',(110.330752509724,-1.8,65.2054426551307));
#192804=CARTESIAN_POINT('',(110.390192570754,-1.8,64.8996515764289));
#192805=CARTESIAN_POINT('Origin',(116.959178380441,-1.8,51.0204257716897));
#192806=CARTESIAN_POINT('Origin',(111.284995270899,-1.8,62.9167226554405));
#192807=CARTESIAN_POINT('',(110.848487876185,-1.3,65.1623473196303));
#192808=CARTESIAN_POINT('',(110.789707405226,-1.3,65.4647451185134));
#192809=CARTESIAN_POINT('',(110.848487876185,-1.3,65.1623473196303));
#192810=CARTESIAN_POINT('Origin',(113.719809263614,1.45439216225896E-14,
50.3907530591246));
#192811=CARTESIAN_POINT('Origin',(113.719809263614,1.45439216225896E-14,
50.3907530591246));
#192812=CARTESIAN_POINT('Origin',(111.284995270899,-1.3,62.9167226554405));
#192813=CARTESIAN_POINT('',(110.380270325233,-1.3,64.9506968497415));
#192814=CARTESIAN_POINT('',(110.321033072279,-1.3,65.2554445765457));
#192815=CARTESIAN_POINT('',(110.380270325233,-1.3,64.9506968497415));
#192816=CARTESIAN_POINT('Origin',(116.959178380441,-1.3,51.0204257716897));
#192817=CARTESIAN_POINT('Origin',(116.959178380441,-1.3,51.0204257716897));
#192818=CARTESIAN_POINT('Origin',(110.79418176835,-1.3,62.8213176989913));
#192819=CARTESIAN_POINT('Origin',(113.228995761065,1.45439216225896E-14,
50.2953481026754));
#192820=CARTESIAN_POINT('Origin',(113.228995761065,1.45439216225896E-14,
50.2953481026754));
#192821=CARTESIAN_POINT('Origin',(111.284995270899,-0.799999999999986,62.9167226554405));
#192822=CARTESIAN_POINT('',(110.838361713079,-0.299999999999985,65.2144416527366));
#192823=CARTESIAN_POINT('',(110.779783689389,-0.299999999999985,65.51579795591));
#192824=CARTESIAN_POINT('',(110.838361713079,-0.299999999999985,65.2144416527366));
#192825=CARTESIAN_POINT('',(110.841838562944,-0.799999999999986,65.1965549000608));
#192826=CARTESIAN_POINT('Origin',(113.719809263614,1.45439216225896E-14,
50.3907530591246));
#192827=CARTESIAN_POINT('',(110.783191184168,-0.799999999999986,65.4982680024364));
#192828=CARTESIAN_POINT('',(110.841838562944,-0.799999999999986,65.1965549000608));
#192829=CARTESIAN_POINT('Origin',(113.719809263614,1.45439216225896E-14,
50.3907530591246));
#192830=CARTESIAN_POINT('Origin',(111.284995270899,-0.299999999999985,62.9167226554405));
#192831=CARTESIAN_POINT('',(110.370064127511,-0.299999999999985,65.003202923203));
#192832=CARTESIAN_POINT('',(110.311034062217,-0.299999999999985,65.3068847672175));
#192833=CARTESIAN_POINT('',(110.370064127511,-0.299999999999985,65.003202923203));
#192834=CARTESIAN_POINT('Origin',(116.959178380441,-0.299999999999985,51.0204257716897));
#192835=CARTESIAN_POINT('Origin',(116.959178380441,-0.299999999999985,51.0204257716897));
#192836=CARTESIAN_POINT('Origin',(110.79418176835,-0.299999999999985,62.8213176989913));
#192837=CARTESIAN_POINT('',(110.373568393268,-0.799999999999986,64.9851751286904));
#192838=CARTESIAN_POINT('',(110.314467352665,-0.799999999999986,65.2892221071964));
#192839=CARTESIAN_POINT('',(110.373568393268,-0.799999999999986,64.9851751286904));
#192840=CARTESIAN_POINT('Origin',(113.228995761065,1.45439216225896E-14,
50.2953481026754));
#192841=CARTESIAN_POINT('Origin',(113.228995761065,1.45439216225896E-14,
50.2953481026754));
#192842=CARTESIAN_POINT('Origin',(110.79418176835,-0.799999999999986,62.8213176989913));
#192843=CARTESIAN_POINT('Origin',(116.959178380441,-0.799999999999986,51.0204257716897));
#192844=CARTESIAN_POINT('Origin',(116.959178380441,-0.799999999999986,51.0204257716897));
#192845=CARTESIAN_POINT('Origin',(118.647197809142,-0.799999999999986,64.3477970021793));
#192846=CARTESIAN_POINT('',(118.766592773437,-0.799999999999986,66.3539751559262));
#192847=CARTESIAN_POINT('',(118.706477208223,-0.799999999999986,66.6632413850446));
#192848=CARTESIAN_POINT('',(118.766592773437,-0.799999999999986,66.3539751559262));
#192849=CARTESIAN_POINT('',(118.247058804081,-0.799999999999986,66.4063234549974));
#192850=CARTESIAN_POINT('Origin',(116.959178380441,-0.799999999999986,51.0204257716897));
#192851=CARTESIAN_POINT('',(118.187539675506,-0.799999999999986,66.7125212989234));
#192852=CARTESIAN_POINT('',(118.247058804081,-0.799999999999986,66.4063234549974));
#192853=CARTESIAN_POINT('Origin',(116.959178380441,-0.799999999999986,51.0204257716897));
#192854=CARTESIAN_POINT('Origin',(119.138011311691,-0.799999999999986,64.4432019586286));
#192855=CARTESIAN_POINT('',(118.763027153213,-0.299999999999985,66.3723185902268));
#192856=CARTESIAN_POINT('',(118.702986277376,-0.299999999999985,66.6812005777294));
#192857=CARTESIAN_POINT('',(118.763027153213,-0.299999999999985,66.3723185902268));
#192858=CARTESIAN_POINT('Origin',(121.572825304407,1.45439216225896E-14,
51.9172323623126));
#192859=CARTESIAN_POINT('Origin',(121.572825304407,1.45439216225896E-14,
51.9172323623126));
#192860=CARTESIAN_POINT('Origin',(119.138011311691,-0.299999999999985,64.4432019586286));
#192861=CARTESIAN_POINT('',(118.243529261453,-0.299999999999985,66.4244812870825));
#192862=CARTESIAN_POINT('',(118.184082623495,-0.299999999999985,66.7303062009751));
#192863=CARTESIAN_POINT('',(118.243529261453,-0.299999999999985,66.4244812870825));
#192864=CARTESIAN_POINT('Origin',(116.959178380441,-0.299999999999985,51.0204257716897));
#192865=CARTESIAN_POINT('Origin',(116.959178380441,-0.299999999999985,51.0204257716897));
#192866=CARTESIAN_POINT('Origin',(118.647197809142,-0.299999999999985,64.3477970021793));
#192867=CARTESIAN_POINT('Origin',(121.082011801857,1.45439216225896E-14,
51.8218274058634));
#192868=CARTESIAN_POINT('Origin',(121.082011801857,1.45439216225896E-14,
51.8218274058634));
#192869=CARTESIAN_POINT('Origin',(118.647197809142,-1.8,64.3477970021793));
#192870=CARTESIAN_POINT('',(118.783510134254,-1.8,66.2669433137069));
#192871=CARTESIAN_POINT('',(118.723037679152,-1.8,66.5780455729693));
#192872=CARTESIAN_POINT('',(118.783510134254,-1.8,66.2669433137069));
#192873=CARTESIAN_POINT('',(118.263803754148,-1.8,66.3201785847698));
#192874=CARTESIAN_POINT('Origin',(116.959178380441,-1.8,51.0204257716897));
#192875=CARTESIAN_POINT('',(118.203938315861,-1.8,66.6281580288199));
#192876=CARTESIAN_POINT('',(118.263803754148,-1.8,66.3201785847698));
#192877=CARTESIAN_POINT('Origin',(116.959178380441,-1.8,51.0204257716897));
#192878=CARTESIAN_POINT('Origin',(119.138011311691,-1.8,64.4432019586286));
#192879=CARTESIAN_POINT('',(118.773412477781,-1.3,66.3188909936332));
#192880=CARTESIAN_POINT('',(118.713153546234,-1.3,66.6288947749162));
#192881=CARTESIAN_POINT('',(118.773412477781,-1.3,66.3188909936332));
#192882=CARTESIAN_POINT('Origin',(121.572825304407,1.45439216225896E-14,
51.9172323623126));
#192883=CARTESIAN_POINT('Origin',(121.572825304407,1.45439216225896E-14,
51.9172323623126));
#192884=CARTESIAN_POINT('Origin',(119.138011311691,-1.3,64.4432019586286));
#192885=CARTESIAN_POINT('',(118.253809253311,-1.3,66.3715955776028));
#192886=CARTESIAN_POINT('',(118.194150993884,-1.3,66.6785091841359));
#192887=CARTESIAN_POINT('',(118.253809253311,-1.3,66.3715955776028));
#192888=CARTESIAN_POINT('Origin',(116.959178380441,-1.3,51.0204257716897));
#192889=CARTESIAN_POINT('Origin',(116.959178380441,-1.3,51.0204257716897));
#192890=CARTESIAN_POINT('Origin',(118.647197809142,-1.3,64.3477970021793));
#192891=CARTESIAN_POINT('Origin',(121.082011801857,1.45439216225896E-14,
51.8218274058634));
#192892=CARTESIAN_POINT('Origin',(121.082011801857,1.45439216225896E-14,
51.8218274058634));
#192893=CARTESIAN_POINT('Origin',(118.647197809142,-2.8,64.3477970021793));
#192894=CARTESIAN_POINT('',(118.813694939004,-2.8,66.1116567301338));
#192895=CARTESIAN_POINT('',(118.752575180056,-2.8,66.4260890623797));
#192896=CARTESIAN_POINT('',(118.813694939004,-2.8,66.1116567301338));
#192897=CARTESIAN_POINT('',(118.293675764896,-2.8,66.1665011788025));
#192898=CARTESIAN_POINT('Origin',(116.959178380441,-2.8,51.0204257716897));
#192899=CARTESIAN_POINT('',(118.233182525534,-2.8,66.4777103632785));
#192900=CARTESIAN_POINT('',(118.293675764896,-2.8,66.1665011788025));
#192901=CARTESIAN_POINT('Origin',(116.959178380441,-2.8,51.0204257716897));
#192902=CARTESIAN_POINT('Origin',(119.138011311691,-2.8,64.4432019586286));
#192903=CARTESIAN_POINT('',(118.796921514364,-2.3,66.1979480886086));
#192904=CARTESIAN_POINT('',(118.736163138728,-2.3,66.5105212741601));
#192905=CARTESIAN_POINT('',(118.796921514364,-2.3,66.1979480886086));
#192906=CARTESIAN_POINT('Origin',(121.572825304407,1.45439216225896E-14,
51.9172323623126));
#192907=CARTESIAN_POINT('Origin',(121.572825304407,1.45439216225896E-14,
51.9172323623126));
#192908=CARTESIAN_POINT('Origin',(119.138011311691,-2.3,64.4432019586286));
#192909=CARTESIAN_POINT('',(118.277076983843,-2.3,66.2518940783944));
#192910=CARTESIAN_POINT('',(118.216934189658,-2.3,66.5613003877282));
#192911=CARTESIAN_POINT('',(118.277076983843,-2.3,66.2518940783944));
#192912=CARTESIAN_POINT('Origin',(116.959178380441,-2.3,51.0204257716897));
#192913=CARTESIAN_POINT('Origin',(116.959178380441,-2.3,51.0204257716897));
#192914=CARTESIAN_POINT('Origin',(118.647197809142,-2.3,64.3477970021793));
#192915=CARTESIAN_POINT('Origin',(121.082011801857,1.45439216225896E-14,
51.8218274058634));
#192916=CARTESIAN_POINT('Origin',(121.082011801857,1.45439216225896E-14,
51.8218274058634));
#192917=CARTESIAN_POINT('Origin',(117.665570804043,-2.8,64.1569870892808));
#192918=CARTESIAN_POINT('',(117.777192058143,-2.8,66.2031573154554));
#192919=CARTESIAN_POINT('',(117.717239093625,-2.8,66.5115870406867));
#192920=CARTESIAN_POINT('',(117.777192058143,-2.8,66.2031573154554));
#192921=CARTESIAN_POINT('',(117.264147820731,-2.8,66.2221190045997));
#192922=CARTESIAN_POINT('Origin',(116.959178380441,-2.8,51.0204257716897));
#192923=CARTESIAN_POINT('',(117.20465508306,-2.8,66.5281810797731));
#192924=CARTESIAN_POINT('',(117.264147820731,-2.8,66.2221190045997));
#192925=CARTESIAN_POINT('Origin',(116.959178380441,-2.8,51.0204257716897));
#192926=CARTESIAN_POINT('Origin',(118.156384306592,-2.8,64.25239204573));
#192927=CARTESIAN_POINT('',(117.760743812198,-2.3,66.2877757829205));
#192928=CARTESIAN_POINT('',(117.701132038091,-2.3,66.5944502444126));
#192929=CARTESIAN_POINT('',(117.760743812198,-2.3,66.2877757829205));
#192930=CARTESIAN_POINT('Origin',(120.591198299308,1.45439216225896E-14,
51.7264224494141));
#192931=CARTESIAN_POINT('Origin',(120.591198299308,1.45439216225896E-14,
51.7264224494141));
#192932=CARTESIAN_POINT('Origin',(118.156384306592,-2.3,64.25239204573));
#192933=CARTESIAN_POINT('',(117.247827757456,-2.3,66.3060780326826));
#192934=CARTESIAN_POINT('',(117.188668455303,-2.3,66.6104247393819));
#192935=CARTESIAN_POINT('',(117.247827757456,-2.3,66.3060780326826));
#192936=CARTESIAN_POINT('Origin',(116.959178380441,-2.3,51.0204257716897));
#192937=CARTESIAN_POINT('Origin',(116.959178380441,-2.3,51.0204257716897));
#192938=CARTESIAN_POINT('Origin',(117.665570804043,-2.3,64.1569870892808));
#192939=CARTESIAN_POINT('Origin',(120.100384796758,1.45439216225896E-14,
51.6310174929649));
#192940=CARTESIAN_POINT('Origin',(120.100384796758,1.45439216225896E-14,
51.6310174929649));
#192941=CARTESIAN_POINT('Origin',(116.683943798944,-2.8,63.9661771763823));
#192942=CARTESIAN_POINT('',(116.754462709301,-2.8,66.223799574922));
#192943=CARTESIAN_POINT('',(116.695355203691,-2.8,66.5278798128357));
#192944=CARTESIAN_POINT('',(116.754462709301,-2.8,66.223799574922));
#192945=CARTESIAN_POINT('',(116.248070475418,-2.8,66.2085398433723));
#192946=CARTESIAN_POINT('Origin',(116.959178380441,-2.8,51.0204257716897));
#192947=CARTESIAN_POINT('',(116.189277281699,-2.8,66.511003094857));
#192948=CARTESIAN_POINT('',(116.248070475418,-2.8,66.2085398433723));
#192949=CARTESIAN_POINT('Origin',(116.959178380441,-2.8,51.0204257716897));
#192950=CARTESIAN_POINT('Origin',(117.174757301493,-2.8,64.0615821328315));
#192951=CARTESIAN_POINT('',(116.738249906779,-2.3,66.3072067970213));
#192952=CARTESIAN_POINT('',(116.67946943582,-2.3,66.6096045959044));
#192953=CARTESIAN_POINT('',(116.738249906779,-2.3,66.3072067970213));
#192954=CARTESIAN_POINT('Origin',(119.609571294209,1.45439216225896E-14,
51.5356125365156));
#192955=CARTESIAN_POINT('Origin',(119.609571294209,1.45439216225896E-14,
51.5356125365156));
#192956=CARTESIAN_POINT('Origin',(117.174757301493,-2.3,64.0615821328315));
#192957=CARTESIAN_POINT('',(116.231945164223,-2.3,66.2914969638595));
#192958=CARTESIAN_POINT('',(116.173473843287,-2.3,66.5923043316899));
#192959=CARTESIAN_POINT('',(116.231945164223,-2.3,66.2914969638595));
#192960=CARTESIAN_POINT('Origin',(116.959178380441,-2.3,51.0204257716897));
#192961=CARTESIAN_POINT('Origin',(116.959178380441,-2.3,51.0204257716897));
#192962=CARTESIAN_POINT('Origin',(116.683943798944,-2.3,63.9661771763823));
#192963=CARTESIAN_POINT('Origin',(119.118757791659,1.45439216225896E-14,
51.4402075800664));
#192964=CARTESIAN_POINT('Origin',(119.118757791659,1.45439216225896E-14,
51.4402075800664));
#192965=CARTESIAN_POINT('Origin',(115.702316793845,-2.8,63.7753672634838));
#192966=CARTESIAN_POINT('',(115.744917738381,-2.8,66.1766144284786));
#192967=CARTESIAN_POINT('',(115.686371158483,-2.8,66.4778089681697));
#192968=CARTESIAN_POINT('',(115.744917738381,-2.8,66.1766144284786));
#192969=CARTESIAN_POINT('',(115.244963034622,-2.8,66.1282366407438));
#192970=CARTESIAN_POINT('Origin',(116.959178380441,-2.8,51.0204257716897));
#192971=CARTESIAN_POINT('',(115.186597835385,-2.8,66.4284980624817));
#192972=CARTESIAN_POINT('',(115.244963034622,-2.8,66.1282366407438));
#192973=CARTESIAN_POINT('Origin',(116.959178380441,-2.8,51.0204257716897));
#192974=CARTESIAN_POINT('Origin',(116.193130296394,-2.8,63.870772219933));
#192975=CARTESIAN_POINT('',(115.728861059795,-2.3,66.2592184665667));
#192976=CARTESIAN_POINT('',(115.670632340546,-2.3,66.5587777631371));
#192977=CARTESIAN_POINT('',(115.728861059795,-2.3,66.2592184665667));
#192978=CARTESIAN_POINT('Origin',(118.62794428911,1.45439216225896E-14,
51.3448026236171));
#192979=CARTESIAN_POINT('Origin',(118.62794428911,1.45439216225896E-14,
51.3448026236171));
#192980=CARTESIAN_POINT('Origin',(116.193130296394,-2.3,63.870772219933));
#192981=CARTESIAN_POINT('',(115.228956826212,-2.3,66.2105810335809));
#192982=CARTESIAN_POINT('',(115.170906557973,-2.3,66.5092222838734));
#192983=CARTESIAN_POINT('',(115.228956826212,-2.3,66.2105810335809));
#192984=CARTESIAN_POINT('Origin',(116.959178380441,-2.3,51.0204257716897));
#192985=CARTESIAN_POINT('Origin',(116.959178380441,-2.3,51.0204257716897));
#192986=CARTESIAN_POINT('Origin',(115.702316793845,-2.3,63.7753672634838));
#192987=CARTESIAN_POINT('Origin',(118.13713078656,1.45439216225896E-14,
51.2493976671679));
#192988=CARTESIAN_POINT('Origin',(118.13713078656,1.45439216225896E-14,
51.2493976671679));
#192989=CARTESIAN_POINT('Origin',(114.720689788746,-2.8,63.5845573505853));
#192990=CARTESIAN_POINT('',(114.748176102656,-2.8,66.063562161234));
#192991=CARTESIAN_POINT('',(114.689928828871,-2.8,66.363216912147));
#192992=CARTESIAN_POINT('',(114.748176102656,-2.8,66.063562161234));
#192993=CARTESIAN_POINT('',(114.254537373977,-2.8,65.9826916606871));
#192994=CARTESIAN_POINT('Origin',(116.959178380441,-2.8,51.0204257716897));
#192995=CARTESIAN_POINT('',(114.196345710662,-2.8,66.2820603219557));
#192996=CARTESIAN_POINT('',(114.254537373977,-2.8,65.9826916606871));
#192997=CARTESIAN_POINT('Origin',(116.959178380441,-2.8,51.0204257716897));
#192998=CARTESIAN_POINT('Origin',(115.211503291295,-2.8,63.6799623070345));
#192999=CARTESIAN_POINT('',(114.732202704012,-2.3,66.1457377632978));
#193000=CARTESIAN_POINT('',(114.674268466112,-2.3,66.4437820922258));
#193001=CARTESIAN_POINT('',(114.732202704012,-2.3,66.1457377632978));
#193002=CARTESIAN_POINT('Origin',(117.64631728401,1.45439216225896E-14,
51.1539927107186));
#193003=CARTESIAN_POINT('Origin',(117.64631728401,1.45439216225896E-14,
51.1539927107186));
#193004=CARTESIAN_POINT('Origin',(115.211503291295,-2.3,63.6799623070345));
#193005=CARTESIAN_POINT('',(114.238579446542,-2.3,66.0647876706762));
#193006=CARTESIAN_POINT('',(114.180699928051,-2.3,66.36255049405));
#193007=CARTESIAN_POINT('',(114.238579446542,-2.3,66.0647876706762));
#193008=CARTESIAN_POINT('Origin',(116.959178380441,-2.3,51.0204257716897));
#193009=CARTESIAN_POINT('Origin',(116.959178380441,-2.3,51.0204257716897));
#193010=CARTESIAN_POINT('Origin',(114.720689788746,-2.3,63.5845573505853));
#193011=CARTESIAN_POINT('Origin',(117.155503781461,1.45439216225896E-14,
51.0585877542694));
#193012=CARTESIAN_POINT('Origin',(117.155503781461,1.45439216225896E-14,
51.0585877542694));
#193013=CARTESIAN_POINT('Origin',(113.739062783647,-2.8,63.3937474376868));
#193014=CARTESIAN_POINT('',(113.764037649552,-2.8,65.8856724637829));
#193015=CARTESIAN_POINT('',(113.705839815162,-2.8,66.1850728723215));
#193016=CARTESIAN_POINT('',(113.764037649552,-2.8,65.8856724637829));
#193017=CARTESIAN_POINT('',(113.276677949281,-2.8,65.7724993236168));
#193018=CARTESIAN_POINT('Origin',(116.959178380441,-2.8,51.0204257716897));
#193019=CARTESIAN_POINT('',(113.218412103209,-2.8,66.0722496201832));
#193020=CARTESIAN_POINT('',(113.276677949281,-2.8,65.7724993236168));
#193021=CARTESIAN_POINT('Origin',(116.959178380441,-2.8,51.0204257716897));
#193022=CARTESIAN_POINT('Origin',(114.229876286196,-2.8,63.489152394136));
#193023=CARTESIAN_POINT('',(113.748078005312,-2.3,65.9677773059216));
#193024=CARTESIAN_POINT('',(113.690192414544,-2.3,66.2655713682987));
#193025=CARTESIAN_POINT('',(113.748078005312,-2.3,65.9677773059216));
#193026=CARTESIAN_POINT('Origin',(116.664690278911,1.45439216225896E-14,
50.9631827978201));
#193027=CARTESIAN_POINT('Origin',(116.664690278911,1.45439216225896E-14,
50.9631827978201));
#193028=CARTESIAN_POINT('Origin',(114.229876286196,-2.3,63.489152394136));
#193029=CARTESIAN_POINT('',(113.26069938356,-2.3,65.8547015078552));
#193030=CARTESIAN_POINT('',(113.202746871335,-2.3,66.1528398495673));
#193031=CARTESIAN_POINT('',(113.26069938356,-2.3,65.8547015078552));
#193032=CARTESIAN_POINT('Origin',(116.959178380441,-2.3,51.0204257716897));
#193033=CARTESIAN_POINT('Origin',(116.959178380441,-2.3,51.0204257716897));
#193034=CARTESIAN_POINT('Origin',(113.739062783647,-2.3,63.3937474376868));
#193035=CARTESIAN_POINT('Origin',(116.173876776362,1.45439216225896E-14,
50.8677778413709));
#193036=CARTESIAN_POINT('Origin',(116.173876776362,1.45439216225896E-14,
50.8677778413709));
#193037=CARTESIAN_POINT('Origin',(112.757435778548,-2.8,63.2029375247883));
#193038=CARTESIAN_POINT('',(112.792469528639,-2.8,65.6431143360832));
#193039=CARTESIAN_POINT('',(112.734073177143,-2.8,65.943536021505));
#193040=CARTESIAN_POINT('',(112.792469528639,-2.8,65.6431143360832));
#193041=CARTESIAN_POINT('',(112.311434063134,-2.8,65.4974059909163));
#193042=CARTESIAN_POINT('Origin',(116.959178380441,-2.8,51.0204257716897));
#193043=CARTESIAN_POINT('',(112.252843447732,-2.8,65.7988270725098));
#193044=CARTESIAN_POINT('',(112.311434063134,-2.8,65.4974059909163));
#193045=CARTESIAN_POINT('Origin',(116.959178380441,-2.8,51.0204257716897));
#193046=CARTESIAN_POINT('Origin',(113.248249281097,-2.8,63.2983424812375));
#193047=CARTESIAN_POINT('',(112.776454652423,-2.3,65.7255033206915));
#193048=CARTESIAN_POINT('',(112.71837373382,-2.3,66.024302252655));
#193049=CARTESIAN_POINT('',(112.776454652423,-2.3,65.7255033206915));
#193050=CARTESIAN_POINT('Origin',(115.683063273812,1.45439216225896E-14,
50.7723728849216));
#193051=CARTESIAN_POINT('Origin',(115.683063273812,1.45439216225896E-14,
50.7723728849216));
#193052=CARTESIAN_POINT('Origin',(113.248249281097,-2.3,63.2983424812375));
#193053=CARTESIAN_POINT('',(112.295365130396,-2.3,65.580073070838));
#193054=CARTESIAN_POINT('',(112.237093089611,-2.3,65.8798552362785));
#193055=CARTESIAN_POINT('',(112.295365130396,-2.3,65.580073070838));
#193056=CARTESIAN_POINT('Origin',(116.959178380441,-2.3,51.0204257716897));
#193057=CARTESIAN_POINT('Origin',(116.959178380441,-2.3,51.0204257716897));
#193058=CARTESIAN_POINT('Origin',(112.757435778548,-2.3,63.2029375247883));
#193059=CARTESIAN_POINT('Origin',(115.192249771263,1.45439216225896E-14,
50.6769679284724));
#193060=CARTESIAN_POINT('Origin',(115.192249771263,1.45439216225896E-14,
50.6769679284724));
#193061=CARTESIAN_POINT('Origin',(111.775808773449,-2.8,63.0121276118898));
#193062=CARTESIAN_POINT('',(111.833604007695,-2.8,65.3352073228156));
#193063=CARTESIAN_POINT('',(111.774753459122,-2.8,65.637965637969));
#193064=CARTESIAN_POINT('',(111.833604007695,-2.8,65.3352073228156));
#193065=CARTESIAN_POINT('',(111.359023145067,-2.8,65.1562930902008));
#193066=CARTESIAN_POINT('Origin',(116.959178380441,-2.8,51.0204257716897));
#193067=CARTESIAN_POINT('',(111.299844384071,-2.8,65.4607399034676));
#193068=CARTESIAN_POINT('',(111.359023145067,-2.8,65.1562930902008));
#193069=CARTESIAN_POINT('Origin',(116.959178380441,-2.8,51.0204257716897));
#193070=CARTESIAN_POINT('Origin',(112.266622275998,-2.8,63.107532568339));
#193071=CARTESIAN_POINT('',(111.817462732837,-2.3,65.4182465688194));
#193072=CARTESIAN_POINT('',(111.758934994926,-2.3,65.7193441753763));
#193073=CARTESIAN_POINT('',(111.817462732837,-2.3,65.4182465688194));
#193074=CARTESIAN_POINT('Origin',(114.701436268713,1.45439216225896E-14,
50.5815629720231));
#193075=CARTESIAN_POINT('Origin',(114.701436268713,1.45439216225896E-14,
50.5815629720231));
#193076=CARTESIAN_POINT('Origin',(112.266622275998,-2.3,63.107532568339));
#193077=CARTESIAN_POINT('',(111.342790505145,-2.3,65.2398023663664));
#193078=CARTESIAN_POINT('',(111.283939956573,-2.3,65.5425606815198));
#193079=CARTESIAN_POINT('',(111.342790505145,-2.3,65.2398023663664));
#193080=CARTESIAN_POINT('Origin',(116.959178380441,-2.3,51.0204257716897));
#193081=CARTESIAN_POINT('Origin',(116.959178380441,-2.3,51.0204257716897));
#193082=CARTESIAN_POINT('Origin',(111.775808773449,-2.3,63.0121276118898));
#193083=CARTESIAN_POINT('Origin',(114.210622766164,1.45439216225896E-14,
50.4861580155739));
#193084=CARTESIAN_POINT('Origin',(114.210622766164,1.45439216225896E-14,
50.4861580155739));
#193085=CARTESIAN_POINT('Origin',(111.775808773449,-1.8,63.0121276118898));
#193086=CARTESIAN_POINT('',(111.804551627846,-1.8,65.4846681143887));
#193087=CARTESIAN_POINT('',(111.746279587062,-1.8,65.7844502798292));
#193088=CARTESIAN_POINT('',(111.804551627846,-1.8,65.4846681143887));
#193089=CARTESIAN_POINT('',(111.329807058035,-1.8,65.3065960780178));
#193090=CARTESIAN_POINT('Origin',(116.959178380441,-1.8,51.0204257716897));
#193091=CARTESIAN_POINT('',(111.271216442633,-1.8,65.6080171596113));
#193092=CARTESIAN_POINT('',(111.329807058035,-1.8,65.3065960780178));
#193093=CARTESIAN_POINT('Origin',(116.959178380441,-1.8,51.0204257716897));
#193094=CARTESIAN_POINT('Origin',(112.266622275998,-1.8,63.107532568339));
#193095=CARTESIAN_POINT('',(111.794827647324,-1.3,65.534693407793));
#193096=CARTESIAN_POINT('',(111.736746728721,-1.3,65.8334923397565));
#193097=CARTESIAN_POINT('',(111.794827647324,-1.3,65.534693407793));
#193098=CARTESIAN_POINT('Origin',(114.701436268713,1.45439216225896E-14,
50.5815629720231));
#193099=CARTESIAN_POINT('Origin',(114.701436268713,1.45439216225896E-14,
50.5815629720231));
#193100=CARTESIAN_POINT('Origin',(112.266622275998,-1.3,63.107532568339));
#193101=CARTESIAN_POINT('',(111.320029020991,-1.3,65.3568994667354));
#193102=CARTESIAN_POINT('',(111.261632669494,-1.3,65.6573211521572));
#193103=CARTESIAN_POINT('',(111.320029020991,-1.3,65.3568994667354));
#193104=CARTESIAN_POINT('Origin',(116.959178380441,-1.3,51.0204257716897));
#193105=CARTESIAN_POINT('Origin',(116.959178380441,-1.3,51.0204257716897));
#193106=CARTESIAN_POINT('Origin',(111.775808773449,-1.3,63.0121276118898));
#193107=CARTESIAN_POINT('Origin',(114.210622766164,1.45439216225896E-14,
50.4861580155739));
#193108=CARTESIAN_POINT('Origin',(114.210622766164,1.45439216225896E-14,
50.4861580155739));
#193109=CARTESIAN_POINT('Origin',(111.775808773449,-0.799999999999986,63.0121276118898));
#193110=CARTESIAN_POINT('',(111.788258875911,-0.799999999999986,65.5684866385074));
#193111=CARTESIAN_POINT('',(111.730306363686,-0.799999999999986,65.8666249802195));
#193112=CARTESIAN_POINT('',(111.788258875911,-0.799999999999986,65.5684866385074));
#193113=CARTESIAN_POINT('',(111.313423939083,-0.799999999999986,65.3908794978198));
#193114=CARTESIAN_POINT('Origin',(116.959178380441,-0.799999999999986,51.0204257716897));
#193115=CARTESIAN_POINT('',(111.255158093011,-0.799999999999986,65.6906297943862));
#193116=CARTESIAN_POINT('',(111.313423939083,-0.799999999999986,65.3908794978198));
#193117=CARTESIAN_POINT('Origin',(116.959178380441,-0.799999999999986,51.0204257716897));
#193118=CARTESIAN_POINT('Origin',(112.266622275998,-0.799999999999986,63.107532568339));
#193119=CARTESIAN_POINT('',(111.784823995114,-0.299999999999985,65.5861574801246));
#193120=CARTESIAN_POINT('',(111.726938404346,-0.299999999999985,65.8839515425017));
#193121=CARTESIAN_POINT('',(111.784823995114,-0.299999999999985,65.5861574801246));
#193122=CARTESIAN_POINT('Origin',(114.701436268713,1.45439216225896E-14,
50.5815629720231));
#193123=CARTESIAN_POINT('Origin',(114.701436268713,1.45439216225896E-14,
50.5815629720231));
#193124=CARTESIAN_POINT('Origin',(112.266622275998,-0.299999999999985,63.107532568339));
#193125=CARTESIAN_POINT('',(111.309970136804,-0.299999999999985,65.4086476815366));
#193126=CARTESIAN_POINT('',(111.251772302414,-0.299999999999985,65.7080480900753));
#193127=CARTESIAN_POINT('',(111.309970136804,-0.299999999999985,65.4086476815366));
#193128=CARTESIAN_POINT('Origin',(116.959178380441,-0.299999999999985,51.0204257716897));
#193129=CARTESIAN_POINT('Origin',(116.959178380441,-0.299999999999985,51.0204257716897));
#193130=CARTESIAN_POINT('Origin',(111.775808773449,-0.299999999999985,63.0121276118898));
#193131=CARTESIAN_POINT('Origin',(114.210622766164,1.45439216225896E-14,
50.4861580155739));
#193132=CARTESIAN_POINT('Origin',(114.210622766164,1.45439216225896E-14,
50.4861580155739));
#193133=CARTESIAN_POINT('Origin',(117.665570804043,-0.799999999999986,64.1569870892808));
#193134=CARTESIAN_POINT('',(117.730993451766,-0.799999999999986,66.4408273553883));
#193135=CARTESIAN_POINT('',(117.671989132337,-0.799999999999986,66.7443767490697));
#193136=CARTESIAN_POINT('',(117.730993451766,-0.799999999999986,66.4408273553883));
#193137=CARTESIAN_POINT('',(117.218305542335,-0.799999999999986,66.4579559051328));
#193138=CARTESIAN_POINT('Origin',(116.959178380441,-0.799999999999986,51.0204257716897));
#193139=CARTESIAN_POINT('',(117.159740102242,-0.799999999999986,66.7592474716348));
#193140=CARTESIAN_POINT('',(117.218305542335,-0.799999999999986,66.4579559051328));
#193141=CARTESIAN_POINT('Origin',(116.959178380441,-0.799999999999986,51.0204257716897));
#193142=CARTESIAN_POINT('Origin',(118.156384306592,-0.799999999999986,64.25239204573));
#193143=CARTESIAN_POINT('',(117.727495032124,-0.299999999999985,66.4588250743906));
#193144=CARTESIAN_POINT('',(117.668561340481,-0.299999999999985,66.7620111214277));
#193145=CARTESIAN_POINT('',(117.727495032124,-0.299999999999985,66.4588250743906));
#193146=CARTESIAN_POINT('Origin',(120.591198299308,1.45439216225896E-14,
51.7264224494141));
#193147=CARTESIAN_POINT('Origin',(120.591198299308,1.45439216225896E-14,
51.7264224494141));
#193148=CARTESIAN_POINT('Origin',(118.156384306592,-0.299999999999985,64.25239204573));
#193149=CARTESIAN_POINT('',(117.214833642932,-0.299999999999985,66.4758171900162));
#193150=CARTESIAN_POINT('',(117.156337267937,-0.299999999999985,66.7767534491633));
#193151=CARTESIAN_POINT('',(117.214833642932,-0.299999999999985,66.4758171900162));
#193152=CARTESIAN_POINT('Origin',(116.959178380441,-0.299999999999985,51.0204257716897));
#193153=CARTESIAN_POINT('Origin',(116.959178380441,-0.299999999999985,51.0204257716897));
#193154=CARTESIAN_POINT('Origin',(117.665570804043,-0.299999999999985,64.1569870892808));
#193155=CARTESIAN_POINT('Origin',(120.100384796758,1.45439216225896E-14,
51.6310174929649));
#193156=CARTESIAN_POINT('Origin',(120.100384796758,1.45439216225896E-14,
51.6310174929649));
#193157=CARTESIAN_POINT('Origin',(117.665570804043,-1.8,64.1569870892808));
#193158=CARTESIAN_POINT('',(117.747589699224,-1.8,66.3554474899478));
#193159=CARTESIAN_POINT('',(117.688248030859,-1.8,66.6607323847921));
#193160=CARTESIAN_POINT('',(117.747589699224,-1.8,66.3554474899478));
#193161=CARTESIAN_POINT('',(117.23477510084,-1.8,66.3732277946038));
#193162=CARTESIAN_POINT('Origin',(116.959178380441,-1.8,51.0204257716897));
#193163=CARTESIAN_POINT('',(117.175879826691,-1.8,66.6762162017529));
#193164=CARTESIAN_POINT('',(117.23477510084,-1.8,66.3732277946038));
#193165=CARTESIAN_POINT('Origin',(116.959178380441,-1.8,51.0204257716897));
#193166=CARTESIAN_POINT('Origin',(118.156384306592,-1.8,64.25239204573));
#193167=CARTESIAN_POINT('',(117.737684163035,-1.3,66.4064068016241));
#193168=CARTESIAN_POINT('',(117.678544300543,-1.3,66.710653500439));
#193169=CARTESIAN_POINT('',(117.737684163035,-1.3,66.4064068016241));
#193170=CARTESIAN_POINT('Origin',(120.591198299308,1.45439216225896E-14,
51.7264224494141));
#193171=CARTESIAN_POINT('Origin',(120.591198299308,1.45439216225896E-14,
51.7264224494141));
#193172=CARTESIAN_POINT('Origin',(118.156384306592,-1.3,64.25239204573));
#193173=CARTESIAN_POINT('',(117.22494535473,-1.3,66.4237972020704));
#193174=CARTESIAN_POINT('',(117.166247380857,-1.3,66.7257705923584));
#193175=CARTESIAN_POINT('',(117.22494535473,-1.3,66.4237972020704));
#193176=CARTESIAN_POINT('Origin',(116.959178380441,-1.3,51.0204257716897));
#193177=CARTESIAN_POINT('Origin',(116.959178380441,-1.3,51.0204257716897));
#193178=CARTESIAN_POINT('Origin',(117.665570804043,-1.3,64.1569870892808));
#193179=CARTESIAN_POINT('Origin',(120.100384796758,1.45439216225896E-14,
51.6310174929649));
#193180=CARTESIAN_POINT('Origin',(120.100384796758,1.45439216225896E-14,
51.6310174929649));
#193181=CARTESIAN_POINT('Origin',(116.683943798944,-1.8,63.9661771763823));
#193182=CARTESIAN_POINT('',(116.72528216571,-1.8,66.3739197084998));
#193183=CARTESIAN_POINT('',(116.666760704416,-1.8,66.6749850248193));
#193184=CARTESIAN_POINT('',(116.72528216571,-1.8,66.3739197084998));
#193185=CARTESIAN_POINT('',(116.219046700398,-1.8,66.3578534765906));
#193186=CARTESIAN_POINT('Origin',(116.959178380441,-1.8,51.0204257716897));
#193187=CARTESIAN_POINT('',(116.160830340994,-1.8,66.6573491875945));
#193188=CARTESIAN_POINT('',(116.219046700398,-1.8,66.3578534765906));
#193189=CARTESIAN_POINT('Origin',(116.959178380441,-1.8,51.0204257716897));
#193190=CARTESIAN_POINT('Origin',(117.174757301493,-1.8,64.0615821328315));
#193191=CARTESIAN_POINT('',(116.715515864156,-1.3,66.4241627236523));
#193192=CARTESIAN_POINT('',(116.657187981895,-1.3,66.7242321671538));
#193193=CARTESIAN_POINT('',(116.715515864156,-1.3,66.4241627236523));
#193194=CARTESIAN_POINT('Origin',(119.609571294209,1.45439216225896E-14,
51.5356125365156));
#193195=CARTESIAN_POINT('Origin',(119.609571294209,1.45439216225896E-14,
51.5356125365156));
#193196=CARTESIAN_POINT('Origin',(117.174757301493,-1.3,64.0615821328315));
#193197=CARTESIAN_POINT('',(116.209332166521,-1.3,66.4078301714677));
#193198=CARTESIAN_POINT('',(116.151306383661,-1.3,66.7063454560356));
#193199=CARTESIAN_POINT('',(116.209332166521,-1.3,66.4078301714677));
#193200=CARTESIAN_POINT('Origin',(116.959178380441,-1.3,51.0204257716897));
#193201=CARTESIAN_POINT('Origin',(116.959178380441,-1.3,51.0204257716897));
#193202=CARTESIAN_POINT('Origin',(116.683943798944,-1.3,63.9661771763823));
#193203=CARTESIAN_POINT('Origin',(119.118757791659,1.45439216225896E-14,
51.4402075800664));
#193204=CARTESIAN_POINT('Origin',(119.118757791659,1.45439216225896E-14,
51.4402075800664));
#193205=CARTESIAN_POINT('Origin',(115.702316793845,-1.8,63.7753672634838));
#193206=CARTESIAN_POINT('',(115.716016948437,-1.8,66.3252953614908));
#193207=CARTESIAN_POINT('',(115.658040043519,-1.8,66.6235591921022));
#193208=CARTESIAN_POINT('',(115.716016948437,-1.8,66.3252953614908));
#193209=CARTESIAN_POINT('',(115.216152688302,-1.8,66.2764522839691));
#193210=CARTESIAN_POINT('Origin',(116.959178380441,-1.8,51.0204257716897));
#193211=CARTESIAN_POINT('',(115.158351935903,-1.8,66.573809892952));
#193212=CARTESIAN_POINT('',(115.216152688302,-1.8,66.2764522839691));
#193213=CARTESIAN_POINT('Origin',(116.959178380441,-1.8,51.0204257716897));
#193214=CARTESIAN_POINT('Origin',(116.193130296394,-1.8,63.870772219933));
#193215=CARTESIAN_POINT('',(115.706343034183,-1.3,66.3750630875619));
#193216=CARTESIAN_POINT('',(115.64855437112,-1.3,66.6723585026113));
#193217=CARTESIAN_POINT('',(115.706343034183,-1.3,66.3750630875619));
#193218=CARTESIAN_POINT('Origin',(118.62794428911,1.45439216225896E-14,
51.3448026236171));
#193219=CARTESIAN_POINT('Origin',(118.62794428911,1.45439216225896E-14,
51.3448026236171));
#193220=CARTESIAN_POINT('Origin',(116.193130296394,-1.3,63.870772219933));
#193221=CARTESIAN_POINT('',(115.20650865023,-1.3,66.3260663111735));
#193222=CARTESIAN_POINT('',(115.148894434369,-1.3,66.6224642776501));
#193223=CARTESIAN_POINT('',(115.20650865023,-1.3,66.3260663111735));
#193224=CARTESIAN_POINT('Origin',(116.959178380441,-1.3,51.0204257716897));
#193225=CARTESIAN_POINT('Origin',(116.959178380441,-1.3,51.0204257716897));
#193226=CARTESIAN_POINT('Origin',(115.702316793845,-1.3,63.7753672634838));
#193227=CARTESIAN_POINT('Origin',(118.13713078656,1.45439216225896E-14,
51.2493976671679));
#193228=CARTESIAN_POINT('Origin',(118.13713078656,1.45439216225896E-14,
51.2493976671679));
#193229=CARTESIAN_POINT('Origin',(114.720689788746,-1.8,63.5845573505853));
#193230=CARTESIAN_POINT('',(114.71942455413,-1.8,66.2114753175407));
#193231=CARTESIAN_POINT('',(114.661738345058,-1.8,66.5082436551355));
#193232=CARTESIAN_POINT('',(114.71942455413,-1.8,66.2114753175407));
#193233=CARTESIAN_POINT('',(114.225813551673,-1.8,66.1304621786584));
#193234=CARTESIAN_POINT('Origin',(116.959178380441,-1.8,51.0204257716897));
#193235=CARTESIAN_POINT('',(114.168181362785,-1.8,66.4269526078809));
#193236=CARTESIAN_POINT('',(114.225813551673,-1.8,66.1304621786584));
#193237=CARTESIAN_POINT('Origin',(116.959178380441,-1.8,51.0204257716897));
#193238=CARTESIAN_POINT('Origin',(115.211503291295,-1.8,63.6799623070345));
#193239=CARTESIAN_POINT('',(114.709799940683,-1.3,66.2609894142129));
#193240=CARTESIAN_POINT('',(114.652299164781,-1.3,66.5568037856086));
#193241=CARTESIAN_POINT('',(114.709799940683,-1.3,66.2609894142129));
#193242=CARTESIAN_POINT('Origin',(117.64631728401,1.45439216225896E-14,
51.1539927107186));
#193243=CARTESIAN_POINT('Origin',(117.64631728401,1.45439216225896E-14,
51.1539927107186));
#193244=CARTESIAN_POINT('Origin',(115.211503291295,-1.3,63.6799623070345));
#193245=CARTESIAN_POINT('',(114.216198098491,-1.3,66.1799291500881));
#193246=CARTESIAN_POINT('',(114.158750823915,-1.3,66.4754682823909));
#193247=CARTESIAN_POINT('',(114.216198098491,-1.3,66.1799291500881));
#193248=CARTESIAN_POINT('Origin',(116.959178380441,-1.3,51.0204257716897));
#193249=CARTESIAN_POINT('Origin',(116.959178380441,-1.3,51.0204257716897));
#193250=CARTESIAN_POINT('Origin',(114.720689788746,-1.3,63.5845573505853));
#193251=CARTESIAN_POINT('Origin',(117.155503781461,1.45439216225896E-14,
51.0585877542694));
#193252=CARTESIAN_POINT('Origin',(117.155503781461,1.45439216225896E-14,
51.0585877542694));
#193253=CARTESIAN_POINT('Origin',(113.739062783647,-1.8,63.3937474376868));
#193254=CARTESIAN_POINT('',(113.735310750518,-1.8,66.0334588100773));
#193255=CARTESIAN_POINT('',(113.677672566881,-1.8,66.3299800794583));
#193256=CARTESIAN_POINT('',(113.735310750518,-1.8,66.0334588100773));
#193257=CARTESIAN_POINT('',(113.247917140825,-1.8,65.9204601178992));
#193258=CARTESIAN_POINT('Origin',(116.959178380441,-1.8,51.0204257716897));
#193259=CARTESIAN_POINT('',(113.190212891236,-1.8,66.2173212654414));
#193260=CARTESIAN_POINT('',(113.247917140825,-1.8,65.9204601178992));
#193261=CARTESIAN_POINT('Origin',(116.959178380441,-1.8,51.0204257716897));
#193262=CARTESIAN_POINT('Origin',(114.229876286196,-1.8,63.489152394136));
#193263=CARTESIAN_POINT('',(113.725694280819,-1.3,66.0829310110071));
#193264=CARTESIAN_POINT('',(113.668241069027,-1.3,66.3785006874882));
#193265=CARTESIAN_POINT('',(113.725694280819,-1.3,66.0829310110071));
#193266=CARTESIAN_POINT('Origin',(116.664690278911,1.45439216225896E-14,
50.9631827978201));
#193267=CARTESIAN_POINT('Origin',(116.664690278911,1.45439216225896E-14,
50.9631827978201));
#193268=CARTESIAN_POINT('Origin',(114.229876286196,-1.3,63.489152394136));
#193269=CARTESIAN_POINT('',(113.238289468134,-1.3,65.9699899529383));
#193270=CARTESIAN_POINT('',(113.180770825207,-1.3,66.2658962417468));
#193271=CARTESIAN_POINT('',(113.238289468134,-1.3,65.9699899529383));
#193272=CARTESIAN_POINT('Origin',(116.959178380441,-1.3,51.0204257716897));
#193273=CARTESIAN_POINT('Origin',(116.959178380441,-1.3,51.0204257716897));
#193274=CARTESIAN_POINT('Origin',(113.739062783647,-1.3,63.3937474376868));
#193275=CARTESIAN_POINT('Origin',(116.173876776362,1.45439216225896E-14,
50.8677778413709));
#193276=CARTESIAN_POINT('Origin',(116.173876776362,1.45439216225896E-14,
50.8677778413709));
#193277=CARTESIAN_POINT('Origin',(112.757435778548,-1.8,63.2029375247883));
#193278=CARTESIAN_POINT('',(112.763643649162,-1.8,65.7914098900782));
#193279=CARTESIAN_POINT('',(112.705812640189,-1.8,66.0889231548602));
#193280=CARTESIAN_POINT('',(112.763643649162,-1.8,65.7914098900782));
#193281=CARTESIAN_POINT('',(112.282511314055,-1.8,65.6461998933239));
#193282=CARTESIAN_POINT('Origin',(116.959178380441,-1.8,51.0204257716897));
#193283=CARTESIAN_POINT('',(112.2244916477,-1.8,65.9446837113571));
#193284=CARTESIAN_POINT('',(112.282511314055,-1.8,65.6461998933239));
#193285=CARTESIAN_POINT('Origin',(116.959178380441,-1.8,51.0204257716897));
#193286=CARTESIAN_POINT('Origin',(113.248249281097,-1.8,63.2983424812375));
#193287=CARTESIAN_POINT('',(112.753994479771,-1.3,65.8410503155003));
#193288=CARTESIAN_POINT('',(112.696350299514,-1.3,66.1376024346597));
#193289=CARTESIAN_POINT('',(112.753994479771,-1.3,65.8410503155003));
#193290=CARTESIAN_POINT('Origin',(115.683063273812,1.45439216225896E-14,
50.7723728849216));
#193291=CARTESIAN_POINT('Origin',(115.683063273812,1.45439216225896E-14,
50.7723728849216));
#193292=CARTESIAN_POINT('Origin',(113.248249281097,-1.3,63.2983424812375));
#193293=CARTESIAN_POINT('',(112.272830146612,-1.3,65.696004933629));
#193294=CARTESIAN_POINT('',(112.21499913764,-1.3,65.993518198411));
#193295=CARTESIAN_POINT('',(112.272830146612,-1.3,65.696004933629));
#193296=CARTESIAN_POINT('Origin',(116.959178380441,-1.3,51.0204257716897));
#193297=CARTESIAN_POINT('Origin',(116.959178380441,-1.3,51.0204257716897));
#193298=CARTESIAN_POINT('Origin',(112.757435778548,-1.3,63.2029375247883));
#193299=CARTESIAN_POINT('Origin',(115.192249771263,1.45439216225896E-14,
50.6769679284724));
#193300=CARTESIAN_POINT('Origin',(115.192249771263,1.45439216225896E-14,
50.6769679284724));
#193301=CARTESIAN_POINT('Origin',(112.757435778548,-0.799999999999986,63.2029375247883));
#193302=CARTESIAN_POINT('',(112.747475965584,-0.799999999999986,65.874584996489));
#193303=CARTESIAN_POINT('',(112.689957322657,-0.799999999999986,66.1704912852975));
#193304=CARTESIAN_POINT('',(112.747475965584,-0.799999999999986,65.874584996489));
#193305=CARTESIAN_POINT('',(112.266290135726,-0.799999999999986,65.7296502050007));
#193306=CARTESIAN_POINT('Origin',(116.959178380441,-0.799999999999986,51.0204257716897));
#193307=CARTESIAN_POINT('',(112.208585886137,-0.799999999999986,66.0265113525429));
#193308=CARTESIAN_POINT('',(112.266290135726,-0.799999999999986,65.7296502050007));
#193309=CARTESIAN_POINT('Origin',(116.959178380441,-0.799999999999986,51.0204257716897));
#193310=CARTESIAN_POINT('Origin',(113.248249281097,-0.799999999999986,63.2983424812375));
#193311=CARTESIAN_POINT('',(112.74406727572,-0.299999999999985,65.8921210981086));
#193312=CARTESIAN_POINT('',(112.686614063928,-0.299999999999985,66.1876907745897));
#193313=CARTESIAN_POINT('',(112.74406727572,-0.299999999999985,65.8921210981086));
#193314=CARTESIAN_POINT('Origin',(115.683063273812,1.45439216225896E-14,
50.7723728849216));
#193315=CARTESIAN_POINT('Origin',(115.683063273812,1.45439216225896E-14,
50.7723728849216));
#193316=CARTESIAN_POINT('Origin',(113.248249281097,-0.299999999999985,63.2983424812375));
#193317=CARTESIAN_POINT('',(112.26287024287,-0.299999999999985,65.7472439407296));
#193318=CARTESIAN_POINT('',(112.205232059232,-0.299999999999985,66.0437652101105));
#193319=CARTESIAN_POINT('',(112.26287024287,-0.299999999999985,65.7472439407296));
#193320=CARTESIAN_POINT('Origin',(116.959178380441,-0.299999999999985,51.0204257716897));
#193321=CARTESIAN_POINT('Origin',(116.959178380441,-0.299999999999985,51.0204257716897));
#193322=CARTESIAN_POINT('Origin',(112.757435778548,-0.299999999999985,63.2029375247883));
#193323=CARTESIAN_POINT('Origin',(115.192249771263,1.45439216225896E-14,
50.6769679284724));
#193324=CARTESIAN_POINT('Origin',(115.192249771263,1.45439216225896E-14,
50.6769679284724));
#193325=CARTESIAN_POINT('Origin',(116.683943798944,-0.799999999999986,63.9661771763823));
#193326=CARTESIAN_POINT('',(116.708918664849,-0.799999999999986,66.4581022024784));
#193327=CARTESIAN_POINT('',(116.650720830459,-0.799999999999986,66.757502611017));
#193328=CARTESIAN_POINT('',(116.708918664849,-0.799999999999986,66.4581022024784));
#193329=CARTESIAN_POINT('',(116.202769740892,-0.799999999999986,66.4415907561147));
#193330=CARTESIAN_POINT('Origin',(116.959178380441,-0.799999999999986,51.0204257716897));
#193331=CARTESIAN_POINT('',(116.144871999832,-0.799999999999986,66.739447326016));
#193332=CARTESIAN_POINT('',(116.202769740892,-0.799999999999986,66.4415907561147));
#193333=CARTESIAN_POINT('Origin',(116.959178380441,-0.799999999999986,51.0204257716897));
#193334=CARTESIAN_POINT('Origin',(117.174757301493,-0.799999999999986,64.0615821328315));
#193335=CARTESIAN_POINT('',(116.705468970119,-0.299999999999985,66.4758492547892));
#193336=CARTESIAN_POINT('',(116.647338909772,-0.299999999999985,66.7749009978478));
#193337=CARTESIAN_POINT('',(116.705468970119,-0.299999999999985,66.4758492547892));
#193338=CARTESIAN_POINT('Origin',(119.609571294209,1.45439216225896E-14,
51.5356125365156));
#193339=CARTESIAN_POINT('Origin',(119.609571294209,1.45439216225896E-14,
51.5356125365156));
#193340=CARTESIAN_POINT('Origin',(117.174757301493,-0.299999999999985,64.0615821328315));
#193341=CARTESIAN_POINT('',(116.199338167008,-0.299999999999985,66.459244585223));
#193342=CARTESIAN_POINT('',(116.141507158036,-0.299999999999985,66.756757850005));
#193343=CARTESIAN_POINT('',(116.199338167008,-0.299999999999985,66.459244585223));
#193344=CARTESIAN_POINT('Origin',(116.959178380441,-0.299999999999985,51.0204257716897));
#193345=CARTESIAN_POINT('Origin',(116.959178380441,-0.299999999999985,51.0204257716897));
#193346=CARTESIAN_POINT('Origin',(116.683943798944,-0.299999999999985,63.9661771763823));
#193347=CARTESIAN_POINT('Origin',(119.118757791659,1.45439216225896E-14,
51.4402075800664));
#193348=CARTESIAN_POINT('Origin',(119.118757791659,1.45439216225896E-14,
51.4402075800664));
#193349=CARTESIAN_POINT('Origin',(115.702316793845,-0.799999999999986,63.7753672634838));
#193350=CARTESIAN_POINT('',(115.699807895975,-0.799999999999986,66.4086832913015));
#193351=CARTESIAN_POINT('',(115.642145714621,-0.799999999999986,66.7053280176139));
#193352=CARTESIAN_POINT('',(115.699807895975,-0.799999999999986,66.4086832913015));
#193353=CARTESIAN_POINT('',(115.199993583441,-0.799999999999986,66.3595832569304));
#193354=CARTESIAN_POINT('Origin',(116.959178380441,-0.799999999999986,51.0204257716897));
#193355=CARTESIAN_POINT('',(115.142504709642,-0.799999999999986,66.655336397614));
#193356=CARTESIAN_POINT('',(115.199993583441,-0.799999999999986,66.3595832569304));
#193357=CARTESIAN_POINT('Origin',(116.959178380441,-0.799999999999986,51.0204257716897));
#193358=CARTESIAN_POINT('Origin',(116.193130296394,-0.799999999999986,63.870772219933));
#193359=CARTESIAN_POINT('',(115.696390542482,-0.299999999999985,66.4262639632045));
#193360=CARTESIAN_POINT('',(115.638794282839,-0.299999999999985,66.7225695534067));
#193361=CARTESIAN_POINT('',(115.696390542482,-0.299999999999985,66.4262639632045));
#193362=CARTESIAN_POINT('Origin',(118.62794428911,1.45439216225896E-14,
51.3448026236171));
#193363=CARTESIAN_POINT('Origin',(118.62794428911,1.45439216225896E-14,
51.3448026236171));
#193364=CARTESIAN_POINT('Origin',(116.193130296394,-0.299999999999985,63.870772219933));
#193365=CARTESIAN_POINT('',(115.19658669022,-0.299999999999985,66.3771101156678));
#193366=CARTESIAN_POINT('',(115.139163146118,-0.299999999999985,66.6725271658766));
#193367=CARTESIAN_POINT('',(115.19658669022,-0.299999999999985,66.3771101156678));
#193368=CARTESIAN_POINT('Origin',(116.959178380441,-0.299999999999985,51.0204257716897));
#193369=CARTESIAN_POINT('Origin',(116.959178380441,-0.299999999999985,51.0204257716897));
#193370=CARTESIAN_POINT('Origin',(115.702316793845,-0.299999999999985,63.7753672634838));
#193371=CARTESIAN_POINT('Origin',(118.13713078656,1.45439216225896E-14,
51.2493976671679));
#193372=CARTESIAN_POINT('Origin',(118.13713078656,1.45439216225896E-14,
51.2493976671679));
#193373=CARTESIAN_POINT('Origin',(114.720689788746,-0.799999999999986,63.5845573505853));
#193374=CARTESIAN_POINT('',(114.703297924294,-0.799999999999986,66.2944392218165));
#193375=CARTESIAN_POINT('',(114.645921753038,-0.799999999999986,66.5896125610739));
#193376=CARTESIAN_POINT('',(114.703297924294,-0.799999999999986,66.2944392218165));
#193377=CARTESIAN_POINT('',(114.209702236559,-0.799999999999986,66.2133472959115));
#193378=CARTESIAN_POINT('Origin',(116.959178380441,-0.799999999999986,51.0204257716897));
#193379=CARTESIAN_POINT('',(114.152379219848,-0.799999999999986,66.5082471801045));
#193380=CARTESIAN_POINT('',(114.209702236559,-0.799999999999986,66.2133472959115));
#193381=CARTESIAN_POINT('Origin',(116.959178380441,-0.799999999999986,51.0204257716897));
#193382=CARTESIAN_POINT('Origin',(115.211503291295,-0.799999999999986,63.6799623070345));
#193383=CARTESIAN_POINT('',(114.6998978325,-0.299999999999985,66.3119310904201));
#193384=CARTESIAN_POINT('',(114.642586607859,-0.299999999999985,66.6067703099759));
#193385=CARTESIAN_POINT('',(114.6998978325,-0.299999999999985,66.3119310904201));
#193386=CARTESIAN_POINT('Origin',(117.64631728401,1.45439216225896E-14,
51.1539927107186));
#193387=CARTESIAN_POINT('Origin',(117.64631728401,1.45439216225896E-14,
51.1539927107186));
#193388=CARTESIAN_POINT('Origin',(115.211503291295,-0.299999999999985,63.6799623070345));
#193389=CARTESIAN_POINT('',(114.206305352308,-0.299999999999985,66.2308226632179));
#193390=CARTESIAN_POINT('',(114.149047102056,-0.299999999999985,66.5253893545321));
#193391=CARTESIAN_POINT('',(114.206305352308,-0.299999999999985,66.2308226632179));
#193392=CARTESIAN_POINT('Origin',(116.959178380441,-0.299999999999985,51.0204257716897));
#193393=CARTESIAN_POINT('Origin',(116.959178380441,-0.299999999999985,51.0204257716897));
#193394=CARTESIAN_POINT('Origin',(114.720689788746,-0.299999999999985,63.5845573505853));
#193395=CARTESIAN_POINT('Origin',(117.155503781461,1.45439216225896E-14,
51.0585877542694));
#193396=CARTESIAN_POINT('Origin',(117.155503781461,1.45439216225896E-14,
51.0585877542694));
#193397=CARTESIAN_POINT('Origin',(113.739062783647,-0.799999999999986,63.3937474376868));
#193398=CARTESIAN_POINT('',(113.719197735921,-0.799999999999986,66.116352670368));
#193399=CARTESIAN_POINT('',(113.661868820446,-0.799999999999986,66.4112829009218));
#193400=CARTESIAN_POINT('',(113.719197735921,-0.799999999999986,66.116352670368));
#193401=CARTESIAN_POINT('',(113.231785396369,-0.799999999999986,66.0034503344807));
#193402=CARTESIAN_POINT('Origin',(116.959178380441,-0.799999999999986,51.0204257716897));
#193403=CARTESIAN_POINT('',(113.17439147404,-0.799999999999986,66.2987149946358));
#193404=CARTESIAN_POINT('',(113.231785396369,-0.799999999999986,66.0034503344807));
#193405=CARTESIAN_POINT('Origin',(116.959178380441,-0.799999999999986,51.0204257716897));
#193406=CARTESIAN_POINT('Origin',(114.229876286196,-0.799999999999986,63.489152394136));
#193407=CARTESIAN_POINT('',(113.715800495726,-0.299999999999985,66.1338298688407));
#193408=CARTESIAN_POINT('',(113.658536366685,-0.299999999999985,66.4284268037491));
#193409=CARTESIAN_POINT('',(113.715800495726,-0.299999999999985,66.1338298688407));
#193410=CARTESIAN_POINT('Origin',(116.664690278911,1.45439216225896E-14,
50.9631827978201));
#193411=CARTESIAN_POINT('Origin',(116.664690278911,1.45439216225896E-14,
50.9631827978201));
#193412=CARTESIAN_POINT('Origin',(114.229876286196,-0.299999999999985,63.489152394136));
#193413=CARTESIAN_POINT('',(113.228384233372,-0.299999999999985,66.0209477139188));
#193414=CARTESIAN_POINT('',(113.171055317897,-0.299999999999985,66.3158779444725));
#193415=CARTESIAN_POINT('',(113.228384233372,-0.299999999999985,66.0209477139188));
#193416=CARTESIAN_POINT('Origin',(116.959178380441,-0.299999999999985,51.0204257716897));
#193417=CARTESIAN_POINT('Origin',(116.959178380441,-0.299999999999985,51.0204257716897));
#193418=CARTESIAN_POINT('Origin',(113.739062783647,-0.299999999999985,63.3937474376868));
#193419=CARTESIAN_POINT('Origin',(116.173876776362,1.45439216225896E-14,
50.8677778413709));
#193420=CARTESIAN_POINT('Origin',(116.173876776362,1.45439216225896E-14,
50.8677778413709));
#193421=CARTESIAN_POINT('Origin',(114.581607361595,1.45439216225896E-14,
63.2519072664759));
#193422=CARTESIAN_POINT('Origin',(108.407383728608,3.45,47.5859740823384));
#193423=CARTESIAN_POINT('',(108.898197231158,3.45,47.6813790387876));
#193424=CARTESIAN_POINT('',(108.840954257288,3.45,47.9758671403173));
#193425=CARTESIAN_POINT('',(108.898197231158,3.45,47.6813790387876));
#193426=CARTESIAN_POINT('',(108.350140754738,3.45,47.8804621838681));
#193427=CARTESIAN_POINT('',(108.350140754738,3.45,47.8804621838681));
#193428=CARTESIAN_POINT('',(108.407383728608,3.45,47.5859740823384));
#193429=CARTESIAN_POINT('',(108.407383728608,3.45,47.5859740823384));
#193430=CARTESIAN_POINT('',(108.407383728608,3.45,47.5859740823384));
#193431=CARTESIAN_POINT('Origin',(108.898197231158,3.45,47.6813790387876));
#193432=CARTESIAN_POINT('',(108.898197231158,2.95,47.6813790387876));
#193433=CARTESIAN_POINT('',(108.840954257288,2.95,47.9758671403173));
#193434=CARTESIAN_POINT('',(108.898197231158,2.95,47.6813790387876));
#193435=CARTESIAN_POINT('',(108.840954257288,3.45,47.9758671403173));
#193436=CARTESIAN_POINT('',(108.898197231158,3.45,47.6813790387876));
#193437=CARTESIAN_POINT('Origin',(108.898197231158,2.95,47.6813790387876));
#193438=CARTESIAN_POINT('',(108.407383728608,2.95,47.5859740823384));
#193439=CARTESIAN_POINT('',(108.350140754738,2.95,47.8804621838681));
#193440=CARTESIAN_POINT('',(108.407383728608,2.95,47.5859740823384));
#193441=CARTESIAN_POINT('',(108.840954257288,2.95,47.9758671403173));
#193442=CARTESIAN_POINT('',(108.898197231158,2.95,47.6813790387876));
#193443=CARTESIAN_POINT('Origin',(108.407383728608,2.95,47.5859740823384));
#193444=CARTESIAN_POINT('',(108.350140754738,2.95,47.8804621838681));
#193445=CARTESIAN_POINT('',(108.407383728608,2.95,47.5859740823384));
#193446=CARTESIAN_POINT('Origin',(108.407383728608,2.65,47.5859740823384));
#193447=CARTESIAN_POINT('',(108.898197231158,2.65,47.6813790387876));
#193448=CARTESIAN_POINT('',(108.840954257288,2.65,47.9758671403173));
#193449=CARTESIAN_POINT('',(108.898197231158,2.65,47.6813790387876));
#193450=CARTESIAN_POINT('',(108.350140754738,2.65,47.8804621838681));
#193451=CARTESIAN_POINT('',(108.350140754738,2.65,47.8804621838681));
#193452=CARTESIAN_POINT('',(108.407383728608,2.65,47.5859740823384));
#193453=CARTESIAN_POINT('',(108.407383728608,2.65,47.5859740823384));
#193454=CARTESIAN_POINT('',(108.407383728608,2.65,47.5859740823384));
#193455=CARTESIAN_POINT('Origin',(108.898197231158,2.65,47.6813790387876));
#193456=CARTESIAN_POINT('',(108.898197231158,2.15,47.6813790387876));
#193457=CARTESIAN_POINT('',(108.840954257288,2.15,47.9758671403173));
#193458=CARTESIAN_POINT('',(108.898197231158,2.15,47.6813790387876));
#193459=CARTESIAN_POINT('',(108.840954257288,2.65,47.9758671403173));
#193460=CARTESIAN_POINT('',(108.898197231158,2.65,47.6813790387876));
#193461=CARTESIAN_POINT('Origin',(108.898197231158,2.15,47.6813790387876));
#193462=CARTESIAN_POINT('',(108.407383728608,2.15,47.5859740823384));
#193463=CARTESIAN_POINT('',(108.350140754738,2.15,47.8804621838681));
#193464=CARTESIAN_POINT('',(108.407383728608,2.15,47.5859740823384));
#193465=CARTESIAN_POINT('',(108.840954257288,2.15,47.9758671403173));
#193466=CARTESIAN_POINT('',(108.898197231158,2.15,47.6813790387876));
#193467=CARTESIAN_POINT('Origin',(108.407383728608,2.15,47.5859740823384));
#193468=CARTESIAN_POINT('',(108.350140754738,2.15,47.8804621838681));
#193469=CARTESIAN_POINT('',(108.407383728608,2.15,47.5859740823384));
#193470=CARTESIAN_POINT('Origin',(108.407383728608,1.85,47.5859740823384));
#193471=CARTESIAN_POINT('',(108.898197231158,1.85,47.6813790387876));
#193472=CARTESIAN_POINT('',(108.840954257288,1.85,47.9758671403173));
#193473=CARTESIAN_POINT('',(108.898197231158,1.85,47.6813790387876));
#193474=CARTESIAN_POINT('',(108.350140754738,1.85,47.8804621838681));
#193475=CARTESIAN_POINT('',(108.350140754738,1.85,47.8804621838681));
#193476=CARTESIAN_POINT('',(108.407383728608,1.85,47.5859740823384));
#193477=CARTESIAN_POINT('',(108.407383728608,1.85,47.5859740823384));
#193478=CARTESIAN_POINT('',(108.407383728608,1.85,47.5859740823384));
#193479=CARTESIAN_POINT('Origin',(108.898197231158,1.85,47.6813790387876));
#193480=CARTESIAN_POINT('',(108.898197231158,1.35,47.6813790387876));
#193481=CARTESIAN_POINT('',(108.840954257288,1.35,47.9758671403173));
#193482=CARTESIAN_POINT('',(108.898197231158,1.35,47.6813790387876));
#193483=CARTESIAN_POINT('',(108.840954257288,1.85,47.9758671403173));
#193484=CARTESIAN_POINT('',(108.898197231158,1.85,47.6813790387876));
#193485=CARTESIAN_POINT('Origin',(108.898197231158,1.35,47.6813790387876));
#193486=CARTESIAN_POINT('',(108.407383728608,1.35,47.5859740823384));
#193487=CARTESIAN_POINT('',(108.350140754738,1.35,47.8804621838681));
#193488=CARTESIAN_POINT('',(108.407383728608,1.35,47.5859740823384));
#193489=CARTESIAN_POINT('',(108.840954257288,1.35,47.9758671403173));
#193490=CARTESIAN_POINT('',(108.898197231158,1.35,47.6813790387876));
#193491=CARTESIAN_POINT('Origin',(108.407383728608,1.35,47.5859740823384));
#193492=CARTESIAN_POINT('',(108.350140754738,1.35,47.8804621838681));
#193493=CARTESIAN_POINT('',(108.407383728608,1.35,47.5859740823384));
#193494=CARTESIAN_POINT('Origin',(108.407383728608,1.05,47.5859740823384));
#193495=CARTESIAN_POINT('',(108.898197231158,1.05,47.6813790387876));
#193496=CARTESIAN_POINT('',(108.840954257288,1.05,47.9758671403173));
#193497=CARTESIAN_POINT('',(108.898197231158,1.05,47.6813790387876));
#193498=CARTESIAN_POINT('',(108.350140754738,1.05,47.8804621838681));
#193499=CARTESIAN_POINT('',(108.350140754738,1.05,47.8804621838681));
#193500=CARTESIAN_POINT('',(108.407383728608,1.05,47.5859740823384));
#193501=CARTESIAN_POINT('',(108.407383728608,1.05,47.5859740823384));
#193502=CARTESIAN_POINT('',(108.407383728608,1.05,47.5859740823384));
#193503=CARTESIAN_POINT('Origin',(108.898197231158,1.05,47.6813790387876));
#193504=CARTESIAN_POINT('',(108.898197231158,0.550000000000015,47.6813790387876));
#193505=CARTESIAN_POINT('',(108.840954257288,0.550000000000015,47.9758671403173));
#193506=CARTESIAN_POINT('',(108.898197231158,0.550000000000015,47.6813790387876));
#193507=CARTESIAN_POINT('',(108.840954257288,1.05,47.9758671403173));
#193508=CARTESIAN_POINT('',(108.898197231158,1.05,47.6813790387876));
#193509=CARTESIAN_POINT('Origin',(108.898197231158,0.550000000000015,47.6813790387876));
#193510=CARTESIAN_POINT('',(108.407383728608,0.550000000000015,47.5859740823384));
#193511=CARTESIAN_POINT('',(108.350140754738,0.550000000000015,47.8804621838681));
#193512=CARTESIAN_POINT('',(108.407383728608,0.550000000000015,47.5859740823384));
#193513=CARTESIAN_POINT('',(108.840954257288,0.550000000000015,47.9758671403173));
#193514=CARTESIAN_POINT('',(108.898197231158,0.550000000000015,47.6813790387876));
#193515=CARTESIAN_POINT('Origin',(108.407383728608,0.550000000000015,47.5859740823384));
#193516=CARTESIAN_POINT('',(108.350140754738,0.550000000000015,47.8804621838681));
#193517=CARTESIAN_POINT('',(108.407383728608,0.550000000000015,47.5859740823384));
#193518=CARTESIAN_POINT('Origin',(108.407383728608,0.250000000000015,47.5859740823384));
#193519=CARTESIAN_POINT('',(108.898197231158,0.250000000000015,47.6813790387876));
#193520=CARTESIAN_POINT('',(108.840954257288,0.250000000000015,47.9758671403173));
#193521=CARTESIAN_POINT('',(108.898197231158,0.250000000000015,47.6813790387876));
#193522=CARTESIAN_POINT('',(108.350140754738,0.250000000000015,47.8804621838681));
#193523=CARTESIAN_POINT('',(108.350140754738,0.250000000000015,47.8804621838681));
#193524=CARTESIAN_POINT('',(108.407383728608,0.250000000000015,47.5859740823384));
#193525=CARTESIAN_POINT('',(108.407383728608,0.250000000000015,47.5859740823384));
#193526=CARTESIAN_POINT('',(108.407383728608,0.250000000000015,47.5859740823384));
#193527=CARTESIAN_POINT('Origin',(108.898197231158,0.250000000000015,47.6813790387876));
#193528=CARTESIAN_POINT('',(108.898197231158,-0.249999999999985,47.6813790387876));
#193529=CARTESIAN_POINT('',(108.840954257288,-0.249999999999985,47.9758671403173));
#193530=CARTESIAN_POINT('',(108.898197231158,-0.249999999999985,47.6813790387876));
#193531=CARTESIAN_POINT('',(108.840954257288,0.250000000000015,47.9758671403173));
#193532=CARTESIAN_POINT('',(108.898197231158,0.250000000000015,47.6813790387876));
#193533=CARTESIAN_POINT('Origin',(108.898197231158,-0.249999999999985,47.6813790387876));
#193534=CARTESIAN_POINT('',(108.407383728608,-0.249999999999985,47.5859740823384));
#193535=CARTESIAN_POINT('',(108.350140754738,-0.249999999999985,47.8804621838681));
#193536=CARTESIAN_POINT('',(108.407383728608,-0.249999999999985,47.5859740823384));
#193537=CARTESIAN_POINT('',(108.840954257288,-0.249999999999985,47.9758671403173));
#193538=CARTESIAN_POINT('',(108.898197231158,-0.249999999999985,47.6813790387876));
#193539=CARTESIAN_POINT('Origin',(108.407383728608,-0.249999999999985,47.5859740823384));
#193540=CARTESIAN_POINT('',(108.350140754738,-0.249999999999985,47.8804621838681));
#193541=CARTESIAN_POINT('',(108.407383728608,-0.249999999999985,47.5859740823384));
#193542=CARTESIAN_POINT('Origin',(108.407383728608,-0.549999999999986,47.5859740823384));
#193543=CARTESIAN_POINT('',(108.898197231158,-0.549999999999986,47.6813790387876));
#193544=CARTESIAN_POINT('',(108.840954257288,-0.549999999999986,47.9758671403173));
#193545=CARTESIAN_POINT('',(108.898197231158,-0.549999999999986,47.6813790387876));
#193546=CARTESIAN_POINT('',(108.350140754738,-0.549999999999986,47.8804621838681));
#193547=CARTESIAN_POINT('',(108.350140754738,-0.549999999999986,47.8804621838681));
#193548=CARTESIAN_POINT('',(108.407383728608,-0.549999999999986,47.5859740823384));
#193549=CARTESIAN_POINT('',(108.407383728608,-0.549999999999986,47.5859740823384));
#193550=CARTESIAN_POINT('',(108.407383728608,-0.549999999999986,47.5859740823384));
#193551=CARTESIAN_POINT('Origin',(108.898197231158,-0.549999999999986,47.6813790387876));
#193552=CARTESIAN_POINT('',(108.898197231158,-1.05,47.6813790387876));
#193553=CARTESIAN_POINT('',(108.840954257288,-1.05,47.9758671403173));
#193554=CARTESIAN_POINT('',(108.898197231158,-1.05,47.6813790387876));
#193555=CARTESIAN_POINT('',(108.840954257288,-0.549999999999986,47.9758671403173));
#193556=CARTESIAN_POINT('',(108.898197231158,-0.549999999999986,47.6813790387876));
#193557=CARTESIAN_POINT('Origin',(108.898197231158,-1.05,47.6813790387876));
#193558=CARTESIAN_POINT('',(108.407383728608,-1.05,47.5859740823384));
#193559=CARTESIAN_POINT('',(108.350140754738,-1.05,47.8804621838681));
#193560=CARTESIAN_POINT('',(108.407383728608,-1.05,47.5859740823384));
#193561=CARTESIAN_POINT('',(108.840954257288,-1.05,47.9758671403173));
#193562=CARTESIAN_POINT('',(108.898197231158,-1.05,47.6813790387876));
#193563=CARTESIAN_POINT('Origin',(108.407383728608,-1.05,47.5859740823384));
#193564=CARTESIAN_POINT('',(108.350140754738,-1.05,47.8804621838681));
#193565=CARTESIAN_POINT('',(108.407383728608,-1.05,47.5859740823384));
#193566=CARTESIAN_POINT('Origin',(108.407383728608,-1.35,47.5859740823384));
#193567=CARTESIAN_POINT('',(108.898197231158,-1.35,47.6813790387876));
#193568=CARTESIAN_POINT('',(108.840954257288,-1.35,47.9758671403173));
#193569=CARTESIAN_POINT('',(108.898197231158,-1.35,47.6813790387876));
#193570=CARTESIAN_POINT('',(108.350140754738,-1.35,47.8804621838681));
#193571=CARTESIAN_POINT('',(108.350140754738,-1.35,47.8804621838681));
#193572=CARTESIAN_POINT('',(108.407383728608,-1.35,47.5859740823384));
#193573=CARTESIAN_POINT('',(108.407383728608,-1.35,47.5859740823384));
#193574=CARTESIAN_POINT('',(108.407383728608,-1.35,47.5859740823384));
#193575=CARTESIAN_POINT('Origin',(108.898197231158,-1.35,47.6813790387876));
#193576=CARTESIAN_POINT('',(108.898197231158,-1.85,47.6813790387876));
#193577=CARTESIAN_POINT('',(108.840954257288,-1.85,47.9758671403173));
#193578=CARTESIAN_POINT('',(108.898197231158,-1.85,47.6813790387876));
#193579=CARTESIAN_POINT('',(108.840954257288,-1.35,47.9758671403173));
#193580=CARTESIAN_POINT('',(108.898197231158,-1.35,47.6813790387876));
#193581=CARTESIAN_POINT('Origin',(108.898197231158,-1.85,47.6813790387876));
#193582=CARTESIAN_POINT('',(108.407383728608,-1.85,47.5859740823384));
#193583=CARTESIAN_POINT('',(108.350140754738,-1.85,47.8804621838681));
#193584=CARTESIAN_POINT('',(108.407383728608,-1.85,47.5859740823384));
#193585=CARTESIAN_POINT('',(108.840954257288,-1.85,47.9758671403173));
#193586=CARTESIAN_POINT('',(108.898197231158,-1.85,47.6813790387876));
#193587=CARTESIAN_POINT('Origin',(108.407383728608,-1.85,47.5859740823384));
#193588=CARTESIAN_POINT('',(108.350140754738,-1.85,47.8804621838681));
#193589=CARTESIAN_POINT('',(108.407383728608,-1.85,47.5859740823384));
#193590=CARTESIAN_POINT('Origin',(108.407383728608,-2.15,47.5859740823384));
#193591=CARTESIAN_POINT('',(108.898197231158,-2.15,47.6813790387876));
#193592=CARTESIAN_POINT('',(108.840954257288,-2.15,47.9758671403173));
#193593=CARTESIAN_POINT('',(108.898197231158,-2.15,47.6813790387876));
#193594=CARTESIAN_POINT('',(108.350140754738,-2.15,47.8804621838681));
#193595=CARTESIAN_POINT('',(108.350140754738,-2.15,47.8804621838681));
#193596=CARTESIAN_POINT('',(108.407383728608,-2.15,47.5859740823384));
#193597=CARTESIAN_POINT('',(108.407383728608,-2.15,47.5859740823384));
#193598=CARTESIAN_POINT('',(108.407383728608,-2.15,47.5859740823384));
#193599=CARTESIAN_POINT('Origin',(108.898197231158,-2.15,47.6813790387876));
#193600=CARTESIAN_POINT('',(108.898197231158,-2.65,47.6813790387876));
#193601=CARTESIAN_POINT('',(108.840954257288,-2.65,47.9758671403173));
#193602=CARTESIAN_POINT('',(108.898197231158,-2.65,47.6813790387876));
#193603=CARTESIAN_POINT('',(108.840954257288,-2.15,47.9758671403173));
#193604=CARTESIAN_POINT('',(108.898197231158,-2.15,47.6813790387876));
#193605=CARTESIAN_POINT('Origin',(108.898197231158,-2.65,47.6813790387876));
#193606=CARTESIAN_POINT('',(108.407383728608,-2.65,47.5859740823384));
#193607=CARTESIAN_POINT('',(108.350140754738,-2.65,47.8804621838681));
#193608=CARTESIAN_POINT('',(108.407383728608,-2.65,47.5859740823384));
#193609=CARTESIAN_POINT('',(108.840954257288,-2.65,47.9758671403173));
#193610=CARTESIAN_POINT('',(108.898197231158,-2.65,47.6813790387876));
#193611=CARTESIAN_POINT('Origin',(108.407383728608,-2.65,47.5859740823384));
#193612=CARTESIAN_POINT('',(108.350140754738,-2.65,47.8804621838681));
#193613=CARTESIAN_POINT('',(108.407383728608,-2.65,47.5859740823384));
#193614=CARTESIAN_POINT('Origin',(108.407383728608,-2.95,47.5859740823384));
#193615=CARTESIAN_POINT('',(108.898197231158,-2.95,47.6813790387876));
#193616=CARTESIAN_POINT('',(108.840954257288,-2.95,47.9758671403173));
#193617=CARTESIAN_POINT('',(108.898197231158,-2.95,47.6813790387876));
#193618=CARTESIAN_POINT('',(108.350140754738,-2.95,47.8804621838681));
#193619=CARTESIAN_POINT('',(108.350140754738,-2.95,47.8804621838681));
#193620=CARTESIAN_POINT('',(108.407383728608,-2.95,47.5859740823384));
#193621=CARTESIAN_POINT('',(108.407383728608,-2.95,47.5859740823384));
#193622=CARTESIAN_POINT('',(108.407383728608,-2.95,47.5859740823384));
#193623=CARTESIAN_POINT('Origin',(108.898197231158,-2.95,47.6813790387876));
#193624=CARTESIAN_POINT('',(108.898197231158,-3.45,47.6813790387876));
#193625=CARTESIAN_POINT('',(108.840954257288,-3.45,47.9758671403173));
#193626=CARTESIAN_POINT('',(108.898197231158,-3.45,47.6813790387876));
#193627=CARTESIAN_POINT('',(108.840954257288,-2.95,47.9758671403173));
#193628=CARTESIAN_POINT('',(108.898197231158,-2.95,47.6813790387876));
#193629=CARTESIAN_POINT('Origin',(108.898197231158,-3.45,47.6813790387876));
#193630=CARTESIAN_POINT('',(108.407383728608,-3.45,47.5859740823384));
#193631=CARTESIAN_POINT('',(108.350140754738,-3.45,47.8804621838681));
#193632=CARTESIAN_POINT('',(108.407383728608,-3.45,47.5859740823384));
#193633=CARTESIAN_POINT('',(108.840954257288,-3.45,47.9758671403173));
#193634=CARTESIAN_POINT('',(108.898197231158,-3.45,47.6813790387876));
#193635=CARTESIAN_POINT('Origin',(108.407383728608,-3.45,47.5859740823384));
#193636=CARTESIAN_POINT('',(108.350140754738,-3.45,47.8804621838681));
#193637=CARTESIAN_POINT('',(108.407383728608,-3.45,47.5859740823384));
#193638=CARTESIAN_POINT('Origin',(113.904494957163,-8.55,48.65450959457));
#193639=CARTESIAN_POINT('',(114.395308459712,-8.55,48.7499145510193));
#193640=CARTESIAN_POINT('',(114.338065485842,-8.55,49.044402652549));
#193641=CARTESIAN_POINT('',(114.395308459712,-8.55,48.7499145510193));
#193642=CARTESIAN_POINT('',(113.847251983293,-8.55,48.9489976960997));
#193643=CARTESIAN_POINT('',(113.847251983293,-8.55,48.9489976960997));
#193644=CARTESIAN_POINT('',(113.904494957163,-8.55,48.65450959457));
#193645=CARTESIAN_POINT('',(113.904494957163,-8.55,48.65450959457));
#193646=CARTESIAN_POINT('',(113.904494957163,-8.55,48.65450959457));
#193647=CARTESIAN_POINT('Origin',(114.395308459712,-8.55,48.7499145510193));
#193648=CARTESIAN_POINT('',(114.395308459712,-9.05,48.7499145510193));
#193649=CARTESIAN_POINT('',(114.338065485842,-9.05,49.044402652549));
#193650=CARTESIAN_POINT('',(114.395308459712,-9.05,48.7499145510193));
#193651=CARTESIAN_POINT('',(114.338065485842,-8.55,49.044402652549));
#193652=CARTESIAN_POINT('',(114.395308459712,-8.55,48.7499145510193));
#193653=CARTESIAN_POINT('Origin',(114.395308459712,-9.05,48.7499145510193));
#193654=CARTESIAN_POINT('',(113.904494957163,-9.05,48.65450959457));
#193655=CARTESIAN_POINT('',(113.847251983293,-9.05,48.9489976960997));
#193656=CARTESIAN_POINT('',(113.904494957163,-9.05,48.65450959457));
#193657=CARTESIAN_POINT('',(114.338065485842,-9.05,49.044402652549));
#193658=CARTESIAN_POINT('',(114.395308459712,-9.05,48.7499145510193));
#193659=CARTESIAN_POINT('Origin',(113.904494957163,-9.05,48.65450959457));
#193660=CARTESIAN_POINT('',(113.847251983293,-9.05,48.9489976960997));
#193661=CARTESIAN_POINT('',(113.904494957163,-9.05,48.65450959457));
#193662=CARTESIAN_POINT('Origin',(114.689796561242,-8.55,48.8071575248888));
#193663=CARTESIAN_POINT('',(115.180610063791,-8.55,48.9025624813381));
#193664=CARTESIAN_POINT('',(115.123367089922,-8.55,49.1970505828678));
#193665=CARTESIAN_POINT('',(115.180610063791,-8.55,48.9025624813381));
#193666=CARTESIAN_POINT('',(114.632553587372,-8.55,49.1016456264185));
#193667=CARTESIAN_POINT('',(114.632553587372,-8.55,49.1016456264185));
#193668=CARTESIAN_POINT('',(114.689796561242,-8.55,48.8071575248888));
#193669=CARTESIAN_POINT('',(114.689796561242,-8.55,48.8071575248888));
#193670=CARTESIAN_POINT('',(114.689796561242,-8.55,48.8071575248888));
#193671=CARTESIAN_POINT('Origin',(115.180610063791,-8.55,48.9025624813381));
#193672=CARTESIAN_POINT('',(115.180610063791,-9.05,48.9025624813381));
#193673=CARTESIAN_POINT('',(115.123367089922,-9.05,49.1970505828678));
#193674=CARTESIAN_POINT('',(115.180610063791,-9.05,48.9025624813381));
#193675=CARTESIAN_POINT('',(115.123367089922,-8.55,49.1970505828678));
#193676=CARTESIAN_POINT('',(115.180610063791,-8.55,48.9025624813381));
#193677=CARTESIAN_POINT('Origin',(115.180610063791,-9.05,48.9025624813381));
#193678=CARTESIAN_POINT('',(114.689796561242,-9.05,48.8071575248888));
#193679=CARTESIAN_POINT('',(114.632553587372,-9.05,49.1016456264185));
#193680=CARTESIAN_POINT('',(114.689796561242,-9.05,48.8071575248888));
#193681=CARTESIAN_POINT('',(115.123367089922,-9.05,49.1970505828678));
#193682=CARTESIAN_POINT('',(115.180610063791,-9.05,48.9025624813381));
#193683=CARTESIAN_POINT('Origin',(114.689796561242,-9.05,48.8071575248888));
#193684=CARTESIAN_POINT('',(114.632553587372,-9.05,49.1016456264185));
#193685=CARTESIAN_POINT('',(114.689796561242,-9.05,48.8071575248888));
#193686=CARTESIAN_POINT('Origin',(115.475098165321,-8.55,48.9598054552076));
#193687=CARTESIAN_POINT('',(115.96591166787,-8.55,49.0552104116569));
#193688=CARTESIAN_POINT('',(115.908668694001,-8.55,49.3496985131866));
#193689=CARTESIAN_POINT('',(115.96591166787,-8.55,49.0552104116569));
#193690=CARTESIAN_POINT('',(115.417855191451,-8.55,49.2542935567373));
#193691=CARTESIAN_POINT('',(115.417855191451,-8.55,49.2542935567373));
#193692=CARTESIAN_POINT('',(115.475098165321,-8.55,48.9598054552076));
#193693=CARTESIAN_POINT('',(115.475098165321,-8.55,48.9598054552076));
#193694=CARTESIAN_POINT('',(115.475098165321,-8.55,48.9598054552076));
#193695=CARTESIAN_POINT('Origin',(115.96591166787,-8.55,49.0552104116569));
#193696=CARTESIAN_POINT('',(115.96591166787,-9.05,49.0552104116569));
#193697=CARTESIAN_POINT('',(115.908668694001,-9.05,49.3496985131866));
#193698=CARTESIAN_POINT('',(115.96591166787,-9.05,49.0552104116569));
#193699=CARTESIAN_POINT('',(115.908668694001,-8.55,49.3496985131866));
#193700=CARTESIAN_POINT('',(115.96591166787,-8.55,49.0552104116569));
#193701=CARTESIAN_POINT('Origin',(115.96591166787,-9.05,49.0552104116569));
#193702=CARTESIAN_POINT('',(115.475098165321,-9.05,48.9598054552076));
#193703=CARTESIAN_POINT('',(115.417855191451,-9.05,49.2542935567373));
#193704=CARTESIAN_POINT('',(115.475098165321,-9.05,48.9598054552076));
#193705=CARTESIAN_POINT('',(115.908668694001,-9.05,49.3496985131866));
#193706=CARTESIAN_POINT('',(115.96591166787,-9.05,49.0552104116569));
#193707=CARTESIAN_POINT('Origin',(115.475098165321,-9.05,48.9598054552076));
#193708=CARTESIAN_POINT('',(115.417855191451,-9.05,49.2542935567373));
#193709=CARTESIAN_POINT('',(115.475098165321,-9.05,48.9598054552076));
#193710=CARTESIAN_POINT('Origin',(116.2603997694,-8.55,49.1124533855264));
#193711=CARTESIAN_POINT('',(116.75121327195,-8.55,49.2078583419757));
#193712=CARTESIAN_POINT('',(116.69397029808,-8.55,49.5023464435054));
#193713=CARTESIAN_POINT('',(116.75121327195,-8.55,49.2078583419757));
#193714=CARTESIAN_POINT('',(116.203156795531,-8.55,49.4069414870561));
#193715=CARTESIAN_POINT('',(116.203156795531,-8.55,49.4069414870561));
#193716=CARTESIAN_POINT('',(116.2603997694,-8.55,49.1124533855264));
#193717=CARTESIAN_POINT('',(116.2603997694,-8.55,49.1124533855264));
#193718=CARTESIAN_POINT('',(116.2603997694,-8.55,49.1124533855264));
#193719=CARTESIAN_POINT('Origin',(116.75121327195,-8.55,49.2078583419757));
#193720=CARTESIAN_POINT('',(116.75121327195,-9.05,49.2078583419757));
#193721=CARTESIAN_POINT('',(116.69397029808,-9.05,49.5023464435054));
#193722=CARTESIAN_POINT('',(116.75121327195,-9.05,49.2078583419757));
#193723=CARTESIAN_POINT('',(116.69397029808,-8.55,49.5023464435054));
#193724=CARTESIAN_POINT('',(116.75121327195,-8.55,49.2078583419757));
#193725=CARTESIAN_POINT('Origin',(116.75121327195,-9.05,49.2078583419757));
#193726=CARTESIAN_POINT('',(116.2603997694,-9.05,49.1124533855264));
#193727=CARTESIAN_POINT('',(116.203156795531,-9.05,49.4069414870561));
#193728=CARTESIAN_POINT('',(116.2603997694,-9.05,49.1124533855264));
#193729=CARTESIAN_POINT('',(116.69397029808,-9.05,49.5023464435054));
#193730=CARTESIAN_POINT('',(116.75121327195,-9.05,49.2078583419757));
#193731=CARTESIAN_POINT('Origin',(116.2603997694,-9.05,49.1124533855264));
#193732=CARTESIAN_POINT('',(116.203156795531,-9.05,49.4069414870561));
#193733=CARTESIAN_POINT('',(116.2603997694,-9.05,49.1124533855264));
#193734=CARTESIAN_POINT('Origin',(117.045701373479,-8.55,49.2651013158452));
#193735=CARTESIAN_POINT('',(117.536514876029,-8.55,49.3605062722945));
#193736=CARTESIAN_POINT('',(117.479271902159,-8.55,49.6549943738242));
#193737=CARTESIAN_POINT('',(117.536514876029,-8.55,49.3605062722945));
#193738=CARTESIAN_POINT('',(116.98845839961,-8.55,49.5595894173749));
#193739=CARTESIAN_POINT('',(116.98845839961,-8.55,49.5595894173749));
#193740=CARTESIAN_POINT('',(117.045701373479,-8.55,49.2651013158452));
#193741=CARTESIAN_POINT('',(117.045701373479,-8.55,49.2651013158452));
#193742=CARTESIAN_POINT('',(117.045701373479,-8.55,49.2651013158452));
#193743=CARTESIAN_POINT('Origin',(117.536514876029,-8.55,49.3605062722945));
#193744=CARTESIAN_POINT('',(117.536514876029,-9.05,49.3605062722945));
#193745=CARTESIAN_POINT('',(117.479271902159,-9.05,49.6549943738242));
#193746=CARTESIAN_POINT('',(117.536514876029,-9.05,49.3605062722945));
#193747=CARTESIAN_POINT('',(117.479271902159,-8.55,49.6549943738242));
#193748=CARTESIAN_POINT('',(117.536514876029,-8.55,49.3605062722945));
#193749=CARTESIAN_POINT('Origin',(117.536514876029,-9.05,49.3605062722945));
#193750=CARTESIAN_POINT('',(117.045701373479,-9.05,49.2651013158452));
#193751=CARTESIAN_POINT('',(116.98845839961,-9.05,49.5595894173749));
#193752=CARTESIAN_POINT('',(117.045701373479,-9.05,49.2651013158452));
#193753=CARTESIAN_POINT('',(117.479271902159,-9.05,49.6549943738242));
#193754=CARTESIAN_POINT('',(117.536514876029,-9.05,49.3605062722945));
#193755=CARTESIAN_POINT('Origin',(117.045701373479,-9.05,49.2651013158452));
#193756=CARTESIAN_POINT('',(116.98845839961,-9.05,49.5595894173749));
#193757=CARTESIAN_POINT('',(117.045701373479,-9.05,49.2651013158452));
#193758=CARTESIAN_POINT('Origin',(117.831002977559,-8.55,49.417749246164));
#193759=CARTESIAN_POINT('',(118.321816480108,-8.55,49.5131542026133));
#193760=CARTESIAN_POINT('',(118.264573506239,-8.55,49.807642304143));
#193761=CARTESIAN_POINT('',(118.321816480108,-8.55,49.5131542026133));
#193762=CARTESIAN_POINT('',(117.773760003689,-8.55,49.7122373476937));
#193763=CARTESIAN_POINT('',(117.773760003689,-8.55,49.7122373476937));
#193764=CARTESIAN_POINT('',(117.831002977559,-8.55,49.417749246164));
#193765=CARTESIAN_POINT('',(117.831002977559,-8.55,49.417749246164));
#193766=CARTESIAN_POINT('',(117.831002977559,-8.55,49.417749246164));
#193767=CARTESIAN_POINT('Origin',(118.321816480108,-8.55,49.5131542026133));
#193768=CARTESIAN_POINT('',(118.321816480108,-9.05,49.5131542026133));
#193769=CARTESIAN_POINT('',(118.264573506239,-9.05,49.807642304143));
#193770=CARTESIAN_POINT('',(118.321816480108,-9.05,49.5131542026133));
#193771=CARTESIAN_POINT('',(118.264573506239,-8.55,49.807642304143));
#193772=CARTESIAN_POINT('',(118.321816480108,-8.55,49.5131542026133));
#193773=CARTESIAN_POINT('Origin',(118.321816480108,-9.05,49.5131542026133));
#193774=CARTESIAN_POINT('',(117.831002977559,-9.05,49.417749246164));
#193775=CARTESIAN_POINT('',(117.773760003689,-9.05,49.7122373476937));
#193776=CARTESIAN_POINT('',(117.831002977559,-9.05,49.417749246164));
#193777=CARTESIAN_POINT('',(118.264573506239,-9.05,49.807642304143));
#193778=CARTESIAN_POINT('',(118.321816480108,-9.05,49.5131542026133));
#193779=CARTESIAN_POINT('Origin',(117.831002977559,-9.05,49.417749246164));
#193780=CARTESIAN_POINT('',(117.773760003689,-9.05,49.7122373476937));
#193781=CARTESIAN_POINT('',(117.831002977559,-9.05,49.417749246164));
#193782=CARTESIAN_POINT('Origin',(118.616304581638,-8.55,49.5703971764828));
#193783=CARTESIAN_POINT('',(119.107118084187,-8.55,49.6658021329321));
#193784=CARTESIAN_POINT('',(119.049875110318,-8.55,49.9602902344618));
#193785=CARTESIAN_POINT('',(119.107118084187,-8.55,49.6658021329321));
#193786=CARTESIAN_POINT('',(118.559061607768,-8.55,49.8648852780125));
#193787=CARTESIAN_POINT('',(118.559061607768,-8.55,49.8648852780125));
#193788=CARTESIAN_POINT('',(118.616304581638,-8.55,49.5703971764828));
#193789=CARTESIAN_POINT('',(118.616304581638,-8.55,49.5703971764828));
#193790=CARTESIAN_POINT('',(118.616304581638,-8.55,49.5703971764828));
#193791=CARTESIAN_POINT('Origin',(119.107118084187,-8.55,49.6658021329321));
#193792=CARTESIAN_POINT('',(119.107118084187,-9.05,49.6658021329321));
#193793=CARTESIAN_POINT('',(119.049875110318,-9.05,49.9602902344618));
#193794=CARTESIAN_POINT('',(119.107118084187,-9.05,49.6658021329321));
#193795=CARTESIAN_POINT('',(119.049875110318,-8.55,49.9602902344618));
#193796=CARTESIAN_POINT('',(119.107118084187,-8.55,49.6658021329321));
#193797=CARTESIAN_POINT('Origin',(119.107118084187,-9.05,49.6658021329321));
#193798=CARTESIAN_POINT('',(118.616304581638,-9.05,49.5703971764828));
#193799=CARTESIAN_POINT('',(118.559061607768,-9.05,49.8648852780125));
#193800=CARTESIAN_POINT('',(118.616304581638,-9.05,49.5703971764828));
#193801=CARTESIAN_POINT('',(119.049875110318,-9.05,49.9602902344618));
#193802=CARTESIAN_POINT('',(119.107118084187,-9.05,49.6658021329321));
#193803=CARTESIAN_POINT('Origin',(118.616304581638,-9.05,49.5703971764828));
#193804=CARTESIAN_POINT('',(118.559061607768,-9.05,49.8648852780125));
#193805=CARTESIAN_POINT('',(118.616304581638,-9.05,49.5703971764828));
#193806=CARTESIAN_POINT('Origin',(119.401606185717,-8.55,49.7230451068016));
#193807=CARTESIAN_POINT('',(119.892419688267,-8.55,49.8184500632509));
#193808=CARTESIAN_POINT('',(119.835176714397,-8.55,50.1129381647806));
#193809=CARTESIAN_POINT('',(119.892419688267,-8.55,49.8184500632509));
#193810=CARTESIAN_POINT('',(119.344363211847,-8.55,50.0175332083313));
#193811=CARTESIAN_POINT('',(119.344363211847,-8.55,50.0175332083313));
#193812=CARTESIAN_POINT('',(119.401606185717,-8.55,49.7230451068016));
#193813=CARTESIAN_POINT('',(119.401606185717,-8.55,49.7230451068016));
#193814=CARTESIAN_POINT('',(119.401606185717,-8.55,49.7230451068016));
#193815=CARTESIAN_POINT('Origin',(119.892419688267,-8.55,49.8184500632509));
#193816=CARTESIAN_POINT('',(119.892419688267,-9.05,49.8184500632509));
#193817=CARTESIAN_POINT('',(119.835176714397,-9.05,50.1129381647806));
#193818=CARTESIAN_POINT('',(119.892419688267,-9.05,49.8184500632509));
#193819=CARTESIAN_POINT('',(119.835176714397,-8.55,50.1129381647806));
#193820=CARTESIAN_POINT('',(119.892419688267,-8.55,49.8184500632509));
#193821=CARTESIAN_POINT('Origin',(119.892419688267,-9.05,49.8184500632509));
#193822=CARTESIAN_POINT('',(119.401606185717,-9.05,49.7230451068016));
#193823=CARTESIAN_POINT('',(119.344363211847,-9.05,50.0175332083313));
#193824=CARTESIAN_POINT('',(119.401606185717,-9.05,49.7230451068016));
#193825=CARTESIAN_POINT('',(119.835176714397,-9.05,50.1129381647806));
#193826=CARTESIAN_POINT('',(119.892419688267,-9.05,49.8184500632509));
#193827=CARTESIAN_POINT('Origin',(119.401606185717,-9.05,49.7230451068016));
#193828=CARTESIAN_POINT('',(119.344363211847,-9.05,50.0175332083313));
#193829=CARTESIAN_POINT('',(119.401606185717,-9.05,49.7230451068016));
#193830=CARTESIAN_POINT('Origin',(120.186907789796,-8.55,49.8756930371204));
#193831=CARTESIAN_POINT('',(120.677721292346,-8.55,49.9710979935697));
#193832=CARTESIAN_POINT('',(120.620478318476,-8.55,50.2655860950994));
#193833=CARTESIAN_POINT('',(120.677721292346,-8.55,49.9710979935697));
#193834=CARTESIAN_POINT('',(120.129664815927,-8.55,50.1701811386501));
#193835=CARTESIAN_POINT('',(120.129664815927,-8.55,50.1701811386501));
#193836=CARTESIAN_POINT('',(120.186907789796,-8.55,49.8756930371204));
#193837=CARTESIAN_POINT('',(120.186907789796,-8.55,49.8756930371204));
#193838=CARTESIAN_POINT('',(120.186907789796,-8.55,49.8756930371204));
#193839=CARTESIAN_POINT('Origin',(120.677721292346,-8.55,49.9710979935697));
#193840=CARTESIAN_POINT('',(120.677721292346,-9.05,49.9710979935697));
#193841=CARTESIAN_POINT('',(120.620478318476,-9.05,50.2655860950994));
#193842=CARTESIAN_POINT('',(120.677721292346,-9.05,49.9710979935697));
#193843=CARTESIAN_POINT('',(120.620478318476,-8.55,50.2655860950994));
#193844=CARTESIAN_POINT('',(120.677721292346,-8.55,49.9710979935697));
#193845=CARTESIAN_POINT('Origin',(120.677721292346,-9.05,49.9710979935697));
#193846=CARTESIAN_POINT('',(120.186907789796,-9.05,49.8756930371204));
#193847=CARTESIAN_POINT('',(120.129664815927,-9.05,50.1701811386501));
#193848=CARTESIAN_POINT('',(120.186907789796,-9.05,49.8756930371204));
#193849=CARTESIAN_POINT('',(120.620478318476,-9.05,50.2655860950994));
#193850=CARTESIAN_POINT('',(120.677721292346,-9.05,49.9710979935697));
#193851=CARTESIAN_POINT('Origin',(120.186907789796,-9.05,49.8756930371204));
#193852=CARTESIAN_POINT('',(120.129664815927,-9.05,50.1701811386501));
#193853=CARTESIAN_POINT('',(120.186907789796,-9.05,49.8756930371204));
#193854=CARTESIAN_POINT('Origin',(125.684019018351,-2.95,50.944228549352));
#193855=CARTESIAN_POINT('',(126.1748325209,-2.95,51.0396335058013));
#193856=CARTESIAN_POINT('',(126.117589547031,-2.95,51.334121607331));
#193857=CARTESIAN_POINT('',(126.1748325209,-2.95,51.0396335058013));
#193858=CARTESIAN_POINT('',(125.626776044481,-2.95,51.2387166508817));
#193859=CARTESIAN_POINT('',(125.626776044481,-2.95,51.2387166508817));
#193860=CARTESIAN_POINT('',(125.684019018351,-2.95,50.944228549352));
#193861=CARTESIAN_POINT('',(125.684019018351,-2.95,50.944228549352));
#193862=CARTESIAN_POINT('',(125.684019018351,-2.95,50.944228549352));
#193863=CARTESIAN_POINT('Origin',(126.1748325209,-2.95,51.0396335058013));
#193864=CARTESIAN_POINT('',(126.1748325209,-3.45,51.0396335058013));
#193865=CARTESIAN_POINT('',(126.117589547031,-3.45,51.334121607331));
#193866=CARTESIAN_POINT('',(126.1748325209,-3.45,51.0396335058013));
#193867=CARTESIAN_POINT('',(126.117589547031,-2.95,51.334121607331));
#193868=CARTESIAN_POINT('',(126.1748325209,-2.95,51.0396335058013));
#193869=CARTESIAN_POINT('Origin',(126.1748325209,-3.45,51.0396335058013));
#193870=CARTESIAN_POINT('',(125.684019018351,-3.45,50.944228549352));
#193871=CARTESIAN_POINT('',(125.626776044481,-3.45,51.2387166508817));
#193872=CARTESIAN_POINT('',(125.684019018351,-3.45,50.944228549352));
#193873=CARTESIAN_POINT('',(126.117589547031,-3.45,51.334121607331));
#193874=CARTESIAN_POINT('',(126.1748325209,-3.45,51.0396335058013));
#193875=CARTESIAN_POINT('Origin',(125.684019018351,-3.45,50.944228549352));
#193876=CARTESIAN_POINT('',(125.626776044481,-3.45,51.2387166508817));
#193877=CARTESIAN_POINT('',(125.684019018351,-3.45,50.944228549352));
#193878=CARTESIAN_POINT('Origin',(125.684019018351,-2.15,50.944228549352));
#193879=CARTESIAN_POINT('',(126.1748325209,-2.15,51.0396335058013));
#193880=CARTESIAN_POINT('',(126.117589547031,-2.15,51.334121607331));
#193881=CARTESIAN_POINT('',(126.1748325209,-2.15,51.0396335058013));
#193882=CARTESIAN_POINT('',(125.626776044481,-2.15,51.2387166508817));
#193883=CARTESIAN_POINT('',(125.626776044481,-2.15,51.2387166508817));
#193884=CARTESIAN_POINT('',(125.684019018351,-2.15,50.944228549352));
#193885=CARTESIAN_POINT('',(125.684019018351,-2.15,50.944228549352));
#193886=CARTESIAN_POINT('',(125.684019018351,-2.15,50.944228549352));
#193887=CARTESIAN_POINT('Origin',(126.1748325209,-2.15,51.0396335058013));
#193888=CARTESIAN_POINT('',(126.1748325209,-2.65,51.0396335058013));
#193889=CARTESIAN_POINT('',(126.117589547031,-2.65,51.334121607331));
#193890=CARTESIAN_POINT('',(126.1748325209,-2.65,51.0396335058013));
#193891=CARTESIAN_POINT('',(126.117589547031,-2.15,51.334121607331));
#193892=CARTESIAN_POINT('',(126.1748325209,-2.15,51.0396335058013));
#193893=CARTESIAN_POINT('Origin',(126.1748325209,-2.65,51.0396335058013));
#193894=CARTESIAN_POINT('',(125.684019018351,-2.65,50.944228549352));
#193895=CARTESIAN_POINT('',(125.626776044481,-2.65,51.2387166508817));
#193896=CARTESIAN_POINT('',(125.684019018351,-2.65,50.944228549352));
#193897=CARTESIAN_POINT('',(126.117589547031,-2.65,51.334121607331));
#193898=CARTESIAN_POINT('',(126.1748325209,-2.65,51.0396335058013));
#193899=CARTESIAN_POINT('Origin',(125.684019018351,-2.65,50.944228549352));
#193900=CARTESIAN_POINT('',(125.626776044481,-2.65,51.2387166508817));
#193901=CARTESIAN_POINT('',(125.684019018351,-2.65,50.944228549352));
#193902=CARTESIAN_POINT('Origin',(125.684019018351,-1.35,50.944228549352));
#193903=CARTESIAN_POINT('',(126.1748325209,-1.35,51.0396335058013));
#193904=CARTESIAN_POINT('',(126.117589547031,-1.35,51.334121607331));
#193905=CARTESIAN_POINT('',(126.1748325209,-1.35,51.0396335058013));
#193906=CARTESIAN_POINT('',(125.626776044481,-1.35,51.2387166508817));
#193907=CARTESIAN_POINT('',(125.626776044481,-1.35,51.2387166508817));
#193908=CARTESIAN_POINT('',(125.684019018351,-1.35,50.944228549352));
#193909=CARTESIAN_POINT('',(125.684019018351,-1.35,50.944228549352));
#193910=CARTESIAN_POINT('',(125.684019018351,-1.35,50.944228549352));
#193911=CARTESIAN_POINT('Origin',(126.1748325209,-1.35,51.0396335058013));
#193912=CARTESIAN_POINT('',(126.1748325209,-1.85,51.0396335058013));
#193913=CARTESIAN_POINT('',(126.117589547031,-1.85,51.334121607331));
#193914=CARTESIAN_POINT('',(126.1748325209,-1.85,51.0396335058013));
#193915=CARTESIAN_POINT('',(126.117589547031,-1.35,51.334121607331));
#193916=CARTESIAN_POINT('',(126.1748325209,-1.35,51.0396335058013));
#193917=CARTESIAN_POINT('Origin',(126.1748325209,-1.85,51.0396335058013));
#193918=CARTESIAN_POINT('',(125.684019018351,-1.85,50.944228549352));
#193919=CARTESIAN_POINT('',(125.626776044481,-1.85,51.2387166508817));
#193920=CARTESIAN_POINT('',(125.684019018351,-1.85,50.944228549352));
#193921=CARTESIAN_POINT('',(126.117589547031,-1.85,51.334121607331));
#193922=CARTESIAN_POINT('',(126.1748325209,-1.85,51.0396335058013));
#193923=CARTESIAN_POINT('Origin',(125.684019018351,-1.85,50.944228549352));
#193924=CARTESIAN_POINT('',(125.626776044481,-1.85,51.2387166508817));
#193925=CARTESIAN_POINT('',(125.684019018351,-1.85,50.944228549352));
#193926=CARTESIAN_POINT('Origin',(125.684019018351,-0.549999999999986,50.944228549352));
#193927=CARTESIAN_POINT('',(126.1748325209,-0.549999999999986,51.0396335058013));
#193928=CARTESIAN_POINT('',(126.117589547031,-0.549999999999986,51.334121607331));
#193929=CARTESIAN_POINT('',(126.1748325209,-0.549999999999986,51.0396335058013));
#193930=CARTESIAN_POINT('',(125.626776044481,-0.549999999999986,51.2387166508817));
#193931=CARTESIAN_POINT('',(125.626776044481,-0.549999999999986,51.2387166508817));
#193932=CARTESIAN_POINT('',(125.684019018351,-0.549999999999986,50.944228549352));
#193933=CARTESIAN_POINT('',(125.684019018351,-0.549999999999986,50.944228549352));
#193934=CARTESIAN_POINT('',(125.684019018351,-0.549999999999986,50.944228549352));
#193935=CARTESIAN_POINT('Origin',(126.1748325209,-0.549999999999986,51.0396335058013));
#193936=CARTESIAN_POINT('',(126.1748325209,-1.05,51.0396335058013));
#193937=CARTESIAN_POINT('',(126.117589547031,-1.05,51.334121607331));
#193938=CARTESIAN_POINT('',(126.1748325209,-1.05,51.0396335058013));
#193939=CARTESIAN_POINT('',(126.117589547031,-0.549999999999986,51.334121607331));
#193940=CARTESIAN_POINT('',(126.1748325209,-0.549999999999986,51.0396335058013));
#193941=CARTESIAN_POINT('Origin',(126.1748325209,-1.05,51.0396335058013));
#193942=CARTESIAN_POINT('',(125.684019018351,-1.05,50.944228549352));
#193943=CARTESIAN_POINT('',(125.626776044481,-1.05,51.2387166508817));
#193944=CARTESIAN_POINT('',(125.684019018351,-1.05,50.944228549352));
#193945=CARTESIAN_POINT('',(126.117589547031,-1.05,51.334121607331));
#193946=CARTESIAN_POINT('',(126.1748325209,-1.05,51.0396335058013));
#193947=CARTESIAN_POINT('Origin',(125.684019018351,-1.05,50.944228549352));
#193948=CARTESIAN_POINT('',(125.626776044481,-1.05,51.2387166508817));
#193949=CARTESIAN_POINT('',(125.684019018351,-1.05,50.944228549352));
#193950=CARTESIAN_POINT('Origin',(125.684019018351,0.250000000000015,50.944228549352));
#193951=CARTESIAN_POINT('',(126.1748325209,0.250000000000015,51.0396335058013));
#193952=CARTESIAN_POINT('',(126.117589547031,0.250000000000015,51.334121607331));
#193953=CARTESIAN_POINT('',(126.1748325209,0.250000000000015,51.0396335058013));
#193954=CARTESIAN_POINT('',(125.626776044481,0.250000000000015,51.2387166508817));
#193955=CARTESIAN_POINT('',(125.626776044481,0.250000000000015,51.2387166508817));
#193956=CARTESIAN_POINT('',(125.684019018351,0.250000000000015,50.944228549352));
#193957=CARTESIAN_POINT('',(125.684019018351,0.250000000000015,50.944228549352));
#193958=CARTESIAN_POINT('',(125.684019018351,0.250000000000015,50.944228549352));
#193959=CARTESIAN_POINT('Origin',(126.1748325209,0.250000000000015,51.0396335058013));
#193960=CARTESIAN_POINT('',(126.1748325209,-0.249999999999985,51.0396335058013));
#193961=CARTESIAN_POINT('',(126.117589547031,-0.249999999999985,51.334121607331));
#193962=CARTESIAN_POINT('',(126.1748325209,-0.249999999999985,51.0396335058013));
#193963=CARTESIAN_POINT('',(126.117589547031,0.250000000000015,51.334121607331));
#193964=CARTESIAN_POINT('',(126.1748325209,0.250000000000015,51.0396335058013));
#193965=CARTESIAN_POINT('Origin',(126.1748325209,-0.249999999999985,51.0396335058013));
#193966=CARTESIAN_POINT('',(125.684019018351,-0.249999999999985,50.944228549352));
#193967=CARTESIAN_POINT('',(125.626776044481,-0.249999999999985,51.2387166508817));
#193968=CARTESIAN_POINT('',(125.684019018351,-0.249999999999985,50.944228549352));
#193969=CARTESIAN_POINT('',(126.117589547031,-0.249999999999985,51.334121607331));
#193970=CARTESIAN_POINT('',(126.1748325209,-0.249999999999985,51.0396335058013));
#193971=CARTESIAN_POINT('Origin',(125.684019018351,-0.249999999999985,50.944228549352));
#193972=CARTESIAN_POINT('',(125.626776044481,-0.249999999999985,51.2387166508817));
#193973=CARTESIAN_POINT('',(125.684019018351,-0.249999999999985,50.944228549352));
#193974=CARTESIAN_POINT('Origin',(125.684019018351,1.05,50.944228549352));
#193975=CARTESIAN_POINT('',(126.1748325209,1.05,51.0396335058013));
#193976=CARTESIAN_POINT('',(126.117589547031,1.05,51.334121607331));
#193977=CARTESIAN_POINT('',(126.1748325209,1.05,51.0396335058013));
#193978=CARTESIAN_POINT('',(125.626776044481,1.05,51.2387166508817));
#193979=CARTESIAN_POINT('',(125.626776044481,1.05,51.2387166508817));
#193980=CARTESIAN_POINT('',(125.684019018351,1.05,50.944228549352));
#193981=CARTESIAN_POINT('',(125.684019018351,1.05,50.944228549352));
#193982=CARTESIAN_POINT('',(125.684019018351,1.05,50.944228549352));
#193983=CARTESIAN_POINT('Origin',(126.1748325209,1.05,51.0396335058013));
#193984=CARTESIAN_POINT('',(126.1748325209,0.550000000000015,51.0396335058013));
#193985=CARTESIAN_POINT('',(126.117589547031,0.550000000000015,51.334121607331));
#193986=CARTESIAN_POINT('',(126.1748325209,0.550000000000015,51.0396335058013));
#193987=CARTESIAN_POINT('',(126.117589547031,1.05,51.334121607331));
#193988=CARTESIAN_POINT('',(126.1748325209,1.05,51.0396335058013));
#193989=CARTESIAN_POINT('Origin',(126.1748325209,0.550000000000015,51.0396335058013));
#193990=CARTESIAN_POINT('',(125.684019018351,0.550000000000015,50.944228549352));
#193991=CARTESIAN_POINT('',(125.626776044481,0.550000000000015,51.2387166508817));
#193992=CARTESIAN_POINT('',(125.684019018351,0.550000000000015,50.944228549352));
#193993=CARTESIAN_POINT('',(126.117589547031,0.550000000000015,51.334121607331));
#193994=CARTESIAN_POINT('',(126.1748325209,0.550000000000015,51.0396335058013));
#193995=CARTESIAN_POINT('Origin',(125.684019018351,0.550000000000015,50.944228549352));
#193996=CARTESIAN_POINT('',(125.626776044481,0.550000000000015,51.2387166508817));
#193997=CARTESIAN_POINT('',(125.684019018351,0.550000000000015,50.944228549352));
#193998=CARTESIAN_POINT('Origin',(125.684019018351,1.85,50.944228549352));
#193999=CARTESIAN_POINT('',(126.1748325209,1.85,51.0396335058013));
#194000=CARTESIAN_POINT('',(126.117589547031,1.85,51.334121607331));
#194001=CARTESIAN_POINT('',(126.1748325209,1.85,51.0396335058013));
#194002=CARTESIAN_POINT('',(125.626776044481,1.85,51.2387166508817));
#194003=CARTESIAN_POINT('',(125.626776044481,1.85,51.2387166508817));
#194004=CARTESIAN_POINT('',(125.684019018351,1.85,50.944228549352));
#194005=CARTESIAN_POINT('',(125.684019018351,1.85,50.944228549352));
#194006=CARTESIAN_POINT('',(125.684019018351,1.85,50.944228549352));
#194007=CARTESIAN_POINT('Origin',(126.1748325209,1.85,51.0396335058013));
#194008=CARTESIAN_POINT('',(126.1748325209,1.35,51.0396335058013));
#194009=CARTESIAN_POINT('',(126.117589547031,1.35,51.334121607331));
#194010=CARTESIAN_POINT('',(126.1748325209,1.35,51.0396335058013));
#194011=CARTESIAN_POINT('',(126.117589547031,1.85,51.334121607331));
#194012=CARTESIAN_POINT('',(126.1748325209,1.85,51.0396335058013));
#194013=CARTESIAN_POINT('Origin',(126.1748325209,1.35,51.0396335058013));
#194014=CARTESIAN_POINT('',(125.684019018351,1.35,50.944228549352));
#194015=CARTESIAN_POINT('',(125.626776044481,1.35,51.2387166508817));
#194016=CARTESIAN_POINT('',(125.684019018351,1.35,50.944228549352));
#194017=CARTESIAN_POINT('',(126.117589547031,1.35,51.334121607331));
#194018=CARTESIAN_POINT('',(126.1748325209,1.35,51.0396335058013));
#194019=CARTESIAN_POINT('Origin',(125.684019018351,1.35,50.944228549352));
#194020=CARTESIAN_POINT('',(125.626776044481,1.35,51.2387166508817));
#194021=CARTESIAN_POINT('',(125.684019018351,1.35,50.944228549352));
#194022=CARTESIAN_POINT('Origin',(125.684019018351,2.65,50.944228549352));
#194023=CARTESIAN_POINT('',(126.1748325209,2.65,51.0396335058013));
#194024=CARTESIAN_POINT('',(126.117589547031,2.65,51.334121607331));
#194025=CARTESIAN_POINT('',(126.1748325209,2.65,51.0396335058013));
#194026=CARTESIAN_POINT('',(125.626776044481,2.65,51.2387166508817));
#194027=CARTESIAN_POINT('',(125.626776044481,2.65,51.2387166508817));
#194028=CARTESIAN_POINT('',(125.684019018351,2.65,50.944228549352));
#194029=CARTESIAN_POINT('',(125.684019018351,2.65,50.944228549352));
#194030=CARTESIAN_POINT('',(125.684019018351,2.65,50.944228549352));
#194031=CARTESIAN_POINT('Origin',(126.1748325209,2.65,51.0396335058013));
#194032=CARTESIAN_POINT('',(126.1748325209,2.15,51.0396335058013));
#194033=CARTESIAN_POINT('',(126.117589547031,2.15,51.334121607331));
#194034=CARTESIAN_POINT('',(126.1748325209,2.15,51.0396335058013));
#194035=CARTESIAN_POINT('',(126.117589547031,2.65,51.334121607331));
#194036=CARTESIAN_POINT('',(126.1748325209,2.65,51.0396335058013));
#194037=CARTESIAN_POINT('Origin',(126.1748325209,2.15,51.0396335058013));
#194038=CARTESIAN_POINT('',(125.684019018351,2.15,50.944228549352));
#194039=CARTESIAN_POINT('',(125.626776044481,2.15,51.2387166508817));
#194040=CARTESIAN_POINT('',(125.684019018351,2.15,50.944228549352));
#194041=CARTESIAN_POINT('',(126.117589547031,2.15,51.334121607331));
#194042=CARTESIAN_POINT('',(126.1748325209,2.15,51.0396335058013));
#194043=CARTESIAN_POINT('Origin',(125.684019018351,2.15,50.944228549352));
#194044=CARTESIAN_POINT('',(125.626776044481,2.15,51.2387166508817));
#194045=CARTESIAN_POINT('',(125.684019018351,2.15,50.944228549352));
#194046=CARTESIAN_POINT('Origin',(125.684019018351,3.45,50.944228549352));
#194047=CARTESIAN_POINT('',(126.1748325209,3.45,51.0396335058013));
#194048=CARTESIAN_POINT('',(126.117589547031,3.45,51.334121607331));
#194049=CARTESIAN_POINT('',(126.1748325209,3.45,51.0396335058013));
#194050=CARTESIAN_POINT('',(125.626776044481,3.45,51.2387166508817));
#194051=CARTESIAN_POINT('',(125.626776044481,3.45,51.2387166508817));
#194052=CARTESIAN_POINT('',(125.684019018351,3.45,50.944228549352));
#194053=CARTESIAN_POINT('',(125.684019018351,3.45,50.944228549352));
#194054=CARTESIAN_POINT('',(125.684019018351,3.45,50.944228549352));
#194055=CARTESIAN_POINT('Origin',(126.1748325209,3.45,51.0396335058013));
#194056=CARTESIAN_POINT('',(126.1748325209,2.95,51.0396335058013));
#194057=CARTESIAN_POINT('',(126.117589547031,2.95,51.334121607331));
#194058=CARTESIAN_POINT('',(126.1748325209,2.95,51.0396335058013));
#194059=CARTESIAN_POINT('',(126.117589547031,3.45,51.334121607331));
#194060=CARTESIAN_POINT('',(126.1748325209,3.45,51.0396335058013));
#194061=CARTESIAN_POINT('Origin',(126.1748325209,2.95,51.0396335058013));
#194062=CARTESIAN_POINT('',(125.684019018351,2.95,50.944228549352));
#194063=CARTESIAN_POINT('',(125.626776044481,2.95,51.2387166508817));
#194064=CARTESIAN_POINT('',(125.684019018351,2.95,50.944228549352));
#194065=CARTESIAN_POINT('',(126.117589547031,2.95,51.334121607331));
#194066=CARTESIAN_POINT('',(126.1748325209,2.95,51.0396335058013));
#194067=CARTESIAN_POINT('Origin',(125.684019018351,2.95,50.944228549352));
#194068=CARTESIAN_POINT('',(125.626776044481,2.95,51.2387166508817));
#194069=CARTESIAN_POINT('',(125.684019018351,2.95,50.944228549352));
#194070=CARTESIAN_POINT('Origin',(120.186907789796,9.05,49.8756930371204));
#194071=CARTESIAN_POINT('',(120.677721292346,9.05,49.9710979935697));
#194072=CARTESIAN_POINT('',(120.620478318476,9.05,50.2655860950994));
#194073=CARTESIAN_POINT('',(120.677721292346,9.05,49.9710979935697));
#194074=CARTESIAN_POINT('',(120.129664815927,9.05,50.1701811386501));
#194075=CARTESIAN_POINT('',(120.129664815927,9.05,50.1701811386501));
#194076=CARTESIAN_POINT('',(120.186907789796,9.05,49.8756930371204));
#194077=CARTESIAN_POINT('',(120.186907789796,9.05,49.8756930371204));
#194078=CARTESIAN_POINT('',(120.186907789796,9.05,49.8756930371204));
#194079=CARTESIAN_POINT('Origin',(120.677721292346,9.05,49.9710979935697));
#194080=CARTESIAN_POINT('',(120.677721292346,8.55,49.9710979935697));
#194081=CARTESIAN_POINT('',(120.620478318476,8.55,50.2655860950994));
#194082=CARTESIAN_POINT('',(120.677721292346,8.55,49.9710979935697));
#194083=CARTESIAN_POINT('',(120.620478318476,9.05,50.2655860950994));
#194084=CARTESIAN_POINT('',(120.677721292346,9.05,49.9710979935697));
#194085=CARTESIAN_POINT('Origin',(120.677721292346,8.55,49.9710979935697));
#194086=CARTESIAN_POINT('',(120.186907789796,8.55,49.8756930371204));
#194087=CARTESIAN_POINT('',(120.129664815927,8.55,50.1701811386501));
#194088=CARTESIAN_POINT('',(120.186907789796,8.55,49.8756930371204));
#194089=CARTESIAN_POINT('',(120.620478318476,8.55,50.2655860950994));
#194090=CARTESIAN_POINT('',(120.677721292346,8.55,49.9710979935697));
#194091=CARTESIAN_POINT('Origin',(120.186907789796,8.55,49.8756930371204));
#194092=CARTESIAN_POINT('',(120.129664815927,8.55,50.1701811386501));
#194093=CARTESIAN_POINT('',(120.186907789796,8.55,49.8756930371204));
#194094=CARTESIAN_POINT('Origin',(119.401606185717,9.05,49.7230451068016));
#194095=CARTESIAN_POINT('',(119.892419688267,9.05,49.8184500632509));
#194096=CARTESIAN_POINT('',(119.835176714397,9.05,50.1129381647806));
#194097=CARTESIAN_POINT('',(119.892419688267,9.05,49.8184500632509));
#194098=CARTESIAN_POINT('',(119.344363211847,9.05,50.0175332083313));
#194099=CARTESIAN_POINT('',(119.344363211847,9.05,50.0175332083313));
#194100=CARTESIAN_POINT('',(119.401606185717,9.05,49.7230451068016));
#194101=CARTESIAN_POINT('',(119.401606185717,9.05,49.7230451068016));
#194102=CARTESIAN_POINT('',(119.401606185717,9.05,49.7230451068016));
#194103=CARTESIAN_POINT('Origin',(119.892419688267,9.05,49.8184500632509));
#194104=CARTESIAN_POINT('',(119.892419688267,8.55,49.8184500632509));
#194105=CARTESIAN_POINT('',(119.835176714397,8.55,50.1129381647806));
#194106=CARTESIAN_POINT('',(119.892419688267,8.55,49.8184500632509));
#194107=CARTESIAN_POINT('',(119.835176714397,9.05,50.1129381647806));
#194108=CARTESIAN_POINT('',(119.892419688267,9.05,49.8184500632509));
#194109=CARTESIAN_POINT('Origin',(119.892419688267,8.55,49.8184500632509));
#194110=CARTESIAN_POINT('',(119.401606185717,8.55,49.7230451068016));
#194111=CARTESIAN_POINT('',(119.344363211847,8.55,50.0175332083313));
#194112=CARTESIAN_POINT('',(119.401606185717,8.55,49.7230451068016));
#194113=CARTESIAN_POINT('',(119.835176714397,8.55,50.1129381647806));
#194114=CARTESIAN_POINT('',(119.892419688267,8.55,49.8184500632509));
#194115=CARTESIAN_POINT('Origin',(119.401606185717,8.55,49.7230451068016));
#194116=CARTESIAN_POINT('',(119.344363211847,8.55,50.0175332083313));
#194117=CARTESIAN_POINT('',(119.401606185717,8.55,49.7230451068016));
#194118=CARTESIAN_POINT('Origin',(118.616304581638,9.05,49.5703971764828));
#194119=CARTESIAN_POINT('',(119.107118084187,9.05,49.6658021329321));
#194120=CARTESIAN_POINT('',(119.049875110318,9.05,49.9602902344618));
#194121=CARTESIAN_POINT('',(119.107118084187,9.05,49.6658021329321));
#194122=CARTESIAN_POINT('',(118.559061607768,9.05,49.8648852780125));
#194123=CARTESIAN_POINT('',(118.559061607768,9.05,49.8648852780125));
#194124=CARTESIAN_POINT('',(118.616304581638,9.05,49.5703971764828));
#194125=CARTESIAN_POINT('',(118.616304581638,9.05,49.5703971764828));
#194126=CARTESIAN_POINT('',(118.616304581638,9.05,49.5703971764828));
#194127=CARTESIAN_POINT('Origin',(119.107118084187,9.05,49.6658021329321));
#194128=CARTESIAN_POINT('',(119.107118084187,8.55,49.6658021329321));
#194129=CARTESIAN_POINT('',(119.049875110318,8.55,49.9602902344618));
#194130=CARTESIAN_POINT('',(119.107118084187,8.55,49.6658021329321));
#194131=CARTESIAN_POINT('',(119.049875110318,9.05,49.9602902344618));
#194132=CARTESIAN_POINT('',(119.107118084187,9.05,49.6658021329321));
#194133=CARTESIAN_POINT('Origin',(119.107118084187,8.55,49.6658021329321));
#194134=CARTESIAN_POINT('',(118.616304581638,8.55,49.5703971764828));
#194135=CARTESIAN_POINT('',(118.559061607768,8.55,49.8648852780125));
#194136=CARTESIAN_POINT('',(118.616304581638,8.55,49.5703971764828));
#194137=CARTESIAN_POINT('',(119.049875110318,8.55,49.9602902344618));
#194138=CARTESIAN_POINT('',(119.107118084187,8.55,49.6658021329321));
#194139=CARTESIAN_POINT('Origin',(118.616304581638,8.55,49.5703971764828));
#194140=CARTESIAN_POINT('',(118.559061607768,8.55,49.8648852780125));
#194141=CARTESIAN_POINT('',(118.616304581638,8.55,49.5703971764828));
#194142=CARTESIAN_POINT('Origin',(117.831002977559,9.05,49.417749246164));
#194143=CARTESIAN_POINT('',(118.321816480108,9.05,49.5131542026133));
#194144=CARTESIAN_POINT('',(118.264573506239,9.05,49.807642304143));
#194145=CARTESIAN_POINT('',(118.321816480108,9.05,49.5131542026133));
#194146=CARTESIAN_POINT('',(117.773760003689,9.05,49.7122373476937));
#194147=CARTESIAN_POINT('',(117.773760003689,9.05,49.7122373476937));
#194148=CARTESIAN_POINT('',(117.831002977559,9.05,49.417749246164));
#194149=CARTESIAN_POINT('',(117.831002977559,9.05,49.417749246164));
#194150=CARTESIAN_POINT('',(117.831002977559,9.05,49.417749246164));
#194151=CARTESIAN_POINT('Origin',(118.321816480108,9.05,49.5131542026133));
#194152=CARTESIAN_POINT('',(118.321816480108,8.55,49.5131542026133));
#194153=CARTESIAN_POINT('',(118.264573506239,8.55,49.807642304143));
#194154=CARTESIAN_POINT('',(118.321816480108,8.55,49.5131542026133));
#194155=CARTESIAN_POINT('',(118.264573506239,9.05,49.807642304143));
#194156=CARTESIAN_POINT('',(118.321816480108,9.05,49.5131542026133));
#194157=CARTESIAN_POINT('Origin',(118.321816480108,8.55,49.5131542026133));
#194158=CARTESIAN_POINT('',(117.831002977559,8.55,49.417749246164));
#194159=CARTESIAN_POINT('',(117.773760003689,8.55,49.7122373476937));
#194160=CARTESIAN_POINT('',(117.831002977559,8.55,49.417749246164));
#194161=CARTESIAN_POINT('',(118.264573506239,8.55,49.807642304143));
#194162=CARTESIAN_POINT('',(118.321816480108,8.55,49.5131542026133));
#194163=CARTESIAN_POINT('Origin',(117.831002977559,8.55,49.417749246164));
#194164=CARTESIAN_POINT('',(117.773760003689,8.55,49.7122373476937));
#194165=CARTESIAN_POINT('',(117.831002977559,8.55,49.417749246164));
#194166=CARTESIAN_POINT('Origin',(117.045701373479,9.05,49.2651013158452));
#194167=CARTESIAN_POINT('',(117.536514876029,9.05,49.3605062722945));
#194168=CARTESIAN_POINT('',(117.479271902159,9.05,49.6549943738242));
#194169=CARTESIAN_POINT('',(117.536514876029,9.05,49.3605062722945));
#194170=CARTESIAN_POINT('',(116.98845839961,9.05,49.5595894173749));
#194171=CARTESIAN_POINT('',(116.98845839961,9.05,49.5595894173749));
#194172=CARTESIAN_POINT('',(117.045701373479,9.05,49.2651013158452));
#194173=CARTESIAN_POINT('',(117.045701373479,9.05,49.2651013158452));
#194174=CARTESIAN_POINT('',(117.045701373479,9.05,49.2651013158452));
#194175=CARTESIAN_POINT('Origin',(117.536514876029,9.05,49.3605062722945));
#194176=CARTESIAN_POINT('',(117.536514876029,8.55,49.3605062722945));
#194177=CARTESIAN_POINT('',(117.479271902159,8.55,49.6549943738242));
#194178=CARTESIAN_POINT('',(117.536514876029,8.55,49.3605062722945));
#194179=CARTESIAN_POINT('',(117.479271902159,9.05,49.6549943738242));
#194180=CARTESIAN_POINT('',(117.536514876029,9.05,49.3605062722945));
#194181=CARTESIAN_POINT('Origin',(117.536514876029,8.55,49.3605062722945));
#194182=CARTESIAN_POINT('',(117.045701373479,8.55,49.2651013158452));
#194183=CARTESIAN_POINT('',(116.98845839961,8.55,49.5595894173749));
#194184=CARTESIAN_POINT('',(117.045701373479,8.55,49.2651013158452));
#194185=CARTESIAN_POINT('',(117.479271902159,8.55,49.6549943738242));
#194186=CARTESIAN_POINT('',(117.536514876029,8.55,49.3605062722945));
#194187=CARTESIAN_POINT('Origin',(117.045701373479,8.55,49.2651013158452));
#194188=CARTESIAN_POINT('',(116.98845839961,8.55,49.5595894173749));
#194189=CARTESIAN_POINT('',(117.045701373479,8.55,49.2651013158452));
#194190=CARTESIAN_POINT('Origin',(116.2603997694,9.05,49.1124533855264));
#194191=CARTESIAN_POINT('',(116.75121327195,9.05,49.2078583419757));
#194192=CARTESIAN_POINT('',(116.69397029808,9.05,49.5023464435054));
#194193=CARTESIAN_POINT('',(116.75121327195,9.05,49.2078583419757));
#194194=CARTESIAN_POINT('',(116.203156795531,9.05,49.4069414870561));
#194195=CARTESIAN_POINT('',(116.203156795531,9.05,49.4069414870561));
#194196=CARTESIAN_POINT('',(116.2603997694,9.05,49.1124533855264));
#194197=CARTESIAN_POINT('',(116.2603997694,9.05,49.1124533855264));
#194198=CARTESIAN_POINT('',(116.2603997694,9.05,49.1124533855264));
#194199=CARTESIAN_POINT('Origin',(116.75121327195,9.05,49.2078583419757));
#194200=CARTESIAN_POINT('',(116.75121327195,8.55,49.2078583419757));
#194201=CARTESIAN_POINT('',(116.69397029808,8.55,49.5023464435054));
#194202=CARTESIAN_POINT('',(116.75121327195,8.55,49.2078583419757));
#194203=CARTESIAN_POINT('',(116.69397029808,9.05,49.5023464435054));
#194204=CARTESIAN_POINT('',(116.75121327195,9.05,49.2078583419757));
#194205=CARTESIAN_POINT('Origin',(116.75121327195,8.55,49.2078583419757));
#194206=CARTESIAN_POINT('',(116.2603997694,8.55,49.1124533855264));
#194207=CARTESIAN_POINT('',(116.203156795531,8.55,49.4069414870561));
#194208=CARTESIAN_POINT('',(116.2603997694,8.55,49.1124533855264));
#194209=CARTESIAN_POINT('',(116.69397029808,8.55,49.5023464435054));
#194210=CARTESIAN_POINT('',(116.75121327195,8.55,49.2078583419757));
#194211=CARTESIAN_POINT('Origin',(116.2603997694,8.55,49.1124533855264));
#194212=CARTESIAN_POINT('',(116.203156795531,8.55,49.4069414870561));
#194213=CARTESIAN_POINT('',(116.2603997694,8.55,49.1124533855264));
#194214=CARTESIAN_POINT('Origin',(115.475098165321,9.05,48.9598054552076));
#194215=CARTESIAN_POINT('',(115.96591166787,9.05,49.0552104116569));
#194216=CARTESIAN_POINT('',(115.908668694001,9.05,49.3496985131866));
#194217=CARTESIAN_POINT('',(115.96591166787,9.05,49.0552104116569));
#194218=CARTESIAN_POINT('',(115.417855191451,9.05,49.2542935567373));
#194219=CARTESIAN_POINT('',(115.417855191451,9.05,49.2542935567373));
#194220=CARTESIAN_POINT('',(115.475098165321,9.05,48.9598054552076));
#194221=CARTESIAN_POINT('',(115.475098165321,9.05,48.9598054552076));
#194222=CARTESIAN_POINT('',(115.475098165321,9.05,48.9598054552076));
#194223=CARTESIAN_POINT('Origin',(115.96591166787,9.05,49.0552104116569));
#194224=CARTESIAN_POINT('',(115.96591166787,8.55,49.0552104116569));
#194225=CARTESIAN_POINT('',(115.908668694001,8.55,49.3496985131866));
#194226=CARTESIAN_POINT('',(115.96591166787,8.55,49.0552104116569));
#194227=CARTESIAN_POINT('',(115.908668694001,9.05,49.3496985131866));
#194228=CARTESIAN_POINT('',(115.96591166787,9.05,49.0552104116569));
#194229=CARTESIAN_POINT('Origin',(115.96591166787,8.55,49.0552104116569));
#194230=CARTESIAN_POINT('',(115.475098165321,8.55,48.9598054552076));
#194231=CARTESIAN_POINT('',(115.417855191451,8.55,49.2542935567373));
#194232=CARTESIAN_POINT('',(115.475098165321,8.55,48.9598054552076));
#194233=CARTESIAN_POINT('',(115.908668694001,8.55,49.3496985131866));
#194234=CARTESIAN_POINT('',(115.96591166787,8.55,49.0552104116569));
#194235=CARTESIAN_POINT('Origin',(115.475098165321,8.55,48.9598054552076));
#194236=CARTESIAN_POINT('',(115.417855191451,8.55,49.2542935567373));
#194237=CARTESIAN_POINT('',(115.475098165321,8.55,48.9598054552076));
#194238=CARTESIAN_POINT('Origin',(114.689796561242,9.05,48.8071575248888));
#194239=CARTESIAN_POINT('',(115.180610063791,9.05,48.9025624813381));
#194240=CARTESIAN_POINT('',(115.123367089922,9.05,49.1970505828678));
#194241=CARTESIAN_POINT('',(115.180610063791,9.05,48.9025624813381));
#194242=CARTESIAN_POINT('',(114.632553587372,9.05,49.1016456264185));
#194243=CARTESIAN_POINT('',(114.632553587372,9.05,49.1016456264185));
#194244=CARTESIAN_POINT('',(114.689796561242,9.05,48.8071575248888));
#194245=CARTESIAN_POINT('',(114.689796561242,9.05,48.8071575248888));
#194246=CARTESIAN_POINT('',(114.689796561242,9.05,48.8071575248888));
#194247=CARTESIAN_POINT('Origin',(115.180610063791,9.05,48.9025624813381));
#194248=CARTESIAN_POINT('',(115.180610063791,8.55,48.9025624813381));
#194249=CARTESIAN_POINT('',(115.123367089922,8.55,49.1970505828678));
#194250=CARTESIAN_POINT('',(115.180610063791,8.55,48.9025624813381));
#194251=CARTESIAN_POINT('',(115.123367089922,9.05,49.1970505828678));
#194252=CARTESIAN_POINT('',(115.180610063791,9.05,48.9025624813381));
#194253=CARTESIAN_POINT('Origin',(115.180610063791,8.55,48.9025624813381));
#194254=CARTESIAN_POINT('',(114.689796561242,8.55,48.8071575248888));
#194255=CARTESIAN_POINT('',(114.632553587372,8.55,49.1016456264185));
#194256=CARTESIAN_POINT('',(114.689796561242,8.55,48.8071575248888));
#194257=CARTESIAN_POINT('',(115.123367089922,8.55,49.1970505828678));
#194258=CARTESIAN_POINT('',(115.180610063791,8.55,48.9025624813381));
#194259=CARTESIAN_POINT('Origin',(114.689796561242,8.55,48.8071575248888));
#194260=CARTESIAN_POINT('',(114.632553587372,8.55,49.1016456264185));
#194261=CARTESIAN_POINT('',(114.689796561242,8.55,48.8071575248888));
#194262=CARTESIAN_POINT('Origin',(113.904494957163,9.05,48.65450959457));
#194263=CARTESIAN_POINT('',(114.395308459712,9.05,48.7499145510193));
#194264=CARTESIAN_POINT('',(114.338065485842,9.05,49.044402652549));
#194265=CARTESIAN_POINT('',(114.395308459712,9.05,48.7499145510193));
#194266=CARTESIAN_POINT('',(113.847251983293,9.05,48.9489976960997));
#194267=CARTESIAN_POINT('',(113.847251983293,9.05,48.9489976960997));
#194268=CARTESIAN_POINT('',(113.904494957163,9.05,48.65450959457));
#194269=CARTESIAN_POINT('',(113.904494957163,9.05,48.65450959457));
#194270=CARTESIAN_POINT('',(113.904494957163,9.05,48.65450959457));
#194271=CARTESIAN_POINT('Origin',(114.395308459712,9.05,48.7499145510193));
#194272=CARTESIAN_POINT('',(114.395308459712,8.55,48.7499145510193));
#194273=CARTESIAN_POINT('',(114.338065485842,8.55,49.044402652549));
#194274=CARTESIAN_POINT('',(114.395308459712,8.55,48.7499145510193));
#194275=CARTESIAN_POINT('',(114.338065485842,9.05,49.044402652549));
#194276=CARTESIAN_POINT('',(114.395308459712,9.05,48.7499145510193));
#194277=CARTESIAN_POINT('Origin',(114.395308459712,8.55,48.7499145510193));
#194278=CARTESIAN_POINT('',(113.904494957163,8.55,48.65450959457));
#194279=CARTESIAN_POINT('',(113.847251983293,8.55,48.9489976960997));
#194280=CARTESIAN_POINT('',(113.904494957163,8.55,48.65450959457));
#194281=CARTESIAN_POINT('',(114.338065485842,8.55,49.044402652549));
#194282=CARTESIAN_POINT('',(114.395308459712,8.55,48.7499145510193));
#194283=CARTESIAN_POINT('Origin',(113.904494957163,8.55,48.65450959457));
#194284=CARTESIAN_POINT('',(113.847251983293,8.55,48.9489976960997));
#194285=CARTESIAN_POINT('',(113.904494957163,8.55,48.65450959457));
#194286=CARTESIAN_POINT('Origin',(109.192685332687,5.05,47.7386220126572));
#194287=CARTESIAN_POINT('',(109.683498835237,5.05,47.8340269691064));
#194288=CARTESIAN_POINT('',(109.626255861367,5.05,48.1285150706361));
#194289=CARTESIAN_POINT('',(109.683498835237,5.05,47.8340269691064));
#194290=CARTESIAN_POINT('',(109.135442358818,5.05,48.0331101141869));
#194291=CARTESIAN_POINT('',(109.135442358818,5.05,48.0331101141869));
#194292=CARTESIAN_POINT('',(109.192685332687,5.05,47.7386220126572));
#194293=CARTESIAN_POINT('',(109.192685332687,5.05,47.7386220126572));
#194294=CARTESIAN_POINT('',(109.192685332687,5.05,47.7386220126572));
#194295=CARTESIAN_POINT('Origin',(109.683498835237,5.05,47.8340269691064));
#194296=CARTESIAN_POINT('',(109.683498835237,4.55,47.8340269691064));
#194297=CARTESIAN_POINT('',(109.626255861367,4.55,48.1285150706361));
#194298=CARTESIAN_POINT('',(109.683498835237,4.55,47.8340269691064));
#194299=CARTESIAN_POINT('',(109.626255861367,5.05,48.1285150706361));
#194300=CARTESIAN_POINT('',(109.683498835237,5.05,47.8340269691064));
#194301=CARTESIAN_POINT('Origin',(109.683498835237,4.55,47.8340269691064));
#194302=CARTESIAN_POINT('',(109.192685332687,4.55,47.7386220126572));
#194303=CARTESIAN_POINT('',(109.135442358818,4.55,48.0331101141869));
#194304=CARTESIAN_POINT('',(109.192685332687,4.55,47.7386220126572));
#194305=CARTESIAN_POINT('',(109.626255861367,4.55,48.1285150706361));
#194306=CARTESIAN_POINT('',(109.683498835237,4.55,47.8340269691064));
#194307=CARTESIAN_POINT('Origin',(109.192685332687,4.55,47.7386220126572));
#194308=CARTESIAN_POINT('',(109.135442358818,4.55,48.0331101141869));
#194309=CARTESIAN_POINT('',(109.192685332687,4.55,47.7386220126572));
#194310=CARTESIAN_POINT('Origin',(109.192685332687,4.25,47.7386220126572));
#194311=CARTESIAN_POINT('',(109.683498835237,4.25,47.8340269691064));
#194312=CARTESIAN_POINT('',(109.626255861367,4.25,48.1285150706361));
#194313=CARTESIAN_POINT('',(109.683498835237,4.25,47.8340269691064));
#194314=CARTESIAN_POINT('',(109.135442358818,4.25,48.0331101141869));
#194315=CARTESIAN_POINT('',(109.135442358818,4.25,48.0331101141869));
#194316=CARTESIAN_POINT('',(109.192685332687,4.25,47.7386220126572));
#194317=CARTESIAN_POINT('',(109.192685332687,4.25,47.7386220126572));
#194318=CARTESIAN_POINT('',(109.192685332687,4.25,47.7386220126572));
#194319=CARTESIAN_POINT('Origin',(109.683498835237,4.25,47.8340269691064));
#194320=CARTESIAN_POINT('',(109.683498835237,3.75,47.8340269691064));
#194321=CARTESIAN_POINT('',(109.626255861367,3.75,48.1285150706361));
#194322=CARTESIAN_POINT('',(109.683498835237,3.75,47.8340269691064));
#194323=CARTESIAN_POINT('',(109.626255861367,4.25,48.1285150706361));
#194324=CARTESIAN_POINT('',(109.683498835237,4.25,47.8340269691064));
#194325=CARTESIAN_POINT('Origin',(109.683498835237,3.75,47.8340269691064));
#194326=CARTESIAN_POINT('',(109.192685332687,3.75,47.7386220126572));
#194327=CARTESIAN_POINT('',(109.135442358818,3.75,48.0331101141869));
#194328=CARTESIAN_POINT('',(109.192685332687,3.75,47.7386220126572));
#194329=CARTESIAN_POINT('',(109.626255861367,3.75,48.1285150706361));
#194330=CARTESIAN_POINT('',(109.683498835237,3.75,47.8340269691064));
#194331=CARTESIAN_POINT('Origin',(109.192685332687,3.75,47.7386220126572));
#194332=CARTESIAN_POINT('',(109.135442358818,3.75,48.0331101141869));
#194333=CARTESIAN_POINT('',(109.192685332687,3.75,47.7386220126572));
#194334=CARTESIAN_POINT('Origin',(109.192685332687,3.45,47.7386220126572));
#194335=CARTESIAN_POINT('',(109.683498835237,3.45,47.8340269691064));
#194336=CARTESIAN_POINT('',(109.626255861367,3.45,48.1285150706361));
#194337=CARTESIAN_POINT('',(109.683498835237,3.45,47.8340269691064));
#194338=CARTESIAN_POINT('',(109.135442358818,3.45,48.0331101141869));
#194339=CARTESIAN_POINT('',(109.135442358818,3.45,48.0331101141869));
#194340=CARTESIAN_POINT('',(109.192685332687,3.45,47.7386220126572));
#194341=CARTESIAN_POINT('',(109.192685332687,3.45,47.7386220126572));
#194342=CARTESIAN_POINT('',(109.192685332687,3.45,47.7386220126572));
#194343=CARTESIAN_POINT('Origin',(109.683498835237,3.45,47.8340269691064));
#194344=CARTESIAN_POINT('',(109.683498835237,2.95,47.8340269691064));
#194345=CARTESIAN_POINT('',(109.626255861367,2.95,48.1285150706361));
#194346=CARTESIAN_POINT('',(109.683498835237,2.95,47.8340269691064));
#194347=CARTESIAN_POINT('',(109.626255861367,3.45,48.1285150706361));
#194348=CARTESIAN_POINT('',(109.683498835237,3.45,47.8340269691064));
#194349=CARTESIAN_POINT('Origin',(109.683498835237,2.95,47.8340269691064));
#194350=CARTESIAN_POINT('',(109.192685332687,2.95,47.7386220126572));
#194351=CARTESIAN_POINT('',(109.135442358818,2.95,48.0331101141869));
#194352=CARTESIAN_POINT('',(109.192685332687,2.95,47.7386220126572));
#194353=CARTESIAN_POINT('',(109.626255861367,2.95,48.1285150706361));
#194354=CARTESIAN_POINT('',(109.683498835237,2.95,47.8340269691064));
#194355=CARTESIAN_POINT('Origin',(109.192685332687,2.95,47.7386220126572));
#194356=CARTESIAN_POINT('',(109.135442358818,2.95,48.0331101141869));
#194357=CARTESIAN_POINT('',(109.192685332687,2.95,47.7386220126572));
#194358=CARTESIAN_POINT('Origin',(109.192685332687,2.65,47.7386220126572));
#194359=CARTESIAN_POINT('',(109.683498835237,2.65,47.8340269691064));
#194360=CARTESIAN_POINT('',(109.626255861367,2.65,48.1285150706361));
#194361=CARTESIAN_POINT('',(109.683498835237,2.65,47.8340269691064));
#194362=CARTESIAN_POINT('',(109.135442358818,2.65,48.0331101141869));
#194363=CARTESIAN_POINT('',(109.135442358818,2.65,48.0331101141869));
#194364=CARTESIAN_POINT('',(109.192685332687,2.65,47.7386220126572));
#194365=CARTESIAN_POINT('',(109.192685332687,2.65,47.7386220126572));
#194366=CARTESIAN_POINT('',(109.192685332687,2.65,47.7386220126572));
#194367=CARTESIAN_POINT('Origin',(109.683498835237,2.65,47.8340269691064));
#194368=CARTESIAN_POINT('',(109.683498835237,2.15,47.8340269691064));
#194369=CARTESIAN_POINT('',(109.626255861367,2.15,48.1285150706361));
#194370=CARTESIAN_POINT('',(109.683498835237,2.15,47.8340269691064));
#194371=CARTESIAN_POINT('',(109.626255861367,2.65,48.1285150706361));
#194372=CARTESIAN_POINT('',(109.683498835237,2.65,47.8340269691064));
#194373=CARTESIAN_POINT('Origin',(109.683498835237,2.15,47.8340269691064));
#194374=CARTESIAN_POINT('',(109.192685332687,2.15,47.7386220126572));
#194375=CARTESIAN_POINT('',(109.135442358818,2.15,48.0331101141869));
#194376=CARTESIAN_POINT('',(109.192685332687,2.15,47.7386220126572));
#194377=CARTESIAN_POINT('',(109.626255861367,2.15,48.1285150706361));
#194378=CARTESIAN_POINT('',(109.683498835237,2.15,47.8340269691064));
#194379=CARTESIAN_POINT('Origin',(109.192685332687,2.15,47.7386220126572));
#194380=CARTESIAN_POINT('',(109.135442358818,2.15,48.0331101141869));
#194381=CARTESIAN_POINT('',(109.192685332687,2.15,47.7386220126572));
#194382=CARTESIAN_POINT('Origin',(109.192685332687,1.85,47.7386220126572));
#194383=CARTESIAN_POINT('',(109.683498835237,1.85,47.8340269691064));
#194384=CARTESIAN_POINT('',(109.626255861367,1.85,48.1285150706361));
#194385=CARTESIAN_POINT('',(109.683498835237,1.85,47.8340269691064));
#194386=CARTESIAN_POINT('',(109.135442358818,1.85,48.0331101141869));
#194387=CARTESIAN_POINT('',(109.135442358818,1.85,48.0331101141869));
#194388=CARTESIAN_POINT('',(109.192685332687,1.85,47.7386220126572));
#194389=CARTESIAN_POINT('',(109.192685332687,1.85,47.7386220126572));
#194390=CARTESIAN_POINT('',(109.192685332687,1.85,47.7386220126572));
#194391=CARTESIAN_POINT('Origin',(109.683498835237,1.85,47.8340269691064));
#194392=CARTESIAN_POINT('',(109.683498835237,1.35,47.8340269691064));
#194393=CARTESIAN_POINT('',(109.626255861367,1.35,48.1285150706361));
#194394=CARTESIAN_POINT('',(109.683498835237,1.35,47.8340269691064));
#194395=CARTESIAN_POINT('',(109.626255861367,1.85,48.1285150706361));
#194396=CARTESIAN_POINT('',(109.683498835237,1.85,47.8340269691064));
#194397=CARTESIAN_POINT('Origin',(109.683498835237,1.35,47.8340269691064));
#194398=CARTESIAN_POINT('',(109.192685332687,1.35,47.7386220126572));
#194399=CARTESIAN_POINT('',(109.135442358818,1.35,48.0331101141869));
#194400=CARTESIAN_POINT('',(109.192685332687,1.35,47.7386220126572));
#194401=CARTESIAN_POINT('',(109.626255861367,1.35,48.1285150706361));
#194402=CARTESIAN_POINT('',(109.683498835237,1.35,47.8340269691064));
#194403=CARTESIAN_POINT('Origin',(109.192685332687,1.35,47.7386220126572));
#194404=CARTESIAN_POINT('',(109.135442358818,1.35,48.0331101141869));
#194405=CARTESIAN_POINT('',(109.192685332687,1.35,47.7386220126572));
#194406=CARTESIAN_POINT('Origin',(109.192685332687,1.05,47.7386220126572));
#194407=CARTESIAN_POINT('',(109.683498835237,1.05,47.8340269691064));
#194408=CARTESIAN_POINT('',(109.626255861367,1.05,48.1285150706361));
#194409=CARTESIAN_POINT('',(109.683498835237,1.05,47.8340269691064));
#194410=CARTESIAN_POINT('',(109.135442358818,1.05,48.0331101141869));
#194411=CARTESIAN_POINT('',(109.135442358818,1.05,48.0331101141869));
#194412=CARTESIAN_POINT('',(109.192685332687,1.05,47.7386220126572));
#194413=CARTESIAN_POINT('',(109.192685332687,1.05,47.7386220126572));
#194414=CARTESIAN_POINT('',(109.192685332687,1.05,47.7386220126572));
#194415=CARTESIAN_POINT('Origin',(109.683498835237,1.05,47.8340269691064));
#194416=CARTESIAN_POINT('',(109.683498835237,0.550000000000015,47.8340269691064));
#194417=CARTESIAN_POINT('',(109.626255861367,0.550000000000015,48.1285150706361));
#194418=CARTESIAN_POINT('',(109.683498835237,0.550000000000015,47.8340269691064));
#194419=CARTESIAN_POINT('',(109.626255861367,1.05,48.1285150706361));
#194420=CARTESIAN_POINT('',(109.683498835237,1.05,47.8340269691064));
#194421=CARTESIAN_POINT('Origin',(109.683498835237,0.550000000000015,47.8340269691064));
#194422=CARTESIAN_POINT('',(109.192685332687,0.550000000000015,47.7386220126572));
#194423=CARTESIAN_POINT('',(109.135442358818,0.550000000000015,48.0331101141869));
#194424=CARTESIAN_POINT('',(109.192685332687,0.550000000000015,47.7386220126572));
#194425=CARTESIAN_POINT('',(109.626255861367,0.550000000000015,48.1285150706361));
#194426=CARTESIAN_POINT('',(109.683498835237,0.550000000000015,47.8340269691064));
#194427=CARTESIAN_POINT('Origin',(109.192685332687,0.550000000000015,47.7386220126572));
#194428=CARTESIAN_POINT('',(109.135442358818,0.550000000000015,48.0331101141869));
#194429=CARTESIAN_POINT('',(109.192685332687,0.550000000000015,47.7386220126572));
#194430=CARTESIAN_POINT('Origin',(109.192685332687,0.250000000000015,47.7386220126572));
#194431=CARTESIAN_POINT('',(109.683498835237,0.250000000000015,47.8340269691064));
#194432=CARTESIAN_POINT('',(109.626255861367,0.250000000000015,48.1285150706361));
#194433=CARTESIAN_POINT('',(109.683498835237,0.250000000000015,47.8340269691064));
#194434=CARTESIAN_POINT('',(109.135442358818,0.250000000000015,48.0331101141869));
#194435=CARTESIAN_POINT('',(109.135442358818,0.250000000000015,48.0331101141869));
#194436=CARTESIAN_POINT('',(109.192685332687,0.250000000000015,47.7386220126572));
#194437=CARTESIAN_POINT('',(109.192685332687,0.250000000000015,47.7386220126572));
#194438=CARTESIAN_POINT('',(109.192685332687,0.250000000000015,47.7386220126572));
#194439=CARTESIAN_POINT('Origin',(109.683498835237,0.250000000000015,47.8340269691064));
#194440=CARTESIAN_POINT('',(109.683498835237,-0.249999999999985,47.8340269691064));
#194441=CARTESIAN_POINT('',(109.626255861367,-0.249999999999985,48.1285150706361));
#194442=CARTESIAN_POINT('',(109.683498835237,-0.249999999999985,47.8340269691064));
#194443=CARTESIAN_POINT('',(109.626255861367,0.250000000000015,48.1285150706361));
#194444=CARTESIAN_POINT('',(109.683498835237,0.250000000000015,47.8340269691064));
#194445=CARTESIAN_POINT('Origin',(109.683498835237,-0.249999999999985,47.8340269691064));
#194446=CARTESIAN_POINT('',(109.192685332687,-0.249999999999985,47.7386220126572));
#194447=CARTESIAN_POINT('',(109.135442358818,-0.249999999999985,48.0331101141869));
#194448=CARTESIAN_POINT('',(109.192685332687,-0.249999999999985,47.7386220126572));
#194449=CARTESIAN_POINT('',(109.626255861367,-0.249999999999985,48.1285150706361));
#194450=CARTESIAN_POINT('',(109.683498835237,-0.249999999999985,47.8340269691064));
#194451=CARTESIAN_POINT('Origin',(109.192685332687,-0.249999999999985,47.7386220126572));
#194452=CARTESIAN_POINT('',(109.135442358818,-0.249999999999985,48.0331101141869));
#194453=CARTESIAN_POINT('',(109.192685332687,-0.249999999999985,47.7386220126572));
#194454=CARTESIAN_POINT('Origin',(109.192685332687,-0.549999999999986,47.7386220126572));
#194455=CARTESIAN_POINT('',(109.683498835237,-0.549999999999986,47.8340269691064));
#194456=CARTESIAN_POINT('',(109.626255861367,-0.549999999999986,48.1285150706361));
#194457=CARTESIAN_POINT('',(109.683498835237,-0.549999999999986,47.8340269691064));
#194458=CARTESIAN_POINT('',(109.135442358818,-0.549999999999986,48.0331101141869));
#194459=CARTESIAN_POINT('',(109.135442358818,-0.549999999999986,48.0331101141869));
#194460=CARTESIAN_POINT('',(109.192685332687,-0.549999999999986,47.7386220126572));
#194461=CARTESIAN_POINT('',(109.192685332687,-0.549999999999986,47.7386220126572));
#194462=CARTESIAN_POINT('',(109.192685332687,-0.549999999999986,47.7386220126572));
#194463=CARTESIAN_POINT('Origin',(109.683498835237,-0.549999999999986,47.8340269691064));
#194464=CARTESIAN_POINT('',(109.683498835237,-1.05,47.8340269691064));
#194465=CARTESIAN_POINT('',(109.626255861367,-1.05,48.1285150706361));
#194466=CARTESIAN_POINT('',(109.683498835237,-1.05,47.8340269691064));
#194467=CARTESIAN_POINT('',(109.626255861367,-0.549999999999986,48.1285150706361));
#194468=CARTESIAN_POINT('',(109.683498835237,-0.549999999999986,47.8340269691064));
#194469=CARTESIAN_POINT('Origin',(109.683498835237,-1.05,47.8340269691064));
#194470=CARTESIAN_POINT('',(109.192685332687,-1.05,47.7386220126572));
#194471=CARTESIAN_POINT('',(109.135442358818,-1.05,48.0331101141869));
#194472=CARTESIAN_POINT('',(109.192685332687,-1.05,47.7386220126572));
#194473=CARTESIAN_POINT('',(109.626255861367,-1.05,48.1285150706361));
#194474=CARTESIAN_POINT('',(109.683498835237,-1.05,47.8340269691064));
#194475=CARTESIAN_POINT('Origin',(109.192685332687,-1.05,47.7386220126572));
#194476=CARTESIAN_POINT('',(109.135442358818,-1.05,48.0331101141869));
#194477=CARTESIAN_POINT('',(109.192685332687,-1.05,47.7386220126572));
#194478=CARTESIAN_POINT('Origin',(109.192685332687,-1.35,47.7386220126572));
#194479=CARTESIAN_POINT('',(109.683498835237,-1.35,47.8340269691064));
#194480=CARTESIAN_POINT('',(109.626255861367,-1.35,48.1285150706361));
#194481=CARTESIAN_POINT('',(109.683498835237,-1.35,47.8340269691064));
#194482=CARTESIAN_POINT('',(109.135442358818,-1.35,48.0331101141869));
#194483=CARTESIAN_POINT('',(109.135442358818,-1.35,48.0331101141869));
#194484=CARTESIAN_POINT('',(109.192685332687,-1.35,47.7386220126572));
#194485=CARTESIAN_POINT('',(109.192685332687,-1.35,47.7386220126572));
#194486=CARTESIAN_POINT('',(109.192685332687,-1.35,47.7386220126572));
#194487=CARTESIAN_POINT('Origin',(109.683498835237,-1.35,47.8340269691064));
#194488=CARTESIAN_POINT('',(109.683498835237,-1.85,47.8340269691064));
#194489=CARTESIAN_POINT('',(109.626255861367,-1.85,48.1285150706361));
#194490=CARTESIAN_POINT('',(109.683498835237,-1.85,47.8340269691064));
#194491=CARTESIAN_POINT('',(109.626255861367,-1.35,48.1285150706361));
#194492=CARTESIAN_POINT('',(109.683498835237,-1.35,47.8340269691064));
#194493=CARTESIAN_POINT('Origin',(109.683498835237,-1.85,47.8340269691064));
#194494=CARTESIAN_POINT('',(109.192685332687,-1.85,47.7386220126572));
#194495=CARTESIAN_POINT('',(109.135442358818,-1.85,48.0331101141869));
#194496=CARTESIAN_POINT('',(109.192685332687,-1.85,47.7386220126572));
#194497=CARTESIAN_POINT('',(109.626255861367,-1.85,48.1285150706361));
#194498=CARTESIAN_POINT('',(109.683498835237,-1.85,47.8340269691064));
#194499=CARTESIAN_POINT('Origin',(109.192685332687,-1.85,47.7386220126572));
#194500=CARTESIAN_POINT('',(109.135442358818,-1.85,48.0331101141869));
#194501=CARTESIAN_POINT('',(109.192685332687,-1.85,47.7386220126572));
#194502=CARTESIAN_POINT('Origin',(109.192685332687,-2.15,47.7386220126572));
#194503=CARTESIAN_POINT('',(109.683498835237,-2.15,47.8340269691064));
#194504=CARTESIAN_POINT('',(109.626255861367,-2.15,48.1285150706361));
#194505=CARTESIAN_POINT('',(109.683498835237,-2.15,47.8340269691064));
#194506=CARTESIAN_POINT('',(109.135442358818,-2.15,48.0331101141869));
#194507=CARTESIAN_POINT('',(109.135442358818,-2.15,48.0331101141869));
#194508=CARTESIAN_POINT('',(109.192685332687,-2.15,47.7386220126572));
#194509=CARTESIAN_POINT('',(109.192685332687,-2.15,47.7386220126572));
#194510=CARTESIAN_POINT('',(109.192685332687,-2.15,47.7386220126572));
#194511=CARTESIAN_POINT('Origin',(109.683498835237,-2.15,47.8340269691064));
#194512=CARTESIAN_POINT('',(109.683498835237,-2.65,47.8340269691064));
#194513=CARTESIAN_POINT('',(109.626255861367,-2.65,48.1285150706361));
#194514=CARTESIAN_POINT('',(109.683498835237,-2.65,47.8340269691064));
#194515=CARTESIAN_POINT('',(109.626255861367,-2.15,48.1285150706361));
#194516=CARTESIAN_POINT('',(109.683498835237,-2.15,47.8340269691064));
#194517=CARTESIAN_POINT('Origin',(109.683498835237,-2.65,47.8340269691064));
#194518=CARTESIAN_POINT('',(109.192685332687,-2.65,47.7386220126572));
#194519=CARTESIAN_POINT('',(109.135442358818,-2.65,48.0331101141869));
#194520=CARTESIAN_POINT('',(109.192685332687,-2.65,47.7386220126572));
#194521=CARTESIAN_POINT('',(109.626255861367,-2.65,48.1285150706361));
#194522=CARTESIAN_POINT('',(109.683498835237,-2.65,47.8340269691064));
#194523=CARTESIAN_POINT('Origin',(109.192685332687,-2.65,47.7386220126572));
#194524=CARTESIAN_POINT('',(109.135442358818,-2.65,48.0331101141869));
#194525=CARTESIAN_POINT('',(109.192685332687,-2.65,47.7386220126572));
#194526=CARTESIAN_POINT('Origin',(109.192685332687,-2.95,47.7386220126572));
#194527=CARTESIAN_POINT('',(109.683498835237,-2.95,47.8340269691064));
#194528=CARTESIAN_POINT('',(109.626255861367,-2.95,48.1285150706361));
#194529=CARTESIAN_POINT('',(109.683498835237,-2.95,47.8340269691064));
#194530=CARTESIAN_POINT('',(109.135442358818,-2.95,48.0331101141869));
#194531=CARTESIAN_POINT('',(109.135442358818,-2.95,48.0331101141869));
#194532=CARTESIAN_POINT('',(109.192685332687,-2.95,47.7386220126572));
#194533=CARTESIAN_POINT('',(109.192685332687,-2.95,47.7386220126572));
#194534=CARTESIAN_POINT('',(109.192685332687,-2.95,47.7386220126572));
#194535=CARTESIAN_POINT('Origin',(109.683498835237,-2.95,47.8340269691064));
#194536=CARTESIAN_POINT('',(109.683498835237,-3.45,47.8340269691064));
#194537=CARTESIAN_POINT('',(109.626255861367,-3.45,48.1285150706361));
#194538=CARTESIAN_POINT('',(109.683498835237,-3.45,47.8340269691064));
#194539=CARTESIAN_POINT('',(109.626255861367,-2.95,48.1285150706361));
#194540=CARTESIAN_POINT('',(109.683498835237,-2.95,47.8340269691064));
#194541=CARTESIAN_POINT('Origin',(109.683498835237,-3.45,47.8340269691064));
#194542=CARTESIAN_POINT('',(109.192685332687,-3.45,47.7386220126572));
#194543=CARTESIAN_POINT('',(109.135442358818,-3.45,48.0331101141869));
#194544=CARTESIAN_POINT('',(109.192685332687,-3.45,47.7386220126572));
#194545=CARTESIAN_POINT('',(109.626255861367,-3.45,48.1285150706361));
#194546=CARTESIAN_POINT('',(109.683498835237,-3.45,47.8340269691064));
#194547=CARTESIAN_POINT('Origin',(109.192685332687,-3.45,47.7386220126572));
#194548=CARTESIAN_POINT('',(109.135442358818,-3.45,48.0331101141869));
#194549=CARTESIAN_POINT('',(109.192685332687,-3.45,47.7386220126572));
#194550=CARTESIAN_POINT('Origin',(109.192685332687,-3.75,47.7386220126572));
#194551=CARTESIAN_POINT('',(109.683498835237,-3.75,47.8340269691064));
#194552=CARTESIAN_POINT('',(109.626255861367,-3.75,48.1285150706361));
#194553=CARTESIAN_POINT('',(109.683498835237,-3.75,47.8340269691064));
#194554=CARTESIAN_POINT('',(109.135442358818,-3.75,48.0331101141869));
#194555=CARTESIAN_POINT('',(109.135442358818,-3.75,48.0331101141869));
#194556=CARTESIAN_POINT('',(109.192685332687,-3.75,47.7386220126572));
#194557=CARTESIAN_POINT('',(109.192685332687,-3.75,47.7386220126572));
#194558=CARTESIAN_POINT('',(109.192685332687,-3.75,47.7386220126572));
#194559=CARTESIAN_POINT('Origin',(109.683498835237,-3.75,47.8340269691064));
#194560=CARTESIAN_POINT('',(109.683498835237,-4.25,47.8340269691064));
#194561=CARTESIAN_POINT('',(109.626255861367,-4.25,48.1285150706361));
#194562=CARTESIAN_POINT('',(109.683498835237,-4.25,47.8340269691064));
#194563=CARTESIAN_POINT('',(109.626255861367,-3.75,48.1285150706361));
#194564=CARTESIAN_POINT('',(109.683498835237,-3.75,47.8340269691064));
#194565=CARTESIAN_POINT('Origin',(109.683498835237,-4.25,47.8340269691064));
#194566=CARTESIAN_POINT('',(109.192685332687,-4.25,47.7386220126572));
#194567=CARTESIAN_POINT('',(109.135442358818,-4.25,48.0331101141869));
#194568=CARTESIAN_POINT('',(109.192685332687,-4.25,47.7386220126572));
#194569=CARTESIAN_POINT('',(109.626255861367,-4.25,48.1285150706361));
#194570=CARTESIAN_POINT('',(109.683498835237,-4.25,47.8340269691064));
#194571=CARTESIAN_POINT('Origin',(109.192685332687,-4.25,47.7386220126572));
#194572=CARTESIAN_POINT('',(109.135442358818,-4.25,48.0331101141869));
#194573=CARTESIAN_POINT('',(109.192685332687,-4.25,47.7386220126572));
#194574=CARTESIAN_POINT('Origin',(109.192685332687,-4.55,47.7386220126572));
#194575=CARTESIAN_POINT('',(109.683498835237,-4.55,47.8340269691064));
#194576=CARTESIAN_POINT('',(109.626255861367,-4.55,48.1285150706361));
#194577=CARTESIAN_POINT('',(109.683498835237,-4.55,47.8340269691064));
#194578=CARTESIAN_POINT('',(109.135442358818,-4.55,48.0331101141869));
#194579=CARTESIAN_POINT('',(109.135442358818,-4.55,48.0331101141869));
#194580=CARTESIAN_POINT('',(109.192685332687,-4.55,47.7386220126572));
#194581=CARTESIAN_POINT('',(109.192685332687,-4.55,47.7386220126572));
#194582=CARTESIAN_POINT('',(109.192685332687,-4.55,47.7386220126572));
#194583=CARTESIAN_POINT('Origin',(109.683498835237,-4.55,47.8340269691064));
#194584=CARTESIAN_POINT('',(109.683498835237,-5.05,47.8340269691064));
#194585=CARTESIAN_POINT('',(109.626255861367,-5.05,48.1285150706361));
#194586=CARTESIAN_POINT('',(109.683498835237,-5.05,47.8340269691064));
#194587=CARTESIAN_POINT('',(109.626255861367,-4.55,48.1285150706361));
#194588=CARTESIAN_POINT('',(109.683498835237,-4.55,47.8340269691064));
#194589=CARTESIAN_POINT('Origin',(109.683498835237,-5.05,47.8340269691064));
#194590=CARTESIAN_POINT('',(109.192685332687,-5.05,47.7386220126572));
#194591=CARTESIAN_POINT('',(109.135442358818,-5.05,48.0331101141869));
#194592=CARTESIAN_POINT('',(109.192685332687,-5.05,47.7386220126572));
#194593=CARTESIAN_POINT('',(109.626255861367,-5.05,48.1285150706361));
#194594=CARTESIAN_POINT('',(109.683498835237,-5.05,47.8340269691064));
#194595=CARTESIAN_POINT('Origin',(109.192685332687,-5.05,47.7386220126572));
#194596=CARTESIAN_POINT('',(109.135442358818,-5.05,48.0331101141869));
#194597=CARTESIAN_POINT('',(109.192685332687,-5.05,47.7386220126572));
#194598=CARTESIAN_POINT('Origin',(112.333891749004,-7.75,48.3492137339324));
#194599=CARTESIAN_POINT('',(112.824705251554,-7.75,48.4446186903817));
#194600=CARTESIAN_POINT('',(112.767462277684,-7.75,48.7391067919114));
#194601=CARTESIAN_POINT('',(112.824705251554,-7.75,48.4446186903817));
#194602=CARTESIAN_POINT('',(112.276648775135,-7.75,48.6437018354621));
#194603=CARTESIAN_POINT('',(112.276648775135,-7.75,48.6437018354621));
#194604=CARTESIAN_POINT('',(112.333891749004,-7.75,48.3492137339324));
#194605=CARTESIAN_POINT('',(112.333891749004,-7.75,48.3492137339324));
#194606=CARTESIAN_POINT('',(112.333891749004,-7.75,48.3492137339324));
#194607=CARTESIAN_POINT('Origin',(112.824705251554,-7.75,48.4446186903817));
#194608=CARTESIAN_POINT('',(112.824705251554,-8.25,48.4446186903817));
#194609=CARTESIAN_POINT('',(112.767462277684,-8.25,48.7391067919114));
#194610=CARTESIAN_POINT('',(112.824705251554,-8.25,48.4446186903817));
#194611=CARTESIAN_POINT('',(112.767462277684,-7.75,48.7391067919114));
#194612=CARTESIAN_POINT('',(112.824705251554,-7.75,48.4446186903817));
#194613=CARTESIAN_POINT('Origin',(112.824705251554,-8.25,48.4446186903817));
#194614=CARTESIAN_POINT('',(112.333891749004,-8.25,48.3492137339324));
#194615=CARTESIAN_POINT('',(112.276648775135,-8.25,48.6437018354621));
#194616=CARTESIAN_POINT('',(112.333891749004,-8.25,48.3492137339324));
#194617=CARTESIAN_POINT('',(112.767462277684,-8.25,48.7391067919114));
#194618=CARTESIAN_POINT('',(112.824705251554,-8.25,48.4446186903817));
#194619=CARTESIAN_POINT('Origin',(112.333891749004,-8.25,48.3492137339324));
#194620=CARTESIAN_POINT('',(112.276648775135,-8.25,48.6437018354621));
#194621=CARTESIAN_POINT('',(112.333891749004,-8.25,48.3492137339324));
#194622=CARTESIAN_POINT('Origin',(113.119193353083,-7.75,48.5018616642512));
#194623=CARTESIAN_POINT('',(113.610006855633,-7.75,48.5972666207005));
#194624=CARTESIAN_POINT('',(113.552763881763,-7.75,48.8917547222302));
#194625=CARTESIAN_POINT('',(113.610006855633,-7.75,48.5972666207005));
#194626=CARTESIAN_POINT('',(113.061950379214,-7.75,48.7963497657809));
#194627=CARTESIAN_POINT('',(113.061950379214,-7.75,48.7963497657809));
#194628=CARTESIAN_POINT('',(113.119193353083,-7.75,48.5018616642512));
#194629=CARTESIAN_POINT('',(113.119193353083,-7.75,48.5018616642512));
#194630=CARTESIAN_POINT('',(113.119193353083,-7.75,48.5018616642512));
#194631=CARTESIAN_POINT('Origin',(113.610006855633,-7.75,48.5972666207005));
#194632=CARTESIAN_POINT('',(113.610006855633,-8.25,48.5972666207005));
#194633=CARTESIAN_POINT('',(113.552763881763,-8.25,48.8917547222302));
#194634=CARTESIAN_POINT('',(113.610006855633,-8.25,48.5972666207005));
#194635=CARTESIAN_POINT('',(113.552763881763,-7.75,48.8917547222302));
#194636=CARTESIAN_POINT('',(113.610006855633,-7.75,48.5972666207005));
#194637=CARTESIAN_POINT('Origin',(113.610006855633,-8.25,48.5972666207005));
#194638=CARTESIAN_POINT('',(113.119193353083,-8.25,48.5018616642512));
#194639=CARTESIAN_POINT('',(113.061950379214,-8.25,48.7963497657809));
#194640=CARTESIAN_POINT('',(113.119193353083,-8.25,48.5018616642512));
#194641=CARTESIAN_POINT('',(113.552763881763,-8.25,48.8917547222302));
#194642=CARTESIAN_POINT('',(113.610006855633,-8.25,48.5972666207005));
#194643=CARTESIAN_POINT('Origin',(113.119193353083,-8.25,48.5018616642512));
#194644=CARTESIAN_POINT('',(113.061950379214,-8.25,48.7963497657809));
#194645=CARTESIAN_POINT('',(113.119193353083,-8.25,48.5018616642512));
#194646=CARTESIAN_POINT('Origin',(113.904494957163,-7.75,48.65450959457));
#194647=CARTESIAN_POINT('',(114.395308459712,-7.75,48.7499145510193));
#194648=CARTESIAN_POINT('',(114.338065485842,-7.75,49.044402652549));
#194649=CARTESIAN_POINT('',(114.395308459712,-7.75,48.7499145510193));
#194650=CARTESIAN_POINT('',(113.847251983293,-7.75,48.9489976960997));
#194651=CARTESIAN_POINT('',(113.847251983293,-7.75,48.9489976960997));
#194652=CARTESIAN_POINT('',(113.904494957163,-7.75,48.65450959457));
#194653=CARTESIAN_POINT('',(113.904494957163,-7.75,48.65450959457));
#194654=CARTESIAN_POINT('',(113.904494957163,-7.75,48.65450959457));
#194655=CARTESIAN_POINT('Origin',(114.395308459712,-7.75,48.7499145510193));
#194656=CARTESIAN_POINT('',(114.395308459712,-8.25,48.7499145510193));
#194657=CARTESIAN_POINT('',(114.338065485842,-8.25,49.044402652549));
#194658=CARTESIAN_POINT('',(114.395308459712,-8.25,48.7499145510193));
#194659=CARTESIAN_POINT('',(114.338065485842,-7.75,49.044402652549));
#194660=CARTESIAN_POINT('',(114.395308459712,-7.75,48.7499145510193));
#194661=CARTESIAN_POINT('Origin',(114.395308459712,-8.25,48.7499145510193));
#194662=CARTESIAN_POINT('',(113.904494957163,-8.25,48.65450959457));
#194663=CARTESIAN_POINT('',(113.847251983293,-8.25,48.9489976960997));
#194664=CARTESIAN_POINT('',(113.904494957163,-8.25,48.65450959457));
#194665=CARTESIAN_POINT('',(114.338065485842,-8.25,49.044402652549));
#194666=CARTESIAN_POINT('',(114.395308459712,-8.25,48.7499145510193));
#194667=CARTESIAN_POINT('Origin',(113.904494957163,-8.25,48.65450959457));
#194668=CARTESIAN_POINT('',(113.847251983293,-8.25,48.9489976960997));
#194669=CARTESIAN_POINT('',(113.904494957163,-8.25,48.65450959457));
#194670=CARTESIAN_POINT('Origin',(114.689796561242,-7.75,48.8071575248888));
#194671=CARTESIAN_POINT('',(115.180610063791,-7.75,48.9025624813381));
#194672=CARTESIAN_POINT('',(115.123367089922,-7.75,49.1970505828678));
#194673=CARTESIAN_POINT('',(115.180610063791,-7.75,48.9025624813381));
#194674=CARTESIAN_POINT('',(114.632553587372,-7.75,49.1016456264185));
#194675=CARTESIAN_POINT('',(114.632553587372,-7.75,49.1016456264185));
#194676=CARTESIAN_POINT('',(114.689796561242,-7.75,48.8071575248888));
#194677=CARTESIAN_POINT('',(114.689796561242,-7.75,48.8071575248888));
#194678=CARTESIAN_POINT('',(114.689796561242,-7.75,48.8071575248888));
#194679=CARTESIAN_POINT('Origin',(115.180610063791,-7.75,48.9025624813381));
#194680=CARTESIAN_POINT('',(115.180610063791,-8.25,48.9025624813381));
#194681=CARTESIAN_POINT('',(115.123367089922,-8.25,49.1970505828678));
#194682=CARTESIAN_POINT('',(115.180610063791,-8.25,48.9025624813381));
#194683=CARTESIAN_POINT('',(115.123367089922,-7.75,49.1970505828678));
#194684=CARTESIAN_POINT('',(115.180610063791,-7.75,48.9025624813381));
#194685=CARTESIAN_POINT('Origin',(115.180610063791,-8.25,48.9025624813381));
#194686=CARTESIAN_POINT('',(114.689796561242,-8.25,48.8071575248888));
#194687=CARTESIAN_POINT('',(114.632553587372,-8.25,49.1016456264185));
#194688=CARTESIAN_POINT('',(114.689796561242,-8.25,48.8071575248888));
#194689=CARTESIAN_POINT('',(115.123367089922,-8.25,49.1970505828678));
#194690=CARTESIAN_POINT('',(115.180610063791,-8.25,48.9025624813381));
#194691=CARTESIAN_POINT('Origin',(114.689796561242,-8.25,48.8071575248888));
#194692=CARTESIAN_POINT('',(114.632553587372,-8.25,49.1016456264185));
#194693=CARTESIAN_POINT('',(114.689796561242,-8.25,48.8071575248888));
#194694=CARTESIAN_POINT('Origin',(115.475098165321,-7.75,48.9598054552076));
#194695=CARTESIAN_POINT('',(115.96591166787,-7.75,49.0552104116569));
#194696=CARTESIAN_POINT('',(115.908668694001,-7.75,49.3496985131866));
#194697=CARTESIAN_POINT('',(115.96591166787,-7.75,49.0552104116569));
#194698=CARTESIAN_POINT('',(115.417855191451,-7.75,49.2542935567373));
#194699=CARTESIAN_POINT('',(115.417855191451,-7.75,49.2542935567373));
#194700=CARTESIAN_POINT('',(115.475098165321,-7.75,48.9598054552076));
#194701=CARTESIAN_POINT('',(115.475098165321,-7.75,48.9598054552076));
#194702=CARTESIAN_POINT('',(115.475098165321,-7.75,48.9598054552076));
#194703=CARTESIAN_POINT('Origin',(115.96591166787,-7.75,49.0552104116569));
#194704=CARTESIAN_POINT('',(115.96591166787,-8.25,49.0552104116569));
#194705=CARTESIAN_POINT('',(115.908668694001,-8.25,49.3496985131866));
#194706=CARTESIAN_POINT('',(115.96591166787,-8.25,49.0552104116569));
#194707=CARTESIAN_POINT('',(115.908668694001,-7.75,49.3496985131866));
#194708=CARTESIAN_POINT('',(115.96591166787,-7.75,49.0552104116569));
#194709=CARTESIAN_POINT('Origin',(115.96591166787,-8.25,49.0552104116569));
#194710=CARTESIAN_POINT('',(115.475098165321,-8.25,48.9598054552076));
#194711=CARTESIAN_POINT('',(115.417855191451,-8.25,49.2542935567373));
#194712=CARTESIAN_POINT('',(115.475098165321,-8.25,48.9598054552076));
#194713=CARTESIAN_POINT('',(115.908668694001,-8.25,49.3496985131866));
#194714=CARTESIAN_POINT('',(115.96591166787,-8.25,49.0552104116569));
#194715=CARTESIAN_POINT('Origin',(115.475098165321,-8.25,48.9598054552076));
#194716=CARTESIAN_POINT('',(115.417855191451,-8.25,49.2542935567373));
#194717=CARTESIAN_POINT('',(115.475098165321,-8.25,48.9598054552076));
#194718=CARTESIAN_POINT('Origin',(116.2603997694,-7.75,49.1124533855264));
#194719=CARTESIAN_POINT('',(116.75121327195,-7.75,49.2078583419757));
#194720=CARTESIAN_POINT('',(116.69397029808,-7.75,49.5023464435054));
#194721=CARTESIAN_POINT('',(116.75121327195,-7.75,49.2078583419757));
#194722=CARTESIAN_POINT('',(116.203156795531,-7.75,49.4069414870561));
#194723=CARTESIAN_POINT('',(116.203156795531,-7.75,49.4069414870561));
#194724=CARTESIAN_POINT('',(116.2603997694,-7.75,49.1124533855264));
#194725=CARTESIAN_POINT('',(116.2603997694,-7.75,49.1124533855264));
#194726=CARTESIAN_POINT('',(116.2603997694,-7.75,49.1124533855264));
#194727=CARTESIAN_POINT('Origin',(116.75121327195,-7.75,49.2078583419757));
#194728=CARTESIAN_POINT('',(116.75121327195,-8.25,49.2078583419757));
#194729=CARTESIAN_POINT('',(116.69397029808,-8.25,49.5023464435054));
#194730=CARTESIAN_POINT('',(116.75121327195,-8.25,49.2078583419757));
#194731=CARTESIAN_POINT('',(116.69397029808,-7.75,49.5023464435054));
#194732=CARTESIAN_POINT('',(116.75121327195,-7.75,49.2078583419757));
#194733=CARTESIAN_POINT('Origin',(116.75121327195,-8.25,49.2078583419757));
#194734=CARTESIAN_POINT('',(116.2603997694,-8.25,49.1124533855264));
#194735=CARTESIAN_POINT('',(116.203156795531,-8.25,49.4069414870561));
#194736=CARTESIAN_POINT('',(116.2603997694,-8.25,49.1124533855264));
#194737=CARTESIAN_POINT('',(116.69397029808,-8.25,49.5023464435054));
#194738=CARTESIAN_POINT('',(116.75121327195,-8.25,49.2078583419757));
#194739=CARTESIAN_POINT('Origin',(116.2603997694,-8.25,49.1124533855264));
#194740=CARTESIAN_POINT('',(116.203156795531,-8.25,49.4069414870561));
#194741=CARTESIAN_POINT('',(116.2603997694,-8.25,49.1124533855264));
#194742=CARTESIAN_POINT('Origin',(117.045701373479,-7.75,49.2651013158452));
#194743=CARTESIAN_POINT('',(117.536514876029,-7.75,49.3605062722945));
#194744=CARTESIAN_POINT('',(117.479271902159,-7.75,49.6549943738242));
#194745=CARTESIAN_POINT('',(117.536514876029,-7.75,49.3605062722945));
#194746=CARTESIAN_POINT('',(116.98845839961,-7.75,49.5595894173749));
#194747=CARTESIAN_POINT('',(116.98845839961,-7.75,49.5595894173749));
#194748=CARTESIAN_POINT('',(117.045701373479,-7.75,49.2651013158452));
#194749=CARTESIAN_POINT('',(117.045701373479,-7.75,49.2651013158452));
#194750=CARTESIAN_POINT('',(117.045701373479,-7.75,49.2651013158452));
#194751=CARTESIAN_POINT('Origin',(117.536514876029,-7.75,49.3605062722945));
#194752=CARTESIAN_POINT('',(117.536514876029,-8.25,49.3605062722945));
#194753=CARTESIAN_POINT('',(117.479271902159,-8.25,49.6549943738242));
#194754=CARTESIAN_POINT('',(117.536514876029,-8.25,49.3605062722945));
#194755=CARTESIAN_POINT('',(117.479271902159,-7.75,49.6549943738242));
#194756=CARTESIAN_POINT('',(117.536514876029,-7.75,49.3605062722945));
#194757=CARTESIAN_POINT('Origin',(117.536514876029,-8.25,49.3605062722945));
#194758=CARTESIAN_POINT('',(117.045701373479,-8.25,49.2651013158452));
#194759=CARTESIAN_POINT('',(116.98845839961,-8.25,49.5595894173749));
#194760=CARTESIAN_POINT('',(117.045701373479,-8.25,49.2651013158452));
#194761=CARTESIAN_POINT('',(117.479271902159,-8.25,49.6549943738242));
#194762=CARTESIAN_POINT('',(117.536514876029,-8.25,49.3605062722945));
#194763=CARTESIAN_POINT('Origin',(117.045701373479,-8.25,49.2651013158452));
#194764=CARTESIAN_POINT('',(116.98845839961,-8.25,49.5595894173749));
#194765=CARTESIAN_POINT('',(117.045701373479,-8.25,49.2651013158452));
#194766=CARTESIAN_POINT('Origin',(117.831002977559,-7.75,49.417749246164));
#194767=CARTESIAN_POINT('',(118.321816480108,-7.75,49.5131542026133));
#194768=CARTESIAN_POINT('',(118.264573506239,-7.75,49.807642304143));
#194769=CARTESIAN_POINT('',(118.321816480108,-7.75,49.5131542026133));
#194770=CARTESIAN_POINT('',(117.773760003689,-7.75,49.7122373476937));
#194771=CARTESIAN_POINT('',(117.773760003689,-7.75,49.7122373476937));
#194772=CARTESIAN_POINT('',(117.831002977559,-7.75,49.417749246164));
#194773=CARTESIAN_POINT('',(117.831002977559,-7.75,49.417749246164));
#194774=CARTESIAN_POINT('',(117.831002977559,-7.75,49.417749246164));
#194775=CARTESIAN_POINT('Origin',(118.321816480108,-7.75,49.5131542026133));
#194776=CARTESIAN_POINT('',(118.321816480108,-8.25,49.5131542026133));
#194777=CARTESIAN_POINT('',(118.264573506239,-8.25,49.807642304143));
#194778=CARTESIAN_POINT('',(118.321816480108,-8.25,49.5131542026133));
#194779=CARTESIAN_POINT('',(118.264573506239,-7.75,49.807642304143));
#194780=CARTESIAN_POINT('',(118.321816480108,-7.75,49.5131542026133));
#194781=CARTESIAN_POINT('Origin',(118.321816480108,-8.25,49.5131542026133));
#194782=CARTESIAN_POINT('',(117.831002977559,-8.25,49.417749246164));
#194783=CARTESIAN_POINT('',(117.773760003689,-8.25,49.7122373476937));
#194784=CARTESIAN_POINT('',(117.831002977559,-8.25,49.417749246164));
#194785=CARTESIAN_POINT('',(118.264573506239,-8.25,49.807642304143));
#194786=CARTESIAN_POINT('',(118.321816480108,-8.25,49.5131542026133));
#194787=CARTESIAN_POINT('Origin',(117.831002977559,-8.25,49.417749246164));
#194788=CARTESIAN_POINT('',(117.773760003689,-8.25,49.7122373476937));
#194789=CARTESIAN_POINT('',(117.831002977559,-8.25,49.417749246164));
#194790=CARTESIAN_POINT('Origin',(118.616304581638,-7.75,49.5703971764828));
#194791=CARTESIAN_POINT('',(119.107118084187,-7.75,49.6658021329321));
#194792=CARTESIAN_POINT('',(119.049875110318,-7.75,49.9602902344618));
#194793=CARTESIAN_POINT('',(119.107118084187,-7.75,49.6658021329321));
#194794=CARTESIAN_POINT('',(118.559061607768,-7.75,49.8648852780125));
#194795=CARTESIAN_POINT('',(118.559061607768,-7.75,49.8648852780125));
#194796=CARTESIAN_POINT('',(118.616304581638,-7.75,49.5703971764828));
#194797=CARTESIAN_POINT('',(118.616304581638,-7.75,49.5703971764828));
#194798=CARTESIAN_POINT('',(118.616304581638,-7.75,49.5703971764828));
#194799=CARTESIAN_POINT('Origin',(119.107118084187,-7.75,49.6658021329321));
#194800=CARTESIAN_POINT('',(119.107118084187,-8.25,49.6658021329321));
#194801=CARTESIAN_POINT('',(119.049875110318,-8.25,49.9602902344618));
#194802=CARTESIAN_POINT('',(119.107118084187,-8.25,49.6658021329321));
#194803=CARTESIAN_POINT('',(119.049875110318,-7.75,49.9602902344618));
#194804=CARTESIAN_POINT('',(119.107118084187,-7.75,49.6658021329321));
#194805=CARTESIAN_POINT('Origin',(119.107118084187,-8.25,49.6658021329321));
#194806=CARTESIAN_POINT('',(118.616304581638,-8.25,49.5703971764828));
#194807=CARTESIAN_POINT('',(118.559061607768,-8.25,49.8648852780125));
#194808=CARTESIAN_POINT('',(118.616304581638,-8.25,49.5703971764828));
#194809=CARTESIAN_POINT('',(119.049875110318,-8.25,49.9602902344618));
#194810=CARTESIAN_POINT('',(119.107118084187,-8.25,49.6658021329321));
#194811=CARTESIAN_POINT('Origin',(118.616304581638,-8.25,49.5703971764828));
#194812=CARTESIAN_POINT('',(118.559061607768,-8.25,49.8648852780125));
#194813=CARTESIAN_POINT('',(118.616304581638,-8.25,49.5703971764828));
#194814=CARTESIAN_POINT('Origin',(119.401606185717,-7.75,49.7230451068016));
#194815=CARTESIAN_POINT('',(119.892419688267,-7.75,49.8184500632509));
#194816=CARTESIAN_POINT('',(119.835176714397,-7.75,50.1129381647806));
#194817=CARTESIAN_POINT('',(119.892419688267,-7.75,49.8184500632509));
#194818=CARTESIAN_POINT('',(119.344363211847,-7.75,50.0175332083313));
#194819=CARTESIAN_POINT('',(119.344363211847,-7.75,50.0175332083313));
#194820=CARTESIAN_POINT('',(119.401606185717,-7.75,49.7230451068016));
#194821=CARTESIAN_POINT('',(119.401606185717,-7.75,49.7230451068016));
#194822=CARTESIAN_POINT('',(119.401606185717,-7.75,49.7230451068016));
#194823=CARTESIAN_POINT('Origin',(119.892419688267,-7.75,49.8184500632509));
#194824=CARTESIAN_POINT('',(119.892419688267,-8.25,49.8184500632509));
#194825=CARTESIAN_POINT('',(119.835176714397,-8.25,50.1129381647806));
#194826=CARTESIAN_POINT('',(119.892419688267,-8.25,49.8184500632509));
#194827=CARTESIAN_POINT('',(119.835176714397,-7.75,50.1129381647806));
#194828=CARTESIAN_POINT('',(119.892419688267,-7.75,49.8184500632509));
#194829=CARTESIAN_POINT('Origin',(119.892419688267,-8.25,49.8184500632509));
#194830=CARTESIAN_POINT('',(119.401606185717,-8.25,49.7230451068016));
#194831=CARTESIAN_POINT('',(119.344363211847,-8.25,50.0175332083313));
#194832=CARTESIAN_POINT('',(119.401606185717,-8.25,49.7230451068016));
#194833=CARTESIAN_POINT('',(119.835176714397,-8.25,50.1129381647806));
#194834=CARTESIAN_POINT('',(119.892419688267,-8.25,49.8184500632509));
#194835=CARTESIAN_POINT('Origin',(119.401606185717,-8.25,49.7230451068016));
#194836=CARTESIAN_POINT('',(119.344363211847,-8.25,50.0175332083313));
#194837=CARTESIAN_POINT('',(119.401606185717,-8.25,49.7230451068016));
#194838=CARTESIAN_POINT('Origin',(120.186907789796,-7.75,49.8756930371204));
#194839=CARTESIAN_POINT('',(120.677721292346,-7.75,49.9710979935697));
#194840=CARTESIAN_POINT('',(120.620478318476,-7.75,50.2655860950994));
#194841=CARTESIAN_POINT('',(120.677721292346,-7.75,49.9710979935697));
#194842=CARTESIAN_POINT('',(120.129664815927,-7.75,50.1701811386501));
#194843=CARTESIAN_POINT('',(120.129664815927,-7.75,50.1701811386501));
#194844=CARTESIAN_POINT('',(120.186907789796,-7.75,49.8756930371204));
#194845=CARTESIAN_POINT('',(120.186907789796,-7.75,49.8756930371204));
#194846=CARTESIAN_POINT('',(120.186907789796,-7.75,49.8756930371204));
#194847=CARTESIAN_POINT('Origin',(120.677721292346,-7.75,49.9710979935697));
#194848=CARTESIAN_POINT('',(120.677721292346,-8.25,49.9710979935697));
#194849=CARTESIAN_POINT('',(120.620478318476,-8.25,50.2655860950994));
#194850=CARTESIAN_POINT('',(120.677721292346,-8.25,49.9710979935697));
#194851=CARTESIAN_POINT('',(120.620478318476,-7.75,50.2655860950994));
#194852=CARTESIAN_POINT('',(120.677721292346,-7.75,49.9710979935697));
#194853=CARTESIAN_POINT('Origin',(120.677721292346,-8.25,49.9710979935697));
#194854=CARTESIAN_POINT('',(120.186907789796,-8.25,49.8756930371204));
#194855=CARTESIAN_POINT('',(120.129664815927,-8.25,50.1701811386501));
#194856=CARTESIAN_POINT('',(120.186907789796,-8.25,49.8756930371204));
#194857=CARTESIAN_POINT('',(120.620478318476,-8.25,50.2655860950994));
#194858=CARTESIAN_POINT('',(120.677721292346,-8.25,49.9710979935697));
#194859=CARTESIAN_POINT('Origin',(120.186907789796,-8.25,49.8756930371204));
#194860=CARTESIAN_POINT('',(120.129664815927,-8.25,50.1701811386501));
#194861=CARTESIAN_POINT('',(120.186907789796,-8.25,49.8756930371204));
#194862=CARTESIAN_POINT('Origin',(120.972209393875,-7.75,50.0283409674392));
#194863=CARTESIAN_POINT('',(121.463022896425,-7.75,50.1237459238885));
#194864=CARTESIAN_POINT('',(121.405779922555,-7.75,50.4182340254182));
#194865=CARTESIAN_POINT('',(121.463022896425,-7.75,50.1237459238885));
#194866=CARTESIAN_POINT('',(120.914966420006,-7.75,50.3228290689689));
#194867=CARTESIAN_POINT('',(120.914966420006,-7.75,50.3228290689689));
#194868=CARTESIAN_POINT('',(120.972209393875,-7.75,50.0283409674392));
#194869=CARTESIAN_POINT('',(120.972209393875,-7.75,50.0283409674392));
#194870=CARTESIAN_POINT('',(120.972209393875,-7.75,50.0283409674392));
#194871=CARTESIAN_POINT('Origin',(121.463022896425,-7.75,50.1237459238885));
#194872=CARTESIAN_POINT('',(121.463022896425,-8.25,50.1237459238885));
#194873=CARTESIAN_POINT('',(121.405779922555,-8.25,50.4182340254182));
#194874=CARTESIAN_POINT('',(121.463022896425,-8.25,50.1237459238885));
#194875=CARTESIAN_POINT('',(121.405779922555,-7.75,50.4182340254182));
#194876=CARTESIAN_POINT('',(121.463022896425,-7.75,50.1237459238885));
#194877=CARTESIAN_POINT('Origin',(121.463022896425,-8.25,50.1237459238885));
#194878=CARTESIAN_POINT('',(120.972209393875,-8.25,50.0283409674392));
#194879=CARTESIAN_POINT('',(120.914966420006,-8.25,50.3228290689689));
#194880=CARTESIAN_POINT('',(120.972209393875,-8.25,50.0283409674392));
#194881=CARTESIAN_POINT('',(121.405779922555,-8.25,50.4182340254182));
#194882=CARTESIAN_POINT('',(121.463022896425,-8.25,50.1237459238885));
#194883=CARTESIAN_POINT('Origin',(120.972209393875,-8.25,50.0283409674392));
#194884=CARTESIAN_POINT('',(120.914966420006,-8.25,50.3228290689689));
#194885=CARTESIAN_POINT('',(120.972209393875,-8.25,50.0283409674392));
#194886=CARTESIAN_POINT('Origin',(121.757510997955,-7.75,50.180988897758));
#194887=CARTESIAN_POINT('',(122.248324500504,-7.75,50.2763938542073));
#194888=CARTESIAN_POINT('',(122.191081526635,-7.75,50.570881955737));
#194889=CARTESIAN_POINT('',(122.248324500504,-7.75,50.2763938542073));
#194890=CARTESIAN_POINT('',(121.700268024085,-7.75,50.4754769992877));
#194891=CARTESIAN_POINT('',(121.700268024085,-7.75,50.4754769992877));
#194892=CARTESIAN_POINT('',(121.757510997955,-7.75,50.180988897758));
#194893=CARTESIAN_POINT('',(121.757510997955,-7.75,50.180988897758));
#194894=CARTESIAN_POINT('',(121.757510997955,-7.75,50.180988897758));
#194895=CARTESIAN_POINT('Origin',(122.248324500504,-7.75,50.2763938542073));
#194896=CARTESIAN_POINT('',(122.248324500504,-8.25,50.2763938542073));
#194897=CARTESIAN_POINT('',(122.191081526635,-8.25,50.570881955737));
#194898=CARTESIAN_POINT('',(122.248324500504,-8.25,50.2763938542073));
#194899=CARTESIAN_POINT('',(122.191081526635,-7.75,50.570881955737));
#194900=CARTESIAN_POINT('',(122.248324500504,-7.75,50.2763938542073));
#194901=CARTESIAN_POINT('Origin',(122.248324500504,-8.25,50.2763938542073));
#194902=CARTESIAN_POINT('',(121.757510997955,-8.25,50.180988897758));
#194903=CARTESIAN_POINT('',(121.700268024085,-8.25,50.4754769992877));
#194904=CARTESIAN_POINT('',(121.757510997955,-8.25,50.180988897758));
#194905=CARTESIAN_POINT('',(122.191081526635,-8.25,50.570881955737));
#194906=CARTESIAN_POINT('',(122.248324500504,-8.25,50.2763938542073));
#194907=CARTESIAN_POINT('Origin',(121.757510997955,-8.25,50.180988897758));
#194908=CARTESIAN_POINT('',(121.700268024085,-8.25,50.4754769992877));
#194909=CARTESIAN_POINT('',(121.757510997955,-8.25,50.180988897758));
#194910=CARTESIAN_POINT('Origin',(124.898717414272,-4.55,50.7915806190332));
#194911=CARTESIAN_POINT('',(125.389530916821,-4.55,50.8869855754825));
#194912=CARTESIAN_POINT('',(125.332287942951,-4.55,51.1814736770122));
#194913=CARTESIAN_POINT('',(125.389530916821,-4.55,50.8869855754825));
#194914=CARTESIAN_POINT('',(124.841474440402,-4.55,51.0860687205629));
#194915=CARTESIAN_POINT('',(124.841474440402,-4.55,51.0860687205629));
#194916=CARTESIAN_POINT('',(124.898717414272,-4.55,50.7915806190332));
#194917=CARTESIAN_POINT('',(124.898717414272,-4.55,50.7915806190332));
#194918=CARTESIAN_POINT('',(124.898717414272,-4.55,50.7915806190332));
#194919=CARTESIAN_POINT('Origin',(125.389530916821,-4.55,50.8869855754825));
#194920=CARTESIAN_POINT('',(125.389530916821,-5.05,50.8869855754825));
#194921=CARTESIAN_POINT('',(125.332287942951,-5.05,51.1814736770122));
#194922=CARTESIAN_POINT('',(125.389530916821,-5.05,50.8869855754825));
#194923=CARTESIAN_POINT('',(125.332287942951,-4.55,51.1814736770122));
#194924=CARTESIAN_POINT('',(125.389530916821,-4.55,50.8869855754825));
#194925=CARTESIAN_POINT('Origin',(125.389530916821,-5.05,50.8869855754825));
#194926=CARTESIAN_POINT('',(124.898717414272,-5.05,50.7915806190332));
#194927=CARTESIAN_POINT('',(124.841474440402,-5.05,51.0860687205629));
#194928=CARTESIAN_POINT('',(124.898717414272,-5.05,50.7915806190332));
#194929=CARTESIAN_POINT('',(125.332287942951,-5.05,51.1814736770122));
#194930=CARTESIAN_POINT('',(125.389530916821,-5.05,50.8869855754825));
#194931=CARTESIAN_POINT('Origin',(124.898717414272,-5.05,50.7915806190332));
#194932=CARTESIAN_POINT('',(124.841474440402,-5.05,51.0860687205629));
#194933=CARTESIAN_POINT('',(124.898717414272,-5.05,50.7915806190332));
#194934=CARTESIAN_POINT('Origin',(124.898717414272,-3.75,50.7915806190332));
#194935=CARTESIAN_POINT('',(125.389530916821,-3.75,50.8869855754825));
#194936=CARTESIAN_POINT('',(125.332287942951,-3.75,51.1814736770122));
#194937=CARTESIAN_POINT('',(125.389530916821,-3.75,50.8869855754825));
#194938=CARTESIAN_POINT('',(124.841474440402,-3.75,51.0860687205629));
#194939=CARTESIAN_POINT('',(124.841474440402,-3.75,51.0860687205629));
#194940=CARTESIAN_POINT('',(124.898717414272,-3.75,50.7915806190332));
#194941=CARTESIAN_POINT('',(124.898717414272,-3.75,50.7915806190332));
#194942=CARTESIAN_POINT('',(124.898717414272,-3.75,50.7915806190332));
#194943=CARTESIAN_POINT('Origin',(125.389530916821,-3.75,50.8869855754825));
#194944=CARTESIAN_POINT('',(125.389530916821,-4.25,50.8869855754825));
#194945=CARTESIAN_POINT('',(125.332287942951,-4.25,51.1814736770122));
#194946=CARTESIAN_POINT('',(125.389530916821,-4.25,50.8869855754825));
#194947=CARTESIAN_POINT('',(125.332287942951,-3.75,51.1814736770122));
#194948=CARTESIAN_POINT('',(125.389530916821,-3.75,50.8869855754825));
#194949=CARTESIAN_POINT('Origin',(125.389530916821,-4.25,50.8869855754825));
#194950=CARTESIAN_POINT('',(124.898717414272,-4.25,50.7915806190332));
#194951=CARTESIAN_POINT('',(124.841474440402,-4.25,51.0860687205629));
#194952=CARTESIAN_POINT('',(124.898717414272,-4.25,50.7915806190332));
#194953=CARTESIAN_POINT('',(125.332287942951,-4.25,51.1814736770122));
#194954=CARTESIAN_POINT('',(125.389530916821,-4.25,50.8869855754825));
#194955=CARTESIAN_POINT('Origin',(124.898717414272,-4.25,50.7915806190332));
#194956=CARTESIAN_POINT('',(124.841474440402,-4.25,51.0860687205629));
#194957=CARTESIAN_POINT('',(124.898717414272,-4.25,50.7915806190332));
#194958=CARTESIAN_POINT('Origin',(124.898717414272,-2.95,50.7915806190332));
#194959=CARTESIAN_POINT('',(125.389530916821,-2.95,50.8869855754825));
#194960=CARTESIAN_POINT('',(125.332287942951,-2.95,51.1814736770122));
#194961=CARTESIAN_POINT('',(125.389530916821,-2.95,50.8869855754825));
#194962=CARTESIAN_POINT('',(124.841474440402,-2.95,51.0860687205629));
#194963=CARTESIAN_POINT('',(124.841474440402,-2.95,51.0860687205629));
#194964=CARTESIAN_POINT('',(124.898717414272,-2.95,50.7915806190332));
#194965=CARTESIAN_POINT('',(124.898717414272,-2.95,50.7915806190332));
#194966=CARTESIAN_POINT('',(124.898717414272,-2.95,50.7915806190332));
#194967=CARTESIAN_POINT('Origin',(125.389530916821,-2.95,50.8869855754825));
#194968=CARTESIAN_POINT('',(125.389530916821,-3.45,50.8869855754825));
#194969=CARTESIAN_POINT('',(125.332287942951,-3.45,51.1814736770122));
#194970=CARTESIAN_POINT('',(125.389530916821,-3.45,50.8869855754825));
#194971=CARTESIAN_POINT('',(125.332287942951,-2.95,51.1814736770122));
#194972=CARTESIAN_POINT('',(125.389530916821,-2.95,50.8869855754825));
#194973=CARTESIAN_POINT('Origin',(125.389530916821,-3.45,50.8869855754825));
#194974=CARTESIAN_POINT('',(124.898717414272,-3.45,50.7915806190332));
#194975=CARTESIAN_POINT('',(124.841474440402,-3.45,51.0860687205629));
#194976=CARTESIAN_POINT('',(124.898717414272,-3.45,50.7915806190332));
#194977=CARTESIAN_POINT('',(125.332287942951,-3.45,51.1814736770122));
#194978=CARTESIAN_POINT('',(125.389530916821,-3.45,50.8869855754825));
#194979=CARTESIAN_POINT('Origin',(124.898717414272,-3.45,50.7915806190332));
#194980=CARTESIAN_POINT('',(124.841474440402,-3.45,51.0860687205629));
#194981=CARTESIAN_POINT('',(124.898717414272,-3.45,50.7915806190332));
#194982=CARTESIAN_POINT('Origin',(124.898717414272,-2.15,50.7915806190332));
#194983=CARTESIAN_POINT('',(125.389530916821,-2.15,50.8869855754825));
#194984=CARTESIAN_POINT('',(125.332287942951,-2.15,51.1814736770122));
#194985=CARTESIAN_POINT('',(125.389530916821,-2.15,50.8869855754825));
#194986=CARTESIAN_POINT('',(124.841474440402,-2.15,51.0860687205629));
#194987=CARTESIAN_POINT('',(124.841474440402,-2.15,51.0860687205629));
#194988=CARTESIAN_POINT('',(124.898717414272,-2.15,50.7915806190332));
#194989=CARTESIAN_POINT('',(124.898717414272,-2.15,50.7915806190332));
#194990=CARTESIAN_POINT('',(124.898717414272,-2.15,50.7915806190332));
#194991=CARTESIAN_POINT('Origin',(125.389530916821,-2.15,50.8869855754825));
#194992=CARTESIAN_POINT('',(125.389530916821,-2.65,50.8869855754825));
#194993=CARTESIAN_POINT('',(125.332287942951,-2.65,51.1814736770122));
#194994=CARTESIAN_POINT('',(125.389530916821,-2.65,50.8869855754825));
#194995=CARTESIAN_POINT('',(125.332287942951,-2.15,51.1814736770122));
#194996=CARTESIAN_POINT('',(125.389530916821,-2.15,50.8869855754825));
#194997=CARTESIAN_POINT('Origin',(125.389530916821,-2.65,50.8869855754825));
#194998=CARTESIAN_POINT('',(124.898717414272,-2.65,50.7915806190332));
#194999=CARTESIAN_POINT('',(124.841474440402,-2.65,51.0860687205629));
#195000=CARTESIAN_POINT('',(124.898717414272,-2.65,50.7915806190332));
#195001=CARTESIAN_POINT('',(125.332287942951,-2.65,51.1814736770122));
#195002=CARTESIAN_POINT('',(125.389530916821,-2.65,50.8869855754825));
#195003=CARTESIAN_POINT('Origin',(124.898717414272,-2.65,50.7915806190332));
#195004=CARTESIAN_POINT('',(124.841474440402,-2.65,51.0860687205629));
#195005=CARTESIAN_POINT('',(124.898717414272,-2.65,50.7915806190332));
#195006=CARTESIAN_POINT('Origin',(124.898717414272,-1.35,50.7915806190332));
#195007=CARTESIAN_POINT('',(125.389530916821,-1.35,50.8869855754825));
#195008=CARTESIAN_POINT('',(125.332287942951,-1.35,51.1814736770122));
#195009=CARTESIAN_POINT('',(125.389530916821,-1.35,50.8869855754825));
#195010=CARTESIAN_POINT('',(124.841474440402,-1.35,51.0860687205629));
#195011=CARTESIAN_POINT('',(124.841474440402,-1.35,51.0860687205629));
#195012=CARTESIAN_POINT('',(124.898717414272,-1.35,50.7915806190332));
#195013=CARTESIAN_POINT('',(124.898717414272,-1.35,50.7915806190332));
#195014=CARTESIAN_POINT('',(124.898717414272,-1.35,50.7915806190332));
#195015=CARTESIAN_POINT('Origin',(125.389530916821,-1.35,50.8869855754825));
#195016=CARTESIAN_POINT('',(125.389530916821,-1.85,50.8869855754825));
#195017=CARTESIAN_POINT('',(125.332287942951,-1.85,51.1814736770122));
#195018=CARTESIAN_POINT('',(125.389530916821,-1.85,50.8869855754825));
#195019=CARTESIAN_POINT('',(125.332287942951,-1.35,51.1814736770122));
#195020=CARTESIAN_POINT('',(125.389530916821,-1.35,50.8869855754825));
#195021=CARTESIAN_POINT('Origin',(125.389530916821,-1.85,50.8869855754825));
#195022=CARTESIAN_POINT('',(124.898717414272,-1.85,50.7915806190332));
#195023=CARTESIAN_POINT('',(124.841474440402,-1.85,51.0860687205629));
#195024=CARTESIAN_POINT('',(124.898717414272,-1.85,50.7915806190332));
#195025=CARTESIAN_POINT('',(125.332287942951,-1.85,51.1814736770122));
#195026=CARTESIAN_POINT('',(125.389530916821,-1.85,50.8869855754825));
#195027=CARTESIAN_POINT('Origin',(124.898717414272,-1.85,50.7915806190332));
#195028=CARTESIAN_POINT('',(124.841474440402,-1.85,51.0860687205629));
#195029=CARTESIAN_POINT('',(124.898717414272,-1.85,50.7915806190332));
#195030=CARTESIAN_POINT('Origin',(124.898717414272,-0.549999999999986,50.7915806190332));
#195031=CARTESIAN_POINT('',(125.389530916821,-0.549999999999986,50.8869855754825));
#195032=CARTESIAN_POINT('',(125.332287942951,-0.549999999999986,51.1814736770122));
#195033=CARTESIAN_POINT('',(125.389530916821,-0.549999999999986,50.8869855754825));
#195034=CARTESIAN_POINT('',(124.841474440402,-0.549999999999986,51.0860687205629));
#195035=CARTESIAN_POINT('',(124.841474440402,-0.549999999999986,51.0860687205629));
#195036=CARTESIAN_POINT('',(124.898717414272,-0.549999999999986,50.7915806190332));
#195037=CARTESIAN_POINT('',(124.898717414272,-0.549999999999986,50.7915806190332));
#195038=CARTESIAN_POINT('',(124.898717414272,-0.549999999999986,50.7915806190332));
#195039=CARTESIAN_POINT('Origin',(125.389530916821,-0.549999999999986,50.8869855754825));
#195040=CARTESIAN_POINT('',(125.389530916821,-1.05,50.8869855754825));
#195041=CARTESIAN_POINT('',(125.332287942951,-1.05,51.1814736770122));
#195042=CARTESIAN_POINT('',(125.389530916821,-1.05,50.8869855754825));
#195043=CARTESIAN_POINT('',(125.332287942951,-0.549999999999986,51.1814736770122));
#195044=CARTESIAN_POINT('',(125.389530916821,-0.549999999999986,50.8869855754825));
#195045=CARTESIAN_POINT('Origin',(125.389530916821,-1.05,50.8869855754825));
#195046=CARTESIAN_POINT('',(124.898717414272,-1.05,50.7915806190332));
#195047=CARTESIAN_POINT('',(124.841474440402,-1.05,51.0860687205629));
#195048=CARTESIAN_POINT('',(124.898717414272,-1.05,50.7915806190332));
#195049=CARTESIAN_POINT('',(125.332287942951,-1.05,51.1814736770122));
#195050=CARTESIAN_POINT('',(125.389530916821,-1.05,50.8869855754825));
#195051=CARTESIAN_POINT('Origin',(124.898717414272,-1.05,50.7915806190332));
#195052=CARTESIAN_POINT('',(124.841474440402,-1.05,51.0860687205629));
#195053=CARTESIAN_POINT('',(124.898717414272,-1.05,50.7915806190332));
#195054=CARTESIAN_POINT('Origin',(124.898717414272,0.250000000000015,50.7915806190332));
#195055=CARTESIAN_POINT('',(125.389530916821,0.250000000000015,50.8869855754825));
#195056=CARTESIAN_POINT('',(125.332287942951,0.250000000000015,51.1814736770122));
#195057=CARTESIAN_POINT('',(125.389530916821,0.250000000000015,50.8869855754825));
#195058=CARTESIAN_POINT('',(124.841474440402,0.250000000000015,51.0860687205629));
#195059=CARTESIAN_POINT('',(124.841474440402,0.250000000000015,51.0860687205629));
#195060=CARTESIAN_POINT('',(124.898717414272,0.250000000000015,50.7915806190332));
#195061=CARTESIAN_POINT('',(124.898717414272,0.250000000000015,50.7915806190332));
#195062=CARTESIAN_POINT('',(124.898717414272,0.250000000000015,50.7915806190332));
#195063=CARTESIAN_POINT('Origin',(125.389530916821,0.250000000000015,50.8869855754825));
#195064=CARTESIAN_POINT('',(125.389530916821,-0.249999999999985,50.8869855754825));
#195065=CARTESIAN_POINT('',(125.332287942951,-0.249999999999985,51.1814736770122));
#195066=CARTESIAN_POINT('',(125.389530916821,-0.249999999999985,50.8869855754825));
#195067=CARTESIAN_POINT('',(125.332287942951,0.250000000000015,51.1814736770122));
#195068=CARTESIAN_POINT('',(125.389530916821,0.250000000000015,50.8869855754825));
#195069=CARTESIAN_POINT('Origin',(125.389530916821,-0.249999999999985,50.8869855754825));
#195070=CARTESIAN_POINT('',(124.898717414272,-0.249999999999985,50.7915806190332));
#195071=CARTESIAN_POINT('',(124.841474440402,-0.249999999999985,51.0860687205629));
#195072=CARTESIAN_POINT('',(124.898717414272,-0.249999999999985,50.7915806190332));
#195073=CARTESIAN_POINT('',(125.332287942951,-0.249999999999985,51.1814736770122));
#195074=CARTESIAN_POINT('',(125.389530916821,-0.249999999999985,50.8869855754825));
#195075=CARTESIAN_POINT('Origin',(124.898717414272,-0.249999999999985,50.7915806190332));
#195076=CARTESIAN_POINT('',(124.841474440402,-0.249999999999985,51.0860687205629));
#195077=CARTESIAN_POINT('',(124.898717414272,-0.249999999999985,50.7915806190332));
#195078=CARTESIAN_POINT('Origin',(124.898717414272,1.05,50.7915806190332));
#195079=CARTESIAN_POINT('',(125.389530916821,1.05,50.8869855754825));
#195080=CARTESIAN_POINT('',(125.332287942951,1.05,51.1814736770122));
#195081=CARTESIAN_POINT('',(125.389530916821,1.05,50.8869855754825));
#195082=CARTESIAN_POINT('',(124.841474440402,1.05,51.0860687205629));
#195083=CARTESIAN_POINT('',(124.841474440402,1.05,51.0860687205629));
#195084=CARTESIAN_POINT('',(124.898717414272,1.05,50.7915806190332));
#195085=CARTESIAN_POINT('',(124.898717414272,1.05,50.7915806190332));
#195086=CARTESIAN_POINT('',(124.898717414272,1.05,50.7915806190332));
#195087=CARTESIAN_POINT('Origin',(125.389530916821,1.05,50.8869855754825));
#195088=CARTESIAN_POINT('',(125.389530916821,0.550000000000015,50.8869855754825));
#195089=CARTESIAN_POINT('',(125.332287942951,0.550000000000015,51.1814736770122));
#195090=CARTESIAN_POINT('',(125.389530916821,0.550000000000015,50.8869855754825));
#195091=CARTESIAN_POINT('',(125.332287942951,1.05,51.1814736770122));
#195092=CARTESIAN_POINT('',(125.389530916821,1.05,50.8869855754825));
#195093=CARTESIAN_POINT('Origin',(125.389530916821,0.550000000000015,50.8869855754825));
#195094=CARTESIAN_POINT('',(124.898717414272,0.550000000000015,50.7915806190332));
#195095=CARTESIAN_POINT('',(124.841474440402,0.550000000000015,51.0860687205629));
#195096=CARTESIAN_POINT('',(124.898717414272,0.550000000000015,50.7915806190332));
#195097=CARTESIAN_POINT('',(125.332287942951,0.550000000000015,51.1814736770122));
#195098=CARTESIAN_POINT('',(125.389530916821,0.550000000000015,50.8869855754825));
#195099=CARTESIAN_POINT('Origin',(124.898717414272,0.550000000000015,50.7915806190332));
#195100=CARTESIAN_POINT('',(124.841474440402,0.550000000000015,51.0860687205629));
#195101=CARTESIAN_POINT('',(124.898717414272,0.550000000000015,50.7915806190332));
#195102=CARTESIAN_POINT('Origin',(124.898717414272,1.85,50.7915806190332));
#195103=CARTESIAN_POINT('',(125.389530916821,1.85,50.8869855754825));
#195104=CARTESIAN_POINT('',(125.332287942951,1.85,51.1814736770122));
#195105=CARTESIAN_POINT('',(125.389530916821,1.85,50.8869855754825));
#195106=CARTESIAN_POINT('',(124.841474440402,1.85,51.0860687205629));
#195107=CARTESIAN_POINT('',(124.841474440402,1.85,51.0860687205629));
#195108=CARTESIAN_POINT('',(124.898717414272,1.85,50.7915806190332));
#195109=CARTESIAN_POINT('',(124.898717414272,1.85,50.7915806190332));
#195110=CARTESIAN_POINT('',(124.898717414272,1.85,50.7915806190332));
#195111=CARTESIAN_POINT('Origin',(125.389530916821,1.85,50.8869855754825));
#195112=CARTESIAN_POINT('',(125.389530916821,1.35,50.8869855754825));
#195113=CARTESIAN_POINT('',(125.332287942951,1.35,51.1814736770122));
#195114=CARTESIAN_POINT('',(125.389530916821,1.35,50.8869855754825));
#195115=CARTESIAN_POINT('',(125.332287942951,1.85,51.1814736770122));
#195116=CARTESIAN_POINT('',(125.389530916821,1.85,50.8869855754825));
#195117=CARTESIAN_POINT('Origin',(125.389530916821,1.35,50.8869855754825));
#195118=CARTESIAN_POINT('',(124.898717414272,1.35,50.7915806190332));
#195119=CARTESIAN_POINT('',(124.841474440402,1.35,51.0860687205629));
#195120=CARTESIAN_POINT('',(124.898717414272,1.35,50.7915806190332));
#195121=CARTESIAN_POINT('',(125.332287942951,1.35,51.1814736770122));
#195122=CARTESIAN_POINT('',(125.389530916821,1.35,50.8869855754825));
#195123=CARTESIAN_POINT('Origin',(124.898717414272,1.35,50.7915806190332));
#195124=CARTESIAN_POINT('',(124.841474440402,1.35,51.0860687205629));
#195125=CARTESIAN_POINT('',(124.898717414272,1.35,50.7915806190332));
#195126=CARTESIAN_POINT('Origin',(124.898717414272,2.65,50.7915806190332));
#195127=CARTESIAN_POINT('',(125.389530916821,2.65,50.8869855754825));
#195128=CARTESIAN_POINT('',(125.332287942951,2.65,51.1814736770122));
#195129=CARTESIAN_POINT('',(125.389530916821,2.65,50.8869855754825));
#195130=CARTESIAN_POINT('',(124.841474440402,2.65,51.0860687205629));
#195131=CARTESIAN_POINT('',(124.841474440402,2.65,51.0860687205629));
#195132=CARTESIAN_POINT('',(124.898717414272,2.65,50.7915806190332));
#195133=CARTESIAN_POINT('',(124.898717414272,2.65,50.7915806190332));
#195134=CARTESIAN_POINT('',(124.898717414272,2.65,50.7915806190332));
#195135=CARTESIAN_POINT('Origin',(125.389530916821,2.65,50.8869855754825));
#195136=CARTESIAN_POINT('',(125.389530916821,2.15,50.8869855754825));
#195137=CARTESIAN_POINT('',(125.332287942951,2.15,51.1814736770122));
#195138=CARTESIAN_POINT('',(125.389530916821,2.15,50.8869855754825));
#195139=CARTESIAN_POINT('',(125.332287942951,2.65,51.1814736770122));
#195140=CARTESIAN_POINT('',(125.389530916821,2.65,50.8869855754825));
#195141=CARTESIAN_POINT('Origin',(125.389530916821,2.15,50.8869855754825));
#195142=CARTESIAN_POINT('',(124.898717414272,2.15,50.7915806190332));
#195143=CARTESIAN_POINT('',(124.841474440402,2.15,51.0860687205629));
#195144=CARTESIAN_POINT('',(124.898717414272,2.15,50.7915806190332));
#195145=CARTESIAN_POINT('',(125.332287942951,2.15,51.1814736770122));
#195146=CARTESIAN_POINT('',(125.389530916821,2.15,50.8869855754825));
#195147=CARTESIAN_POINT('Origin',(124.898717414272,2.15,50.7915806190332));
#195148=CARTESIAN_POINT('',(124.841474440402,2.15,51.0860687205629));
#195149=CARTESIAN_POINT('',(124.898717414272,2.15,50.7915806190332));
#195150=CARTESIAN_POINT('Origin',(124.898717414272,3.45,50.7915806190332));
#195151=CARTESIAN_POINT('',(125.389530916821,3.45,50.8869855754825));
#195152=CARTESIAN_POINT('',(125.332287942951,3.45,51.1814736770122));
#195153=CARTESIAN_POINT('',(125.389530916821,3.45,50.8869855754825));
#195154=CARTESIAN_POINT('',(124.841474440402,3.45,51.0860687205629));
#195155=CARTESIAN_POINT('',(124.841474440402,3.45,51.0860687205629));
#195156=CARTESIAN_POINT('',(124.898717414272,3.45,50.7915806190332));
#195157=CARTESIAN_POINT('',(124.898717414272,3.45,50.7915806190332));
#195158=CARTESIAN_POINT('',(124.898717414272,3.45,50.7915806190332));
#195159=CARTESIAN_POINT('Origin',(125.389530916821,3.45,50.8869855754825));
#195160=CARTESIAN_POINT('',(125.389530916821,2.95,50.8869855754825));
#195161=CARTESIAN_POINT('',(125.332287942951,2.95,51.1814736770122));
#195162=CARTESIAN_POINT('',(125.389530916821,2.95,50.8869855754825));
#195163=CARTESIAN_POINT('',(125.332287942951,3.45,51.1814736770122));
#195164=CARTESIAN_POINT('',(125.389530916821,3.45,50.8869855754825));
#195165=CARTESIAN_POINT('Origin',(125.389530916821,2.95,50.8869855754825));
#195166=CARTESIAN_POINT('',(124.898717414272,2.95,50.7915806190332));
#195167=CARTESIAN_POINT('',(124.841474440402,2.95,51.0860687205629));
#195168=CARTESIAN_POINT('',(124.898717414272,2.95,50.7915806190332));
#195169=CARTESIAN_POINT('',(125.332287942951,2.95,51.1814736770122));
#195170=CARTESIAN_POINT('',(125.389530916821,2.95,50.8869855754825));
#195171=CARTESIAN_POINT('Origin',(124.898717414272,2.95,50.7915806190332));
#195172=CARTESIAN_POINT('',(124.841474440402,2.95,51.0860687205629));
#195173=CARTESIAN_POINT('',(124.898717414272,2.95,50.7915806190332));
#195174=CARTESIAN_POINT('Origin',(124.898717414272,4.25,50.7915806190332));
#195175=CARTESIAN_POINT('',(125.389530916821,4.25,50.8869855754825));
#195176=CARTESIAN_POINT('',(125.332287942951,4.25,51.1814736770122));
#195177=CARTESIAN_POINT('',(125.389530916821,4.25,50.8869855754825));
#195178=CARTESIAN_POINT('',(124.841474440402,4.25,51.0860687205629));
#195179=CARTESIAN_POINT('',(124.841474440402,4.25,51.0860687205629));
#195180=CARTESIAN_POINT('',(124.898717414272,4.25,50.7915806190332));
#195181=CARTESIAN_POINT('',(124.898717414272,4.25,50.7915806190332));
#195182=CARTESIAN_POINT('',(124.898717414272,4.25,50.7915806190332));
#195183=CARTESIAN_POINT('Origin',(125.389530916821,4.25,50.8869855754825));
#195184=CARTESIAN_POINT('',(125.389530916821,3.75,50.8869855754825));
#195185=CARTESIAN_POINT('',(125.332287942951,3.75,51.1814736770122));
#195186=CARTESIAN_POINT('',(125.389530916821,3.75,50.8869855754825));
#195187=CARTESIAN_POINT('',(125.332287942951,4.25,51.1814736770122));
#195188=CARTESIAN_POINT('',(125.389530916821,4.25,50.8869855754825));
#195189=CARTESIAN_POINT('Origin',(125.389530916821,3.75,50.8869855754825));
#195190=CARTESIAN_POINT('',(124.898717414272,3.75,50.7915806190332));
#195191=CARTESIAN_POINT('',(124.841474440402,3.75,51.0860687205629));
#195192=CARTESIAN_POINT('',(124.898717414272,3.75,50.7915806190332));
#195193=CARTESIAN_POINT('',(125.332287942951,3.75,51.1814736770122));
#195194=CARTESIAN_POINT('',(125.389530916821,3.75,50.8869855754825));
#195195=CARTESIAN_POINT('Origin',(124.898717414272,3.75,50.7915806190332));
#195196=CARTESIAN_POINT('',(124.841474440402,3.75,51.0860687205629));
#195197=CARTESIAN_POINT('',(124.898717414272,3.75,50.7915806190332));
#195198=CARTESIAN_POINT('Origin',(124.898717414272,5.05,50.7915806190332));
#195199=CARTESIAN_POINT('',(125.389530916821,5.05,50.8869855754825));
#195200=CARTESIAN_POINT('',(125.332287942951,5.05,51.1814736770122));
#195201=CARTESIAN_POINT('',(125.389530916821,5.05,50.8869855754825));
#195202=CARTESIAN_POINT('',(124.841474440402,5.05,51.0860687205629));
#195203=CARTESIAN_POINT('',(124.841474440402,5.05,51.0860687205629));
#195204=CARTESIAN_POINT('',(124.898717414272,5.05,50.7915806190332));
#195205=CARTESIAN_POINT('',(124.898717414272,5.05,50.7915806190332));
#195206=CARTESIAN_POINT('',(124.898717414272,5.05,50.7915806190332));
#195207=CARTESIAN_POINT('Origin',(125.389530916821,5.05,50.8869855754825));
#195208=CARTESIAN_POINT('',(125.389530916821,4.55,50.8869855754825));
#195209=CARTESIAN_POINT('',(125.332287942951,4.55,51.1814736770122));
#195210=CARTESIAN_POINT('',(125.389530916821,4.55,50.8869855754825));
#195211=CARTESIAN_POINT('',(125.332287942951,5.05,51.1814736770122));
#195212=CARTESIAN_POINT('',(125.389530916821,5.05,50.8869855754825));
#195213=CARTESIAN_POINT('Origin',(125.389530916821,4.55,50.8869855754825));
#195214=CARTESIAN_POINT('',(124.898717414272,4.55,50.7915806190332));
#195215=CARTESIAN_POINT('',(124.841474440402,4.55,51.0860687205629));
#195216=CARTESIAN_POINT('',(124.898717414272,4.55,50.7915806190332));
#195217=CARTESIAN_POINT('',(125.332287942951,4.55,51.1814736770122));
#195218=CARTESIAN_POINT('',(125.389530916821,4.55,50.8869855754825));
#195219=CARTESIAN_POINT('Origin',(124.898717414272,4.55,50.7915806190332));
#195220=CARTESIAN_POINT('',(124.841474440402,4.55,51.0860687205629));
#195221=CARTESIAN_POINT('',(124.898717414272,4.55,50.7915806190332));
#195222=CARTESIAN_POINT('Origin',(121.757510997955,8.25,50.180988897758));
#195223=CARTESIAN_POINT('',(122.248324500504,8.25,50.2763938542073));
#195224=CARTESIAN_POINT('',(122.191081526635,8.25,50.570881955737));
#195225=CARTESIAN_POINT('',(122.248324500504,8.25,50.2763938542073));
#195226=CARTESIAN_POINT('',(121.700268024085,8.25,50.4754769992877));
#195227=CARTESIAN_POINT('',(121.700268024085,8.25,50.4754769992877));
#195228=CARTESIAN_POINT('',(121.757510997955,8.25,50.180988897758));
#195229=CARTESIAN_POINT('',(121.757510997955,8.25,50.180988897758));
#195230=CARTESIAN_POINT('',(121.757510997955,8.25,50.180988897758));
#195231=CARTESIAN_POINT('Origin',(122.248324500504,8.25,50.2763938542073));
#195232=CARTESIAN_POINT('',(122.248324500504,7.75,50.2763938542073));
#195233=CARTESIAN_POINT('',(122.191081526635,7.75,50.570881955737));
#195234=CARTESIAN_POINT('',(122.248324500504,7.75,50.2763938542073));
#195235=CARTESIAN_POINT('',(122.191081526635,8.25,50.570881955737));
#195236=CARTESIAN_POINT('',(122.248324500504,8.25,50.2763938542073));
#195237=CARTESIAN_POINT('Origin',(122.248324500504,7.75,50.2763938542073));
#195238=CARTESIAN_POINT('',(121.757510997955,7.75,50.180988897758));
#195239=CARTESIAN_POINT('',(121.700268024085,7.75,50.4754769992877));
#195240=CARTESIAN_POINT('',(121.757510997955,7.75,50.180988897758));
#195241=CARTESIAN_POINT('',(122.191081526635,7.75,50.570881955737));
#195242=CARTESIAN_POINT('',(122.248324500504,7.75,50.2763938542073));
#195243=CARTESIAN_POINT('Origin',(121.757510997955,7.75,50.180988897758));
#195244=CARTESIAN_POINT('',(121.700268024085,7.75,50.4754769992877));
#195245=CARTESIAN_POINT('',(121.757510997955,7.75,50.180988897758));
#195246=CARTESIAN_POINT('Origin',(120.972209393875,8.25,50.0283409674392));
#195247=CARTESIAN_POINT('',(121.463022896425,8.25,50.1237459238885));
#195248=CARTESIAN_POINT('',(121.405779922555,8.25,50.4182340254182));
#195249=CARTESIAN_POINT('',(121.463022896425,8.25,50.1237459238885));
#195250=CARTESIAN_POINT('',(120.914966420006,8.25,50.3228290689689));
#195251=CARTESIAN_POINT('',(120.914966420006,8.25,50.3228290689689));
#195252=CARTESIAN_POINT('',(120.972209393875,8.25,50.0283409674392));
#195253=CARTESIAN_POINT('',(120.972209393875,8.25,50.0283409674392));
#195254=CARTESIAN_POINT('',(120.972209393875,8.25,50.0283409674392));
#195255=CARTESIAN_POINT('Origin',(121.463022896425,8.25,50.1237459238885));
#195256=CARTESIAN_POINT('',(121.463022896425,7.75,50.1237459238885));
#195257=CARTESIAN_POINT('',(121.405779922555,7.75,50.4182340254182));
#195258=CARTESIAN_POINT('',(121.463022896425,7.75,50.1237459238885));
#195259=CARTESIAN_POINT('',(121.405779922555,8.25,50.4182340254182));
#195260=CARTESIAN_POINT('',(121.463022896425,8.25,50.1237459238885));
#195261=CARTESIAN_POINT('Origin',(121.463022896425,7.75,50.1237459238885));
#195262=CARTESIAN_POINT('',(120.972209393875,7.75,50.0283409674392));
#195263=CARTESIAN_POINT('',(120.914966420006,7.75,50.3228290689689));
#195264=CARTESIAN_POINT('',(120.972209393875,7.75,50.0283409674392));
#195265=CARTESIAN_POINT('',(121.405779922555,7.75,50.4182340254182));
#195266=CARTESIAN_POINT('',(121.463022896425,7.75,50.1237459238885));
#195267=CARTESIAN_POINT('Origin',(120.972209393875,7.75,50.0283409674392));
#195268=CARTESIAN_POINT('',(120.914966420006,7.75,50.3228290689689));
#195269=CARTESIAN_POINT('',(120.972209393875,7.75,50.0283409674392));
#195270=CARTESIAN_POINT('Origin',(120.186907789796,8.25,49.8756930371204));
#195271=CARTESIAN_POINT('',(120.677721292346,8.25,49.9710979935697));
#195272=CARTESIAN_POINT('',(120.620478318476,8.25,50.2655860950994));
#195273=CARTESIAN_POINT('',(120.677721292346,8.25,49.9710979935697));
#195274=CARTESIAN_POINT('',(120.129664815927,8.25,50.1701811386501));
#195275=CARTESIAN_POINT('',(120.129664815927,8.25,50.1701811386501));
#195276=CARTESIAN_POINT('',(120.186907789796,8.25,49.8756930371204));
#195277=CARTESIAN_POINT('',(120.186907789796,8.25,49.8756930371204));
#195278=CARTESIAN_POINT('',(120.186907789796,8.25,49.8756930371204));
#195279=CARTESIAN_POINT('Origin',(120.677721292346,8.25,49.9710979935697));
#195280=CARTESIAN_POINT('',(120.677721292346,7.75,49.9710979935697));
#195281=CARTESIAN_POINT('',(120.620478318476,7.75,50.2655860950994));
#195282=CARTESIAN_POINT('',(120.677721292346,7.75,49.9710979935697));
#195283=CARTESIAN_POINT('',(120.620478318476,8.25,50.2655860950994));
#195284=CARTESIAN_POINT('',(120.677721292346,8.25,49.9710979935697));
#195285=CARTESIAN_POINT('Origin',(120.677721292346,7.75,49.9710979935697));
#195286=CARTESIAN_POINT('',(120.186907789796,7.75,49.8756930371204));
#195287=CARTESIAN_POINT('',(120.129664815927,7.75,50.1701811386501));
#195288=CARTESIAN_POINT('',(120.186907789796,7.75,49.8756930371204));
#195289=CARTESIAN_POINT('',(120.620478318476,7.75,50.2655860950994));
#195290=CARTESIAN_POINT('',(120.677721292346,7.75,49.9710979935697));
#195291=CARTESIAN_POINT('Origin',(120.186907789796,7.75,49.8756930371204));
#195292=CARTESIAN_POINT('',(120.129664815927,7.75,50.1701811386501));
#195293=CARTESIAN_POINT('',(120.186907789796,7.75,49.8756930371204));
#195294=CARTESIAN_POINT('Origin',(119.401606185717,8.25,49.7230451068016));
#195295=CARTESIAN_POINT('',(119.892419688267,8.25,49.8184500632509));
#195296=CARTESIAN_POINT('',(119.835176714397,8.25,50.1129381647806));
#195297=CARTESIAN_POINT('',(119.892419688267,8.25,49.8184500632509));
#195298=CARTESIAN_POINT('',(119.344363211847,8.25,50.0175332083313));
#195299=CARTESIAN_POINT('',(119.344363211847,8.25,50.0175332083313));
#195300=CARTESIAN_POINT('',(119.401606185717,8.25,49.7230451068016));
#195301=CARTESIAN_POINT('',(119.401606185717,8.25,49.7230451068016));
#195302=CARTESIAN_POINT('',(119.401606185717,8.25,49.7230451068016));
#195303=CARTESIAN_POINT('Origin',(119.892419688267,8.25,49.8184500632509));
#195304=CARTESIAN_POINT('',(119.892419688267,7.75,49.8184500632509));
#195305=CARTESIAN_POINT('',(119.835176714397,7.75,50.1129381647806));
#195306=CARTESIAN_POINT('',(119.892419688267,7.75,49.8184500632509));
#195307=CARTESIAN_POINT('',(119.835176714397,8.25,50.1129381647806));
#195308=CARTESIAN_POINT('',(119.892419688267,8.25,49.8184500632509));
#195309=CARTESIAN_POINT('Origin',(119.892419688267,7.75,49.8184500632509));
#195310=CARTESIAN_POINT('',(119.401606185717,7.75,49.7230451068016));
#195311=CARTESIAN_POINT('',(119.344363211847,7.75,50.0175332083313));
#195312=CARTESIAN_POINT('',(119.401606185717,7.75,49.7230451068016));
#195313=CARTESIAN_POINT('',(119.835176714397,7.75,50.1129381647806));
#195314=CARTESIAN_POINT('',(119.892419688267,7.75,49.8184500632509));
#195315=CARTESIAN_POINT('Origin',(119.401606185717,7.75,49.7230451068016));
#195316=CARTESIAN_POINT('',(119.344363211847,7.75,50.0175332083313));
#195317=CARTESIAN_POINT('',(119.401606185717,7.75,49.7230451068016));
#195318=CARTESIAN_POINT('Origin',(118.616304581638,8.25,49.5703971764828));
#195319=CARTESIAN_POINT('',(119.107118084187,8.25,49.6658021329321));
#195320=CARTESIAN_POINT('',(119.049875110318,8.25,49.9602902344618));
#195321=CARTESIAN_POINT('',(119.107118084187,8.25,49.6658021329321));
#195322=CARTESIAN_POINT('',(118.559061607768,8.25,49.8648852780125));
#195323=CARTESIAN_POINT('',(118.559061607768,8.25,49.8648852780125));
#195324=CARTESIAN_POINT('',(118.616304581638,8.25,49.5703971764828));
#195325=CARTESIAN_POINT('',(118.616304581638,8.25,49.5703971764828));
#195326=CARTESIAN_POINT('',(118.616304581638,8.25,49.5703971764828));
#195327=CARTESIAN_POINT('Origin',(119.107118084187,8.25,49.6658021329321));
#195328=CARTESIAN_POINT('',(119.107118084187,7.75,49.6658021329321));
#195329=CARTESIAN_POINT('',(119.049875110318,7.75,49.9602902344618));
#195330=CARTESIAN_POINT('',(119.107118084187,7.75,49.6658021329321));
#195331=CARTESIAN_POINT('',(119.049875110318,8.25,49.9602902344618));
#195332=CARTESIAN_POINT('',(119.107118084187,8.25,49.6658021329321));
#195333=CARTESIAN_POINT('Origin',(119.107118084187,7.75,49.6658021329321));
#195334=CARTESIAN_POINT('',(118.616304581638,7.75,49.5703971764828));
#195335=CARTESIAN_POINT('',(118.559061607768,7.75,49.8648852780125));
#195336=CARTESIAN_POINT('',(118.616304581638,7.75,49.5703971764828));
#195337=CARTESIAN_POINT('',(119.049875110318,7.75,49.9602902344618));
#195338=CARTESIAN_POINT('',(119.107118084187,7.75,49.6658021329321));
#195339=CARTESIAN_POINT('Origin',(118.616304581638,7.75,49.5703971764828));
#195340=CARTESIAN_POINT('',(118.559061607768,7.75,49.8648852780125));
#195341=CARTESIAN_POINT('',(118.616304581638,7.75,49.5703971764828));
#195342=CARTESIAN_POINT('Origin',(117.831002977559,8.25,49.417749246164));
#195343=CARTESIAN_POINT('',(118.321816480108,8.25,49.5131542026133));
#195344=CARTESIAN_POINT('',(118.264573506239,8.25,49.807642304143));
#195345=CARTESIAN_POINT('',(118.321816480108,8.25,49.5131542026133));
#195346=CARTESIAN_POINT('',(117.773760003689,8.25,49.7122373476937));
#195347=CARTESIAN_POINT('',(117.773760003689,8.25,49.7122373476937));
#195348=CARTESIAN_POINT('',(117.831002977559,8.25,49.417749246164));
#195349=CARTESIAN_POINT('',(117.831002977559,8.25,49.417749246164));
#195350=CARTESIAN_POINT('',(117.831002977559,8.25,49.417749246164));
#195351=CARTESIAN_POINT('Origin',(118.321816480108,8.25,49.5131542026133));
#195352=CARTESIAN_POINT('',(118.321816480108,7.75,49.5131542026133));
#195353=CARTESIAN_POINT('',(118.264573506239,7.75,49.807642304143));
#195354=CARTESIAN_POINT('',(118.321816480108,7.75,49.5131542026133));
#195355=CARTESIAN_POINT('',(118.264573506239,8.25,49.807642304143));
#195356=CARTESIAN_POINT('',(118.321816480108,8.25,49.5131542026133));
#195357=CARTESIAN_POINT('Origin',(118.321816480108,7.75,49.5131542026133));
#195358=CARTESIAN_POINT('',(117.831002977559,7.75,49.417749246164));
#195359=CARTESIAN_POINT('',(117.773760003689,7.75,49.7122373476937));
#195360=CARTESIAN_POINT('',(117.831002977559,7.75,49.417749246164));
#195361=CARTESIAN_POINT('',(118.264573506239,7.75,49.807642304143));
#195362=CARTESIAN_POINT('',(118.321816480108,7.75,49.5131542026133));
#195363=CARTESIAN_POINT('Origin',(117.831002977559,7.75,49.417749246164));
#195364=CARTESIAN_POINT('',(117.773760003689,7.75,49.7122373476937));
#195365=CARTESIAN_POINT('',(117.831002977559,7.75,49.417749246164));
#195366=CARTESIAN_POINT('Origin',(117.045701373479,8.25,49.2651013158452));
#195367=CARTESIAN_POINT('',(117.536514876029,8.25,49.3605062722945));
#195368=CARTESIAN_POINT('',(117.479271902159,8.25,49.6549943738242));
#195369=CARTESIAN_POINT('',(117.536514876029,8.25,49.3605062722945));
#195370=CARTESIAN_POINT('',(116.98845839961,8.25,49.5595894173749));
#195371=CARTESIAN_POINT('',(116.98845839961,8.25,49.5595894173749));
#195372=CARTESIAN_POINT('',(117.045701373479,8.25,49.2651013158452));
#195373=CARTESIAN_POINT('',(117.045701373479,8.25,49.2651013158452));
#195374=CARTESIAN_POINT('',(117.045701373479,8.25,49.2651013158452));
#195375=CARTESIAN_POINT('Origin',(117.536514876029,8.25,49.3605062722945));
#195376=CARTESIAN_POINT('',(117.536514876029,7.75,49.3605062722945));
#195377=CARTESIAN_POINT('',(117.479271902159,7.75,49.6549943738242));
#195378=CARTESIAN_POINT('',(117.536514876029,7.75,49.3605062722945));
#195379=CARTESIAN_POINT('',(117.479271902159,8.25,49.6549943738242));
#195380=CARTESIAN_POINT('',(117.536514876029,8.25,49.3605062722945));
#195381=CARTESIAN_POINT('Origin',(117.536514876029,7.75,49.3605062722945));
#195382=CARTESIAN_POINT('',(117.045701373479,7.75,49.2651013158452));
#195383=CARTESIAN_POINT('',(116.98845839961,7.75,49.5595894173749));
#195384=CARTESIAN_POINT('',(117.045701373479,7.75,49.2651013158452));
#195385=CARTESIAN_POINT('',(117.479271902159,7.75,49.6549943738242));
#195386=CARTESIAN_POINT('',(117.536514876029,7.75,49.3605062722945));
#195387=CARTESIAN_POINT('Origin',(117.045701373479,7.75,49.2651013158452));
#195388=CARTESIAN_POINT('',(116.98845839961,7.75,49.5595894173749));
#195389=CARTESIAN_POINT('',(117.045701373479,7.75,49.2651013158452));
#195390=CARTESIAN_POINT('Origin',(116.2603997694,8.25,49.1124533855264));
#195391=CARTESIAN_POINT('',(116.75121327195,8.25,49.2078583419757));
#195392=CARTESIAN_POINT('',(116.69397029808,8.25,49.5023464435054));
#195393=CARTESIAN_POINT('',(116.75121327195,8.25,49.2078583419757));
#195394=CARTESIAN_POINT('',(116.203156795531,8.25,49.4069414870561));
#195395=CARTESIAN_POINT('',(116.203156795531,8.25,49.4069414870561));
#195396=CARTESIAN_POINT('',(116.2603997694,8.25,49.1124533855264));
#195397=CARTESIAN_POINT('',(116.2603997694,8.25,49.1124533855264));
#195398=CARTESIAN_POINT('',(116.2603997694,8.25,49.1124533855264));
#195399=CARTESIAN_POINT('Origin',(116.75121327195,8.25,49.2078583419757));
#195400=CARTESIAN_POINT('',(116.75121327195,7.75,49.2078583419757));
#195401=CARTESIAN_POINT('',(116.69397029808,7.75,49.5023464435054));
#195402=CARTESIAN_POINT('',(116.75121327195,7.75,49.2078583419757));
#195403=CARTESIAN_POINT('',(116.69397029808,8.25,49.5023464435054));
#195404=CARTESIAN_POINT('',(116.75121327195,8.25,49.2078583419757));
#195405=CARTESIAN_POINT('Origin',(116.75121327195,7.75,49.2078583419757));
#195406=CARTESIAN_POINT('',(116.2603997694,7.75,49.1124533855264));
#195407=CARTESIAN_POINT('',(116.203156795531,7.75,49.4069414870561));
#195408=CARTESIAN_POINT('',(116.2603997694,7.75,49.1124533855264));
#195409=CARTESIAN_POINT('',(116.69397029808,7.75,49.5023464435054));
#195410=CARTESIAN_POINT('',(116.75121327195,7.75,49.2078583419757));
#195411=CARTESIAN_POINT('Origin',(116.2603997694,7.75,49.1124533855264));
#195412=CARTESIAN_POINT('',(116.203156795531,7.75,49.4069414870561));
#195413=CARTESIAN_POINT('',(116.2603997694,7.75,49.1124533855264));
#195414=CARTESIAN_POINT('Origin',(115.475098165321,8.25,48.9598054552076));
#195415=CARTESIAN_POINT('',(115.96591166787,8.25,49.0552104116569));
#195416=CARTESIAN_POINT('',(115.908668694001,8.25,49.3496985131866));
#195417=CARTESIAN_POINT('',(115.96591166787,8.25,49.0552104116569));
#195418=CARTESIAN_POINT('',(115.417855191451,8.25,49.2542935567373));
#195419=CARTESIAN_POINT('',(115.417855191451,8.25,49.2542935567373));
#195420=CARTESIAN_POINT('',(115.475098165321,8.25,48.9598054552076));
#195421=CARTESIAN_POINT('',(115.475098165321,8.25,48.9598054552076));
#195422=CARTESIAN_POINT('',(115.475098165321,8.25,48.9598054552076));
#195423=CARTESIAN_POINT('Origin',(115.96591166787,8.25,49.0552104116569));
#195424=CARTESIAN_POINT('',(115.96591166787,7.75,49.0552104116569));
#195425=CARTESIAN_POINT('',(115.908668694001,7.75,49.3496985131866));
#195426=CARTESIAN_POINT('',(115.96591166787,7.75,49.0552104116569));
#195427=CARTESIAN_POINT('',(115.908668694001,8.25,49.3496985131866));
#195428=CARTESIAN_POINT('',(115.96591166787,8.25,49.0552104116569));
#195429=CARTESIAN_POINT('Origin',(115.96591166787,7.75,49.0552104116569));
#195430=CARTESIAN_POINT('',(115.475098165321,7.75,48.9598054552076));
#195431=CARTESIAN_POINT('',(115.417855191451,7.75,49.2542935567373));
#195432=CARTESIAN_POINT('',(115.475098165321,7.75,48.9598054552076));
#195433=CARTESIAN_POINT('',(115.908668694001,7.75,49.3496985131866));
#195434=CARTESIAN_POINT('',(115.96591166787,7.75,49.0552104116569));
#195435=CARTESIAN_POINT('Origin',(115.475098165321,7.75,48.9598054552076));
#195436=CARTESIAN_POINT('',(115.417855191451,7.75,49.2542935567373));
#195437=CARTESIAN_POINT('',(115.475098165321,7.75,48.9598054552076));
#195438=CARTESIAN_POINT('Origin',(114.689796561242,8.25,48.8071575248888));
#195439=CARTESIAN_POINT('',(115.180610063791,8.25,48.9025624813381));
#195440=CARTESIAN_POINT('',(115.123367089922,8.25,49.1970505828678));
#195441=CARTESIAN_POINT('',(115.180610063791,8.25,48.9025624813381));
#195442=CARTESIAN_POINT('',(114.632553587372,8.25,49.1016456264185));
#195443=CARTESIAN_POINT('',(114.632553587372,8.25,49.1016456264185));
#195444=CARTESIAN_POINT('',(114.689796561242,8.25,48.8071575248888));
#195445=CARTESIAN_POINT('',(114.689796561242,8.25,48.8071575248888));
#195446=CARTESIAN_POINT('',(114.689796561242,8.25,48.8071575248888));
#195447=CARTESIAN_POINT('Origin',(115.180610063791,8.25,48.9025624813381));
#195448=CARTESIAN_POINT('',(115.180610063791,7.75,48.9025624813381));
#195449=CARTESIAN_POINT('',(115.123367089922,7.75,49.1970505828678));
#195450=CARTESIAN_POINT('',(115.180610063791,7.75,48.9025624813381));
#195451=CARTESIAN_POINT('',(115.123367089922,8.25,49.1970505828678));
#195452=CARTESIAN_POINT('',(115.180610063791,8.25,48.9025624813381));
#195453=CARTESIAN_POINT('Origin',(115.180610063791,7.75,48.9025624813381));
#195454=CARTESIAN_POINT('',(114.689796561242,7.75,48.8071575248888));
#195455=CARTESIAN_POINT('',(114.632553587372,7.75,49.1016456264185));
#195456=CARTESIAN_POINT('',(114.689796561242,7.75,48.8071575248888));
#195457=CARTESIAN_POINT('',(115.123367089922,7.75,49.1970505828678));
#195458=CARTESIAN_POINT('',(115.180610063791,7.75,48.9025624813381));
#195459=CARTESIAN_POINT('Origin',(114.689796561242,7.75,48.8071575248888));
#195460=CARTESIAN_POINT('',(114.632553587372,7.75,49.1016456264185));
#195461=CARTESIAN_POINT('',(114.689796561242,7.75,48.8071575248888));
#195462=CARTESIAN_POINT('Origin',(113.904494957163,8.25,48.65450959457));
#195463=CARTESIAN_POINT('',(114.395308459712,8.25,48.7499145510193));
#195464=CARTESIAN_POINT('',(114.338065485842,8.25,49.044402652549));
#195465=CARTESIAN_POINT('',(114.395308459712,8.25,48.7499145510193));
#195466=CARTESIAN_POINT('',(113.847251983293,8.25,48.9489976960997));
#195467=CARTESIAN_POINT('',(113.847251983293,8.25,48.9489976960997));
#195468=CARTESIAN_POINT('',(113.904494957163,8.25,48.65450959457));
#195469=CARTESIAN_POINT('',(113.904494957163,8.25,48.65450959457));
#195470=CARTESIAN_POINT('',(113.904494957163,8.25,48.65450959457));
#195471=CARTESIAN_POINT('Origin',(114.395308459712,8.25,48.7499145510193));
#195472=CARTESIAN_POINT('',(114.395308459712,7.75,48.7499145510193));
#195473=CARTESIAN_POINT('',(114.338065485842,7.75,49.044402652549));
#195474=CARTESIAN_POINT('',(114.395308459712,7.75,48.7499145510193));
#195475=CARTESIAN_POINT('',(114.338065485842,8.25,49.044402652549));
#195476=CARTESIAN_POINT('',(114.395308459712,8.25,48.7499145510193));
#195477=CARTESIAN_POINT('Origin',(114.395308459712,7.75,48.7499145510193));
#195478=CARTESIAN_POINT('',(113.904494957163,7.75,48.65450959457));
#195479=CARTESIAN_POINT('',(113.847251983293,7.75,48.9489976960997));
#195480=CARTESIAN_POINT('',(113.904494957163,7.75,48.65450959457));
#195481=CARTESIAN_POINT('',(114.338065485842,7.75,49.044402652549));
#195482=CARTESIAN_POINT('',(114.395308459712,7.75,48.7499145510193));
#195483=CARTESIAN_POINT('Origin',(113.904494957163,7.75,48.65450959457));
#195484=CARTESIAN_POINT('',(113.847251983293,7.75,48.9489976960997));
#195485=CARTESIAN_POINT('',(113.904494957163,7.75,48.65450959457));
#195486=CARTESIAN_POINT('Origin',(113.119193353083,8.25,48.5018616642512));
#195487=CARTESIAN_POINT('',(113.610006855633,8.25,48.5972666207005));
#195488=CARTESIAN_POINT('',(113.552763881763,8.25,48.8917547222302));
#195489=CARTESIAN_POINT('',(113.610006855633,8.25,48.5972666207005));
#195490=CARTESIAN_POINT('',(113.061950379214,8.25,48.7963497657809));
#195491=CARTESIAN_POINT('',(113.061950379214,8.25,48.7963497657809));
#195492=CARTESIAN_POINT('',(113.119193353083,8.25,48.5018616642512));
#195493=CARTESIAN_POINT('',(113.119193353083,8.25,48.5018616642512));
#195494=CARTESIAN_POINT('',(113.119193353083,8.25,48.5018616642512));
#195495=CARTESIAN_POINT('Origin',(113.610006855633,8.25,48.5972666207005));
#195496=CARTESIAN_POINT('',(113.610006855633,7.75,48.5972666207005));
#195497=CARTESIAN_POINT('',(113.552763881763,7.75,48.8917547222302));
#195498=CARTESIAN_POINT('',(113.610006855633,7.75,48.5972666207005));
#195499=CARTESIAN_POINT('',(113.552763881763,8.25,48.8917547222302));
#195500=CARTESIAN_POINT('',(113.610006855633,8.25,48.5972666207005));
#195501=CARTESIAN_POINT('Origin',(113.610006855633,7.75,48.5972666207005));
#195502=CARTESIAN_POINT('',(113.119193353083,7.75,48.5018616642512));
#195503=CARTESIAN_POINT('',(113.061950379214,7.75,48.7963497657809));
#195504=CARTESIAN_POINT('',(113.119193353083,7.75,48.5018616642512));
#195505=CARTESIAN_POINT('',(113.552763881763,7.75,48.8917547222302));
#195506=CARTESIAN_POINT('',(113.610006855633,7.75,48.5972666207005));
#195507=CARTESIAN_POINT('Origin',(113.119193353083,7.75,48.5018616642512));
#195508=CARTESIAN_POINT('',(113.061950379214,7.75,48.7963497657809));
#195509=CARTESIAN_POINT('',(113.119193353083,7.75,48.5018616642512));
#195510=CARTESIAN_POINT('Origin',(112.333891749004,8.25,48.3492137339324));
#195511=CARTESIAN_POINT('',(112.824705251554,8.25,48.4446186903817));
#195512=CARTESIAN_POINT('',(112.767462277684,8.25,48.7391067919114));
#195513=CARTESIAN_POINT('',(112.824705251554,8.25,48.4446186903817));
#195514=CARTESIAN_POINT('',(112.276648775135,8.25,48.6437018354621));
#195515=CARTESIAN_POINT('',(112.276648775135,8.25,48.6437018354621));
#195516=CARTESIAN_POINT('',(112.333891749004,8.25,48.3492137339324));
#195517=CARTESIAN_POINT('',(112.333891749004,8.25,48.3492137339324));
#195518=CARTESIAN_POINT('',(112.333891749004,8.25,48.3492137339324));
#195519=CARTESIAN_POINT('Origin',(112.824705251554,8.25,48.4446186903817));
#195520=CARTESIAN_POINT('',(112.824705251554,7.75,48.4446186903817));
#195521=CARTESIAN_POINT('',(112.767462277684,7.75,48.7391067919114));
#195522=CARTESIAN_POINT('',(112.824705251554,7.75,48.4446186903817));
#195523=CARTESIAN_POINT('',(112.767462277684,8.25,48.7391067919114));
#195524=CARTESIAN_POINT('',(112.824705251554,8.25,48.4446186903817));
#195525=CARTESIAN_POINT('Origin',(112.824705251554,7.75,48.4446186903817));
#195526=CARTESIAN_POINT('',(112.333891749004,7.75,48.3492137339324));
#195527=CARTESIAN_POINT('',(112.276648775135,7.75,48.6437018354621));
#195528=CARTESIAN_POINT('',(112.333891749004,7.75,48.3492137339324));
#195529=CARTESIAN_POINT('',(112.767462277684,7.75,48.7391067919114));
#195530=CARTESIAN_POINT('',(112.824705251554,7.75,48.4446186903817));
#195531=CARTESIAN_POINT('Origin',(112.333891749004,7.75,48.3492137339324));
#195532=CARTESIAN_POINT('',(112.276648775135,7.75,48.6437018354621));
#195533=CARTESIAN_POINT('',(112.333891749004,7.75,48.3492137339324));
#195534=CARTESIAN_POINT('Origin',(109.977986936766,5.85,47.891269942976));
#195535=CARTESIAN_POINT('',(110.468800439316,5.85,47.9866748994252));
#195536=CARTESIAN_POINT('',(110.411557465446,5.85,48.2811630009549));
#195537=CARTESIAN_POINT('',(110.468800439316,5.85,47.9866748994252));
#195538=CARTESIAN_POINT('',(109.920743962897,5.85,48.1857580445057));
#195539=CARTESIAN_POINT('',(109.920743962897,5.85,48.1857580445057));
#195540=CARTESIAN_POINT('',(109.977986936766,5.85,47.891269942976));
#195541=CARTESIAN_POINT('',(109.977986936766,5.85,47.891269942976));
#195542=CARTESIAN_POINT('',(109.977986936766,5.85,47.891269942976));
#195543=CARTESIAN_POINT('Origin',(110.468800439316,5.85,47.9866748994252));
#195544=CARTESIAN_POINT('',(110.468800439316,5.35,47.9866748994252));
#195545=CARTESIAN_POINT('',(110.411557465446,5.35,48.2811630009549));
#195546=CARTESIAN_POINT('',(110.468800439316,5.35,47.9866748994252));
#195547=CARTESIAN_POINT('',(110.411557465446,5.85,48.2811630009549));
#195548=CARTESIAN_POINT('',(110.468800439316,5.85,47.9866748994252));
#195549=CARTESIAN_POINT('Origin',(110.468800439316,5.35,47.9866748994252));
#195550=CARTESIAN_POINT('',(109.977986936766,5.35,47.891269942976));
#195551=CARTESIAN_POINT('',(109.920743962897,5.35,48.1857580445057));
#195552=CARTESIAN_POINT('',(109.977986936766,5.35,47.891269942976));
#195553=CARTESIAN_POINT('',(110.411557465446,5.35,48.2811630009549));
#195554=CARTESIAN_POINT('',(110.468800439316,5.35,47.9866748994252));
#195555=CARTESIAN_POINT('Origin',(109.977986936766,5.35,47.891269942976));
#195556=CARTESIAN_POINT('',(109.920743962897,5.35,48.1857580445057));
#195557=CARTESIAN_POINT('',(109.977986936766,5.35,47.891269942976));
#195558=CARTESIAN_POINT('Origin',(109.977986936766,5.05,47.891269942976));
#195559=CARTESIAN_POINT('',(110.468800439316,5.05,47.9866748994252));
#195560=CARTESIAN_POINT('',(110.411557465446,5.05,48.2811630009549));
#195561=CARTESIAN_POINT('',(110.468800439316,5.05,47.9866748994252));
#195562=CARTESIAN_POINT('',(109.920743962897,5.05,48.1857580445057));
#195563=CARTESIAN_POINT('',(109.920743962897,5.05,48.1857580445057));
#195564=CARTESIAN_POINT('',(109.977986936766,5.05,47.891269942976));
#195565=CARTESIAN_POINT('',(109.977986936766,5.05,47.891269942976));
#195566=CARTESIAN_POINT('',(109.977986936766,5.05,47.891269942976));
#195567=CARTESIAN_POINT('Origin',(110.468800439316,5.05,47.9866748994252));
#195568=CARTESIAN_POINT('',(110.468800439316,4.55,47.9866748994252));
#195569=CARTESIAN_POINT('',(110.411557465446,4.55,48.2811630009549));
#195570=CARTESIAN_POINT('',(110.468800439316,4.55,47.9866748994252));
#195571=CARTESIAN_POINT('',(110.411557465446,5.05,48.2811630009549));
#195572=CARTESIAN_POINT('',(110.468800439316,5.05,47.9866748994252));
#195573=CARTESIAN_POINT('Origin',(110.468800439316,4.55,47.9866748994252));
#195574=CARTESIAN_POINT('',(109.977986936766,4.55,47.891269942976));
#195575=CARTESIAN_POINT('',(109.920743962897,4.55,48.1857580445057));
#195576=CARTESIAN_POINT('',(109.977986936766,4.55,47.891269942976));
#195577=CARTESIAN_POINT('',(110.411557465446,4.55,48.2811630009549));
#195578=CARTESIAN_POINT('',(110.468800439316,4.55,47.9866748994252));
#195579=CARTESIAN_POINT('Origin',(109.977986936766,4.55,47.891269942976));
#195580=CARTESIAN_POINT('',(109.920743962897,4.55,48.1857580445057));
#195581=CARTESIAN_POINT('',(109.977986936766,4.55,47.891269942976));
#195582=CARTESIAN_POINT('Origin',(109.977986936766,4.25,47.891269942976));
#195583=CARTESIAN_POINT('',(110.468800439316,4.25,47.9866748994252));
#195584=CARTESIAN_POINT('',(110.411557465446,4.25,48.2811630009549));
#195585=CARTESIAN_POINT('',(110.468800439316,4.25,47.9866748994252));
#195586=CARTESIAN_POINT('',(109.920743962897,4.25,48.1857580445057));
#195587=CARTESIAN_POINT('',(109.920743962897,4.25,48.1857580445057));
#195588=CARTESIAN_POINT('',(109.977986936766,4.25,47.891269942976));
#195589=CARTESIAN_POINT('',(109.977986936766,4.25,47.891269942976));
#195590=CARTESIAN_POINT('',(109.977986936766,4.25,47.891269942976));
#195591=CARTESIAN_POINT('Origin',(110.468800439316,4.25,47.9866748994252));
#195592=CARTESIAN_POINT('',(110.468800439316,3.75,47.9866748994252));
#195593=CARTESIAN_POINT('',(110.411557465446,3.75,48.2811630009549));
#195594=CARTESIAN_POINT('',(110.468800439316,3.75,47.9866748994252));
#195595=CARTESIAN_POINT('',(110.411557465446,4.25,48.2811630009549));
#195596=CARTESIAN_POINT('',(110.468800439316,4.25,47.9866748994252));
#195597=CARTESIAN_POINT('Origin',(110.468800439316,3.75,47.9866748994252));
#195598=CARTESIAN_POINT('',(109.977986936766,3.75,47.891269942976));
#195599=CARTESIAN_POINT('',(109.920743962897,3.75,48.1857580445057));
#195600=CARTESIAN_POINT('',(109.977986936766,3.75,47.891269942976));
#195601=CARTESIAN_POINT('',(110.411557465446,3.75,48.2811630009549));
#195602=CARTESIAN_POINT('',(110.468800439316,3.75,47.9866748994252));
#195603=CARTESIAN_POINT('Origin',(109.977986936766,3.75,47.891269942976));
#195604=CARTESIAN_POINT('',(109.920743962897,3.75,48.1857580445057));
#195605=CARTESIAN_POINT('',(109.977986936766,3.75,47.891269942976));
#195606=CARTESIAN_POINT('Origin',(109.977986936766,3.45,47.891269942976));
#195607=CARTESIAN_POINT('',(110.468800439316,3.45,47.9866748994252));
#195608=CARTESIAN_POINT('',(110.411557465446,3.45,48.2811630009549));
#195609=CARTESIAN_POINT('',(110.468800439316,3.45,47.9866748994252));
#195610=CARTESIAN_POINT('',(109.920743962897,3.45,48.1857580445057));
#195611=CARTESIAN_POINT('',(109.920743962897,3.45,48.1857580445057));
#195612=CARTESIAN_POINT('',(109.977986936766,3.45,47.891269942976));
#195613=CARTESIAN_POINT('',(109.977986936766,3.45,47.891269942976));
#195614=CARTESIAN_POINT('',(109.977986936766,3.45,47.891269942976));
#195615=CARTESIAN_POINT('Origin',(110.468800439316,3.45,47.9866748994252));
#195616=CARTESIAN_POINT('',(110.468800439316,2.95,47.9866748994252));
#195617=CARTESIAN_POINT('',(110.411557465446,2.95,48.2811630009549));
#195618=CARTESIAN_POINT('',(110.468800439316,2.95,47.9866748994252));
#195619=CARTESIAN_POINT('',(110.411557465446,3.45,48.2811630009549));
#195620=CARTESIAN_POINT('',(110.468800439316,3.45,47.9866748994252));
#195621=CARTESIAN_POINT('Origin',(110.468800439316,2.95,47.9866748994252));
#195622=CARTESIAN_POINT('',(109.977986936766,2.95,47.891269942976));
#195623=CARTESIAN_POINT('',(109.920743962897,2.95,48.1857580445057));
#195624=CARTESIAN_POINT('',(109.977986936766,2.95,47.891269942976));
#195625=CARTESIAN_POINT('',(110.411557465446,2.95,48.2811630009549));
#195626=CARTESIAN_POINT('',(110.468800439316,2.95,47.9866748994252));
#195627=CARTESIAN_POINT('Origin',(109.977986936766,2.95,47.891269942976));
#195628=CARTESIAN_POINT('',(109.920743962897,2.95,48.1857580445057));
#195629=CARTESIAN_POINT('',(109.977986936766,2.95,47.891269942976));
#195630=CARTESIAN_POINT('Origin',(109.977986936766,2.65,47.891269942976));
#195631=CARTESIAN_POINT('',(110.468800439316,2.65,47.9866748994252));
#195632=CARTESIAN_POINT('',(110.411557465446,2.65,48.2811630009549));
#195633=CARTESIAN_POINT('',(110.468800439316,2.65,47.9866748994252));
#195634=CARTESIAN_POINT('',(109.920743962897,2.65,48.1857580445057));
#195635=CARTESIAN_POINT('',(109.920743962897,2.65,48.1857580445057));
#195636=CARTESIAN_POINT('',(109.977986936766,2.65,47.891269942976));
#195637=CARTESIAN_POINT('',(109.977986936766,2.65,47.891269942976));
#195638=CARTESIAN_POINT('',(109.977986936766,2.65,47.891269942976));
#195639=CARTESIAN_POINT('Origin',(110.468800439316,2.65,47.9866748994252));
#195640=CARTESIAN_POINT('',(110.468800439316,2.15,47.9866748994252));
#195641=CARTESIAN_POINT('',(110.411557465446,2.15,48.2811630009549));
#195642=CARTESIAN_POINT('',(110.468800439316,2.15,47.9866748994252));
#195643=CARTESIAN_POINT('',(110.411557465446,2.65,48.2811630009549));
#195644=CARTESIAN_POINT('',(110.468800439316,2.65,47.9866748994252));
#195645=CARTESIAN_POINT('Origin',(110.468800439316,2.15,47.9866748994252));
#195646=CARTESIAN_POINT('',(109.977986936766,2.15,47.891269942976));
#195647=CARTESIAN_POINT('',(109.920743962897,2.15,48.1857580445057));
#195648=CARTESIAN_POINT('',(109.977986936766,2.15,47.891269942976));
#195649=CARTESIAN_POINT('',(110.411557465446,2.15,48.2811630009549));
#195650=CARTESIAN_POINT('',(110.468800439316,2.15,47.9866748994252));
#195651=CARTESIAN_POINT('Origin',(109.977986936766,2.15,47.891269942976));
#195652=CARTESIAN_POINT('',(109.920743962897,2.15,48.1857580445057));
#195653=CARTESIAN_POINT('',(109.977986936766,2.15,47.891269942976));
#195654=CARTESIAN_POINT('Origin',(109.977986936766,1.85,47.891269942976));
#195655=CARTESIAN_POINT('',(110.468800439316,1.85,47.9866748994252));
#195656=CARTESIAN_POINT('',(110.411557465446,1.85,48.2811630009549));
#195657=CARTESIAN_POINT('',(110.468800439316,1.85,47.9866748994252));
#195658=CARTESIAN_POINT('',(109.920743962897,1.85,48.1857580445057));
#195659=CARTESIAN_POINT('',(109.920743962897,1.85,48.1857580445057));
#195660=CARTESIAN_POINT('',(109.977986936766,1.85,47.891269942976));
#195661=CARTESIAN_POINT('',(109.977986936766,1.85,47.891269942976));
#195662=CARTESIAN_POINT('',(109.977986936766,1.85,47.891269942976));
#195663=CARTESIAN_POINT('Origin',(110.468800439316,1.85,47.9866748994252));
#195664=CARTESIAN_POINT('',(110.468800439316,1.35,47.9866748994252));
#195665=CARTESIAN_POINT('',(110.411557465446,1.35,48.2811630009549));
#195666=CARTESIAN_POINT('',(110.468800439316,1.35,47.9866748994252));
#195667=CARTESIAN_POINT('',(110.411557465446,1.85,48.2811630009549));
#195668=CARTESIAN_POINT('',(110.468800439316,1.85,47.9866748994252));
#195669=CARTESIAN_POINT('Origin',(110.468800439316,1.35,47.9866748994252));
#195670=CARTESIAN_POINT('',(109.977986936766,1.35,47.891269942976));
#195671=CARTESIAN_POINT('',(109.920743962897,1.35,48.1857580445057));
#195672=CARTESIAN_POINT('',(109.977986936766,1.35,47.891269942976));
#195673=CARTESIAN_POINT('',(110.411557465446,1.35,48.2811630009549));
#195674=CARTESIAN_POINT('',(110.468800439316,1.35,47.9866748994252));
#195675=CARTESIAN_POINT('Origin',(109.977986936766,1.35,47.891269942976));
#195676=CARTESIAN_POINT('',(109.920743962897,1.35,48.1857580445057));
#195677=CARTESIAN_POINT('',(109.977986936766,1.35,47.891269942976));
#195678=CARTESIAN_POINT('Origin',(109.977986936766,1.05,47.891269942976));
#195679=CARTESIAN_POINT('',(110.468800439316,1.05,47.9866748994252));
#195680=CARTESIAN_POINT('',(110.411557465446,1.05,48.2811630009549));
#195681=CARTESIAN_POINT('',(110.468800439316,1.05,47.9866748994252));
#195682=CARTESIAN_POINT('',(109.920743962897,1.05,48.1857580445057));
#195683=CARTESIAN_POINT('',(109.920743962897,1.05,48.1857580445057));
#195684=CARTESIAN_POINT('',(109.977986936766,1.05,47.891269942976));
#195685=CARTESIAN_POINT('',(109.977986936766,1.05,47.891269942976));
#195686=CARTESIAN_POINT('',(109.977986936766,1.05,47.891269942976));
#195687=CARTESIAN_POINT('Origin',(110.468800439316,1.05,47.9866748994252));
#195688=CARTESIAN_POINT('',(110.468800439316,0.550000000000015,47.9866748994252));
#195689=CARTESIAN_POINT('',(110.411557465446,0.550000000000015,48.2811630009549));
#195690=CARTESIAN_POINT('',(110.468800439316,0.550000000000015,47.9866748994252));
#195691=CARTESIAN_POINT('',(110.411557465446,1.05,48.2811630009549));
#195692=CARTESIAN_POINT('',(110.468800439316,1.05,47.9866748994252));
#195693=CARTESIAN_POINT('Origin',(110.468800439316,0.550000000000015,47.9866748994252));
#195694=CARTESIAN_POINT('',(109.977986936766,0.550000000000015,47.891269942976));
#195695=CARTESIAN_POINT('',(109.920743962897,0.550000000000015,48.1857580445057));
#195696=CARTESIAN_POINT('',(109.977986936766,0.550000000000015,47.891269942976));
#195697=CARTESIAN_POINT('',(110.411557465446,0.550000000000015,48.2811630009549));
#195698=CARTESIAN_POINT('',(110.468800439316,0.550000000000015,47.9866748994252));
#195699=CARTESIAN_POINT('Origin',(109.977986936766,0.550000000000015,47.891269942976));
#195700=CARTESIAN_POINT('',(109.920743962897,0.550000000000015,48.1857580445057));
#195701=CARTESIAN_POINT('',(109.977986936766,0.550000000000015,47.891269942976));
#195702=CARTESIAN_POINT('Origin',(109.977986936766,0.250000000000015,47.891269942976));
#195703=CARTESIAN_POINT('',(110.468800439316,0.250000000000015,47.9866748994252));
#195704=CARTESIAN_POINT('',(110.411557465446,0.250000000000015,48.2811630009549));
#195705=CARTESIAN_POINT('',(110.468800439316,0.250000000000015,47.9866748994252));
#195706=CARTESIAN_POINT('',(109.920743962897,0.250000000000015,48.1857580445057));
#195707=CARTESIAN_POINT('',(109.920743962897,0.250000000000015,48.1857580445057));
#195708=CARTESIAN_POINT('',(109.977986936766,0.250000000000015,47.891269942976));
#195709=CARTESIAN_POINT('',(109.977986936766,0.250000000000015,47.891269942976));
#195710=CARTESIAN_POINT('',(109.977986936766,0.250000000000015,47.891269942976));
#195711=CARTESIAN_POINT('Origin',(110.468800439316,0.250000000000015,47.9866748994252));
#195712=CARTESIAN_POINT('',(110.468800439316,-0.249999999999985,47.9866748994252));
#195713=CARTESIAN_POINT('',(110.411557465446,-0.249999999999985,48.2811630009549));
#195714=CARTESIAN_POINT('',(110.468800439316,-0.249999999999985,47.9866748994252));
#195715=CARTESIAN_POINT('',(110.411557465446,0.250000000000015,48.2811630009549));
#195716=CARTESIAN_POINT('',(110.468800439316,0.250000000000015,47.9866748994252));
#195717=CARTESIAN_POINT('Origin',(110.468800439316,-0.249999999999985,47.9866748994252));
#195718=CARTESIAN_POINT('',(109.977986936766,-0.249999999999985,47.891269942976));
#195719=CARTESIAN_POINT('',(109.920743962897,-0.249999999999985,48.1857580445057));
#195720=CARTESIAN_POINT('',(109.977986936766,-0.249999999999985,47.891269942976));
#195721=CARTESIAN_POINT('',(110.411557465446,-0.249999999999985,48.2811630009549));
#195722=CARTESIAN_POINT('',(110.468800439316,-0.249999999999985,47.9866748994252));
#195723=CARTESIAN_POINT('Origin',(109.977986936766,-0.249999999999985,47.891269942976));
#195724=CARTESIAN_POINT('',(109.920743962897,-0.249999999999985,48.1857580445057));
#195725=CARTESIAN_POINT('',(109.977986936766,-0.249999999999985,47.891269942976));
#195726=CARTESIAN_POINT('Origin',(109.977986936766,-0.549999999999986,47.891269942976));
#195727=CARTESIAN_POINT('',(110.468800439316,-0.549999999999986,47.9866748994252));
#195728=CARTESIAN_POINT('',(110.411557465446,-0.549999999999986,48.2811630009549));
#195729=CARTESIAN_POINT('',(110.468800439316,-0.549999999999986,47.9866748994252));
#195730=CARTESIAN_POINT('',(109.920743962897,-0.549999999999986,48.1857580445057));
#195731=CARTESIAN_POINT('',(109.920743962897,-0.549999999999986,48.1857580445057));
#195732=CARTESIAN_POINT('',(109.977986936766,-0.549999999999986,47.891269942976));
#195733=CARTESIAN_POINT('',(109.977986936766,-0.549999999999986,47.891269942976));
#195734=CARTESIAN_POINT('',(109.977986936766,-0.549999999999986,47.891269942976));
#195735=CARTESIAN_POINT('Origin',(110.468800439316,-0.549999999999986,47.9866748994252));
#195736=CARTESIAN_POINT('',(110.468800439316,-1.05,47.9866748994252));
#195737=CARTESIAN_POINT('',(110.411557465446,-1.05,48.2811630009549));
#195738=CARTESIAN_POINT('',(110.468800439316,-1.05,47.9866748994252));
#195739=CARTESIAN_POINT('',(110.411557465446,-0.549999999999986,48.2811630009549));
#195740=CARTESIAN_POINT('',(110.468800439316,-0.549999999999986,47.9866748994252));
#195741=CARTESIAN_POINT('Origin',(110.468800439316,-1.05,47.9866748994252));
#195742=CARTESIAN_POINT('',(109.977986936766,-1.05,47.891269942976));
#195743=CARTESIAN_POINT('',(109.920743962897,-1.05,48.1857580445057));
#195744=CARTESIAN_POINT('',(109.977986936766,-1.05,47.891269942976));
#195745=CARTESIAN_POINT('',(110.411557465446,-1.05,48.2811630009549));
#195746=CARTESIAN_POINT('',(110.468800439316,-1.05,47.9866748994252));
#195747=CARTESIAN_POINT('Origin',(109.977986936766,-1.05,47.891269942976));
#195748=CARTESIAN_POINT('',(109.920743962897,-1.05,48.1857580445057));
#195749=CARTESIAN_POINT('',(109.977986936766,-1.05,47.891269942976));
#195750=CARTESIAN_POINT('Origin',(109.977986936766,-1.35,47.891269942976));
#195751=CARTESIAN_POINT('',(110.468800439316,-1.35,47.9866748994252));
#195752=CARTESIAN_POINT('',(110.411557465446,-1.35,48.2811630009549));
#195753=CARTESIAN_POINT('',(110.468800439316,-1.35,47.9866748994252));
#195754=CARTESIAN_POINT('',(109.920743962897,-1.35,48.1857580445057));
#195755=CARTESIAN_POINT('',(109.920743962897,-1.35,48.1857580445057));
#195756=CARTESIAN_POINT('',(109.977986936766,-1.35,47.891269942976));
#195757=CARTESIAN_POINT('',(109.977986936766,-1.35,47.891269942976));
#195758=CARTESIAN_POINT('',(109.977986936766,-1.35,47.891269942976));
#195759=CARTESIAN_POINT('Origin',(110.468800439316,-1.35,47.9866748994252));
#195760=CARTESIAN_POINT('',(110.468800439316,-1.85,47.9866748994252));
#195761=CARTESIAN_POINT('',(110.411557465446,-1.85,48.2811630009549));
#195762=CARTESIAN_POINT('',(110.468800439316,-1.85,47.9866748994252));
#195763=CARTESIAN_POINT('',(110.411557465446,-1.35,48.2811630009549));
#195764=CARTESIAN_POINT('',(110.468800439316,-1.35,47.9866748994252));
#195765=CARTESIAN_POINT('Origin',(110.468800439316,-1.85,47.9866748994252));
#195766=CARTESIAN_POINT('',(109.977986936766,-1.85,47.891269942976));
#195767=CARTESIAN_POINT('',(109.920743962897,-1.85,48.1857580445057));
#195768=CARTESIAN_POINT('',(109.977986936766,-1.85,47.891269942976));
#195769=CARTESIAN_POINT('',(110.411557465446,-1.85,48.2811630009549));
#195770=CARTESIAN_POINT('',(110.468800439316,-1.85,47.9866748994252));
#195771=CARTESIAN_POINT('Origin',(109.977986936766,-1.85,47.891269942976));
#195772=CARTESIAN_POINT('',(109.920743962897,-1.85,48.1857580445057));
#195773=CARTESIAN_POINT('',(109.977986936766,-1.85,47.891269942976));
#195774=CARTESIAN_POINT('Origin',(109.977986936766,-2.15,47.891269942976));
#195775=CARTESIAN_POINT('',(110.468800439316,-2.15,47.9866748994252));
#195776=CARTESIAN_POINT('',(110.411557465446,-2.15,48.2811630009549));
#195777=CARTESIAN_POINT('',(110.468800439316,-2.15,47.9866748994252));
#195778=CARTESIAN_POINT('',(109.920743962897,-2.15,48.1857580445057));
#195779=CARTESIAN_POINT('',(109.920743962897,-2.15,48.1857580445057));
#195780=CARTESIAN_POINT('',(109.977986936766,-2.15,47.891269942976));
#195781=CARTESIAN_POINT('',(109.977986936766,-2.15,47.891269942976));
#195782=CARTESIAN_POINT('',(109.977986936766,-2.15,47.891269942976));
#195783=CARTESIAN_POINT('Origin',(110.468800439316,-2.15,47.9866748994252));
#195784=CARTESIAN_POINT('',(110.468800439316,-2.65,47.9866748994252));
#195785=CARTESIAN_POINT('',(110.411557465446,-2.65,48.2811630009549));
#195786=CARTESIAN_POINT('',(110.468800439316,-2.65,47.9866748994252));
#195787=CARTESIAN_POINT('',(110.411557465446,-2.15,48.2811630009549));
#195788=CARTESIAN_POINT('',(110.468800439316,-2.15,47.9866748994252));
#195789=CARTESIAN_POINT('Origin',(110.468800439316,-2.65,47.9866748994252));
#195790=CARTESIAN_POINT('',(109.977986936766,-2.65,47.891269942976));
#195791=CARTESIAN_POINT('',(109.920743962897,-2.65,48.1857580445057));
#195792=CARTESIAN_POINT('',(109.977986936766,-2.65,47.891269942976));
#195793=CARTESIAN_POINT('',(110.411557465446,-2.65,48.2811630009549));
#195794=CARTESIAN_POINT('',(110.468800439316,-2.65,47.9866748994252));
#195795=CARTESIAN_POINT('Origin',(109.977986936766,-2.65,47.891269942976));
#195796=CARTESIAN_POINT('',(109.920743962897,-2.65,48.1857580445057));
#195797=CARTESIAN_POINT('',(109.977986936766,-2.65,47.891269942976));
#195798=CARTESIAN_POINT('Origin',(109.977986936766,-2.95,47.891269942976));
#195799=CARTESIAN_POINT('',(110.468800439316,-2.95,47.9866748994252));
#195800=CARTESIAN_POINT('',(110.411557465446,-2.95,48.2811630009549));
#195801=CARTESIAN_POINT('',(110.468800439316,-2.95,47.9866748994252));
#195802=CARTESIAN_POINT('',(109.920743962897,-2.95,48.1857580445057));
#195803=CARTESIAN_POINT('',(109.920743962897,-2.95,48.1857580445057));
#195804=CARTESIAN_POINT('',(109.977986936766,-2.95,47.891269942976));
#195805=CARTESIAN_POINT('',(109.977986936766,-2.95,47.891269942976));
#195806=CARTESIAN_POINT('',(109.977986936766,-2.95,47.891269942976));
#195807=CARTESIAN_POINT('Origin',(110.468800439316,-2.95,47.9866748994252));
#195808=CARTESIAN_POINT('',(110.468800439316,-3.45,47.9866748994252));
#195809=CARTESIAN_POINT('',(110.411557465446,-3.45,48.2811630009549));
#195810=CARTESIAN_POINT('',(110.468800439316,-3.45,47.9866748994252));
#195811=CARTESIAN_POINT('',(110.411557465446,-2.95,48.2811630009549));
#195812=CARTESIAN_POINT('',(110.468800439316,-2.95,47.9866748994252));
#195813=CARTESIAN_POINT('Origin',(110.468800439316,-3.45,47.9866748994252));
#195814=CARTESIAN_POINT('',(109.977986936766,-3.45,47.891269942976));
#195815=CARTESIAN_POINT('',(109.920743962897,-3.45,48.1857580445057));
#195816=CARTESIAN_POINT('',(109.977986936766,-3.45,47.891269942976));
#195817=CARTESIAN_POINT('',(110.411557465446,-3.45,48.2811630009549));
#195818=CARTESIAN_POINT('',(110.468800439316,-3.45,47.9866748994252));
#195819=CARTESIAN_POINT('Origin',(109.977986936766,-3.45,47.891269942976));
#195820=CARTESIAN_POINT('',(109.920743962897,-3.45,48.1857580445057));
#195821=CARTESIAN_POINT('',(109.977986936766,-3.45,47.891269942976));
#195822=CARTESIAN_POINT('Origin',(109.977986936766,-3.75,47.891269942976));
#195823=CARTESIAN_POINT('',(110.468800439316,-3.75,47.9866748994252));
#195824=CARTESIAN_POINT('',(110.411557465446,-3.75,48.2811630009549));
#195825=CARTESIAN_POINT('',(110.468800439316,-3.75,47.9866748994252));
#195826=CARTESIAN_POINT('',(109.920743962897,-3.75,48.1857580445057));
#195827=CARTESIAN_POINT('',(109.920743962897,-3.75,48.1857580445057));
#195828=CARTESIAN_POINT('',(109.977986936766,-3.75,47.891269942976));
#195829=CARTESIAN_POINT('',(109.977986936766,-3.75,47.891269942976));
#195830=CARTESIAN_POINT('',(109.977986936766,-3.75,47.891269942976));
#195831=CARTESIAN_POINT('Origin',(110.468800439316,-3.75,47.9866748994252));
#195832=CARTESIAN_POINT('',(110.468800439316,-4.25,47.9866748994252));
#195833=CARTESIAN_POINT('',(110.411557465446,-4.25,48.2811630009549));
#195834=CARTESIAN_POINT('',(110.468800439316,-4.25,47.9866748994252));
#195835=CARTESIAN_POINT('',(110.411557465446,-3.75,48.2811630009549));
#195836=CARTESIAN_POINT('',(110.468800439316,-3.75,47.9866748994252));
#195837=CARTESIAN_POINT('Origin',(110.468800439316,-4.25,47.9866748994252));
#195838=CARTESIAN_POINT('',(109.977986936766,-4.25,47.891269942976));
#195839=CARTESIAN_POINT('',(109.920743962897,-4.25,48.1857580445057));
#195840=CARTESIAN_POINT('',(109.977986936766,-4.25,47.891269942976));
#195841=CARTESIAN_POINT('',(110.411557465446,-4.25,48.2811630009549));
#195842=CARTESIAN_POINT('',(110.468800439316,-4.25,47.9866748994252));
#195843=CARTESIAN_POINT('Origin',(109.977986936766,-4.25,47.891269942976));
#195844=CARTESIAN_POINT('',(109.920743962897,-4.25,48.1857580445057));
#195845=CARTESIAN_POINT('',(109.977986936766,-4.25,47.891269942976));
#195846=CARTESIAN_POINT('Origin',(109.977986936766,-4.55,47.891269942976));
#195847=CARTESIAN_POINT('',(110.468800439316,-4.55,47.9866748994252));
#195848=CARTESIAN_POINT('',(110.411557465446,-4.55,48.2811630009549));
#195849=CARTESIAN_POINT('',(110.468800439316,-4.55,47.9866748994252));
#195850=CARTESIAN_POINT('',(109.920743962897,-4.55,48.1857580445057));
#195851=CARTESIAN_POINT('',(109.920743962897,-4.55,48.1857580445057));
#195852=CARTESIAN_POINT('',(109.977986936766,-4.55,47.891269942976));
#195853=CARTESIAN_POINT('',(109.977986936766,-4.55,47.891269942976));
#195854=CARTESIAN_POINT('',(109.977986936766,-4.55,47.891269942976));
#195855=CARTESIAN_POINT('Origin',(110.468800439316,-4.55,47.9866748994252));
#195856=CARTESIAN_POINT('',(110.468800439316,-5.05,47.9866748994252));
#195857=CARTESIAN_POINT('',(110.411557465446,-5.05,48.2811630009549));
#195858=CARTESIAN_POINT('',(110.468800439316,-5.05,47.9866748994252));
#195859=CARTESIAN_POINT('',(110.411557465446,-4.55,48.2811630009549));
#195860=CARTESIAN_POINT('',(110.468800439316,-4.55,47.9866748994252));
#195861=CARTESIAN_POINT('Origin',(110.468800439316,-5.05,47.9866748994252));
#195862=CARTESIAN_POINT('',(109.977986936766,-5.05,47.891269942976));
#195863=CARTESIAN_POINT('',(109.920743962897,-5.05,48.1857580445057));
#195864=CARTESIAN_POINT('',(109.977986936766,-5.05,47.891269942976));
#195865=CARTESIAN_POINT('',(110.411557465446,-5.05,48.2811630009549));
#195866=CARTESIAN_POINT('',(110.468800439316,-5.05,47.9866748994252));
#195867=CARTESIAN_POINT('Origin',(109.977986936766,-5.05,47.891269942976));
#195868=CARTESIAN_POINT('',(109.920743962897,-5.05,48.1857580445057));
#195869=CARTESIAN_POINT('',(109.977986936766,-5.05,47.891269942976));
#195870=CARTESIAN_POINT('Origin',(109.977986936766,-5.35,47.891269942976));
#195871=CARTESIAN_POINT('',(110.468800439316,-5.35,47.9866748994252));
#195872=CARTESIAN_POINT('',(110.411557465446,-5.35,48.2811630009549));
#195873=CARTESIAN_POINT('',(110.468800439316,-5.35,47.9866748994252));
#195874=CARTESIAN_POINT('',(109.920743962897,-5.35,48.1857580445057));
#195875=CARTESIAN_POINT('',(109.920743962897,-5.35,48.1857580445057));
#195876=CARTESIAN_POINT('',(109.977986936766,-5.35,47.891269942976));
#195877=CARTESIAN_POINT('',(109.977986936766,-5.35,47.891269942976));
#195878=CARTESIAN_POINT('',(109.977986936766,-5.35,47.891269942976));
#195879=CARTESIAN_POINT('Origin',(110.468800439316,-5.35,47.9866748994252));
#195880=CARTESIAN_POINT('',(110.468800439316,-5.85,47.9866748994252));
#195881=CARTESIAN_POINT('',(110.411557465446,-5.85,48.2811630009549));
#195882=CARTESIAN_POINT('',(110.468800439316,-5.85,47.9866748994252));
#195883=CARTESIAN_POINT('',(110.411557465446,-5.35,48.2811630009549));
#195884=CARTESIAN_POINT('',(110.468800439316,-5.35,47.9866748994252));
#195885=CARTESIAN_POINT('Origin',(110.468800439316,-5.85,47.9866748994252));
#195886=CARTESIAN_POINT('',(109.977986936766,-5.85,47.891269942976));
#195887=CARTESIAN_POINT('',(109.920743962897,-5.85,48.1857580445057));
#195888=CARTESIAN_POINT('',(109.977986936766,-5.85,47.891269942976));
#195889=CARTESIAN_POINT('',(110.411557465446,-5.85,48.2811630009549));
#195890=CARTESIAN_POINT('',(110.468800439316,-5.85,47.9866748994252));
#195891=CARTESIAN_POINT('Origin',(109.977986936766,-5.85,47.891269942976));
#195892=CARTESIAN_POINT('',(109.920743962897,-5.85,48.1857580445057));
#195893=CARTESIAN_POINT('',(109.977986936766,-5.85,47.891269942976));
#195894=CARTESIAN_POINT('Origin',(111.548590144925,-6.95,48.1965658036136));
#195895=CARTESIAN_POINT('',(112.039403647474,-6.95,48.2919707600629));
#195896=CARTESIAN_POINT('',(111.982160673605,-6.95,48.5864588615926));
#195897=CARTESIAN_POINT('',(112.039403647474,-6.95,48.2919707600629));
#195898=CARTESIAN_POINT('',(111.491347171055,-6.95,48.4910539051433));
#195899=CARTESIAN_POINT('',(111.491347171055,-6.95,48.4910539051433));
#195900=CARTESIAN_POINT('',(111.548590144925,-6.95,48.1965658036136));
#195901=CARTESIAN_POINT('',(111.548590144925,-6.95,48.1965658036136));
#195902=CARTESIAN_POINT('',(111.548590144925,-6.95,48.1965658036136));
#195903=CARTESIAN_POINT('Origin',(112.039403647474,-6.95,48.2919707600629));
#195904=CARTESIAN_POINT('',(112.039403647474,-7.45,48.2919707600629));
#195905=CARTESIAN_POINT('',(111.982160673605,-7.45,48.5864588615926));
#195906=CARTESIAN_POINT('',(112.039403647474,-7.45,48.2919707600629));
#195907=CARTESIAN_POINT('',(111.982160673605,-6.95,48.5864588615926));
#195908=CARTESIAN_POINT('',(112.039403647474,-6.95,48.2919707600629));
#195909=CARTESIAN_POINT('Origin',(112.039403647474,-7.45,48.2919707600629));
#195910=CARTESIAN_POINT('',(111.548590144925,-7.45,48.1965658036136));
#195911=CARTESIAN_POINT('',(111.491347171055,-7.45,48.4910539051433));
#195912=CARTESIAN_POINT('',(111.548590144925,-7.45,48.1965658036136));
#195913=CARTESIAN_POINT('',(111.982160673605,-7.45,48.5864588615926));
#195914=CARTESIAN_POINT('',(112.039403647474,-7.45,48.2919707600629));
#195915=CARTESIAN_POINT('Origin',(111.548590144925,-7.45,48.1965658036136));
#195916=CARTESIAN_POINT('',(111.491347171055,-7.45,48.4910539051433));
#195917=CARTESIAN_POINT('',(111.548590144925,-7.45,48.1965658036136));
#195918=CARTESIAN_POINT('Origin',(112.333891749004,-6.95,48.3492137339324));
#195919=CARTESIAN_POINT('',(112.824705251554,-6.95,48.4446186903817));
#195920=CARTESIAN_POINT('',(112.767462277684,-6.95,48.7391067919114));
#195921=CARTESIAN_POINT('',(112.824705251554,-6.95,48.4446186903817));
#195922=CARTESIAN_POINT('',(112.276648775135,-6.95,48.6437018354621));
#195923=CARTESIAN_POINT('',(112.276648775135,-6.95,48.6437018354621));
#195924=CARTESIAN_POINT('',(112.333891749004,-6.95,48.3492137339324));
#195925=CARTESIAN_POINT('',(112.333891749004,-6.95,48.3492137339324));
#195926=CARTESIAN_POINT('',(112.333891749004,-6.95,48.3492137339324));
#195927=CARTESIAN_POINT('Origin',(112.824705251554,-6.95,48.4446186903817));
#195928=CARTESIAN_POINT('',(112.824705251554,-7.45,48.4446186903817));
#195929=CARTESIAN_POINT('',(112.767462277684,-7.45,48.7391067919114));
#195930=CARTESIAN_POINT('',(112.824705251554,-7.45,48.4446186903817));
#195931=CARTESIAN_POINT('',(112.767462277684,-6.95,48.7391067919114));
#195932=CARTESIAN_POINT('',(112.824705251554,-6.95,48.4446186903817));
#195933=CARTESIAN_POINT('Origin',(112.824705251554,-7.45,48.4446186903817));
#195934=CARTESIAN_POINT('',(112.333891749004,-7.45,48.3492137339324));
#195935=CARTESIAN_POINT('',(112.276648775135,-7.45,48.6437018354621));
#195936=CARTESIAN_POINT('',(112.333891749004,-7.45,48.3492137339324));
#195937=CARTESIAN_POINT('',(112.767462277684,-7.45,48.7391067919114));
#195938=CARTESIAN_POINT('',(112.824705251554,-7.45,48.4446186903817));
#195939=CARTESIAN_POINT('Origin',(112.333891749004,-7.45,48.3492137339324));
#195940=CARTESIAN_POINT('',(112.276648775135,-7.45,48.6437018354621));
#195941=CARTESIAN_POINT('',(112.333891749004,-7.45,48.3492137339324));
#195942=CARTESIAN_POINT('Origin',(113.119193353083,-6.95,48.5018616642512));
#195943=CARTESIAN_POINT('',(113.610006855633,-6.95,48.5972666207005));
#195944=CARTESIAN_POINT('',(113.552763881763,-6.95,48.8917547222302));
#195945=CARTESIAN_POINT('',(113.610006855633,-6.95,48.5972666207005));
#195946=CARTESIAN_POINT('',(113.061950379214,-6.95,48.7963497657809));
#195947=CARTESIAN_POINT('',(113.061950379214,-6.95,48.7963497657809));
#195948=CARTESIAN_POINT('',(113.119193353083,-6.95,48.5018616642512));
#195949=CARTESIAN_POINT('',(113.119193353083,-6.95,48.5018616642512));
#195950=CARTESIAN_POINT('',(113.119193353083,-6.95,48.5018616642512));
#195951=CARTESIAN_POINT('Origin',(113.610006855633,-6.95,48.5972666207005));
#195952=CARTESIAN_POINT('',(113.610006855633,-7.45,48.5972666207005));
#195953=CARTESIAN_POINT('',(113.552763881763,-7.45,48.8917547222302));
#195954=CARTESIAN_POINT('',(113.610006855633,-7.45,48.5972666207005));
#195955=CARTESIAN_POINT('',(113.552763881763,-6.95,48.8917547222302));
#195956=CARTESIAN_POINT('',(113.610006855633,-6.95,48.5972666207005));
#195957=CARTESIAN_POINT('Origin',(113.610006855633,-7.45,48.5972666207005));
#195958=CARTESIAN_POINT('',(113.119193353083,-7.45,48.5018616642512));
#195959=CARTESIAN_POINT('',(113.061950379214,-7.45,48.7963497657809));
#195960=CARTESIAN_POINT('',(113.119193353083,-7.45,48.5018616642512));
#195961=CARTESIAN_POINT('',(113.552763881763,-7.45,48.8917547222302));
#195962=CARTESIAN_POINT('',(113.610006855633,-7.45,48.5972666207005));
#195963=CARTESIAN_POINT('Origin',(113.119193353083,-7.45,48.5018616642512));
#195964=CARTESIAN_POINT('',(113.061950379214,-7.45,48.7963497657809));
#195965=CARTESIAN_POINT('',(113.119193353083,-7.45,48.5018616642512));
#195966=CARTESIAN_POINT('Origin',(113.904494957163,-6.95,48.65450959457));
#195967=CARTESIAN_POINT('',(114.395308459712,-6.95,48.7499145510193));
#195968=CARTESIAN_POINT('',(114.338065485842,-6.95,49.044402652549));
#195969=CARTESIAN_POINT('',(114.395308459712,-6.95,48.7499145510193));
#195970=CARTESIAN_POINT('',(113.847251983293,-6.95,48.9489976960997));
#195971=CARTESIAN_POINT('',(113.847251983293,-6.95,48.9489976960997));
#195972=CARTESIAN_POINT('',(113.904494957163,-6.95,48.65450959457));
#195973=CARTESIAN_POINT('',(113.904494957163,-6.95,48.65450959457));
#195974=CARTESIAN_POINT('',(113.904494957163,-6.95,48.65450959457));
#195975=CARTESIAN_POINT('Origin',(114.395308459712,-6.95,48.7499145510193));
#195976=CARTESIAN_POINT('',(114.395308459712,-7.45,48.7499145510193));
#195977=CARTESIAN_POINT('',(114.338065485842,-7.45,49.044402652549));
#195978=CARTESIAN_POINT('',(114.395308459712,-7.45,48.7499145510193));
#195979=CARTESIAN_POINT('',(114.338065485842,-6.95,49.044402652549));
#195980=CARTESIAN_POINT('',(114.395308459712,-6.95,48.7499145510193));
#195981=CARTESIAN_POINT('Origin',(114.395308459712,-7.45,48.7499145510193));
#195982=CARTESIAN_POINT('',(113.904494957163,-7.45,48.65450959457));
#195983=CARTESIAN_POINT('',(113.847251983293,-7.45,48.9489976960997));
#195984=CARTESIAN_POINT('',(113.904494957163,-7.45,48.65450959457));
#195985=CARTESIAN_POINT('',(114.338065485842,-7.45,49.044402652549));
#195986=CARTESIAN_POINT('',(114.395308459712,-7.45,48.7499145510193));
#195987=CARTESIAN_POINT('Origin',(113.904494957163,-7.45,48.65450959457));
#195988=CARTESIAN_POINT('',(113.847251983293,-7.45,48.9489976960997));
#195989=CARTESIAN_POINT('',(113.904494957163,-7.45,48.65450959457));
#195990=CARTESIAN_POINT('Origin',(114.689796561242,-6.95,48.8071575248888));
#195991=CARTESIAN_POINT('',(115.180610063791,-6.95,48.9025624813381));
#195992=CARTESIAN_POINT('',(115.123367089922,-6.95,49.1970505828678));
#195993=CARTESIAN_POINT('',(115.180610063791,-6.95,48.9025624813381));
#195994=CARTESIAN_POINT('',(114.632553587372,-6.95,49.1016456264185));
#195995=CARTESIAN_POINT('',(114.632553587372,-6.95,49.1016456264185));
#195996=CARTESIAN_POINT('',(114.689796561242,-6.95,48.8071575248888));
#195997=CARTESIAN_POINT('',(114.689796561242,-6.95,48.8071575248888));
#195998=CARTESIAN_POINT('',(114.689796561242,-6.95,48.8071575248888));
#195999=CARTESIAN_POINT('Origin',(115.180610063791,-6.95,48.9025624813381));
#196000=CARTESIAN_POINT('',(115.180610063791,-7.45,48.9025624813381));
#196001=CARTESIAN_POINT('',(115.123367089922,-7.45,49.1970505828678));
#196002=CARTESIAN_POINT('',(115.180610063791,-7.45,48.9025624813381));
#196003=CARTESIAN_POINT('',(115.123367089922,-6.95,49.1970505828678));
#196004=CARTESIAN_POINT('',(115.180610063791,-6.95,48.9025624813381));
#196005=CARTESIAN_POINT('Origin',(115.180610063791,-7.45,48.9025624813381));
#196006=CARTESIAN_POINT('',(114.689796561242,-7.45,48.8071575248888));
#196007=CARTESIAN_POINT('',(114.632553587372,-7.45,49.1016456264185));
#196008=CARTESIAN_POINT('',(114.689796561242,-7.45,48.8071575248888));
#196009=CARTESIAN_POINT('',(115.123367089922,-7.45,49.1970505828678));
#196010=CARTESIAN_POINT('',(115.180610063791,-7.45,48.9025624813381));
#196011=CARTESIAN_POINT('Origin',(114.689796561242,-7.45,48.8071575248888));
#196012=CARTESIAN_POINT('',(114.632553587372,-7.45,49.1016456264185));
#196013=CARTESIAN_POINT('',(114.689796561242,-7.45,48.8071575248888));
#196014=CARTESIAN_POINT('Origin',(115.475098165321,-6.95,48.9598054552076));
#196015=CARTESIAN_POINT('',(115.96591166787,-6.95,49.0552104116569));
#196016=CARTESIAN_POINT('',(115.908668694001,-6.95,49.3496985131866));
#196017=CARTESIAN_POINT('',(115.96591166787,-6.95,49.0552104116569));
#196018=CARTESIAN_POINT('',(115.417855191451,-6.95,49.2542935567373));
#196019=CARTESIAN_POINT('',(115.417855191451,-6.95,49.2542935567373));
#196020=CARTESIAN_POINT('',(115.475098165321,-6.95,48.9598054552076));
#196021=CARTESIAN_POINT('',(115.475098165321,-6.95,48.9598054552076));
#196022=CARTESIAN_POINT('',(115.475098165321,-6.95,48.9598054552076));
#196023=CARTESIAN_POINT('Origin',(115.96591166787,-6.95,49.0552104116569));
#196024=CARTESIAN_POINT('',(115.96591166787,-7.45,49.0552104116569));
#196025=CARTESIAN_POINT('',(115.908668694001,-7.45,49.3496985131866));
#196026=CARTESIAN_POINT('',(115.96591166787,-7.45,49.0552104116569));
#196027=CARTESIAN_POINT('',(115.908668694001,-6.95,49.3496985131866));
#196028=CARTESIAN_POINT('',(115.96591166787,-6.95,49.0552104116569));
#196029=CARTESIAN_POINT('Origin',(115.96591166787,-7.45,49.0552104116569));
#196030=CARTESIAN_POINT('',(115.475098165321,-7.45,48.9598054552076));
#196031=CARTESIAN_POINT('',(115.417855191451,-7.45,49.2542935567373));
#196032=CARTESIAN_POINT('',(115.475098165321,-7.45,48.9598054552076));
#196033=CARTESIAN_POINT('',(115.908668694001,-7.45,49.3496985131866));
#196034=CARTESIAN_POINT('',(115.96591166787,-7.45,49.0552104116569));
#196035=CARTESIAN_POINT('Origin',(115.475098165321,-7.45,48.9598054552076));
#196036=CARTESIAN_POINT('',(115.417855191451,-7.45,49.2542935567373));
#196037=CARTESIAN_POINT('',(115.475098165321,-7.45,48.9598054552076));
#196038=CARTESIAN_POINT('Origin',(116.2603997694,-6.95,49.1124533855264));
#196039=CARTESIAN_POINT('',(116.75121327195,-6.95,49.2078583419757));
#196040=CARTESIAN_POINT('',(116.69397029808,-6.95,49.5023464435054));
#196041=CARTESIAN_POINT('',(116.75121327195,-6.95,49.2078583419757));
#196042=CARTESIAN_POINT('',(116.203156795531,-6.95,49.4069414870561));
#196043=CARTESIAN_POINT('',(116.203156795531,-6.95,49.4069414870561));
#196044=CARTESIAN_POINT('',(116.2603997694,-6.95,49.1124533855264));
#196045=CARTESIAN_POINT('',(116.2603997694,-6.95,49.1124533855264));
#196046=CARTESIAN_POINT('',(116.2603997694,-6.95,49.1124533855264));
#196047=CARTESIAN_POINT('Origin',(116.75121327195,-6.95,49.2078583419757));
#196048=CARTESIAN_POINT('',(116.75121327195,-7.45,49.2078583419757));
#196049=CARTESIAN_POINT('',(116.69397029808,-7.45,49.5023464435054));
#196050=CARTESIAN_POINT('',(116.75121327195,-7.45,49.2078583419757));
#196051=CARTESIAN_POINT('',(116.69397029808,-6.95,49.5023464435054));
#196052=CARTESIAN_POINT('',(116.75121327195,-6.95,49.2078583419757));
#196053=CARTESIAN_POINT('Origin',(116.75121327195,-7.45,49.2078583419757));
#196054=CARTESIAN_POINT('',(116.2603997694,-7.45,49.1124533855264));
#196055=CARTESIAN_POINT('',(116.203156795531,-7.45,49.4069414870561));
#196056=CARTESIAN_POINT('',(116.2603997694,-7.45,49.1124533855264));
#196057=CARTESIAN_POINT('',(116.69397029808,-7.45,49.5023464435054));
#196058=CARTESIAN_POINT('',(116.75121327195,-7.45,49.2078583419757));
#196059=CARTESIAN_POINT('Origin',(116.2603997694,-7.45,49.1124533855264));
#196060=CARTESIAN_POINT('',(116.203156795531,-7.45,49.4069414870561));
#196061=CARTESIAN_POINT('',(116.2603997694,-7.45,49.1124533855264));
#196062=CARTESIAN_POINT('Origin',(117.045701373479,-6.95,49.2651013158452));
#196063=CARTESIAN_POINT('',(117.536514876029,-6.95,49.3605062722945));
#196064=CARTESIAN_POINT('',(117.479271902159,-6.95,49.6549943738242));
#196065=CARTESIAN_POINT('',(117.536514876029,-6.95,49.3605062722945));
#196066=CARTESIAN_POINT('',(116.98845839961,-6.95,49.5595894173749));
#196067=CARTESIAN_POINT('',(116.98845839961,-6.95,49.5595894173749));
#196068=CARTESIAN_POINT('',(117.045701373479,-6.95,49.2651013158452));
#196069=CARTESIAN_POINT('',(117.045701373479,-6.95,49.2651013158452));
#196070=CARTESIAN_POINT('',(117.045701373479,-6.95,49.2651013158452));
#196071=CARTESIAN_POINT('Origin',(117.536514876029,-6.95,49.3605062722945));
#196072=CARTESIAN_POINT('',(117.536514876029,-7.45,49.3605062722945));
#196073=CARTESIAN_POINT('',(117.479271902159,-7.45,49.6549943738242));
#196074=CARTESIAN_POINT('',(117.536514876029,-7.45,49.3605062722945));
#196075=CARTESIAN_POINT('',(117.479271902159,-6.95,49.6549943738242));
#196076=CARTESIAN_POINT('',(117.536514876029,-6.95,49.3605062722945));
#196077=CARTESIAN_POINT('Origin',(117.536514876029,-7.45,49.3605062722945));
#196078=CARTESIAN_POINT('',(117.045701373479,-7.45,49.2651013158452));
#196079=CARTESIAN_POINT('',(116.98845839961,-7.45,49.5595894173749));
#196080=CARTESIAN_POINT('',(117.045701373479,-7.45,49.2651013158452));
#196081=CARTESIAN_POINT('',(117.479271902159,-7.45,49.6549943738242));
#196082=CARTESIAN_POINT('',(117.536514876029,-7.45,49.3605062722945));
#196083=CARTESIAN_POINT('Origin',(117.045701373479,-7.45,49.2651013158452));
#196084=CARTESIAN_POINT('',(116.98845839961,-7.45,49.5595894173749));
#196085=CARTESIAN_POINT('',(117.045701373479,-7.45,49.2651013158452));
#196086=CARTESIAN_POINT('Origin',(117.831002977559,-6.95,49.417749246164));
#196087=CARTESIAN_POINT('',(118.321816480108,-6.95,49.5131542026133));
#196088=CARTESIAN_POINT('',(118.264573506239,-6.95,49.807642304143));
#196089=CARTESIAN_POINT('',(118.321816480108,-6.95,49.5131542026133));
#196090=CARTESIAN_POINT('',(117.773760003689,-6.95,49.7122373476937));
#196091=CARTESIAN_POINT('',(117.773760003689,-6.95,49.7122373476937));
#196092=CARTESIAN_POINT('',(117.831002977559,-6.95,49.417749246164));
#196093=CARTESIAN_POINT('',(117.831002977559,-6.95,49.417749246164));
#196094=CARTESIAN_POINT('',(117.831002977559,-6.95,49.417749246164));
#196095=CARTESIAN_POINT('Origin',(118.321816480108,-6.95,49.5131542026133));
#196096=CARTESIAN_POINT('',(118.321816480108,-7.45,49.5131542026133));
#196097=CARTESIAN_POINT('',(118.264573506239,-7.45,49.807642304143));
#196098=CARTESIAN_POINT('',(118.321816480108,-7.45,49.5131542026133));
#196099=CARTESIAN_POINT('',(118.264573506239,-6.95,49.807642304143));
#196100=CARTESIAN_POINT('',(118.321816480108,-6.95,49.5131542026133));
#196101=CARTESIAN_POINT('Origin',(118.321816480108,-7.45,49.5131542026133));
#196102=CARTESIAN_POINT('',(117.831002977559,-7.45,49.417749246164));
#196103=CARTESIAN_POINT('',(117.773760003689,-7.45,49.7122373476937));
#196104=CARTESIAN_POINT('',(117.831002977559,-7.45,49.417749246164));
#196105=CARTESIAN_POINT('',(118.264573506239,-7.45,49.807642304143));
#196106=CARTESIAN_POINT('',(118.321816480108,-7.45,49.5131542026133));
#196107=CARTESIAN_POINT('Origin',(117.831002977559,-7.45,49.417749246164));
#196108=CARTESIAN_POINT('',(117.773760003689,-7.45,49.7122373476937));
#196109=CARTESIAN_POINT('',(117.831002977559,-7.45,49.417749246164));
#196110=CARTESIAN_POINT('Origin',(118.616304581638,-6.95,49.5703971764828));
#196111=CARTESIAN_POINT('',(119.107118084187,-6.95,49.6658021329321));
#196112=CARTESIAN_POINT('',(119.049875110318,-6.95,49.9602902344618));
#196113=CARTESIAN_POINT('',(119.107118084187,-6.95,49.6658021329321));
#196114=CARTESIAN_POINT('',(118.559061607768,-6.95,49.8648852780125));
#196115=CARTESIAN_POINT('',(118.559061607768,-6.95,49.8648852780125));
#196116=CARTESIAN_POINT('',(118.616304581638,-6.95,49.5703971764828));
#196117=CARTESIAN_POINT('',(118.616304581638,-6.95,49.5703971764828));
#196118=CARTESIAN_POINT('',(118.616304581638,-6.95,49.5703971764828));
#196119=CARTESIAN_POINT('Origin',(119.107118084187,-6.95,49.6658021329321));
#196120=CARTESIAN_POINT('',(119.107118084187,-7.45,49.6658021329321));
#196121=CARTESIAN_POINT('',(119.049875110318,-7.45,49.9602902344618));
#196122=CARTESIAN_POINT('',(119.107118084187,-7.45,49.6658021329321));
#196123=CARTESIAN_POINT('',(119.049875110318,-6.95,49.9602902344618));
#196124=CARTESIAN_POINT('',(119.107118084187,-6.95,49.6658021329321));
#196125=CARTESIAN_POINT('Origin',(119.107118084187,-7.45,49.6658021329321));
#196126=CARTESIAN_POINT('',(118.616304581638,-7.45,49.5703971764828));
#196127=CARTESIAN_POINT('',(118.559061607768,-7.45,49.8648852780125));
#196128=CARTESIAN_POINT('',(118.616304581638,-7.45,49.5703971764828));
#196129=CARTESIAN_POINT('',(119.049875110318,-7.45,49.9602902344618));
#196130=CARTESIAN_POINT('',(119.107118084187,-7.45,49.6658021329321));
#196131=CARTESIAN_POINT('Origin',(118.616304581638,-7.45,49.5703971764828));
#196132=CARTESIAN_POINT('',(118.559061607768,-7.45,49.8648852780125));
#196133=CARTESIAN_POINT('',(118.616304581638,-7.45,49.5703971764828));
#196134=CARTESIAN_POINT('Origin',(119.401606185717,-6.95,49.7230451068016));
#196135=CARTESIAN_POINT('',(119.892419688267,-6.95,49.8184500632509));
#196136=CARTESIAN_POINT('',(119.835176714397,-6.95,50.1129381647806));
#196137=CARTESIAN_POINT('',(119.892419688267,-6.95,49.8184500632509));
#196138=CARTESIAN_POINT('',(119.344363211847,-6.95,50.0175332083313));
#196139=CARTESIAN_POINT('',(119.344363211847,-6.95,50.0175332083313));
#196140=CARTESIAN_POINT('',(119.401606185717,-6.95,49.7230451068016));
#196141=CARTESIAN_POINT('',(119.401606185717,-6.95,49.7230451068016));
#196142=CARTESIAN_POINT('',(119.401606185717,-6.95,49.7230451068016));
#196143=CARTESIAN_POINT('Origin',(119.892419688267,-6.95,49.8184500632509));
#196144=CARTESIAN_POINT('',(119.892419688267,-7.45,49.8184500632509));
#196145=CARTESIAN_POINT('',(119.835176714397,-7.45,50.1129381647806));
#196146=CARTESIAN_POINT('',(119.892419688267,-7.45,49.8184500632509));
#196147=CARTESIAN_POINT('',(119.835176714397,-6.95,50.1129381647806));
#196148=CARTESIAN_POINT('',(119.892419688267,-6.95,49.8184500632509));
#196149=CARTESIAN_POINT('Origin',(119.892419688267,-7.45,49.8184500632509));
#196150=CARTESIAN_POINT('',(119.401606185717,-7.45,49.7230451068016));
#196151=CARTESIAN_POINT('',(119.344363211847,-7.45,50.0175332083313));
#196152=CARTESIAN_POINT('',(119.401606185717,-7.45,49.7230451068016));
#196153=CARTESIAN_POINT('',(119.835176714397,-7.45,50.1129381647806));
#196154=CARTESIAN_POINT('',(119.892419688267,-7.45,49.8184500632509));
#196155=CARTESIAN_POINT('Origin',(119.401606185717,-7.45,49.7230451068016));
#196156=CARTESIAN_POINT('',(119.344363211847,-7.45,50.0175332083313));
#196157=CARTESIAN_POINT('',(119.401606185717,-7.45,49.7230451068016));
#196158=CARTESIAN_POINT('Origin',(120.186907789796,-6.95,49.8756930371204));
#196159=CARTESIAN_POINT('',(120.677721292346,-6.95,49.9710979935697));
#196160=CARTESIAN_POINT('',(120.620478318476,-6.95,50.2655860950994));
#196161=CARTESIAN_POINT('',(120.677721292346,-6.95,49.9710979935697));
#196162=CARTESIAN_POINT('',(120.129664815927,-6.95,50.1701811386501));
#196163=CARTESIAN_POINT('',(120.129664815927,-6.95,50.1701811386501));
#196164=CARTESIAN_POINT('',(120.186907789796,-6.95,49.8756930371204));
#196165=CARTESIAN_POINT('',(120.186907789796,-6.95,49.8756930371204));
#196166=CARTESIAN_POINT('',(120.186907789796,-6.95,49.8756930371204));
#196167=CARTESIAN_POINT('Origin',(120.677721292346,-6.95,49.9710979935697));
#196168=CARTESIAN_POINT('',(120.677721292346,-7.45,49.9710979935697));
#196169=CARTESIAN_POINT('',(120.620478318476,-7.45,50.2655860950994));
#196170=CARTESIAN_POINT('',(120.677721292346,-7.45,49.9710979935697));
#196171=CARTESIAN_POINT('',(120.620478318476,-6.95,50.2655860950994));
#196172=CARTESIAN_POINT('',(120.677721292346,-6.95,49.9710979935697));
#196173=CARTESIAN_POINT('Origin',(120.677721292346,-7.45,49.9710979935697));
#196174=CARTESIAN_POINT('',(120.186907789796,-7.45,49.8756930371204));
#196175=CARTESIAN_POINT('',(120.129664815927,-7.45,50.1701811386501));
#196176=CARTESIAN_POINT('',(120.186907789796,-7.45,49.8756930371204));
#196177=CARTESIAN_POINT('',(120.620478318476,-7.45,50.2655860950994));
#196178=CARTESIAN_POINT('',(120.677721292346,-7.45,49.9710979935697));
#196179=CARTESIAN_POINT('Origin',(120.186907789796,-7.45,49.8756930371204));
#196180=CARTESIAN_POINT('',(120.129664815927,-7.45,50.1701811386501));
#196181=CARTESIAN_POINT('',(120.186907789796,-7.45,49.8756930371204));
#196182=CARTESIAN_POINT('Origin',(120.972209393875,-6.95,50.0283409674392));
#196183=CARTESIAN_POINT('',(121.463022896425,-6.95,50.1237459238885));
#196184=CARTESIAN_POINT('',(121.405779922555,-6.95,50.4182340254182));
#196185=CARTESIAN_POINT('',(121.463022896425,-6.95,50.1237459238885));
#196186=CARTESIAN_POINT('',(120.914966420006,-6.95,50.3228290689689));
#196187=CARTESIAN_POINT('',(120.914966420006,-6.95,50.3228290689689));
#196188=CARTESIAN_POINT('',(120.972209393875,-6.95,50.0283409674392));
#196189=CARTESIAN_POINT('',(120.972209393875,-6.95,50.0283409674392));
#196190=CARTESIAN_POINT('',(120.972209393875,-6.95,50.0283409674392));
#196191=CARTESIAN_POINT('Origin',(121.463022896425,-6.95,50.1237459238885));
#196192=CARTESIAN_POINT('',(121.463022896425,-7.45,50.1237459238885));
#196193=CARTESIAN_POINT('',(121.405779922555,-7.45,50.4182340254182));
#196194=CARTESIAN_POINT('',(121.463022896425,-7.45,50.1237459238885));
#196195=CARTESIAN_POINT('',(121.405779922555,-6.95,50.4182340254182));
#196196=CARTESIAN_POINT('',(121.463022896425,-6.95,50.1237459238885));
#196197=CARTESIAN_POINT('Origin',(121.463022896425,-7.45,50.1237459238885));
#196198=CARTESIAN_POINT('',(120.972209393875,-7.45,50.0283409674392));
#196199=CARTESIAN_POINT('',(120.914966420006,-7.45,50.3228290689689));
#196200=CARTESIAN_POINT('',(120.972209393875,-7.45,50.0283409674392));
#196201=CARTESIAN_POINT('',(121.405779922555,-7.45,50.4182340254182));
#196202=CARTESIAN_POINT('',(121.463022896425,-7.45,50.1237459238885));
#196203=CARTESIAN_POINT('Origin',(120.972209393875,-7.45,50.0283409674392));
#196204=CARTESIAN_POINT('',(120.914966420006,-7.45,50.3228290689689));
#196205=CARTESIAN_POINT('',(120.972209393875,-7.45,50.0283409674392));
#196206=CARTESIAN_POINT('Origin',(121.757510997955,-6.95,50.180988897758));
#196207=CARTESIAN_POINT('',(122.248324500504,-6.95,50.2763938542073));
#196208=CARTESIAN_POINT('',(122.191081526635,-6.95,50.570881955737));
#196209=CARTESIAN_POINT('',(122.248324500504,-6.95,50.2763938542073));
#196210=CARTESIAN_POINT('',(121.700268024085,-6.95,50.4754769992877));
#196211=CARTESIAN_POINT('',(121.700268024085,-6.95,50.4754769992877));
#196212=CARTESIAN_POINT('',(121.757510997955,-6.95,50.180988897758));
#196213=CARTESIAN_POINT('',(121.757510997955,-6.95,50.180988897758));
#196214=CARTESIAN_POINT('',(121.757510997955,-6.95,50.180988897758));
#196215=CARTESIAN_POINT('Origin',(122.248324500504,-6.95,50.2763938542073));
#196216=CARTESIAN_POINT('',(122.248324500504,-7.45,50.2763938542073));
#196217=CARTESIAN_POINT('',(122.191081526635,-7.45,50.570881955737));
#196218=CARTESIAN_POINT('',(122.248324500504,-7.45,50.2763938542073));
#196219=CARTESIAN_POINT('',(122.191081526635,-6.95,50.570881955737));
#196220=CARTESIAN_POINT('',(122.248324500504,-6.95,50.2763938542073));
#196221=CARTESIAN_POINT('Origin',(122.248324500504,-7.45,50.2763938542073));
#196222=CARTESIAN_POINT('',(121.757510997955,-7.45,50.180988897758));
#196223=CARTESIAN_POINT('',(121.700268024085,-7.45,50.4754769992877));
#196224=CARTESIAN_POINT('',(121.757510997955,-7.45,50.180988897758));
#196225=CARTESIAN_POINT('',(122.191081526635,-7.45,50.570881955737));
#196226=CARTESIAN_POINT('',(122.248324500504,-7.45,50.2763938542073));
#196227=CARTESIAN_POINT('Origin',(121.757510997955,-7.45,50.180988897758));
#196228=CARTESIAN_POINT('',(121.700268024085,-7.45,50.4754769992877));
#196229=CARTESIAN_POINT('',(121.757510997955,-7.45,50.180988897758));
#196230=CARTESIAN_POINT('Origin',(122.542812602034,-6.95,50.3336368280768));
#196231=CARTESIAN_POINT('',(123.033626104583,-6.95,50.4290417845261));
#196232=CARTESIAN_POINT('',(122.976383130714,-6.95,50.7235298860558));
#196233=CARTESIAN_POINT('',(123.033626104583,-6.95,50.4290417845261));
#196234=CARTESIAN_POINT('',(122.485569628164,-6.95,50.6281249296065));
#196235=CARTESIAN_POINT('',(122.485569628164,-6.95,50.6281249296065));
#196236=CARTESIAN_POINT('',(122.542812602034,-6.95,50.3336368280768));
#196237=CARTESIAN_POINT('',(122.542812602034,-6.95,50.3336368280768));
#196238=CARTESIAN_POINT('',(122.542812602034,-6.95,50.3336368280768));
#196239=CARTESIAN_POINT('Origin',(123.033626104583,-6.95,50.4290417845261));
#196240=CARTESIAN_POINT('',(123.033626104583,-7.45,50.4290417845261));
#196241=CARTESIAN_POINT('',(122.976383130714,-7.45,50.7235298860558));
#196242=CARTESIAN_POINT('',(123.033626104583,-7.45,50.4290417845261));
#196243=CARTESIAN_POINT('',(122.976383130714,-6.95,50.7235298860558));
#196244=CARTESIAN_POINT('',(123.033626104583,-6.95,50.4290417845261));
#196245=CARTESIAN_POINT('Origin',(123.033626104583,-7.45,50.4290417845261));
#196246=CARTESIAN_POINT('',(122.542812602034,-7.45,50.3336368280768));
#196247=CARTESIAN_POINT('',(122.485569628164,-7.45,50.6281249296065));
#196248=CARTESIAN_POINT('',(122.542812602034,-7.45,50.3336368280768));
#196249=CARTESIAN_POINT('',(122.976383130714,-7.45,50.7235298860558));
#196250=CARTESIAN_POINT('',(123.033626104583,-7.45,50.4290417845261));
#196251=CARTESIAN_POINT('Origin',(122.542812602034,-7.45,50.3336368280768));
#196252=CARTESIAN_POINT('',(122.485569628164,-7.45,50.6281249296065));
#196253=CARTESIAN_POINT('',(122.542812602034,-7.45,50.3336368280768));
#196254=CARTESIAN_POINT('Origin',(124.113415810192,-5.35,50.6389326887144));
#196255=CARTESIAN_POINT('',(124.604229312742,-5.35,50.7343376451637));
#196256=CARTESIAN_POINT('',(124.546986338872,-5.35,51.0288257466934));
#196257=CARTESIAN_POINT('',(124.604229312742,-5.35,50.7343376451637));
#196258=CARTESIAN_POINT('',(124.056172836323,-5.35,50.9334207902441));
#196259=CARTESIAN_POINT('',(124.056172836323,-5.35,50.9334207902441));
#196260=CARTESIAN_POINT('',(124.113415810192,-5.35,50.6389326887144));
#196261=CARTESIAN_POINT('',(124.113415810192,-5.35,50.6389326887144));
#196262=CARTESIAN_POINT('',(124.113415810192,-5.35,50.6389326887144));
#196263=CARTESIAN_POINT('Origin',(124.604229312742,-5.35,50.7343376451637));
#196264=CARTESIAN_POINT('',(124.604229312742,-5.85,50.7343376451637));
#196265=CARTESIAN_POINT('',(124.546986338872,-5.85,51.0288257466934));
#196266=CARTESIAN_POINT('',(124.604229312742,-5.85,50.7343376451637));
#196267=CARTESIAN_POINT('',(124.546986338872,-5.35,51.0288257466934));
#196268=CARTESIAN_POINT('',(124.604229312742,-5.35,50.7343376451637));
#196269=CARTESIAN_POINT('Origin',(124.604229312742,-5.85,50.7343376451637));
#196270=CARTESIAN_POINT('',(124.113415810192,-5.85,50.6389326887144));
#196271=CARTESIAN_POINT('',(124.056172836323,-5.85,50.9334207902441));
#196272=CARTESIAN_POINT('',(124.113415810192,-5.85,50.6389326887144));
#196273=CARTESIAN_POINT('',(124.546986338872,-5.85,51.0288257466934));
#196274=CARTESIAN_POINT('',(124.604229312742,-5.85,50.7343376451637));
#196275=CARTESIAN_POINT('Origin',(124.113415810192,-5.85,50.6389326887144));
#196276=CARTESIAN_POINT('',(124.056172836323,-5.85,50.9334207902441));
#196277=CARTESIAN_POINT('',(124.113415810192,-5.85,50.6389326887144));
#196278=CARTESIAN_POINT('Origin',(124.113415810192,-4.55,50.6389326887144));
#196279=CARTESIAN_POINT('',(124.604229312742,-4.55,50.7343376451637));
#196280=CARTESIAN_POINT('',(124.546986338872,-4.55,51.0288257466934));
#196281=CARTESIAN_POINT('',(124.604229312742,-4.55,50.7343376451637));
#196282=CARTESIAN_POINT('',(124.056172836323,-4.55,50.9334207902441));
#196283=CARTESIAN_POINT('',(124.056172836323,-4.55,50.9334207902441));
#196284=CARTESIAN_POINT('',(124.113415810192,-4.55,50.6389326887144));
#196285=CARTESIAN_POINT('',(124.113415810192,-4.55,50.6389326887144));
#196286=CARTESIAN_POINT('',(124.113415810192,-4.55,50.6389326887144));
#196287=CARTESIAN_POINT('Origin',(124.604229312742,-4.55,50.7343376451637));
#196288=CARTESIAN_POINT('',(124.604229312742,-5.05,50.7343376451637));
#196289=CARTESIAN_POINT('',(124.546986338872,-5.05,51.0288257466934));
#196290=CARTESIAN_POINT('',(124.604229312742,-5.05,50.7343376451637));
#196291=CARTESIAN_POINT('',(124.546986338872,-4.55,51.0288257466934));
#196292=CARTESIAN_POINT('',(124.604229312742,-4.55,50.7343376451637));
#196293=CARTESIAN_POINT('Origin',(124.604229312742,-5.05,50.7343376451637));
#196294=CARTESIAN_POINT('',(124.113415810192,-5.05,50.6389326887144));
#196295=CARTESIAN_POINT('',(124.056172836323,-5.05,50.9334207902441));
#196296=CARTESIAN_POINT('',(124.113415810192,-5.05,50.6389326887144));
#196297=CARTESIAN_POINT('',(124.546986338872,-5.05,51.0288257466934));
#196298=CARTESIAN_POINT('',(124.604229312742,-5.05,50.7343376451637));
#196299=CARTESIAN_POINT('Origin',(124.113415810192,-5.05,50.6389326887144));
#196300=CARTESIAN_POINT('',(124.056172836323,-5.05,50.9334207902441));
#196301=CARTESIAN_POINT('',(124.113415810192,-5.05,50.6389326887144));
#196302=CARTESIAN_POINT('Origin',(124.113415810192,-3.75,50.6389326887144));
#196303=CARTESIAN_POINT('',(124.604229312742,-3.75,50.7343376451637));
#196304=CARTESIAN_POINT('',(124.546986338872,-3.75,51.0288257466934));
#196305=CARTESIAN_POINT('',(124.604229312742,-3.75,50.7343376451637));
#196306=CARTESIAN_POINT('',(124.056172836323,-3.75,50.9334207902441));
#196307=CARTESIAN_POINT('',(124.056172836323,-3.75,50.9334207902441));
#196308=CARTESIAN_POINT('',(124.113415810192,-3.75,50.6389326887144));
#196309=CARTESIAN_POINT('',(124.113415810192,-3.75,50.6389326887144));
#196310=CARTESIAN_POINT('',(124.113415810192,-3.75,50.6389326887144));
#196311=CARTESIAN_POINT('Origin',(124.604229312742,-3.75,50.7343376451637));
#196312=CARTESIAN_POINT('',(124.604229312742,-4.25,50.7343376451637));
#196313=CARTESIAN_POINT('',(124.546986338872,-4.25,51.0288257466934));
#196314=CARTESIAN_POINT('',(124.604229312742,-4.25,50.7343376451637));
#196315=CARTESIAN_POINT('',(124.546986338872,-3.75,51.0288257466934));
#196316=CARTESIAN_POINT('',(124.604229312742,-3.75,50.7343376451637));
#196317=CARTESIAN_POINT('Origin',(124.604229312742,-4.25,50.7343376451637));
#196318=CARTESIAN_POINT('',(124.113415810192,-4.25,50.6389326887144));
#196319=CARTESIAN_POINT('',(124.056172836323,-4.25,50.9334207902441));
#196320=CARTESIAN_POINT('',(124.113415810192,-4.25,50.6389326887144));
#196321=CARTESIAN_POINT('',(124.546986338872,-4.25,51.0288257466934));
#196322=CARTESIAN_POINT('',(124.604229312742,-4.25,50.7343376451637));
#196323=CARTESIAN_POINT('Origin',(124.113415810192,-4.25,50.6389326887144));
#196324=CARTESIAN_POINT('',(124.056172836323,-4.25,50.9334207902441));
#196325=CARTESIAN_POINT('',(124.113415810192,-4.25,50.6389326887144));
#196326=CARTESIAN_POINT('Origin',(124.113415810192,-2.95,50.6389326887144));
#196327=CARTESIAN_POINT('',(124.604229312742,-2.95,50.7343376451637));
#196328=CARTESIAN_POINT('',(124.546986338872,-2.95,51.0288257466934));
#196329=CARTESIAN_POINT('',(124.604229312742,-2.95,50.7343376451637));
#196330=CARTESIAN_POINT('',(124.056172836323,-2.95,50.9334207902441));
#196331=CARTESIAN_POINT('',(124.056172836323,-2.95,50.9334207902441));
#196332=CARTESIAN_POINT('',(124.113415810192,-2.95,50.6389326887144));
#196333=CARTESIAN_POINT('',(124.113415810192,-2.95,50.6389326887144));
#196334=CARTESIAN_POINT('',(124.113415810192,-2.95,50.6389326887144));
#196335=CARTESIAN_POINT('Origin',(124.604229312742,-2.95,50.7343376451637));
#196336=CARTESIAN_POINT('',(124.604229312742,-3.45,50.7343376451637));
#196337=CARTESIAN_POINT('',(124.546986338872,-3.45,51.0288257466934));
#196338=CARTESIAN_POINT('',(124.604229312742,-3.45,50.7343376451637));
#196339=CARTESIAN_POINT('',(124.546986338872,-2.95,51.0288257466934));
#196340=CARTESIAN_POINT('',(124.604229312742,-2.95,50.7343376451637));
#196341=CARTESIAN_POINT('Origin',(124.604229312742,-3.45,50.7343376451637));
#196342=CARTESIAN_POINT('',(124.113415810192,-3.45,50.6389326887144));
#196343=CARTESIAN_POINT('',(124.056172836323,-3.45,50.9334207902441));
#196344=CARTESIAN_POINT('',(124.113415810192,-3.45,50.6389326887144));
#196345=CARTESIAN_POINT('',(124.546986338872,-3.45,51.0288257466934));
#196346=CARTESIAN_POINT('',(124.604229312742,-3.45,50.7343376451637));
#196347=CARTESIAN_POINT('Origin',(124.113415810192,-3.45,50.6389326887144));
#196348=CARTESIAN_POINT('',(124.056172836323,-3.45,50.9334207902441));
#196349=CARTESIAN_POINT('',(124.113415810192,-3.45,50.6389326887144));
#196350=CARTESIAN_POINT('Origin',(124.113415810192,-2.15,50.6389326887144));
#196351=CARTESIAN_POINT('',(124.604229312742,-2.15,50.7343376451637));
#196352=CARTESIAN_POINT('',(124.546986338872,-2.15,51.0288257466934));
#196353=CARTESIAN_POINT('',(124.604229312742,-2.15,50.7343376451637));
#196354=CARTESIAN_POINT('',(124.056172836323,-2.15,50.9334207902441));
#196355=CARTESIAN_POINT('',(124.056172836323,-2.15,50.9334207902441));
#196356=CARTESIAN_POINT('',(124.113415810192,-2.15,50.6389326887144));
#196357=CARTESIAN_POINT('',(124.113415810192,-2.15,50.6389326887144));
#196358=CARTESIAN_POINT('',(124.113415810192,-2.15,50.6389326887144));
#196359=CARTESIAN_POINT('Origin',(124.604229312742,-2.15,50.7343376451637));
#196360=CARTESIAN_POINT('',(124.604229312742,-2.65,50.7343376451637));
#196361=CARTESIAN_POINT('',(124.546986338872,-2.65,51.0288257466934));
#196362=CARTESIAN_POINT('',(124.604229312742,-2.65,50.7343376451637));
#196363=CARTESIAN_POINT('',(124.546986338872,-2.15,51.0288257466934));
#196364=CARTESIAN_POINT('',(124.604229312742,-2.15,50.7343376451637));
#196365=CARTESIAN_POINT('Origin',(124.604229312742,-2.65,50.7343376451637));
#196366=CARTESIAN_POINT('',(124.113415810192,-2.65,50.6389326887144));
#196367=CARTESIAN_POINT('',(124.056172836323,-2.65,50.9334207902441));
#196368=CARTESIAN_POINT('',(124.113415810192,-2.65,50.6389326887144));
#196369=CARTESIAN_POINT('',(124.546986338872,-2.65,51.0288257466934));
#196370=CARTESIAN_POINT('',(124.604229312742,-2.65,50.7343376451637));
#196371=CARTESIAN_POINT('Origin',(124.113415810192,-2.65,50.6389326887144));
#196372=CARTESIAN_POINT('',(124.056172836323,-2.65,50.9334207902441));
#196373=CARTESIAN_POINT('',(124.113415810192,-2.65,50.6389326887144));
#196374=CARTESIAN_POINT('Origin',(124.113415810192,-1.35,50.6389326887144));
#196375=CARTESIAN_POINT('',(124.604229312742,-1.35,50.7343376451637));
#196376=CARTESIAN_POINT('',(124.546986338872,-1.35,51.0288257466934));
#196377=CARTESIAN_POINT('',(124.604229312742,-1.35,50.7343376451637));
#196378=CARTESIAN_POINT('',(124.056172836323,-1.35,50.9334207902441));
#196379=CARTESIAN_POINT('',(124.056172836323,-1.35,50.9334207902441));
#196380=CARTESIAN_POINT('',(124.113415810192,-1.35,50.6389326887144));
#196381=CARTESIAN_POINT('',(124.113415810192,-1.35,50.6389326887144));
#196382=CARTESIAN_POINT('',(124.113415810192,-1.35,50.6389326887144));
#196383=CARTESIAN_POINT('Origin',(124.604229312742,-1.35,50.7343376451637));
#196384=CARTESIAN_POINT('',(124.604229312742,-1.85,50.7343376451637));
#196385=CARTESIAN_POINT('',(124.546986338872,-1.85,51.0288257466934));
#196386=CARTESIAN_POINT('',(124.604229312742,-1.85,50.7343376451637));
#196387=CARTESIAN_POINT('',(124.546986338872,-1.35,51.0288257466934));
#196388=CARTESIAN_POINT('',(124.604229312742,-1.35,50.7343376451637));
#196389=CARTESIAN_POINT('Origin',(124.604229312742,-1.85,50.7343376451637));
#196390=CARTESIAN_POINT('',(124.113415810192,-1.85,50.6389326887144));
#196391=CARTESIAN_POINT('',(124.056172836323,-1.85,50.9334207902441));
#196392=CARTESIAN_POINT('',(124.113415810192,-1.85,50.6389326887144));
#196393=CARTESIAN_POINT('',(124.546986338872,-1.85,51.0288257466934));
#196394=CARTESIAN_POINT('',(124.604229312742,-1.85,50.7343376451637));
#196395=CARTESIAN_POINT('Origin',(124.113415810192,-1.85,50.6389326887144));
#196396=CARTESIAN_POINT('',(124.056172836323,-1.85,50.9334207902441));
#196397=CARTESIAN_POINT('',(124.113415810192,-1.85,50.6389326887144));
#196398=CARTESIAN_POINT('Origin',(124.113415810192,-0.549999999999986,50.6389326887144));
#196399=CARTESIAN_POINT('',(124.604229312742,-0.549999999999986,50.7343376451637));
#196400=CARTESIAN_POINT('',(124.546986338872,-0.549999999999986,51.0288257466934));
#196401=CARTESIAN_POINT('',(124.604229312742,-0.549999999999986,50.7343376451637));
#196402=CARTESIAN_POINT('',(124.056172836323,-0.549999999999986,50.9334207902441));
#196403=CARTESIAN_POINT('',(124.056172836323,-0.549999999999986,50.9334207902441));
#196404=CARTESIAN_POINT('',(124.113415810192,-0.549999999999986,50.6389326887144));
#196405=CARTESIAN_POINT('',(124.113415810192,-0.549999999999986,50.6389326887144));
#196406=CARTESIAN_POINT('',(124.113415810192,-0.549999999999986,50.6389326887144));
#196407=CARTESIAN_POINT('Origin',(124.604229312742,-0.549999999999986,50.7343376451637));
#196408=CARTESIAN_POINT('',(124.604229312742,-1.05,50.7343376451637));
#196409=CARTESIAN_POINT('',(124.546986338872,-1.05,51.0288257466934));
#196410=CARTESIAN_POINT('',(124.604229312742,-1.05,50.7343376451637));
#196411=CARTESIAN_POINT('',(124.546986338872,-0.549999999999986,51.0288257466934));
#196412=CARTESIAN_POINT('',(124.604229312742,-0.549999999999986,50.7343376451637));
#196413=CARTESIAN_POINT('Origin',(124.604229312742,-1.05,50.7343376451637));
#196414=CARTESIAN_POINT('',(124.113415810192,-1.05,50.6389326887144));
#196415=CARTESIAN_POINT('',(124.056172836323,-1.05,50.9334207902441));
#196416=CARTESIAN_POINT('',(124.113415810192,-1.05,50.6389326887144));
#196417=CARTESIAN_POINT('',(124.546986338872,-1.05,51.0288257466934));
#196418=CARTESIAN_POINT('',(124.604229312742,-1.05,50.7343376451637));
#196419=CARTESIAN_POINT('Origin',(124.113415810192,-1.05,50.6389326887144));
#196420=CARTESIAN_POINT('',(124.056172836323,-1.05,50.9334207902441));
#196421=CARTESIAN_POINT('',(124.113415810192,-1.05,50.6389326887144));
#196422=CARTESIAN_POINT('Origin',(124.113415810192,0.250000000000015,50.6389326887144));
#196423=CARTESIAN_POINT('',(124.604229312742,0.250000000000015,50.7343376451637));
#196424=CARTESIAN_POINT('',(124.546986338872,0.250000000000015,51.0288257466934));
#196425=CARTESIAN_POINT('',(124.604229312742,0.250000000000015,50.7343376451637));
#196426=CARTESIAN_POINT('',(124.056172836323,0.250000000000015,50.9334207902441));
#196427=CARTESIAN_POINT('',(124.056172836323,0.250000000000015,50.9334207902441));
#196428=CARTESIAN_POINT('',(124.113415810192,0.250000000000015,50.6389326887144));
#196429=CARTESIAN_POINT('',(124.113415810192,0.250000000000015,50.6389326887144));
#196430=CARTESIAN_POINT('',(124.113415810192,0.250000000000015,50.6389326887144));
#196431=CARTESIAN_POINT('Origin',(124.604229312742,0.250000000000015,50.7343376451637));
#196432=CARTESIAN_POINT('',(124.604229312742,-0.249999999999985,50.7343376451637));
#196433=CARTESIAN_POINT('',(124.546986338872,-0.249999999999985,51.0288257466934));
#196434=CARTESIAN_POINT('',(124.604229312742,-0.249999999999985,50.7343376451637));
#196435=CARTESIAN_POINT('',(124.546986338872,0.250000000000015,51.0288257466934));
#196436=CARTESIAN_POINT('',(124.604229312742,0.250000000000015,50.7343376451637));
#196437=CARTESIAN_POINT('Origin',(124.604229312742,-0.249999999999985,50.7343376451637));
#196438=CARTESIAN_POINT('',(124.113415810192,-0.249999999999985,50.6389326887144));
#196439=CARTESIAN_POINT('',(124.056172836323,-0.249999999999985,50.9334207902441));
#196440=CARTESIAN_POINT('',(124.113415810192,-0.249999999999985,50.6389326887144));
#196441=CARTESIAN_POINT('',(124.546986338872,-0.249999999999985,51.0288257466934));
#196442=CARTESIAN_POINT('',(124.604229312742,-0.249999999999985,50.7343376451637));
#196443=CARTESIAN_POINT('Origin',(124.113415810192,-0.249999999999985,50.6389326887144));
#196444=CARTESIAN_POINT('',(124.056172836323,-0.249999999999985,50.9334207902441));
#196445=CARTESIAN_POINT('',(124.113415810192,-0.249999999999985,50.6389326887144));
#196446=CARTESIAN_POINT('Origin',(124.113415810192,1.05,50.6389326887144));
#196447=CARTESIAN_POINT('',(124.604229312742,1.05,50.7343376451637));
#196448=CARTESIAN_POINT('',(124.546986338872,1.05,51.0288257466934));
#196449=CARTESIAN_POINT('',(124.604229312742,1.05,50.7343376451637));
#196450=CARTESIAN_POINT('',(124.056172836323,1.05,50.9334207902441));
#196451=CARTESIAN_POINT('',(124.056172836323,1.05,50.9334207902441));
#196452=CARTESIAN_POINT('',(124.113415810192,1.05,50.6389326887144));
#196453=CARTESIAN_POINT('',(124.113415810192,1.05,50.6389326887144));
#196454=CARTESIAN_POINT('',(124.113415810192,1.05,50.6389326887144));
#196455=CARTESIAN_POINT('Origin',(124.604229312742,1.05,50.7343376451637));
#196456=CARTESIAN_POINT('',(124.604229312742,0.550000000000015,50.7343376451637));
#196457=CARTESIAN_POINT('',(124.546986338872,0.550000000000015,51.0288257466934));
#196458=CARTESIAN_POINT('',(124.604229312742,0.550000000000015,50.7343376451637));
#196459=CARTESIAN_POINT('',(124.546986338872,1.05,51.0288257466934));
#196460=CARTESIAN_POINT('',(124.604229312742,1.05,50.7343376451637));
#196461=CARTESIAN_POINT('Origin',(124.604229312742,0.550000000000015,50.7343376451637));
#196462=CARTESIAN_POINT('',(124.113415810192,0.550000000000015,50.6389326887144));
#196463=CARTESIAN_POINT('',(124.056172836323,0.550000000000015,50.9334207902441));
#196464=CARTESIAN_POINT('',(124.113415810192,0.550000000000015,50.6389326887144));
#196465=CARTESIAN_POINT('',(124.546986338872,0.550000000000015,51.0288257466934));
#196466=CARTESIAN_POINT('',(124.604229312742,0.550000000000015,50.7343376451637));
#196467=CARTESIAN_POINT('Origin',(124.113415810192,0.550000000000015,50.6389326887144));
#196468=CARTESIAN_POINT('',(124.056172836323,0.550000000000015,50.9334207902441));
#196469=CARTESIAN_POINT('',(124.113415810192,0.550000000000015,50.6389326887144));
#196470=CARTESIAN_POINT('Origin',(124.113415810192,1.85,50.6389326887144));
#196471=CARTESIAN_POINT('',(124.604229312742,1.85,50.7343376451637));
#196472=CARTESIAN_POINT('',(124.546986338872,1.85,51.0288257466934));
#196473=CARTESIAN_POINT('',(124.604229312742,1.85,50.7343376451637));
#196474=CARTESIAN_POINT('',(124.056172836323,1.85,50.9334207902441));
#196475=CARTESIAN_POINT('',(124.056172836323,1.85,50.9334207902441));
#196476=CARTESIAN_POINT('',(124.113415810192,1.85,50.6389326887144));
#196477=CARTESIAN_POINT('',(124.113415810192,1.85,50.6389326887144));
#196478=CARTESIAN_POINT('',(124.113415810192,1.85,50.6389326887144));
#196479=CARTESIAN_POINT('Origin',(124.604229312742,1.85,50.7343376451637));
#196480=CARTESIAN_POINT('',(124.604229312742,1.35,50.7343376451637));
#196481=CARTESIAN_POINT('',(124.546986338872,1.35,51.0288257466934));
#196482=CARTESIAN_POINT('',(124.604229312742,1.35,50.7343376451637));
#196483=CARTESIAN_POINT('',(124.546986338872,1.85,51.0288257466934));
#196484=CARTESIAN_POINT('',(124.604229312742,1.85,50.7343376451637));
#196485=CARTESIAN_POINT('Origin',(124.604229312742,1.35,50.7343376451637));
#196486=CARTESIAN_POINT('',(124.113415810192,1.35,50.6389326887144));
#196487=CARTESIAN_POINT('',(124.056172836323,1.35,50.9334207902441));
#196488=CARTESIAN_POINT('',(124.113415810192,1.35,50.6389326887144));
#196489=CARTESIAN_POINT('',(124.546986338872,1.35,51.0288257466934));
#196490=CARTESIAN_POINT('',(124.604229312742,1.35,50.7343376451637));
#196491=CARTESIAN_POINT('Origin',(124.113415810192,1.35,50.6389326887144));
#196492=CARTESIAN_POINT('',(124.056172836323,1.35,50.9334207902441));
#196493=CARTESIAN_POINT('',(124.113415810192,1.35,50.6389326887144));
#196494=CARTESIAN_POINT('Origin',(124.113415810192,2.65,50.6389326887144));
#196495=CARTESIAN_POINT('',(124.604229312742,2.65,50.7343376451637));
#196496=CARTESIAN_POINT('',(124.546986338872,2.65,51.0288257466934));
#196497=CARTESIAN_POINT('',(124.604229312742,2.65,50.7343376451637));
#196498=CARTESIAN_POINT('',(124.056172836323,2.65,50.9334207902441));
#196499=CARTESIAN_POINT('',(124.056172836323,2.65,50.9334207902441));
#196500=CARTESIAN_POINT('',(124.113415810192,2.65,50.6389326887144));
#196501=CARTESIAN_POINT('',(124.113415810192,2.65,50.6389326887144));
#196502=CARTESIAN_POINT('',(124.113415810192,2.65,50.6389326887144));
#196503=CARTESIAN_POINT('Origin',(124.604229312742,2.65,50.7343376451637));
#196504=CARTESIAN_POINT('',(124.604229312742,2.15,50.7343376451637));
#196505=CARTESIAN_POINT('',(124.546986338872,2.15,51.0288257466934));
#196506=CARTESIAN_POINT('',(124.604229312742,2.15,50.7343376451637));
#196507=CARTESIAN_POINT('',(124.546986338872,2.65,51.0288257466934));
#196508=CARTESIAN_POINT('',(124.604229312742,2.65,50.7343376451637));
#196509=CARTESIAN_POINT('Origin',(124.604229312742,2.15,50.7343376451637));
#196510=CARTESIAN_POINT('',(124.113415810192,2.15,50.6389326887144));
#196511=CARTESIAN_POINT('',(124.056172836323,2.15,50.9334207902441));
#196512=CARTESIAN_POINT('',(124.113415810192,2.15,50.6389326887144));
#196513=CARTESIAN_POINT('',(124.546986338872,2.15,51.0288257466934));
#196514=CARTESIAN_POINT('',(124.604229312742,2.15,50.7343376451637));
#196515=CARTESIAN_POINT('Origin',(124.113415810192,2.15,50.6389326887144));
#196516=CARTESIAN_POINT('',(124.056172836323,2.15,50.9334207902441));
#196517=CARTESIAN_POINT('',(124.113415810192,2.15,50.6389326887144));
#196518=CARTESIAN_POINT('Origin',(124.113415810192,3.45,50.6389326887144));
#196519=CARTESIAN_POINT('',(124.604229312742,3.45,50.7343376451637));
#196520=CARTESIAN_POINT('',(124.546986338872,3.45,51.0288257466934));
#196521=CARTESIAN_POINT('',(124.604229312742,3.45,50.7343376451637));
#196522=CARTESIAN_POINT('',(124.056172836323,3.45,50.9334207902441));
#196523=CARTESIAN_POINT('',(124.056172836323,3.45,50.9334207902441));
#196524=CARTESIAN_POINT('',(124.113415810192,3.45,50.6389326887144));
#196525=CARTESIAN_POINT('',(124.113415810192,3.45,50.6389326887144));
#196526=CARTESIAN_POINT('',(124.113415810192,3.45,50.6389326887144));
#196527=CARTESIAN_POINT('Origin',(124.604229312742,3.45,50.7343376451637));
#196528=CARTESIAN_POINT('',(124.604229312742,2.95,50.7343376451637));
#196529=CARTESIAN_POINT('',(124.546986338872,2.95,51.0288257466934));
#196530=CARTESIAN_POINT('',(124.604229312742,2.95,50.7343376451637));
#196531=CARTESIAN_POINT('',(124.546986338872,3.45,51.0288257466934));
#196532=CARTESIAN_POINT('',(124.604229312742,3.45,50.7343376451637));
#196533=CARTESIAN_POINT('Origin',(124.604229312742,2.95,50.7343376451637));
#196534=CARTESIAN_POINT('',(124.113415810192,2.95,50.6389326887144));
#196535=CARTESIAN_POINT('',(124.056172836323,2.95,50.9334207902441));
#196536=CARTESIAN_POINT('',(124.113415810192,2.95,50.6389326887144));
#196537=CARTESIAN_POINT('',(124.546986338872,2.95,51.0288257466934));
#196538=CARTESIAN_POINT('',(124.604229312742,2.95,50.7343376451637));
#196539=CARTESIAN_POINT('Origin',(124.113415810192,2.95,50.6389326887144));
#196540=CARTESIAN_POINT('',(124.056172836323,2.95,50.9334207902441));
#196541=CARTESIAN_POINT('',(124.113415810192,2.95,50.6389326887144));
#196542=CARTESIAN_POINT('Origin',(124.113415810192,4.25,50.6389326887144));
#196543=CARTESIAN_POINT('',(124.604229312742,4.25,50.7343376451637));
#196544=CARTESIAN_POINT('',(124.546986338872,4.25,51.0288257466934));
#196545=CARTESIAN_POINT('',(124.604229312742,4.25,50.7343376451637));
#196546=CARTESIAN_POINT('',(124.056172836323,4.25,50.9334207902441));
#196547=CARTESIAN_POINT('',(124.056172836323,4.25,50.9334207902441));
#196548=CARTESIAN_POINT('',(124.113415810192,4.25,50.6389326887144));
#196549=CARTESIAN_POINT('',(124.113415810192,4.25,50.6389326887144));
#196550=CARTESIAN_POINT('',(124.113415810192,4.25,50.6389326887144));
#196551=CARTESIAN_POINT('Origin',(124.604229312742,4.25,50.7343376451637));
#196552=CARTESIAN_POINT('',(124.604229312742,3.75,50.7343376451637));
#196553=CARTESIAN_POINT('',(124.546986338872,3.75,51.0288257466934));
#196554=CARTESIAN_POINT('',(124.604229312742,3.75,50.7343376451637));
#196555=CARTESIAN_POINT('',(124.546986338872,4.25,51.0288257466934));
#196556=CARTESIAN_POINT('',(124.604229312742,4.25,50.7343376451637));
#196557=CARTESIAN_POINT('Origin',(124.604229312742,3.75,50.7343376451637));
#196558=CARTESIAN_POINT('',(124.113415810192,3.75,50.6389326887144));
#196559=CARTESIAN_POINT('',(124.056172836323,3.75,50.9334207902441));
#196560=CARTESIAN_POINT('',(124.113415810192,3.75,50.6389326887144));
#196561=CARTESIAN_POINT('',(124.546986338872,3.75,51.0288257466934));
#196562=CARTESIAN_POINT('',(124.604229312742,3.75,50.7343376451637));
#196563=CARTESIAN_POINT('Origin',(124.113415810192,3.75,50.6389326887144));
#196564=CARTESIAN_POINT('',(124.056172836323,3.75,50.9334207902441));
#196565=CARTESIAN_POINT('',(124.113415810192,3.75,50.6389326887144));
#196566=CARTESIAN_POINT('Origin',(124.113415810192,5.05,50.6389326887144));
#196567=CARTESIAN_POINT('',(124.604229312742,5.05,50.7343376451637));
#196568=CARTESIAN_POINT('',(124.546986338872,5.05,51.0288257466934));
#196569=CARTESIAN_POINT('',(124.604229312742,5.05,50.7343376451637));
#196570=CARTESIAN_POINT('',(124.056172836323,5.05,50.9334207902441));
#196571=CARTESIAN_POINT('',(124.056172836323,5.05,50.9334207902441));
#196572=CARTESIAN_POINT('',(124.113415810192,5.05,50.6389326887144));
#196573=CARTESIAN_POINT('',(124.113415810192,5.05,50.6389326887144));
#196574=CARTESIAN_POINT('',(124.113415810192,5.05,50.6389326887144));
#196575=CARTESIAN_POINT('Origin',(124.604229312742,5.05,50.7343376451637));
#196576=CARTESIAN_POINT('',(124.604229312742,4.55,50.7343376451637));
#196577=CARTESIAN_POINT('',(124.546986338872,4.55,51.0288257466934));
#196578=CARTESIAN_POINT('',(124.604229312742,4.55,50.7343376451637));
#196579=CARTESIAN_POINT('',(124.546986338872,5.05,51.0288257466934));
#196580=CARTESIAN_POINT('',(124.604229312742,5.05,50.7343376451637));
#196581=CARTESIAN_POINT('Origin',(124.604229312742,4.55,50.7343376451637));
#196582=CARTESIAN_POINT('',(124.113415810192,4.55,50.6389326887144));
#196583=CARTESIAN_POINT('',(124.056172836323,4.55,50.9334207902441));
#196584=CARTESIAN_POINT('',(124.113415810192,4.55,50.6389326887144));
#196585=CARTESIAN_POINT('',(124.546986338872,4.55,51.0288257466934));
#196586=CARTESIAN_POINT('',(124.604229312742,4.55,50.7343376451637));
#196587=CARTESIAN_POINT('Origin',(124.113415810192,4.55,50.6389326887144));
#196588=CARTESIAN_POINT('',(124.056172836323,4.55,50.9334207902441));
#196589=CARTESIAN_POINT('',(124.113415810192,4.55,50.6389326887144));
#196590=CARTESIAN_POINT('Origin',(124.113415810192,5.85,50.6389326887144));
#196591=CARTESIAN_POINT('',(124.604229312742,5.85,50.7343376451637));
#196592=CARTESIAN_POINT('',(124.546986338872,5.85,51.0288257466934));
#196593=CARTESIAN_POINT('',(124.604229312742,5.85,50.7343376451637));
#196594=CARTESIAN_POINT('',(124.056172836323,5.85,50.9334207902441));
#196595=CARTESIAN_POINT('',(124.056172836323,5.85,50.9334207902441));
#196596=CARTESIAN_POINT('',(124.113415810192,5.85,50.6389326887144));
#196597=CARTESIAN_POINT('',(124.113415810192,5.85,50.6389326887144));
#196598=CARTESIAN_POINT('',(124.113415810192,5.85,50.6389326887144));
#196599=CARTESIAN_POINT('Origin',(124.604229312742,5.85,50.7343376451637));
#196600=CARTESIAN_POINT('',(124.604229312742,5.35,50.7343376451637));
#196601=CARTESIAN_POINT('',(124.546986338872,5.35,51.0288257466934));
#196602=CARTESIAN_POINT('',(124.604229312742,5.35,50.7343376451637));
#196603=CARTESIAN_POINT('',(124.546986338872,5.85,51.0288257466934));
#196604=CARTESIAN_POINT('',(124.604229312742,5.85,50.7343376451637));
#196605=CARTESIAN_POINT('Origin',(124.604229312742,5.35,50.7343376451637));
#196606=CARTESIAN_POINT('',(124.113415810192,5.35,50.6389326887144));
#196607=CARTESIAN_POINT('',(124.056172836323,5.35,50.9334207902441));
#196608=CARTESIAN_POINT('',(124.113415810192,5.35,50.6389326887144));
#196609=CARTESIAN_POINT('',(124.546986338872,5.35,51.0288257466934));
#196610=CARTESIAN_POINT('',(124.604229312742,5.35,50.7343376451637));
#196611=CARTESIAN_POINT('Origin',(124.113415810192,5.35,50.6389326887144));
#196612=CARTESIAN_POINT('',(124.056172836323,5.35,50.9334207902441));
#196613=CARTESIAN_POINT('',(124.113415810192,5.35,50.6389326887144));
#196614=CARTESIAN_POINT('Origin',(122.542812602034,7.45,50.3336368280768));
#196615=CARTESIAN_POINT('',(123.033626104583,7.45,50.4290417845261));
#196616=CARTESIAN_POINT('',(122.976383130714,7.45,50.7235298860558));
#196617=CARTESIAN_POINT('',(123.033626104583,7.45,50.4290417845261));
#196618=CARTESIAN_POINT('',(122.485569628164,7.45,50.6281249296065));
#196619=CARTESIAN_POINT('',(122.485569628164,7.45,50.6281249296065));
#196620=CARTESIAN_POINT('',(122.542812602034,7.45,50.3336368280768));
#196621=CARTESIAN_POINT('',(122.542812602034,7.45,50.3336368280768));
#196622=CARTESIAN_POINT('',(122.542812602034,7.45,50.3336368280768));
#196623=CARTESIAN_POINT('Origin',(123.033626104583,7.45,50.4290417845261));
#196624=CARTESIAN_POINT('',(123.033626104583,6.95,50.4290417845261));
#196625=CARTESIAN_POINT('',(122.976383130714,6.95,50.7235298860558));
#196626=CARTESIAN_POINT('',(123.033626104583,6.95,50.4290417845261));
#196627=CARTESIAN_POINT('',(122.976383130714,7.45,50.7235298860558));
#196628=CARTESIAN_POINT('',(123.033626104583,7.45,50.4290417845261));
#196629=CARTESIAN_POINT('Origin',(123.033626104583,6.95,50.4290417845261));
#196630=CARTESIAN_POINT('',(122.542812602034,6.95,50.3336368280768));
#196631=CARTESIAN_POINT('',(122.485569628164,6.95,50.6281249296065));
#196632=CARTESIAN_POINT('',(122.542812602034,6.95,50.3336368280768));
#196633=CARTESIAN_POINT('',(122.976383130714,6.95,50.7235298860558));
#196634=CARTESIAN_POINT('',(123.033626104583,6.95,50.4290417845261));
#196635=CARTESIAN_POINT('Origin',(122.542812602034,6.95,50.3336368280768));
#196636=CARTESIAN_POINT('',(122.485569628164,6.95,50.6281249296065));
#196637=CARTESIAN_POINT('',(122.542812602034,6.95,50.3336368280768));
#196638=CARTESIAN_POINT('Origin',(121.757510997955,7.45,50.180988897758));
#196639=CARTESIAN_POINT('',(122.248324500504,7.45,50.2763938542073));
#196640=CARTESIAN_POINT('',(122.191081526635,7.45,50.570881955737));
#196641=CARTESIAN_POINT('',(122.248324500504,7.45,50.2763938542073));
#196642=CARTESIAN_POINT('',(121.700268024085,7.45,50.4754769992877));
#196643=CARTESIAN_POINT('',(121.700268024085,7.45,50.4754769992877));
#196644=CARTESIAN_POINT('',(121.757510997955,7.45,50.180988897758));
#196645=CARTESIAN_POINT('',(121.757510997955,7.45,50.180988897758));
#196646=CARTESIAN_POINT('',(121.757510997955,7.45,50.180988897758));
#196647=CARTESIAN_POINT('Origin',(122.248324500504,7.45,50.2763938542073));
#196648=CARTESIAN_POINT('',(122.248324500504,6.95,50.2763938542073));
#196649=CARTESIAN_POINT('',(122.191081526635,6.95,50.570881955737));
#196650=CARTESIAN_POINT('',(122.248324500504,6.95,50.2763938542073));
#196651=CARTESIAN_POINT('',(122.191081526635,7.45,50.570881955737));
#196652=CARTESIAN_POINT('',(122.248324500504,7.45,50.2763938542073));
#196653=CARTESIAN_POINT('Origin',(122.248324500504,6.95,50.2763938542073));
#196654=CARTESIAN_POINT('',(121.757510997955,6.95,50.180988897758));
#196655=CARTESIAN_POINT('',(121.700268024085,6.95,50.4754769992877));
#196656=CARTESIAN_POINT('',(121.757510997955,6.95,50.180988897758));
#196657=CARTESIAN_POINT('',(122.191081526635,6.95,50.570881955737));
#196658=CARTESIAN_POINT('',(122.248324500504,6.95,50.2763938542073));
#196659=CARTESIAN_POINT('Origin',(121.757510997955,6.95,50.180988897758));
#196660=CARTESIAN_POINT('',(121.700268024085,6.95,50.4754769992877));
#196661=CARTESIAN_POINT('',(121.757510997955,6.95,50.180988897758));
#196662=CARTESIAN_POINT('Origin',(120.972209393875,7.45,50.0283409674392));
#196663=CARTESIAN_POINT('',(121.463022896425,7.45,50.1237459238885));
#196664=CARTESIAN_POINT('',(121.405779922555,7.45,50.4182340254182));
#196665=CARTESIAN_POINT('',(121.463022896425,7.45,50.1237459238885));
#196666=CARTESIAN_POINT('',(120.914966420006,7.45,50.3228290689689));
#196667=CARTESIAN_POINT('',(120.914966420006,7.45,50.3228290689689));
#196668=CARTESIAN_POINT('',(120.972209393875,7.45,50.0283409674392));
#196669=CARTESIAN_POINT('',(120.972209393875,7.45,50.0283409674392));
#196670=CARTESIAN_POINT('',(120.972209393875,7.45,50.0283409674392));
#196671=CARTESIAN_POINT('Origin',(121.463022896425,7.45,50.1237459238885));
#196672=CARTESIAN_POINT('',(121.463022896425,6.95,50.1237459238885));
#196673=CARTESIAN_POINT('',(121.405779922555,6.95,50.4182340254182));
#196674=CARTESIAN_POINT('',(121.463022896425,6.95,50.1237459238885));
#196675=CARTESIAN_POINT('',(121.405779922555,7.45,50.4182340254182));
#196676=CARTESIAN_POINT('',(121.463022896425,7.45,50.1237459238885));
#196677=CARTESIAN_POINT('Origin',(121.463022896425,6.95,50.1237459238885));
#196678=CARTESIAN_POINT('',(120.972209393875,6.95,50.0283409674392));
#196679=CARTESIAN_POINT('',(120.914966420006,6.95,50.3228290689689));
#196680=CARTESIAN_POINT('',(120.972209393875,6.95,50.0283409674392));
#196681=CARTESIAN_POINT('',(121.405779922555,6.95,50.4182340254182));
#196682=CARTESIAN_POINT('',(121.463022896425,6.95,50.1237459238885));
#196683=CARTESIAN_POINT('Origin',(120.972209393875,6.95,50.0283409674392));
#196684=CARTESIAN_POINT('',(120.914966420006,6.95,50.3228290689689));
#196685=CARTESIAN_POINT('',(120.972209393875,6.95,50.0283409674392));
#196686=CARTESIAN_POINT('Origin',(120.186907789796,7.45,49.8756930371204));
#196687=CARTESIAN_POINT('',(120.677721292346,7.45,49.9710979935697));
#196688=CARTESIAN_POINT('',(120.620478318476,7.45,50.2655860950994));
#196689=CARTESIAN_POINT('',(120.677721292346,7.45,49.9710979935697));
#196690=CARTESIAN_POINT('',(120.129664815927,7.45,50.1701811386501));
#196691=CARTESIAN_POINT('',(120.129664815927,7.45,50.1701811386501));
#196692=CARTESIAN_POINT('',(120.186907789796,7.45,49.8756930371204));
#196693=CARTESIAN_POINT('',(120.186907789796,7.45,49.8756930371204));
#196694=CARTESIAN_POINT('',(120.186907789796,7.45,49.8756930371204));
#196695=CARTESIAN_POINT('Origin',(120.677721292346,7.45,49.9710979935697));
#196696=CARTESIAN_POINT('',(120.677721292346,6.95,49.9710979935697));
#196697=CARTESIAN_POINT('',(120.620478318476,6.95,50.2655860950994));
#196698=CARTESIAN_POINT('',(120.677721292346,6.95,49.9710979935697));
#196699=CARTESIAN_POINT('',(120.620478318476,7.45,50.2655860950994));
#196700=CARTESIAN_POINT('',(120.677721292346,7.45,49.9710979935697));
#196701=CARTESIAN_POINT('Origin',(120.677721292346,6.95,49.9710979935697));
#196702=CARTESIAN_POINT('',(120.186907789796,6.95,49.8756930371204));
#196703=CARTESIAN_POINT('',(120.129664815927,6.95,50.1701811386501));
#196704=CARTESIAN_POINT('',(120.186907789796,6.95,49.8756930371204));
#196705=CARTESIAN_POINT('',(120.620478318476,6.95,50.2655860950994));
#196706=CARTESIAN_POINT('',(120.677721292346,6.95,49.9710979935697));
#196707=CARTESIAN_POINT('Origin',(120.186907789796,6.95,49.8756930371204));
#196708=CARTESIAN_POINT('',(120.129664815927,6.95,50.1701811386501));
#196709=CARTESIAN_POINT('',(120.186907789796,6.95,49.8756930371204));
#196710=CARTESIAN_POINT('Origin',(119.401606185717,7.45,49.7230451068016));
#196711=CARTESIAN_POINT('',(119.892419688267,7.45,49.8184500632509));
#196712=CARTESIAN_POINT('',(119.835176714397,7.45,50.1129381647806));
#196713=CARTESIAN_POINT('',(119.892419688267,7.45,49.8184500632509));
#196714=CARTESIAN_POINT('',(119.344363211847,7.45,50.0175332083313));
#196715=CARTESIAN_POINT('',(119.344363211847,7.45,50.0175332083313));
#196716=CARTESIAN_POINT('',(119.401606185717,7.45,49.7230451068016));
#196717=CARTESIAN_POINT('',(119.401606185717,7.45,49.7230451068016));
#196718=CARTESIAN_POINT('',(119.401606185717,7.45,49.7230451068016));
#196719=CARTESIAN_POINT('Origin',(119.892419688267,7.45,49.8184500632509));
#196720=CARTESIAN_POINT('',(119.892419688267,6.95,49.8184500632509));
#196721=CARTESIAN_POINT('',(119.835176714397,6.95,50.1129381647806));
#196722=CARTESIAN_POINT('',(119.892419688267,6.95,49.8184500632509));
#196723=CARTESIAN_POINT('',(119.835176714397,7.45,50.1129381647806));
#196724=CARTESIAN_POINT('',(119.892419688267,7.45,49.8184500632509));
#196725=CARTESIAN_POINT('Origin',(119.892419688267,6.95,49.8184500632509));
#196726=CARTESIAN_POINT('',(119.401606185717,6.95,49.7230451068016));
#196727=CARTESIAN_POINT('',(119.344363211847,6.95,50.0175332083313));
#196728=CARTESIAN_POINT('',(119.401606185717,6.95,49.7230451068016));
#196729=CARTESIAN_POINT('',(119.835176714397,6.95,50.1129381647806));
#196730=CARTESIAN_POINT('',(119.892419688267,6.95,49.8184500632509));
#196731=CARTESIAN_POINT('Origin',(119.401606185717,6.95,49.7230451068016));
#196732=CARTESIAN_POINT('',(119.344363211847,6.95,50.0175332083313));
#196733=CARTESIAN_POINT('',(119.401606185717,6.95,49.7230451068016));
#196734=CARTESIAN_POINT('Origin',(118.616304581638,7.45,49.5703971764828));
#196735=CARTESIAN_POINT('',(119.107118084187,7.45,49.6658021329321));
#196736=CARTESIAN_POINT('',(119.049875110318,7.45,49.9602902344618));
#196737=CARTESIAN_POINT('',(119.107118084187,7.45,49.6658021329321));
#196738=CARTESIAN_POINT('',(118.559061607768,7.45,49.8648852780125));
#196739=CARTESIAN_POINT('',(118.559061607768,7.45,49.8648852780125));
#196740=CARTESIAN_POINT('',(118.616304581638,7.45,49.5703971764828));
#196741=CARTESIAN_POINT('',(118.616304581638,7.45,49.5703971764828));
#196742=CARTESIAN_POINT('',(118.616304581638,7.45,49.5703971764828));
#196743=CARTESIAN_POINT('Origin',(119.107118084187,7.45,49.6658021329321));
#196744=CARTESIAN_POINT('',(119.107118084187,6.95,49.6658021329321));
#196745=CARTESIAN_POINT('',(119.049875110318,6.95,49.9602902344618));
#196746=CARTESIAN_POINT('',(119.107118084187,6.95,49.6658021329321));
#196747=CARTESIAN_POINT('',(119.049875110318,7.45,49.9602902344618));
#196748=CARTESIAN_POINT('',(119.107118084187,7.45,49.6658021329321));
#196749=CARTESIAN_POINT('Origin',(119.107118084187,6.95,49.6658021329321));
#196750=CARTESIAN_POINT('',(118.616304581638,6.95,49.5703971764828));
#196751=CARTESIAN_POINT('',(118.559061607768,6.95,49.8648852780125));
#196752=CARTESIAN_POINT('',(118.616304581638,6.95,49.5703971764828));
#196753=CARTESIAN_POINT('',(119.049875110318,6.95,49.9602902344618));
#196754=CARTESIAN_POINT('',(119.107118084187,6.95,49.6658021329321));
#196755=CARTESIAN_POINT('Origin',(118.616304581638,6.95,49.5703971764828));
#196756=CARTESIAN_POINT('',(118.559061607768,6.95,49.8648852780125));
#196757=CARTESIAN_POINT('',(118.616304581638,6.95,49.5703971764828));
#196758=CARTESIAN_POINT('Origin',(117.831002977559,7.45,49.417749246164));
#196759=CARTESIAN_POINT('',(118.321816480108,7.45,49.5131542026133));
#196760=CARTESIAN_POINT('',(118.264573506239,7.45,49.807642304143));
#196761=CARTESIAN_POINT('',(118.321816480108,7.45,49.5131542026133));
#196762=CARTESIAN_POINT('',(117.773760003689,7.45,49.7122373476937));
#196763=CARTESIAN_POINT('',(117.773760003689,7.45,49.7122373476937));
#196764=CARTESIAN_POINT('',(117.831002977559,7.45,49.417749246164));
#196765=CARTESIAN_POINT('',(117.831002977559,7.45,49.417749246164));
#196766=CARTESIAN_POINT('',(117.831002977559,7.45,49.417749246164));
#196767=CARTESIAN_POINT('Origin',(118.321816480108,7.45,49.5131542026133));
#196768=CARTESIAN_POINT('',(118.321816480108,6.95,49.5131542026133));
#196769=CARTESIAN_POINT('',(118.264573506239,6.95,49.807642304143));
#196770=CARTESIAN_POINT('',(118.321816480108,6.95,49.5131542026133));
#196771=CARTESIAN_POINT('',(118.264573506239,7.45,49.807642304143));
#196772=CARTESIAN_POINT('',(118.321816480108,7.45,49.5131542026133));
#196773=CARTESIAN_POINT('Origin',(118.321816480108,6.95,49.5131542026133));
#196774=CARTESIAN_POINT('',(117.831002977559,6.95,49.417749246164));
#196775=CARTESIAN_POINT('',(117.773760003689,6.95,49.7122373476937));
#196776=CARTESIAN_POINT('',(117.831002977559,6.95,49.417749246164));
#196777=CARTESIAN_POINT('',(118.264573506239,6.95,49.807642304143));
#196778=CARTESIAN_POINT('',(118.321816480108,6.95,49.5131542026133));
#196779=CARTESIAN_POINT('Origin',(117.831002977559,6.95,49.417749246164));
#196780=CARTESIAN_POINT('',(117.773760003689,6.95,49.7122373476937));
#196781=CARTESIAN_POINT('',(117.831002977559,6.95,49.417749246164));
#196782=CARTESIAN_POINT('Origin',(117.045701373479,7.45,49.2651013158452));
#196783=CARTESIAN_POINT('',(117.536514876029,7.45,49.3605062722945));
#196784=CARTESIAN_POINT('',(117.479271902159,7.45,49.6549943738242));
#196785=CARTESIAN_POINT('',(117.536514876029,7.45,49.3605062722945));
#196786=CARTESIAN_POINT('',(116.98845839961,7.45,49.5595894173749));
#196787=CARTESIAN_POINT('',(116.98845839961,7.45,49.5595894173749));
#196788=CARTESIAN_POINT('',(117.045701373479,7.45,49.2651013158452));
#196789=CARTESIAN_POINT('',(117.045701373479,7.45,49.2651013158452));
#196790=CARTESIAN_POINT('',(117.045701373479,7.45,49.2651013158452));
#196791=CARTESIAN_POINT('Origin',(117.536514876029,7.45,49.3605062722945));
#196792=CARTESIAN_POINT('',(117.536514876029,6.95,49.3605062722945));
#196793=CARTESIAN_POINT('',(117.479271902159,6.95,49.6549943738242));
#196794=CARTESIAN_POINT('',(117.536514876029,6.95,49.3605062722945));
#196795=CARTESIAN_POINT('',(117.479271902159,7.45,49.6549943738242));
#196796=CARTESIAN_POINT('',(117.536514876029,7.45,49.3605062722945));
#196797=CARTESIAN_POINT('Origin',(117.536514876029,6.95,49.3605062722945));
#196798=CARTESIAN_POINT('',(117.045701373479,6.95,49.2651013158452));
#196799=CARTESIAN_POINT('',(116.98845839961,6.95,49.5595894173749));
#196800=CARTESIAN_POINT('',(117.045701373479,6.95,49.2651013158452));
#196801=CARTESIAN_POINT('',(117.479271902159,6.95,49.6549943738242));
#196802=CARTESIAN_POINT('',(117.536514876029,6.95,49.3605062722945));
#196803=CARTESIAN_POINT('Origin',(117.045701373479,6.95,49.2651013158452));
#196804=CARTESIAN_POINT('',(116.98845839961,6.95,49.5595894173749));
#196805=CARTESIAN_POINT('',(117.045701373479,6.95,49.2651013158452));
#196806=CARTESIAN_POINT('Origin',(116.2603997694,7.45,49.1124533855264));
#196807=CARTESIAN_POINT('',(116.75121327195,7.45,49.2078583419757));
#196808=CARTESIAN_POINT('',(116.69397029808,7.45,49.5023464435054));
#196809=CARTESIAN_POINT('',(116.75121327195,7.45,49.2078583419757));
#196810=CARTESIAN_POINT('',(116.203156795531,7.45,49.4069414870561));
#196811=CARTESIAN_POINT('',(116.203156795531,7.45,49.4069414870561));
#196812=CARTESIAN_POINT('',(116.2603997694,7.45,49.1124533855264));
#196813=CARTESIAN_POINT('',(116.2603997694,7.45,49.1124533855264));
#196814=CARTESIAN_POINT('',(116.2603997694,7.45,49.1124533855264));
#196815=CARTESIAN_POINT('Origin',(116.75121327195,7.45,49.2078583419757));
#196816=CARTESIAN_POINT('',(116.75121327195,6.95,49.2078583419757));
#196817=CARTESIAN_POINT('',(116.69397029808,6.95,49.5023464435054));
#196818=CARTESIAN_POINT('',(116.75121327195,6.95,49.2078583419757));
#196819=CARTESIAN_POINT('',(116.69397029808,7.45,49.5023464435054));
#196820=CARTESIAN_POINT('',(116.75121327195,7.45,49.2078583419757));
#196821=CARTESIAN_POINT('Origin',(116.75121327195,6.95,49.2078583419757));
#196822=CARTESIAN_POINT('',(116.2603997694,6.95,49.1124533855264));
#196823=CARTESIAN_POINT('',(116.203156795531,6.95,49.4069414870561));
#196824=CARTESIAN_POINT('',(116.2603997694,6.95,49.1124533855264));
#196825=CARTESIAN_POINT('',(116.69397029808,6.95,49.5023464435054));
#196826=CARTESIAN_POINT('',(116.75121327195,6.95,49.2078583419757));
#196827=CARTESIAN_POINT('Origin',(116.2603997694,6.95,49.1124533855264));
#196828=CARTESIAN_POINT('',(116.203156795531,6.95,49.4069414870561));
#196829=CARTESIAN_POINT('',(116.2603997694,6.95,49.1124533855264));
#196830=CARTESIAN_POINT('Origin',(115.475098165321,7.45,48.9598054552076));
#196831=CARTESIAN_POINT('',(115.96591166787,7.45,49.0552104116569));
#196832=CARTESIAN_POINT('',(115.908668694001,7.45,49.3496985131866));
#196833=CARTESIAN_POINT('',(115.96591166787,7.45,49.0552104116569));
#196834=CARTESIAN_POINT('',(115.417855191451,7.45,49.2542935567373));
#196835=CARTESIAN_POINT('',(115.417855191451,7.45,49.2542935567373));
#196836=CARTESIAN_POINT('',(115.475098165321,7.45,48.9598054552076));
#196837=CARTESIAN_POINT('',(115.475098165321,7.45,48.9598054552076));
#196838=CARTESIAN_POINT('',(115.475098165321,7.45,48.9598054552076));
#196839=CARTESIAN_POINT('Origin',(115.96591166787,7.45,49.0552104116569));
#196840=CARTESIAN_POINT('',(115.96591166787,6.95,49.0552104116569));
#196841=CARTESIAN_POINT('',(115.908668694001,6.95,49.3496985131866));
#196842=CARTESIAN_POINT('',(115.96591166787,6.95,49.0552104116569));
#196843=CARTESIAN_POINT('',(115.908668694001,7.45,49.3496985131866));
#196844=CARTESIAN_POINT('',(115.96591166787,7.45,49.0552104116569));
#196845=CARTESIAN_POINT('Origin',(115.96591166787,6.95,49.0552104116569));
#196846=CARTESIAN_POINT('',(115.475098165321,6.95,48.9598054552076));
#196847=CARTESIAN_POINT('',(115.417855191451,6.95,49.2542935567373));
#196848=CARTESIAN_POINT('',(115.475098165321,6.95,48.9598054552076));
#196849=CARTESIAN_POINT('',(115.908668694001,6.95,49.3496985131866));
#196850=CARTESIAN_POINT('',(115.96591166787,6.95,49.0552104116569));
#196851=CARTESIAN_POINT('Origin',(115.475098165321,6.95,48.9598054552076));
#196852=CARTESIAN_POINT('',(115.417855191451,6.95,49.2542935567373));
#196853=CARTESIAN_POINT('',(115.475098165321,6.95,48.9598054552076));
#196854=CARTESIAN_POINT('Origin',(114.689796561242,7.45,48.8071575248888));
#196855=CARTESIAN_POINT('',(115.180610063791,7.45,48.9025624813381));
#196856=CARTESIAN_POINT('',(115.123367089922,7.45,49.1970505828678));
#196857=CARTESIAN_POINT('',(115.180610063791,7.45,48.9025624813381));
#196858=CARTESIAN_POINT('',(114.632553587372,7.45,49.1016456264185));
#196859=CARTESIAN_POINT('',(114.632553587372,7.45,49.1016456264185));
#196860=CARTESIAN_POINT('',(114.689796561242,7.45,48.8071575248888));
#196861=CARTESIAN_POINT('',(114.689796561242,7.45,48.8071575248888));
#196862=CARTESIAN_POINT('',(114.689796561242,7.45,48.8071575248888));
#196863=CARTESIAN_POINT('Origin',(115.180610063791,7.45,48.9025624813381));
#196864=CARTESIAN_POINT('',(115.180610063791,6.95,48.9025624813381));
#196865=CARTESIAN_POINT('',(115.123367089922,6.95,49.1970505828678));
#196866=CARTESIAN_POINT('',(115.180610063791,6.95,48.9025624813381));
#196867=CARTESIAN_POINT('',(115.123367089922,7.45,49.1970505828678));
#196868=CARTESIAN_POINT('',(115.180610063791,7.45,48.9025624813381));
#196869=CARTESIAN_POINT('Origin',(115.180610063791,6.95,48.9025624813381));
#196870=CARTESIAN_POINT('',(114.689796561242,6.95,48.8071575248888));
#196871=CARTESIAN_POINT('',(114.632553587372,6.95,49.1016456264185));
#196872=CARTESIAN_POINT('',(114.689796561242,6.95,48.8071575248888));
#196873=CARTESIAN_POINT('',(115.123367089922,6.95,49.1970505828678));
#196874=CARTESIAN_POINT('',(115.180610063791,6.95,48.9025624813381));
#196875=CARTESIAN_POINT('Origin',(114.689796561242,6.95,48.8071575248888));
#196876=CARTESIAN_POINT('',(114.632553587372,6.95,49.1016456264185));
#196877=CARTESIAN_POINT('',(114.689796561242,6.95,48.8071575248888));
#196878=CARTESIAN_POINT('Origin',(113.904494957163,7.45,48.65450959457));
#196879=CARTESIAN_POINT('',(114.395308459712,7.45,48.7499145510193));
#196880=CARTESIAN_POINT('',(114.338065485842,7.45,49.044402652549));
#196881=CARTESIAN_POINT('',(114.395308459712,7.45,48.7499145510193));
#196882=CARTESIAN_POINT('',(113.847251983293,7.45,48.9489976960997));
#196883=CARTESIAN_POINT('',(113.847251983293,7.45,48.9489976960997));
#196884=CARTESIAN_POINT('',(113.904494957163,7.45,48.65450959457));
#196885=CARTESIAN_POINT('',(113.904494957163,7.45,48.65450959457));
#196886=CARTESIAN_POINT('',(113.904494957163,7.45,48.65450959457));
#196887=CARTESIAN_POINT('Origin',(114.395308459712,7.45,48.7499145510193));
#196888=CARTESIAN_POINT('',(114.395308459712,6.95,48.7499145510193));
#196889=CARTESIAN_POINT('',(114.338065485842,6.95,49.044402652549));
#196890=CARTESIAN_POINT('',(114.395308459712,6.95,48.7499145510193));
#196891=CARTESIAN_POINT('',(114.338065485842,7.45,49.044402652549));
#196892=CARTESIAN_POINT('',(114.395308459712,7.45,48.7499145510193));
#196893=CARTESIAN_POINT('Origin',(114.395308459712,6.95,48.7499145510193));
#196894=CARTESIAN_POINT('',(113.904494957163,6.95,48.65450959457));
#196895=CARTESIAN_POINT('',(113.847251983293,6.95,48.9489976960997));
#196896=CARTESIAN_POINT('',(113.904494957163,6.95,48.65450959457));
#196897=CARTESIAN_POINT('',(114.338065485842,6.95,49.044402652549));
#196898=CARTESIAN_POINT('',(114.395308459712,6.95,48.7499145510193));
#196899=CARTESIAN_POINT('Origin',(113.904494957163,6.95,48.65450959457));
#196900=CARTESIAN_POINT('',(113.847251983293,6.95,48.9489976960997));
#196901=CARTESIAN_POINT('',(113.904494957163,6.95,48.65450959457));
#196902=CARTESIAN_POINT('Origin',(113.119193353083,7.45,48.5018616642512));
#196903=CARTESIAN_POINT('',(113.610006855633,7.45,48.5972666207005));
#196904=CARTESIAN_POINT('',(113.552763881763,7.45,48.8917547222302));
#196905=CARTESIAN_POINT('',(113.610006855633,7.45,48.5972666207005));
#196906=CARTESIAN_POINT('',(113.061950379214,7.45,48.7963497657809));
#196907=CARTESIAN_POINT('',(113.061950379214,7.45,48.7963497657809));
#196908=CARTESIAN_POINT('',(113.119193353083,7.45,48.5018616642512));
#196909=CARTESIAN_POINT('',(113.119193353083,7.45,48.5018616642512));
#196910=CARTESIAN_POINT('',(113.119193353083,7.45,48.5018616642512));
#196911=CARTESIAN_POINT('Origin',(113.610006855633,7.45,48.5972666207005));
#196912=CARTESIAN_POINT('',(113.610006855633,6.95,48.5972666207005));
#196913=CARTESIAN_POINT('',(113.552763881763,6.95,48.8917547222302));
#196914=CARTESIAN_POINT('',(113.610006855633,6.95,48.5972666207005));
#196915=CARTESIAN_POINT('',(113.552763881763,7.45,48.8917547222302));
#196916=CARTESIAN_POINT('',(113.610006855633,7.45,48.5972666207005));
#196917=CARTESIAN_POINT('Origin',(113.610006855633,6.95,48.5972666207005));
#196918=CARTESIAN_POINT('',(113.119193353083,6.95,48.5018616642512));
#196919=CARTESIAN_POINT('',(113.061950379214,6.95,48.7963497657809));
#196920=CARTESIAN_POINT('',(113.119193353083,6.95,48.5018616642512));
#196921=CARTESIAN_POINT('',(113.552763881763,6.95,48.8917547222302));
#196922=CARTESIAN_POINT('',(113.610006855633,6.95,48.5972666207005));
#196923=CARTESIAN_POINT('Origin',(113.119193353083,6.95,48.5018616642512));
#196924=CARTESIAN_POINT('',(113.061950379214,6.95,48.7963497657809));
#196925=CARTESIAN_POINT('',(113.119193353083,6.95,48.5018616642512));
#196926=CARTESIAN_POINT('Origin',(112.333891749004,7.45,48.3492137339324));
#196927=CARTESIAN_POINT('',(112.824705251554,7.45,48.4446186903817));
#196928=CARTESIAN_POINT('',(112.767462277684,7.45,48.7391067919114));
#196929=CARTESIAN_POINT('',(112.824705251554,7.45,48.4446186903817));
#196930=CARTESIAN_POINT('',(112.276648775135,7.45,48.6437018354621));
#196931=CARTESIAN_POINT('',(112.276648775135,7.45,48.6437018354621));
#196932=CARTESIAN_POINT('',(112.333891749004,7.45,48.3492137339324));
#196933=CARTESIAN_POINT('',(112.333891749004,7.45,48.3492137339324));
#196934=CARTESIAN_POINT('',(112.333891749004,7.45,48.3492137339324));
#196935=CARTESIAN_POINT('Origin',(112.824705251554,7.45,48.4446186903817));
#196936=CARTESIAN_POINT('',(112.824705251554,6.95,48.4446186903817));
#196937=CARTESIAN_POINT('',(112.767462277684,6.95,48.7391067919114));
#196938=CARTESIAN_POINT('',(112.824705251554,6.95,48.4446186903817));
#196939=CARTESIAN_POINT('',(112.767462277684,7.45,48.7391067919114));
#196940=CARTESIAN_POINT('',(112.824705251554,7.45,48.4446186903817));
#196941=CARTESIAN_POINT('Origin',(112.824705251554,6.95,48.4446186903817));
#196942=CARTESIAN_POINT('',(112.333891749004,6.95,48.3492137339324));
#196943=CARTESIAN_POINT('',(112.276648775135,6.95,48.6437018354621));
#196944=CARTESIAN_POINT('',(112.333891749004,6.95,48.3492137339324));
#196945=CARTESIAN_POINT('',(112.767462277684,6.95,48.7391067919114));
#196946=CARTESIAN_POINT('',(112.824705251554,6.95,48.4446186903817));
#196947=CARTESIAN_POINT('Origin',(112.333891749004,6.95,48.3492137339324));
#196948=CARTESIAN_POINT('',(112.276648775135,6.95,48.6437018354621));
#196949=CARTESIAN_POINT('',(112.333891749004,6.95,48.3492137339324));
#196950=CARTESIAN_POINT('Origin',(111.548590144925,7.45,48.1965658036136));
#196951=CARTESIAN_POINT('',(112.039403647474,7.45,48.2919707600629));
#196952=CARTESIAN_POINT('',(111.982160673605,7.45,48.5864588615926));
#196953=CARTESIAN_POINT('',(112.039403647474,7.45,48.2919707600629));
#196954=CARTESIAN_POINT('',(111.491347171055,7.45,48.4910539051433));
#196955=CARTESIAN_POINT('',(111.491347171055,7.45,48.4910539051433));
#196956=CARTESIAN_POINT('',(111.548590144925,7.45,48.1965658036136));
#196957=CARTESIAN_POINT('',(111.548590144925,7.45,48.1965658036136));
#196958=CARTESIAN_POINT('',(111.548590144925,7.45,48.1965658036136));
#196959=CARTESIAN_POINT('Origin',(112.039403647474,7.45,48.2919707600629));
#196960=CARTESIAN_POINT('',(112.039403647474,6.95,48.2919707600629));
#196961=CARTESIAN_POINT('',(111.982160673605,6.95,48.5864588615926));
#196962=CARTESIAN_POINT('',(112.039403647474,6.95,48.2919707600629));
#196963=CARTESIAN_POINT('',(111.982160673605,7.45,48.5864588615926));
#196964=CARTESIAN_POINT('',(112.039403647474,7.45,48.2919707600629));
#196965=CARTESIAN_POINT('Origin',(112.039403647474,6.95,48.2919707600629));
#196966=CARTESIAN_POINT('',(111.548590144925,6.95,48.1965658036136));
#196967=CARTESIAN_POINT('',(111.491347171055,6.95,48.4910539051433));
#196968=CARTESIAN_POINT('',(111.548590144925,6.95,48.1965658036136));
#196969=CARTESIAN_POINT('',(111.982160673605,6.95,48.5864588615926));
#196970=CARTESIAN_POINT('',(112.039403647474,6.95,48.2919707600629));
#196971=CARTESIAN_POINT('Origin',(111.548590144925,6.95,48.1965658036136));
#196972=CARTESIAN_POINT('',(111.491347171055,6.95,48.4910539051433));
#196973=CARTESIAN_POINT('',(111.548590144925,6.95,48.1965658036136));
#196974=CARTESIAN_POINT('Origin',(110.763288540846,6.65,48.0439178732948));
#196975=CARTESIAN_POINT('',(111.254102043395,6.65,48.139322829744));
#196976=CARTESIAN_POINT('',(111.196859069526,6.65,48.4338109312737));
#196977=CARTESIAN_POINT('',(111.254102043395,6.65,48.139322829744));
#196978=CARTESIAN_POINT('',(110.706045566976,6.65,48.3384059748245));
#196979=CARTESIAN_POINT('',(110.706045566976,6.65,48.3384059748245));
#196980=CARTESIAN_POINT('',(110.763288540846,6.65,48.0439178732948));
#196981=CARTESIAN_POINT('',(110.763288540846,6.65,48.0439178732948));
#196982=CARTESIAN_POINT('',(110.763288540846,6.65,48.0439178732948));
#196983=CARTESIAN_POINT('Origin',(111.254102043395,6.65,48.139322829744));
#196984=CARTESIAN_POINT('',(111.254102043395,6.15,48.139322829744));
#196985=CARTESIAN_POINT('',(111.196859069526,6.15,48.4338109312737));
#196986=CARTESIAN_POINT('',(111.254102043395,6.15,48.139322829744));
#196987=CARTESIAN_POINT('',(111.196859069526,6.65,48.4338109312737));
#196988=CARTESIAN_POINT('',(111.254102043395,6.65,48.139322829744));
#196989=CARTESIAN_POINT('Origin',(111.254102043395,6.15,48.139322829744));
#196990=CARTESIAN_POINT('',(110.763288540846,6.15,48.0439178732948));
#196991=CARTESIAN_POINT('',(110.706045566976,6.15,48.3384059748245));
#196992=CARTESIAN_POINT('',(110.763288540846,6.15,48.0439178732948));
#196993=CARTESIAN_POINT('',(111.196859069526,6.15,48.4338109312737));
#196994=CARTESIAN_POINT('',(111.254102043395,6.15,48.139322829744));
#196995=CARTESIAN_POINT('Origin',(110.763288540846,6.15,48.0439178732948));
#196996=CARTESIAN_POINT('',(110.706045566976,6.15,48.3384059748245));
#196997=CARTESIAN_POINT('',(110.763288540846,6.15,48.0439178732948));
#196998=CARTESIAN_POINT('Origin',(110.763288540846,5.85,48.0439178732948));
#196999=CARTESIAN_POINT('',(111.254102043395,5.85,48.139322829744));
#197000=CARTESIAN_POINT('',(111.196859069526,5.85,48.4338109312737));
#197001=CARTESIAN_POINT('',(111.254102043395,5.85,48.139322829744));
#197002=CARTESIAN_POINT('',(110.706045566976,5.85,48.3384059748245));
#197003=CARTESIAN_POINT('',(110.706045566976,5.85,48.3384059748245));
#197004=CARTESIAN_POINT('',(110.763288540846,5.85,48.0439178732948));
#197005=CARTESIAN_POINT('',(110.763288540846,5.85,48.0439178732948));
#197006=CARTESIAN_POINT('',(110.763288540846,5.85,48.0439178732948));
#197007=CARTESIAN_POINT('Origin',(111.254102043395,5.85,48.139322829744));
#197008=CARTESIAN_POINT('',(111.254102043395,5.35,48.139322829744));
#197009=CARTESIAN_POINT('',(111.196859069526,5.35,48.4338109312737));
#197010=CARTESIAN_POINT('',(111.254102043395,5.35,48.139322829744));
#197011=CARTESIAN_POINT('',(111.196859069526,5.85,48.4338109312737));
#197012=CARTESIAN_POINT('',(111.254102043395,5.85,48.139322829744));
#197013=CARTESIAN_POINT('Origin',(111.254102043395,5.35,48.139322829744));
#197014=CARTESIAN_POINT('',(110.763288540846,5.35,48.0439178732948));
#197015=CARTESIAN_POINT('',(110.706045566976,5.35,48.3384059748245));
#197016=CARTESIAN_POINT('',(110.763288540846,5.35,48.0439178732948));
#197017=CARTESIAN_POINT('',(111.196859069526,5.35,48.4338109312737));
#197018=CARTESIAN_POINT('',(111.254102043395,5.35,48.139322829744));
#197019=CARTESIAN_POINT('Origin',(110.763288540846,5.35,48.0439178732948));
#197020=CARTESIAN_POINT('',(110.706045566976,5.35,48.3384059748245));
#197021=CARTESIAN_POINT('',(110.763288540846,5.35,48.0439178732948));
#197022=CARTESIAN_POINT('Origin',(110.763288540846,5.05,48.0439178732948));
#197023=CARTESIAN_POINT('',(111.254102043395,5.05,48.139322829744));
#197024=CARTESIAN_POINT('',(111.196859069526,5.05,48.4338109312737));
#197025=CARTESIAN_POINT('',(111.254102043395,5.05,48.139322829744));
#197026=CARTESIAN_POINT('',(110.706045566976,5.05,48.3384059748245));
#197027=CARTESIAN_POINT('',(110.706045566976,5.05,48.3384059748245));
#197028=CARTESIAN_POINT('',(110.763288540846,5.05,48.0439178732948));
#197029=CARTESIAN_POINT('',(110.763288540846,5.05,48.0439178732948));
#197030=CARTESIAN_POINT('',(110.763288540846,5.05,48.0439178732948));
#197031=CARTESIAN_POINT('Origin',(111.254102043395,5.05,48.139322829744));
#197032=CARTESIAN_POINT('',(111.254102043395,4.55,48.139322829744));
#197033=CARTESIAN_POINT('',(111.196859069526,4.55,48.4338109312737));
#197034=CARTESIAN_POINT('',(111.254102043395,4.55,48.139322829744));
#197035=CARTESIAN_POINT('',(111.196859069526,5.05,48.4338109312737));
#197036=CARTESIAN_POINT('',(111.254102043395,5.05,48.139322829744));
#197037=CARTESIAN_POINT('Origin',(111.254102043395,4.55,48.139322829744));
#197038=CARTESIAN_POINT('',(110.763288540846,4.55,48.0439178732948));
#197039=CARTESIAN_POINT('',(110.706045566976,4.55,48.3384059748245));
#197040=CARTESIAN_POINT('',(110.763288540846,4.55,48.0439178732948));
#197041=CARTESIAN_POINT('',(111.196859069526,4.55,48.4338109312737));
#197042=CARTESIAN_POINT('',(111.254102043395,4.55,48.139322829744));
#197043=CARTESIAN_POINT('Origin',(110.763288540846,4.55,48.0439178732948));
#197044=CARTESIAN_POINT('',(110.706045566976,4.55,48.3384059748245));
#197045=CARTESIAN_POINT('',(110.763288540846,4.55,48.0439178732948));
#197046=CARTESIAN_POINT('Origin',(110.763288540846,4.25,48.0439178732948));
#197047=CARTESIAN_POINT('',(111.254102043395,4.25,48.139322829744));
#197048=CARTESIAN_POINT('',(111.196859069526,4.25,48.4338109312737));
#197049=CARTESIAN_POINT('',(111.254102043395,4.25,48.139322829744));
#197050=CARTESIAN_POINT('',(110.706045566976,4.25,48.3384059748245));
#197051=CARTESIAN_POINT('',(110.706045566976,4.25,48.3384059748245));
#197052=CARTESIAN_POINT('',(110.763288540846,4.25,48.0439178732948));
#197053=CARTESIAN_POINT('',(110.763288540846,4.25,48.0439178732948));
#197054=CARTESIAN_POINT('',(110.763288540846,4.25,48.0439178732948));
#197055=CARTESIAN_POINT('Origin',(111.254102043395,4.25,48.139322829744));
#197056=CARTESIAN_POINT('',(111.254102043395,3.75,48.139322829744));
#197057=CARTESIAN_POINT('',(111.196859069526,3.75,48.4338109312737));
#197058=CARTESIAN_POINT('',(111.254102043395,3.75,48.139322829744));
#197059=CARTESIAN_POINT('',(111.196859069526,4.25,48.4338109312737));
#197060=CARTESIAN_POINT('',(111.254102043395,4.25,48.139322829744));
#197061=CARTESIAN_POINT('Origin',(111.254102043395,3.75,48.139322829744));
#197062=CARTESIAN_POINT('',(110.763288540846,3.75,48.0439178732948));
#197063=CARTESIAN_POINT('',(110.706045566976,3.75,48.3384059748245));
#197064=CARTESIAN_POINT('',(110.763288540846,3.75,48.0439178732948));
#197065=CARTESIAN_POINT('',(111.196859069526,3.75,48.4338109312737));
#197066=CARTESIAN_POINT('',(111.254102043395,3.75,48.139322829744));
#197067=CARTESIAN_POINT('Origin',(110.763288540846,3.75,48.0439178732948));
#197068=CARTESIAN_POINT('',(110.706045566976,3.75,48.3384059748245));
#197069=CARTESIAN_POINT('',(110.763288540846,3.75,48.0439178732948));
#197070=CARTESIAN_POINT('Origin',(110.763288540846,3.45,48.0439178732948));
#197071=CARTESIAN_POINT('',(111.254102043395,3.45,48.139322829744));
#197072=CARTESIAN_POINT('',(111.196859069526,3.45,48.4338109312737));
#197073=CARTESIAN_POINT('',(111.254102043395,3.45,48.139322829744));
#197074=CARTESIAN_POINT('',(110.706045566976,3.45,48.3384059748245));
#197075=CARTESIAN_POINT('',(110.706045566976,3.45,48.3384059748245));
#197076=CARTESIAN_POINT('',(110.763288540846,3.45,48.0439178732948));
#197077=CARTESIAN_POINT('',(110.763288540846,3.45,48.0439178732948));
#197078=CARTESIAN_POINT('',(110.763288540846,3.45,48.0439178732948));
#197079=CARTESIAN_POINT('Origin',(111.254102043395,3.45,48.139322829744));
#197080=CARTESIAN_POINT('',(111.254102043395,2.95,48.139322829744));
#197081=CARTESIAN_POINT('',(111.196859069526,2.95,48.4338109312737));
#197082=CARTESIAN_POINT('',(111.254102043395,2.95,48.139322829744));
#197083=CARTESIAN_POINT('',(111.196859069526,3.45,48.4338109312737));
#197084=CARTESIAN_POINT('',(111.254102043395,3.45,48.139322829744));
#197085=CARTESIAN_POINT('Origin',(111.254102043395,2.95,48.139322829744));
#197086=CARTESIAN_POINT('',(110.763288540846,2.95,48.0439178732948));
#197087=CARTESIAN_POINT('',(110.706045566976,2.95,48.3384059748245));
#197088=CARTESIAN_POINT('',(110.763288540846,2.95,48.0439178732948));
#197089=CARTESIAN_POINT('',(111.196859069526,2.95,48.4338109312737));
#197090=CARTESIAN_POINT('',(111.254102043395,2.95,48.139322829744));
#197091=CARTESIAN_POINT('Origin',(110.763288540846,2.95,48.0439178732948));
#197092=CARTESIAN_POINT('',(110.706045566976,2.95,48.3384059748245));
#197093=CARTESIAN_POINT('',(110.763288540846,2.95,48.0439178732948));
#197094=CARTESIAN_POINT('Origin',(110.763288540846,2.65,48.0439178732948));
#197095=CARTESIAN_POINT('',(111.254102043395,2.65,48.139322829744));
#197096=CARTESIAN_POINT('',(111.196859069526,2.65,48.4338109312737));
#197097=CARTESIAN_POINT('',(111.254102043395,2.65,48.139322829744));
#197098=CARTESIAN_POINT('',(110.706045566976,2.65,48.3384059748245));
#197099=CARTESIAN_POINT('',(110.706045566976,2.65,48.3384059748245));
#197100=CARTESIAN_POINT('',(110.763288540846,2.65,48.0439178732948));
#197101=CARTESIAN_POINT('',(110.763288540846,2.65,48.0439178732948));
#197102=CARTESIAN_POINT('',(110.763288540846,2.65,48.0439178732948));
#197103=CARTESIAN_POINT('Origin',(111.254102043395,2.65,48.139322829744));
#197104=CARTESIAN_POINT('',(111.254102043395,2.15,48.139322829744));
#197105=CARTESIAN_POINT('',(111.196859069526,2.15,48.4338109312737));
#197106=CARTESIAN_POINT('',(111.254102043395,2.15,48.139322829744));
#197107=CARTESIAN_POINT('',(111.196859069526,2.65,48.4338109312737));
#197108=CARTESIAN_POINT('',(111.254102043395,2.65,48.139322829744));
#197109=CARTESIAN_POINT('Origin',(111.254102043395,2.15,48.139322829744));
#197110=CARTESIAN_POINT('',(110.763288540846,2.15,48.0439178732948));
#197111=CARTESIAN_POINT('',(110.706045566976,2.15,48.3384059748245));
#197112=CARTESIAN_POINT('',(110.763288540846,2.15,48.0439178732948));
#197113=CARTESIAN_POINT('',(111.196859069526,2.15,48.4338109312737));
#197114=CARTESIAN_POINT('',(111.254102043395,2.15,48.139322829744));
#197115=CARTESIAN_POINT('Origin',(110.763288540846,2.15,48.0439178732948));
#197116=CARTESIAN_POINT('',(110.706045566976,2.15,48.3384059748245));
#197117=CARTESIAN_POINT('',(110.763288540846,2.15,48.0439178732948));
#197118=CARTESIAN_POINT('Origin',(110.763288540846,1.85,48.0439178732948));
#197119=CARTESIAN_POINT('',(111.254102043395,1.85,48.139322829744));
#197120=CARTESIAN_POINT('',(111.196859069526,1.85,48.4338109312737));
#197121=CARTESIAN_POINT('',(111.254102043395,1.85,48.139322829744));
#197122=CARTESIAN_POINT('',(110.706045566976,1.85,48.3384059748245));
#197123=CARTESIAN_POINT('',(110.706045566976,1.85,48.3384059748245));
#197124=CARTESIAN_POINT('',(110.763288540846,1.85,48.0439178732948));
#197125=CARTESIAN_POINT('',(110.763288540846,1.85,48.0439178732948));
#197126=CARTESIAN_POINT('',(110.763288540846,1.85,48.0439178732948));
#197127=CARTESIAN_POINT('Origin',(111.254102043395,1.85,48.139322829744));
#197128=CARTESIAN_POINT('',(111.254102043395,1.35,48.139322829744));
#197129=CARTESIAN_POINT('',(111.196859069526,1.35,48.4338109312737));
#197130=CARTESIAN_POINT('',(111.254102043395,1.35,48.139322829744));
#197131=CARTESIAN_POINT('',(111.196859069526,1.85,48.4338109312737));
#197132=CARTESIAN_POINT('',(111.254102043395,1.85,48.139322829744));
#197133=CARTESIAN_POINT('Origin',(111.254102043395,1.35,48.139322829744));
#197134=CARTESIAN_POINT('',(110.763288540846,1.35,48.0439178732948));
#197135=CARTESIAN_POINT('',(110.706045566976,1.35,48.3384059748245));
#197136=CARTESIAN_POINT('',(110.763288540846,1.35,48.0439178732948));
#197137=CARTESIAN_POINT('',(111.196859069526,1.35,48.4338109312737));
#197138=CARTESIAN_POINT('',(111.254102043395,1.35,48.139322829744));
#197139=CARTESIAN_POINT('Origin',(110.763288540846,1.35,48.0439178732948));
#197140=CARTESIAN_POINT('',(110.706045566976,1.35,48.3384059748245));
#197141=CARTESIAN_POINT('',(110.763288540846,1.35,48.0439178732948));
#197142=CARTESIAN_POINT('Origin',(110.763288540846,1.05,48.0439178732948));
#197143=CARTESIAN_POINT('',(111.254102043395,1.05,48.139322829744));
#197144=CARTESIAN_POINT('',(111.196859069526,1.05,48.4338109312737));
#197145=CARTESIAN_POINT('',(111.254102043395,1.05,48.139322829744));
#197146=CARTESIAN_POINT('',(110.706045566976,1.05,48.3384059748245));
#197147=CARTESIAN_POINT('',(110.706045566976,1.05,48.3384059748245));
#197148=CARTESIAN_POINT('',(110.763288540846,1.05,48.0439178732948));
#197149=CARTESIAN_POINT('',(110.763288540846,1.05,48.0439178732948));
#197150=CARTESIAN_POINT('',(110.763288540846,1.05,48.0439178732948));
#197151=CARTESIAN_POINT('Origin',(111.254102043395,1.05,48.139322829744));
#197152=CARTESIAN_POINT('',(111.254102043395,0.550000000000015,48.139322829744));
#197153=CARTESIAN_POINT('',(111.196859069526,0.550000000000015,48.4338109312737));
#197154=CARTESIAN_POINT('',(111.254102043395,0.550000000000015,48.139322829744));
#197155=CARTESIAN_POINT('',(111.196859069526,1.05,48.4338109312737));
#197156=CARTESIAN_POINT('',(111.254102043395,1.05,48.139322829744));
#197157=CARTESIAN_POINT('Origin',(111.254102043395,0.550000000000015,48.139322829744));
#197158=CARTESIAN_POINT('',(110.763288540846,0.550000000000015,48.0439178732948));
#197159=CARTESIAN_POINT('',(110.706045566976,0.550000000000015,48.3384059748245));
#197160=CARTESIAN_POINT('',(110.763288540846,0.550000000000015,48.0439178732948));
#197161=CARTESIAN_POINT('',(111.196859069526,0.550000000000015,48.4338109312737));
#197162=CARTESIAN_POINT('',(111.254102043395,0.550000000000015,48.139322829744));
#197163=CARTESIAN_POINT('Origin',(110.763288540846,0.550000000000015,48.0439178732948));
#197164=CARTESIAN_POINT('',(110.706045566976,0.550000000000015,48.3384059748245));
#197165=CARTESIAN_POINT('',(110.763288540846,0.550000000000015,48.0439178732948));
#197166=CARTESIAN_POINT('Origin',(110.763288540846,0.250000000000015,48.0439178732948));
#197167=CARTESIAN_POINT('',(111.254102043395,0.250000000000015,48.139322829744));
#197168=CARTESIAN_POINT('',(111.196859069526,0.250000000000015,48.4338109312737));
#197169=CARTESIAN_POINT('',(111.254102043395,0.250000000000015,48.139322829744));
#197170=CARTESIAN_POINT('',(110.706045566976,0.250000000000015,48.3384059748245));
#197171=CARTESIAN_POINT('',(110.706045566976,0.250000000000015,48.3384059748245));
#197172=CARTESIAN_POINT('',(110.763288540846,0.250000000000015,48.0439178732948));
#197173=CARTESIAN_POINT('',(110.763288540846,0.250000000000015,48.0439178732948));
#197174=CARTESIAN_POINT('',(110.763288540846,0.250000000000015,48.0439178732948));
#197175=CARTESIAN_POINT('Origin',(111.254102043395,0.250000000000015,48.139322829744));
#197176=CARTESIAN_POINT('',(111.254102043395,-0.249999999999985,48.139322829744));
#197177=CARTESIAN_POINT('',(111.196859069526,-0.249999999999985,48.4338109312737));
#197178=CARTESIAN_POINT('',(111.254102043395,-0.249999999999985,48.139322829744));
#197179=CARTESIAN_POINT('',(111.196859069526,0.250000000000015,48.4338109312737));
#197180=CARTESIAN_POINT('',(111.254102043395,0.250000000000015,48.139322829744));
#197181=CARTESIAN_POINT('Origin',(111.254102043395,-0.249999999999985,48.139322829744));
#197182=CARTESIAN_POINT('',(110.763288540846,-0.249999999999985,48.0439178732948));
#197183=CARTESIAN_POINT('',(110.706045566976,-0.249999999999985,48.3384059748245));
#197184=CARTESIAN_POINT('',(110.763288540846,-0.249999999999985,48.0439178732948));
#197185=CARTESIAN_POINT('',(111.196859069526,-0.249999999999985,48.4338109312737));
#197186=CARTESIAN_POINT('',(111.254102043395,-0.249999999999985,48.139322829744));
#197187=CARTESIAN_POINT('Origin',(110.763288540846,-0.249999999999985,48.0439178732948));
#197188=CARTESIAN_POINT('',(110.706045566976,-0.249999999999985,48.3384059748245));
#197189=CARTESIAN_POINT('',(110.763288540846,-0.249999999999985,48.0439178732948));
#197190=CARTESIAN_POINT('Origin',(110.763288540846,-0.549999999999986,48.0439178732948));
#197191=CARTESIAN_POINT('',(111.254102043395,-0.549999999999986,48.139322829744));
#197192=CARTESIAN_POINT('',(111.196859069526,-0.549999999999986,48.4338109312737));
#197193=CARTESIAN_POINT('',(111.254102043395,-0.549999999999986,48.139322829744));
#197194=CARTESIAN_POINT('',(110.706045566976,-0.549999999999986,48.3384059748245));
#197195=CARTESIAN_POINT('',(110.706045566976,-0.549999999999986,48.3384059748245));
#197196=CARTESIAN_POINT('',(110.763288540846,-0.549999999999986,48.0439178732948));
#197197=CARTESIAN_POINT('',(110.763288540846,-0.549999999999986,48.0439178732948));
#197198=CARTESIAN_POINT('',(110.763288540846,-0.549999999999986,48.0439178732948));
#197199=CARTESIAN_POINT('Origin',(111.254102043395,-0.549999999999986,48.139322829744));
#197200=CARTESIAN_POINT('',(111.254102043395,-1.05,48.139322829744));
#197201=CARTESIAN_POINT('',(111.196859069526,-1.05,48.4338109312737));
#197202=CARTESIAN_POINT('',(111.254102043395,-1.05,48.139322829744));
#197203=CARTESIAN_POINT('',(111.196859069526,-0.549999999999986,48.4338109312737));
#197204=CARTESIAN_POINT('',(111.254102043395,-0.549999999999986,48.139322829744));
#197205=CARTESIAN_POINT('Origin',(111.254102043395,-1.05,48.139322829744));
#197206=CARTESIAN_POINT('',(110.763288540846,-1.05,48.0439178732948));
#197207=CARTESIAN_POINT('',(110.706045566976,-1.05,48.3384059748245));
#197208=CARTESIAN_POINT('',(110.763288540846,-1.05,48.0439178732948));
#197209=CARTESIAN_POINT('',(111.196859069526,-1.05,48.4338109312737));
#197210=CARTESIAN_POINT('',(111.254102043395,-1.05,48.139322829744));
#197211=CARTESIAN_POINT('Origin',(110.763288540846,-1.05,48.0439178732948));
#197212=CARTESIAN_POINT('',(110.706045566976,-1.05,48.3384059748245));
#197213=CARTESIAN_POINT('',(110.763288540846,-1.05,48.0439178732948));
#197214=CARTESIAN_POINT('Origin',(110.763288540846,-1.35,48.0439178732948));
#197215=CARTESIAN_POINT('',(111.254102043395,-1.35,48.139322829744));
#197216=CARTESIAN_POINT('',(111.196859069526,-1.35,48.4338109312737));
#197217=CARTESIAN_POINT('',(111.254102043395,-1.35,48.139322829744));
#197218=CARTESIAN_POINT('',(110.706045566976,-1.35,48.3384059748245));
#197219=CARTESIAN_POINT('',(110.706045566976,-1.35,48.3384059748245));
#197220=CARTESIAN_POINT('',(110.763288540846,-1.35,48.0439178732948));
#197221=CARTESIAN_POINT('',(110.763288540846,-1.35,48.0439178732948));
#197222=CARTESIAN_POINT('',(110.763288540846,-1.35,48.0439178732948));
#197223=CARTESIAN_POINT('Origin',(111.254102043395,-1.35,48.139322829744));
#197224=CARTESIAN_POINT('',(111.254102043395,-1.85,48.139322829744));
#197225=CARTESIAN_POINT('',(111.196859069526,-1.85,48.4338109312737));
#197226=CARTESIAN_POINT('',(111.254102043395,-1.85,48.139322829744));
#197227=CARTESIAN_POINT('',(111.196859069526,-1.35,48.4338109312737));
#197228=CARTESIAN_POINT('',(111.254102043395,-1.35,48.139322829744));
#197229=CARTESIAN_POINT('Origin',(111.254102043395,-1.85,48.139322829744));
#197230=CARTESIAN_POINT('',(110.763288540846,-1.85,48.0439178732948));
#197231=CARTESIAN_POINT('',(110.706045566976,-1.85,48.3384059748245));
#197232=CARTESIAN_POINT('',(110.763288540846,-1.85,48.0439178732948));
#197233=CARTESIAN_POINT('',(111.196859069526,-1.85,48.4338109312737));
#197234=CARTESIAN_POINT('',(111.254102043395,-1.85,48.139322829744));
#197235=CARTESIAN_POINT('Origin',(110.763288540846,-1.85,48.0439178732948));
#197236=CARTESIAN_POINT('',(110.706045566976,-1.85,48.3384059748245));
#197237=CARTESIAN_POINT('',(110.763288540846,-1.85,48.0439178732948));
#197238=CARTESIAN_POINT('Origin',(110.763288540846,-2.15,48.0439178732948));
#197239=CARTESIAN_POINT('',(111.254102043395,-2.15,48.139322829744));
#197240=CARTESIAN_POINT('',(111.196859069526,-2.15,48.4338109312737));
#197241=CARTESIAN_POINT('',(111.254102043395,-2.15,48.139322829744));
#197242=CARTESIAN_POINT('',(110.706045566976,-2.15,48.3384059748245));
#197243=CARTESIAN_POINT('',(110.706045566976,-2.15,48.3384059748245));
#197244=CARTESIAN_POINT('',(110.763288540846,-2.15,48.0439178732948));
#197245=CARTESIAN_POINT('',(110.763288540846,-2.15,48.0439178732948));
#197246=CARTESIAN_POINT('',(110.763288540846,-2.15,48.0439178732948));
#197247=CARTESIAN_POINT('Origin',(111.254102043395,-2.15,48.139322829744));
#197248=CARTESIAN_POINT('',(111.254102043395,-2.65,48.139322829744));
#197249=CARTESIAN_POINT('',(111.196859069526,-2.65,48.4338109312737));
#197250=CARTESIAN_POINT('',(111.254102043395,-2.65,48.139322829744));
#197251=CARTESIAN_POINT('',(111.196859069526,-2.15,48.4338109312737));
#197252=CARTESIAN_POINT('',(111.254102043395,-2.15,48.139322829744));
#197253=CARTESIAN_POINT('Origin',(111.254102043395,-2.65,48.139322829744));
#197254=CARTESIAN_POINT('',(110.763288540846,-2.65,48.0439178732948));
#197255=CARTESIAN_POINT('',(110.706045566976,-2.65,48.3384059748245));
#197256=CARTESIAN_POINT('',(110.763288540846,-2.65,48.0439178732948));
#197257=CARTESIAN_POINT('',(111.196859069526,-2.65,48.4338109312737));
#197258=CARTESIAN_POINT('',(111.254102043395,-2.65,48.139322829744));
#197259=CARTESIAN_POINT('Origin',(110.763288540846,-2.65,48.0439178732948));
#197260=CARTESIAN_POINT('',(110.706045566976,-2.65,48.3384059748245));
#197261=CARTESIAN_POINT('',(110.763288540846,-2.65,48.0439178732948));
#197262=CARTESIAN_POINT('Origin',(110.763288540846,-2.95,48.0439178732948));
#197263=CARTESIAN_POINT('',(111.254102043395,-2.95,48.139322829744));
#197264=CARTESIAN_POINT('',(111.196859069526,-2.95,48.4338109312737));
#197265=CARTESIAN_POINT('',(111.254102043395,-2.95,48.139322829744));
#197266=CARTESIAN_POINT('',(110.706045566976,-2.95,48.3384059748245));
#197267=CARTESIAN_POINT('',(110.706045566976,-2.95,48.3384059748245));
#197268=CARTESIAN_POINT('',(110.763288540846,-2.95,48.0439178732948));
#197269=CARTESIAN_POINT('',(110.763288540846,-2.95,48.0439178732948));
#197270=CARTESIAN_POINT('',(110.763288540846,-2.95,48.0439178732948));
#197271=CARTESIAN_POINT('Origin',(111.254102043395,-2.95,48.139322829744));
#197272=CARTESIAN_POINT('',(111.254102043395,-3.45,48.139322829744));
#197273=CARTESIAN_POINT('',(111.196859069526,-3.45,48.4338109312737));
#197274=CARTESIAN_POINT('',(111.254102043395,-3.45,48.139322829744));
#197275=CARTESIAN_POINT('',(111.196859069526,-2.95,48.4338109312737));
#197276=CARTESIAN_POINT('',(111.254102043395,-2.95,48.139322829744));
#197277=CARTESIAN_POINT('Origin',(111.254102043395,-3.45,48.139322829744));
#197278=CARTESIAN_POINT('',(110.763288540846,-3.45,48.0439178732948));
#197279=CARTESIAN_POINT('',(110.706045566976,-3.45,48.3384059748245));
#197280=CARTESIAN_POINT('',(110.763288540846,-3.45,48.0439178732948));
#197281=CARTESIAN_POINT('',(111.196859069526,-3.45,48.4338109312737));
#197282=CARTESIAN_POINT('',(111.254102043395,-3.45,48.139322829744));
#197283=CARTESIAN_POINT('Origin',(110.763288540846,-3.45,48.0439178732948));
#197284=CARTESIAN_POINT('',(110.706045566976,-3.45,48.3384059748245));
#197285=CARTESIAN_POINT('',(110.763288540846,-3.45,48.0439178732948));
#197286=CARTESIAN_POINT('Origin',(110.763288540846,-3.75,48.0439178732948));
#197287=CARTESIAN_POINT('',(111.254102043395,-3.75,48.139322829744));
#197288=CARTESIAN_POINT('',(111.196859069526,-3.75,48.4338109312737));
#197289=CARTESIAN_POINT('',(111.254102043395,-3.75,48.139322829744));
#197290=CARTESIAN_POINT('',(110.706045566976,-3.75,48.3384059748245));
#197291=CARTESIAN_POINT('',(110.706045566976,-3.75,48.3384059748245));
#197292=CARTESIAN_POINT('',(110.763288540846,-3.75,48.0439178732948));
#197293=CARTESIAN_POINT('',(110.763288540846,-3.75,48.0439178732948));
#197294=CARTESIAN_POINT('',(110.763288540846,-3.75,48.0439178732948));
#197295=CARTESIAN_POINT('Origin',(111.254102043395,-3.75,48.139322829744));
#197296=CARTESIAN_POINT('',(111.254102043395,-4.25,48.139322829744));
#197297=CARTESIAN_POINT('',(111.196859069526,-4.25,48.4338109312737));
#197298=CARTESIAN_POINT('',(111.254102043395,-4.25,48.139322829744));
#197299=CARTESIAN_POINT('',(111.196859069526,-3.75,48.4338109312737));
#197300=CARTESIAN_POINT('',(111.254102043395,-3.75,48.139322829744));
#197301=CARTESIAN_POINT('Origin',(111.254102043395,-4.25,48.139322829744));
#197302=CARTESIAN_POINT('',(110.763288540846,-4.25,48.0439178732948));
#197303=CARTESIAN_POINT('',(110.706045566976,-4.25,48.3384059748245));
#197304=CARTESIAN_POINT('',(110.763288540846,-4.25,48.0439178732948));
#197305=CARTESIAN_POINT('',(111.196859069526,-4.25,48.4338109312737));
#197306=CARTESIAN_POINT('',(111.254102043395,-4.25,48.139322829744));
#197307=CARTESIAN_POINT('Origin',(110.763288540846,-4.25,48.0439178732948));
#197308=CARTESIAN_POINT('',(110.706045566976,-4.25,48.3384059748245));
#197309=CARTESIAN_POINT('',(110.763288540846,-4.25,48.0439178732948));
#197310=CARTESIAN_POINT('Origin',(110.763288540846,-4.55,48.0439178732948));
#197311=CARTESIAN_POINT('',(111.254102043395,-4.55,48.139322829744));
#197312=CARTESIAN_POINT('',(111.196859069526,-4.55,48.4338109312737));
#197313=CARTESIAN_POINT('',(111.254102043395,-4.55,48.139322829744));
#197314=CARTESIAN_POINT('',(110.706045566976,-4.55,48.3384059748245));
#197315=CARTESIAN_POINT('',(110.706045566976,-4.55,48.3384059748245));
#197316=CARTESIAN_POINT('',(110.763288540846,-4.55,48.0439178732948));
#197317=CARTESIAN_POINT('',(110.763288540846,-4.55,48.0439178732948));
#197318=CARTESIAN_POINT('',(110.763288540846,-4.55,48.0439178732948));
#197319=CARTESIAN_POINT('Origin',(111.254102043395,-4.55,48.139322829744));
#197320=CARTESIAN_POINT('',(111.254102043395,-5.05,48.139322829744));
#197321=CARTESIAN_POINT('',(111.196859069526,-5.05,48.4338109312737));
#197322=CARTESIAN_POINT('',(111.254102043395,-5.05,48.139322829744));
#197323=CARTESIAN_POINT('',(111.196859069526,-4.55,48.4338109312737));
#197324=CARTESIAN_POINT('',(111.254102043395,-4.55,48.139322829744));
#197325=CARTESIAN_POINT('Origin',(111.254102043395,-5.05,48.139322829744));
#197326=CARTESIAN_POINT('',(110.763288540846,-5.05,48.0439178732948));
#197327=CARTESIAN_POINT('',(110.706045566976,-5.05,48.3384059748245));
#197328=CARTESIAN_POINT('',(110.763288540846,-5.05,48.0439178732948));
#197329=CARTESIAN_POINT('',(111.196859069526,-5.05,48.4338109312737));
#197330=CARTESIAN_POINT('',(111.254102043395,-5.05,48.139322829744));
#197331=CARTESIAN_POINT('Origin',(110.763288540846,-5.05,48.0439178732948));
#197332=CARTESIAN_POINT('',(110.706045566976,-5.05,48.3384059748245));
#197333=CARTESIAN_POINT('',(110.763288540846,-5.05,48.0439178732948));
#197334=CARTESIAN_POINT('Origin',(110.763288540846,-5.35,48.0439178732948));
#197335=CARTESIAN_POINT('',(111.254102043395,-5.35,48.139322829744));
#197336=CARTESIAN_POINT('',(111.196859069526,-5.35,48.4338109312737));
#197337=CARTESIAN_POINT('',(111.254102043395,-5.35,48.139322829744));
#197338=CARTESIAN_POINT('',(110.706045566976,-5.35,48.3384059748245));
#197339=CARTESIAN_POINT('',(110.706045566976,-5.35,48.3384059748245));
#197340=CARTESIAN_POINT('',(110.763288540846,-5.35,48.0439178732948));
#197341=CARTESIAN_POINT('',(110.763288540846,-5.35,48.0439178732948));
#197342=CARTESIAN_POINT('',(110.763288540846,-5.35,48.0439178732948));
#197343=CARTESIAN_POINT('Origin',(111.254102043395,-5.35,48.139322829744));
#197344=CARTESIAN_POINT('',(111.254102043395,-5.85,48.139322829744));
#197345=CARTESIAN_POINT('',(111.196859069526,-5.85,48.4338109312737));
#197346=CARTESIAN_POINT('',(111.254102043395,-5.85,48.139322829744));
#197347=CARTESIAN_POINT('',(111.196859069526,-5.35,48.4338109312737));
#197348=CARTESIAN_POINT('',(111.254102043395,-5.35,48.139322829744));
#197349=CARTESIAN_POINT('Origin',(111.254102043395,-5.85,48.139322829744));
#197350=CARTESIAN_POINT('',(110.763288540846,-5.85,48.0439178732948));
#197351=CARTESIAN_POINT('',(110.706045566976,-5.85,48.3384059748245));
#197352=CARTESIAN_POINT('',(110.763288540846,-5.85,48.0439178732948));
#197353=CARTESIAN_POINT('',(111.196859069526,-5.85,48.4338109312737));
#197354=CARTESIAN_POINT('',(111.254102043395,-5.85,48.139322829744));
#197355=CARTESIAN_POINT('Origin',(110.763288540846,-5.85,48.0439178732948));
#197356=CARTESIAN_POINT('',(110.706045566976,-5.85,48.3384059748245));
#197357=CARTESIAN_POINT('',(110.763288540846,-5.85,48.0439178732948));
#197358=CARTESIAN_POINT('Origin',(110.763288540846,-6.15,48.0439178732948));
#197359=CARTESIAN_POINT('',(111.254102043395,-6.15,48.139322829744));
#197360=CARTESIAN_POINT('',(111.196859069526,-6.15,48.4338109312737));
#197361=CARTESIAN_POINT('',(111.254102043395,-6.15,48.139322829744));
#197362=CARTESIAN_POINT('',(110.706045566976,-6.15,48.3384059748245));
#197363=CARTESIAN_POINT('',(110.706045566976,-6.15,48.3384059748245));
#197364=CARTESIAN_POINT('',(110.763288540846,-6.15,48.0439178732948));
#197365=CARTESIAN_POINT('',(110.763288540846,-6.15,48.0439178732948));
#197366=CARTESIAN_POINT('',(110.763288540846,-6.15,48.0439178732948));
#197367=CARTESIAN_POINT('Origin',(111.254102043395,-6.15,48.139322829744));
#197368=CARTESIAN_POINT('',(111.254102043395,-6.65,48.139322829744));
#197369=CARTESIAN_POINT('',(111.196859069526,-6.65,48.4338109312737));
#197370=CARTESIAN_POINT('',(111.254102043395,-6.65,48.139322829744));
#197371=CARTESIAN_POINT('',(111.196859069526,-6.15,48.4338109312737));
#197372=CARTESIAN_POINT('',(111.254102043395,-6.15,48.139322829744));
#197373=CARTESIAN_POINT('Origin',(111.254102043395,-6.65,48.139322829744));
#197374=CARTESIAN_POINT('',(110.763288540846,-6.65,48.0439178732948));
#197375=CARTESIAN_POINT('',(110.706045566976,-6.65,48.3384059748245));
#197376=CARTESIAN_POINT('',(110.763288540846,-6.65,48.0439178732948));
#197377=CARTESIAN_POINT('',(111.196859069526,-6.65,48.4338109312737));
#197378=CARTESIAN_POINT('',(111.254102043395,-6.65,48.139322829744));
#197379=CARTESIAN_POINT('Origin',(110.763288540846,-6.65,48.0439178732948));
#197380=CARTESIAN_POINT('',(110.706045566976,-6.65,48.3384059748245));
#197381=CARTESIAN_POINT('',(110.763288540846,-6.65,48.0439178732948));
#197382=CARTESIAN_POINT('Origin',(111.548590144925,-6.15,48.1965658036136));
#197383=CARTESIAN_POINT('',(112.039403647474,-6.15,48.2919707600629));
#197384=CARTESIAN_POINT('',(111.982160673605,-6.15,48.5864588615926));
#197385=CARTESIAN_POINT('',(112.039403647474,-6.15,48.2919707600629));
#197386=CARTESIAN_POINT('',(111.491347171055,-6.15,48.4910539051433));
#197387=CARTESIAN_POINT('',(111.491347171055,-6.15,48.4910539051433));
#197388=CARTESIAN_POINT('',(111.548590144925,-6.15,48.1965658036136));
#197389=CARTESIAN_POINT('',(111.548590144925,-6.15,48.1965658036136));
#197390=CARTESIAN_POINT('',(111.548590144925,-6.15,48.1965658036136));
#197391=CARTESIAN_POINT('Origin',(112.039403647474,-6.15,48.2919707600629));
#197392=CARTESIAN_POINT('',(112.039403647474,-6.65,48.2919707600629));
#197393=CARTESIAN_POINT('',(111.982160673605,-6.65,48.5864588615926));
#197394=CARTESIAN_POINT('',(112.039403647474,-6.65,48.2919707600629));
#197395=CARTESIAN_POINT('',(111.982160673605,-6.15,48.5864588615926));
#197396=CARTESIAN_POINT('',(112.039403647474,-6.15,48.2919707600629));
#197397=CARTESIAN_POINT('Origin',(112.039403647474,-6.65,48.2919707600629));
#197398=CARTESIAN_POINT('',(111.548590144925,-6.65,48.1965658036136));
#197399=CARTESIAN_POINT('',(111.491347171055,-6.65,48.4910539051433));
#197400=CARTESIAN_POINT('',(111.548590144925,-6.65,48.1965658036136));
#197401=CARTESIAN_POINT('',(111.982160673605,-6.65,48.5864588615926));
#197402=CARTESIAN_POINT('',(112.039403647474,-6.65,48.2919707600629));
#197403=CARTESIAN_POINT('Origin',(111.548590144925,-6.65,48.1965658036136));
#197404=CARTESIAN_POINT('',(111.491347171055,-6.65,48.4910539051433));
#197405=CARTESIAN_POINT('',(111.548590144925,-6.65,48.1965658036136));
#197406=CARTESIAN_POINT('Origin',(112.333891749004,-6.15,48.3492137339324));
#197407=CARTESIAN_POINT('',(112.824705251554,-6.15,48.4446186903817));
#197408=CARTESIAN_POINT('',(112.767462277684,-6.15,48.7391067919114));
#197409=CARTESIAN_POINT('',(112.824705251554,-6.15,48.4446186903817));
#197410=CARTESIAN_POINT('',(112.276648775135,-6.15,48.6437018354621));
#197411=CARTESIAN_POINT('',(112.276648775135,-6.15,48.6437018354621));
#197412=CARTESIAN_POINT('',(112.333891749004,-6.15,48.3492137339324));
#197413=CARTESIAN_POINT('',(112.333891749004,-6.15,48.3492137339324));
#197414=CARTESIAN_POINT('',(112.333891749004,-6.15,48.3492137339324));
#197415=CARTESIAN_POINT('Origin',(112.824705251554,-6.15,48.4446186903817));
#197416=CARTESIAN_POINT('',(112.824705251554,-6.65,48.4446186903817));
#197417=CARTESIAN_POINT('',(112.767462277684,-6.65,48.7391067919114));
#197418=CARTESIAN_POINT('',(112.824705251554,-6.65,48.4446186903817));
#197419=CARTESIAN_POINT('',(112.767462277684,-6.15,48.7391067919114));
#197420=CARTESIAN_POINT('',(112.824705251554,-6.15,48.4446186903817));
#197421=CARTESIAN_POINT('Origin',(112.824705251554,-6.65,48.4446186903817));
#197422=CARTESIAN_POINT('',(112.333891749004,-6.65,48.3492137339324));
#197423=CARTESIAN_POINT('',(112.276648775135,-6.65,48.6437018354621));
#197424=CARTESIAN_POINT('',(112.333891749004,-6.65,48.3492137339324));
#197425=CARTESIAN_POINT('',(112.767462277684,-6.65,48.7391067919114));
#197426=CARTESIAN_POINT('',(112.824705251554,-6.65,48.4446186903817));
#197427=CARTESIAN_POINT('Origin',(112.333891749004,-6.65,48.3492137339324));
#197428=CARTESIAN_POINT('',(112.276648775135,-6.65,48.6437018354621));
#197429=CARTESIAN_POINT('',(112.333891749004,-6.65,48.3492137339324));
#197430=CARTESIAN_POINT('Origin',(113.119193353083,-6.15,48.5018616642512));
#197431=CARTESIAN_POINT('',(113.610006855633,-6.15,48.5972666207005));
#197432=CARTESIAN_POINT('',(113.552763881763,-6.15,48.8917547222302));
#197433=CARTESIAN_POINT('',(113.610006855633,-6.15,48.5972666207005));
#197434=CARTESIAN_POINT('',(113.061950379214,-6.15,48.7963497657809));
#197435=CARTESIAN_POINT('',(113.061950379214,-6.15,48.7963497657809));
#197436=CARTESIAN_POINT('',(113.119193353083,-6.15,48.5018616642512));
#197437=CARTESIAN_POINT('',(113.119193353083,-6.15,48.5018616642512));
#197438=CARTESIAN_POINT('',(113.119193353083,-6.15,48.5018616642512));
#197439=CARTESIAN_POINT('Origin',(113.610006855633,-6.15,48.5972666207005));
#197440=CARTESIAN_POINT('',(113.610006855633,-6.65,48.5972666207005));
#197441=CARTESIAN_POINT('',(113.552763881763,-6.65,48.8917547222302));
#197442=CARTESIAN_POINT('',(113.610006855633,-6.65,48.5972666207005));
#197443=CARTESIAN_POINT('',(113.552763881763,-6.15,48.8917547222302));
#197444=CARTESIAN_POINT('',(113.610006855633,-6.15,48.5972666207005));
#197445=CARTESIAN_POINT('Origin',(113.610006855633,-6.65,48.5972666207005));
#197446=CARTESIAN_POINT('',(113.119193353083,-6.65,48.5018616642512));
#197447=CARTESIAN_POINT('',(113.061950379214,-6.65,48.7963497657809));
#197448=CARTESIAN_POINT('',(113.119193353083,-6.65,48.5018616642512));
#197449=CARTESIAN_POINT('',(113.552763881763,-6.65,48.8917547222302));
#197450=CARTESIAN_POINT('',(113.610006855633,-6.65,48.5972666207005));
#197451=CARTESIAN_POINT('Origin',(113.119193353083,-6.65,48.5018616642512));
#197452=CARTESIAN_POINT('',(113.061950379214,-6.65,48.7963497657809));
#197453=CARTESIAN_POINT('',(113.119193353083,-6.65,48.5018616642512));
#197454=CARTESIAN_POINT('Origin',(113.904494957163,-6.15,48.65450959457));
#197455=CARTESIAN_POINT('',(114.395308459712,-6.15,48.7499145510193));
#197456=CARTESIAN_POINT('',(114.338065485842,-6.15,49.044402652549));
#197457=CARTESIAN_POINT('',(114.395308459712,-6.15,48.7499145510193));
#197458=CARTESIAN_POINT('',(113.847251983293,-6.15,48.9489976960997));
#197459=CARTESIAN_POINT('',(113.847251983293,-6.15,48.9489976960997));
#197460=CARTESIAN_POINT('',(113.904494957163,-6.15,48.65450959457));
#197461=CARTESIAN_POINT('',(113.904494957163,-6.15,48.65450959457));
#197462=CARTESIAN_POINT('',(113.904494957163,-6.15,48.65450959457));
#197463=CARTESIAN_POINT('Origin',(114.395308459712,-6.15,48.7499145510193));
#197464=CARTESIAN_POINT('',(114.395308459712,-6.65,48.7499145510193));
#197465=CARTESIAN_POINT('',(114.338065485842,-6.65,49.044402652549));
#197466=CARTESIAN_POINT('',(114.395308459712,-6.65,48.7499145510193));
#197467=CARTESIAN_POINT('',(114.338065485842,-6.15,49.044402652549));
#197468=CARTESIAN_POINT('',(114.395308459712,-6.15,48.7499145510193));
#197469=CARTESIAN_POINT('Origin',(114.395308459712,-6.65,48.7499145510193));
#197470=CARTESIAN_POINT('',(113.904494957163,-6.65,48.65450959457));
#197471=CARTESIAN_POINT('',(113.847251983293,-6.65,48.9489976960997));
#197472=CARTESIAN_POINT('',(113.904494957163,-6.65,48.65450959457));
#197473=CARTESIAN_POINT('',(114.338065485842,-6.65,49.044402652549));
#197474=CARTESIAN_POINT('',(114.395308459712,-6.65,48.7499145510193));
#197475=CARTESIAN_POINT('Origin',(113.904494957163,-6.65,48.65450959457));
#197476=CARTESIAN_POINT('',(113.847251983293,-6.65,48.9489976960997));
#197477=CARTESIAN_POINT('',(113.904494957163,-6.65,48.65450959457));
#197478=CARTESIAN_POINT('Origin',(114.689796561242,-6.15,48.8071575248888));
#197479=CARTESIAN_POINT('',(115.180610063791,-6.15,48.9025624813381));
#197480=CARTESIAN_POINT('',(115.123367089922,-6.15,49.1970505828678));
#197481=CARTESIAN_POINT('',(115.180610063791,-6.15,48.9025624813381));
#197482=CARTESIAN_POINT('',(114.632553587372,-6.15,49.1016456264185));
#197483=CARTESIAN_POINT('',(114.632553587372,-6.15,49.1016456264185));
#197484=CARTESIAN_POINT('',(114.689796561242,-6.15,48.8071575248888));
#197485=CARTESIAN_POINT('',(114.689796561242,-6.15,48.8071575248888));
#197486=CARTESIAN_POINT('',(114.689796561242,-6.15,48.8071575248888));
#197487=CARTESIAN_POINT('Origin',(115.180610063791,-6.15,48.9025624813381));
#197488=CARTESIAN_POINT('',(115.180610063791,-6.65,48.9025624813381));
#197489=CARTESIAN_POINT('',(115.123367089922,-6.65,49.1970505828678));
#197490=CARTESIAN_POINT('',(115.180610063791,-6.65,48.9025624813381));
#197491=CARTESIAN_POINT('',(115.123367089922,-6.15,49.1970505828678));
#197492=CARTESIAN_POINT('',(115.180610063791,-6.15,48.9025624813381));
#197493=CARTESIAN_POINT('Origin',(115.180610063791,-6.65,48.9025624813381));
#197494=CARTESIAN_POINT('',(114.689796561242,-6.65,48.8071575248888));
#197495=CARTESIAN_POINT('',(114.632553587372,-6.65,49.1016456264185));
#197496=CARTESIAN_POINT('',(114.689796561242,-6.65,48.8071575248888));
#197497=CARTESIAN_POINT('',(115.123367089922,-6.65,49.1970505828678));
#197498=CARTESIAN_POINT('',(115.180610063791,-6.65,48.9025624813381));
#197499=CARTESIAN_POINT('Origin',(114.689796561242,-6.65,48.8071575248888));
#197500=CARTESIAN_POINT('',(114.632553587372,-6.65,49.1016456264185));
#197501=CARTESIAN_POINT('',(114.689796561242,-6.65,48.8071575248888));
#197502=CARTESIAN_POINT('Origin',(115.475098165321,-6.15,48.9598054552076));
#197503=CARTESIAN_POINT('',(115.96591166787,-6.15,49.0552104116569));
#197504=CARTESIAN_POINT('',(115.908668694001,-6.15,49.3496985131866));
#197505=CARTESIAN_POINT('',(115.96591166787,-6.15,49.0552104116569));
#197506=CARTESIAN_POINT('',(115.417855191451,-6.15,49.2542935567373));
#197507=CARTESIAN_POINT('',(115.417855191451,-6.15,49.2542935567373));
#197508=CARTESIAN_POINT('',(115.475098165321,-6.15,48.9598054552076));
#197509=CARTESIAN_POINT('',(115.475098165321,-6.15,48.9598054552076));
#197510=CARTESIAN_POINT('',(115.475098165321,-6.15,48.9598054552076));
#197511=CARTESIAN_POINT('Origin',(115.96591166787,-6.15,49.0552104116569));
#197512=CARTESIAN_POINT('',(115.96591166787,-6.65,49.0552104116569));
#197513=CARTESIAN_POINT('',(115.908668694001,-6.65,49.3496985131866));
#197514=CARTESIAN_POINT('',(115.96591166787,-6.65,49.0552104116569));
#197515=CARTESIAN_POINT('',(115.908668694001,-6.15,49.3496985131866));
#197516=CARTESIAN_POINT('',(115.96591166787,-6.15,49.0552104116569));
#197517=CARTESIAN_POINT('Origin',(115.96591166787,-6.65,49.0552104116569));
#197518=CARTESIAN_POINT('',(115.475098165321,-6.65,48.9598054552076));
#197519=CARTESIAN_POINT('',(115.417855191451,-6.65,49.2542935567373));
#197520=CARTESIAN_POINT('',(115.475098165321,-6.65,48.9598054552076));
#197521=CARTESIAN_POINT('',(115.908668694001,-6.65,49.3496985131866));
#197522=CARTESIAN_POINT('',(115.96591166787,-6.65,49.0552104116569));
#197523=CARTESIAN_POINT('Origin',(115.475098165321,-6.65,48.9598054552076));
#197524=CARTESIAN_POINT('',(115.417855191451,-6.65,49.2542935567373));
#197525=CARTESIAN_POINT('',(115.475098165321,-6.65,48.9598054552076));
#197526=CARTESIAN_POINT('Origin',(116.2603997694,-6.15,49.1124533855264));
#197527=CARTESIAN_POINT('',(116.75121327195,-6.15,49.2078583419757));
#197528=CARTESIAN_POINT('',(116.69397029808,-6.15,49.5023464435054));
#197529=CARTESIAN_POINT('',(116.75121327195,-6.15,49.2078583419757));
#197530=CARTESIAN_POINT('',(116.203156795531,-6.15,49.4069414870561));
#197531=CARTESIAN_POINT('',(116.203156795531,-6.15,49.4069414870561));
#197532=CARTESIAN_POINT('',(116.2603997694,-6.15,49.1124533855264));
#197533=CARTESIAN_POINT('',(116.2603997694,-6.15,49.1124533855264));
#197534=CARTESIAN_POINT('',(116.2603997694,-6.15,49.1124533855264));
#197535=CARTESIAN_POINT('Origin',(116.75121327195,-6.15,49.2078583419757));
#197536=CARTESIAN_POINT('',(116.75121327195,-6.65,49.2078583419757));
#197537=CARTESIAN_POINT('',(116.69397029808,-6.65,49.5023464435054));
#197538=CARTESIAN_POINT('',(116.75121327195,-6.65,49.2078583419757));
#197539=CARTESIAN_POINT('',(116.69397029808,-6.15,49.5023464435054));
#197540=CARTESIAN_POINT('',(116.75121327195,-6.15,49.2078583419757));
#197541=CARTESIAN_POINT('Origin',(116.75121327195,-6.65,49.2078583419757));
#197542=CARTESIAN_POINT('',(116.2603997694,-6.65,49.1124533855264));
#197543=CARTESIAN_POINT('',(116.203156795531,-6.65,49.4069414870561));
#197544=CARTESIAN_POINT('',(116.2603997694,-6.65,49.1124533855264));
#197545=CARTESIAN_POINT('',(116.69397029808,-6.65,49.5023464435054));
#197546=CARTESIAN_POINT('',(116.75121327195,-6.65,49.2078583419757));
#197547=CARTESIAN_POINT('Origin',(116.2603997694,-6.65,49.1124533855264));
#197548=CARTESIAN_POINT('',(116.203156795531,-6.65,49.4069414870561));
#197549=CARTESIAN_POINT('',(116.2603997694,-6.65,49.1124533855264));
#197550=CARTESIAN_POINT('Origin',(117.045701373479,-6.15,49.2651013158452));
#197551=CARTESIAN_POINT('',(117.536514876029,-6.15,49.3605062722945));
#197552=CARTESIAN_POINT('',(117.479271902159,-6.15,49.6549943738242));
#197553=CARTESIAN_POINT('',(117.536514876029,-6.15,49.3605062722945));
#197554=CARTESIAN_POINT('',(116.98845839961,-6.15,49.5595894173749));
#197555=CARTESIAN_POINT('',(116.98845839961,-6.15,49.5595894173749));
#197556=CARTESIAN_POINT('',(117.045701373479,-6.15,49.2651013158452));
#197557=CARTESIAN_POINT('',(117.045701373479,-6.15,49.2651013158452));
#197558=CARTESIAN_POINT('',(117.045701373479,-6.15,49.2651013158452));
#197559=CARTESIAN_POINT('Origin',(117.536514876029,-6.15,49.3605062722945));
#197560=CARTESIAN_POINT('',(117.536514876029,-6.65,49.3605062722945));
#197561=CARTESIAN_POINT('',(117.479271902159,-6.65,49.6549943738242));
#197562=CARTESIAN_POINT('',(117.536514876029,-6.65,49.3605062722945));
#197563=CARTESIAN_POINT('',(117.479271902159,-6.15,49.6549943738242));
#197564=CARTESIAN_POINT('',(117.536514876029,-6.15,49.3605062722945));
#197565=CARTESIAN_POINT('Origin',(117.536514876029,-6.65,49.3605062722945));
#197566=CARTESIAN_POINT('',(117.045701373479,-6.65,49.2651013158452));
#197567=CARTESIAN_POINT('',(116.98845839961,-6.65,49.5595894173749));
#197568=CARTESIAN_POINT('',(117.045701373479,-6.65,49.2651013158452));
#197569=CARTESIAN_POINT('',(117.479271902159,-6.65,49.6549943738242));
#197570=CARTESIAN_POINT('',(117.536514876029,-6.65,49.3605062722945));
#197571=CARTESIAN_POINT('Origin',(117.045701373479,-6.65,49.2651013158452));
#197572=CARTESIAN_POINT('',(116.98845839961,-6.65,49.5595894173749));
#197573=CARTESIAN_POINT('',(117.045701373479,-6.65,49.2651013158452));
#197574=CARTESIAN_POINT('Origin',(117.831002977559,-6.15,49.417749246164));
#197575=CARTESIAN_POINT('',(118.321816480108,-6.15,49.5131542026133));
#197576=CARTESIAN_POINT('',(118.264573506239,-6.15,49.807642304143));
#197577=CARTESIAN_POINT('',(118.321816480108,-6.15,49.5131542026133));
#197578=CARTESIAN_POINT('',(117.773760003689,-6.15,49.7122373476937));
#197579=CARTESIAN_POINT('',(117.773760003689,-6.15,49.7122373476937));
#197580=CARTESIAN_POINT('',(117.831002977559,-6.15,49.417749246164));
#197581=CARTESIAN_POINT('',(117.831002977559,-6.15,49.417749246164));
#197582=CARTESIAN_POINT('',(117.831002977559,-6.15,49.417749246164));
#197583=CARTESIAN_POINT('Origin',(118.321816480108,-6.15,49.5131542026133));
#197584=CARTESIAN_POINT('',(118.321816480108,-6.65,49.5131542026133));
#197585=CARTESIAN_POINT('',(118.264573506239,-6.65,49.807642304143));
#197586=CARTESIAN_POINT('',(118.321816480108,-6.65,49.5131542026133));
#197587=CARTESIAN_POINT('',(118.264573506239,-6.15,49.807642304143));
#197588=CARTESIAN_POINT('',(118.321816480108,-6.15,49.5131542026133));
#197589=CARTESIAN_POINT('Origin',(118.321816480108,-6.65,49.5131542026133));
#197590=CARTESIAN_POINT('',(117.831002977559,-6.65,49.417749246164));
#197591=CARTESIAN_POINT('',(117.773760003689,-6.65,49.7122373476937));
#197592=CARTESIAN_POINT('',(117.831002977559,-6.65,49.417749246164));
#197593=CARTESIAN_POINT('',(118.264573506239,-6.65,49.807642304143));
#197594=CARTESIAN_POINT('',(118.321816480108,-6.65,49.5131542026133));
#197595=CARTESIAN_POINT('Origin',(117.831002977559,-6.65,49.417749246164));
#197596=CARTESIAN_POINT('',(117.773760003689,-6.65,49.7122373476937));
#197597=CARTESIAN_POINT('',(117.831002977559,-6.65,49.417749246164));
#197598=CARTESIAN_POINT('Origin',(118.616304581638,-6.15,49.5703971764828));
#197599=CARTESIAN_POINT('',(119.107118084187,-6.15,49.6658021329321));
#197600=CARTESIAN_POINT('',(119.049875110318,-6.15,49.9602902344618));
#197601=CARTESIAN_POINT('',(119.107118084187,-6.15,49.6658021329321));
#197602=CARTESIAN_POINT('',(118.559061607768,-6.15,49.8648852780125));
#197603=CARTESIAN_POINT('',(118.559061607768,-6.15,49.8648852780125));
#197604=CARTESIAN_POINT('',(118.616304581638,-6.15,49.5703971764828));
#197605=CARTESIAN_POINT('',(118.616304581638,-6.15,49.5703971764828));
#197606=CARTESIAN_POINT('',(118.616304581638,-6.15,49.5703971764828));
#197607=CARTESIAN_POINT('Origin',(119.107118084187,-6.15,49.6658021329321));
#197608=CARTESIAN_POINT('',(119.107118084187,-6.65,49.6658021329321));
#197609=CARTESIAN_POINT('',(119.049875110318,-6.65,49.9602902344618));
#197610=CARTESIAN_POINT('',(119.107118084187,-6.65,49.6658021329321));
#197611=CARTESIAN_POINT('',(119.049875110318,-6.15,49.9602902344618));
#197612=CARTESIAN_POINT('',(119.107118084187,-6.15,49.6658021329321));
#197613=CARTESIAN_POINT('Origin',(119.107118084187,-6.65,49.6658021329321));
#197614=CARTESIAN_POINT('',(118.616304581638,-6.65,49.5703971764828));
#197615=CARTESIAN_POINT('',(118.559061607768,-6.65,49.8648852780125));
#197616=CARTESIAN_POINT('',(118.616304581638,-6.65,49.5703971764828));
#197617=CARTESIAN_POINT('',(119.049875110318,-6.65,49.9602902344618));
#197618=CARTESIAN_POINT('',(119.107118084187,-6.65,49.6658021329321));
#197619=CARTESIAN_POINT('Origin',(118.616304581638,-6.65,49.5703971764828));
#197620=CARTESIAN_POINT('',(118.559061607768,-6.65,49.8648852780125));
#197621=CARTESIAN_POINT('',(118.616304581638,-6.65,49.5703971764828));
#197622=CARTESIAN_POINT('Origin',(119.401606185717,-6.15,49.7230451068016));
#197623=CARTESIAN_POINT('',(119.892419688267,-6.15,49.8184500632509));
#197624=CARTESIAN_POINT('',(119.835176714397,-6.15,50.1129381647806));
#197625=CARTESIAN_POINT('',(119.892419688267,-6.15,49.8184500632509));
#197626=CARTESIAN_POINT('',(119.344363211847,-6.15,50.0175332083313));
#197627=CARTESIAN_POINT('',(119.344363211847,-6.15,50.0175332083313));
#197628=CARTESIAN_POINT('',(119.401606185717,-6.15,49.7230451068016));
#197629=CARTESIAN_POINT('',(119.401606185717,-6.15,49.7230451068016));
#197630=CARTESIAN_POINT('',(119.401606185717,-6.15,49.7230451068016));
#197631=CARTESIAN_POINT('Origin',(119.892419688267,-6.15,49.8184500632509));
#197632=CARTESIAN_POINT('',(119.892419688267,-6.65,49.8184500632509));
#197633=CARTESIAN_POINT('',(119.835176714397,-6.65,50.1129381647806));
#197634=CARTESIAN_POINT('',(119.892419688267,-6.65,49.8184500632509));
#197635=CARTESIAN_POINT('',(119.835176714397,-6.15,50.1129381647806));
#197636=CARTESIAN_POINT('',(119.892419688267,-6.15,49.8184500632509));
#197637=CARTESIAN_POINT('Origin',(119.892419688267,-6.65,49.8184500632509));
#197638=CARTESIAN_POINT('',(119.401606185717,-6.65,49.7230451068016));
#197639=CARTESIAN_POINT('',(119.344363211847,-6.65,50.0175332083313));
#197640=CARTESIAN_POINT('',(119.401606185717,-6.65,49.7230451068016));
#197641=CARTESIAN_POINT('',(119.835176714397,-6.65,50.1129381647806));
#197642=CARTESIAN_POINT('',(119.892419688267,-6.65,49.8184500632509));
#197643=CARTESIAN_POINT('Origin',(119.401606185717,-6.65,49.7230451068016));
#197644=CARTESIAN_POINT('',(119.344363211847,-6.65,50.0175332083313));
#197645=CARTESIAN_POINT('',(119.401606185717,-6.65,49.7230451068016));
#197646=CARTESIAN_POINT('Origin',(120.186907789796,-6.15,49.8756930371204));
#197647=CARTESIAN_POINT('',(120.677721292346,-6.15,49.9710979935697));
#197648=CARTESIAN_POINT('',(120.620478318476,-6.15,50.2655860950994));
#197649=CARTESIAN_POINT('',(120.677721292346,-6.15,49.9710979935697));
#197650=CARTESIAN_POINT('',(120.129664815927,-6.15,50.1701811386501));
#197651=CARTESIAN_POINT('',(120.129664815927,-6.15,50.1701811386501));
#197652=CARTESIAN_POINT('',(120.186907789796,-6.15,49.8756930371204));
#197653=CARTESIAN_POINT('',(120.186907789796,-6.15,49.8756930371204));
#197654=CARTESIAN_POINT('',(120.186907789796,-6.15,49.8756930371204));
#197655=CARTESIAN_POINT('Origin',(120.677721292346,-6.15,49.9710979935697));
#197656=CARTESIAN_POINT('',(120.677721292346,-6.65,49.9710979935697));
#197657=CARTESIAN_POINT('',(120.620478318476,-6.65,50.2655860950994));
#197658=CARTESIAN_POINT('',(120.677721292346,-6.65,49.9710979935697));
#197659=CARTESIAN_POINT('',(120.620478318476,-6.15,50.2655860950994));
#197660=CARTESIAN_POINT('',(120.677721292346,-6.15,49.9710979935697));
#197661=CARTESIAN_POINT('Origin',(120.677721292346,-6.65,49.9710979935697));
#197662=CARTESIAN_POINT('',(120.186907789796,-6.65,49.8756930371204));
#197663=CARTESIAN_POINT('',(120.129664815927,-6.65,50.1701811386501));
#197664=CARTESIAN_POINT('',(120.186907789796,-6.65,49.8756930371204));
#197665=CARTESIAN_POINT('',(120.620478318476,-6.65,50.2655860950994));
#197666=CARTESIAN_POINT('',(120.677721292346,-6.65,49.9710979935697));
#197667=CARTESIAN_POINT('Origin',(120.186907789796,-6.65,49.8756930371204));
#197668=CARTESIAN_POINT('',(120.129664815927,-6.65,50.1701811386501));
#197669=CARTESIAN_POINT('',(120.186907789796,-6.65,49.8756930371204));
#197670=CARTESIAN_POINT('Origin',(120.972209393875,-6.15,50.0283409674392));
#197671=CARTESIAN_POINT('',(121.463022896425,-6.15,50.1237459238885));
#197672=CARTESIAN_POINT('',(121.405779922555,-6.15,50.4182340254182));
#197673=CARTESIAN_POINT('',(121.463022896425,-6.15,50.1237459238885));
#197674=CARTESIAN_POINT('',(120.914966420006,-6.15,50.3228290689689));
#197675=CARTESIAN_POINT('',(120.914966420006,-6.15,50.3228290689689));
#197676=CARTESIAN_POINT('',(120.972209393875,-6.15,50.0283409674392));
#197677=CARTESIAN_POINT('',(120.972209393875,-6.15,50.0283409674392));
#197678=CARTESIAN_POINT('',(120.972209393875,-6.15,50.0283409674392));
#197679=CARTESIAN_POINT('Origin',(121.463022896425,-6.15,50.1237459238885));
#197680=CARTESIAN_POINT('',(121.463022896425,-6.65,50.1237459238885));
#197681=CARTESIAN_POINT('',(121.405779922555,-6.65,50.4182340254182));
#197682=CARTESIAN_POINT('',(121.463022896425,-6.65,50.1237459238885));
#197683=CARTESIAN_POINT('',(121.405779922555,-6.15,50.4182340254182));
#197684=CARTESIAN_POINT('',(121.463022896425,-6.15,50.1237459238885));
#197685=CARTESIAN_POINT('Origin',(121.463022896425,-6.65,50.1237459238885));
#197686=CARTESIAN_POINT('',(120.972209393875,-6.65,50.0283409674392));
#197687=CARTESIAN_POINT('',(120.914966420006,-6.65,50.3228290689689));
#197688=CARTESIAN_POINT('',(120.972209393875,-6.65,50.0283409674392));
#197689=CARTESIAN_POINT('',(121.405779922555,-6.65,50.4182340254182));
#197690=CARTESIAN_POINT('',(121.463022896425,-6.65,50.1237459238885));
#197691=CARTESIAN_POINT('Origin',(120.972209393875,-6.65,50.0283409674392));
#197692=CARTESIAN_POINT('',(120.914966420006,-6.65,50.3228290689689));
#197693=CARTESIAN_POINT('',(120.972209393875,-6.65,50.0283409674392));
#197694=CARTESIAN_POINT('Origin',(121.757510997955,-6.15,50.180988897758));
#197695=CARTESIAN_POINT('',(122.248324500504,-6.15,50.2763938542073));
#197696=CARTESIAN_POINT('',(122.191081526635,-6.15,50.570881955737));
#197697=CARTESIAN_POINT('',(122.248324500504,-6.15,50.2763938542073));
#197698=CARTESIAN_POINT('',(121.700268024085,-6.15,50.4754769992877));
#197699=CARTESIAN_POINT('',(121.700268024085,-6.15,50.4754769992877));
#197700=CARTESIAN_POINT('',(121.757510997955,-6.15,50.180988897758));
#197701=CARTESIAN_POINT('',(121.757510997955,-6.15,50.180988897758));
#197702=CARTESIAN_POINT('',(121.757510997955,-6.15,50.180988897758));
#197703=CARTESIAN_POINT('Origin',(122.248324500504,-6.15,50.2763938542073));
#197704=CARTESIAN_POINT('',(122.248324500504,-6.65,50.2763938542073));
#197705=CARTESIAN_POINT('',(122.191081526635,-6.65,50.570881955737));
#197706=CARTESIAN_POINT('',(122.248324500504,-6.65,50.2763938542073));
#197707=CARTESIAN_POINT('',(122.191081526635,-6.15,50.570881955737));
#197708=CARTESIAN_POINT('',(122.248324500504,-6.15,50.2763938542073));
#197709=CARTESIAN_POINT('Origin',(122.248324500504,-6.65,50.2763938542073));
#197710=CARTESIAN_POINT('',(121.757510997955,-6.65,50.180988897758));
#197711=CARTESIAN_POINT('',(121.700268024085,-6.65,50.4754769992877));
#197712=CARTESIAN_POINT('',(121.757510997955,-6.65,50.180988897758));
#197713=CARTESIAN_POINT('',(122.191081526635,-6.65,50.570881955737));
#197714=CARTESIAN_POINT('',(122.248324500504,-6.65,50.2763938542073));
#197715=CARTESIAN_POINT('Origin',(121.757510997955,-6.65,50.180988897758));
#197716=CARTESIAN_POINT('',(121.700268024085,-6.65,50.4754769992877));
#197717=CARTESIAN_POINT('',(121.757510997955,-6.65,50.180988897758));
#197718=CARTESIAN_POINT('Origin',(122.542812602034,-6.15,50.3336368280768));
#197719=CARTESIAN_POINT('',(123.033626104583,-6.15,50.4290417845261));
#197720=CARTESIAN_POINT('',(122.976383130714,-6.15,50.7235298860558));
#197721=CARTESIAN_POINT('',(123.033626104583,-6.15,50.4290417845261));
#197722=CARTESIAN_POINT('',(122.485569628164,-6.15,50.6281249296065));
#197723=CARTESIAN_POINT('',(122.485569628164,-6.15,50.6281249296065));
#197724=CARTESIAN_POINT('',(122.542812602034,-6.15,50.3336368280768));
#197725=CARTESIAN_POINT('',(122.542812602034,-6.15,50.3336368280768));
#197726=CARTESIAN_POINT('',(122.542812602034,-6.15,50.3336368280768));
#197727=CARTESIAN_POINT('Origin',(123.033626104583,-6.15,50.4290417845261));
#197728=CARTESIAN_POINT('',(123.033626104583,-6.65,50.4290417845261));
#197729=CARTESIAN_POINT('',(122.976383130714,-6.65,50.7235298860558));
#197730=CARTESIAN_POINT('',(123.033626104583,-6.65,50.4290417845261));
#197731=CARTESIAN_POINT('',(122.976383130714,-6.15,50.7235298860558));
#197732=CARTESIAN_POINT('',(123.033626104583,-6.15,50.4290417845261));
#197733=CARTESIAN_POINT('Origin',(123.033626104583,-6.65,50.4290417845261));
#197734=CARTESIAN_POINT('',(122.542812602034,-6.65,50.3336368280768));
#197735=CARTESIAN_POINT('',(122.485569628164,-6.65,50.6281249296065));
#197736=CARTESIAN_POINT('',(122.542812602034,-6.65,50.3336368280768));
#197737=CARTESIAN_POINT('',(122.976383130714,-6.65,50.7235298860558));
#197738=CARTESIAN_POINT('',(123.033626104583,-6.65,50.4290417845261));
#197739=CARTESIAN_POINT('Origin',(122.542812602034,-6.65,50.3336368280768));
#197740=CARTESIAN_POINT('',(122.485569628164,-6.65,50.6281249296065));
#197741=CARTESIAN_POINT('',(122.542812602034,-6.65,50.3336368280768));
#197742=CARTESIAN_POINT('Origin',(123.328114206113,-6.15,50.4862847583956));
#197743=CARTESIAN_POINT('',(123.818927708663,-6.15,50.5816897148449));
#197744=CARTESIAN_POINT('',(123.761684734793,-6.15,50.8761778163746));
#197745=CARTESIAN_POINT('',(123.818927708663,-6.15,50.5816897148449));
#197746=CARTESIAN_POINT('',(123.270871232244,-6.15,50.7807728599253));
#197747=CARTESIAN_POINT('',(123.270871232244,-6.15,50.7807728599253));
#197748=CARTESIAN_POINT('',(123.328114206113,-6.15,50.4862847583956));
#197749=CARTESIAN_POINT('',(123.328114206113,-6.15,50.4862847583956));
#197750=CARTESIAN_POINT('',(123.328114206113,-6.15,50.4862847583956));
#197751=CARTESIAN_POINT('Origin',(123.818927708663,-6.15,50.5816897148449));
#197752=CARTESIAN_POINT('',(123.818927708663,-6.65,50.5816897148449));
#197753=CARTESIAN_POINT('',(123.761684734793,-6.65,50.8761778163746));
#197754=CARTESIAN_POINT('',(123.818927708663,-6.65,50.5816897148449));
#197755=CARTESIAN_POINT('',(123.761684734793,-6.15,50.8761778163746));
#197756=CARTESIAN_POINT('',(123.818927708663,-6.15,50.5816897148449));
#197757=CARTESIAN_POINT('Origin',(123.818927708663,-6.65,50.5816897148449));
#197758=CARTESIAN_POINT('',(123.328114206113,-6.65,50.4862847583956));
#197759=CARTESIAN_POINT('',(123.270871232244,-6.65,50.7807728599253));
#197760=CARTESIAN_POINT('',(123.328114206113,-6.65,50.4862847583956));
#197761=CARTESIAN_POINT('',(123.761684734793,-6.65,50.8761778163746));
#197762=CARTESIAN_POINT('',(123.818927708663,-6.65,50.5816897148449));
#197763=CARTESIAN_POINT('Origin',(123.328114206113,-6.65,50.4862847583956));
#197764=CARTESIAN_POINT('',(123.270871232244,-6.65,50.7807728599253));
#197765=CARTESIAN_POINT('',(123.328114206113,-6.65,50.4862847583956));
#197766=CARTESIAN_POINT('Origin',(123.328114206113,-5.35,50.4862847583956));
#197767=CARTESIAN_POINT('',(123.818927708663,-5.35,50.5816897148449));
#197768=CARTESIAN_POINT('',(123.761684734793,-5.35,50.8761778163746));
#197769=CARTESIAN_POINT('',(123.818927708663,-5.35,50.5816897148449));
#197770=CARTESIAN_POINT('',(123.270871232244,-5.35,50.7807728599253));
#197771=CARTESIAN_POINT('',(123.270871232244,-5.35,50.7807728599253));
#197772=CARTESIAN_POINT('',(123.328114206113,-5.35,50.4862847583956));
#197773=CARTESIAN_POINT('',(123.328114206113,-5.35,50.4862847583956));
#197774=CARTESIAN_POINT('',(123.328114206113,-5.35,50.4862847583956));
#197775=CARTESIAN_POINT('Origin',(123.818927708663,-5.35,50.5816897148449));
#197776=CARTESIAN_POINT('',(123.818927708663,-5.85,50.5816897148449));
#197777=CARTESIAN_POINT('',(123.761684734793,-5.85,50.8761778163746));
#197778=CARTESIAN_POINT('',(123.818927708663,-5.85,50.5816897148449));
#197779=CARTESIAN_POINT('',(123.761684734793,-5.35,50.8761778163746));
#197780=CARTESIAN_POINT('',(123.818927708663,-5.35,50.5816897148449));
#197781=CARTESIAN_POINT('Origin',(123.818927708663,-5.85,50.5816897148449));
#197782=CARTESIAN_POINT('',(123.328114206113,-5.85,50.4862847583956));
#197783=CARTESIAN_POINT('',(123.270871232244,-5.85,50.7807728599253));
#197784=CARTESIAN_POINT('',(123.328114206113,-5.85,50.4862847583956));
#197785=CARTESIAN_POINT('',(123.761684734793,-5.85,50.8761778163746));
#197786=CARTESIAN_POINT('',(123.818927708663,-5.85,50.5816897148449));
#197787=CARTESIAN_POINT('Origin',(123.328114206113,-5.85,50.4862847583956));
#197788=CARTESIAN_POINT('',(123.270871232244,-5.85,50.7807728599253));
#197789=CARTESIAN_POINT('',(123.328114206113,-5.85,50.4862847583956));
#197790=CARTESIAN_POINT('Origin',(123.328114206113,-4.55,50.4862847583956));
#197791=CARTESIAN_POINT('',(123.818927708663,-4.55,50.5816897148449));
#197792=CARTESIAN_POINT('',(123.761684734793,-4.55,50.8761778163746));
#197793=CARTESIAN_POINT('',(123.818927708663,-4.55,50.5816897148449));
#197794=CARTESIAN_POINT('',(123.270871232244,-4.55,50.7807728599253));
#197795=CARTESIAN_POINT('',(123.270871232244,-4.55,50.7807728599253));
#197796=CARTESIAN_POINT('',(123.328114206113,-4.55,50.4862847583956));
#197797=CARTESIAN_POINT('',(123.328114206113,-4.55,50.4862847583956));
#197798=CARTESIAN_POINT('',(123.328114206113,-4.55,50.4862847583956));
#197799=CARTESIAN_POINT('Origin',(123.818927708663,-4.55,50.5816897148449));
#197800=CARTESIAN_POINT('',(123.818927708663,-5.05,50.5816897148449));
#197801=CARTESIAN_POINT('',(123.761684734793,-5.05,50.8761778163746));
#197802=CARTESIAN_POINT('',(123.818927708663,-5.05,50.5816897148449));
#197803=CARTESIAN_POINT('',(123.761684734793,-4.55,50.8761778163746));
#197804=CARTESIAN_POINT('',(123.818927708663,-4.55,50.5816897148449));
#197805=CARTESIAN_POINT('Origin',(123.818927708663,-5.05,50.5816897148449));
#197806=CARTESIAN_POINT('',(123.328114206113,-5.05,50.4862847583956));
#197807=CARTESIAN_POINT('',(123.270871232244,-5.05,50.7807728599253));
#197808=CARTESIAN_POINT('',(123.328114206113,-5.05,50.4862847583956));
#197809=CARTESIAN_POINT('',(123.761684734793,-5.05,50.8761778163746));
#197810=CARTESIAN_POINT('',(123.818927708663,-5.05,50.5816897148449));
#197811=CARTESIAN_POINT('Origin',(123.328114206113,-5.05,50.4862847583956));
#197812=CARTESIAN_POINT('',(123.270871232244,-5.05,50.7807728599253));
#197813=CARTESIAN_POINT('',(123.328114206113,-5.05,50.4862847583956));
#197814=CARTESIAN_POINT('Origin',(123.328114206113,-3.75,50.4862847583956));
#197815=CARTESIAN_POINT('',(123.818927708663,-3.75,50.5816897148449));
#197816=CARTESIAN_POINT('',(123.761684734793,-3.75,50.8761778163746));
#197817=CARTESIAN_POINT('',(123.818927708663,-3.75,50.5816897148449));
#197818=CARTESIAN_POINT('',(123.270871232244,-3.75,50.7807728599253));
#197819=CARTESIAN_POINT('',(123.270871232244,-3.75,50.7807728599253));
#197820=CARTESIAN_POINT('',(123.328114206113,-3.75,50.4862847583956));
#197821=CARTESIAN_POINT('',(123.328114206113,-3.75,50.4862847583956));
#197822=CARTESIAN_POINT('',(123.328114206113,-3.75,50.4862847583956));
#197823=CARTESIAN_POINT('Origin',(123.818927708663,-3.75,50.5816897148449));
#197824=CARTESIAN_POINT('',(123.818927708663,-4.25,50.5816897148449));
#197825=CARTESIAN_POINT('',(123.761684734793,-4.25,50.8761778163746));
#197826=CARTESIAN_POINT('',(123.818927708663,-4.25,50.5816897148449));
#197827=CARTESIAN_POINT('',(123.761684734793,-3.75,50.8761778163746));
#197828=CARTESIAN_POINT('',(123.818927708663,-3.75,50.5816897148449));
#197829=CARTESIAN_POINT('Origin',(123.818927708663,-4.25,50.5816897148449));
#197830=CARTESIAN_POINT('',(123.328114206113,-4.25,50.4862847583956));
#197831=CARTESIAN_POINT('',(123.270871232244,-4.25,50.7807728599253));
#197832=CARTESIAN_POINT('',(123.328114206113,-4.25,50.4862847583956));
#197833=CARTESIAN_POINT('',(123.761684734793,-4.25,50.8761778163746));
#197834=CARTESIAN_POINT('',(123.818927708663,-4.25,50.5816897148449));
#197835=CARTESIAN_POINT('Origin',(123.328114206113,-4.25,50.4862847583956));
#197836=CARTESIAN_POINT('',(123.270871232244,-4.25,50.7807728599253));
#197837=CARTESIAN_POINT('',(123.328114206113,-4.25,50.4862847583956));
#197838=CARTESIAN_POINT('Origin',(123.328114206113,-2.95,50.4862847583956));
#197839=CARTESIAN_POINT('',(123.818927708663,-2.95,50.5816897148449));
#197840=CARTESIAN_POINT('',(123.761684734793,-2.95,50.8761778163746));
#197841=CARTESIAN_POINT('',(123.818927708663,-2.95,50.5816897148449));
#197842=CARTESIAN_POINT('',(123.270871232244,-2.95,50.7807728599253));
#197843=CARTESIAN_POINT('',(123.270871232244,-2.95,50.7807728599253));
#197844=CARTESIAN_POINT('',(123.328114206113,-2.95,50.4862847583956));
#197845=CARTESIAN_POINT('',(123.328114206113,-2.95,50.4862847583956));
#197846=CARTESIAN_POINT('',(123.328114206113,-2.95,50.4862847583956));
#197847=CARTESIAN_POINT('Origin',(123.818927708663,-2.95,50.5816897148449));
#197848=CARTESIAN_POINT('',(123.818927708663,-3.45,50.5816897148449));
#197849=CARTESIAN_POINT('',(123.761684734793,-3.45,50.8761778163746));
#197850=CARTESIAN_POINT('',(123.818927708663,-3.45,50.5816897148449));
#197851=CARTESIAN_POINT('',(123.761684734793,-2.95,50.8761778163746));
#197852=CARTESIAN_POINT('',(123.818927708663,-2.95,50.5816897148449));
#197853=CARTESIAN_POINT('Origin',(123.818927708663,-3.45,50.5816897148449));
#197854=CARTESIAN_POINT('',(123.328114206113,-3.45,50.4862847583956));
#197855=CARTESIAN_POINT('',(123.270871232244,-3.45,50.7807728599253));
#197856=CARTESIAN_POINT('',(123.328114206113,-3.45,50.4862847583956));
#197857=CARTESIAN_POINT('',(123.761684734793,-3.45,50.8761778163746));
#197858=CARTESIAN_POINT('',(123.818927708663,-3.45,50.5816897148449));
#197859=CARTESIAN_POINT('Origin',(123.328114206113,-3.45,50.4862847583956));
#197860=CARTESIAN_POINT('',(123.270871232244,-3.45,50.7807728599253));
#197861=CARTESIAN_POINT('',(123.328114206113,-3.45,50.4862847583956));
#197862=CARTESIAN_POINT('Origin',(123.328114206113,-2.15,50.4862847583956));
#197863=CARTESIAN_POINT('',(123.818927708663,-2.15,50.5816897148449));
#197864=CARTESIAN_POINT('',(123.761684734793,-2.15,50.8761778163746));
#197865=CARTESIAN_POINT('',(123.818927708663,-2.15,50.5816897148449));
#197866=CARTESIAN_POINT('',(123.270871232244,-2.15,50.7807728599253));
#197867=CARTESIAN_POINT('',(123.270871232244,-2.15,50.7807728599253));
#197868=CARTESIAN_POINT('',(123.328114206113,-2.15,50.4862847583956));
#197869=CARTESIAN_POINT('',(123.328114206113,-2.15,50.4862847583956));
#197870=CARTESIAN_POINT('',(123.328114206113,-2.15,50.4862847583956));
#197871=CARTESIAN_POINT('Origin',(123.818927708663,-2.15,50.5816897148449));
#197872=CARTESIAN_POINT('',(123.818927708663,-2.65,50.5816897148449));
#197873=CARTESIAN_POINT('',(123.761684734793,-2.65,50.8761778163746));
#197874=CARTESIAN_POINT('',(123.818927708663,-2.65,50.5816897148449));
#197875=CARTESIAN_POINT('',(123.761684734793,-2.15,50.8761778163746));
#197876=CARTESIAN_POINT('',(123.818927708663,-2.15,50.5816897148449));
#197877=CARTESIAN_POINT('Origin',(123.818927708663,-2.65,50.5816897148449));
#197878=CARTESIAN_POINT('',(123.328114206113,-2.65,50.4862847583956));
#197879=CARTESIAN_POINT('',(123.270871232244,-2.65,50.7807728599253));
#197880=CARTESIAN_POINT('',(123.328114206113,-2.65,50.4862847583956));
#197881=CARTESIAN_POINT('',(123.761684734793,-2.65,50.8761778163746));
#197882=CARTESIAN_POINT('',(123.818927708663,-2.65,50.5816897148449));
#197883=CARTESIAN_POINT('Origin',(123.328114206113,-2.65,50.4862847583956));
#197884=CARTESIAN_POINT('',(123.270871232244,-2.65,50.7807728599253));
#197885=CARTESIAN_POINT('',(123.328114206113,-2.65,50.4862847583956));
#197886=CARTESIAN_POINT('Origin',(123.328114206113,-1.35,50.4862847583956));
#197887=CARTESIAN_POINT('',(123.818927708663,-1.35,50.5816897148449));
#197888=CARTESIAN_POINT('',(123.761684734793,-1.35,50.8761778163746));
#197889=CARTESIAN_POINT('',(123.818927708663,-1.35,50.5816897148449));
#197890=CARTESIAN_POINT('',(123.270871232244,-1.35,50.7807728599253));
#197891=CARTESIAN_POINT('',(123.270871232244,-1.35,50.7807728599253));
#197892=CARTESIAN_POINT('',(123.328114206113,-1.35,50.4862847583956));
#197893=CARTESIAN_POINT('',(123.328114206113,-1.35,50.4862847583956));
#197894=CARTESIAN_POINT('',(123.328114206113,-1.35,50.4862847583956));
#197895=CARTESIAN_POINT('Origin',(123.818927708663,-1.35,50.5816897148449));
#197896=CARTESIAN_POINT('',(123.818927708663,-1.85,50.5816897148449));
#197897=CARTESIAN_POINT('',(123.761684734793,-1.85,50.8761778163746));
#197898=CARTESIAN_POINT('',(123.818927708663,-1.85,50.5816897148449));
#197899=CARTESIAN_POINT('',(123.761684734793,-1.35,50.8761778163746));
#197900=CARTESIAN_POINT('',(123.818927708663,-1.35,50.5816897148449));
#197901=CARTESIAN_POINT('Origin',(123.818927708663,-1.85,50.5816897148449));
#197902=CARTESIAN_POINT('',(123.328114206113,-1.85,50.4862847583956));
#197903=CARTESIAN_POINT('',(123.270871232244,-1.85,50.7807728599253));
#197904=CARTESIAN_POINT('',(123.328114206113,-1.85,50.4862847583956));
#197905=CARTESIAN_POINT('',(123.761684734793,-1.85,50.8761778163746));
#197906=CARTESIAN_POINT('',(123.818927708663,-1.85,50.5816897148449));
#197907=CARTESIAN_POINT('Origin',(123.328114206113,-1.85,50.4862847583956));
#197908=CARTESIAN_POINT('',(123.270871232244,-1.85,50.7807728599253));
#197909=CARTESIAN_POINT('',(123.328114206113,-1.85,50.4862847583956));
#197910=CARTESIAN_POINT('Origin',(123.328114206113,-0.549999999999986,50.4862847583956));
#197911=CARTESIAN_POINT('',(123.818927708663,-0.549999999999986,50.5816897148449));
#197912=CARTESIAN_POINT('',(123.761684734793,-0.549999999999986,50.8761778163746));
#197913=CARTESIAN_POINT('',(123.818927708663,-0.549999999999986,50.5816897148449));
#197914=CARTESIAN_POINT('',(123.270871232244,-0.549999999999986,50.7807728599253));
#197915=CARTESIAN_POINT('',(123.270871232244,-0.549999999999986,50.7807728599253));
#197916=CARTESIAN_POINT('',(123.328114206113,-0.549999999999986,50.4862847583956));
#197917=CARTESIAN_POINT('',(123.328114206113,-0.549999999999986,50.4862847583956));
#197918=CARTESIAN_POINT('',(123.328114206113,-0.549999999999986,50.4862847583956));
#197919=CARTESIAN_POINT('Origin',(123.818927708663,-0.549999999999986,50.5816897148449));
#197920=CARTESIAN_POINT('',(123.818927708663,-1.05,50.5816897148449));
#197921=CARTESIAN_POINT('',(123.761684734793,-1.05,50.8761778163746));
#197922=CARTESIAN_POINT('',(123.818927708663,-1.05,50.5816897148449));
#197923=CARTESIAN_POINT('',(123.761684734793,-0.549999999999986,50.8761778163746));
#197924=CARTESIAN_POINT('',(123.818927708663,-0.549999999999986,50.5816897148449));
#197925=CARTESIAN_POINT('Origin',(123.818927708663,-1.05,50.5816897148449));
#197926=CARTESIAN_POINT('',(123.328114206113,-1.05,50.4862847583956));
#197927=CARTESIAN_POINT('',(123.270871232244,-1.05,50.7807728599253));
#197928=CARTESIAN_POINT('',(123.328114206113,-1.05,50.4862847583956));
#197929=CARTESIAN_POINT('',(123.761684734793,-1.05,50.8761778163746));
#197930=CARTESIAN_POINT('',(123.818927708663,-1.05,50.5816897148449));
#197931=CARTESIAN_POINT('Origin',(123.328114206113,-1.05,50.4862847583956));
#197932=CARTESIAN_POINT('',(123.270871232244,-1.05,50.7807728599253));
#197933=CARTESIAN_POINT('',(123.328114206113,-1.05,50.4862847583956));
#197934=CARTESIAN_POINT('Origin',(123.328114206113,0.250000000000015,50.4862847583956));
#197935=CARTESIAN_POINT('',(123.818927708663,0.250000000000015,50.5816897148449));
#197936=CARTESIAN_POINT('',(123.761684734793,0.250000000000015,50.8761778163746));
#197937=CARTESIAN_POINT('',(123.818927708663,0.250000000000015,50.5816897148449));
#197938=CARTESIAN_POINT('',(123.270871232244,0.250000000000015,50.7807728599253));
#197939=CARTESIAN_POINT('',(123.270871232244,0.250000000000015,50.7807728599253));
#197940=CARTESIAN_POINT('',(123.328114206113,0.250000000000015,50.4862847583956));
#197941=CARTESIAN_POINT('',(123.328114206113,0.250000000000015,50.4862847583956));
#197942=CARTESIAN_POINT('',(123.328114206113,0.250000000000015,50.4862847583956));
#197943=CARTESIAN_POINT('Origin',(123.818927708663,0.250000000000015,50.5816897148449));
#197944=CARTESIAN_POINT('',(123.818927708663,-0.249999999999985,50.5816897148449));
#197945=CARTESIAN_POINT('',(123.761684734793,-0.249999999999985,50.8761778163746));
#197946=CARTESIAN_POINT('',(123.818927708663,-0.249999999999985,50.5816897148449));
#197947=CARTESIAN_POINT('',(123.761684734793,0.250000000000015,50.8761778163746));
#197948=CARTESIAN_POINT('',(123.818927708663,0.250000000000015,50.5816897148449));
#197949=CARTESIAN_POINT('Origin',(123.818927708663,-0.249999999999985,50.5816897148449));
#197950=CARTESIAN_POINT('',(123.328114206113,-0.249999999999985,50.4862847583956));
#197951=CARTESIAN_POINT('',(123.270871232244,-0.249999999999985,50.7807728599253));
#197952=CARTESIAN_POINT('',(123.328114206113,-0.249999999999985,50.4862847583956));
#197953=CARTESIAN_POINT('',(123.761684734793,-0.249999999999985,50.8761778163746));
#197954=CARTESIAN_POINT('',(123.818927708663,-0.249999999999985,50.5816897148449));
#197955=CARTESIAN_POINT('Origin',(123.328114206113,-0.249999999999985,50.4862847583956));
#197956=CARTESIAN_POINT('',(123.270871232244,-0.249999999999985,50.7807728599253));
#197957=CARTESIAN_POINT('',(123.328114206113,-0.249999999999985,50.4862847583956));
#197958=CARTESIAN_POINT('Origin',(123.328114206113,1.05,50.4862847583956));
#197959=CARTESIAN_POINT('',(123.818927708663,1.05,50.5816897148449));
#197960=CARTESIAN_POINT('',(123.761684734793,1.05,50.8761778163746));
#197961=CARTESIAN_POINT('',(123.818927708663,1.05,50.5816897148449));
#197962=CARTESIAN_POINT('',(123.270871232244,1.05,50.7807728599253));
#197963=CARTESIAN_POINT('',(123.270871232244,1.05,50.7807728599253));
#197964=CARTESIAN_POINT('',(123.328114206113,1.05,50.4862847583956));
#197965=CARTESIAN_POINT('',(123.328114206113,1.05,50.4862847583956));
#197966=CARTESIAN_POINT('',(123.328114206113,1.05,50.4862847583956));
#197967=CARTESIAN_POINT('Origin',(123.818927708663,1.05,50.5816897148449));
#197968=CARTESIAN_POINT('',(123.818927708663,0.550000000000015,50.5816897148449));
#197969=CARTESIAN_POINT('',(123.761684734793,0.550000000000015,50.8761778163746));
#197970=CARTESIAN_POINT('',(123.818927708663,0.550000000000015,50.5816897148449));
#197971=CARTESIAN_POINT('',(123.761684734793,1.05,50.8761778163746));
#197972=CARTESIAN_POINT('',(123.818927708663,1.05,50.5816897148449));
#197973=CARTESIAN_POINT('Origin',(123.818927708663,0.550000000000015,50.5816897148449));
#197974=CARTESIAN_POINT('',(123.328114206113,0.550000000000015,50.4862847583956));
#197975=CARTESIAN_POINT('',(123.270871232244,0.550000000000015,50.7807728599253));
#197976=CARTESIAN_POINT('',(123.328114206113,0.550000000000015,50.4862847583956));
#197977=CARTESIAN_POINT('',(123.761684734793,0.550000000000015,50.8761778163746));
#197978=CARTESIAN_POINT('',(123.818927708663,0.550000000000015,50.5816897148449));
#197979=CARTESIAN_POINT('Origin',(123.328114206113,0.550000000000015,50.4862847583956));
#197980=CARTESIAN_POINT('',(123.270871232244,0.550000000000015,50.7807728599253));
#197981=CARTESIAN_POINT('',(123.328114206113,0.550000000000015,50.4862847583956));
#197982=CARTESIAN_POINT('Origin',(123.328114206113,1.85,50.4862847583956));
#197983=CARTESIAN_POINT('',(123.818927708663,1.85,50.5816897148449));
#197984=CARTESIAN_POINT('',(123.761684734793,1.85,50.8761778163746));
#197985=CARTESIAN_POINT('',(123.818927708663,1.85,50.5816897148449));
#197986=CARTESIAN_POINT('',(123.270871232244,1.85,50.7807728599253));
#197987=CARTESIAN_POINT('',(123.270871232244,1.85,50.7807728599253));
#197988=CARTESIAN_POINT('',(123.328114206113,1.85,50.4862847583956));
#197989=CARTESIAN_POINT('',(123.328114206113,1.85,50.4862847583956));
#197990=CARTESIAN_POINT('',(123.328114206113,1.85,50.4862847583956));
#197991=CARTESIAN_POINT('Origin',(123.818927708663,1.85,50.5816897148449));
#197992=CARTESIAN_POINT('',(123.818927708663,1.35,50.5816897148449));
#197993=CARTESIAN_POINT('',(123.761684734793,1.35,50.8761778163746));
#197994=CARTESIAN_POINT('',(123.818927708663,1.35,50.5816897148449));
#197995=CARTESIAN_POINT('',(123.761684734793,1.85,50.8761778163746));
#197996=CARTESIAN_POINT('',(123.818927708663,1.85,50.5816897148449));
#197997=CARTESIAN_POINT('Origin',(123.818927708663,1.35,50.5816897148449));
#197998=CARTESIAN_POINT('',(123.328114206113,1.35,50.4862847583956));
#197999=CARTESIAN_POINT('',(123.270871232244,1.35,50.7807728599253));
#198000=CARTESIAN_POINT('',(123.328114206113,1.35,50.4862847583956));
#198001=CARTESIAN_POINT('',(123.761684734793,1.35,50.8761778163746));
#198002=CARTESIAN_POINT('',(123.818927708663,1.35,50.5816897148449));
#198003=CARTESIAN_POINT('Origin',(123.328114206113,1.35,50.4862847583956));
#198004=CARTESIAN_POINT('',(123.270871232244,1.35,50.7807728599253));
#198005=CARTESIAN_POINT('',(123.328114206113,1.35,50.4862847583956));
#198006=CARTESIAN_POINT('Origin',(123.328114206113,2.65,50.4862847583956));
#198007=CARTESIAN_POINT('',(123.818927708663,2.65,50.5816897148449));
#198008=CARTESIAN_POINT('',(123.761684734793,2.65,50.8761778163746));
#198009=CARTESIAN_POINT('',(123.818927708663,2.65,50.5816897148449));
#198010=CARTESIAN_POINT('',(123.270871232244,2.65,50.7807728599253));
#198011=CARTESIAN_POINT('',(123.270871232244,2.65,50.7807728599253));
#198012=CARTESIAN_POINT('',(123.328114206113,2.65,50.4862847583956));
#198013=CARTESIAN_POINT('',(123.328114206113,2.65,50.4862847583956));
#198014=CARTESIAN_POINT('',(123.328114206113,2.65,50.4862847583956));
#198015=CARTESIAN_POINT('Origin',(123.818927708663,2.65,50.5816897148449));
#198016=CARTESIAN_POINT('',(123.818927708663,2.15,50.5816897148449));
#198017=CARTESIAN_POINT('',(123.761684734793,2.15,50.8761778163746));
#198018=CARTESIAN_POINT('',(123.818927708663,2.15,50.5816897148449));
#198019=CARTESIAN_POINT('',(123.761684734793,2.65,50.8761778163746));
#198020=CARTESIAN_POINT('',(123.818927708663,2.65,50.5816897148449));
#198021=CARTESIAN_POINT('Origin',(123.818927708663,2.15,50.5816897148449));
#198022=CARTESIAN_POINT('',(123.328114206113,2.15,50.4862847583956));
#198023=CARTESIAN_POINT('',(123.270871232244,2.15,50.7807728599253));
#198024=CARTESIAN_POINT('',(123.328114206113,2.15,50.4862847583956));
#198025=CARTESIAN_POINT('',(123.761684734793,2.15,50.8761778163746));
#198026=CARTESIAN_POINT('',(123.818927708663,2.15,50.5816897148449));
#198027=CARTESIAN_POINT('Origin',(123.328114206113,2.15,50.4862847583956));
#198028=CARTESIAN_POINT('',(123.270871232244,2.15,50.7807728599253));
#198029=CARTESIAN_POINT('',(123.328114206113,2.15,50.4862847583956));
#198030=CARTESIAN_POINT('Origin',(123.328114206113,3.45,50.4862847583956));
#198031=CARTESIAN_POINT('',(123.818927708663,3.45,50.5816897148449));
#198032=CARTESIAN_POINT('',(123.761684734793,3.45,50.8761778163746));
#198033=CARTESIAN_POINT('',(123.818927708663,3.45,50.5816897148449));
#198034=CARTESIAN_POINT('',(123.270871232244,3.45,50.7807728599253));
#198035=CARTESIAN_POINT('',(123.270871232244,3.45,50.7807728599253));
#198036=CARTESIAN_POINT('',(123.328114206113,3.45,50.4862847583956));
#198037=CARTESIAN_POINT('',(123.328114206113,3.45,50.4862847583956));
#198038=CARTESIAN_POINT('',(123.328114206113,3.45,50.4862847583956));
#198039=CARTESIAN_POINT('Origin',(123.818927708663,3.45,50.5816897148449));
#198040=CARTESIAN_POINT('',(123.818927708663,2.95,50.5816897148449));
#198041=CARTESIAN_POINT('',(123.761684734793,2.95,50.8761778163746));
#198042=CARTESIAN_POINT('',(123.818927708663,2.95,50.5816897148449));
#198043=CARTESIAN_POINT('',(123.761684734793,3.45,50.8761778163746));
#198044=CARTESIAN_POINT('',(123.818927708663,3.45,50.5816897148449));
#198045=CARTESIAN_POINT('Origin',(123.818927708663,2.95,50.5816897148449));
#198046=CARTESIAN_POINT('',(123.328114206113,2.95,50.4862847583956));
#198047=CARTESIAN_POINT('',(123.270871232244,2.95,50.7807728599253));
#198048=CARTESIAN_POINT('',(123.328114206113,2.95,50.4862847583956));
#198049=CARTESIAN_POINT('',(123.761684734793,2.95,50.8761778163746));
#198050=CARTESIAN_POINT('',(123.818927708663,2.95,50.5816897148449));
#198051=CARTESIAN_POINT('Origin',(123.328114206113,2.95,50.4862847583956));
#198052=CARTESIAN_POINT('',(123.270871232244,2.95,50.7807728599253));
#198053=CARTESIAN_POINT('',(123.328114206113,2.95,50.4862847583956));
#198054=CARTESIAN_POINT('Origin',(123.328114206113,4.25,50.4862847583956));
#198055=CARTESIAN_POINT('',(123.818927708663,4.25,50.5816897148449));
#198056=CARTESIAN_POINT('',(123.761684734793,4.25,50.8761778163746));
#198057=CARTESIAN_POINT('',(123.818927708663,4.25,50.5816897148449));
#198058=CARTESIAN_POINT('',(123.270871232244,4.25,50.7807728599253));
#198059=CARTESIAN_POINT('',(123.270871232244,4.25,50.7807728599253));
#198060=CARTESIAN_POINT('',(123.328114206113,4.25,50.4862847583956));
#198061=CARTESIAN_POINT('',(123.328114206113,4.25,50.4862847583956));
#198062=CARTESIAN_POINT('',(123.328114206113,4.25,50.4862847583956));
#198063=CARTESIAN_POINT('Origin',(123.818927708663,4.25,50.5816897148449));
#198064=CARTESIAN_POINT('',(123.818927708663,3.75,50.5816897148449));
#198065=CARTESIAN_POINT('',(123.761684734793,3.75,50.8761778163746));
#198066=CARTESIAN_POINT('',(123.818927708663,3.75,50.5816897148449));
#198067=CARTESIAN_POINT('',(123.761684734793,4.25,50.8761778163746));
#198068=CARTESIAN_POINT('',(123.818927708663,4.25,50.5816897148449));
#198069=CARTESIAN_POINT('Origin',(123.818927708663,3.75,50.5816897148449));
#198070=CARTESIAN_POINT('',(123.328114206113,3.75,50.4862847583956));
#198071=CARTESIAN_POINT('',(123.270871232244,3.75,50.7807728599253));
#198072=CARTESIAN_POINT('',(123.328114206113,3.75,50.4862847583956));
#198073=CARTESIAN_POINT('',(123.761684734793,3.75,50.8761778163746));
#198074=CARTESIAN_POINT('',(123.818927708663,3.75,50.5816897148449));
#198075=CARTESIAN_POINT('Origin',(123.328114206113,3.75,50.4862847583956));
#198076=CARTESIAN_POINT('',(123.270871232244,3.75,50.7807728599253));
#198077=CARTESIAN_POINT('',(123.328114206113,3.75,50.4862847583956));
#198078=CARTESIAN_POINT('Origin',(123.328114206113,5.05,50.4862847583956));
#198079=CARTESIAN_POINT('',(123.818927708663,5.05,50.5816897148449));
#198080=CARTESIAN_POINT('',(123.761684734793,5.05,50.8761778163746));
#198081=CARTESIAN_POINT('',(123.818927708663,5.05,50.5816897148449));
#198082=CARTESIAN_POINT('',(123.270871232244,5.05,50.7807728599253));
#198083=CARTESIAN_POINT('',(123.270871232244,5.05,50.7807728599253));
#198084=CARTESIAN_POINT('',(123.328114206113,5.05,50.4862847583956));
#198085=CARTESIAN_POINT('',(123.328114206113,5.05,50.4862847583956));
#198086=CARTESIAN_POINT('',(123.328114206113,5.05,50.4862847583956));
#198087=CARTESIAN_POINT('Origin',(123.818927708663,5.05,50.5816897148449));
#198088=CARTESIAN_POINT('',(123.818927708663,4.55,50.5816897148449));
#198089=CARTESIAN_POINT('',(123.761684734793,4.55,50.8761778163746));
#198090=CARTESIAN_POINT('',(123.818927708663,4.55,50.5816897148449));
#198091=CARTESIAN_POINT('',(123.761684734793,5.05,50.8761778163746));
#198092=CARTESIAN_POINT('',(123.818927708663,5.05,50.5816897148449));
#198093=CARTESIAN_POINT('Origin',(123.818927708663,4.55,50.5816897148449));
#198094=CARTESIAN_POINT('',(123.328114206113,4.55,50.4862847583956));
#198095=CARTESIAN_POINT('',(123.270871232244,4.55,50.7807728599253));
#198096=CARTESIAN_POINT('',(123.328114206113,4.55,50.4862847583956));
#198097=CARTESIAN_POINT('',(123.761684734793,4.55,50.8761778163746));
#198098=CARTESIAN_POINT('',(123.818927708663,4.55,50.5816897148449));
#198099=CARTESIAN_POINT('Origin',(123.328114206113,4.55,50.4862847583956));
#198100=CARTESIAN_POINT('',(123.270871232244,4.55,50.7807728599253));
#198101=CARTESIAN_POINT('',(123.328114206113,4.55,50.4862847583956));
#198102=CARTESIAN_POINT('Origin',(123.328114206113,5.85,50.4862847583956));
#198103=CARTESIAN_POINT('',(123.818927708663,5.85,50.5816897148449));
#198104=CARTESIAN_POINT('',(123.761684734793,5.85,50.8761778163746));
#198105=CARTESIAN_POINT('',(123.818927708663,5.85,50.5816897148449));
#198106=CARTESIAN_POINT('',(123.270871232244,5.85,50.7807728599253));
#198107=CARTESIAN_POINT('',(123.270871232244,5.85,50.7807728599253));
#198108=CARTESIAN_POINT('',(123.328114206113,5.85,50.4862847583956));
#198109=CARTESIAN_POINT('',(123.328114206113,5.85,50.4862847583956));
#198110=CARTESIAN_POINT('',(123.328114206113,5.85,50.4862847583956));
#198111=CARTESIAN_POINT('Origin',(123.818927708663,5.85,50.5816897148449));
#198112=CARTESIAN_POINT('',(123.818927708663,5.35,50.5816897148449));
#198113=CARTESIAN_POINT('',(123.761684734793,5.35,50.8761778163746));
#198114=CARTESIAN_POINT('',(123.818927708663,5.35,50.5816897148449));
#198115=CARTESIAN_POINT('',(123.761684734793,5.85,50.8761778163746));
#198116=CARTESIAN_POINT('',(123.818927708663,5.85,50.5816897148449));
#198117=CARTESIAN_POINT('Origin',(123.818927708663,5.35,50.5816897148449));
#198118=CARTESIAN_POINT('',(123.328114206113,5.35,50.4862847583956));
#198119=CARTESIAN_POINT('',(123.270871232244,5.35,50.7807728599253));
#198120=CARTESIAN_POINT('',(123.328114206113,5.35,50.4862847583956));
#198121=CARTESIAN_POINT('',(123.761684734793,5.35,50.8761778163746));
#198122=CARTESIAN_POINT('',(123.818927708663,5.35,50.5816897148449));
#198123=CARTESIAN_POINT('Origin',(123.328114206113,5.35,50.4862847583956));
#198124=CARTESIAN_POINT('',(123.270871232244,5.35,50.7807728599253));
#198125=CARTESIAN_POINT('',(123.328114206113,5.35,50.4862847583956));
#198126=CARTESIAN_POINT('Origin',(123.328114206113,6.65,50.4862847583956));
#198127=CARTESIAN_POINT('',(123.818927708663,6.65,50.5816897148449));
#198128=CARTESIAN_POINT('',(123.761684734793,6.65,50.8761778163746));
#198129=CARTESIAN_POINT('',(123.818927708663,6.65,50.5816897148449));
#198130=CARTESIAN_POINT('',(123.270871232244,6.65,50.7807728599253));
#198131=CARTESIAN_POINT('',(123.270871232244,6.65,50.7807728599253));
#198132=CARTESIAN_POINT('',(123.328114206113,6.65,50.4862847583956));
#198133=CARTESIAN_POINT('',(123.328114206113,6.65,50.4862847583956));
#198134=CARTESIAN_POINT('',(123.328114206113,6.65,50.4862847583956));
#198135=CARTESIAN_POINT('Origin',(123.818927708663,6.65,50.5816897148449));
#198136=CARTESIAN_POINT('',(123.818927708663,6.15,50.5816897148449));
#198137=CARTESIAN_POINT('',(123.761684734793,6.15,50.8761778163746));
#198138=CARTESIAN_POINT('',(123.818927708663,6.15,50.5816897148449));
#198139=CARTESIAN_POINT('',(123.761684734793,6.65,50.8761778163746));
#198140=CARTESIAN_POINT('',(123.818927708663,6.65,50.5816897148449));
#198141=CARTESIAN_POINT('Origin',(123.818927708663,6.15,50.5816897148449));
#198142=CARTESIAN_POINT('',(123.328114206113,6.15,50.4862847583956));
#198143=CARTESIAN_POINT('',(123.270871232244,6.15,50.7807728599253));
#198144=CARTESIAN_POINT('',(123.328114206113,6.15,50.4862847583956));
#198145=CARTESIAN_POINT('',(123.761684734793,6.15,50.8761778163746));
#198146=CARTESIAN_POINT('',(123.818927708663,6.15,50.5816897148449));
#198147=CARTESIAN_POINT('Origin',(123.328114206113,6.15,50.4862847583956));
#198148=CARTESIAN_POINT('',(123.270871232244,6.15,50.7807728599253));
#198149=CARTESIAN_POINT('',(123.328114206113,6.15,50.4862847583956));
#198150=CARTESIAN_POINT('Origin',(122.542812602034,6.65,50.3336368280768));
#198151=CARTESIAN_POINT('',(123.033626104583,6.65,50.4290417845261));
#198152=CARTESIAN_POINT('',(122.976383130714,6.65,50.7235298860558));
#198153=CARTESIAN_POINT('',(123.033626104583,6.65,50.4290417845261));
#198154=CARTESIAN_POINT('',(122.485569628164,6.65,50.6281249296065));
#198155=CARTESIAN_POINT('',(122.485569628164,6.65,50.6281249296065));
#198156=CARTESIAN_POINT('',(122.542812602034,6.65,50.3336368280768));
#198157=CARTESIAN_POINT('',(122.542812602034,6.65,50.3336368280768));
#198158=CARTESIAN_POINT('',(122.542812602034,6.65,50.3336368280768));
#198159=CARTESIAN_POINT('Origin',(123.033626104583,6.65,50.4290417845261));
#198160=CARTESIAN_POINT('',(123.033626104583,6.15,50.4290417845261));
#198161=CARTESIAN_POINT('',(122.976383130714,6.15,50.7235298860558));
#198162=CARTESIAN_POINT('',(123.033626104583,6.15,50.4290417845261));
#198163=CARTESIAN_POINT('',(122.976383130714,6.65,50.7235298860558));
#198164=CARTESIAN_POINT('',(123.033626104583,6.65,50.4290417845261));
#198165=CARTESIAN_POINT('Origin',(123.033626104583,6.15,50.4290417845261));
#198166=CARTESIAN_POINT('',(122.542812602034,6.15,50.3336368280768));
#198167=CARTESIAN_POINT('',(122.485569628164,6.15,50.6281249296065));
#198168=CARTESIAN_POINT('',(122.542812602034,6.15,50.3336368280768));
#198169=CARTESIAN_POINT('',(122.976383130714,6.15,50.7235298860558));
#198170=CARTESIAN_POINT('',(123.033626104583,6.15,50.4290417845261));
#198171=CARTESIAN_POINT('Origin',(122.542812602034,6.15,50.3336368280768));
#198172=CARTESIAN_POINT('',(122.485569628164,6.15,50.6281249296065));
#198173=CARTESIAN_POINT('',(122.542812602034,6.15,50.3336368280768));
#198174=CARTESIAN_POINT('Origin',(121.757510997955,6.65,50.180988897758));
#198175=CARTESIAN_POINT('',(122.248324500504,6.65,50.2763938542073));
#198176=CARTESIAN_POINT('',(122.191081526635,6.65,50.570881955737));
#198177=CARTESIAN_POINT('',(122.248324500504,6.65,50.2763938542073));
#198178=CARTESIAN_POINT('',(121.700268024085,6.65,50.4754769992877));
#198179=CARTESIAN_POINT('',(121.700268024085,6.65,50.4754769992877));
#198180=CARTESIAN_POINT('',(121.757510997955,6.65,50.180988897758));
#198181=CARTESIAN_POINT('',(121.757510997955,6.65,50.180988897758));
#198182=CARTESIAN_POINT('',(121.757510997955,6.65,50.180988897758));
#198183=CARTESIAN_POINT('Origin',(122.248324500504,6.65,50.2763938542073));
#198184=CARTESIAN_POINT('',(122.248324500504,6.15,50.2763938542073));
#198185=CARTESIAN_POINT('',(122.191081526635,6.15,50.570881955737));
#198186=CARTESIAN_POINT('',(122.248324500504,6.15,50.2763938542073));
#198187=CARTESIAN_POINT('',(122.191081526635,6.65,50.570881955737));
#198188=CARTESIAN_POINT('',(122.248324500504,6.65,50.2763938542073));
#198189=CARTESIAN_POINT('Origin',(122.248324500504,6.15,50.2763938542073));
#198190=CARTESIAN_POINT('',(121.757510997955,6.15,50.180988897758));
#198191=CARTESIAN_POINT('',(121.700268024085,6.15,50.4754769992877));
#198192=CARTESIAN_POINT('',(121.757510997955,6.15,50.180988897758));
#198193=CARTESIAN_POINT('',(122.191081526635,6.15,50.570881955737));
#198194=CARTESIAN_POINT('',(122.248324500504,6.15,50.2763938542073));
#198195=CARTESIAN_POINT('Origin',(121.757510997955,6.15,50.180988897758));
#198196=CARTESIAN_POINT('',(121.700268024085,6.15,50.4754769992877));
#198197=CARTESIAN_POINT('',(121.757510997955,6.15,50.180988897758));
#198198=CARTESIAN_POINT('Origin',(120.972209393875,6.65,50.0283409674392));
#198199=CARTESIAN_POINT('',(121.463022896425,6.65,50.1237459238885));
#198200=CARTESIAN_POINT('',(121.405779922555,6.65,50.4182340254182));
#198201=CARTESIAN_POINT('',(121.463022896425,6.65,50.1237459238885));
#198202=CARTESIAN_POINT('',(120.914966420006,6.65,50.3228290689689));
#198203=CARTESIAN_POINT('',(120.914966420006,6.65,50.3228290689689));
#198204=CARTESIAN_POINT('',(120.972209393875,6.65,50.0283409674392));
#198205=CARTESIAN_POINT('',(120.972209393875,6.65,50.0283409674392));
#198206=CARTESIAN_POINT('',(120.972209393875,6.65,50.0283409674392));
#198207=CARTESIAN_POINT('Origin',(121.463022896425,6.65,50.1237459238885));
#198208=CARTESIAN_POINT('',(121.463022896425,6.15,50.1237459238885));
#198209=CARTESIAN_POINT('',(121.405779922555,6.15,50.4182340254182));
#198210=CARTESIAN_POINT('',(121.463022896425,6.15,50.1237459238885));
#198211=CARTESIAN_POINT('',(121.405779922555,6.65,50.4182340254182));
#198212=CARTESIAN_POINT('',(121.463022896425,6.65,50.1237459238885));
#198213=CARTESIAN_POINT('Origin',(121.463022896425,6.15,50.1237459238885));
#198214=CARTESIAN_POINT('',(120.972209393875,6.15,50.0283409674392));
#198215=CARTESIAN_POINT('',(120.914966420006,6.15,50.3228290689689));
#198216=CARTESIAN_POINT('',(120.972209393875,6.15,50.0283409674392));
#198217=CARTESIAN_POINT('',(121.405779922555,6.15,50.4182340254182));
#198218=CARTESIAN_POINT('',(121.463022896425,6.15,50.1237459238885));
#198219=CARTESIAN_POINT('Origin',(120.972209393875,6.15,50.0283409674392));
#198220=CARTESIAN_POINT('',(120.914966420006,6.15,50.3228290689689));
#198221=CARTESIAN_POINT('',(120.972209393875,6.15,50.0283409674392));
#198222=CARTESIAN_POINT('Origin',(120.186907789796,6.65,49.8756930371204));
#198223=CARTESIAN_POINT('',(120.677721292346,6.65,49.9710979935697));
#198224=CARTESIAN_POINT('',(120.620478318476,6.65,50.2655860950994));
#198225=CARTESIAN_POINT('',(120.677721292346,6.65,49.9710979935697));
#198226=CARTESIAN_POINT('',(120.129664815927,6.65,50.1701811386501));
#198227=CARTESIAN_POINT('',(120.129664815927,6.65,50.1701811386501));
#198228=CARTESIAN_POINT('',(120.186907789796,6.65,49.8756930371204));
#198229=CARTESIAN_POINT('',(120.186907789796,6.65,49.8756930371204));
#198230=CARTESIAN_POINT('',(120.186907789796,6.65,49.8756930371204));
#198231=CARTESIAN_POINT('Origin',(120.677721292346,6.65,49.9710979935697));
#198232=CARTESIAN_POINT('',(120.677721292346,6.15,49.9710979935697));
#198233=CARTESIAN_POINT('',(120.620478318476,6.15,50.2655860950994));
#198234=CARTESIAN_POINT('',(120.677721292346,6.15,49.9710979935697));
#198235=CARTESIAN_POINT('',(120.620478318476,6.65,50.2655860950994));
#198236=CARTESIAN_POINT('',(120.677721292346,6.65,49.9710979935697));
#198237=CARTESIAN_POINT('Origin',(120.677721292346,6.15,49.9710979935697));
#198238=CARTESIAN_POINT('',(120.186907789796,6.15,49.8756930371204));
#198239=CARTESIAN_POINT('',(120.129664815927,6.15,50.1701811386501));
#198240=CARTESIAN_POINT('',(120.186907789796,6.15,49.8756930371204));
#198241=CARTESIAN_POINT('',(120.620478318476,6.15,50.2655860950994));
#198242=CARTESIAN_POINT('',(120.677721292346,6.15,49.9710979935697));
#198243=CARTESIAN_POINT('Origin',(120.186907789796,6.15,49.8756930371204));
#198244=CARTESIAN_POINT('',(120.129664815927,6.15,50.1701811386501));
#198245=CARTESIAN_POINT('',(120.186907789796,6.15,49.8756930371204));
#198246=CARTESIAN_POINT('Origin',(119.401606185717,6.65,49.7230451068016));
#198247=CARTESIAN_POINT('',(119.892419688267,6.65,49.8184500632509));
#198248=CARTESIAN_POINT('',(119.835176714397,6.65,50.1129381647806));
#198249=CARTESIAN_POINT('',(119.892419688267,6.65,49.8184500632509));
#198250=CARTESIAN_POINT('',(119.344363211847,6.65,50.0175332083313));
#198251=CARTESIAN_POINT('',(119.344363211847,6.65,50.0175332083313));
#198252=CARTESIAN_POINT('',(119.401606185717,6.65,49.7230451068016));
#198253=CARTESIAN_POINT('',(119.401606185717,6.65,49.7230451068016));
#198254=CARTESIAN_POINT('',(119.401606185717,6.65,49.7230451068016));
#198255=CARTESIAN_POINT('Origin',(119.892419688267,6.65,49.8184500632509));
#198256=CARTESIAN_POINT('',(119.892419688267,6.15,49.8184500632509));
#198257=CARTESIAN_POINT('',(119.835176714397,6.15,50.1129381647806));
#198258=CARTESIAN_POINT('',(119.892419688267,6.15,49.8184500632509));
#198259=CARTESIAN_POINT('',(119.835176714397,6.65,50.1129381647806));
#198260=CARTESIAN_POINT('',(119.892419688267,6.65,49.8184500632509));
#198261=CARTESIAN_POINT('Origin',(119.892419688267,6.15,49.8184500632509));
#198262=CARTESIAN_POINT('',(119.401606185717,6.15,49.7230451068016));
#198263=CARTESIAN_POINT('',(119.344363211847,6.15,50.0175332083313));
#198264=CARTESIAN_POINT('',(119.401606185717,6.15,49.7230451068016));
#198265=CARTESIAN_POINT('',(119.835176714397,6.15,50.1129381647806));
#198266=CARTESIAN_POINT('',(119.892419688267,6.15,49.8184500632509));
#198267=CARTESIAN_POINT('Origin',(119.401606185717,6.15,49.7230451068016));
#198268=CARTESIAN_POINT('',(119.344363211847,6.15,50.0175332083313));
#198269=CARTESIAN_POINT('',(119.401606185717,6.15,49.7230451068016));
#198270=CARTESIAN_POINT('Origin',(118.616304581638,6.65,49.5703971764828));
#198271=CARTESIAN_POINT('',(119.107118084187,6.65,49.6658021329321));
#198272=CARTESIAN_POINT('',(119.049875110318,6.65,49.9602902344618));
#198273=CARTESIAN_POINT('',(119.107118084187,6.65,49.6658021329321));
#198274=CARTESIAN_POINT('',(118.559061607768,6.65,49.8648852780125));
#198275=CARTESIAN_POINT('',(118.559061607768,6.65,49.8648852780125));
#198276=CARTESIAN_POINT('',(118.616304581638,6.65,49.5703971764828));
#198277=CARTESIAN_POINT('',(118.616304581638,6.65,49.5703971764828));
#198278=CARTESIAN_POINT('',(118.616304581638,6.65,49.5703971764828));
#198279=CARTESIAN_POINT('Origin',(119.107118084187,6.65,49.6658021329321));
#198280=CARTESIAN_POINT('',(119.107118084187,6.15,49.6658021329321));
#198281=CARTESIAN_POINT('',(119.049875110318,6.15,49.9602902344618));
#198282=CARTESIAN_POINT('',(119.107118084187,6.15,49.6658021329321));
#198283=CARTESIAN_POINT('',(119.049875110318,6.65,49.9602902344618));
#198284=CARTESIAN_POINT('',(119.107118084187,6.65,49.6658021329321));
#198285=CARTESIAN_POINT('Origin',(119.107118084187,6.15,49.6658021329321));
#198286=CARTESIAN_POINT('',(118.616304581638,6.15,49.5703971764828));
#198287=CARTESIAN_POINT('',(118.559061607768,6.15,49.8648852780125));
#198288=CARTESIAN_POINT('',(118.616304581638,6.15,49.5703971764828));
#198289=CARTESIAN_POINT('',(119.049875110318,6.15,49.9602902344618));
#198290=CARTESIAN_POINT('',(119.107118084187,6.15,49.6658021329321));
#198291=CARTESIAN_POINT('Origin',(118.616304581638,6.15,49.5703971764828));
#198292=CARTESIAN_POINT('',(118.559061607768,6.15,49.8648852780125));
#198293=CARTESIAN_POINT('',(118.616304581638,6.15,49.5703971764828));
#198294=CARTESIAN_POINT('Origin',(117.831002977559,6.65,49.417749246164));
#198295=CARTESIAN_POINT('',(118.321816480108,6.65,49.5131542026133));
#198296=CARTESIAN_POINT('',(118.264573506239,6.65,49.807642304143));
#198297=CARTESIAN_POINT('',(118.321816480108,6.65,49.5131542026133));
#198298=CARTESIAN_POINT('',(117.773760003689,6.65,49.7122373476937));
#198299=CARTESIAN_POINT('',(117.773760003689,6.65,49.7122373476937));
#198300=CARTESIAN_POINT('',(117.831002977559,6.65,49.417749246164));
#198301=CARTESIAN_POINT('',(117.831002977559,6.65,49.417749246164));
#198302=CARTESIAN_POINT('',(117.831002977559,6.65,49.417749246164));
#198303=CARTESIAN_POINT('Origin',(118.321816480108,6.65,49.5131542026133));
#198304=CARTESIAN_POINT('',(118.321816480108,6.15,49.5131542026133));
#198305=CARTESIAN_POINT('',(118.264573506239,6.15,49.807642304143));
#198306=CARTESIAN_POINT('',(118.321816480108,6.15,49.5131542026133));
#198307=CARTESIAN_POINT('',(118.264573506239,6.65,49.807642304143));
#198308=CARTESIAN_POINT('',(118.321816480108,6.65,49.5131542026133));
#198309=CARTESIAN_POINT('Origin',(118.321816480108,6.15,49.5131542026133));
#198310=CARTESIAN_POINT('',(117.831002977559,6.15,49.417749246164));
#198311=CARTESIAN_POINT('',(117.773760003689,6.15,49.7122373476937));
#198312=CARTESIAN_POINT('',(117.831002977559,6.15,49.417749246164));
#198313=CARTESIAN_POINT('',(118.264573506239,6.15,49.807642304143));
#198314=CARTESIAN_POINT('',(118.321816480108,6.15,49.5131542026133));
#198315=CARTESIAN_POINT('Origin',(117.831002977559,6.15,49.417749246164));
#198316=CARTESIAN_POINT('',(117.773760003689,6.15,49.7122373476937));
#198317=CARTESIAN_POINT('',(117.831002977559,6.15,49.417749246164));
#198318=CARTESIAN_POINT('Origin',(117.045701373479,6.65,49.2651013158452));
#198319=CARTESIAN_POINT('',(117.536514876029,6.65,49.3605062722945));
#198320=CARTESIAN_POINT('',(117.479271902159,6.65,49.6549943738242));
#198321=CARTESIAN_POINT('',(117.536514876029,6.65,49.3605062722945));
#198322=CARTESIAN_POINT('',(116.98845839961,6.65,49.5595894173749));
#198323=CARTESIAN_POINT('',(116.98845839961,6.65,49.5595894173749));
#198324=CARTESIAN_POINT('',(117.045701373479,6.65,49.2651013158452));
#198325=CARTESIAN_POINT('',(117.045701373479,6.65,49.2651013158452));
#198326=CARTESIAN_POINT('',(117.045701373479,6.65,49.2651013158452));
#198327=CARTESIAN_POINT('Origin',(117.536514876029,6.65,49.3605062722945));
#198328=CARTESIAN_POINT('',(117.536514876029,6.15,49.3605062722945));
#198329=CARTESIAN_POINT('',(117.479271902159,6.15,49.6549943738242));
#198330=CARTESIAN_POINT('',(117.536514876029,6.15,49.3605062722945));
#198331=CARTESIAN_POINT('',(117.479271902159,6.65,49.6549943738242));
#198332=CARTESIAN_POINT('',(117.536514876029,6.65,49.3605062722945));
#198333=CARTESIAN_POINT('Origin',(117.536514876029,6.15,49.3605062722945));
#198334=CARTESIAN_POINT('',(117.045701373479,6.15,49.2651013158452));
#198335=CARTESIAN_POINT('',(116.98845839961,6.15,49.5595894173749));
#198336=CARTESIAN_POINT('',(117.045701373479,6.15,49.2651013158452));
#198337=CARTESIAN_POINT('',(117.479271902159,6.15,49.6549943738242));
#198338=CARTESIAN_POINT('',(117.536514876029,6.15,49.3605062722945));
#198339=CARTESIAN_POINT('Origin',(117.045701373479,6.15,49.2651013158452));
#198340=CARTESIAN_POINT('',(116.98845839961,6.15,49.5595894173749));
#198341=CARTESIAN_POINT('',(117.045701373479,6.15,49.2651013158452));
#198342=CARTESIAN_POINT('Origin',(116.2603997694,6.65,49.1124533855264));
#198343=CARTESIAN_POINT('',(116.75121327195,6.65,49.2078583419757));
#198344=CARTESIAN_POINT('',(116.69397029808,6.65,49.5023464435054));
#198345=CARTESIAN_POINT('',(116.75121327195,6.65,49.2078583419757));
#198346=CARTESIAN_POINT('',(116.203156795531,6.65,49.4069414870561));
#198347=CARTESIAN_POINT('',(116.203156795531,6.65,49.4069414870561));
#198348=CARTESIAN_POINT('',(116.2603997694,6.65,49.1124533855264));
#198349=CARTESIAN_POINT('',(116.2603997694,6.65,49.1124533855264));
#198350=CARTESIAN_POINT('',(116.2603997694,6.65,49.1124533855264));
#198351=CARTESIAN_POINT('Origin',(116.75121327195,6.65,49.2078583419757));
#198352=CARTESIAN_POINT('',(116.75121327195,6.15,49.2078583419757));
#198353=CARTESIAN_POINT('',(116.69397029808,6.15,49.5023464435054));
#198354=CARTESIAN_POINT('',(116.75121327195,6.15,49.2078583419757));
#198355=CARTESIAN_POINT('',(116.69397029808,6.65,49.5023464435054));
#198356=CARTESIAN_POINT('',(116.75121327195,6.65,49.2078583419757));
#198357=CARTESIAN_POINT('Origin',(116.75121327195,6.15,49.2078583419757));
#198358=CARTESIAN_POINT('',(116.2603997694,6.15,49.1124533855264));
#198359=CARTESIAN_POINT('',(116.203156795531,6.15,49.4069414870561));
#198360=CARTESIAN_POINT('',(116.2603997694,6.15,49.1124533855264));
#198361=CARTESIAN_POINT('',(116.69397029808,6.15,49.5023464435054));
#198362=CARTESIAN_POINT('',(116.75121327195,6.15,49.2078583419757));
#198363=CARTESIAN_POINT('Origin',(116.2603997694,6.15,49.1124533855264));
#198364=CARTESIAN_POINT('',(116.203156795531,6.15,49.4069414870561));
#198365=CARTESIAN_POINT('',(116.2603997694,6.15,49.1124533855264));
#198366=CARTESIAN_POINT('Origin',(115.475098165321,6.65,48.9598054552076));
#198367=CARTESIAN_POINT('',(115.96591166787,6.65,49.0552104116569));
#198368=CARTESIAN_POINT('',(115.908668694001,6.65,49.3496985131866));
#198369=CARTESIAN_POINT('',(115.96591166787,6.65,49.0552104116569));
#198370=CARTESIAN_POINT('',(115.417855191451,6.65,49.2542935567373));
#198371=CARTESIAN_POINT('',(115.417855191451,6.65,49.2542935567373));
#198372=CARTESIAN_POINT('',(115.475098165321,6.65,48.9598054552076));
#198373=CARTESIAN_POINT('',(115.475098165321,6.65,48.9598054552076));
#198374=CARTESIAN_POINT('',(115.475098165321,6.65,48.9598054552076));
#198375=CARTESIAN_POINT('Origin',(115.96591166787,6.65,49.0552104116569));
#198376=CARTESIAN_POINT('',(115.96591166787,6.15,49.0552104116569));
#198377=CARTESIAN_POINT('',(115.908668694001,6.15,49.3496985131866));
#198378=CARTESIAN_POINT('',(115.96591166787,6.15,49.0552104116569));
#198379=CARTESIAN_POINT('',(115.908668694001,6.65,49.3496985131866));
#198380=CARTESIAN_POINT('',(115.96591166787,6.65,49.0552104116569));
#198381=CARTESIAN_POINT('Origin',(115.96591166787,6.15,49.0552104116569));
#198382=CARTESIAN_POINT('',(115.475098165321,6.15,48.9598054552076));
#198383=CARTESIAN_POINT('',(115.417855191451,6.15,49.2542935567373));
#198384=CARTESIAN_POINT('',(115.475098165321,6.15,48.9598054552076));
#198385=CARTESIAN_POINT('',(115.908668694001,6.15,49.3496985131866));
#198386=CARTESIAN_POINT('',(115.96591166787,6.15,49.0552104116569));
#198387=CARTESIAN_POINT('Origin',(115.475098165321,6.15,48.9598054552076));
#198388=CARTESIAN_POINT('',(115.417855191451,6.15,49.2542935567373));
#198389=CARTESIAN_POINT('',(115.475098165321,6.15,48.9598054552076));
#198390=CARTESIAN_POINT('Origin',(114.689796561242,6.65,48.8071575248888));
#198391=CARTESIAN_POINT('',(115.180610063791,6.65,48.9025624813381));
#198392=CARTESIAN_POINT('',(115.123367089922,6.65,49.1970505828678));
#198393=CARTESIAN_POINT('',(115.180610063791,6.65,48.9025624813381));
#198394=CARTESIAN_POINT('',(114.632553587372,6.65,49.1016456264185));
#198395=CARTESIAN_POINT('',(114.632553587372,6.65,49.1016456264185));
#198396=CARTESIAN_POINT('',(114.689796561242,6.65,48.8071575248888));
#198397=CARTESIAN_POINT('',(114.689796561242,6.65,48.8071575248888));
#198398=CARTESIAN_POINT('',(114.689796561242,6.65,48.8071575248888));
#198399=CARTESIAN_POINT('Origin',(115.180610063791,6.65,48.9025624813381));
#198400=CARTESIAN_POINT('',(115.180610063791,6.15,48.9025624813381));
#198401=CARTESIAN_POINT('',(115.123367089922,6.15,49.1970505828678));
#198402=CARTESIAN_POINT('',(115.180610063791,6.15,48.9025624813381));
#198403=CARTESIAN_POINT('',(115.123367089922,6.65,49.1970505828678));
#198404=CARTESIAN_POINT('',(115.180610063791,6.65,48.9025624813381));
#198405=CARTESIAN_POINT('Origin',(115.180610063791,6.15,48.9025624813381));
#198406=CARTESIAN_POINT('',(114.689796561242,6.15,48.8071575248888));
#198407=CARTESIAN_POINT('',(114.632553587372,6.15,49.1016456264185));
#198408=CARTESIAN_POINT('',(114.689796561242,6.15,48.8071575248888));
#198409=CARTESIAN_POINT('',(115.123367089922,6.15,49.1970505828678));
#198410=CARTESIAN_POINT('',(115.180610063791,6.15,48.9025624813381));
#198411=CARTESIAN_POINT('Origin',(114.689796561242,6.15,48.8071575248888));
#198412=CARTESIAN_POINT('',(114.632553587372,6.15,49.1016456264185));
#198413=CARTESIAN_POINT('',(114.689796561242,6.15,48.8071575248888));
#198414=CARTESIAN_POINT('Origin',(113.904494957163,6.65,48.65450959457));
#198415=CARTESIAN_POINT('',(114.395308459712,6.65,48.7499145510193));
#198416=CARTESIAN_POINT('',(114.338065485842,6.65,49.044402652549));
#198417=CARTESIAN_POINT('',(114.395308459712,6.65,48.7499145510193));
#198418=CARTESIAN_POINT('',(113.847251983293,6.65,48.9489976960997));
#198419=CARTESIAN_POINT('',(113.847251983293,6.65,48.9489976960997));
#198420=CARTESIAN_POINT('',(113.904494957163,6.65,48.65450959457));
#198421=CARTESIAN_POINT('',(113.904494957163,6.65,48.65450959457));
#198422=CARTESIAN_POINT('',(113.904494957163,6.65,48.65450959457));
#198423=CARTESIAN_POINT('Origin',(114.395308459712,6.65,48.7499145510193));
#198424=CARTESIAN_POINT('',(114.395308459712,6.15,48.7499145510193));
#198425=CARTESIAN_POINT('',(114.338065485842,6.15,49.044402652549));
#198426=CARTESIAN_POINT('',(114.395308459712,6.15,48.7499145510193));
#198427=CARTESIAN_POINT('',(114.338065485842,6.65,49.044402652549));
#198428=CARTESIAN_POINT('',(114.395308459712,6.65,48.7499145510193));
#198429=CARTESIAN_POINT('Origin',(114.395308459712,6.15,48.7499145510193));
#198430=CARTESIAN_POINT('',(113.904494957163,6.15,48.65450959457));
#198431=CARTESIAN_POINT('',(113.847251983293,6.15,48.9489976960997));
#198432=CARTESIAN_POINT('',(113.904494957163,6.15,48.65450959457));
#198433=CARTESIAN_POINT('',(114.338065485842,6.15,49.044402652549));
#198434=CARTESIAN_POINT('',(114.395308459712,6.15,48.7499145510193));
#198435=CARTESIAN_POINT('Origin',(113.904494957163,6.15,48.65450959457));
#198436=CARTESIAN_POINT('',(113.847251983293,6.15,48.9489976960997));
#198437=CARTESIAN_POINT('',(113.904494957163,6.15,48.65450959457));
#198438=CARTESIAN_POINT('Origin',(113.119193353083,6.65,48.5018616642512));
#198439=CARTESIAN_POINT('',(113.610006855633,6.65,48.5972666207005));
#198440=CARTESIAN_POINT('',(113.552763881763,6.65,48.8917547222302));
#198441=CARTESIAN_POINT('',(113.610006855633,6.65,48.5972666207005));
#198442=CARTESIAN_POINT('',(113.061950379214,6.65,48.7963497657809));
#198443=CARTESIAN_POINT('',(113.061950379214,6.65,48.7963497657809));
#198444=CARTESIAN_POINT('',(113.119193353083,6.65,48.5018616642512));
#198445=CARTESIAN_POINT('',(113.119193353083,6.65,48.5018616642512));
#198446=CARTESIAN_POINT('',(113.119193353083,6.65,48.5018616642512));
#198447=CARTESIAN_POINT('Origin',(113.610006855633,6.65,48.5972666207005));
#198448=CARTESIAN_POINT('',(113.610006855633,6.15,48.5972666207005));
#198449=CARTESIAN_POINT('',(113.552763881763,6.15,48.8917547222302));
#198450=CARTESIAN_POINT('',(113.610006855633,6.15,48.5972666207005));
#198451=CARTESIAN_POINT('',(113.552763881763,6.65,48.8917547222302));
#198452=CARTESIAN_POINT('',(113.610006855633,6.65,48.5972666207005));
#198453=CARTESIAN_POINT('Origin',(113.610006855633,6.15,48.5972666207005));
#198454=CARTESIAN_POINT('',(113.119193353083,6.15,48.5018616642512));
#198455=CARTESIAN_POINT('',(113.061950379214,6.15,48.7963497657809));
#198456=CARTESIAN_POINT('',(113.119193353083,6.15,48.5018616642512));
#198457=CARTESIAN_POINT('',(113.552763881763,6.15,48.8917547222302));
#198458=CARTESIAN_POINT('',(113.610006855633,6.15,48.5972666207005));
#198459=CARTESIAN_POINT('Origin',(113.119193353083,6.15,48.5018616642512));
#198460=CARTESIAN_POINT('',(113.061950379214,6.15,48.7963497657809));
#198461=CARTESIAN_POINT('',(113.119193353083,6.15,48.5018616642512));
#198462=CARTESIAN_POINT('Origin',(112.333891749004,6.65,48.3492137339324));
#198463=CARTESIAN_POINT('',(112.824705251554,6.65,48.4446186903817));
#198464=CARTESIAN_POINT('',(112.767462277684,6.65,48.7391067919114));
#198465=CARTESIAN_POINT('',(112.824705251554,6.65,48.4446186903817));
#198466=CARTESIAN_POINT('',(112.276648775135,6.65,48.6437018354621));
#198467=CARTESIAN_POINT('',(112.276648775135,6.65,48.6437018354621));
#198468=CARTESIAN_POINT('',(112.333891749004,6.65,48.3492137339324));
#198469=CARTESIAN_POINT('',(112.333891749004,6.65,48.3492137339324));
#198470=CARTESIAN_POINT('',(112.333891749004,6.65,48.3492137339324));
#198471=CARTESIAN_POINT('Origin',(112.824705251554,6.65,48.4446186903817));
#198472=CARTESIAN_POINT('',(112.824705251554,6.15,48.4446186903817));
#198473=CARTESIAN_POINT('',(112.767462277684,6.15,48.7391067919114));
#198474=CARTESIAN_POINT('',(112.824705251554,6.15,48.4446186903817));
#198475=CARTESIAN_POINT('',(112.767462277684,6.65,48.7391067919114));
#198476=CARTESIAN_POINT('',(112.824705251554,6.65,48.4446186903817));
#198477=CARTESIAN_POINT('Origin',(112.824705251554,6.15,48.4446186903817));
#198478=CARTESIAN_POINT('',(112.333891749004,6.15,48.3492137339324));
#198479=CARTESIAN_POINT('',(112.276648775135,6.15,48.6437018354621));
#198480=CARTESIAN_POINT('',(112.333891749004,6.15,48.3492137339324));
#198481=CARTESIAN_POINT('',(112.767462277684,6.15,48.7391067919114));
#198482=CARTESIAN_POINT('',(112.824705251554,6.15,48.4446186903817));
#198483=CARTESIAN_POINT('Origin',(112.333891749004,6.15,48.3492137339324));
#198484=CARTESIAN_POINT('',(112.276648775135,6.15,48.6437018354621));
#198485=CARTESIAN_POINT('',(112.333891749004,6.15,48.3492137339324));
#198486=CARTESIAN_POINT('Origin',(111.548590144925,6.65,48.1965658036136));
#198487=CARTESIAN_POINT('',(112.039403647474,6.65,48.2919707600629));
#198488=CARTESIAN_POINT('',(111.982160673605,6.65,48.5864588615926));
#198489=CARTESIAN_POINT('',(112.039403647474,6.65,48.2919707600629));
#198490=CARTESIAN_POINT('',(111.491347171055,6.65,48.4910539051433));
#198491=CARTESIAN_POINT('',(111.491347171055,6.65,48.4910539051433));
#198492=CARTESIAN_POINT('',(111.548590144925,6.65,48.1965658036136));
#198493=CARTESIAN_POINT('',(111.548590144925,6.65,48.1965658036136));
#198494=CARTESIAN_POINT('',(111.548590144925,6.65,48.1965658036136));
#198495=CARTESIAN_POINT('Origin',(112.039403647474,6.65,48.2919707600629));
#198496=CARTESIAN_POINT('',(112.039403647474,6.15,48.2919707600629));
#198497=CARTESIAN_POINT('',(111.982160673605,6.15,48.5864588615926));
#198498=CARTESIAN_POINT('',(112.039403647474,6.15,48.2919707600629));
#198499=CARTESIAN_POINT('',(111.982160673605,6.65,48.5864588615926));
#198500=CARTESIAN_POINT('',(112.039403647474,6.65,48.2919707600629));
#198501=CARTESIAN_POINT('Origin',(112.039403647474,6.15,48.2919707600629));
#198502=CARTESIAN_POINT('',(111.548590144925,6.15,48.1965658036136));
#198503=CARTESIAN_POINT('',(111.491347171055,6.15,48.4910539051433));
#198504=CARTESIAN_POINT('',(111.548590144925,6.15,48.1965658036136));
#198505=CARTESIAN_POINT('',(111.982160673605,6.15,48.5864588615926));
#198506=CARTESIAN_POINT('',(112.039403647474,6.15,48.2919707600629));
#198507=CARTESIAN_POINT('Origin',(111.548590144925,6.15,48.1965658036136));
#198508=CARTESIAN_POINT('',(111.491347171055,6.15,48.4910539051433));
#198509=CARTESIAN_POINT('',(111.548590144925,6.15,48.1965658036136));
#198510=CARTESIAN_POINT('Origin',(111.548590144925,5.85,48.1965658036136));
#198511=CARTESIAN_POINT('',(112.039403647474,5.85,48.2919707600629));
#198512=CARTESIAN_POINT('',(111.982160673605,5.85,48.5864588615926));
#198513=CARTESIAN_POINT('',(112.039403647474,5.85,48.2919707600629));
#198514=CARTESIAN_POINT('',(111.491347171055,5.85,48.4910539051433));
#198515=CARTESIAN_POINT('',(111.491347171055,5.85,48.4910539051433));
#198516=CARTESIAN_POINT('',(111.548590144925,5.85,48.1965658036136));
#198517=CARTESIAN_POINT('',(111.548590144925,5.85,48.1965658036136));
#198518=CARTESIAN_POINT('',(111.548590144925,5.85,48.1965658036136));
#198519=CARTESIAN_POINT('Origin',(112.039403647474,5.85,48.2919707600629));
#198520=CARTESIAN_POINT('',(112.039403647474,5.35,48.2919707600629));
#198521=CARTESIAN_POINT('',(111.982160673605,5.35,48.5864588615926));
#198522=CARTESIAN_POINT('',(112.039403647474,5.35,48.2919707600629));
#198523=CARTESIAN_POINT('',(111.982160673605,5.85,48.5864588615926));
#198524=CARTESIAN_POINT('',(112.039403647474,5.85,48.2919707600629));
#198525=CARTESIAN_POINT('Origin',(112.039403647474,5.35,48.2919707600629));
#198526=CARTESIAN_POINT('',(111.548590144925,5.35,48.1965658036136));
#198527=CARTESIAN_POINT('',(111.491347171055,5.35,48.4910539051433));
#198528=CARTESIAN_POINT('',(111.548590144925,5.35,48.1965658036136));
#198529=CARTESIAN_POINT('',(111.982160673605,5.35,48.5864588615926));
#198530=CARTESIAN_POINT('',(112.039403647474,5.35,48.2919707600629));
#198531=CARTESIAN_POINT('Origin',(111.548590144925,5.35,48.1965658036136));
#198532=CARTESIAN_POINT('',(111.491347171055,5.35,48.4910539051433));
#198533=CARTESIAN_POINT('',(111.548590144925,5.35,48.1965658036136));
#198534=CARTESIAN_POINT('Origin',(111.548590144925,5.05,48.1965658036136));
#198535=CARTESIAN_POINT('',(112.039403647474,5.05,48.2919707600629));
#198536=CARTESIAN_POINT('',(111.982160673605,5.05,48.5864588615926));
#198537=CARTESIAN_POINT('',(112.039403647474,5.05,48.2919707600629));
#198538=CARTESIAN_POINT('',(111.491347171055,5.05,48.4910539051433));
#198539=CARTESIAN_POINT('',(111.491347171055,5.05,48.4910539051433));
#198540=CARTESIAN_POINT('',(111.548590144925,5.05,48.1965658036136));
#198541=CARTESIAN_POINT('',(111.548590144925,5.05,48.1965658036136));
#198542=CARTESIAN_POINT('',(111.548590144925,5.05,48.1965658036136));
#198543=CARTESIAN_POINT('Origin',(112.039403647474,5.05,48.2919707600629));
#198544=CARTESIAN_POINT('',(112.039403647474,4.55,48.2919707600629));
#198545=CARTESIAN_POINT('',(111.982160673605,4.55,48.5864588615926));
#198546=CARTESIAN_POINT('',(112.039403647474,4.55,48.2919707600629));
#198547=CARTESIAN_POINT('',(111.982160673605,5.05,48.5864588615926));
#198548=CARTESIAN_POINT('',(112.039403647474,5.05,48.2919707600629));
#198549=CARTESIAN_POINT('Origin',(112.039403647474,4.55,48.2919707600629));
#198550=CARTESIAN_POINT('',(111.548590144925,4.55,48.1965658036136));
#198551=CARTESIAN_POINT('',(111.491347171055,4.55,48.4910539051433));
#198552=CARTESIAN_POINT('',(111.548590144925,4.55,48.1965658036136));
#198553=CARTESIAN_POINT('',(111.982160673605,4.55,48.5864588615926));
#198554=CARTESIAN_POINT('',(112.039403647474,4.55,48.2919707600629));
#198555=CARTESIAN_POINT('Origin',(111.548590144925,4.55,48.1965658036136));
#198556=CARTESIAN_POINT('',(111.491347171055,4.55,48.4910539051433));
#198557=CARTESIAN_POINT('',(111.548590144925,4.55,48.1965658036136));
#198558=CARTESIAN_POINT('Origin',(111.548590144925,4.25,48.1965658036136));
#198559=CARTESIAN_POINT('',(112.039403647474,4.25,48.2919707600629));
#198560=CARTESIAN_POINT('',(111.982160673605,4.25,48.5864588615926));
#198561=CARTESIAN_POINT('',(112.039403647474,4.25,48.2919707600629));
#198562=CARTESIAN_POINT('',(111.491347171055,4.25,48.4910539051433));
#198563=CARTESIAN_POINT('',(111.491347171055,4.25,48.4910539051433));
#198564=CARTESIAN_POINT('',(111.548590144925,4.25,48.1965658036136));
#198565=CARTESIAN_POINT('',(111.548590144925,4.25,48.1965658036136));
#198566=CARTESIAN_POINT('',(111.548590144925,4.25,48.1965658036136));
#198567=CARTESIAN_POINT('Origin',(112.039403647474,4.25,48.2919707600629));
#198568=CARTESIAN_POINT('',(112.039403647474,3.75,48.2919707600629));
#198569=CARTESIAN_POINT('',(111.982160673605,3.75,48.5864588615926));
#198570=CARTESIAN_POINT('',(112.039403647474,3.75,48.2919707600629));
#198571=CARTESIAN_POINT('',(111.982160673605,4.25,48.5864588615926));
#198572=CARTESIAN_POINT('',(112.039403647474,4.25,48.2919707600629));
#198573=CARTESIAN_POINT('Origin',(112.039403647474,3.75,48.2919707600629));
#198574=CARTESIAN_POINT('',(111.548590144925,3.75,48.1965658036136));
#198575=CARTESIAN_POINT('',(111.491347171055,3.75,48.4910539051433));
#198576=CARTESIAN_POINT('',(111.548590144925,3.75,48.1965658036136));
#198577=CARTESIAN_POINT('',(111.982160673605,3.75,48.5864588615926));
#198578=CARTESIAN_POINT('',(112.039403647474,3.75,48.2919707600629));
#198579=CARTESIAN_POINT('Origin',(111.548590144925,3.75,48.1965658036136));
#198580=CARTESIAN_POINT('',(111.491347171055,3.75,48.4910539051433));
#198581=CARTESIAN_POINT('',(111.548590144925,3.75,48.1965658036136));
#198582=CARTESIAN_POINT('Origin',(111.548590144925,3.45,48.1965658036136));
#198583=CARTESIAN_POINT('',(112.039403647474,3.45,48.2919707600629));
#198584=CARTESIAN_POINT('',(111.982160673605,3.45,48.5864588615926));
#198585=CARTESIAN_POINT('',(112.039403647474,3.45,48.2919707600629));
#198586=CARTESIAN_POINT('',(111.491347171055,3.45,48.4910539051433));
#198587=CARTESIAN_POINT('',(111.491347171055,3.45,48.4910539051433));
#198588=CARTESIAN_POINT('',(111.548590144925,3.45,48.1965658036136));
#198589=CARTESIAN_POINT('',(111.548590144925,3.45,48.1965658036136));
#198590=CARTESIAN_POINT('',(111.548590144925,3.45,48.1965658036136));
#198591=CARTESIAN_POINT('Origin',(112.039403647474,3.45,48.2919707600629));
#198592=CARTESIAN_POINT('',(112.039403647474,2.95,48.2919707600629));
#198593=CARTESIAN_POINT('',(111.982160673605,2.95,48.5864588615926));
#198594=CARTESIAN_POINT('',(112.039403647474,2.95,48.2919707600629));
#198595=CARTESIAN_POINT('',(111.982160673605,3.45,48.5864588615926));
#198596=CARTESIAN_POINT('',(112.039403647474,3.45,48.2919707600629));
#198597=CARTESIAN_POINT('Origin',(112.039403647474,2.95,48.2919707600629));
#198598=CARTESIAN_POINT('',(111.548590144925,2.95,48.1965658036136));
#198599=CARTESIAN_POINT('',(111.491347171055,2.95,48.4910539051433));
#198600=CARTESIAN_POINT('',(111.548590144925,2.95,48.1965658036136));
#198601=CARTESIAN_POINT('',(111.982160673605,2.95,48.5864588615926));
#198602=CARTESIAN_POINT('',(112.039403647474,2.95,48.2919707600629));
#198603=CARTESIAN_POINT('Origin',(111.548590144925,2.95,48.1965658036136));
#198604=CARTESIAN_POINT('',(111.491347171055,2.95,48.4910539051433));
#198605=CARTESIAN_POINT('',(111.548590144925,2.95,48.1965658036136));
#198606=CARTESIAN_POINT('Origin',(111.548590144925,2.65,48.1965658036136));
#198607=CARTESIAN_POINT('',(112.039403647474,2.65,48.2919707600629));
#198608=CARTESIAN_POINT('',(111.982160673605,2.65,48.5864588615926));
#198609=CARTESIAN_POINT('',(112.039403647474,2.65,48.2919707600629));
#198610=CARTESIAN_POINT('',(111.491347171055,2.65,48.4910539051433));
#198611=CARTESIAN_POINT('',(111.491347171055,2.65,48.4910539051433));
#198612=CARTESIAN_POINT('',(111.548590144925,2.65,48.1965658036136));
#198613=CARTESIAN_POINT('',(111.548590144925,2.65,48.1965658036136));
#198614=CARTESIAN_POINT('',(111.548590144925,2.65,48.1965658036136));
#198615=CARTESIAN_POINT('Origin',(112.039403647474,2.65,48.2919707600629));
#198616=CARTESIAN_POINT('',(112.039403647474,2.15,48.2919707600629));
#198617=CARTESIAN_POINT('',(111.982160673605,2.15,48.5864588615926));
#198618=CARTESIAN_POINT('',(112.039403647474,2.15,48.2919707600629));
#198619=CARTESIAN_POINT('',(111.982160673605,2.65,48.5864588615926));
#198620=CARTESIAN_POINT('',(112.039403647474,2.65,48.2919707600629));
#198621=CARTESIAN_POINT('Origin',(112.039403647474,2.15,48.2919707600629));
#198622=CARTESIAN_POINT('',(111.548590144925,2.15,48.1965658036136));
#198623=CARTESIAN_POINT('',(111.491347171055,2.15,48.4910539051433));
#198624=CARTESIAN_POINT('',(111.548590144925,2.15,48.1965658036136));
#198625=CARTESIAN_POINT('',(111.982160673605,2.15,48.5864588615926));
#198626=CARTESIAN_POINT('',(112.039403647474,2.15,48.2919707600629));
#198627=CARTESIAN_POINT('Origin',(111.548590144925,2.15,48.1965658036136));
#198628=CARTESIAN_POINT('',(111.491347171055,2.15,48.4910539051433));
#198629=CARTESIAN_POINT('',(111.548590144925,2.15,48.1965658036136));
#198630=CARTESIAN_POINT('Origin',(111.548590144925,1.85,48.1965658036136));
#198631=CARTESIAN_POINT('',(112.039403647474,1.85,48.2919707600629));
#198632=CARTESIAN_POINT('',(111.982160673605,1.85,48.5864588615926));
#198633=CARTESIAN_POINT('',(112.039403647474,1.85,48.2919707600629));
#198634=CARTESIAN_POINT('',(111.491347171055,1.85,48.4910539051433));
#198635=CARTESIAN_POINT('',(111.491347171055,1.85,48.4910539051433));
#198636=CARTESIAN_POINT('',(111.548590144925,1.85,48.1965658036136));
#198637=CARTESIAN_POINT('',(111.548590144925,1.85,48.1965658036136));
#198638=CARTESIAN_POINT('',(111.548590144925,1.85,48.1965658036136));
#198639=CARTESIAN_POINT('Origin',(112.039403647474,1.85,48.2919707600629));
#198640=CARTESIAN_POINT('',(112.039403647474,1.35,48.2919707600629));
#198641=CARTESIAN_POINT('',(111.982160673605,1.35,48.5864588615926));
#198642=CARTESIAN_POINT('',(112.039403647474,1.35,48.2919707600629));
#198643=CARTESIAN_POINT('',(111.982160673605,1.85,48.5864588615926));
#198644=CARTESIAN_POINT('',(112.039403647474,1.85,48.2919707600629));
#198645=CARTESIAN_POINT('Origin',(112.039403647474,1.35,48.2919707600629));
#198646=CARTESIAN_POINT('',(111.548590144925,1.35,48.1965658036136));
#198647=CARTESIAN_POINT('',(111.491347171055,1.35,48.4910539051433));
#198648=CARTESIAN_POINT('',(111.548590144925,1.35,48.1965658036136));
#198649=CARTESIAN_POINT('',(111.982160673605,1.35,48.5864588615926));
#198650=CARTESIAN_POINT('',(112.039403647474,1.35,48.2919707600629));
#198651=CARTESIAN_POINT('Origin',(111.548590144925,1.35,48.1965658036136));
#198652=CARTESIAN_POINT('',(111.491347171055,1.35,48.4910539051433));
#198653=CARTESIAN_POINT('',(111.548590144925,1.35,48.1965658036136));
#198654=CARTESIAN_POINT('Origin',(111.548590144925,1.05,48.1965658036136));
#198655=CARTESIAN_POINT('',(112.039403647474,1.05,48.2919707600629));
#198656=CARTESIAN_POINT('',(111.982160673605,1.05,48.5864588615926));
#198657=CARTESIAN_POINT('',(112.039403647474,1.05,48.2919707600629));
#198658=CARTESIAN_POINT('',(111.491347171055,1.05,48.4910539051433));
#198659=CARTESIAN_POINT('',(111.491347171055,1.05,48.4910539051433));
#198660=CARTESIAN_POINT('',(111.548590144925,1.05,48.1965658036136));
#198661=CARTESIAN_POINT('',(111.548590144925,1.05,48.1965658036136));
#198662=CARTESIAN_POINT('',(111.548590144925,1.05,48.1965658036136));
#198663=CARTESIAN_POINT('Origin',(112.039403647474,1.05,48.2919707600629));
#198664=CARTESIAN_POINT('',(112.039403647474,0.550000000000015,48.2919707600629));
#198665=CARTESIAN_POINT('',(111.982160673605,0.550000000000015,48.5864588615926));
#198666=CARTESIAN_POINT('',(112.039403647474,0.550000000000015,48.2919707600629));
#198667=CARTESIAN_POINT('',(111.982160673605,1.05,48.5864588615926));
#198668=CARTESIAN_POINT('',(112.039403647474,1.05,48.2919707600629));
#198669=CARTESIAN_POINT('Origin',(112.039403647474,0.550000000000015,48.2919707600629));
#198670=CARTESIAN_POINT('',(111.548590144925,0.550000000000015,48.1965658036136));
#198671=CARTESIAN_POINT('',(111.491347171055,0.550000000000015,48.4910539051433));
#198672=CARTESIAN_POINT('',(111.548590144925,0.550000000000015,48.1965658036136));
#198673=CARTESIAN_POINT('',(111.982160673605,0.550000000000015,48.5864588615926));
#198674=CARTESIAN_POINT('',(112.039403647474,0.550000000000015,48.2919707600629));
#198675=CARTESIAN_POINT('Origin',(111.548590144925,0.550000000000015,48.1965658036136));
#198676=CARTESIAN_POINT('',(111.491347171055,0.550000000000015,48.4910539051433));
#198677=CARTESIAN_POINT('',(111.548590144925,0.550000000000015,48.1965658036136));
#198678=CARTESIAN_POINT('Origin',(111.548590144925,0.250000000000015,48.1965658036136));
#198679=CARTESIAN_POINT('',(112.039403647474,0.250000000000015,48.2919707600629));
#198680=CARTESIAN_POINT('',(111.982160673605,0.250000000000015,48.5864588615926));
#198681=CARTESIAN_POINT('',(112.039403647474,0.250000000000015,48.2919707600629));
#198682=CARTESIAN_POINT('',(111.491347171055,0.250000000000015,48.4910539051433));
#198683=CARTESIAN_POINT('',(111.491347171055,0.250000000000015,48.4910539051433));
#198684=CARTESIAN_POINT('',(111.548590144925,0.250000000000015,48.1965658036136));
#198685=CARTESIAN_POINT('',(111.548590144925,0.250000000000015,48.1965658036136));
#198686=CARTESIAN_POINT('',(111.548590144925,0.250000000000015,48.1965658036136));
#198687=CARTESIAN_POINT('Origin',(112.039403647474,0.250000000000015,48.2919707600629));
#198688=CARTESIAN_POINT('',(112.039403647474,-0.249999999999985,48.2919707600629));
#198689=CARTESIAN_POINT('',(111.982160673605,-0.249999999999985,48.5864588615926));
#198690=CARTESIAN_POINT('',(112.039403647474,-0.249999999999985,48.2919707600629));
#198691=CARTESIAN_POINT('',(111.982160673605,0.250000000000015,48.5864588615926));
#198692=CARTESIAN_POINT('',(112.039403647474,0.250000000000015,48.2919707600629));
#198693=CARTESIAN_POINT('Origin',(112.039403647474,-0.249999999999985,48.2919707600629));
#198694=CARTESIAN_POINT('',(111.548590144925,-0.249999999999985,48.1965658036136));
#198695=CARTESIAN_POINT('',(111.491347171055,-0.249999999999985,48.4910539051433));
#198696=CARTESIAN_POINT('',(111.548590144925,-0.249999999999985,48.1965658036136));
#198697=CARTESIAN_POINT('',(111.982160673605,-0.249999999999985,48.5864588615926));
#198698=CARTESIAN_POINT('',(112.039403647474,-0.249999999999985,48.2919707600629));
#198699=CARTESIAN_POINT('Origin',(111.548590144925,-0.249999999999985,48.1965658036136));
#198700=CARTESIAN_POINT('',(111.491347171055,-0.249999999999985,48.4910539051433));
#198701=CARTESIAN_POINT('',(111.548590144925,-0.249999999999985,48.1965658036136));
#198702=CARTESIAN_POINT('Origin',(111.548590144925,-0.549999999999986,48.1965658036136));
#198703=CARTESIAN_POINT('',(112.039403647474,-0.549999999999986,48.2919707600629));
#198704=CARTESIAN_POINT('',(111.982160673605,-0.549999999999986,48.5864588615926));
#198705=CARTESIAN_POINT('',(112.039403647474,-0.549999999999986,48.2919707600629));
#198706=CARTESIAN_POINT('',(111.491347171055,-0.549999999999986,48.4910539051433));
#198707=CARTESIAN_POINT('',(111.491347171055,-0.549999999999986,48.4910539051433));
#198708=CARTESIAN_POINT('',(111.548590144925,-0.549999999999986,48.1965658036136));
#198709=CARTESIAN_POINT('',(111.548590144925,-0.549999999999986,48.1965658036136));
#198710=CARTESIAN_POINT('',(111.548590144925,-0.549999999999986,48.1965658036136));
#198711=CARTESIAN_POINT('Origin',(112.039403647474,-0.549999999999986,48.2919707600629));
#198712=CARTESIAN_POINT('',(112.039403647474,-1.05,48.2919707600629));
#198713=CARTESIAN_POINT('',(111.982160673605,-1.05,48.5864588615926));
#198714=CARTESIAN_POINT('',(112.039403647474,-1.05,48.2919707600629));
#198715=CARTESIAN_POINT('',(111.982160673605,-0.549999999999986,48.5864588615926));
#198716=CARTESIAN_POINT('',(112.039403647474,-0.549999999999986,48.2919707600629));
#198717=CARTESIAN_POINT('Origin',(112.039403647474,-1.05,48.2919707600629));
#198718=CARTESIAN_POINT('',(111.548590144925,-1.05,48.1965658036136));
#198719=CARTESIAN_POINT('',(111.491347171055,-1.05,48.4910539051433));
#198720=CARTESIAN_POINT('',(111.548590144925,-1.05,48.1965658036136));
#198721=CARTESIAN_POINT('',(111.982160673605,-1.05,48.5864588615926));
#198722=CARTESIAN_POINT('',(112.039403647474,-1.05,48.2919707600629));
#198723=CARTESIAN_POINT('Origin',(111.548590144925,-1.05,48.1965658036136));
#198724=CARTESIAN_POINT('',(111.491347171055,-1.05,48.4910539051433));
#198725=CARTESIAN_POINT('',(111.548590144925,-1.05,48.1965658036136));
#198726=CARTESIAN_POINT('Origin',(111.548590144925,-1.35,48.1965658036136));
#198727=CARTESIAN_POINT('',(112.039403647474,-1.35,48.2919707600629));
#198728=CARTESIAN_POINT('',(111.982160673605,-1.35,48.5864588615926));
#198729=CARTESIAN_POINT('',(112.039403647474,-1.35,48.2919707600629));
#198730=CARTESIAN_POINT('',(111.491347171055,-1.35,48.4910539051433));
#198731=CARTESIAN_POINT('',(111.491347171055,-1.35,48.4910539051433));
#198732=CARTESIAN_POINT('',(111.548590144925,-1.35,48.1965658036136));
#198733=CARTESIAN_POINT('',(111.548590144925,-1.35,48.1965658036136));
#198734=CARTESIAN_POINT('',(111.548590144925,-1.35,48.1965658036136));
#198735=CARTESIAN_POINT('Origin',(112.039403647474,-1.35,48.2919707600629));
#198736=CARTESIAN_POINT('',(112.039403647474,-1.85,48.2919707600629));
#198737=CARTESIAN_POINT('',(111.982160673605,-1.85,48.5864588615926));
#198738=CARTESIAN_POINT('',(112.039403647474,-1.85,48.2919707600629));
#198739=CARTESIAN_POINT('',(111.982160673605,-1.35,48.5864588615926));
#198740=CARTESIAN_POINT('',(112.039403647474,-1.35,48.2919707600629));
#198741=CARTESIAN_POINT('Origin',(112.039403647474,-1.85,48.2919707600629));
#198742=CARTESIAN_POINT('',(111.548590144925,-1.85,48.1965658036136));
#198743=CARTESIAN_POINT('',(111.491347171055,-1.85,48.4910539051433));
#198744=CARTESIAN_POINT('',(111.548590144925,-1.85,48.1965658036136));
#198745=CARTESIAN_POINT('',(111.982160673605,-1.85,48.5864588615926));
#198746=CARTESIAN_POINT('',(112.039403647474,-1.85,48.2919707600629));
#198747=CARTESIAN_POINT('Origin',(111.548590144925,-1.85,48.1965658036136));
#198748=CARTESIAN_POINT('',(111.491347171055,-1.85,48.4910539051433));
#198749=CARTESIAN_POINT('',(111.548590144925,-1.85,48.1965658036136));
#198750=CARTESIAN_POINT('Origin',(111.548590144925,-2.15,48.1965658036136));
#198751=CARTESIAN_POINT('',(112.039403647474,-2.15,48.2919707600629));
#198752=CARTESIAN_POINT('',(111.982160673605,-2.15,48.5864588615926));
#198753=CARTESIAN_POINT('',(112.039403647474,-2.15,48.2919707600629));
#198754=CARTESIAN_POINT('',(111.491347171055,-2.15,48.4910539051433));
#198755=CARTESIAN_POINT('',(111.491347171055,-2.15,48.4910539051433));
#198756=CARTESIAN_POINT('',(111.548590144925,-2.15,48.1965658036136));
#198757=CARTESIAN_POINT('',(111.548590144925,-2.15,48.1965658036136));
#198758=CARTESIAN_POINT('',(111.548590144925,-2.15,48.1965658036136));
#198759=CARTESIAN_POINT('Origin',(112.039403647474,-2.15,48.2919707600629));
#198760=CARTESIAN_POINT('',(112.039403647474,-2.65,48.2919707600629));
#198761=CARTESIAN_POINT('',(111.982160673605,-2.65,48.5864588615926));
#198762=CARTESIAN_POINT('',(112.039403647474,-2.65,48.2919707600629));
#198763=CARTESIAN_POINT('',(111.982160673605,-2.15,48.5864588615926));
#198764=CARTESIAN_POINT('',(112.039403647474,-2.15,48.2919707600629));
#198765=CARTESIAN_POINT('Origin',(112.039403647474,-2.65,48.2919707600629));
#198766=CARTESIAN_POINT('',(111.548590144925,-2.65,48.1965658036136));
#198767=CARTESIAN_POINT('',(111.491347171055,-2.65,48.4910539051433));
#198768=CARTESIAN_POINT('',(111.548590144925,-2.65,48.1965658036136));
#198769=CARTESIAN_POINT('',(111.982160673605,-2.65,48.5864588615926));
#198770=CARTESIAN_POINT('',(112.039403647474,-2.65,48.2919707600629));
#198771=CARTESIAN_POINT('Origin',(111.548590144925,-2.65,48.1965658036136));
#198772=CARTESIAN_POINT('',(111.491347171055,-2.65,48.4910539051433));
#198773=CARTESIAN_POINT('',(111.548590144925,-2.65,48.1965658036136));
#198774=CARTESIAN_POINT('Origin',(111.548590144925,-2.95,48.1965658036136));
#198775=CARTESIAN_POINT('',(112.039403647474,-2.95,48.2919707600629));
#198776=CARTESIAN_POINT('',(111.982160673605,-2.95,48.5864588615926));
#198777=CARTESIAN_POINT('',(112.039403647474,-2.95,48.2919707600629));
#198778=CARTESIAN_POINT('',(111.491347171055,-2.95,48.4910539051433));
#198779=CARTESIAN_POINT('',(111.491347171055,-2.95,48.4910539051433));
#198780=CARTESIAN_POINT('',(111.548590144925,-2.95,48.1965658036136));
#198781=CARTESIAN_POINT('',(111.548590144925,-2.95,48.1965658036136));
#198782=CARTESIAN_POINT('',(111.548590144925,-2.95,48.1965658036136));
#198783=CARTESIAN_POINT('Origin',(112.039403647474,-2.95,48.2919707600629));
#198784=CARTESIAN_POINT('',(112.039403647474,-3.45,48.2919707600629));
#198785=CARTESIAN_POINT('',(111.982160673605,-3.45,48.5864588615926));
#198786=CARTESIAN_POINT('',(112.039403647474,-3.45,48.2919707600629));
#198787=CARTESIAN_POINT('',(111.982160673605,-2.95,48.5864588615926));
#198788=CARTESIAN_POINT('',(112.039403647474,-2.95,48.2919707600629));
#198789=CARTESIAN_POINT('Origin',(112.039403647474,-3.45,48.2919707600629));
#198790=CARTESIAN_POINT('',(111.548590144925,-3.45,48.1965658036136));
#198791=CARTESIAN_POINT('',(111.491347171055,-3.45,48.4910539051433));
#198792=CARTESIAN_POINT('',(111.548590144925,-3.45,48.1965658036136));
#198793=CARTESIAN_POINT('',(111.982160673605,-3.45,48.5864588615926));
#198794=CARTESIAN_POINT('',(112.039403647474,-3.45,48.2919707600629));
#198795=CARTESIAN_POINT('Origin',(111.548590144925,-3.45,48.1965658036136));
#198796=CARTESIAN_POINT('',(111.491347171055,-3.45,48.4910539051433));
#198797=CARTESIAN_POINT('',(111.548590144925,-3.45,48.1965658036136));
#198798=CARTESIAN_POINT('Origin',(111.548590144925,-3.75,48.1965658036136));
#198799=CARTESIAN_POINT('',(112.039403647474,-3.75,48.2919707600629));
#198800=CARTESIAN_POINT('',(111.982160673605,-3.75,48.5864588615926));
#198801=CARTESIAN_POINT('',(112.039403647474,-3.75,48.2919707600629));
#198802=CARTESIAN_POINT('',(111.491347171055,-3.75,48.4910539051433));
#198803=CARTESIAN_POINT('',(111.491347171055,-3.75,48.4910539051433));
#198804=CARTESIAN_POINT('',(111.548590144925,-3.75,48.1965658036136));
#198805=CARTESIAN_POINT('',(111.548590144925,-3.75,48.1965658036136));
#198806=CARTESIAN_POINT('',(111.548590144925,-3.75,48.1965658036136));
#198807=CARTESIAN_POINT('Origin',(112.039403647474,-3.75,48.2919707600629));
#198808=CARTESIAN_POINT('',(112.039403647474,-4.25,48.2919707600629));
#198809=CARTESIAN_POINT('',(111.982160673605,-4.25,48.5864588615926));
#198810=CARTESIAN_POINT('',(112.039403647474,-4.25,48.2919707600629));
#198811=CARTESIAN_POINT('',(111.982160673605,-3.75,48.5864588615926));
#198812=CARTESIAN_POINT('',(112.039403647474,-3.75,48.2919707600629));
#198813=CARTESIAN_POINT('Origin',(112.039403647474,-4.25,48.2919707600629));
#198814=CARTESIAN_POINT('',(111.548590144925,-4.25,48.1965658036136));
#198815=CARTESIAN_POINT('',(111.491347171055,-4.25,48.4910539051433));
#198816=CARTESIAN_POINT('',(111.548590144925,-4.25,48.1965658036136));
#198817=CARTESIAN_POINT('',(111.982160673605,-4.25,48.5864588615926));
#198818=CARTESIAN_POINT('',(112.039403647474,-4.25,48.2919707600629));
#198819=CARTESIAN_POINT('Origin',(111.548590144925,-4.25,48.1965658036136));
#198820=CARTESIAN_POINT('',(111.491347171055,-4.25,48.4910539051433));
#198821=CARTESIAN_POINT('',(111.548590144925,-4.25,48.1965658036136));
#198822=CARTESIAN_POINT('Origin',(111.548590144925,-4.55,48.1965658036136));
#198823=CARTESIAN_POINT('',(112.039403647474,-4.55,48.2919707600629));
#198824=CARTESIAN_POINT('',(111.982160673605,-4.55,48.5864588615926));
#198825=CARTESIAN_POINT('',(112.039403647474,-4.55,48.2919707600629));
#198826=CARTESIAN_POINT('',(111.491347171055,-4.55,48.4910539051433));
#198827=CARTESIAN_POINT('',(111.491347171055,-4.55,48.4910539051433));
#198828=CARTESIAN_POINT('',(111.548590144925,-4.55,48.1965658036136));
#198829=CARTESIAN_POINT('',(111.548590144925,-4.55,48.1965658036136));
#198830=CARTESIAN_POINT('',(111.548590144925,-4.55,48.1965658036136));
#198831=CARTESIAN_POINT('Origin',(112.039403647474,-4.55,48.2919707600629));
#198832=CARTESIAN_POINT('',(112.039403647474,-5.05,48.2919707600629));
#198833=CARTESIAN_POINT('',(111.982160673605,-5.05,48.5864588615926));
#198834=CARTESIAN_POINT('',(112.039403647474,-5.05,48.2919707600629));
#198835=CARTESIAN_POINT('',(111.982160673605,-4.55,48.5864588615926));
#198836=CARTESIAN_POINT('',(112.039403647474,-4.55,48.2919707600629));
#198837=CARTESIAN_POINT('Origin',(112.039403647474,-5.05,48.2919707600629));
#198838=CARTESIAN_POINT('',(111.548590144925,-5.05,48.1965658036136));
#198839=CARTESIAN_POINT('',(111.491347171055,-5.05,48.4910539051433));
#198840=CARTESIAN_POINT('',(111.548590144925,-5.05,48.1965658036136));
#198841=CARTESIAN_POINT('',(111.982160673605,-5.05,48.5864588615926));
#198842=CARTESIAN_POINT('',(112.039403647474,-5.05,48.2919707600629));
#198843=CARTESIAN_POINT('Origin',(111.548590144925,-5.05,48.1965658036136));
#198844=CARTESIAN_POINT('',(111.491347171055,-5.05,48.4910539051433));
#198845=CARTESIAN_POINT('',(111.548590144925,-5.05,48.1965658036136));
#198846=CARTESIAN_POINT('Origin',(111.548590144925,-5.35,48.1965658036136));
#198847=CARTESIAN_POINT('',(112.039403647474,-5.35,48.2919707600629));
#198848=CARTESIAN_POINT('',(111.982160673605,-5.35,48.5864588615926));
#198849=CARTESIAN_POINT('',(112.039403647474,-5.35,48.2919707600629));
#198850=CARTESIAN_POINT('',(111.491347171055,-5.35,48.4910539051433));
#198851=CARTESIAN_POINT('',(111.491347171055,-5.35,48.4910539051433));
#198852=CARTESIAN_POINT('',(111.548590144925,-5.35,48.1965658036136));
#198853=CARTESIAN_POINT('',(111.548590144925,-5.35,48.1965658036136));
#198854=CARTESIAN_POINT('',(111.548590144925,-5.35,48.1965658036136));
#198855=CARTESIAN_POINT('Origin',(112.039403647474,-5.35,48.2919707600629));
#198856=CARTESIAN_POINT('',(112.039403647474,-5.85,48.2919707600629));
#198857=CARTESIAN_POINT('',(111.982160673605,-5.85,48.5864588615926));
#198858=CARTESIAN_POINT('',(112.039403647474,-5.85,48.2919707600629));
#198859=CARTESIAN_POINT('',(111.982160673605,-5.35,48.5864588615926));
#198860=CARTESIAN_POINT('',(112.039403647474,-5.35,48.2919707600629));
#198861=CARTESIAN_POINT('Origin',(112.039403647474,-5.85,48.2919707600629));
#198862=CARTESIAN_POINT('',(111.548590144925,-5.85,48.1965658036136));
#198863=CARTESIAN_POINT('',(111.491347171055,-5.85,48.4910539051433));
#198864=CARTESIAN_POINT('',(111.548590144925,-5.85,48.1965658036136));
#198865=CARTESIAN_POINT('',(111.982160673605,-5.85,48.5864588615926));
#198866=CARTESIAN_POINT('',(112.039403647474,-5.85,48.2919707600629));
#198867=CARTESIAN_POINT('Origin',(111.548590144925,-5.85,48.1965658036136));
#198868=CARTESIAN_POINT('',(111.491347171055,-5.85,48.4910539051433));
#198869=CARTESIAN_POINT('',(111.548590144925,-5.85,48.1965658036136));
#198870=CARTESIAN_POINT('Origin',(112.333891749004,-5.35,48.3492137339324));
#198871=CARTESIAN_POINT('',(112.824705251554,-5.35,48.4446186903817));
#198872=CARTESIAN_POINT('',(112.767462277684,-5.35,48.7391067919114));
#198873=CARTESIAN_POINT('',(112.824705251554,-5.35,48.4446186903817));
#198874=CARTESIAN_POINT('',(112.276648775135,-5.35,48.6437018354621));
#198875=CARTESIAN_POINT('',(112.276648775135,-5.35,48.6437018354621));
#198876=CARTESIAN_POINT('',(112.333891749004,-5.35,48.3492137339324));
#198877=CARTESIAN_POINT('',(112.333891749004,-5.35,48.3492137339324));
#198878=CARTESIAN_POINT('',(112.333891749004,-5.35,48.3492137339324));
#198879=CARTESIAN_POINT('Origin',(112.824705251554,-5.35,48.4446186903817));
#198880=CARTESIAN_POINT('',(112.824705251554,-5.85,48.4446186903817));
#198881=CARTESIAN_POINT('',(112.767462277684,-5.85,48.7391067919114));
#198882=CARTESIAN_POINT('',(112.824705251554,-5.85,48.4446186903817));
#198883=CARTESIAN_POINT('',(112.767462277684,-5.35,48.7391067919114));
#198884=CARTESIAN_POINT('',(112.824705251554,-5.35,48.4446186903817));
#198885=CARTESIAN_POINT('Origin',(112.824705251554,-5.85,48.4446186903817));
#198886=CARTESIAN_POINT('',(112.333891749004,-5.85,48.3492137339324));
#198887=CARTESIAN_POINT('',(112.276648775135,-5.85,48.6437018354621));
#198888=CARTESIAN_POINT('',(112.333891749004,-5.85,48.3492137339324));
#198889=CARTESIAN_POINT('',(112.767462277684,-5.85,48.7391067919114));
#198890=CARTESIAN_POINT('',(112.824705251554,-5.85,48.4446186903817));
#198891=CARTESIAN_POINT('Origin',(112.333891749004,-5.85,48.3492137339324));
#198892=CARTESIAN_POINT('',(112.276648775135,-5.85,48.6437018354621));
#198893=CARTESIAN_POINT('',(112.333891749004,-5.85,48.3492137339324));
#198894=CARTESIAN_POINT('Origin',(113.119193353083,-5.35,48.5018616642512));
#198895=CARTESIAN_POINT('',(113.610006855633,-5.35,48.5972666207005));
#198896=CARTESIAN_POINT('',(113.552763881763,-5.35,48.8917547222302));
#198897=CARTESIAN_POINT('',(113.610006855633,-5.35,48.5972666207005));
#198898=CARTESIAN_POINT('',(113.061950379214,-5.35,48.7963497657809));
#198899=CARTESIAN_POINT('',(113.061950379214,-5.35,48.7963497657809));
#198900=CARTESIAN_POINT('',(113.119193353083,-5.35,48.5018616642512));
#198901=CARTESIAN_POINT('',(113.119193353083,-5.35,48.5018616642512));
#198902=CARTESIAN_POINT('',(113.119193353083,-5.35,48.5018616642512));
#198903=CARTESIAN_POINT('Origin',(113.610006855633,-5.35,48.5972666207005));
#198904=CARTESIAN_POINT('',(113.610006855633,-5.85,48.5972666207005));
#198905=CARTESIAN_POINT('',(113.552763881763,-5.85,48.8917547222302));
#198906=CARTESIAN_POINT('',(113.610006855633,-5.85,48.5972666207005));
#198907=CARTESIAN_POINT('',(113.552763881763,-5.35,48.8917547222302));
#198908=CARTESIAN_POINT('',(113.610006855633,-5.35,48.5972666207005));
#198909=CARTESIAN_POINT('Origin',(113.610006855633,-5.85,48.5972666207005));
#198910=CARTESIAN_POINT('',(113.119193353083,-5.85,48.5018616642512));
#198911=CARTESIAN_POINT('',(113.061950379214,-5.85,48.7963497657809));
#198912=CARTESIAN_POINT('',(113.119193353083,-5.85,48.5018616642512));
#198913=CARTESIAN_POINT('',(113.552763881763,-5.85,48.8917547222302));
#198914=CARTESIAN_POINT('',(113.610006855633,-5.85,48.5972666207005));
#198915=CARTESIAN_POINT('Origin',(113.119193353083,-5.85,48.5018616642512));
#198916=CARTESIAN_POINT('',(113.061950379214,-5.85,48.7963497657809));
#198917=CARTESIAN_POINT('',(113.119193353083,-5.85,48.5018616642512));
#198918=CARTESIAN_POINT('Origin',(113.904494957163,-5.35,48.65450959457));
#198919=CARTESIAN_POINT('',(114.395308459712,-5.35,48.7499145510193));
#198920=CARTESIAN_POINT('',(114.338065485842,-5.35,49.044402652549));
#198921=CARTESIAN_POINT('',(114.395308459712,-5.35,48.7499145510193));
#198922=CARTESIAN_POINT('',(113.847251983293,-5.35,48.9489976960997));
#198923=CARTESIAN_POINT('',(113.847251983293,-5.35,48.9489976960997));
#198924=CARTESIAN_POINT('',(113.904494957163,-5.35,48.65450959457));
#198925=CARTESIAN_POINT('',(113.904494957163,-5.35,48.65450959457));
#198926=CARTESIAN_POINT('',(113.904494957163,-5.35,48.65450959457));
#198927=CARTESIAN_POINT('Origin',(114.395308459712,-5.35,48.7499145510193));
#198928=CARTESIAN_POINT('',(114.395308459712,-5.85,48.7499145510193));
#198929=CARTESIAN_POINT('',(114.338065485842,-5.85,49.044402652549));
#198930=CARTESIAN_POINT('',(114.395308459712,-5.85,48.7499145510193));
#198931=CARTESIAN_POINT('',(114.338065485842,-5.35,49.044402652549));
#198932=CARTESIAN_POINT('',(114.395308459712,-5.35,48.7499145510193));
#198933=CARTESIAN_POINT('Origin',(114.395308459712,-5.85,48.7499145510193));
#198934=CARTESIAN_POINT('',(113.904494957163,-5.85,48.65450959457));
#198935=CARTESIAN_POINT('',(113.847251983293,-5.85,48.9489976960997));
#198936=CARTESIAN_POINT('',(113.904494957163,-5.85,48.65450959457));
#198937=CARTESIAN_POINT('',(114.338065485842,-5.85,49.044402652549));
#198938=CARTESIAN_POINT('',(114.395308459712,-5.85,48.7499145510193));
#198939=CARTESIAN_POINT('Origin',(113.904494957163,-5.85,48.65450959457));
#198940=CARTESIAN_POINT('',(113.847251983293,-5.85,48.9489976960997));
#198941=CARTESIAN_POINT('',(113.904494957163,-5.85,48.65450959457));
#198942=CARTESIAN_POINT('Origin',(114.689796561242,-5.35,48.8071575248888));
#198943=CARTESIAN_POINT('',(115.180610063791,-5.35,48.9025624813381));
#198944=CARTESIAN_POINT('',(115.123367089922,-5.35,49.1970505828678));
#198945=CARTESIAN_POINT('',(115.180610063791,-5.35,48.9025624813381));
#198946=CARTESIAN_POINT('',(114.632553587372,-5.35,49.1016456264185));
#198947=CARTESIAN_POINT('',(114.632553587372,-5.35,49.1016456264185));
#198948=CARTESIAN_POINT('',(114.689796561242,-5.35,48.8071575248888));
#198949=CARTESIAN_POINT('',(114.689796561242,-5.35,48.8071575248888));
#198950=CARTESIAN_POINT('',(114.689796561242,-5.35,48.8071575248888));
#198951=CARTESIAN_POINT('Origin',(115.180610063791,-5.35,48.9025624813381));
#198952=CARTESIAN_POINT('',(115.180610063791,-5.85,48.9025624813381));
#198953=CARTESIAN_POINT('',(115.123367089922,-5.85,49.1970505828678));
#198954=CARTESIAN_POINT('',(115.180610063791,-5.85,48.9025624813381));
#198955=CARTESIAN_POINT('',(115.123367089922,-5.35,49.1970505828678));
#198956=CARTESIAN_POINT('',(115.180610063791,-5.35,48.9025624813381));
#198957=CARTESIAN_POINT('Origin',(115.180610063791,-5.85,48.9025624813381));
#198958=CARTESIAN_POINT('',(114.689796561242,-5.85,48.8071575248888));
#198959=CARTESIAN_POINT('',(114.632553587372,-5.85,49.1016456264185));
#198960=CARTESIAN_POINT('',(114.689796561242,-5.85,48.8071575248888));
#198961=CARTESIAN_POINT('',(115.123367089922,-5.85,49.1970505828678));
#198962=CARTESIAN_POINT('',(115.180610063791,-5.85,48.9025624813381));
#198963=CARTESIAN_POINT('Origin',(114.689796561242,-5.85,48.8071575248888));
#198964=CARTESIAN_POINT('',(114.632553587372,-5.85,49.1016456264185));
#198965=CARTESIAN_POINT('',(114.689796561242,-5.85,48.8071575248888));
#198966=CARTESIAN_POINT('Origin',(115.475098165321,-5.35,48.9598054552076));
#198967=CARTESIAN_POINT('',(115.96591166787,-5.35,49.0552104116569));
#198968=CARTESIAN_POINT('',(115.908668694001,-5.35,49.3496985131866));
#198969=CARTESIAN_POINT('',(115.96591166787,-5.35,49.0552104116569));
#198970=CARTESIAN_POINT('',(115.417855191451,-5.35,49.2542935567373));
#198971=CARTESIAN_POINT('',(115.417855191451,-5.35,49.2542935567373));
#198972=CARTESIAN_POINT('',(115.475098165321,-5.35,48.9598054552076));
#198973=CARTESIAN_POINT('',(115.475098165321,-5.35,48.9598054552076));
#198974=CARTESIAN_POINT('',(115.475098165321,-5.35,48.9598054552076));
#198975=CARTESIAN_POINT('Origin',(115.96591166787,-5.35,49.0552104116569));
#198976=CARTESIAN_POINT('',(115.96591166787,-5.85,49.0552104116569));
#198977=CARTESIAN_POINT('',(115.908668694001,-5.85,49.3496985131866));
#198978=CARTESIAN_POINT('',(115.96591166787,-5.85,49.0552104116569));
#198979=CARTESIAN_POINT('',(115.908668694001,-5.35,49.3496985131866));
#198980=CARTESIAN_POINT('',(115.96591166787,-5.35,49.0552104116569));
#198981=CARTESIAN_POINT('Origin',(115.96591166787,-5.85,49.0552104116569));
#198982=CARTESIAN_POINT('',(115.475098165321,-5.85,48.9598054552076));
#198983=CARTESIAN_POINT('',(115.417855191451,-5.85,49.2542935567373));
#198984=CARTESIAN_POINT('',(115.475098165321,-5.85,48.9598054552076));
#198985=CARTESIAN_POINT('',(115.908668694001,-5.85,49.3496985131866));
#198986=CARTESIAN_POINT('',(115.96591166787,-5.85,49.0552104116569));
#198987=CARTESIAN_POINT('Origin',(115.475098165321,-5.85,48.9598054552076));
#198988=CARTESIAN_POINT('',(115.417855191451,-5.85,49.2542935567373));
#198989=CARTESIAN_POINT('',(115.475098165321,-5.85,48.9598054552076));
#198990=CARTESIAN_POINT('Origin',(116.2603997694,-5.35,49.1124533855264));
#198991=CARTESIAN_POINT('',(116.75121327195,-5.35,49.2078583419757));
#198992=CARTESIAN_POINT('',(116.69397029808,-5.35,49.5023464435054));
#198993=CARTESIAN_POINT('',(116.75121327195,-5.35,49.2078583419757));
#198994=CARTESIAN_POINT('',(116.203156795531,-5.35,49.4069414870561));
#198995=CARTESIAN_POINT('',(116.203156795531,-5.35,49.4069414870561));
#198996=CARTESIAN_POINT('',(116.2603997694,-5.35,49.1124533855264));
#198997=CARTESIAN_POINT('',(116.2603997694,-5.35,49.1124533855264));
#198998=CARTESIAN_POINT('',(116.2603997694,-5.35,49.1124533855264));
#198999=CARTESIAN_POINT('Origin',(116.75121327195,-5.35,49.2078583419757));
#199000=CARTESIAN_POINT('',(116.75121327195,-5.85,49.2078583419757));
#199001=CARTESIAN_POINT('',(116.69397029808,-5.85,49.5023464435054));
#199002=CARTESIAN_POINT('',(116.75121327195,-5.85,49.2078583419757));
#199003=CARTESIAN_POINT('',(116.69397029808,-5.35,49.5023464435054));
#199004=CARTESIAN_POINT('',(116.75121327195,-5.35,49.2078583419757));
#199005=CARTESIAN_POINT('Origin',(116.75121327195,-5.85,49.2078583419757));
#199006=CARTESIAN_POINT('',(116.2603997694,-5.85,49.1124533855264));
#199007=CARTESIAN_POINT('',(116.203156795531,-5.85,49.4069414870561));
#199008=CARTESIAN_POINT('',(116.2603997694,-5.85,49.1124533855264));
#199009=CARTESIAN_POINT('',(116.69397029808,-5.85,49.5023464435054));
#199010=CARTESIAN_POINT('',(116.75121327195,-5.85,49.2078583419757));
#199011=CARTESIAN_POINT('Origin',(116.2603997694,-5.85,49.1124533855264));
#199012=CARTESIAN_POINT('',(116.203156795531,-5.85,49.4069414870561));
#199013=CARTESIAN_POINT('',(116.2603997694,-5.85,49.1124533855264));
#199014=CARTESIAN_POINT('Origin',(117.045701373479,-5.35,49.2651013158452));
#199015=CARTESIAN_POINT('',(117.536514876029,-5.35,49.3605062722945));
#199016=CARTESIAN_POINT('',(117.479271902159,-5.35,49.6549943738242));
#199017=CARTESIAN_POINT('',(117.536514876029,-5.35,49.3605062722945));
#199018=CARTESIAN_POINT('',(116.98845839961,-5.35,49.5595894173749));
#199019=CARTESIAN_POINT('',(116.98845839961,-5.35,49.5595894173749));
#199020=CARTESIAN_POINT('',(117.045701373479,-5.35,49.2651013158452));
#199021=CARTESIAN_POINT('',(117.045701373479,-5.35,49.2651013158452));
#199022=CARTESIAN_POINT('',(117.045701373479,-5.35,49.2651013158452));
#199023=CARTESIAN_POINT('Origin',(117.536514876029,-5.35,49.3605062722945));
#199024=CARTESIAN_POINT('',(117.536514876029,-5.85,49.3605062722945));
#199025=CARTESIAN_POINT('',(117.479271902159,-5.85,49.6549943738242));
#199026=CARTESIAN_POINT('',(117.536514876029,-5.85,49.3605062722945));
#199027=CARTESIAN_POINT('',(117.479271902159,-5.35,49.6549943738242));
#199028=CARTESIAN_POINT('',(117.536514876029,-5.35,49.3605062722945));
#199029=CARTESIAN_POINT('Origin',(117.536514876029,-5.85,49.3605062722945));
#199030=CARTESIAN_POINT('',(117.045701373479,-5.85,49.2651013158452));
#199031=CARTESIAN_POINT('',(116.98845839961,-5.85,49.5595894173749));
#199032=CARTESIAN_POINT('',(117.045701373479,-5.85,49.2651013158452));
#199033=CARTESIAN_POINT('',(117.479271902159,-5.85,49.6549943738242));
#199034=CARTESIAN_POINT('',(117.536514876029,-5.85,49.3605062722945));
#199035=CARTESIAN_POINT('Origin',(117.045701373479,-5.85,49.2651013158452));
#199036=CARTESIAN_POINT('',(116.98845839961,-5.85,49.5595894173749));
#199037=CARTESIAN_POINT('',(117.045701373479,-5.85,49.2651013158452));
#199038=CARTESIAN_POINT('Origin',(117.831002977559,-5.35,49.417749246164));
#199039=CARTESIAN_POINT('',(118.321816480108,-5.35,49.5131542026133));
#199040=CARTESIAN_POINT('',(118.264573506239,-5.35,49.807642304143));
#199041=CARTESIAN_POINT('',(118.321816480108,-5.35,49.5131542026133));
#199042=CARTESIAN_POINT('',(117.773760003689,-5.35,49.7122373476937));
#199043=CARTESIAN_POINT('',(117.773760003689,-5.35,49.7122373476937));
#199044=CARTESIAN_POINT('',(117.831002977559,-5.35,49.417749246164));
#199045=CARTESIAN_POINT('',(117.831002977559,-5.35,49.417749246164));
#199046=CARTESIAN_POINT('',(117.831002977559,-5.35,49.417749246164));
#199047=CARTESIAN_POINT('Origin',(118.321816480108,-5.35,49.5131542026133));
#199048=CARTESIAN_POINT('',(118.321816480108,-5.85,49.5131542026133));
#199049=CARTESIAN_POINT('',(118.264573506239,-5.85,49.807642304143));
#199050=CARTESIAN_POINT('',(118.321816480108,-5.85,49.5131542026133));
#199051=CARTESIAN_POINT('',(118.264573506239,-5.35,49.807642304143));
#199052=CARTESIAN_POINT('',(118.321816480108,-5.35,49.5131542026133));
#199053=CARTESIAN_POINT('Origin',(118.321816480108,-5.85,49.5131542026133));
#199054=CARTESIAN_POINT('',(117.831002977559,-5.85,49.417749246164));
#199055=CARTESIAN_POINT('',(117.773760003689,-5.85,49.7122373476937));
#199056=CARTESIAN_POINT('',(117.831002977559,-5.85,49.417749246164));
#199057=CARTESIAN_POINT('',(118.264573506239,-5.85,49.807642304143));
#199058=CARTESIAN_POINT('',(118.321816480108,-5.85,49.5131542026133));
#199059=CARTESIAN_POINT('Origin',(117.831002977559,-5.85,49.417749246164));
#199060=CARTESIAN_POINT('',(117.773760003689,-5.85,49.7122373476937));
#199061=CARTESIAN_POINT('',(117.831002977559,-5.85,49.417749246164));
#199062=CARTESIAN_POINT('Origin',(118.616304581638,-5.35,49.5703971764828));
#199063=CARTESIAN_POINT('',(119.107118084187,-5.35,49.6658021329321));
#199064=CARTESIAN_POINT('',(119.049875110318,-5.35,49.9602902344618));
#199065=CARTESIAN_POINT('',(119.107118084187,-5.35,49.6658021329321));
#199066=CARTESIAN_POINT('',(118.559061607768,-5.35,49.8648852780125));
#199067=CARTESIAN_POINT('',(118.559061607768,-5.35,49.8648852780125));
#199068=CARTESIAN_POINT('',(118.616304581638,-5.35,49.5703971764828));
#199069=CARTESIAN_POINT('',(118.616304581638,-5.35,49.5703971764828));
#199070=CARTESIAN_POINT('',(118.616304581638,-5.35,49.5703971764828));
#199071=CARTESIAN_POINT('Origin',(119.107118084187,-5.35,49.6658021329321));
#199072=CARTESIAN_POINT('',(119.107118084187,-5.85,49.6658021329321));
#199073=CARTESIAN_POINT('',(119.049875110318,-5.85,49.9602902344618));
#199074=CARTESIAN_POINT('',(119.107118084187,-5.85,49.6658021329321));
#199075=CARTESIAN_POINT('',(119.049875110318,-5.35,49.9602902344618));
#199076=CARTESIAN_POINT('',(119.107118084187,-5.35,49.6658021329321));
#199077=CARTESIAN_POINT('Origin',(119.107118084187,-5.85,49.6658021329321));
#199078=CARTESIAN_POINT('',(118.616304581638,-5.85,49.5703971764828));
#199079=CARTESIAN_POINT('',(118.559061607768,-5.85,49.8648852780125));
#199080=CARTESIAN_POINT('',(118.616304581638,-5.85,49.5703971764828));
#199081=CARTESIAN_POINT('',(119.049875110318,-5.85,49.9602902344618));
#199082=CARTESIAN_POINT('',(119.107118084187,-5.85,49.6658021329321));
#199083=CARTESIAN_POINT('Origin',(118.616304581638,-5.85,49.5703971764828));
#199084=CARTESIAN_POINT('',(118.559061607768,-5.85,49.8648852780125));
#199085=CARTESIAN_POINT('',(118.616304581638,-5.85,49.5703971764828));
#199086=CARTESIAN_POINT('Origin',(119.401606185717,-5.35,49.7230451068016));
#199087=CARTESIAN_POINT('',(119.892419688267,-5.35,49.8184500632509));
#199088=CARTESIAN_POINT('',(119.835176714397,-5.35,50.1129381647806));
#199089=CARTESIAN_POINT('',(119.892419688267,-5.35,49.8184500632509));
#199090=CARTESIAN_POINT('',(119.344363211847,-5.35,50.0175332083313));
#199091=CARTESIAN_POINT('',(119.344363211847,-5.35,50.0175332083313));
#199092=CARTESIAN_POINT('',(119.401606185717,-5.35,49.7230451068016));
#199093=CARTESIAN_POINT('',(119.401606185717,-5.35,49.7230451068016));
#199094=CARTESIAN_POINT('',(119.401606185717,-5.35,49.7230451068016));
#199095=CARTESIAN_POINT('Origin',(119.892419688267,-5.35,49.8184500632509));
#199096=CARTESIAN_POINT('',(119.892419688267,-5.85,49.8184500632509));
#199097=CARTESIAN_POINT('',(119.835176714397,-5.85,50.1129381647806));
#199098=CARTESIAN_POINT('',(119.892419688267,-5.85,49.8184500632509));
#199099=CARTESIAN_POINT('',(119.835176714397,-5.35,50.1129381647806));
#199100=CARTESIAN_POINT('',(119.892419688267,-5.35,49.8184500632509));
#199101=CARTESIAN_POINT('Origin',(119.892419688267,-5.85,49.8184500632509));
#199102=CARTESIAN_POINT('',(119.401606185717,-5.85,49.7230451068016));
#199103=CARTESIAN_POINT('',(119.344363211847,-5.85,50.0175332083313));
#199104=CARTESIAN_POINT('',(119.401606185717,-5.85,49.7230451068016));
#199105=CARTESIAN_POINT('',(119.835176714397,-5.85,50.1129381647806));
#199106=CARTESIAN_POINT('',(119.892419688267,-5.85,49.8184500632509));
#199107=CARTESIAN_POINT('Origin',(119.401606185717,-5.85,49.7230451068016));
#199108=CARTESIAN_POINT('',(119.344363211847,-5.85,50.0175332083313));
#199109=CARTESIAN_POINT('',(119.401606185717,-5.85,49.7230451068016));
#199110=CARTESIAN_POINT('Origin',(120.186907789796,-5.35,49.8756930371204));
#199111=CARTESIAN_POINT('',(120.677721292346,-5.35,49.9710979935697));
#199112=CARTESIAN_POINT('',(120.620478318476,-5.35,50.2655860950994));
#199113=CARTESIAN_POINT('',(120.677721292346,-5.35,49.9710979935697));
#199114=CARTESIAN_POINT('',(120.129664815927,-5.35,50.1701811386501));
#199115=CARTESIAN_POINT('',(120.129664815927,-5.35,50.1701811386501));
#199116=CARTESIAN_POINT('',(120.186907789796,-5.35,49.8756930371204));
#199117=CARTESIAN_POINT('',(120.186907789796,-5.35,49.8756930371204));
#199118=CARTESIAN_POINT('',(120.186907789796,-5.35,49.8756930371204));
#199119=CARTESIAN_POINT('Origin',(120.677721292346,-5.35,49.9710979935697));
#199120=CARTESIAN_POINT('',(120.677721292346,-5.85,49.9710979935697));
#199121=CARTESIAN_POINT('',(120.620478318476,-5.85,50.2655860950994));
#199122=CARTESIAN_POINT('',(120.677721292346,-5.85,49.9710979935697));
#199123=CARTESIAN_POINT('',(120.620478318476,-5.35,50.2655860950994));
#199124=CARTESIAN_POINT('',(120.677721292346,-5.35,49.9710979935697));
#199125=CARTESIAN_POINT('Origin',(120.677721292346,-5.85,49.9710979935697));
#199126=CARTESIAN_POINT('',(120.186907789796,-5.85,49.8756930371204));
#199127=CARTESIAN_POINT('',(120.129664815927,-5.85,50.1701811386501));
#199128=CARTESIAN_POINT('',(120.186907789796,-5.85,49.8756930371204));
#199129=CARTESIAN_POINT('',(120.620478318476,-5.85,50.2655860950994));
#199130=CARTESIAN_POINT('',(120.677721292346,-5.85,49.9710979935697));
#199131=CARTESIAN_POINT('Origin',(120.186907789796,-5.85,49.8756930371204));
#199132=CARTESIAN_POINT('',(120.129664815927,-5.85,50.1701811386501));
#199133=CARTESIAN_POINT('',(120.186907789796,-5.85,49.8756930371204));
#199134=CARTESIAN_POINT('Origin',(120.972209393875,-5.35,50.0283409674392));
#199135=CARTESIAN_POINT('',(121.463022896425,-5.35,50.1237459238885));
#199136=CARTESIAN_POINT('',(121.405779922555,-5.35,50.4182340254182));
#199137=CARTESIAN_POINT('',(121.463022896425,-5.35,50.1237459238885));
#199138=CARTESIAN_POINT('',(120.914966420006,-5.35,50.3228290689689));
#199139=CARTESIAN_POINT('',(120.914966420006,-5.35,50.3228290689689));
#199140=CARTESIAN_POINT('',(120.972209393875,-5.35,50.0283409674392));
#199141=CARTESIAN_POINT('',(120.972209393875,-5.35,50.0283409674392));
#199142=CARTESIAN_POINT('',(120.972209393875,-5.35,50.0283409674392));
#199143=CARTESIAN_POINT('Origin',(121.463022896425,-5.35,50.1237459238885));
#199144=CARTESIAN_POINT('',(121.463022896425,-5.85,50.1237459238885));
#199145=CARTESIAN_POINT('',(121.405779922555,-5.85,50.4182340254182));
#199146=CARTESIAN_POINT('',(121.463022896425,-5.85,50.1237459238885));
#199147=CARTESIAN_POINT('',(121.405779922555,-5.35,50.4182340254182));
#199148=CARTESIAN_POINT('',(121.463022896425,-5.35,50.1237459238885));
#199149=CARTESIAN_POINT('Origin',(121.463022896425,-5.85,50.1237459238885));
#199150=CARTESIAN_POINT('',(120.972209393875,-5.85,50.0283409674392));
#199151=CARTESIAN_POINT('',(120.914966420006,-5.85,50.3228290689689));
#199152=CARTESIAN_POINT('',(120.972209393875,-5.85,50.0283409674392));
#199153=CARTESIAN_POINT('',(121.405779922555,-5.85,50.4182340254182));
#199154=CARTESIAN_POINT('',(121.463022896425,-5.85,50.1237459238885));
#199155=CARTESIAN_POINT('Origin',(120.972209393875,-5.85,50.0283409674392));
#199156=CARTESIAN_POINT('',(120.914966420006,-5.85,50.3228290689689));
#199157=CARTESIAN_POINT('',(120.972209393875,-5.85,50.0283409674392));
#199158=CARTESIAN_POINT('Origin',(121.757510997955,-5.35,50.180988897758));
#199159=CARTESIAN_POINT('',(122.248324500504,-5.35,50.2763938542073));
#199160=CARTESIAN_POINT('',(122.191081526635,-5.35,50.570881955737));
#199161=CARTESIAN_POINT('',(122.248324500504,-5.35,50.2763938542073));
#199162=CARTESIAN_POINT('',(121.700268024085,-5.35,50.4754769992877));
#199163=CARTESIAN_POINT('',(121.700268024085,-5.35,50.4754769992877));
#199164=CARTESIAN_POINT('',(121.757510997955,-5.35,50.180988897758));
#199165=CARTESIAN_POINT('',(121.757510997955,-5.35,50.180988897758));
#199166=CARTESIAN_POINT('',(121.757510997955,-5.35,50.180988897758));
#199167=CARTESIAN_POINT('Origin',(122.248324500504,-5.35,50.2763938542073));
#199168=CARTESIAN_POINT('',(122.248324500504,-5.85,50.2763938542073));
#199169=CARTESIAN_POINT('',(122.191081526635,-5.85,50.570881955737));
#199170=CARTESIAN_POINT('',(122.248324500504,-5.85,50.2763938542073));
#199171=CARTESIAN_POINT('',(122.191081526635,-5.35,50.570881955737));
#199172=CARTESIAN_POINT('',(122.248324500504,-5.35,50.2763938542073));
#199173=CARTESIAN_POINT('Origin',(122.248324500504,-5.85,50.2763938542073));
#199174=CARTESIAN_POINT('',(121.757510997955,-5.85,50.180988897758));
#199175=CARTESIAN_POINT('',(121.700268024085,-5.85,50.4754769992877));
#199176=CARTESIAN_POINT('',(121.757510997955,-5.85,50.180988897758));
#199177=CARTESIAN_POINT('',(122.191081526635,-5.85,50.570881955737));
#199178=CARTESIAN_POINT('',(122.248324500504,-5.85,50.2763938542073));
#199179=CARTESIAN_POINT('Origin',(121.757510997955,-5.85,50.180988897758));
#199180=CARTESIAN_POINT('',(121.700268024085,-5.85,50.4754769992877));
#199181=CARTESIAN_POINT('',(121.757510997955,-5.85,50.180988897758));
#199182=CARTESIAN_POINT('Origin',(122.542812602034,-5.35,50.3336368280768));
#199183=CARTESIAN_POINT('',(123.033626104583,-5.35,50.4290417845261));
#199184=CARTESIAN_POINT('',(122.976383130714,-5.35,50.7235298860558));
#199185=CARTESIAN_POINT('',(123.033626104583,-5.35,50.4290417845261));
#199186=CARTESIAN_POINT('',(122.485569628164,-5.35,50.6281249296065));
#199187=CARTESIAN_POINT('',(122.485569628164,-5.35,50.6281249296065));
#199188=CARTESIAN_POINT('',(122.542812602034,-5.35,50.3336368280768));
#199189=CARTESIAN_POINT('',(122.542812602034,-5.35,50.3336368280768));
#199190=CARTESIAN_POINT('',(122.542812602034,-5.35,50.3336368280768));
#199191=CARTESIAN_POINT('Origin',(123.033626104583,-5.35,50.4290417845261));
#199192=CARTESIAN_POINT('',(123.033626104583,-5.85,50.4290417845261));
#199193=CARTESIAN_POINT('',(122.976383130714,-5.85,50.7235298860558));
#199194=CARTESIAN_POINT('',(123.033626104583,-5.85,50.4290417845261));
#199195=CARTESIAN_POINT('',(122.976383130714,-5.35,50.7235298860558));
#199196=CARTESIAN_POINT('',(123.033626104583,-5.35,50.4290417845261));
#199197=CARTESIAN_POINT('Origin',(123.033626104583,-5.85,50.4290417845261));
#199198=CARTESIAN_POINT('',(122.542812602034,-5.85,50.3336368280768));
#199199=CARTESIAN_POINT('',(122.485569628164,-5.85,50.6281249296065));
#199200=CARTESIAN_POINT('',(122.542812602034,-5.85,50.3336368280768));
#199201=CARTESIAN_POINT('',(122.976383130714,-5.85,50.7235298860558));
#199202=CARTESIAN_POINT('',(123.033626104583,-5.85,50.4290417845261));
#199203=CARTESIAN_POINT('Origin',(122.542812602034,-5.85,50.3336368280768));
#199204=CARTESIAN_POINT('',(122.485569628164,-5.85,50.6281249296065));
#199205=CARTESIAN_POINT('',(122.542812602034,-5.85,50.3336368280768));
#199206=CARTESIAN_POINT('Origin',(122.542812602034,-4.55,50.3336368280768));
#199207=CARTESIAN_POINT('',(123.033626104583,-4.55,50.4290417845261));
#199208=CARTESIAN_POINT('',(122.976383130714,-4.55,50.7235298860558));
#199209=CARTESIAN_POINT('',(123.033626104583,-4.55,50.4290417845261));
#199210=CARTESIAN_POINT('',(122.485569628164,-4.55,50.6281249296065));
#199211=CARTESIAN_POINT('',(122.485569628164,-4.55,50.6281249296065));
#199212=CARTESIAN_POINT('',(122.542812602034,-4.55,50.3336368280768));
#199213=CARTESIAN_POINT('',(122.542812602034,-4.55,50.3336368280768));
#199214=CARTESIAN_POINT('',(122.542812602034,-4.55,50.3336368280768));
#199215=CARTESIAN_POINT('Origin',(123.033626104583,-4.55,50.4290417845261));
#199216=CARTESIAN_POINT('',(123.033626104583,-5.05,50.4290417845261));
#199217=CARTESIAN_POINT('',(122.976383130714,-5.05,50.7235298860558));
#199218=CARTESIAN_POINT('',(123.033626104583,-5.05,50.4290417845261));
#199219=CARTESIAN_POINT('',(122.976383130714,-4.55,50.7235298860558));
#199220=CARTESIAN_POINT('',(123.033626104583,-4.55,50.4290417845261));
#199221=CARTESIAN_POINT('Origin',(123.033626104583,-5.05,50.4290417845261));
#199222=CARTESIAN_POINT('',(122.542812602034,-5.05,50.3336368280768));
#199223=CARTESIAN_POINT('',(122.485569628164,-5.05,50.6281249296065));
#199224=CARTESIAN_POINT('',(122.542812602034,-5.05,50.3336368280768));
#199225=CARTESIAN_POINT('',(122.976383130714,-5.05,50.7235298860558));
#199226=CARTESIAN_POINT('',(123.033626104583,-5.05,50.4290417845261));
#199227=CARTESIAN_POINT('Origin',(122.542812602034,-5.05,50.3336368280768));
#199228=CARTESIAN_POINT('',(122.485569628164,-5.05,50.6281249296065));
#199229=CARTESIAN_POINT('',(122.542812602034,-5.05,50.3336368280768));
#199230=CARTESIAN_POINT('Origin',(122.542812602034,-3.75,50.3336368280768));
#199231=CARTESIAN_POINT('',(123.033626104583,-3.75,50.4290417845261));
#199232=CARTESIAN_POINT('',(122.976383130714,-3.75,50.7235298860558));
#199233=CARTESIAN_POINT('',(123.033626104583,-3.75,50.4290417845261));
#199234=CARTESIAN_POINT('',(122.485569628164,-3.75,50.6281249296065));
#199235=CARTESIAN_POINT('',(122.485569628164,-3.75,50.6281249296065));
#199236=CARTESIAN_POINT('',(122.542812602034,-3.75,50.3336368280768));
#199237=CARTESIAN_POINT('',(122.542812602034,-3.75,50.3336368280768));
#199238=CARTESIAN_POINT('',(122.542812602034,-3.75,50.3336368280768));
#199239=CARTESIAN_POINT('Origin',(123.033626104583,-3.75,50.4290417845261));
#199240=CARTESIAN_POINT('',(123.033626104583,-4.25,50.4290417845261));
#199241=CARTESIAN_POINT('',(122.976383130714,-4.25,50.7235298860558));
#199242=CARTESIAN_POINT('',(123.033626104583,-4.25,50.4290417845261));
#199243=CARTESIAN_POINT('',(122.976383130714,-3.75,50.7235298860558));
#199244=CARTESIAN_POINT('',(123.033626104583,-3.75,50.4290417845261));
#199245=CARTESIAN_POINT('Origin',(123.033626104583,-4.25,50.4290417845261));
#199246=CARTESIAN_POINT('',(122.542812602034,-4.25,50.3336368280768));
#199247=CARTESIAN_POINT('',(122.485569628164,-4.25,50.6281249296065));
#199248=CARTESIAN_POINT('',(122.542812602034,-4.25,50.3336368280768));
#199249=CARTESIAN_POINT('',(122.976383130714,-4.25,50.7235298860558));
#199250=CARTESIAN_POINT('',(123.033626104583,-4.25,50.4290417845261));
#199251=CARTESIAN_POINT('Origin',(122.542812602034,-4.25,50.3336368280768));
#199252=CARTESIAN_POINT('',(122.485569628164,-4.25,50.6281249296065));
#199253=CARTESIAN_POINT('',(122.542812602034,-4.25,50.3336368280768));
#199254=CARTESIAN_POINT('Origin',(122.542812602034,-2.95,50.3336368280768));
#199255=CARTESIAN_POINT('',(123.033626104583,-2.95,50.4290417845261));
#199256=CARTESIAN_POINT('',(122.976383130714,-2.95,50.7235298860558));
#199257=CARTESIAN_POINT('',(123.033626104583,-2.95,50.4290417845261));
#199258=CARTESIAN_POINT('',(122.485569628164,-2.95,50.6281249296065));
#199259=CARTESIAN_POINT('',(122.485569628164,-2.95,50.6281249296065));
#199260=CARTESIAN_POINT('',(122.542812602034,-2.95,50.3336368280768));
#199261=CARTESIAN_POINT('',(122.542812602034,-2.95,50.3336368280768));
#199262=CARTESIAN_POINT('',(122.542812602034,-2.95,50.3336368280768));
#199263=CARTESIAN_POINT('Origin',(123.033626104583,-2.95,50.4290417845261));
#199264=CARTESIAN_POINT('',(123.033626104583,-3.45,50.4290417845261));
#199265=CARTESIAN_POINT('',(122.976383130714,-3.45,50.7235298860558));
#199266=CARTESIAN_POINT('',(123.033626104583,-3.45,50.4290417845261));
#199267=CARTESIAN_POINT('',(122.976383130714,-2.95,50.7235298860558));
#199268=CARTESIAN_POINT('',(123.033626104583,-2.95,50.4290417845261));
#199269=CARTESIAN_POINT('Origin',(123.033626104583,-3.45,50.4290417845261));
#199270=CARTESIAN_POINT('',(122.542812602034,-3.45,50.3336368280768));
#199271=CARTESIAN_POINT('',(122.485569628164,-3.45,50.6281249296065));
#199272=CARTESIAN_POINT('',(122.542812602034,-3.45,50.3336368280768));
#199273=CARTESIAN_POINT('',(122.976383130714,-3.45,50.7235298860558));
#199274=CARTESIAN_POINT('',(123.033626104583,-3.45,50.4290417845261));
#199275=CARTESIAN_POINT('Origin',(122.542812602034,-3.45,50.3336368280768));
#199276=CARTESIAN_POINT('',(122.485569628164,-3.45,50.6281249296065));
#199277=CARTESIAN_POINT('',(122.542812602034,-3.45,50.3336368280768));
#199278=CARTESIAN_POINT('Origin',(122.542812602034,-2.15,50.3336368280768));
#199279=CARTESIAN_POINT('',(123.033626104583,-2.15,50.4290417845261));
#199280=CARTESIAN_POINT('',(122.976383130714,-2.15,50.7235298860558));
#199281=CARTESIAN_POINT('',(123.033626104583,-2.15,50.4290417845261));
#199282=CARTESIAN_POINT('',(122.485569628164,-2.15,50.6281249296065));
#199283=CARTESIAN_POINT('',(122.485569628164,-2.15,50.6281249296065));
#199284=CARTESIAN_POINT('',(122.542812602034,-2.15,50.3336368280768));
#199285=CARTESIAN_POINT('',(122.542812602034,-2.15,50.3336368280768));
#199286=CARTESIAN_POINT('',(122.542812602034,-2.15,50.3336368280768));
#199287=CARTESIAN_POINT('Origin',(123.033626104583,-2.15,50.4290417845261));
#199288=CARTESIAN_POINT('',(123.033626104583,-2.65,50.4290417845261));
#199289=CARTESIAN_POINT('',(122.976383130714,-2.65,50.7235298860558));
#199290=CARTESIAN_POINT('',(123.033626104583,-2.65,50.4290417845261));
#199291=CARTESIAN_POINT('',(122.976383130714,-2.15,50.7235298860558));
#199292=CARTESIAN_POINT('',(123.033626104583,-2.15,50.4290417845261));
#199293=CARTESIAN_POINT('Origin',(123.033626104583,-2.65,50.4290417845261));
#199294=CARTESIAN_POINT('',(122.542812602034,-2.65,50.3336368280768));
#199295=CARTESIAN_POINT('',(122.485569628164,-2.65,50.6281249296065));
#199296=CARTESIAN_POINT('',(122.542812602034,-2.65,50.3336368280768));
#199297=CARTESIAN_POINT('',(122.976383130714,-2.65,50.7235298860558));
#199298=CARTESIAN_POINT('',(123.033626104583,-2.65,50.4290417845261));
#199299=CARTESIAN_POINT('Origin',(122.542812602034,-2.65,50.3336368280768));
#199300=CARTESIAN_POINT('',(122.485569628164,-2.65,50.6281249296065));
#199301=CARTESIAN_POINT('',(122.542812602034,-2.65,50.3336368280768));
#199302=CARTESIAN_POINT('Origin',(122.542812602034,-1.35,50.3336368280768));
#199303=CARTESIAN_POINT('',(123.033626104583,-1.35,50.4290417845261));
#199304=CARTESIAN_POINT('',(122.976383130714,-1.35,50.7235298860558));
#199305=CARTESIAN_POINT('',(123.033626104583,-1.35,50.4290417845261));
#199306=CARTESIAN_POINT('',(122.485569628164,-1.35,50.6281249296065));
#199307=CARTESIAN_POINT('',(122.485569628164,-1.35,50.6281249296065));
#199308=CARTESIAN_POINT('',(122.542812602034,-1.35,50.3336368280768));
#199309=CARTESIAN_POINT('',(122.542812602034,-1.35,50.3336368280768));
#199310=CARTESIAN_POINT('',(122.542812602034,-1.35,50.3336368280768));
#199311=CARTESIAN_POINT('Origin',(123.033626104583,-1.35,50.4290417845261));
#199312=CARTESIAN_POINT('',(123.033626104583,-1.85,50.4290417845261));
#199313=CARTESIAN_POINT('',(122.976383130714,-1.85,50.7235298860558));
#199314=CARTESIAN_POINT('',(123.033626104583,-1.85,50.4290417845261));
#199315=CARTESIAN_POINT('',(122.976383130714,-1.35,50.7235298860558));
#199316=CARTESIAN_POINT('',(123.033626104583,-1.35,50.4290417845261));
#199317=CARTESIAN_POINT('Origin',(123.033626104583,-1.85,50.4290417845261));
#199318=CARTESIAN_POINT('',(122.542812602034,-1.85,50.3336368280768));
#199319=CARTESIAN_POINT('',(122.485569628164,-1.85,50.6281249296065));
#199320=CARTESIAN_POINT('',(122.542812602034,-1.85,50.3336368280768));
#199321=CARTESIAN_POINT('',(122.976383130714,-1.85,50.7235298860558));
#199322=CARTESIAN_POINT('',(123.033626104583,-1.85,50.4290417845261));
#199323=CARTESIAN_POINT('Origin',(122.542812602034,-1.85,50.3336368280768));
#199324=CARTESIAN_POINT('',(122.485569628164,-1.85,50.6281249296065));
#199325=CARTESIAN_POINT('',(122.542812602034,-1.85,50.3336368280768));
#199326=CARTESIAN_POINT('Origin',(122.542812602034,-0.549999999999986,50.3336368280768));
#199327=CARTESIAN_POINT('',(123.033626104583,-0.549999999999986,50.4290417845261));
#199328=CARTESIAN_POINT('',(122.976383130714,-0.549999999999986,50.7235298860558));
#199329=CARTESIAN_POINT('',(123.033626104583,-0.549999999999986,50.4290417845261));
#199330=CARTESIAN_POINT('',(122.485569628164,-0.549999999999986,50.6281249296065));
#199331=CARTESIAN_POINT('',(122.485569628164,-0.549999999999986,50.6281249296065));
#199332=CARTESIAN_POINT('',(122.542812602034,-0.549999999999986,50.3336368280768));
#199333=CARTESIAN_POINT('',(122.542812602034,-0.549999999999986,50.3336368280768));
#199334=CARTESIAN_POINT('',(122.542812602034,-0.549999999999986,50.3336368280768));
#199335=CARTESIAN_POINT('Origin',(123.033626104583,-0.549999999999986,50.4290417845261));
#199336=CARTESIAN_POINT('',(123.033626104583,-1.05,50.4290417845261));
#199337=CARTESIAN_POINT('',(122.976383130714,-1.05,50.7235298860558));
#199338=CARTESIAN_POINT('',(123.033626104583,-1.05,50.4290417845261));
#199339=CARTESIAN_POINT('',(122.976383130714,-0.549999999999986,50.7235298860558));
#199340=CARTESIAN_POINT('',(123.033626104583,-0.549999999999986,50.4290417845261));
#199341=CARTESIAN_POINT('Origin',(123.033626104583,-1.05,50.4290417845261));
#199342=CARTESIAN_POINT('',(122.542812602034,-1.05,50.3336368280768));
#199343=CARTESIAN_POINT('',(122.485569628164,-1.05,50.6281249296065));
#199344=CARTESIAN_POINT('',(122.542812602034,-1.05,50.3336368280768));
#199345=CARTESIAN_POINT('',(122.976383130714,-1.05,50.7235298860558));
#199346=CARTESIAN_POINT('',(123.033626104583,-1.05,50.4290417845261));
#199347=CARTESIAN_POINT('Origin',(122.542812602034,-1.05,50.3336368280768));
#199348=CARTESIAN_POINT('',(122.485569628164,-1.05,50.6281249296065));
#199349=CARTESIAN_POINT('',(122.542812602034,-1.05,50.3336368280768));
#199350=CARTESIAN_POINT('Origin',(122.542812602034,0.250000000000015,50.3336368280768));
#199351=CARTESIAN_POINT('',(123.033626104583,0.250000000000015,50.4290417845261));
#199352=CARTESIAN_POINT('',(122.976383130714,0.250000000000015,50.7235298860558));
#199353=CARTESIAN_POINT('',(123.033626104583,0.250000000000015,50.4290417845261));
#199354=CARTESIAN_POINT('',(122.485569628164,0.250000000000015,50.6281249296065));
#199355=CARTESIAN_POINT('',(122.485569628164,0.250000000000015,50.6281249296065));
#199356=CARTESIAN_POINT('',(122.542812602034,0.250000000000015,50.3336368280768));
#199357=CARTESIAN_POINT('',(122.542812602034,0.250000000000015,50.3336368280768));
#199358=CARTESIAN_POINT('',(122.542812602034,0.250000000000015,50.3336368280768));
#199359=CARTESIAN_POINT('Origin',(123.033626104583,0.250000000000015,50.4290417845261));
#199360=CARTESIAN_POINT('',(123.033626104583,-0.249999999999985,50.4290417845261));
#199361=CARTESIAN_POINT('',(122.976383130714,-0.249999999999985,50.7235298860558));
#199362=CARTESIAN_POINT('',(123.033626104583,-0.249999999999985,50.4290417845261));
#199363=CARTESIAN_POINT('',(122.976383130714,0.250000000000015,50.7235298860558));
#199364=CARTESIAN_POINT('',(123.033626104583,0.250000000000015,50.4290417845261));
#199365=CARTESIAN_POINT('Origin',(123.033626104583,-0.249999999999985,50.4290417845261));
#199366=CARTESIAN_POINT('',(122.542812602034,-0.249999999999985,50.3336368280768));
#199367=CARTESIAN_POINT('',(122.485569628164,-0.249999999999985,50.6281249296065));
#199368=CARTESIAN_POINT('',(122.542812602034,-0.249999999999985,50.3336368280768));
#199369=CARTESIAN_POINT('',(122.976383130714,-0.249999999999985,50.7235298860558));
#199370=CARTESIAN_POINT('',(123.033626104583,-0.249999999999985,50.4290417845261));
#199371=CARTESIAN_POINT('Origin',(122.542812602034,-0.249999999999985,50.3336368280768));
#199372=CARTESIAN_POINT('',(122.485569628164,-0.249999999999985,50.6281249296065));
#199373=CARTESIAN_POINT('',(122.542812602034,-0.249999999999985,50.3336368280768));
#199374=CARTESIAN_POINT('Origin',(122.542812602034,1.05,50.3336368280768));
#199375=CARTESIAN_POINT('',(123.033626104583,1.05,50.4290417845261));
#199376=CARTESIAN_POINT('',(122.976383130714,1.05,50.7235298860558));
#199377=CARTESIAN_POINT('',(123.033626104583,1.05,50.4290417845261));
#199378=CARTESIAN_POINT('',(122.485569628164,1.05,50.6281249296065));
#199379=CARTESIAN_POINT('',(122.485569628164,1.05,50.6281249296065));
#199380=CARTESIAN_POINT('',(122.542812602034,1.05,50.3336368280768));
#199381=CARTESIAN_POINT('',(122.542812602034,1.05,50.3336368280768));
#199382=CARTESIAN_POINT('',(122.542812602034,1.05,50.3336368280768));
#199383=CARTESIAN_POINT('Origin',(123.033626104583,1.05,50.4290417845261));
#199384=CARTESIAN_POINT('',(123.033626104583,0.550000000000015,50.4290417845261));
#199385=CARTESIAN_POINT('',(122.976383130714,0.550000000000015,50.7235298860558));
#199386=CARTESIAN_POINT('',(123.033626104583,0.550000000000015,50.4290417845261));
#199387=CARTESIAN_POINT('',(122.976383130714,1.05,50.7235298860558));
#199388=CARTESIAN_POINT('',(123.033626104583,1.05,50.4290417845261));
#199389=CARTESIAN_POINT('Origin',(123.033626104583,0.550000000000015,50.4290417845261));
#199390=CARTESIAN_POINT('',(122.542812602034,0.550000000000015,50.3336368280768));
#199391=CARTESIAN_POINT('',(122.485569628164,0.550000000000015,50.6281249296065));
#199392=CARTESIAN_POINT('',(122.542812602034,0.550000000000015,50.3336368280768));
#199393=CARTESIAN_POINT('',(122.976383130714,0.550000000000015,50.7235298860558));
#199394=CARTESIAN_POINT('',(123.033626104583,0.550000000000015,50.4290417845261));
#199395=CARTESIAN_POINT('Origin',(122.542812602034,0.550000000000015,50.3336368280768));
#199396=CARTESIAN_POINT('',(122.485569628164,0.550000000000015,50.6281249296065));
#199397=CARTESIAN_POINT('',(122.542812602034,0.550000000000015,50.3336368280768));
#199398=CARTESIAN_POINT('Origin',(122.542812602034,1.85,50.3336368280768));
#199399=CARTESIAN_POINT('',(123.033626104583,1.85,50.4290417845261));
#199400=CARTESIAN_POINT('',(122.976383130714,1.85,50.7235298860558));
#199401=CARTESIAN_POINT('',(123.033626104583,1.85,50.4290417845261));
#199402=CARTESIAN_POINT('',(122.485569628164,1.85,50.6281249296065));
#199403=CARTESIAN_POINT('',(122.485569628164,1.85,50.6281249296065));
#199404=CARTESIAN_POINT('',(122.542812602034,1.85,50.3336368280768));
#199405=CARTESIAN_POINT('',(122.542812602034,1.85,50.3336368280768));
#199406=CARTESIAN_POINT('',(122.542812602034,1.85,50.3336368280768));
#199407=CARTESIAN_POINT('Origin',(123.033626104583,1.85,50.4290417845261));
#199408=CARTESIAN_POINT('',(123.033626104583,1.35,50.4290417845261));
#199409=CARTESIAN_POINT('',(122.976383130714,1.35,50.7235298860558));
#199410=CARTESIAN_POINT('',(123.033626104583,1.35,50.4290417845261));
#199411=CARTESIAN_POINT('',(122.976383130714,1.85,50.7235298860558));
#199412=CARTESIAN_POINT('',(123.033626104583,1.85,50.4290417845261));
#199413=CARTESIAN_POINT('Origin',(123.033626104583,1.35,50.4290417845261));
#199414=CARTESIAN_POINT('',(122.542812602034,1.35,50.3336368280768));
#199415=CARTESIAN_POINT('',(122.485569628164,1.35,50.6281249296065));
#199416=CARTESIAN_POINT('',(122.542812602034,1.35,50.3336368280768));
#199417=CARTESIAN_POINT('',(122.976383130714,1.35,50.7235298860558));
#199418=CARTESIAN_POINT('',(123.033626104583,1.35,50.4290417845261));
#199419=CARTESIAN_POINT('Origin',(122.542812602034,1.35,50.3336368280768));
#199420=CARTESIAN_POINT('',(122.485569628164,1.35,50.6281249296065));
#199421=CARTESIAN_POINT('',(122.542812602034,1.35,50.3336368280768));
#199422=CARTESIAN_POINT('Origin',(122.542812602034,2.65,50.3336368280768));
#199423=CARTESIAN_POINT('',(123.033626104583,2.65,50.4290417845261));
#199424=CARTESIAN_POINT('',(122.976383130714,2.65,50.7235298860558));
#199425=CARTESIAN_POINT('',(123.033626104583,2.65,50.4290417845261));
#199426=CARTESIAN_POINT('',(122.485569628164,2.65,50.6281249296065));
#199427=CARTESIAN_POINT('',(122.485569628164,2.65,50.6281249296065));
#199428=CARTESIAN_POINT('',(122.542812602034,2.65,50.3336368280768));
#199429=CARTESIAN_POINT('',(122.542812602034,2.65,50.3336368280768));
#199430=CARTESIAN_POINT('',(122.542812602034,2.65,50.3336368280768));
#199431=CARTESIAN_POINT('Origin',(123.033626104583,2.65,50.4290417845261));
#199432=CARTESIAN_POINT('',(123.033626104583,2.15,50.4290417845261));
#199433=CARTESIAN_POINT('',(122.976383130714,2.15,50.7235298860558));
#199434=CARTESIAN_POINT('',(123.033626104583,2.15,50.4290417845261));
#199435=CARTESIAN_POINT('',(122.976383130714,2.65,50.7235298860558));
#199436=CARTESIAN_POINT('',(123.033626104583,2.65,50.4290417845261));
#199437=CARTESIAN_POINT('Origin',(123.033626104583,2.15,50.4290417845261));
#199438=CARTESIAN_POINT('',(122.542812602034,2.15,50.3336368280768));
#199439=CARTESIAN_POINT('',(122.485569628164,2.15,50.6281249296065));
#199440=CARTESIAN_POINT('',(122.542812602034,2.15,50.3336368280768));
#199441=CARTESIAN_POINT('',(122.976383130714,2.15,50.7235298860558));
#199442=CARTESIAN_POINT('',(123.033626104583,2.15,50.4290417845261));
#199443=CARTESIAN_POINT('Origin',(122.542812602034,2.15,50.3336368280768));
#199444=CARTESIAN_POINT('',(122.485569628164,2.15,50.6281249296065));
#199445=CARTESIAN_POINT('',(122.542812602034,2.15,50.3336368280768));
#199446=CARTESIAN_POINT('Origin',(122.542812602034,3.45,50.3336368280768));
#199447=CARTESIAN_POINT('',(123.033626104583,3.45,50.4290417845261));
#199448=CARTESIAN_POINT('',(122.976383130714,3.45,50.7235298860558));
#199449=CARTESIAN_POINT('',(123.033626104583,3.45,50.4290417845261));
#199450=CARTESIAN_POINT('',(122.485569628164,3.45,50.6281249296065));
#199451=CARTESIAN_POINT('',(122.485569628164,3.45,50.6281249296065));
#199452=CARTESIAN_POINT('',(122.542812602034,3.45,50.3336368280768));
#199453=CARTESIAN_POINT('',(122.542812602034,3.45,50.3336368280768));
#199454=CARTESIAN_POINT('',(122.542812602034,3.45,50.3336368280768));
#199455=CARTESIAN_POINT('Origin',(123.033626104583,3.45,50.4290417845261));
#199456=CARTESIAN_POINT('',(123.033626104583,2.95,50.4290417845261));
#199457=CARTESIAN_POINT('',(122.976383130714,2.95,50.7235298860558));
#199458=CARTESIAN_POINT('',(123.033626104583,2.95,50.4290417845261));
#199459=CARTESIAN_POINT('',(122.976383130714,3.45,50.7235298860558));
#199460=CARTESIAN_POINT('',(123.033626104583,3.45,50.4290417845261));
#199461=CARTESIAN_POINT('Origin',(123.033626104583,2.95,50.4290417845261));
#199462=CARTESIAN_POINT('',(122.542812602034,2.95,50.3336368280768));
#199463=CARTESIAN_POINT('',(122.485569628164,2.95,50.6281249296065));
#199464=CARTESIAN_POINT('',(122.542812602034,2.95,50.3336368280768));
#199465=CARTESIAN_POINT('',(122.976383130714,2.95,50.7235298860558));
#199466=CARTESIAN_POINT('',(123.033626104583,2.95,50.4290417845261));
#199467=CARTESIAN_POINT('Origin',(122.542812602034,2.95,50.3336368280768));
#199468=CARTESIAN_POINT('',(122.485569628164,2.95,50.6281249296065));
#199469=CARTESIAN_POINT('',(122.542812602034,2.95,50.3336368280768));
#199470=CARTESIAN_POINT('Origin',(122.542812602034,4.25,50.3336368280768));
#199471=CARTESIAN_POINT('',(123.033626104583,4.25,50.4290417845261));
#199472=CARTESIAN_POINT('',(122.976383130714,4.25,50.7235298860558));
#199473=CARTESIAN_POINT('',(123.033626104583,4.25,50.4290417845261));
#199474=CARTESIAN_POINT('',(122.485569628164,4.25,50.6281249296065));
#199475=CARTESIAN_POINT('',(122.485569628164,4.25,50.6281249296065));
#199476=CARTESIAN_POINT('',(122.542812602034,4.25,50.3336368280768));
#199477=CARTESIAN_POINT('',(122.542812602034,4.25,50.3336368280768));
#199478=CARTESIAN_POINT('',(122.542812602034,4.25,50.3336368280768));
#199479=CARTESIAN_POINT('Origin',(123.033626104583,4.25,50.4290417845261));
#199480=CARTESIAN_POINT('',(123.033626104583,3.75,50.4290417845261));
#199481=CARTESIAN_POINT('',(122.976383130714,3.75,50.7235298860558));
#199482=CARTESIAN_POINT('',(123.033626104583,3.75,50.4290417845261));
#199483=CARTESIAN_POINT('',(122.976383130714,4.25,50.7235298860558));
#199484=CARTESIAN_POINT('',(123.033626104583,4.25,50.4290417845261));
#199485=CARTESIAN_POINT('Origin',(123.033626104583,3.75,50.4290417845261));
#199486=CARTESIAN_POINT('',(122.542812602034,3.75,50.3336368280768));
#199487=CARTESIAN_POINT('',(122.485569628164,3.75,50.6281249296065));
#199488=CARTESIAN_POINT('',(122.542812602034,3.75,50.3336368280768));
#199489=CARTESIAN_POINT('',(122.976383130714,3.75,50.7235298860558));
#199490=CARTESIAN_POINT('',(123.033626104583,3.75,50.4290417845261));
#199491=CARTESIAN_POINT('Origin',(122.542812602034,3.75,50.3336368280768));
#199492=CARTESIAN_POINT('',(122.485569628164,3.75,50.6281249296065));
#199493=CARTESIAN_POINT('',(122.542812602034,3.75,50.3336368280768));
#199494=CARTESIAN_POINT('Origin',(122.542812602034,5.05,50.3336368280768));
#199495=CARTESIAN_POINT('',(123.033626104583,5.05,50.4290417845261));
#199496=CARTESIAN_POINT('',(122.976383130714,5.05,50.7235298860558));
#199497=CARTESIAN_POINT('',(123.033626104583,5.05,50.4290417845261));
#199498=CARTESIAN_POINT('',(122.485569628164,5.05,50.6281249296065));
#199499=CARTESIAN_POINT('',(122.485569628164,5.05,50.6281249296065));
#199500=CARTESIAN_POINT('',(122.542812602034,5.05,50.3336368280768));
#199501=CARTESIAN_POINT('',(122.542812602034,5.05,50.3336368280768));
#199502=CARTESIAN_POINT('',(122.542812602034,5.05,50.3336368280768));
#199503=CARTESIAN_POINT('Origin',(123.033626104583,5.05,50.4290417845261));
#199504=CARTESIAN_POINT('',(123.033626104583,4.55,50.4290417845261));
#199505=CARTESIAN_POINT('',(122.976383130714,4.55,50.7235298860558));
#199506=CARTESIAN_POINT('',(123.033626104583,4.55,50.4290417845261));
#199507=CARTESIAN_POINT('',(122.976383130714,5.05,50.7235298860558));
#199508=CARTESIAN_POINT('',(123.033626104583,5.05,50.4290417845261));
#199509=CARTESIAN_POINT('Origin',(123.033626104583,4.55,50.4290417845261));
#199510=CARTESIAN_POINT('',(122.542812602034,4.55,50.3336368280768));
#199511=CARTESIAN_POINT('',(122.485569628164,4.55,50.6281249296065));
#199512=CARTESIAN_POINT('',(122.542812602034,4.55,50.3336368280768));
#199513=CARTESIAN_POINT('',(122.976383130714,4.55,50.7235298860558));
#199514=CARTESIAN_POINT('',(123.033626104583,4.55,50.4290417845261));
#199515=CARTESIAN_POINT('Origin',(122.542812602034,4.55,50.3336368280768));
#199516=CARTESIAN_POINT('',(122.485569628164,4.55,50.6281249296065));
#199517=CARTESIAN_POINT('',(122.542812602034,4.55,50.3336368280768));
#199518=CARTESIAN_POINT('Origin',(122.542812602034,5.85,50.3336368280768));
#199519=CARTESIAN_POINT('',(123.033626104583,5.85,50.4290417845261));
#199520=CARTESIAN_POINT('',(122.976383130714,5.85,50.7235298860558));
#199521=CARTESIAN_POINT('',(123.033626104583,5.85,50.4290417845261));
#199522=CARTESIAN_POINT('',(122.485569628164,5.85,50.6281249296065));
#199523=CARTESIAN_POINT('',(122.485569628164,5.85,50.6281249296065));
#199524=CARTESIAN_POINT('',(122.542812602034,5.85,50.3336368280768));
#199525=CARTESIAN_POINT('',(122.542812602034,5.85,50.3336368280768));
#199526=CARTESIAN_POINT('',(122.542812602034,5.85,50.3336368280768));
#199527=CARTESIAN_POINT('Origin',(123.033626104583,5.85,50.4290417845261));
#199528=CARTESIAN_POINT('',(123.033626104583,5.35,50.4290417845261));
#199529=CARTESIAN_POINT('',(122.976383130714,5.35,50.7235298860558));
#199530=CARTESIAN_POINT('',(123.033626104583,5.35,50.4290417845261));
#199531=CARTESIAN_POINT('',(122.976383130714,5.85,50.7235298860558));
#199532=CARTESIAN_POINT('',(123.033626104583,5.85,50.4290417845261));
#199533=CARTESIAN_POINT('Origin',(123.033626104583,5.35,50.4290417845261));
#199534=CARTESIAN_POINT('',(122.542812602034,5.35,50.3336368280768));
#199535=CARTESIAN_POINT('',(122.485569628164,5.35,50.6281249296065));
#199536=CARTESIAN_POINT('',(122.542812602034,5.35,50.3336368280768));
#199537=CARTESIAN_POINT('',(122.976383130714,5.35,50.7235298860558));
#199538=CARTESIAN_POINT('',(123.033626104583,5.35,50.4290417845261));
#199539=CARTESIAN_POINT('Origin',(122.542812602034,5.35,50.3336368280768));
#199540=CARTESIAN_POINT('',(122.485569628164,5.35,50.6281249296065));
#199541=CARTESIAN_POINT('',(122.542812602034,5.35,50.3336368280768));
#199542=CARTESIAN_POINT('Origin',(121.757510997955,5.85,50.180988897758));
#199543=CARTESIAN_POINT('',(122.248324500504,5.85,50.2763938542073));
#199544=CARTESIAN_POINT('',(122.191081526635,5.85,50.570881955737));
#199545=CARTESIAN_POINT('',(122.248324500504,5.85,50.2763938542073));
#199546=CARTESIAN_POINT('',(121.700268024085,5.85,50.4754769992877));
#199547=CARTESIAN_POINT('',(121.700268024085,5.85,50.4754769992877));
#199548=CARTESIAN_POINT('',(121.757510997955,5.85,50.180988897758));
#199549=CARTESIAN_POINT('',(121.757510997955,5.85,50.180988897758));
#199550=CARTESIAN_POINT('',(121.757510997955,5.85,50.180988897758));
#199551=CARTESIAN_POINT('Origin',(122.248324500504,5.85,50.2763938542073));
#199552=CARTESIAN_POINT('',(122.248324500504,5.35,50.2763938542073));
#199553=CARTESIAN_POINT('',(122.191081526635,5.35,50.570881955737));
#199554=CARTESIAN_POINT('',(122.248324500504,5.35,50.2763938542073));
#199555=CARTESIAN_POINT('',(122.191081526635,5.85,50.570881955737));
#199556=CARTESIAN_POINT('',(122.248324500504,5.85,50.2763938542073));
#199557=CARTESIAN_POINT('Origin',(122.248324500504,5.35,50.2763938542073));
#199558=CARTESIAN_POINT('',(121.757510997955,5.35,50.180988897758));
#199559=CARTESIAN_POINT('',(121.700268024085,5.35,50.4754769992877));
#199560=CARTESIAN_POINT('',(121.757510997955,5.35,50.180988897758));
#199561=CARTESIAN_POINT('',(122.191081526635,5.35,50.570881955737));
#199562=CARTESIAN_POINT('',(122.248324500504,5.35,50.2763938542073));
#199563=CARTESIAN_POINT('Origin',(121.757510997955,5.35,50.180988897758));
#199564=CARTESIAN_POINT('',(121.700268024085,5.35,50.4754769992877));
#199565=CARTESIAN_POINT('',(121.757510997955,5.35,50.180988897758));
#199566=CARTESIAN_POINT('Origin',(120.972209393875,5.85,50.0283409674392));
#199567=CARTESIAN_POINT('',(121.463022896425,5.85,50.1237459238885));
#199568=CARTESIAN_POINT('',(121.405779922555,5.85,50.4182340254182));
#199569=CARTESIAN_POINT('',(121.463022896425,5.85,50.1237459238885));
#199570=CARTESIAN_POINT('',(120.914966420006,5.85,50.3228290689689));
#199571=CARTESIAN_POINT('',(120.914966420006,5.85,50.3228290689689));
#199572=CARTESIAN_POINT('',(120.972209393875,5.85,50.0283409674392));
#199573=CARTESIAN_POINT('',(120.972209393875,5.85,50.0283409674392));
#199574=CARTESIAN_POINT('',(120.972209393875,5.85,50.0283409674392));
#199575=CARTESIAN_POINT('Origin',(121.463022896425,5.85,50.1237459238885));
#199576=CARTESIAN_POINT('',(121.463022896425,5.35,50.1237459238885));
#199577=CARTESIAN_POINT('',(121.405779922555,5.35,50.4182340254182));
#199578=CARTESIAN_POINT('',(121.463022896425,5.35,50.1237459238885));
#199579=CARTESIAN_POINT('',(121.405779922555,5.85,50.4182340254182));
#199580=CARTESIAN_POINT('',(121.463022896425,5.85,50.1237459238885));
#199581=CARTESIAN_POINT('Origin',(121.463022896425,5.35,50.1237459238885));
#199582=CARTESIAN_POINT('',(120.972209393875,5.35,50.0283409674392));
#199583=CARTESIAN_POINT('',(120.914966420006,5.35,50.3228290689689));
#199584=CARTESIAN_POINT('',(120.972209393875,5.35,50.0283409674392));
#199585=CARTESIAN_POINT('',(121.405779922555,5.35,50.4182340254182));
#199586=CARTESIAN_POINT('',(121.463022896425,5.35,50.1237459238885));
#199587=CARTESIAN_POINT('Origin',(120.972209393875,5.35,50.0283409674392));
#199588=CARTESIAN_POINT('',(120.914966420006,5.35,50.3228290689689));
#199589=CARTESIAN_POINT('',(120.972209393875,5.35,50.0283409674392));
#199590=CARTESIAN_POINT('Origin',(120.186907789796,5.85,49.8756930371204));
#199591=CARTESIAN_POINT('',(120.677721292346,5.85,49.9710979935697));
#199592=CARTESIAN_POINT('',(120.620478318476,5.85,50.2655860950994));
#199593=CARTESIAN_POINT('',(120.677721292346,5.85,49.9710979935697));
#199594=CARTESIAN_POINT('',(120.129664815927,5.85,50.1701811386501));
#199595=CARTESIAN_POINT('',(120.129664815927,5.85,50.1701811386501));
#199596=CARTESIAN_POINT('',(120.186907789796,5.85,49.8756930371204));
#199597=CARTESIAN_POINT('',(120.186907789796,5.85,49.8756930371204));
#199598=CARTESIAN_POINT('',(120.186907789796,5.85,49.8756930371204));
#199599=CARTESIAN_POINT('Origin',(120.677721292346,5.85,49.9710979935697));
#199600=CARTESIAN_POINT('',(120.677721292346,5.35,49.9710979935697));
#199601=CARTESIAN_POINT('',(120.620478318476,5.35,50.2655860950994));
#199602=CARTESIAN_POINT('',(120.677721292346,5.35,49.9710979935697));
#199603=CARTESIAN_POINT('',(120.620478318476,5.85,50.2655860950994));
#199604=CARTESIAN_POINT('',(120.677721292346,5.85,49.9710979935697));
#199605=CARTESIAN_POINT('Origin',(120.677721292346,5.35,49.9710979935697));
#199606=CARTESIAN_POINT('',(120.186907789796,5.35,49.8756930371204));
#199607=CARTESIAN_POINT('',(120.129664815927,5.35,50.1701811386501));
#199608=CARTESIAN_POINT('',(120.186907789796,5.35,49.8756930371204));
#199609=CARTESIAN_POINT('',(120.620478318476,5.35,50.2655860950994));
#199610=CARTESIAN_POINT('',(120.677721292346,5.35,49.9710979935697));
#199611=CARTESIAN_POINT('Origin',(120.186907789796,5.35,49.8756930371204));
#199612=CARTESIAN_POINT('',(120.129664815927,5.35,50.1701811386501));
#199613=CARTESIAN_POINT('',(120.186907789796,5.35,49.8756930371204));
#199614=CARTESIAN_POINT('Origin',(119.401606185717,5.85,49.7230451068016));
#199615=CARTESIAN_POINT('',(119.892419688267,5.85,49.8184500632509));
#199616=CARTESIAN_POINT('',(119.835176714397,5.85,50.1129381647806));
#199617=CARTESIAN_POINT('',(119.892419688267,5.85,49.8184500632509));
#199618=CARTESIAN_POINT('',(119.344363211847,5.85,50.0175332083313));
#199619=CARTESIAN_POINT('',(119.344363211847,5.85,50.0175332083313));
#199620=CARTESIAN_POINT('',(119.401606185717,5.85,49.7230451068016));
#199621=CARTESIAN_POINT('',(119.401606185717,5.85,49.7230451068016));
#199622=CARTESIAN_POINT('',(119.401606185717,5.85,49.7230451068016));
#199623=CARTESIAN_POINT('Origin',(119.892419688267,5.85,49.8184500632509));
#199624=CARTESIAN_POINT('',(119.892419688267,5.35,49.8184500632509));
#199625=CARTESIAN_POINT('',(119.835176714397,5.35,50.1129381647806));
#199626=CARTESIAN_POINT('',(119.892419688267,5.35,49.8184500632509));
#199627=CARTESIAN_POINT('',(119.835176714397,5.85,50.1129381647806));
#199628=CARTESIAN_POINT('',(119.892419688267,5.85,49.8184500632509));
#199629=CARTESIAN_POINT('Origin',(119.892419688267,5.35,49.8184500632509));
#199630=CARTESIAN_POINT('',(119.401606185717,5.35,49.7230451068016));
#199631=CARTESIAN_POINT('',(119.344363211847,5.35,50.0175332083313));
#199632=CARTESIAN_POINT('',(119.401606185717,5.35,49.7230451068016));
#199633=CARTESIAN_POINT('',(119.835176714397,5.35,50.1129381647806));
#199634=CARTESIAN_POINT('',(119.892419688267,5.35,49.8184500632509));
#199635=CARTESIAN_POINT('Origin',(119.401606185717,5.35,49.7230451068016));
#199636=CARTESIAN_POINT('',(119.344363211847,5.35,50.0175332083313));
#199637=CARTESIAN_POINT('',(119.401606185717,5.35,49.7230451068016));
#199638=CARTESIAN_POINT('Origin',(118.616304581638,5.85,49.5703971764828));
#199639=CARTESIAN_POINT('',(119.107118084187,5.85,49.6658021329321));
#199640=CARTESIAN_POINT('',(119.049875110318,5.85,49.9602902344618));
#199641=CARTESIAN_POINT('',(119.107118084187,5.85,49.6658021329321));
#199642=CARTESIAN_POINT('',(118.559061607768,5.85,49.8648852780125));
#199643=CARTESIAN_POINT('',(118.559061607768,5.85,49.8648852780125));
#199644=CARTESIAN_POINT('',(118.616304581638,5.85,49.5703971764828));
#199645=CARTESIAN_POINT('',(118.616304581638,5.85,49.5703971764828));
#199646=CARTESIAN_POINT('',(118.616304581638,5.85,49.5703971764828));
#199647=CARTESIAN_POINT('Origin',(119.107118084187,5.85,49.6658021329321));
#199648=CARTESIAN_POINT('',(119.107118084187,5.35,49.6658021329321));
#199649=CARTESIAN_POINT('',(119.049875110318,5.35,49.9602902344618));
#199650=CARTESIAN_POINT('',(119.107118084187,5.35,49.6658021329321));
#199651=CARTESIAN_POINT('',(119.049875110318,5.85,49.9602902344618));
#199652=CARTESIAN_POINT('',(119.107118084187,5.85,49.6658021329321));
#199653=CARTESIAN_POINT('Origin',(119.107118084187,5.35,49.6658021329321));
#199654=CARTESIAN_POINT('',(118.616304581638,5.35,49.5703971764828));
#199655=CARTESIAN_POINT('',(118.559061607768,5.35,49.8648852780125));
#199656=CARTESIAN_POINT('',(118.616304581638,5.35,49.5703971764828));
#199657=CARTESIAN_POINT('',(119.049875110318,5.35,49.9602902344618));
#199658=CARTESIAN_POINT('',(119.107118084187,5.35,49.6658021329321));
#199659=CARTESIAN_POINT('Origin',(118.616304581638,5.35,49.5703971764828));
#199660=CARTESIAN_POINT('',(118.559061607768,5.35,49.8648852780125));
#199661=CARTESIAN_POINT('',(118.616304581638,5.35,49.5703971764828));
#199662=CARTESIAN_POINT('Origin',(117.831002977559,5.85,49.417749246164));
#199663=CARTESIAN_POINT('',(118.321816480108,5.85,49.5131542026133));
#199664=CARTESIAN_POINT('',(118.264573506239,5.85,49.807642304143));
#199665=CARTESIAN_POINT('',(118.321816480108,5.85,49.5131542026133));
#199666=CARTESIAN_POINT('',(117.773760003689,5.85,49.7122373476937));
#199667=CARTESIAN_POINT('',(117.773760003689,5.85,49.7122373476937));
#199668=CARTESIAN_POINT('',(117.831002977559,5.85,49.417749246164));
#199669=CARTESIAN_POINT('',(117.831002977559,5.85,49.417749246164));
#199670=CARTESIAN_POINT('',(117.831002977559,5.85,49.417749246164));
#199671=CARTESIAN_POINT('Origin',(118.321816480108,5.85,49.5131542026133));
#199672=CARTESIAN_POINT('',(118.321816480108,5.35,49.5131542026133));
#199673=CARTESIAN_POINT('',(118.264573506239,5.35,49.807642304143));
#199674=CARTESIAN_POINT('',(118.321816480108,5.35,49.5131542026133));
#199675=CARTESIAN_POINT('',(118.264573506239,5.85,49.807642304143));
#199676=CARTESIAN_POINT('',(118.321816480108,5.85,49.5131542026133));
#199677=CARTESIAN_POINT('Origin',(118.321816480108,5.35,49.5131542026133));
#199678=CARTESIAN_POINT('',(117.831002977559,5.35,49.417749246164));
#199679=CARTESIAN_POINT('',(117.773760003689,5.35,49.7122373476937));
#199680=CARTESIAN_POINT('',(117.831002977559,5.35,49.417749246164));
#199681=CARTESIAN_POINT('',(118.264573506239,5.35,49.807642304143));
#199682=CARTESIAN_POINT('',(118.321816480108,5.35,49.5131542026133));
#199683=CARTESIAN_POINT('Origin',(117.831002977559,5.35,49.417749246164));
#199684=CARTESIAN_POINT('',(117.773760003689,5.35,49.7122373476937));
#199685=CARTESIAN_POINT('',(117.831002977559,5.35,49.417749246164));
#199686=CARTESIAN_POINT('Origin',(117.045701373479,5.85,49.2651013158452));
#199687=CARTESIAN_POINT('',(117.536514876029,5.85,49.3605062722945));
#199688=CARTESIAN_POINT('',(117.479271902159,5.85,49.6549943738242));
#199689=CARTESIAN_POINT('',(117.536514876029,5.85,49.3605062722945));
#199690=CARTESIAN_POINT('',(116.98845839961,5.85,49.5595894173749));
#199691=CARTESIAN_POINT('',(116.98845839961,5.85,49.5595894173749));
#199692=CARTESIAN_POINT('',(117.045701373479,5.85,49.2651013158452));
#199693=CARTESIAN_POINT('',(117.045701373479,5.85,49.2651013158452));
#199694=CARTESIAN_POINT('',(117.045701373479,5.85,49.2651013158452));
#199695=CARTESIAN_POINT('Origin',(117.536514876029,5.85,49.3605062722945));
#199696=CARTESIAN_POINT('',(117.536514876029,5.35,49.3605062722945));
#199697=CARTESIAN_POINT('',(117.479271902159,5.35,49.6549943738242));
#199698=CARTESIAN_POINT('',(117.536514876029,5.35,49.3605062722945));
#199699=CARTESIAN_POINT('',(117.479271902159,5.85,49.6549943738242));
#199700=CARTESIAN_POINT('',(117.536514876029,5.85,49.3605062722945));
#199701=CARTESIAN_POINT('Origin',(117.536514876029,5.35,49.3605062722945));
#199702=CARTESIAN_POINT('',(117.045701373479,5.35,49.2651013158452));
#199703=CARTESIAN_POINT('',(116.98845839961,5.35,49.5595894173749));
#199704=CARTESIAN_POINT('',(117.045701373479,5.35,49.2651013158452));
#199705=CARTESIAN_POINT('',(117.479271902159,5.35,49.6549943738242));
#199706=CARTESIAN_POINT('',(117.536514876029,5.35,49.3605062722945));
#199707=CARTESIAN_POINT('Origin',(117.045701373479,5.35,49.2651013158452));
#199708=CARTESIAN_POINT('',(116.98845839961,5.35,49.5595894173749));
#199709=CARTESIAN_POINT('',(117.045701373479,5.35,49.2651013158452));
#199710=CARTESIAN_POINT('Origin',(116.2603997694,5.85,49.1124533855264));
#199711=CARTESIAN_POINT('',(116.75121327195,5.85,49.2078583419757));
#199712=CARTESIAN_POINT('',(116.69397029808,5.85,49.5023464435054));
#199713=CARTESIAN_POINT('',(116.75121327195,5.85,49.2078583419757));
#199714=CARTESIAN_POINT('',(116.203156795531,5.85,49.4069414870561));
#199715=CARTESIAN_POINT('',(116.203156795531,5.85,49.4069414870561));
#199716=CARTESIAN_POINT('',(116.2603997694,5.85,49.1124533855264));
#199717=CARTESIAN_POINT('',(116.2603997694,5.85,49.1124533855264));
#199718=CARTESIAN_POINT('',(116.2603997694,5.85,49.1124533855264));
#199719=CARTESIAN_POINT('Origin',(116.75121327195,5.85,49.2078583419757));
#199720=CARTESIAN_POINT('',(116.75121327195,5.35,49.2078583419757));
#199721=CARTESIAN_POINT('',(116.69397029808,5.35,49.5023464435054));
#199722=CARTESIAN_POINT('',(116.75121327195,5.35,49.2078583419757));
#199723=CARTESIAN_POINT('',(116.69397029808,5.85,49.5023464435054));
#199724=CARTESIAN_POINT('',(116.75121327195,5.85,49.2078583419757));
#199725=CARTESIAN_POINT('Origin',(116.75121327195,5.35,49.2078583419757));
#199726=CARTESIAN_POINT('',(116.2603997694,5.35,49.1124533855264));
#199727=CARTESIAN_POINT('',(116.203156795531,5.35,49.4069414870561));
#199728=CARTESIAN_POINT('',(116.2603997694,5.35,49.1124533855264));
#199729=CARTESIAN_POINT('',(116.69397029808,5.35,49.5023464435054));
#199730=CARTESIAN_POINT('',(116.75121327195,5.35,49.2078583419757));
#199731=CARTESIAN_POINT('Origin',(116.2603997694,5.35,49.1124533855264));
#199732=CARTESIAN_POINT('',(116.203156795531,5.35,49.4069414870561));
#199733=CARTESIAN_POINT('',(116.2603997694,5.35,49.1124533855264));
#199734=CARTESIAN_POINT('Origin',(115.475098165321,5.85,48.9598054552076));
#199735=CARTESIAN_POINT('',(115.96591166787,5.85,49.0552104116569));
#199736=CARTESIAN_POINT('',(115.908668694001,5.85,49.3496985131866));
#199737=CARTESIAN_POINT('',(115.96591166787,5.85,49.0552104116569));
#199738=CARTESIAN_POINT('',(115.417855191451,5.85,49.2542935567373));
#199739=CARTESIAN_POINT('',(115.417855191451,5.85,49.2542935567373));
#199740=CARTESIAN_POINT('',(115.475098165321,5.85,48.9598054552076));
#199741=CARTESIAN_POINT('',(115.475098165321,5.85,48.9598054552076));
#199742=CARTESIAN_POINT('',(115.475098165321,5.85,48.9598054552076));
#199743=CARTESIAN_POINT('Origin',(115.96591166787,5.85,49.0552104116569));
#199744=CARTESIAN_POINT('',(115.96591166787,5.35,49.0552104116569));
#199745=CARTESIAN_POINT('',(115.908668694001,5.35,49.3496985131866));
#199746=CARTESIAN_POINT('',(115.96591166787,5.35,49.0552104116569));
#199747=CARTESIAN_POINT('',(115.908668694001,5.85,49.3496985131866));
#199748=CARTESIAN_POINT('',(115.96591166787,5.85,49.0552104116569));
#199749=CARTESIAN_POINT('Origin',(115.96591166787,5.35,49.0552104116569));
#199750=CARTESIAN_POINT('',(115.475098165321,5.35,48.9598054552076));
#199751=CARTESIAN_POINT('',(115.417855191451,5.35,49.2542935567373));
#199752=CARTESIAN_POINT('',(115.475098165321,5.35,48.9598054552076));
#199753=CARTESIAN_POINT('',(115.908668694001,5.35,49.3496985131866));
#199754=CARTESIAN_POINT('',(115.96591166787,5.35,49.0552104116569));
#199755=CARTESIAN_POINT('Origin',(115.475098165321,5.35,48.9598054552076));
#199756=CARTESIAN_POINT('',(115.417855191451,5.35,49.2542935567373));
#199757=CARTESIAN_POINT('',(115.475098165321,5.35,48.9598054552076));
#199758=CARTESIAN_POINT('Origin',(114.689796561242,5.85,48.8071575248888));
#199759=CARTESIAN_POINT('',(115.180610063791,5.85,48.9025624813381));
#199760=CARTESIAN_POINT('',(115.123367089922,5.85,49.1970505828678));
#199761=CARTESIAN_POINT('',(115.180610063791,5.85,48.9025624813381));
#199762=CARTESIAN_POINT('',(114.632553587372,5.85,49.1016456264185));
#199763=CARTESIAN_POINT('',(114.632553587372,5.85,49.1016456264185));
#199764=CARTESIAN_POINT('',(114.689796561242,5.85,48.8071575248888));
#199765=CARTESIAN_POINT('',(114.689796561242,5.85,48.8071575248888));
#199766=CARTESIAN_POINT('',(114.689796561242,5.85,48.8071575248888));
#199767=CARTESIAN_POINT('Origin',(115.180610063791,5.85,48.9025624813381));
#199768=CARTESIAN_POINT('',(115.180610063791,5.35,48.9025624813381));
#199769=CARTESIAN_POINT('',(115.123367089922,5.35,49.1970505828678));
#199770=CARTESIAN_POINT('',(115.180610063791,5.35,48.9025624813381));
#199771=CARTESIAN_POINT('',(115.123367089922,5.85,49.1970505828678));
#199772=CARTESIAN_POINT('',(115.180610063791,5.85,48.9025624813381));
#199773=CARTESIAN_POINT('Origin',(115.180610063791,5.35,48.9025624813381));
#199774=CARTESIAN_POINT('',(114.689796561242,5.35,48.8071575248888));
#199775=CARTESIAN_POINT('',(114.632553587372,5.35,49.1016456264185));
#199776=CARTESIAN_POINT('',(114.689796561242,5.35,48.8071575248888));
#199777=CARTESIAN_POINT('',(115.123367089922,5.35,49.1970505828678));
#199778=CARTESIAN_POINT('',(115.180610063791,5.35,48.9025624813381));
#199779=CARTESIAN_POINT('Origin',(114.689796561242,5.35,48.8071575248888));
#199780=CARTESIAN_POINT('',(114.632553587372,5.35,49.1016456264185));
#199781=CARTESIAN_POINT('',(114.689796561242,5.35,48.8071575248888));
#199782=CARTESIAN_POINT('Origin',(113.904494957163,5.85,48.65450959457));
#199783=CARTESIAN_POINT('',(114.395308459712,5.85,48.7499145510193));
#199784=CARTESIAN_POINT('',(114.338065485842,5.85,49.044402652549));
#199785=CARTESIAN_POINT('',(114.395308459712,5.85,48.7499145510193));
#199786=CARTESIAN_POINT('',(113.847251983293,5.85,48.9489976960997));
#199787=CARTESIAN_POINT('',(113.847251983293,5.85,48.9489976960997));
#199788=CARTESIAN_POINT('',(113.904494957163,5.85,48.65450959457));
#199789=CARTESIAN_POINT('',(113.904494957163,5.85,48.65450959457));
#199790=CARTESIAN_POINT('',(113.904494957163,5.85,48.65450959457));
#199791=CARTESIAN_POINT('Origin',(114.395308459712,5.85,48.7499145510193));
#199792=CARTESIAN_POINT('',(114.395308459712,5.35,48.7499145510193));
#199793=CARTESIAN_POINT('',(114.338065485842,5.35,49.044402652549));
#199794=CARTESIAN_POINT('',(114.395308459712,5.35,48.7499145510193));
#199795=CARTESIAN_POINT('',(114.338065485842,5.85,49.044402652549));
#199796=CARTESIAN_POINT('',(114.395308459712,5.85,48.7499145510193));
#199797=CARTESIAN_POINT('Origin',(114.395308459712,5.35,48.7499145510193));
#199798=CARTESIAN_POINT('',(113.904494957163,5.35,48.65450959457));
#199799=CARTESIAN_POINT('',(113.847251983293,5.35,48.9489976960997));
#199800=CARTESIAN_POINT('',(113.904494957163,5.35,48.65450959457));
#199801=CARTESIAN_POINT('',(114.338065485842,5.35,49.044402652549));
#199802=CARTESIAN_POINT('',(114.395308459712,5.35,48.7499145510193));
#199803=CARTESIAN_POINT('Origin',(113.904494957163,5.35,48.65450959457));
#199804=CARTESIAN_POINT('',(113.847251983293,5.35,48.9489976960997));
#199805=CARTESIAN_POINT('',(113.904494957163,5.35,48.65450959457));
#199806=CARTESIAN_POINT('Origin',(113.119193353083,5.85,48.5018616642512));
#199807=CARTESIAN_POINT('',(113.610006855633,5.85,48.5972666207005));
#199808=CARTESIAN_POINT('',(113.552763881763,5.85,48.8917547222302));
#199809=CARTESIAN_POINT('',(113.610006855633,5.85,48.5972666207005));
#199810=CARTESIAN_POINT('',(113.061950379214,5.85,48.7963497657809));
#199811=CARTESIAN_POINT('',(113.061950379214,5.85,48.7963497657809));
#199812=CARTESIAN_POINT('',(113.119193353083,5.85,48.5018616642512));
#199813=CARTESIAN_POINT('',(113.119193353083,5.85,48.5018616642512));
#199814=CARTESIAN_POINT('',(113.119193353083,5.85,48.5018616642512));
#199815=CARTESIAN_POINT('Origin',(113.610006855633,5.85,48.5972666207005));
#199816=CARTESIAN_POINT('',(113.610006855633,5.35,48.5972666207005));
#199817=CARTESIAN_POINT('',(113.552763881763,5.35,48.8917547222302));
#199818=CARTESIAN_POINT('',(113.610006855633,5.35,48.5972666207005));
#199819=CARTESIAN_POINT('',(113.552763881763,5.85,48.8917547222302));
#199820=CARTESIAN_POINT('',(113.610006855633,5.85,48.5972666207005));
#199821=CARTESIAN_POINT('Origin',(113.610006855633,5.35,48.5972666207005));
#199822=CARTESIAN_POINT('',(113.119193353083,5.35,48.5018616642512));
#199823=CARTESIAN_POINT('',(113.061950379214,5.35,48.7963497657809));
#199824=CARTESIAN_POINT('',(113.119193353083,5.35,48.5018616642512));
#199825=CARTESIAN_POINT('',(113.552763881763,5.35,48.8917547222302));
#199826=CARTESIAN_POINT('',(113.610006855633,5.35,48.5972666207005));
#199827=CARTESIAN_POINT('Origin',(113.119193353083,5.35,48.5018616642512));
#199828=CARTESIAN_POINT('',(113.061950379214,5.35,48.7963497657809));
#199829=CARTESIAN_POINT('',(113.119193353083,5.35,48.5018616642512));
#199830=CARTESIAN_POINT('Origin',(112.333891749004,5.85,48.3492137339324));
#199831=CARTESIAN_POINT('',(112.824705251554,5.85,48.4446186903817));
#199832=CARTESIAN_POINT('',(112.767462277684,5.85,48.7391067919114));
#199833=CARTESIAN_POINT('',(112.824705251554,5.85,48.4446186903817));
#199834=CARTESIAN_POINT('',(112.276648775135,5.85,48.6437018354621));
#199835=CARTESIAN_POINT('',(112.276648775135,5.85,48.6437018354621));
#199836=CARTESIAN_POINT('',(112.333891749004,5.85,48.3492137339324));
#199837=CARTESIAN_POINT('',(112.333891749004,5.85,48.3492137339324));
#199838=CARTESIAN_POINT('',(112.333891749004,5.85,48.3492137339324));
#199839=CARTESIAN_POINT('Origin',(112.824705251554,5.85,48.4446186903817));
#199840=CARTESIAN_POINT('',(112.824705251554,5.35,48.4446186903817));
#199841=CARTESIAN_POINT('',(112.767462277684,5.35,48.7391067919114));
#199842=CARTESIAN_POINT('',(112.824705251554,5.35,48.4446186903817));
#199843=CARTESIAN_POINT('',(112.767462277684,5.85,48.7391067919114));
#199844=CARTESIAN_POINT('',(112.824705251554,5.85,48.4446186903817));
#199845=CARTESIAN_POINT('Origin',(112.824705251554,5.35,48.4446186903817));
#199846=CARTESIAN_POINT('',(112.333891749004,5.35,48.3492137339324));
#199847=CARTESIAN_POINT('',(112.276648775135,5.35,48.6437018354621));
#199848=CARTESIAN_POINT('',(112.333891749004,5.35,48.3492137339324));
#199849=CARTESIAN_POINT('',(112.767462277684,5.35,48.7391067919114));
#199850=CARTESIAN_POINT('',(112.824705251554,5.35,48.4446186903817));
#199851=CARTESIAN_POINT('Origin',(112.333891749004,5.35,48.3492137339324));
#199852=CARTESIAN_POINT('',(112.276648775135,5.35,48.6437018354621));
#199853=CARTESIAN_POINT('',(112.333891749004,5.35,48.3492137339324));
#199854=CARTESIAN_POINT('Origin',(112.333891749004,5.05,48.3492137339324));
#199855=CARTESIAN_POINT('',(112.824705251554,5.05,48.4446186903817));
#199856=CARTESIAN_POINT('',(112.767462277684,5.05,48.7391067919114));
#199857=CARTESIAN_POINT('',(112.824705251554,5.05,48.4446186903817));
#199858=CARTESIAN_POINT('',(112.276648775135,5.05,48.6437018354621));
#199859=CARTESIAN_POINT('',(112.276648775135,5.05,48.6437018354621));
#199860=CARTESIAN_POINT('',(112.333891749004,5.05,48.3492137339324));
#199861=CARTESIAN_POINT('',(112.333891749004,5.05,48.3492137339324));
#199862=CARTESIAN_POINT('',(112.333891749004,5.05,48.3492137339324));
#199863=CARTESIAN_POINT('Origin',(112.824705251554,5.05,48.4446186903817));
#199864=CARTESIAN_POINT('',(112.824705251554,4.55,48.4446186903817));
#199865=CARTESIAN_POINT('',(112.767462277684,4.55,48.7391067919114));
#199866=CARTESIAN_POINT('',(112.824705251554,4.55,48.4446186903817));
#199867=CARTESIAN_POINT('',(112.767462277684,5.05,48.7391067919114));
#199868=CARTESIAN_POINT('',(112.824705251554,5.05,48.4446186903817));
#199869=CARTESIAN_POINT('Origin',(112.824705251554,4.55,48.4446186903817));
#199870=CARTESIAN_POINT('',(112.333891749004,4.55,48.3492137339324));
#199871=CARTESIAN_POINT('',(112.276648775135,4.55,48.6437018354621));
#199872=CARTESIAN_POINT('',(112.333891749004,4.55,48.3492137339324));
#199873=CARTESIAN_POINT('',(112.767462277684,4.55,48.7391067919114));
#199874=CARTESIAN_POINT('',(112.824705251554,4.55,48.4446186903817));
#199875=CARTESIAN_POINT('Origin',(112.333891749004,4.55,48.3492137339324));
#199876=CARTESIAN_POINT('',(112.276648775135,4.55,48.6437018354621));
#199877=CARTESIAN_POINT('',(112.333891749004,4.55,48.3492137339324));
#199878=CARTESIAN_POINT('Origin',(112.333891749004,4.25,48.3492137339324));
#199879=CARTESIAN_POINT('',(112.824705251554,4.25,48.4446186903817));
#199880=CARTESIAN_POINT('',(112.767462277684,4.25,48.7391067919114));
#199881=CARTESIAN_POINT('',(112.824705251554,4.25,48.4446186903817));
#199882=CARTESIAN_POINT('',(112.276648775135,4.25,48.6437018354621));
#199883=CARTESIAN_POINT('',(112.276648775135,4.25,48.6437018354621));
#199884=CARTESIAN_POINT('',(112.333891749004,4.25,48.3492137339324));
#199885=CARTESIAN_POINT('',(112.333891749004,4.25,48.3492137339324));
#199886=CARTESIAN_POINT('',(112.333891749004,4.25,48.3492137339324));
#199887=CARTESIAN_POINT('Origin',(112.824705251554,4.25,48.4446186903817));
#199888=CARTESIAN_POINT('',(112.824705251554,3.75,48.4446186903817));
#199889=CARTESIAN_POINT('',(112.767462277684,3.75,48.7391067919114));
#199890=CARTESIAN_POINT('',(112.824705251554,3.75,48.4446186903817));
#199891=CARTESIAN_POINT('',(112.767462277684,4.25,48.7391067919114));
#199892=CARTESIAN_POINT('',(112.824705251554,4.25,48.4446186903817));
#199893=CARTESIAN_POINT('Origin',(112.824705251554,3.75,48.4446186903817));
#199894=CARTESIAN_POINT('',(112.333891749004,3.75,48.3492137339324));
#199895=CARTESIAN_POINT('',(112.276648775135,3.75,48.6437018354621));
#199896=CARTESIAN_POINT('',(112.333891749004,3.75,48.3492137339324));
#199897=CARTESIAN_POINT('',(112.767462277684,3.75,48.7391067919114));
#199898=CARTESIAN_POINT('',(112.824705251554,3.75,48.4446186903817));
#199899=CARTESIAN_POINT('Origin',(112.333891749004,3.75,48.3492137339324));
#199900=CARTESIAN_POINT('',(112.276648775135,3.75,48.6437018354621));
#199901=CARTESIAN_POINT('',(112.333891749004,3.75,48.3492137339324));
#199902=CARTESIAN_POINT('Origin',(112.333891749004,3.45,48.3492137339324));
#199903=CARTESIAN_POINT('',(112.824705251554,3.45,48.4446186903817));
#199904=CARTESIAN_POINT('',(112.767462277684,3.45,48.7391067919114));
#199905=CARTESIAN_POINT('',(112.824705251554,3.45,48.4446186903817));
#199906=CARTESIAN_POINT('',(112.276648775135,3.45,48.6437018354621));
#199907=CARTESIAN_POINT('',(112.276648775135,3.45,48.6437018354621));
#199908=CARTESIAN_POINT('',(112.333891749004,3.45,48.3492137339324));
#199909=CARTESIAN_POINT('',(112.333891749004,3.45,48.3492137339324));
#199910=CARTESIAN_POINT('',(112.333891749004,3.45,48.3492137339324));
#199911=CARTESIAN_POINT('Origin',(112.824705251554,3.45,48.4446186903817));
#199912=CARTESIAN_POINT('',(112.824705251554,2.95,48.4446186903817));
#199913=CARTESIAN_POINT('',(112.767462277684,2.95,48.7391067919114));
#199914=CARTESIAN_POINT('',(112.824705251554,2.95,48.4446186903817));
#199915=CARTESIAN_POINT('',(112.767462277684,3.45,48.7391067919114));
#199916=CARTESIAN_POINT('',(112.824705251554,3.45,48.4446186903817));
#199917=CARTESIAN_POINT('Origin',(112.824705251554,2.95,48.4446186903817));
#199918=CARTESIAN_POINT('',(112.333891749004,2.95,48.3492137339324));
#199919=CARTESIAN_POINT('',(112.276648775135,2.95,48.6437018354621));
#199920=CARTESIAN_POINT('',(112.333891749004,2.95,48.3492137339324));
#199921=CARTESIAN_POINT('',(112.767462277684,2.95,48.7391067919114));
#199922=CARTESIAN_POINT('',(112.824705251554,2.95,48.4446186903817));
#199923=CARTESIAN_POINT('Origin',(112.333891749004,2.95,48.3492137339324));
#199924=CARTESIAN_POINT('',(112.276648775135,2.95,48.6437018354621));
#199925=CARTESIAN_POINT('',(112.333891749004,2.95,48.3492137339324));
#199926=CARTESIAN_POINT('Origin',(112.333891749004,2.65,48.3492137339324));
#199927=CARTESIAN_POINT('',(112.824705251554,2.65,48.4446186903817));
#199928=CARTESIAN_POINT('',(112.767462277684,2.65,48.7391067919114));
#199929=CARTESIAN_POINT('',(112.824705251554,2.65,48.4446186903817));
#199930=CARTESIAN_POINT('',(112.276648775135,2.65,48.6437018354621));
#199931=CARTESIAN_POINT('',(112.276648775135,2.65,48.6437018354621));
#199932=CARTESIAN_POINT('',(112.333891749004,2.65,48.3492137339324));
#199933=CARTESIAN_POINT('',(112.333891749004,2.65,48.3492137339324));
#199934=CARTESIAN_POINT('',(112.333891749004,2.65,48.3492137339324));
#199935=CARTESIAN_POINT('Origin',(112.824705251554,2.65,48.4446186903817));
#199936=CARTESIAN_POINT('',(112.824705251554,2.15,48.4446186903817));
#199937=CARTESIAN_POINT('',(112.767462277684,2.15,48.7391067919114));
#199938=CARTESIAN_POINT('',(112.824705251554,2.15,48.4446186903817));
#199939=CARTESIAN_POINT('',(112.767462277684,2.65,48.7391067919114));
#199940=CARTESIAN_POINT('',(112.824705251554,2.65,48.4446186903817));
#199941=CARTESIAN_POINT('Origin',(112.824705251554,2.15,48.4446186903817));
#199942=CARTESIAN_POINT('',(112.333891749004,2.15,48.3492137339324));
#199943=CARTESIAN_POINT('',(112.276648775135,2.15,48.6437018354621));
#199944=CARTESIAN_POINT('',(112.333891749004,2.15,48.3492137339324));
#199945=CARTESIAN_POINT('',(112.767462277684,2.15,48.7391067919114));
#199946=CARTESIAN_POINT('',(112.824705251554,2.15,48.4446186903817));
#199947=CARTESIAN_POINT('Origin',(112.333891749004,2.15,48.3492137339324));
#199948=CARTESIAN_POINT('',(112.276648775135,2.15,48.6437018354621));
#199949=CARTESIAN_POINT('',(112.333891749004,2.15,48.3492137339324));
#199950=CARTESIAN_POINT('Origin',(112.333891749004,1.85,48.3492137339324));
#199951=CARTESIAN_POINT('',(112.824705251554,1.85,48.4446186903817));
#199952=CARTESIAN_POINT('',(112.767462277684,1.85,48.7391067919114));
#199953=CARTESIAN_POINT('',(112.824705251554,1.85,48.4446186903817));
#199954=CARTESIAN_POINT('',(112.276648775135,1.85,48.6437018354621));
#199955=CARTESIAN_POINT('',(112.276648775135,1.85,48.6437018354621));
#199956=CARTESIAN_POINT('',(112.333891749004,1.85,48.3492137339324));
#199957=CARTESIAN_POINT('',(112.333891749004,1.85,48.3492137339324));
#199958=CARTESIAN_POINT('',(112.333891749004,1.85,48.3492137339324));
#199959=CARTESIAN_POINT('Origin',(112.824705251554,1.85,48.4446186903817));
#199960=CARTESIAN_POINT('',(112.824705251554,1.35,48.4446186903817));
#199961=CARTESIAN_POINT('',(112.767462277684,1.35,48.7391067919114));
#199962=CARTESIAN_POINT('',(112.824705251554,1.35,48.4446186903817));
#199963=CARTESIAN_POINT('',(112.767462277684,1.85,48.7391067919114));
#199964=CARTESIAN_POINT('',(112.824705251554,1.85,48.4446186903817));
#199965=CARTESIAN_POINT('Origin',(112.824705251554,1.35,48.4446186903817));
#199966=CARTESIAN_POINT('',(112.333891749004,1.35,48.3492137339324));
#199967=CARTESIAN_POINT('',(112.276648775135,1.35,48.6437018354621));
#199968=CARTESIAN_POINT('',(112.333891749004,1.35,48.3492137339324));
#199969=CARTESIAN_POINT('',(112.767462277684,1.35,48.7391067919114));
#199970=CARTESIAN_POINT('',(112.824705251554,1.35,48.4446186903817));
#199971=CARTESIAN_POINT('Origin',(112.333891749004,1.35,48.3492137339324));
#199972=CARTESIAN_POINT('',(112.276648775135,1.35,48.6437018354621));
#199973=CARTESIAN_POINT('',(112.333891749004,1.35,48.3492137339324));
#199974=CARTESIAN_POINT('Origin',(112.333891749004,1.05,48.3492137339324));
#199975=CARTESIAN_POINT('',(112.824705251554,1.05,48.4446186903817));
#199976=CARTESIAN_POINT('',(112.767462277684,1.05,48.7391067919114));
#199977=CARTESIAN_POINT('',(112.824705251554,1.05,48.4446186903817));
#199978=CARTESIAN_POINT('',(112.276648775135,1.05,48.6437018354621));
#199979=CARTESIAN_POINT('',(112.276648775135,1.05,48.6437018354621));
#199980=CARTESIAN_POINT('',(112.333891749004,1.05,48.3492137339324));
#199981=CARTESIAN_POINT('',(112.333891749004,1.05,48.3492137339324));
#199982=CARTESIAN_POINT('',(112.333891749004,1.05,48.3492137339324));
#199983=CARTESIAN_POINT('Origin',(112.824705251554,1.05,48.4446186903817));
#199984=CARTESIAN_POINT('',(112.824705251554,0.550000000000015,48.4446186903817));
#199985=CARTESIAN_POINT('',(112.767462277684,0.550000000000015,48.7391067919114));
#199986=CARTESIAN_POINT('',(112.824705251554,0.550000000000015,48.4446186903817));
#199987=CARTESIAN_POINT('',(112.767462277684,1.05,48.7391067919114));
#199988=CARTESIAN_POINT('',(112.824705251554,1.05,48.4446186903817));
#199989=CARTESIAN_POINT('Origin',(112.824705251554,0.550000000000015,48.4446186903817));
#199990=CARTESIAN_POINT('',(112.333891749004,0.550000000000015,48.3492137339324));
#199991=CARTESIAN_POINT('',(112.276648775135,0.550000000000015,48.6437018354621));
#199992=CARTESIAN_POINT('',(112.333891749004,0.550000000000015,48.3492137339324));
#199993=CARTESIAN_POINT('',(112.767462277684,0.550000000000015,48.7391067919114));
#199994=CARTESIAN_POINT('',(112.824705251554,0.550000000000015,48.4446186903817));
#199995=CARTESIAN_POINT('Origin',(112.333891749004,0.550000000000015,48.3492137339324));
#199996=CARTESIAN_POINT('',(112.276648775135,0.550000000000015,48.6437018354621));
#199997=CARTESIAN_POINT('',(112.333891749004,0.550000000000015,48.3492137339324));
#199998=CARTESIAN_POINT('Origin',(112.333891749004,0.250000000000015,48.3492137339324));
#199999=CARTESIAN_POINT('',(112.824705251554,0.250000000000015,48.4446186903817));
#200000=CARTESIAN_POINT('',(112.767462277684,0.250000000000015,48.7391067919114));
#200001=CARTESIAN_POINT('',(112.824705251554,0.250000000000015,48.4446186903817));
#200002=CARTESIAN_POINT('',(112.276648775135,0.250000000000015,48.6437018354621));
#200003=CARTESIAN_POINT('',(112.276648775135,0.250000000000015,48.6437018354621));
#200004=CARTESIAN_POINT('',(112.333891749004,0.250000000000015,48.3492137339324));
#200005=CARTESIAN_POINT('',(112.333891749004,0.250000000000015,48.3492137339324));
#200006=CARTESIAN_POINT('',(112.333891749004,0.250000000000015,48.3492137339324));
#200007=CARTESIAN_POINT('Origin',(112.824705251554,0.250000000000015,48.4446186903817));
#200008=CARTESIAN_POINT('',(112.824705251554,-0.249999999999985,48.4446186903817));
#200009=CARTESIAN_POINT('',(112.767462277684,-0.249999999999985,48.7391067919114));
#200010=CARTESIAN_POINT('',(112.824705251554,-0.249999999999985,48.4446186903817));
#200011=CARTESIAN_POINT('',(112.767462277684,0.250000000000015,48.7391067919114));
#200012=CARTESIAN_POINT('',(112.824705251554,0.250000000000015,48.4446186903817));
#200013=CARTESIAN_POINT('Origin',(112.824705251554,-0.249999999999985,48.4446186903817));
#200014=CARTESIAN_POINT('',(112.333891749004,-0.249999999999985,48.3492137339324));
#200015=CARTESIAN_POINT('',(112.276648775135,-0.249999999999985,48.6437018354621));
#200016=CARTESIAN_POINT('',(112.333891749004,-0.249999999999985,48.3492137339324));
#200017=CARTESIAN_POINT('',(112.767462277684,-0.249999999999985,48.7391067919114));
#200018=CARTESIAN_POINT('',(112.824705251554,-0.249999999999985,48.4446186903817));
#200019=CARTESIAN_POINT('Origin',(112.333891749004,-0.249999999999985,48.3492137339324));
#200020=CARTESIAN_POINT('',(112.276648775135,-0.249999999999985,48.6437018354621));
#200021=CARTESIAN_POINT('',(112.333891749004,-0.249999999999985,48.3492137339324));
#200022=CARTESIAN_POINT('Origin',(112.333891749004,-0.549999999999986,48.3492137339324));
#200023=CARTESIAN_POINT('',(112.824705251554,-0.549999999999986,48.4446186903817));
#200024=CARTESIAN_POINT('',(112.767462277684,-0.549999999999986,48.7391067919114));
#200025=CARTESIAN_POINT('',(112.824705251554,-0.549999999999986,48.4446186903817));
#200026=CARTESIAN_POINT('',(112.276648775135,-0.549999999999986,48.6437018354621));
#200027=CARTESIAN_POINT('',(112.276648775135,-0.549999999999986,48.6437018354621));
#200028=CARTESIAN_POINT('',(112.333891749004,-0.549999999999986,48.3492137339324));
#200029=CARTESIAN_POINT('',(112.333891749004,-0.549999999999986,48.3492137339324));
#200030=CARTESIAN_POINT('',(112.333891749004,-0.549999999999986,48.3492137339324));
#200031=CARTESIAN_POINT('Origin',(112.824705251554,-0.549999999999986,48.4446186903817));
#200032=CARTESIAN_POINT('',(112.824705251554,-1.05,48.4446186903817));
#200033=CARTESIAN_POINT('',(112.767462277684,-1.05,48.7391067919114));
#200034=CARTESIAN_POINT('',(112.824705251554,-1.05,48.4446186903817));
#200035=CARTESIAN_POINT('',(112.767462277684,-0.549999999999986,48.7391067919114));
#200036=CARTESIAN_POINT('',(112.824705251554,-0.549999999999986,48.4446186903817));
#200037=CARTESIAN_POINT('Origin',(112.824705251554,-1.05,48.4446186903817));
#200038=CARTESIAN_POINT('',(112.333891749004,-1.05,48.3492137339324));
#200039=CARTESIAN_POINT('',(112.276648775135,-1.05,48.6437018354621));
#200040=CARTESIAN_POINT('',(112.333891749004,-1.05,48.3492137339324));
#200041=CARTESIAN_POINT('',(112.767462277684,-1.05,48.7391067919114));
#200042=CARTESIAN_POINT('',(112.824705251554,-1.05,48.4446186903817));
#200043=CARTESIAN_POINT('Origin',(112.333891749004,-1.05,48.3492137339324));
#200044=CARTESIAN_POINT('',(112.276648775135,-1.05,48.6437018354621));
#200045=CARTESIAN_POINT('',(112.333891749004,-1.05,48.3492137339324));
#200046=CARTESIAN_POINT('Origin',(112.333891749004,-1.35,48.3492137339324));
#200047=CARTESIAN_POINT('',(112.824705251554,-1.35,48.4446186903817));
#200048=CARTESIAN_POINT('',(112.767462277684,-1.35,48.7391067919114));
#200049=CARTESIAN_POINT('',(112.824705251554,-1.35,48.4446186903817));
#200050=CARTESIAN_POINT('',(112.276648775135,-1.35,48.6437018354621));
#200051=CARTESIAN_POINT('',(112.276648775135,-1.35,48.6437018354621));
#200052=CARTESIAN_POINT('',(112.333891749004,-1.35,48.3492137339324));
#200053=CARTESIAN_POINT('',(112.333891749004,-1.35,48.3492137339324));
#200054=CARTESIAN_POINT('',(112.333891749004,-1.35,48.3492137339324));
#200055=CARTESIAN_POINT('Origin',(112.824705251554,-1.35,48.4446186903817));
#200056=CARTESIAN_POINT('',(112.824705251554,-1.85,48.4446186903817));
#200057=CARTESIAN_POINT('',(112.767462277684,-1.85,48.7391067919114));
#200058=CARTESIAN_POINT('',(112.824705251554,-1.85,48.4446186903817));
#200059=CARTESIAN_POINT('',(112.767462277684,-1.35,48.7391067919114));
#200060=CARTESIAN_POINT('',(112.824705251554,-1.35,48.4446186903817));
#200061=CARTESIAN_POINT('Origin',(112.824705251554,-1.85,48.4446186903817));
#200062=CARTESIAN_POINT('',(112.333891749004,-1.85,48.3492137339324));
#200063=CARTESIAN_POINT('',(112.276648775135,-1.85,48.6437018354621));
#200064=CARTESIAN_POINT('',(112.333891749004,-1.85,48.3492137339324));
#200065=CARTESIAN_POINT('',(112.767462277684,-1.85,48.7391067919114));
#200066=CARTESIAN_POINT('',(112.824705251554,-1.85,48.4446186903817));
#200067=CARTESIAN_POINT('Origin',(112.333891749004,-1.85,48.3492137339324));
#200068=CARTESIAN_POINT('',(112.276648775135,-1.85,48.6437018354621));
#200069=CARTESIAN_POINT('',(112.333891749004,-1.85,48.3492137339324));
#200070=CARTESIAN_POINT('Origin',(112.333891749004,-2.15,48.3492137339324));
#200071=CARTESIAN_POINT('',(112.824705251554,-2.15,48.4446186903817));
#200072=CARTESIAN_POINT('',(112.767462277684,-2.15,48.7391067919114));
#200073=CARTESIAN_POINT('',(112.824705251554,-2.15,48.4446186903817));
#200074=CARTESIAN_POINT('',(112.276648775135,-2.15,48.6437018354621));
#200075=CARTESIAN_POINT('',(112.276648775135,-2.15,48.6437018354621));
#200076=CARTESIAN_POINT('',(112.333891749004,-2.15,48.3492137339324));
#200077=CARTESIAN_POINT('',(112.333891749004,-2.15,48.3492137339324));
#200078=CARTESIAN_POINT('',(112.333891749004,-2.15,48.3492137339324));
#200079=CARTESIAN_POINT('Origin',(112.824705251554,-2.15,48.4446186903817));
#200080=CARTESIAN_POINT('',(112.824705251554,-2.65,48.4446186903817));
#200081=CARTESIAN_POINT('',(112.767462277684,-2.65,48.7391067919114));
#200082=CARTESIAN_POINT('',(112.824705251554,-2.65,48.4446186903817));
#200083=CARTESIAN_POINT('',(112.767462277684,-2.15,48.7391067919114));
#200084=CARTESIAN_POINT('',(112.824705251554,-2.15,48.4446186903817));
#200085=CARTESIAN_POINT('Origin',(112.824705251554,-2.65,48.4446186903817));
#200086=CARTESIAN_POINT('',(112.333891749004,-2.65,48.3492137339324));
#200087=CARTESIAN_POINT('',(112.276648775135,-2.65,48.6437018354621));
#200088=CARTESIAN_POINT('',(112.333891749004,-2.65,48.3492137339324));
#200089=CARTESIAN_POINT('',(112.767462277684,-2.65,48.7391067919114));
#200090=CARTESIAN_POINT('',(112.824705251554,-2.65,48.4446186903817));
#200091=CARTESIAN_POINT('Origin',(112.333891749004,-2.65,48.3492137339324));
#200092=CARTESIAN_POINT('',(112.276648775135,-2.65,48.6437018354621));
#200093=CARTESIAN_POINT('',(112.333891749004,-2.65,48.3492137339324));
#200094=CARTESIAN_POINT('Origin',(112.333891749004,-2.95,48.3492137339324));
#200095=CARTESIAN_POINT('',(112.824705251554,-2.95,48.4446186903817));
#200096=CARTESIAN_POINT('',(112.767462277684,-2.95,48.7391067919114));
#200097=CARTESIAN_POINT('',(112.824705251554,-2.95,48.4446186903817));
#200098=CARTESIAN_POINT('',(112.276648775135,-2.95,48.6437018354621));
#200099=CARTESIAN_POINT('',(112.276648775135,-2.95,48.6437018354621));
#200100=CARTESIAN_POINT('',(112.333891749004,-2.95,48.3492137339324));
#200101=CARTESIAN_POINT('',(112.333891749004,-2.95,48.3492137339324));
#200102=CARTESIAN_POINT('',(112.333891749004,-2.95,48.3492137339324));
#200103=CARTESIAN_POINT('Origin',(112.824705251554,-2.95,48.4446186903817));
#200104=CARTESIAN_POINT('',(112.824705251554,-3.45,48.4446186903817));
#200105=CARTESIAN_POINT('',(112.767462277684,-3.45,48.7391067919114));
#200106=CARTESIAN_POINT('',(112.824705251554,-3.45,48.4446186903817));
#200107=CARTESIAN_POINT('',(112.767462277684,-2.95,48.7391067919114));
#200108=CARTESIAN_POINT('',(112.824705251554,-2.95,48.4446186903817));
#200109=CARTESIAN_POINT('Origin',(112.824705251554,-3.45,48.4446186903817));
#200110=CARTESIAN_POINT('',(112.333891749004,-3.45,48.3492137339324));
#200111=CARTESIAN_POINT('',(112.276648775135,-3.45,48.6437018354621));
#200112=CARTESIAN_POINT('',(112.333891749004,-3.45,48.3492137339324));
#200113=CARTESIAN_POINT('',(112.767462277684,-3.45,48.7391067919114));
#200114=CARTESIAN_POINT('',(112.824705251554,-3.45,48.4446186903817));
#200115=CARTESIAN_POINT('Origin',(112.333891749004,-3.45,48.3492137339324));
#200116=CARTESIAN_POINT('',(112.276648775135,-3.45,48.6437018354621));
#200117=CARTESIAN_POINT('',(112.333891749004,-3.45,48.3492137339324));
#200118=CARTESIAN_POINT('Origin',(112.333891749004,-3.75,48.3492137339324));
#200119=CARTESIAN_POINT('',(112.824705251554,-3.75,48.4446186903817));
#200120=CARTESIAN_POINT('',(112.767462277684,-3.75,48.7391067919114));
#200121=CARTESIAN_POINT('',(112.824705251554,-3.75,48.4446186903817));
#200122=CARTESIAN_POINT('',(112.276648775135,-3.75,48.6437018354621));
#200123=CARTESIAN_POINT('',(112.276648775135,-3.75,48.6437018354621));
#200124=CARTESIAN_POINT('',(112.333891749004,-3.75,48.3492137339324));
#200125=CARTESIAN_POINT('',(112.333891749004,-3.75,48.3492137339324));
#200126=CARTESIAN_POINT('',(112.333891749004,-3.75,48.3492137339324));
#200127=CARTESIAN_POINT('Origin',(112.824705251554,-3.75,48.4446186903817));
#200128=CARTESIAN_POINT('',(112.824705251554,-4.25,48.4446186903817));
#200129=CARTESIAN_POINT('',(112.767462277684,-4.25,48.7391067919114));
#200130=CARTESIAN_POINT('',(112.824705251554,-4.25,48.4446186903817));
#200131=CARTESIAN_POINT('',(112.767462277684,-3.75,48.7391067919114));
#200132=CARTESIAN_POINT('',(112.824705251554,-3.75,48.4446186903817));
#200133=CARTESIAN_POINT('Origin',(112.824705251554,-4.25,48.4446186903817));
#200134=CARTESIAN_POINT('',(112.333891749004,-4.25,48.3492137339324));
#200135=CARTESIAN_POINT('',(112.276648775135,-4.25,48.6437018354621));
#200136=CARTESIAN_POINT('',(112.333891749004,-4.25,48.3492137339324));
#200137=CARTESIAN_POINT('',(112.767462277684,-4.25,48.7391067919114));
#200138=CARTESIAN_POINT('',(112.824705251554,-4.25,48.4446186903817));
#200139=CARTESIAN_POINT('Origin',(112.333891749004,-4.25,48.3492137339324));
#200140=CARTESIAN_POINT('',(112.276648775135,-4.25,48.6437018354621));
#200141=CARTESIAN_POINT('',(112.333891749004,-4.25,48.3492137339324));
#200142=CARTESIAN_POINT('Origin',(112.333891749004,-4.55,48.3492137339324));
#200143=CARTESIAN_POINT('',(112.824705251554,-4.55,48.4446186903817));
#200144=CARTESIAN_POINT('',(112.767462277684,-4.55,48.7391067919114));
#200145=CARTESIAN_POINT('',(112.824705251554,-4.55,48.4446186903817));
#200146=CARTESIAN_POINT('',(112.276648775135,-4.55,48.6437018354621));
#200147=CARTESIAN_POINT('',(112.276648775135,-4.55,48.6437018354621));
#200148=CARTESIAN_POINT('',(112.333891749004,-4.55,48.3492137339324));
#200149=CARTESIAN_POINT('',(112.333891749004,-4.55,48.3492137339324));
#200150=CARTESIAN_POINT('',(112.333891749004,-4.55,48.3492137339324));
#200151=CARTESIAN_POINT('Origin',(112.824705251554,-4.55,48.4446186903817));
#200152=CARTESIAN_POINT('',(112.824705251554,-5.05,48.4446186903817));
#200153=CARTESIAN_POINT('',(112.767462277684,-5.05,48.7391067919114));
#200154=CARTESIAN_POINT('',(112.824705251554,-5.05,48.4446186903817));
#200155=CARTESIAN_POINT('',(112.767462277684,-4.55,48.7391067919114));
#200156=CARTESIAN_POINT('',(112.824705251554,-4.55,48.4446186903817));
#200157=CARTESIAN_POINT('Origin',(112.824705251554,-5.05,48.4446186903817));
#200158=CARTESIAN_POINT('',(112.333891749004,-5.05,48.3492137339324));
#200159=CARTESIAN_POINT('',(112.276648775135,-5.05,48.6437018354621));
#200160=CARTESIAN_POINT('',(112.333891749004,-5.05,48.3492137339324));
#200161=CARTESIAN_POINT('',(112.767462277684,-5.05,48.7391067919114));
#200162=CARTESIAN_POINT('',(112.824705251554,-5.05,48.4446186903817));
#200163=CARTESIAN_POINT('Origin',(112.333891749004,-5.05,48.3492137339324));
#200164=CARTESIAN_POINT('',(112.276648775135,-5.05,48.6437018354621));
#200165=CARTESIAN_POINT('',(112.333891749004,-5.05,48.3492137339324));
#200166=CARTESIAN_POINT('Origin',(113.119193353083,-4.55,48.5018616642512));
#200167=CARTESIAN_POINT('',(113.610006855633,-4.55,48.5972666207005));
#200168=CARTESIAN_POINT('',(113.552763881763,-4.55,48.8917547222302));
#200169=CARTESIAN_POINT('',(113.610006855633,-4.55,48.5972666207005));
#200170=CARTESIAN_POINT('',(113.061950379214,-4.55,48.7963497657809));
#200171=CARTESIAN_POINT('',(113.061950379214,-4.55,48.7963497657809));
#200172=CARTESIAN_POINT('',(113.119193353083,-4.55,48.5018616642512));
#200173=CARTESIAN_POINT('',(113.119193353083,-4.55,48.5018616642512));
#200174=CARTESIAN_POINT('',(113.119193353083,-4.55,48.5018616642512));
#200175=CARTESIAN_POINT('Origin',(113.610006855633,-4.55,48.5972666207005));
#200176=CARTESIAN_POINT('',(113.610006855633,-5.05,48.5972666207005));
#200177=CARTESIAN_POINT('',(113.552763881763,-5.05,48.8917547222302));
#200178=CARTESIAN_POINT('',(113.610006855633,-5.05,48.5972666207005));
#200179=CARTESIAN_POINT('',(113.552763881763,-4.55,48.8917547222302));
#200180=CARTESIAN_POINT('',(113.610006855633,-4.55,48.5972666207005));
#200181=CARTESIAN_POINT('Origin',(113.610006855633,-5.05,48.5972666207005));
#200182=CARTESIAN_POINT('',(113.119193353083,-5.05,48.5018616642512));
#200183=CARTESIAN_POINT('',(113.061950379214,-5.05,48.7963497657809));
#200184=CARTESIAN_POINT('',(113.119193353083,-5.05,48.5018616642512));
#200185=CARTESIAN_POINT('',(113.552763881763,-5.05,48.8917547222302));
#200186=CARTESIAN_POINT('',(113.610006855633,-5.05,48.5972666207005));
#200187=CARTESIAN_POINT('Origin',(113.119193353083,-5.05,48.5018616642512));
#200188=CARTESIAN_POINT('',(113.061950379214,-5.05,48.7963497657809));
#200189=CARTESIAN_POINT('',(113.119193353083,-5.05,48.5018616642512));
#200190=CARTESIAN_POINT('Origin',(113.904494957163,-4.55,48.65450959457));
#200191=CARTESIAN_POINT('',(114.395308459712,-4.55,48.7499145510193));
#200192=CARTESIAN_POINT('',(114.338065485842,-4.55,49.044402652549));
#200193=CARTESIAN_POINT('',(114.395308459712,-4.55,48.7499145510193));
#200194=CARTESIAN_POINT('',(113.847251983293,-4.55,48.9489976960997));
#200195=CARTESIAN_POINT('',(113.847251983293,-4.55,48.9489976960997));
#200196=CARTESIAN_POINT('',(113.904494957163,-4.55,48.65450959457));
#200197=CARTESIAN_POINT('',(113.904494957163,-4.55,48.65450959457));
#200198=CARTESIAN_POINT('',(113.904494957163,-4.55,48.65450959457));
#200199=CARTESIAN_POINT('Origin',(114.395308459712,-4.55,48.7499145510193));
#200200=CARTESIAN_POINT('',(114.395308459712,-5.05,48.7499145510193));
#200201=CARTESIAN_POINT('',(114.338065485842,-5.05,49.044402652549));
#200202=CARTESIAN_POINT('',(114.395308459712,-5.05,48.7499145510193));
#200203=CARTESIAN_POINT('',(114.338065485842,-4.55,49.044402652549));
#200204=CARTESIAN_POINT('',(114.395308459712,-4.55,48.7499145510193));
#200205=CARTESIAN_POINT('Origin',(114.395308459712,-5.05,48.7499145510193));
#200206=CARTESIAN_POINT('',(113.904494957163,-5.05,48.65450959457));
#200207=CARTESIAN_POINT('',(113.847251983293,-5.05,48.9489976960997));
#200208=CARTESIAN_POINT('',(113.904494957163,-5.05,48.65450959457));
#200209=CARTESIAN_POINT('',(114.338065485842,-5.05,49.044402652549));
#200210=CARTESIAN_POINT('',(114.395308459712,-5.05,48.7499145510193));
#200211=CARTESIAN_POINT('Origin',(113.904494957163,-5.05,48.65450959457));
#200212=CARTESIAN_POINT('',(113.847251983293,-5.05,48.9489976960997));
#200213=CARTESIAN_POINT('',(113.904494957163,-5.05,48.65450959457));
#200214=CARTESIAN_POINT('Origin',(114.689796561242,-4.55,48.8071575248888));
#200215=CARTESIAN_POINT('',(115.180610063791,-4.55,48.9025624813381));
#200216=CARTESIAN_POINT('',(115.123367089922,-4.55,49.1970505828678));
#200217=CARTESIAN_POINT('',(115.180610063791,-4.55,48.9025624813381));
#200218=CARTESIAN_POINT('',(114.632553587372,-4.55,49.1016456264185));
#200219=CARTESIAN_POINT('',(114.632553587372,-4.55,49.1016456264185));
#200220=CARTESIAN_POINT('',(114.689796561242,-4.55,48.8071575248888));
#200221=CARTESIAN_POINT('',(114.689796561242,-4.55,48.8071575248888));
#200222=CARTESIAN_POINT('',(114.689796561242,-4.55,48.8071575248888));
#200223=CARTESIAN_POINT('Origin',(115.180610063791,-4.55,48.9025624813381));
#200224=CARTESIAN_POINT('',(115.180610063791,-5.05,48.9025624813381));
#200225=CARTESIAN_POINT('',(115.123367089922,-5.05,49.1970505828678));
#200226=CARTESIAN_POINT('',(115.180610063791,-5.05,48.9025624813381));
#200227=CARTESIAN_POINT('',(115.123367089922,-4.55,49.1970505828678));
#200228=CARTESIAN_POINT('',(115.180610063791,-4.55,48.9025624813381));
#200229=CARTESIAN_POINT('Origin',(115.180610063791,-5.05,48.9025624813381));
#200230=CARTESIAN_POINT('',(114.689796561242,-5.05,48.8071575248888));
#200231=CARTESIAN_POINT('',(114.632553587372,-5.05,49.1016456264185));
#200232=CARTESIAN_POINT('',(114.689796561242,-5.05,48.8071575248888));
#200233=CARTESIAN_POINT('',(115.123367089922,-5.05,49.1970505828678));
#200234=CARTESIAN_POINT('',(115.180610063791,-5.05,48.9025624813381));
#200235=CARTESIAN_POINT('Origin',(114.689796561242,-5.05,48.8071575248888));
#200236=CARTESIAN_POINT('',(114.632553587372,-5.05,49.1016456264185));
#200237=CARTESIAN_POINT('',(114.689796561242,-5.05,48.8071575248888));
#200238=CARTESIAN_POINT('Origin',(115.475098165321,-4.55,48.9598054552076));
#200239=CARTESIAN_POINT('',(115.96591166787,-4.55,49.0552104116569));
#200240=CARTESIAN_POINT('',(115.908668694001,-4.55,49.3496985131866));
#200241=CARTESIAN_POINT('',(115.96591166787,-4.55,49.0552104116569));
#200242=CARTESIAN_POINT('',(115.417855191451,-4.55,49.2542935567373));
#200243=CARTESIAN_POINT('',(115.417855191451,-4.55,49.2542935567373));
#200244=CARTESIAN_POINT('',(115.475098165321,-4.55,48.9598054552076));
#200245=CARTESIAN_POINT('',(115.475098165321,-4.55,48.9598054552076));
#200246=CARTESIAN_POINT('',(115.475098165321,-4.55,48.9598054552076));
#200247=CARTESIAN_POINT('Origin',(115.96591166787,-4.55,49.0552104116569));
#200248=CARTESIAN_POINT('',(115.96591166787,-5.05,49.0552104116569));
#200249=CARTESIAN_POINT('',(115.908668694001,-5.05,49.3496985131866));
#200250=CARTESIAN_POINT('',(115.96591166787,-5.05,49.0552104116569));
#200251=CARTESIAN_POINT('',(115.908668694001,-4.55,49.3496985131866));
#200252=CARTESIAN_POINT('',(115.96591166787,-4.55,49.0552104116569));
#200253=CARTESIAN_POINT('Origin',(115.96591166787,-5.05,49.0552104116569));
#200254=CARTESIAN_POINT('',(115.475098165321,-5.05,48.9598054552076));
#200255=CARTESIAN_POINT('',(115.417855191451,-5.05,49.2542935567373));
#200256=CARTESIAN_POINT('',(115.475098165321,-5.05,48.9598054552076));
#200257=CARTESIAN_POINT('',(115.908668694001,-5.05,49.3496985131866));
#200258=CARTESIAN_POINT('',(115.96591166787,-5.05,49.0552104116569));
#200259=CARTESIAN_POINT('Origin',(115.475098165321,-5.05,48.9598054552076));
#200260=CARTESIAN_POINT('',(115.417855191451,-5.05,49.2542935567373));
#200261=CARTESIAN_POINT('',(115.475098165321,-5.05,48.9598054552076));
#200262=CARTESIAN_POINT('Origin',(116.2603997694,-4.55,49.1124533855264));
#200263=CARTESIAN_POINT('',(116.75121327195,-4.55,49.2078583419757));
#200264=CARTESIAN_POINT('',(116.69397029808,-4.55,49.5023464435054));
#200265=CARTESIAN_POINT('',(116.75121327195,-4.55,49.2078583419757));
#200266=CARTESIAN_POINT('',(116.203156795531,-4.55,49.4069414870561));
#200267=CARTESIAN_POINT('',(116.203156795531,-4.55,49.4069414870561));
#200268=CARTESIAN_POINT('',(116.2603997694,-4.55,49.1124533855264));
#200269=CARTESIAN_POINT('',(116.2603997694,-4.55,49.1124533855264));
#200270=CARTESIAN_POINT('',(116.2603997694,-4.55,49.1124533855264));
#200271=CARTESIAN_POINT('Origin',(116.75121327195,-4.55,49.2078583419757));
#200272=CARTESIAN_POINT('',(116.75121327195,-5.05,49.2078583419757));
#200273=CARTESIAN_POINT('',(116.69397029808,-5.05,49.5023464435054));
#200274=CARTESIAN_POINT('',(116.75121327195,-5.05,49.2078583419757));
#200275=CARTESIAN_POINT('',(116.69397029808,-4.55,49.5023464435054));
#200276=CARTESIAN_POINT('',(116.75121327195,-4.55,49.2078583419757));
#200277=CARTESIAN_POINT('Origin',(116.75121327195,-5.05,49.2078583419757));
#200278=CARTESIAN_POINT('',(116.2603997694,-5.05,49.1124533855264));
#200279=CARTESIAN_POINT('',(116.203156795531,-5.05,49.4069414870561));
#200280=CARTESIAN_POINT('',(116.2603997694,-5.05,49.1124533855264));
#200281=CARTESIAN_POINT('',(116.69397029808,-5.05,49.5023464435054));
#200282=CARTESIAN_POINT('',(116.75121327195,-5.05,49.2078583419757));
#200283=CARTESIAN_POINT('Origin',(116.2603997694,-5.05,49.1124533855264));
#200284=CARTESIAN_POINT('',(116.203156795531,-5.05,49.4069414870561));
#200285=CARTESIAN_POINT('',(116.2603997694,-5.05,49.1124533855264));
#200286=CARTESIAN_POINT('Origin',(117.045701373479,-4.55,49.2651013158452));
#200287=CARTESIAN_POINT('',(117.536514876029,-4.55,49.3605062722945));
#200288=CARTESIAN_POINT('',(117.479271902159,-4.55,49.6549943738242));
#200289=CARTESIAN_POINT('',(117.536514876029,-4.55,49.3605062722945));
#200290=CARTESIAN_POINT('',(116.98845839961,-4.55,49.5595894173749));
#200291=CARTESIAN_POINT('',(116.98845839961,-4.55,49.5595894173749));
#200292=CARTESIAN_POINT('',(117.045701373479,-4.55,49.2651013158452));
#200293=CARTESIAN_POINT('',(117.045701373479,-4.55,49.2651013158452));
#200294=CARTESIAN_POINT('',(117.045701373479,-4.55,49.2651013158452));
#200295=CARTESIAN_POINT('Origin',(117.536514876029,-4.55,49.3605062722945));
#200296=CARTESIAN_POINT('',(117.536514876029,-5.05,49.3605062722945));
#200297=CARTESIAN_POINT('',(117.479271902159,-5.05,49.6549943738242));
#200298=CARTESIAN_POINT('',(117.536514876029,-5.05,49.3605062722945));
#200299=CARTESIAN_POINT('',(117.479271902159,-4.55,49.6549943738242));
#200300=CARTESIAN_POINT('',(117.536514876029,-4.55,49.3605062722945));
#200301=CARTESIAN_POINT('Origin',(117.536514876029,-5.05,49.3605062722945));
#200302=CARTESIAN_POINT('',(117.045701373479,-5.05,49.2651013158452));
#200303=CARTESIAN_POINT('',(116.98845839961,-5.05,49.5595894173749));
#200304=CARTESIAN_POINT('',(117.045701373479,-5.05,49.2651013158452));
#200305=CARTESIAN_POINT('',(117.479271902159,-5.05,49.6549943738242));
#200306=CARTESIAN_POINT('',(117.536514876029,-5.05,49.3605062722945));
#200307=CARTESIAN_POINT('Origin',(117.045701373479,-5.05,49.2651013158452));
#200308=CARTESIAN_POINT('',(116.98845839961,-5.05,49.5595894173749));
#200309=CARTESIAN_POINT('',(117.045701373479,-5.05,49.2651013158452));
#200310=CARTESIAN_POINT('Origin',(117.831002977559,-4.55,49.417749246164));
#200311=CARTESIAN_POINT('',(118.321816480108,-4.55,49.5131542026133));
#200312=CARTESIAN_POINT('',(118.264573506239,-4.55,49.807642304143));
#200313=CARTESIAN_POINT('',(118.321816480108,-4.55,49.5131542026133));
#200314=CARTESIAN_POINT('',(117.773760003689,-4.55,49.7122373476937));
#200315=CARTESIAN_POINT('',(117.773760003689,-4.55,49.7122373476937));
#200316=CARTESIAN_POINT('',(117.831002977559,-4.55,49.417749246164));
#200317=CARTESIAN_POINT('',(117.831002977559,-4.55,49.417749246164));
#200318=CARTESIAN_POINT('',(117.831002977559,-4.55,49.417749246164));
#200319=CARTESIAN_POINT('Origin',(118.321816480108,-4.55,49.5131542026133));
#200320=CARTESIAN_POINT('',(118.321816480108,-5.05,49.5131542026133));
#200321=CARTESIAN_POINT('',(118.264573506239,-5.05,49.807642304143));
#200322=CARTESIAN_POINT('',(118.321816480108,-5.05,49.5131542026133));
#200323=CARTESIAN_POINT('',(118.264573506239,-4.55,49.807642304143));
#200324=CARTESIAN_POINT('',(118.321816480108,-4.55,49.5131542026133));
#200325=CARTESIAN_POINT('Origin',(118.321816480108,-5.05,49.5131542026133));
#200326=CARTESIAN_POINT('',(117.831002977559,-5.05,49.417749246164));
#200327=CARTESIAN_POINT('',(117.773760003689,-5.05,49.7122373476937));
#200328=CARTESIAN_POINT('',(117.831002977559,-5.05,49.417749246164));
#200329=CARTESIAN_POINT('',(118.264573506239,-5.05,49.807642304143));
#200330=CARTESIAN_POINT('',(118.321816480108,-5.05,49.5131542026133));
#200331=CARTESIAN_POINT('Origin',(117.831002977559,-5.05,49.417749246164));
#200332=CARTESIAN_POINT('',(117.773760003689,-5.05,49.7122373476937));
#200333=CARTESIAN_POINT('',(117.831002977559,-5.05,49.417749246164));
#200334=CARTESIAN_POINT('Origin',(118.616304581638,-4.55,49.5703971764828));
#200335=CARTESIAN_POINT('',(119.107118084187,-4.55,49.6658021329321));
#200336=CARTESIAN_POINT('',(119.049875110318,-4.55,49.9602902344618));
#200337=CARTESIAN_POINT('',(119.107118084187,-4.55,49.6658021329321));
#200338=CARTESIAN_POINT('',(118.559061607768,-4.55,49.8648852780125));
#200339=CARTESIAN_POINT('',(118.559061607768,-4.55,49.8648852780125));
#200340=CARTESIAN_POINT('',(118.616304581638,-4.55,49.5703971764828));
#200341=CARTESIAN_POINT('',(118.616304581638,-4.55,49.5703971764828));
#200342=CARTESIAN_POINT('',(118.616304581638,-4.55,49.5703971764828));
#200343=CARTESIAN_POINT('Origin',(119.107118084187,-4.55,49.6658021329321));
#200344=CARTESIAN_POINT('',(119.107118084187,-5.05,49.6658021329321));
#200345=CARTESIAN_POINT('',(119.049875110318,-5.05,49.9602902344618));
#200346=CARTESIAN_POINT('',(119.107118084187,-5.05,49.6658021329321));
#200347=CARTESIAN_POINT('',(119.049875110318,-4.55,49.9602902344618));
#200348=CARTESIAN_POINT('',(119.107118084187,-4.55,49.6658021329321));
#200349=CARTESIAN_POINT('Origin',(119.107118084187,-5.05,49.6658021329321));
#200350=CARTESIAN_POINT('',(118.616304581638,-5.05,49.5703971764828));
#200351=CARTESIAN_POINT('',(118.559061607768,-5.05,49.8648852780125));
#200352=CARTESIAN_POINT('',(118.616304581638,-5.05,49.5703971764828));
#200353=CARTESIAN_POINT('',(119.049875110318,-5.05,49.9602902344618));
#200354=CARTESIAN_POINT('',(119.107118084187,-5.05,49.6658021329321));
#200355=CARTESIAN_POINT('Origin',(118.616304581638,-5.05,49.5703971764828));
#200356=CARTESIAN_POINT('',(118.559061607768,-5.05,49.8648852780125));
#200357=CARTESIAN_POINT('',(118.616304581638,-5.05,49.5703971764828));
#200358=CARTESIAN_POINT('Origin',(119.401606185717,-4.55,49.7230451068016));
#200359=CARTESIAN_POINT('',(119.892419688267,-4.55,49.8184500632509));
#200360=CARTESIAN_POINT('',(119.835176714397,-4.55,50.1129381647806));
#200361=CARTESIAN_POINT('',(119.892419688267,-4.55,49.8184500632509));
#200362=CARTESIAN_POINT('',(119.344363211847,-4.55,50.0175332083313));
#200363=CARTESIAN_POINT('',(119.344363211847,-4.55,50.0175332083313));
#200364=CARTESIAN_POINT('',(119.401606185717,-4.55,49.7230451068016));
#200365=CARTESIAN_POINT('',(119.401606185717,-4.55,49.7230451068016));
#200366=CARTESIAN_POINT('',(119.401606185717,-4.55,49.7230451068016));
#200367=CARTESIAN_POINT('Origin',(119.892419688267,-4.55,49.8184500632509));
#200368=CARTESIAN_POINT('',(119.892419688267,-5.05,49.8184500632509));
#200369=CARTESIAN_POINT('',(119.835176714397,-5.05,50.1129381647806));
#200370=CARTESIAN_POINT('',(119.892419688267,-5.05,49.8184500632509));
#200371=CARTESIAN_POINT('',(119.835176714397,-4.55,50.1129381647806));
#200372=CARTESIAN_POINT('',(119.892419688267,-4.55,49.8184500632509));
#200373=CARTESIAN_POINT('Origin',(119.892419688267,-5.05,49.8184500632509));
#200374=CARTESIAN_POINT('',(119.401606185717,-5.05,49.7230451068016));
#200375=CARTESIAN_POINT('',(119.344363211847,-5.05,50.0175332083313));
#200376=CARTESIAN_POINT('',(119.401606185717,-5.05,49.7230451068016));
#200377=CARTESIAN_POINT('',(119.835176714397,-5.05,50.1129381647806));
#200378=CARTESIAN_POINT('',(119.892419688267,-5.05,49.8184500632509));
#200379=CARTESIAN_POINT('Origin',(119.401606185717,-5.05,49.7230451068016));
#200380=CARTESIAN_POINT('',(119.344363211847,-5.05,50.0175332083313));
#200381=CARTESIAN_POINT('',(119.401606185717,-5.05,49.7230451068016));
#200382=CARTESIAN_POINT('Origin',(120.186907789796,-4.55,49.8756930371204));
#200383=CARTESIAN_POINT('',(120.677721292346,-4.55,49.9710979935697));
#200384=CARTESIAN_POINT('',(120.620478318476,-4.55,50.2655860950994));
#200385=CARTESIAN_POINT('',(120.677721292346,-4.55,49.9710979935697));
#200386=CARTESIAN_POINT('',(120.129664815927,-4.55,50.1701811386501));
#200387=CARTESIAN_POINT('',(120.129664815927,-4.55,50.1701811386501));
#200388=CARTESIAN_POINT('',(120.186907789796,-4.55,49.8756930371204));
#200389=CARTESIAN_POINT('',(120.186907789796,-4.55,49.8756930371204));
#200390=CARTESIAN_POINT('',(120.186907789796,-4.55,49.8756930371204));
#200391=CARTESIAN_POINT('Origin',(120.677721292346,-4.55,49.9710979935697));
#200392=CARTESIAN_POINT('',(120.677721292346,-5.05,49.9710979935697));
#200393=CARTESIAN_POINT('',(120.620478318476,-5.05,50.2655860950994));
#200394=CARTESIAN_POINT('',(120.677721292346,-5.05,49.9710979935697));
#200395=CARTESIAN_POINT('',(120.620478318476,-4.55,50.2655860950994));
#200396=CARTESIAN_POINT('',(120.677721292346,-4.55,49.9710979935697));
#200397=CARTESIAN_POINT('Origin',(120.677721292346,-5.05,49.9710979935697));
#200398=CARTESIAN_POINT('',(120.186907789796,-5.05,49.8756930371204));
#200399=CARTESIAN_POINT('',(120.129664815927,-5.05,50.1701811386501));
#200400=CARTESIAN_POINT('',(120.186907789796,-5.05,49.8756930371204));
#200401=CARTESIAN_POINT('',(120.620478318476,-5.05,50.2655860950994));
#200402=CARTESIAN_POINT('',(120.677721292346,-5.05,49.9710979935697));
#200403=CARTESIAN_POINT('Origin',(120.186907789796,-5.05,49.8756930371204));
#200404=CARTESIAN_POINT('',(120.129664815927,-5.05,50.1701811386501));
#200405=CARTESIAN_POINT('',(120.186907789796,-5.05,49.8756930371204));
#200406=CARTESIAN_POINT('Origin',(120.972209393875,-4.55,50.0283409674392));
#200407=CARTESIAN_POINT('',(121.463022896425,-4.55,50.1237459238885));
#200408=CARTESIAN_POINT('',(121.405779922555,-4.55,50.4182340254182));
#200409=CARTESIAN_POINT('',(121.463022896425,-4.55,50.1237459238885));
#200410=CARTESIAN_POINT('',(120.914966420006,-4.55,50.3228290689689));
#200411=CARTESIAN_POINT('',(120.914966420006,-4.55,50.3228290689689));
#200412=CARTESIAN_POINT('',(120.972209393875,-4.55,50.0283409674392));
#200413=CARTESIAN_POINT('',(120.972209393875,-4.55,50.0283409674392));
#200414=CARTESIAN_POINT('',(120.972209393875,-4.55,50.0283409674392));
#200415=CARTESIAN_POINT('Origin',(121.463022896425,-4.55,50.1237459238885));
#200416=CARTESIAN_POINT('',(121.463022896425,-5.05,50.1237459238885));
#200417=CARTESIAN_POINT('',(121.405779922555,-5.05,50.4182340254182));
#200418=CARTESIAN_POINT('',(121.463022896425,-5.05,50.1237459238885));
#200419=CARTESIAN_POINT('',(121.405779922555,-4.55,50.4182340254182));
#200420=CARTESIAN_POINT('',(121.463022896425,-4.55,50.1237459238885));
#200421=CARTESIAN_POINT('Origin',(121.463022896425,-5.05,50.1237459238885));
#200422=CARTESIAN_POINT('',(120.972209393875,-5.05,50.0283409674392));
#200423=CARTESIAN_POINT('',(120.914966420006,-5.05,50.3228290689689));
#200424=CARTESIAN_POINT('',(120.972209393875,-5.05,50.0283409674392));
#200425=CARTESIAN_POINT('',(121.405779922555,-5.05,50.4182340254182));
#200426=CARTESIAN_POINT('',(121.463022896425,-5.05,50.1237459238885));
#200427=CARTESIAN_POINT('Origin',(120.972209393875,-5.05,50.0283409674392));
#200428=CARTESIAN_POINT('',(120.914966420006,-5.05,50.3228290689689));
#200429=CARTESIAN_POINT('',(120.972209393875,-5.05,50.0283409674392));
#200430=CARTESIAN_POINT('Origin',(121.757510997955,-4.55,50.180988897758));
#200431=CARTESIAN_POINT('',(122.248324500504,-4.55,50.2763938542073));
#200432=CARTESIAN_POINT('',(122.191081526635,-4.55,50.570881955737));
#200433=CARTESIAN_POINT('',(122.248324500504,-4.55,50.2763938542073));
#200434=CARTESIAN_POINT('',(121.700268024085,-4.55,50.4754769992877));
#200435=CARTESIAN_POINT('',(121.700268024085,-4.55,50.4754769992877));
#200436=CARTESIAN_POINT('',(121.757510997955,-4.55,50.180988897758));
#200437=CARTESIAN_POINT('',(121.757510997955,-4.55,50.180988897758));
#200438=CARTESIAN_POINT('',(121.757510997955,-4.55,50.180988897758));
#200439=CARTESIAN_POINT('Origin',(122.248324500504,-4.55,50.2763938542073));
#200440=CARTESIAN_POINT('',(122.248324500504,-5.05,50.2763938542073));
#200441=CARTESIAN_POINT('',(122.191081526635,-5.05,50.570881955737));
#200442=CARTESIAN_POINT('',(122.248324500504,-5.05,50.2763938542073));
#200443=CARTESIAN_POINT('',(122.191081526635,-4.55,50.570881955737));
#200444=CARTESIAN_POINT('',(122.248324500504,-4.55,50.2763938542073));
#200445=CARTESIAN_POINT('Origin',(122.248324500504,-5.05,50.2763938542073));
#200446=CARTESIAN_POINT('',(121.757510997955,-5.05,50.180988897758));
#200447=CARTESIAN_POINT('',(121.700268024085,-5.05,50.4754769992877));
#200448=CARTESIAN_POINT('',(121.757510997955,-5.05,50.180988897758));
#200449=CARTESIAN_POINT('',(122.191081526635,-5.05,50.570881955737));
#200450=CARTESIAN_POINT('',(122.248324500504,-5.05,50.2763938542073));
#200451=CARTESIAN_POINT('Origin',(121.757510997955,-5.05,50.180988897758));
#200452=CARTESIAN_POINT('',(121.700268024085,-5.05,50.4754769992877));
#200453=CARTESIAN_POINT('',(121.757510997955,-5.05,50.180988897758));
#200454=CARTESIAN_POINT('Origin',(121.757510997955,-3.75,50.180988897758));
#200455=CARTESIAN_POINT('',(122.248324500504,-3.75,50.2763938542073));
#200456=CARTESIAN_POINT('',(122.191081526635,-3.75,50.570881955737));
#200457=CARTESIAN_POINT('',(122.248324500504,-3.75,50.2763938542073));
#200458=CARTESIAN_POINT('',(121.700268024085,-3.75,50.4754769992877));
#200459=CARTESIAN_POINT('',(121.700268024085,-3.75,50.4754769992877));
#200460=CARTESIAN_POINT('',(121.757510997955,-3.75,50.180988897758));
#200461=CARTESIAN_POINT('',(121.757510997955,-3.75,50.180988897758));
#200462=CARTESIAN_POINT('',(121.757510997955,-3.75,50.180988897758));
#200463=CARTESIAN_POINT('Origin',(122.248324500504,-3.75,50.2763938542073));
#200464=CARTESIAN_POINT('',(122.248324500504,-4.25,50.2763938542073));
#200465=CARTESIAN_POINT('',(122.191081526635,-4.25,50.570881955737));
#200466=CARTESIAN_POINT('',(122.248324500504,-4.25,50.2763938542073));
#200467=CARTESIAN_POINT('',(122.191081526635,-3.75,50.570881955737));
#200468=CARTESIAN_POINT('',(122.248324500504,-3.75,50.2763938542073));
#200469=CARTESIAN_POINT('Origin',(122.248324500504,-4.25,50.2763938542073));
#200470=CARTESIAN_POINT('',(121.757510997955,-4.25,50.180988897758));
#200471=CARTESIAN_POINT('',(121.700268024085,-4.25,50.4754769992877));
#200472=CARTESIAN_POINT('',(121.757510997955,-4.25,50.180988897758));
#200473=CARTESIAN_POINT('',(122.191081526635,-4.25,50.570881955737));
#200474=CARTESIAN_POINT('',(122.248324500504,-4.25,50.2763938542073));
#200475=CARTESIAN_POINT('Origin',(121.757510997955,-4.25,50.180988897758));
#200476=CARTESIAN_POINT('',(121.700268024085,-4.25,50.4754769992877));
#200477=CARTESIAN_POINT('',(121.757510997955,-4.25,50.180988897758));
#200478=CARTESIAN_POINT('Origin',(121.757510997955,-2.95,50.180988897758));
#200479=CARTESIAN_POINT('',(122.248324500504,-2.95,50.2763938542073));
#200480=CARTESIAN_POINT('',(122.191081526635,-2.95,50.570881955737));
#200481=CARTESIAN_POINT('',(122.248324500504,-2.95,50.2763938542073));
#200482=CARTESIAN_POINT('',(121.700268024085,-2.95,50.4754769992877));
#200483=CARTESIAN_POINT('',(121.700268024085,-2.95,50.4754769992877));
#200484=CARTESIAN_POINT('',(121.757510997955,-2.95,50.180988897758));
#200485=CARTESIAN_POINT('',(121.757510997955,-2.95,50.180988897758));
#200486=CARTESIAN_POINT('',(121.757510997955,-2.95,50.180988897758));
#200487=CARTESIAN_POINT('Origin',(122.248324500504,-2.95,50.2763938542073));
#200488=CARTESIAN_POINT('',(122.248324500504,-3.45,50.2763938542073));
#200489=CARTESIAN_POINT('',(122.191081526635,-3.45,50.570881955737));
#200490=CARTESIAN_POINT('',(122.248324500504,-3.45,50.2763938542073));
#200491=CARTESIAN_POINT('',(122.191081526635,-2.95,50.570881955737));
#200492=CARTESIAN_POINT('',(122.248324500504,-2.95,50.2763938542073));
#200493=CARTESIAN_POINT('Origin',(122.248324500504,-3.45,50.2763938542073));
#200494=CARTESIAN_POINT('',(121.757510997955,-3.45,50.180988897758));
#200495=CARTESIAN_POINT('',(121.700268024085,-3.45,50.4754769992877));
#200496=CARTESIAN_POINT('',(121.757510997955,-3.45,50.180988897758));
#200497=CARTESIAN_POINT('',(122.191081526635,-3.45,50.570881955737));
#200498=CARTESIAN_POINT('',(122.248324500504,-3.45,50.2763938542073));
#200499=CARTESIAN_POINT('Origin',(121.757510997955,-3.45,50.180988897758));
#200500=CARTESIAN_POINT('',(121.700268024085,-3.45,50.4754769992877));
#200501=CARTESIAN_POINT('',(121.757510997955,-3.45,50.180988897758));
#200502=CARTESIAN_POINT('Origin',(121.757510997955,-2.15,50.180988897758));
#200503=CARTESIAN_POINT('',(122.248324500504,-2.15,50.2763938542073));
#200504=CARTESIAN_POINT('',(122.191081526635,-2.15,50.570881955737));
#200505=CARTESIAN_POINT('',(122.248324500504,-2.15,50.2763938542073));
#200506=CARTESIAN_POINT('',(121.700268024085,-2.15,50.4754769992877));
#200507=CARTESIAN_POINT('',(121.700268024085,-2.15,50.4754769992877));
#200508=CARTESIAN_POINT('',(121.757510997955,-2.15,50.180988897758));
#200509=CARTESIAN_POINT('',(121.757510997955,-2.15,50.180988897758));
#200510=CARTESIAN_POINT('',(121.757510997955,-2.15,50.180988897758));
#200511=CARTESIAN_POINT('Origin',(122.248324500504,-2.15,50.2763938542073));
#200512=CARTESIAN_POINT('',(122.248324500504,-2.65,50.2763938542073));
#200513=CARTESIAN_POINT('',(122.191081526635,-2.65,50.570881955737));
#200514=CARTESIAN_POINT('',(122.248324500504,-2.65,50.2763938542073));
#200515=CARTESIAN_POINT('',(122.191081526635,-2.15,50.570881955737));
#200516=CARTESIAN_POINT('',(122.248324500504,-2.15,50.2763938542073));
#200517=CARTESIAN_POINT('Origin',(122.248324500504,-2.65,50.2763938542073));
#200518=CARTESIAN_POINT('',(121.757510997955,-2.65,50.180988897758));
#200519=CARTESIAN_POINT('',(121.700268024085,-2.65,50.4754769992877));
#200520=CARTESIAN_POINT('',(121.757510997955,-2.65,50.180988897758));
#200521=CARTESIAN_POINT('',(122.191081526635,-2.65,50.570881955737));
#200522=CARTESIAN_POINT('',(122.248324500504,-2.65,50.2763938542073));
#200523=CARTESIAN_POINT('Origin',(121.757510997955,-2.65,50.180988897758));
#200524=CARTESIAN_POINT('',(121.700268024085,-2.65,50.4754769992877));
#200525=CARTESIAN_POINT('',(121.757510997955,-2.65,50.180988897758));
#200526=CARTESIAN_POINT('Origin',(121.757510997955,-1.35,50.180988897758));
#200527=CARTESIAN_POINT('',(122.248324500504,-1.35,50.2763938542073));
#200528=CARTESIAN_POINT('',(122.191081526635,-1.35,50.570881955737));
#200529=CARTESIAN_POINT('',(122.248324500504,-1.35,50.2763938542073));
#200530=CARTESIAN_POINT('',(121.700268024085,-1.35,50.4754769992877));
#200531=CARTESIAN_POINT('',(121.700268024085,-1.35,50.4754769992877));
#200532=CARTESIAN_POINT('',(121.757510997955,-1.35,50.180988897758));
#200533=CARTESIAN_POINT('',(121.757510997955,-1.35,50.180988897758));
#200534=CARTESIAN_POINT('',(121.757510997955,-1.35,50.180988897758));
#200535=CARTESIAN_POINT('Origin',(122.248324500504,-1.35,50.2763938542073));
#200536=CARTESIAN_POINT('',(122.248324500504,-1.85,50.2763938542073));
#200537=CARTESIAN_POINT('',(122.191081526635,-1.85,50.570881955737));
#200538=CARTESIAN_POINT('',(122.248324500504,-1.85,50.2763938542073));
#200539=CARTESIAN_POINT('',(122.191081526635,-1.35,50.570881955737));
#200540=CARTESIAN_POINT('',(122.248324500504,-1.35,50.2763938542073));
#200541=CARTESIAN_POINT('Origin',(122.248324500504,-1.85,50.2763938542073));
#200542=CARTESIAN_POINT('',(121.757510997955,-1.85,50.180988897758));
#200543=CARTESIAN_POINT('',(121.700268024085,-1.85,50.4754769992877));
#200544=CARTESIAN_POINT('',(121.757510997955,-1.85,50.180988897758));
#200545=CARTESIAN_POINT('',(122.191081526635,-1.85,50.570881955737));
#200546=CARTESIAN_POINT('',(122.248324500504,-1.85,50.2763938542073));
#200547=CARTESIAN_POINT('Origin',(121.757510997955,-1.85,50.180988897758));
#200548=CARTESIAN_POINT('',(121.700268024085,-1.85,50.4754769992877));
#200549=CARTESIAN_POINT('',(121.757510997955,-1.85,50.180988897758));
#200550=CARTESIAN_POINT('Origin',(121.757510997955,-0.549999999999986,50.180988897758));
#200551=CARTESIAN_POINT('',(122.248324500504,-0.549999999999986,50.2763938542073));
#200552=CARTESIAN_POINT('',(122.191081526635,-0.549999999999986,50.570881955737));
#200553=CARTESIAN_POINT('',(122.248324500504,-0.549999999999986,50.2763938542073));
#200554=CARTESIAN_POINT('',(121.700268024085,-0.549999999999986,50.4754769992877));
#200555=CARTESIAN_POINT('',(121.700268024085,-0.549999999999986,50.4754769992877));
#200556=CARTESIAN_POINT('',(121.757510997955,-0.549999999999986,50.180988897758));
#200557=CARTESIAN_POINT('',(121.757510997955,-0.549999999999986,50.180988897758));
#200558=CARTESIAN_POINT('',(121.757510997955,-0.549999999999986,50.180988897758));
#200559=CARTESIAN_POINT('Origin',(122.248324500504,-0.549999999999986,50.2763938542073));
#200560=CARTESIAN_POINT('',(122.248324500504,-1.05,50.2763938542073));
#200561=CARTESIAN_POINT('',(122.191081526635,-1.05,50.570881955737));
#200562=CARTESIAN_POINT('',(122.248324500504,-1.05,50.2763938542073));
#200563=CARTESIAN_POINT('',(122.191081526635,-0.549999999999986,50.570881955737));
#200564=CARTESIAN_POINT('',(122.248324500504,-0.549999999999986,50.2763938542073));
#200565=CARTESIAN_POINT('Origin',(122.248324500504,-1.05,50.2763938542073));
#200566=CARTESIAN_POINT('',(121.757510997955,-1.05,50.180988897758));
#200567=CARTESIAN_POINT('',(121.700268024085,-1.05,50.4754769992877));
#200568=CARTESIAN_POINT('',(121.757510997955,-1.05,50.180988897758));
#200569=CARTESIAN_POINT('',(122.191081526635,-1.05,50.570881955737));
#200570=CARTESIAN_POINT('',(122.248324500504,-1.05,50.2763938542073));
#200571=CARTESIAN_POINT('Origin',(121.757510997955,-1.05,50.180988897758));
#200572=CARTESIAN_POINT('',(121.700268024085,-1.05,50.4754769992877));
#200573=CARTESIAN_POINT('',(121.757510997955,-1.05,50.180988897758));
#200574=CARTESIAN_POINT('Origin',(121.757510997955,0.250000000000015,50.180988897758));
#200575=CARTESIAN_POINT('',(122.248324500504,0.250000000000015,50.2763938542073));
#200576=CARTESIAN_POINT('',(122.191081526635,0.250000000000015,50.570881955737));
#200577=CARTESIAN_POINT('',(122.248324500504,0.250000000000015,50.2763938542073));
#200578=CARTESIAN_POINT('',(121.700268024085,0.250000000000015,50.4754769992877));
#200579=CARTESIAN_POINT('',(121.700268024085,0.250000000000015,50.4754769992877));
#200580=CARTESIAN_POINT('',(121.757510997955,0.250000000000015,50.180988897758));
#200581=CARTESIAN_POINT('',(121.757510997955,0.250000000000015,50.180988897758));
#200582=CARTESIAN_POINT('',(121.757510997955,0.250000000000015,50.180988897758));
#200583=CARTESIAN_POINT('Origin',(122.248324500504,0.250000000000015,50.2763938542073));
#200584=CARTESIAN_POINT('',(122.248324500504,-0.249999999999985,50.2763938542073));
#200585=CARTESIAN_POINT('',(122.191081526635,-0.249999999999985,50.570881955737));
#200586=CARTESIAN_POINT('',(122.248324500504,-0.249999999999985,50.2763938542073));
#200587=CARTESIAN_POINT('',(122.191081526635,0.250000000000015,50.570881955737));
#200588=CARTESIAN_POINT('',(122.248324500504,0.250000000000015,50.2763938542073));
#200589=CARTESIAN_POINT('Origin',(122.248324500504,-0.249999999999985,50.2763938542073));
#200590=CARTESIAN_POINT('',(121.757510997955,-0.249999999999985,50.180988897758));
#200591=CARTESIAN_POINT('',(121.700268024085,-0.249999999999985,50.4754769992877));
#200592=CARTESIAN_POINT('',(121.757510997955,-0.249999999999985,50.180988897758));
#200593=CARTESIAN_POINT('',(122.191081526635,-0.249999999999985,50.570881955737));
#200594=CARTESIAN_POINT('',(122.248324500504,-0.249999999999985,50.2763938542073));
#200595=CARTESIAN_POINT('Origin',(121.757510997955,-0.249999999999985,50.180988897758));
#200596=CARTESIAN_POINT('',(121.700268024085,-0.249999999999985,50.4754769992877));
#200597=CARTESIAN_POINT('',(121.757510997955,-0.249999999999985,50.180988897758));
#200598=CARTESIAN_POINT('Origin',(121.757510997955,1.05,50.180988897758));
#200599=CARTESIAN_POINT('',(122.248324500504,1.05,50.2763938542073));
#200600=CARTESIAN_POINT('',(122.191081526635,1.05,50.570881955737));
#200601=CARTESIAN_POINT('',(122.248324500504,1.05,50.2763938542073));
#200602=CARTESIAN_POINT('',(121.700268024085,1.05,50.4754769992877));
#200603=CARTESIAN_POINT('',(121.700268024085,1.05,50.4754769992877));
#200604=CARTESIAN_POINT('',(121.757510997955,1.05,50.180988897758));
#200605=CARTESIAN_POINT('',(121.757510997955,1.05,50.180988897758));
#200606=CARTESIAN_POINT('',(121.757510997955,1.05,50.180988897758));
#200607=CARTESIAN_POINT('Origin',(122.248324500504,1.05,50.2763938542073));
#200608=CARTESIAN_POINT('',(122.248324500504,0.550000000000015,50.2763938542073));
#200609=CARTESIAN_POINT('',(122.191081526635,0.550000000000015,50.570881955737));
#200610=CARTESIAN_POINT('',(122.248324500504,0.550000000000015,50.2763938542073));
#200611=CARTESIAN_POINT('',(122.191081526635,1.05,50.570881955737));
#200612=CARTESIAN_POINT('',(122.248324500504,1.05,50.2763938542073));
#200613=CARTESIAN_POINT('Origin',(122.248324500504,0.550000000000015,50.2763938542073));
#200614=CARTESIAN_POINT('',(121.757510997955,0.550000000000015,50.180988897758));
#200615=CARTESIAN_POINT('',(121.700268024085,0.550000000000015,50.4754769992877));
#200616=CARTESIAN_POINT('',(121.757510997955,0.550000000000015,50.180988897758));
#200617=CARTESIAN_POINT('',(122.191081526635,0.550000000000015,50.570881955737));
#200618=CARTESIAN_POINT('',(122.248324500504,0.550000000000015,50.2763938542073));
#200619=CARTESIAN_POINT('Origin',(121.757510997955,0.550000000000015,50.180988897758));
#200620=CARTESIAN_POINT('',(121.700268024085,0.550000000000015,50.4754769992877));
#200621=CARTESIAN_POINT('',(121.757510997955,0.550000000000015,50.180988897758));
#200622=CARTESIAN_POINT('Origin',(121.757510997955,1.85,50.180988897758));
#200623=CARTESIAN_POINT('',(122.248324500504,1.85,50.2763938542073));
#200624=CARTESIAN_POINT('',(122.191081526635,1.85,50.570881955737));
#200625=CARTESIAN_POINT('',(122.248324500504,1.85,50.2763938542073));
#200626=CARTESIAN_POINT('',(121.700268024085,1.85,50.4754769992877));
#200627=CARTESIAN_POINT('',(121.700268024085,1.85,50.4754769992877));
#200628=CARTESIAN_POINT('',(121.757510997955,1.85,50.180988897758));
#200629=CARTESIAN_POINT('',(121.757510997955,1.85,50.180988897758));
#200630=CARTESIAN_POINT('',(121.757510997955,1.85,50.180988897758));
#200631=CARTESIAN_POINT('Origin',(122.248324500504,1.85,50.2763938542073));
#200632=CARTESIAN_POINT('',(122.248324500504,1.35,50.2763938542073));
#200633=CARTESIAN_POINT('',(122.191081526635,1.35,50.570881955737));
#200634=CARTESIAN_POINT('',(122.248324500504,1.35,50.2763938542073));
#200635=CARTESIAN_POINT('',(122.191081526635,1.85,50.570881955737));
#200636=CARTESIAN_POINT('',(122.248324500504,1.85,50.2763938542073));
#200637=CARTESIAN_POINT('Origin',(122.248324500504,1.35,50.2763938542073));
#200638=CARTESIAN_POINT('',(121.757510997955,1.35,50.180988897758));
#200639=CARTESIAN_POINT('',(121.700268024085,1.35,50.4754769992877));
#200640=CARTESIAN_POINT('',(121.757510997955,1.35,50.180988897758));
#200641=CARTESIAN_POINT('',(122.191081526635,1.35,50.570881955737));
#200642=CARTESIAN_POINT('',(122.248324500504,1.35,50.2763938542073));
#200643=CARTESIAN_POINT('Origin',(121.757510997955,1.35,50.180988897758));
#200644=CARTESIAN_POINT('',(121.700268024085,1.35,50.4754769992877));
#200645=CARTESIAN_POINT('',(121.757510997955,1.35,50.180988897758));
#200646=CARTESIAN_POINT('Origin',(121.757510997955,2.65,50.180988897758));
#200647=CARTESIAN_POINT('',(122.248324500504,2.65,50.2763938542073));
#200648=CARTESIAN_POINT('',(122.191081526635,2.65,50.570881955737));
#200649=CARTESIAN_POINT('',(122.248324500504,2.65,50.2763938542073));
#200650=CARTESIAN_POINT('',(121.700268024085,2.65,50.4754769992877));
#200651=CARTESIAN_POINT('',(121.700268024085,2.65,50.4754769992877));
#200652=CARTESIAN_POINT('',(121.757510997955,2.65,50.180988897758));
#200653=CARTESIAN_POINT('',(121.757510997955,2.65,50.180988897758));
#200654=CARTESIAN_POINT('',(121.757510997955,2.65,50.180988897758));
#200655=CARTESIAN_POINT('Origin',(122.248324500504,2.65,50.2763938542073));
#200656=CARTESIAN_POINT('',(122.248324500504,2.15,50.2763938542073));
#200657=CARTESIAN_POINT('',(122.191081526635,2.15,50.570881955737));
#200658=CARTESIAN_POINT('',(122.248324500504,2.15,50.2763938542073));
#200659=CARTESIAN_POINT('',(122.191081526635,2.65,50.570881955737));
#200660=CARTESIAN_POINT('',(122.248324500504,2.65,50.2763938542073));
#200661=CARTESIAN_POINT('Origin',(122.248324500504,2.15,50.2763938542073));
#200662=CARTESIAN_POINT('',(121.757510997955,2.15,50.180988897758));
#200663=CARTESIAN_POINT('',(121.700268024085,2.15,50.4754769992877));
#200664=CARTESIAN_POINT('',(121.757510997955,2.15,50.180988897758));
#200665=CARTESIAN_POINT('',(122.191081526635,2.15,50.570881955737));
#200666=CARTESIAN_POINT('',(122.248324500504,2.15,50.2763938542073));
#200667=CARTESIAN_POINT('Origin',(121.757510997955,2.15,50.180988897758));
#200668=CARTESIAN_POINT('',(121.700268024085,2.15,50.4754769992877));
#200669=CARTESIAN_POINT('',(121.757510997955,2.15,50.180988897758));
#200670=CARTESIAN_POINT('Origin',(121.757510997955,3.45,50.180988897758));
#200671=CARTESIAN_POINT('',(122.248324500504,3.45,50.2763938542073));
#200672=CARTESIAN_POINT('',(122.191081526635,3.45,50.570881955737));
#200673=CARTESIAN_POINT('',(122.248324500504,3.45,50.2763938542073));
#200674=CARTESIAN_POINT('',(121.700268024085,3.45,50.4754769992877));
#200675=CARTESIAN_POINT('',(121.700268024085,3.45,50.4754769992877));
#200676=CARTESIAN_POINT('',(121.757510997955,3.45,50.180988897758));
#200677=CARTESIAN_POINT('',(121.757510997955,3.45,50.180988897758));
#200678=CARTESIAN_POINT('',(121.757510997955,3.45,50.180988897758));
#200679=CARTESIAN_POINT('Origin',(122.248324500504,3.45,50.2763938542073));
#200680=CARTESIAN_POINT('',(122.248324500504,2.95,50.2763938542073));
#200681=CARTESIAN_POINT('',(122.191081526635,2.95,50.570881955737));
#200682=CARTESIAN_POINT('',(122.248324500504,2.95,50.2763938542073));
#200683=CARTESIAN_POINT('',(122.191081526635,3.45,50.570881955737));
#200684=CARTESIAN_POINT('',(122.248324500504,3.45,50.2763938542073));
#200685=CARTESIAN_POINT('Origin',(122.248324500504,2.95,50.2763938542073));
#200686=CARTESIAN_POINT('',(121.757510997955,2.95,50.180988897758));
#200687=CARTESIAN_POINT('',(121.700268024085,2.95,50.4754769992877));
#200688=CARTESIAN_POINT('',(121.757510997955,2.95,50.180988897758));
#200689=CARTESIAN_POINT('',(122.191081526635,2.95,50.570881955737));
#200690=CARTESIAN_POINT('',(122.248324500504,2.95,50.2763938542073));
#200691=CARTESIAN_POINT('Origin',(121.757510997955,2.95,50.180988897758));
#200692=CARTESIAN_POINT('',(121.700268024085,2.95,50.4754769992877));
#200693=CARTESIAN_POINT('',(121.757510997955,2.95,50.180988897758));
#200694=CARTESIAN_POINT('Origin',(121.757510997955,4.25,50.180988897758));
#200695=CARTESIAN_POINT('',(122.248324500504,4.25,50.2763938542073));
#200696=CARTESIAN_POINT('',(122.191081526635,4.25,50.570881955737));
#200697=CARTESIAN_POINT('',(122.248324500504,4.25,50.2763938542073));
#200698=CARTESIAN_POINT('',(121.700268024085,4.25,50.4754769992877));
#200699=CARTESIAN_POINT('',(121.700268024085,4.25,50.4754769992877));
#200700=CARTESIAN_POINT('',(121.757510997955,4.25,50.180988897758));
#200701=CARTESIAN_POINT('',(121.757510997955,4.25,50.180988897758));
#200702=CARTESIAN_POINT('',(121.757510997955,4.25,50.180988897758));
#200703=CARTESIAN_POINT('Origin',(122.248324500504,4.25,50.2763938542073));
#200704=CARTESIAN_POINT('',(122.248324500504,3.75,50.2763938542073));
#200705=CARTESIAN_POINT('',(122.191081526635,3.75,50.570881955737));
#200706=CARTESIAN_POINT('',(122.248324500504,3.75,50.2763938542073));
#200707=CARTESIAN_POINT('',(122.191081526635,4.25,50.570881955737));
#200708=CARTESIAN_POINT('',(122.248324500504,4.25,50.2763938542073));
#200709=CARTESIAN_POINT('Origin',(122.248324500504,3.75,50.2763938542073));
#200710=CARTESIAN_POINT('',(121.757510997955,3.75,50.180988897758));
#200711=CARTESIAN_POINT('',(121.700268024085,3.75,50.4754769992877));
#200712=CARTESIAN_POINT('',(121.757510997955,3.75,50.180988897758));
#200713=CARTESIAN_POINT('',(122.191081526635,3.75,50.570881955737));
#200714=CARTESIAN_POINT('',(122.248324500504,3.75,50.2763938542073));
#200715=CARTESIAN_POINT('Origin',(121.757510997955,3.75,50.180988897758));
#200716=CARTESIAN_POINT('',(121.700268024085,3.75,50.4754769992877));
#200717=CARTESIAN_POINT('',(121.757510997955,3.75,50.180988897758));
#200718=CARTESIAN_POINT('Origin',(121.757510997955,5.05,50.180988897758));
#200719=CARTESIAN_POINT('',(122.248324500504,5.05,50.2763938542073));
#200720=CARTESIAN_POINT('',(122.191081526635,5.05,50.570881955737));
#200721=CARTESIAN_POINT('',(122.248324500504,5.05,50.2763938542073));
#200722=CARTESIAN_POINT('',(121.700268024085,5.05,50.4754769992877));
#200723=CARTESIAN_POINT('',(121.700268024085,5.05,50.4754769992877));
#200724=CARTESIAN_POINT('',(121.757510997955,5.05,50.180988897758));
#200725=CARTESIAN_POINT('',(121.757510997955,5.05,50.180988897758));
#200726=CARTESIAN_POINT('',(121.757510997955,5.05,50.180988897758));
#200727=CARTESIAN_POINT('Origin',(122.248324500504,5.05,50.2763938542073));
#200728=CARTESIAN_POINT('',(122.248324500504,4.55,50.2763938542073));
#200729=CARTESIAN_POINT('',(122.191081526635,4.55,50.570881955737));
#200730=CARTESIAN_POINT('',(122.248324500504,4.55,50.2763938542073));
#200731=CARTESIAN_POINT('',(122.191081526635,5.05,50.570881955737));
#200732=CARTESIAN_POINT('',(122.248324500504,5.05,50.2763938542073));
#200733=CARTESIAN_POINT('Origin',(122.248324500504,4.55,50.2763938542073));
#200734=CARTESIAN_POINT('',(121.757510997955,4.55,50.180988897758));
#200735=CARTESIAN_POINT('',(121.700268024085,4.55,50.4754769992877));
#200736=CARTESIAN_POINT('',(121.757510997955,4.55,50.180988897758));
#200737=CARTESIAN_POINT('',(122.191081526635,4.55,50.570881955737));
#200738=CARTESIAN_POINT('',(122.248324500504,4.55,50.2763938542073));
#200739=CARTESIAN_POINT('Origin',(121.757510997955,4.55,50.180988897758));
#200740=CARTESIAN_POINT('',(121.700268024085,4.55,50.4754769992877));
#200741=CARTESIAN_POINT('',(121.757510997955,4.55,50.180988897758));
#200742=CARTESIAN_POINT('Origin',(120.972209393875,5.05,50.0283409674392));
#200743=CARTESIAN_POINT('',(121.463022896425,5.05,50.1237459238885));
#200744=CARTESIAN_POINT('',(121.405779922555,5.05,50.4182340254182));
#200745=CARTESIAN_POINT('',(121.463022896425,5.05,50.1237459238885));
#200746=CARTESIAN_POINT('',(120.914966420006,5.05,50.3228290689689));
#200747=CARTESIAN_POINT('',(120.914966420006,5.05,50.3228290689689));
#200748=CARTESIAN_POINT('',(120.972209393875,5.05,50.0283409674392));
#200749=CARTESIAN_POINT('',(120.972209393875,5.05,50.0283409674392));
#200750=CARTESIAN_POINT('',(120.972209393875,5.05,50.0283409674392));
#200751=CARTESIAN_POINT('Origin',(121.463022896425,5.05,50.1237459238885));
#200752=CARTESIAN_POINT('',(121.463022896425,4.55,50.1237459238885));
#200753=CARTESIAN_POINT('',(121.405779922555,4.55,50.4182340254182));
#200754=CARTESIAN_POINT('',(121.463022896425,4.55,50.1237459238885));
#200755=CARTESIAN_POINT('',(121.405779922555,5.05,50.4182340254182));
#200756=CARTESIAN_POINT('',(121.463022896425,5.05,50.1237459238885));
#200757=CARTESIAN_POINT('Origin',(121.463022896425,4.55,50.1237459238885));
#200758=CARTESIAN_POINT('',(120.972209393875,4.55,50.0283409674392));
#200759=CARTESIAN_POINT('',(120.914966420006,4.55,50.3228290689689));
#200760=CARTESIAN_POINT('',(120.972209393875,4.55,50.0283409674392));
#200761=CARTESIAN_POINT('',(121.405779922555,4.55,50.4182340254182));
#200762=CARTESIAN_POINT('',(121.463022896425,4.55,50.1237459238885));
#200763=CARTESIAN_POINT('Origin',(120.972209393875,4.55,50.0283409674392));
#200764=CARTESIAN_POINT('',(120.914966420006,4.55,50.3228290689689));
#200765=CARTESIAN_POINT('',(120.972209393875,4.55,50.0283409674392));
#200766=CARTESIAN_POINT('Origin',(120.186907789796,5.05,49.8756930371204));
#200767=CARTESIAN_POINT('',(120.677721292346,5.05,49.9710979935697));
#200768=CARTESIAN_POINT('',(120.620478318476,5.05,50.2655860950994));
#200769=CARTESIAN_POINT('',(120.677721292346,5.05,49.9710979935697));
#200770=CARTESIAN_POINT('',(120.129664815927,5.05,50.1701811386501));
#200771=CARTESIAN_POINT('',(120.129664815927,5.05,50.1701811386501));
#200772=CARTESIAN_POINT('',(120.186907789796,5.05,49.8756930371204));
#200773=CARTESIAN_POINT('',(120.186907789796,5.05,49.8756930371204));
#200774=CARTESIAN_POINT('',(120.186907789796,5.05,49.8756930371204));
#200775=CARTESIAN_POINT('Origin',(120.677721292346,5.05,49.9710979935697));
#200776=CARTESIAN_POINT('',(120.677721292346,4.55,49.9710979935697));
#200777=CARTESIAN_POINT('',(120.620478318476,4.55,50.2655860950994));
#200778=CARTESIAN_POINT('',(120.677721292346,4.55,49.9710979935697));
#200779=CARTESIAN_POINT('',(120.620478318476,5.05,50.2655860950994));
#200780=CARTESIAN_POINT('',(120.677721292346,5.05,49.9710979935697));
#200781=CARTESIAN_POINT('Origin',(120.677721292346,4.55,49.9710979935697));
#200782=CARTESIAN_POINT('',(120.186907789796,4.55,49.8756930371204));
#200783=CARTESIAN_POINT('',(120.129664815927,4.55,50.1701811386501));
#200784=CARTESIAN_POINT('',(120.186907789796,4.55,49.8756930371204));
#200785=CARTESIAN_POINT('',(120.620478318476,4.55,50.2655860950994));
#200786=CARTESIAN_POINT('',(120.677721292346,4.55,49.9710979935697));
#200787=CARTESIAN_POINT('Origin',(120.186907789796,4.55,49.8756930371204));
#200788=CARTESIAN_POINT('',(120.129664815927,4.55,50.1701811386501));
#200789=CARTESIAN_POINT('',(120.186907789796,4.55,49.8756930371204));
#200790=CARTESIAN_POINT('Origin',(119.401606185717,5.05,49.7230451068016));
#200791=CARTESIAN_POINT('',(119.892419688267,5.05,49.8184500632509));
#200792=CARTESIAN_POINT('',(119.835176714397,5.05,50.1129381647806));
#200793=CARTESIAN_POINT('',(119.892419688267,5.05,49.8184500632509));
#200794=CARTESIAN_POINT('',(119.344363211847,5.05,50.0175332083313));
#200795=CARTESIAN_POINT('',(119.344363211847,5.05,50.0175332083313));
#200796=CARTESIAN_POINT('',(119.401606185717,5.05,49.7230451068016));
#200797=CARTESIAN_POINT('',(119.401606185717,5.05,49.7230451068016));
#200798=CARTESIAN_POINT('',(119.401606185717,5.05,49.7230451068016));
#200799=CARTESIAN_POINT('Origin',(119.892419688267,5.05,49.8184500632509));
#200800=CARTESIAN_POINT('',(119.892419688267,4.55,49.8184500632509));
#200801=CARTESIAN_POINT('',(119.835176714397,4.55,50.1129381647806));
#200802=CARTESIAN_POINT('',(119.892419688267,4.55,49.8184500632509));
#200803=CARTESIAN_POINT('',(119.835176714397,5.05,50.1129381647806));
#200804=CARTESIAN_POINT('',(119.892419688267,5.05,49.8184500632509));
#200805=CARTESIAN_POINT('Origin',(119.892419688267,4.55,49.8184500632509));
#200806=CARTESIAN_POINT('',(119.401606185717,4.55,49.7230451068016));
#200807=CARTESIAN_POINT('',(119.344363211847,4.55,50.0175332083313));
#200808=CARTESIAN_POINT('',(119.401606185717,4.55,49.7230451068016));
#200809=CARTESIAN_POINT('',(119.835176714397,4.55,50.1129381647806));
#200810=CARTESIAN_POINT('',(119.892419688267,4.55,49.8184500632509));
#200811=CARTESIAN_POINT('Origin',(119.401606185717,4.55,49.7230451068016));
#200812=CARTESIAN_POINT('',(119.344363211847,4.55,50.0175332083313));
#200813=CARTESIAN_POINT('',(119.401606185717,4.55,49.7230451068016));
#200814=CARTESIAN_POINT('Origin',(118.616304581638,5.05,49.5703971764828));
#200815=CARTESIAN_POINT('',(119.107118084187,5.05,49.6658021329321));
#200816=CARTESIAN_POINT('',(119.049875110318,5.05,49.9602902344618));
#200817=CARTESIAN_POINT('',(119.107118084187,5.05,49.6658021329321));
#200818=CARTESIAN_POINT('',(118.559061607768,5.05,49.8648852780125));
#200819=CARTESIAN_POINT('',(118.559061607768,5.05,49.8648852780125));
#200820=CARTESIAN_POINT('',(118.616304581638,5.05,49.5703971764828));
#200821=CARTESIAN_POINT('',(118.616304581638,5.05,49.5703971764828));
#200822=CARTESIAN_POINT('',(118.616304581638,5.05,49.5703971764828));
#200823=CARTESIAN_POINT('Origin',(119.107118084187,5.05,49.6658021329321));
#200824=CARTESIAN_POINT('',(119.107118084187,4.55,49.6658021329321));
#200825=CARTESIAN_POINT('',(119.049875110318,4.55,49.9602902344618));
#200826=CARTESIAN_POINT('',(119.107118084187,4.55,49.6658021329321));
#200827=CARTESIAN_POINT('',(119.049875110318,5.05,49.9602902344618));
#200828=CARTESIAN_POINT('',(119.107118084187,5.05,49.6658021329321));
#200829=CARTESIAN_POINT('Origin',(119.107118084187,4.55,49.6658021329321));
#200830=CARTESIAN_POINT('',(118.616304581638,4.55,49.5703971764828));
#200831=CARTESIAN_POINT('',(118.559061607768,4.55,49.8648852780125));
#200832=CARTESIAN_POINT('',(118.616304581638,4.55,49.5703971764828));
#200833=CARTESIAN_POINT('',(119.049875110318,4.55,49.9602902344618));
#200834=CARTESIAN_POINT('',(119.107118084187,4.55,49.6658021329321));
#200835=CARTESIAN_POINT('Origin',(118.616304581638,4.55,49.5703971764828));
#200836=CARTESIAN_POINT('',(118.559061607768,4.55,49.8648852780125));
#200837=CARTESIAN_POINT('',(118.616304581638,4.55,49.5703971764828));
#200838=CARTESIAN_POINT('Origin',(117.831002977559,5.05,49.417749246164));
#200839=CARTESIAN_POINT('',(118.321816480108,5.05,49.5131542026133));
#200840=CARTESIAN_POINT('',(118.264573506239,5.05,49.807642304143));
#200841=CARTESIAN_POINT('',(118.321816480108,5.05,49.5131542026133));
#200842=CARTESIAN_POINT('',(117.773760003689,5.05,49.7122373476937));
#200843=CARTESIAN_POINT('',(117.773760003689,5.05,49.7122373476937));
#200844=CARTESIAN_POINT('',(117.831002977559,5.05,49.417749246164));
#200845=CARTESIAN_POINT('',(117.831002977559,5.05,49.417749246164));
#200846=CARTESIAN_POINT('',(117.831002977559,5.05,49.417749246164));
#200847=CARTESIAN_POINT('Origin',(118.321816480108,5.05,49.5131542026133));
#200848=CARTESIAN_POINT('',(118.321816480108,4.55,49.5131542026133));
#200849=CARTESIAN_POINT('',(118.264573506239,4.55,49.807642304143));
#200850=CARTESIAN_POINT('',(118.321816480108,4.55,49.5131542026133));
#200851=CARTESIAN_POINT('',(118.264573506239,5.05,49.807642304143));
#200852=CARTESIAN_POINT('',(118.321816480108,5.05,49.5131542026133));
#200853=CARTESIAN_POINT('Origin',(118.321816480108,4.55,49.5131542026133));
#200854=CARTESIAN_POINT('',(117.831002977559,4.55,49.417749246164));
#200855=CARTESIAN_POINT('',(117.773760003689,4.55,49.7122373476937));
#200856=CARTESIAN_POINT('',(117.831002977559,4.55,49.417749246164));
#200857=CARTESIAN_POINT('',(118.264573506239,4.55,49.807642304143));
#200858=CARTESIAN_POINT('',(118.321816480108,4.55,49.5131542026133));
#200859=CARTESIAN_POINT('Origin',(117.831002977559,4.55,49.417749246164));
#200860=CARTESIAN_POINT('',(117.773760003689,4.55,49.7122373476937));
#200861=CARTESIAN_POINT('',(117.831002977559,4.55,49.417749246164));
#200862=CARTESIAN_POINT('Origin',(117.045701373479,5.05,49.2651013158452));
#200863=CARTESIAN_POINT('',(117.536514876029,5.05,49.3605062722945));
#200864=CARTESIAN_POINT('',(117.479271902159,5.05,49.6549943738242));
#200865=CARTESIAN_POINT('',(117.536514876029,5.05,49.3605062722945));
#200866=CARTESIAN_POINT('',(116.98845839961,5.05,49.5595894173749));
#200867=CARTESIAN_POINT('',(116.98845839961,5.05,49.5595894173749));
#200868=CARTESIAN_POINT('',(117.045701373479,5.05,49.2651013158452));
#200869=CARTESIAN_POINT('',(117.045701373479,5.05,49.2651013158452));
#200870=CARTESIAN_POINT('',(117.045701373479,5.05,49.2651013158452));
#200871=CARTESIAN_POINT('Origin',(117.536514876029,5.05,49.3605062722945));
#200872=CARTESIAN_POINT('',(117.536514876029,4.55,49.3605062722945));
#200873=CARTESIAN_POINT('',(117.479271902159,4.55,49.6549943738242));
#200874=CARTESIAN_POINT('',(117.536514876029,4.55,49.3605062722945));
#200875=CARTESIAN_POINT('',(117.479271902159,5.05,49.6549943738242));
#200876=CARTESIAN_POINT('',(117.536514876029,5.05,49.3605062722945));
#200877=CARTESIAN_POINT('Origin',(117.536514876029,4.55,49.3605062722945));
#200878=CARTESIAN_POINT('',(117.045701373479,4.55,49.2651013158452));
#200879=CARTESIAN_POINT('',(116.98845839961,4.55,49.5595894173749));
#200880=CARTESIAN_POINT('',(117.045701373479,4.55,49.2651013158452));
#200881=CARTESIAN_POINT('',(117.479271902159,4.55,49.6549943738242));
#200882=CARTESIAN_POINT('',(117.536514876029,4.55,49.3605062722945));
#200883=CARTESIAN_POINT('Origin',(117.045701373479,4.55,49.2651013158452));
#200884=CARTESIAN_POINT('',(116.98845839961,4.55,49.5595894173749));
#200885=CARTESIAN_POINT('',(117.045701373479,4.55,49.2651013158452));
#200886=CARTESIAN_POINT('Origin',(116.2603997694,5.05,49.1124533855264));
#200887=CARTESIAN_POINT('',(116.75121327195,5.05,49.2078583419757));
#200888=CARTESIAN_POINT('',(116.69397029808,5.05,49.5023464435054));
#200889=CARTESIAN_POINT('',(116.75121327195,5.05,49.2078583419757));
#200890=CARTESIAN_POINT('',(116.203156795531,5.05,49.4069414870561));
#200891=CARTESIAN_POINT('',(116.203156795531,5.05,49.4069414870561));
#200892=CARTESIAN_POINT('',(116.2603997694,5.05,49.1124533855264));
#200893=CARTESIAN_POINT('',(116.2603997694,5.05,49.1124533855264));
#200894=CARTESIAN_POINT('',(116.2603997694,5.05,49.1124533855264));
#200895=CARTESIAN_POINT('Origin',(116.75121327195,5.05,49.2078583419757));
#200896=CARTESIAN_POINT('',(116.75121327195,4.55,49.2078583419757));
#200897=CARTESIAN_POINT('',(116.69397029808,4.55,49.5023464435054));
#200898=CARTESIAN_POINT('',(116.75121327195,4.55,49.2078583419757));
#200899=CARTESIAN_POINT('',(116.69397029808,5.05,49.5023464435054));
#200900=CARTESIAN_POINT('',(116.75121327195,5.05,49.2078583419757));
#200901=CARTESIAN_POINT('Origin',(116.75121327195,4.55,49.2078583419757));
#200902=CARTESIAN_POINT('',(116.2603997694,4.55,49.1124533855264));
#200903=CARTESIAN_POINT('',(116.203156795531,4.55,49.4069414870561));
#200904=CARTESIAN_POINT('',(116.2603997694,4.55,49.1124533855264));
#200905=CARTESIAN_POINT('',(116.69397029808,4.55,49.5023464435054));
#200906=CARTESIAN_POINT('',(116.75121327195,4.55,49.2078583419757));
#200907=CARTESIAN_POINT('Origin',(116.2603997694,4.55,49.1124533855264));
#200908=CARTESIAN_POINT('',(116.203156795531,4.55,49.4069414870561));
#200909=CARTESIAN_POINT('',(116.2603997694,4.55,49.1124533855264));
#200910=CARTESIAN_POINT('Origin',(115.475098165321,5.05,48.9598054552076));
#200911=CARTESIAN_POINT('',(115.96591166787,5.05,49.0552104116569));
#200912=CARTESIAN_POINT('',(115.908668694001,5.05,49.3496985131866));
#200913=CARTESIAN_POINT('',(115.96591166787,5.05,49.0552104116569));
#200914=CARTESIAN_POINT('',(115.417855191451,5.05,49.2542935567373));
#200915=CARTESIAN_POINT('',(115.417855191451,5.05,49.2542935567373));
#200916=CARTESIAN_POINT('',(115.475098165321,5.05,48.9598054552076));
#200917=CARTESIAN_POINT('',(115.475098165321,5.05,48.9598054552076));
#200918=CARTESIAN_POINT('',(115.475098165321,5.05,48.9598054552076));
#200919=CARTESIAN_POINT('Origin',(115.96591166787,5.05,49.0552104116569));
#200920=CARTESIAN_POINT('',(115.96591166787,4.55,49.0552104116569));
#200921=CARTESIAN_POINT('',(115.908668694001,4.55,49.3496985131866));
#200922=CARTESIAN_POINT('',(115.96591166787,4.55,49.0552104116569));
#200923=CARTESIAN_POINT('',(115.908668694001,5.05,49.3496985131866));
#200924=CARTESIAN_POINT('',(115.96591166787,5.05,49.0552104116569));
#200925=CARTESIAN_POINT('Origin',(115.96591166787,4.55,49.0552104116569));
#200926=CARTESIAN_POINT('',(115.475098165321,4.55,48.9598054552076));
#200927=CARTESIAN_POINT('',(115.417855191451,4.55,49.2542935567373));
#200928=CARTESIAN_POINT('',(115.475098165321,4.55,48.9598054552076));
#200929=CARTESIAN_POINT('',(115.908668694001,4.55,49.3496985131866));
#200930=CARTESIAN_POINT('',(115.96591166787,4.55,49.0552104116569));
#200931=CARTESIAN_POINT('Origin',(115.475098165321,4.55,48.9598054552076));
#200932=CARTESIAN_POINT('',(115.417855191451,4.55,49.2542935567373));
#200933=CARTESIAN_POINT('',(115.475098165321,4.55,48.9598054552076));
#200934=CARTESIAN_POINT('Origin',(114.689796561242,5.05,48.8071575248888));
#200935=CARTESIAN_POINT('',(115.180610063791,5.05,48.9025624813381));
#200936=CARTESIAN_POINT('',(115.123367089922,5.05,49.1970505828678));
#200937=CARTESIAN_POINT('',(115.180610063791,5.05,48.9025624813381));
#200938=CARTESIAN_POINT('',(114.632553587372,5.05,49.1016456264185));
#200939=CARTESIAN_POINT('',(114.632553587372,5.05,49.1016456264185));
#200940=CARTESIAN_POINT('',(114.689796561242,5.05,48.8071575248888));
#200941=CARTESIAN_POINT('',(114.689796561242,5.05,48.8071575248888));
#200942=CARTESIAN_POINT('',(114.689796561242,5.05,48.8071575248888));
#200943=CARTESIAN_POINT('Origin',(115.180610063791,5.05,48.9025624813381));
#200944=CARTESIAN_POINT('',(115.180610063791,4.55,48.9025624813381));
#200945=CARTESIAN_POINT('',(115.123367089922,4.55,49.1970505828678));
#200946=CARTESIAN_POINT('',(115.180610063791,4.55,48.9025624813381));
#200947=CARTESIAN_POINT('',(115.123367089922,5.05,49.1970505828678));
#200948=CARTESIAN_POINT('',(115.180610063791,5.05,48.9025624813381));
#200949=CARTESIAN_POINT('Origin',(115.180610063791,4.55,48.9025624813381));
#200950=CARTESIAN_POINT('',(114.689796561242,4.55,48.8071575248888));
#200951=CARTESIAN_POINT('',(114.632553587372,4.55,49.1016456264185));
#200952=CARTESIAN_POINT('',(114.689796561242,4.55,48.8071575248888));
#200953=CARTESIAN_POINT('',(115.123367089922,4.55,49.1970505828678));
#200954=CARTESIAN_POINT('',(115.180610063791,4.55,48.9025624813381));
#200955=CARTESIAN_POINT('Origin',(114.689796561242,4.55,48.8071575248888));
#200956=CARTESIAN_POINT('',(114.632553587372,4.55,49.1016456264185));
#200957=CARTESIAN_POINT('',(114.689796561242,4.55,48.8071575248888));
#200958=CARTESIAN_POINT('Origin',(113.904494957163,5.05,48.65450959457));
#200959=CARTESIAN_POINT('',(114.395308459712,5.05,48.7499145510193));
#200960=CARTESIAN_POINT('',(114.338065485842,5.05,49.044402652549));
#200961=CARTESIAN_POINT('',(114.395308459712,5.05,48.7499145510193));
#200962=CARTESIAN_POINT('',(113.847251983293,5.05,48.9489976960997));
#200963=CARTESIAN_POINT('',(113.847251983293,5.05,48.9489976960997));
#200964=CARTESIAN_POINT('',(113.904494957163,5.05,48.65450959457));
#200965=CARTESIAN_POINT('',(113.904494957163,5.05,48.65450959457));
#200966=CARTESIAN_POINT('',(113.904494957163,5.05,48.65450959457));
#200967=CARTESIAN_POINT('Origin',(114.395308459712,5.05,48.7499145510193));
#200968=CARTESIAN_POINT('',(114.395308459712,4.55,48.7499145510193));
#200969=CARTESIAN_POINT('',(114.338065485842,4.55,49.044402652549));
#200970=CARTESIAN_POINT('',(114.395308459712,4.55,48.7499145510193));
#200971=CARTESIAN_POINT('',(114.338065485842,5.05,49.044402652549));
#200972=CARTESIAN_POINT('',(114.395308459712,5.05,48.7499145510193));
#200973=CARTESIAN_POINT('Origin',(114.395308459712,4.55,48.7499145510193));
#200974=CARTESIAN_POINT('',(113.904494957163,4.55,48.65450959457));
#200975=CARTESIAN_POINT('',(113.847251983293,4.55,48.9489976960997));
#200976=CARTESIAN_POINT('',(113.904494957163,4.55,48.65450959457));
#200977=CARTESIAN_POINT('',(114.338065485842,4.55,49.044402652549));
#200978=CARTESIAN_POINT('',(114.395308459712,4.55,48.7499145510193));
#200979=CARTESIAN_POINT('Origin',(113.904494957163,4.55,48.65450959457));
#200980=CARTESIAN_POINT('',(113.847251983293,4.55,48.9489976960997));
#200981=CARTESIAN_POINT('',(113.904494957163,4.55,48.65450959457));
#200982=CARTESIAN_POINT('Origin',(113.119193353083,5.05,48.5018616642512));
#200983=CARTESIAN_POINT('',(113.610006855633,5.05,48.5972666207005));
#200984=CARTESIAN_POINT('',(113.552763881763,5.05,48.8917547222302));
#200985=CARTESIAN_POINT('',(113.610006855633,5.05,48.5972666207005));
#200986=CARTESIAN_POINT('',(113.061950379214,5.05,48.7963497657809));
#200987=CARTESIAN_POINT('',(113.061950379214,5.05,48.7963497657809));
#200988=CARTESIAN_POINT('',(113.119193353083,5.05,48.5018616642512));
#200989=CARTESIAN_POINT('',(113.119193353083,5.05,48.5018616642512));
#200990=CARTESIAN_POINT('',(113.119193353083,5.05,48.5018616642512));
#200991=CARTESIAN_POINT('Origin',(113.610006855633,5.05,48.5972666207005));
#200992=CARTESIAN_POINT('',(113.610006855633,4.55,48.5972666207005));
#200993=CARTESIAN_POINT('',(113.552763881763,4.55,48.8917547222302));
#200994=CARTESIAN_POINT('',(113.610006855633,4.55,48.5972666207005));
#200995=CARTESIAN_POINT('',(113.552763881763,5.05,48.8917547222302));
#200996=CARTESIAN_POINT('',(113.610006855633,5.05,48.5972666207005));
#200997=CARTESIAN_POINT('Origin',(113.610006855633,4.55,48.5972666207005));
#200998=CARTESIAN_POINT('',(113.119193353083,4.55,48.5018616642512));
#200999=CARTESIAN_POINT('',(113.061950379214,4.55,48.7963497657809));
#201000=CARTESIAN_POINT('',(113.119193353083,4.55,48.5018616642512));
#201001=CARTESIAN_POINT('',(113.552763881763,4.55,48.8917547222302));
#201002=CARTESIAN_POINT('',(113.610006855633,4.55,48.5972666207005));
#201003=CARTESIAN_POINT('Origin',(113.119193353083,4.55,48.5018616642512));
#201004=CARTESIAN_POINT('',(113.061950379214,4.55,48.7963497657809));
#201005=CARTESIAN_POINT('',(113.119193353083,4.55,48.5018616642512));
#201006=CARTESIAN_POINT('Origin',(113.119193353083,4.25,48.5018616642512));
#201007=CARTESIAN_POINT('',(113.610006855633,4.25,48.5972666207005));
#201008=CARTESIAN_POINT('',(113.552763881763,4.25,48.8917547222302));
#201009=CARTESIAN_POINT('',(113.610006855633,4.25,48.5972666207005));
#201010=CARTESIAN_POINT('',(113.061950379214,4.25,48.7963497657809));
#201011=CARTESIAN_POINT('',(113.061950379214,4.25,48.7963497657809));
#201012=CARTESIAN_POINT('',(113.119193353083,4.25,48.5018616642512));
#201013=CARTESIAN_POINT('',(113.119193353083,4.25,48.5018616642512));
#201014=CARTESIAN_POINT('',(113.119193353083,4.25,48.5018616642512));
#201015=CARTESIAN_POINT('Origin',(113.610006855633,4.25,48.5972666207005));
#201016=CARTESIAN_POINT('',(113.610006855633,3.75,48.5972666207005));
#201017=CARTESIAN_POINT('',(113.552763881763,3.75,48.8917547222302));
#201018=CARTESIAN_POINT('',(113.610006855633,3.75,48.5972666207005));
#201019=CARTESIAN_POINT('',(113.552763881763,4.25,48.8917547222302));
#201020=CARTESIAN_POINT('',(113.610006855633,4.25,48.5972666207005));
#201021=CARTESIAN_POINT('Origin',(113.610006855633,3.75,48.5972666207005));
#201022=CARTESIAN_POINT('',(113.119193353083,3.75,48.5018616642512));
#201023=CARTESIAN_POINT('',(113.061950379214,3.75,48.7963497657809));
#201024=CARTESIAN_POINT('',(113.119193353083,3.75,48.5018616642512));
#201025=CARTESIAN_POINT('',(113.552763881763,3.75,48.8917547222302));
#201026=CARTESIAN_POINT('',(113.610006855633,3.75,48.5972666207005));
#201027=CARTESIAN_POINT('Origin',(113.119193353083,3.75,48.5018616642512));
#201028=CARTESIAN_POINT('',(113.061950379214,3.75,48.7963497657809));
#201029=CARTESIAN_POINT('',(113.119193353083,3.75,48.5018616642512));
#201030=CARTESIAN_POINT('Origin',(113.119193353083,3.45,48.5018616642512));
#201031=CARTESIAN_POINT('',(113.610006855633,3.45,48.5972666207005));
#201032=CARTESIAN_POINT('',(113.552763881763,3.45,48.8917547222302));
#201033=CARTESIAN_POINT('',(113.610006855633,3.45,48.5972666207005));
#201034=CARTESIAN_POINT('',(113.061950379214,3.45,48.7963497657809));
#201035=CARTESIAN_POINT('',(113.061950379214,3.45,48.7963497657809));
#201036=CARTESIAN_POINT('',(113.119193353083,3.45,48.5018616642512));
#201037=CARTESIAN_POINT('',(113.119193353083,3.45,48.5018616642512));
#201038=CARTESIAN_POINT('',(113.119193353083,3.45,48.5018616642512));
#201039=CARTESIAN_POINT('Origin',(113.610006855633,3.45,48.5972666207005));
#201040=CARTESIAN_POINT('',(113.610006855633,2.95,48.5972666207005));
#201041=CARTESIAN_POINT('',(113.552763881763,2.95,48.8917547222302));
#201042=CARTESIAN_POINT('',(113.610006855633,2.95,48.5972666207005));
#201043=CARTESIAN_POINT('',(113.552763881763,3.45,48.8917547222302));
#201044=CARTESIAN_POINT('',(113.610006855633,3.45,48.5972666207005));
#201045=CARTESIAN_POINT('Origin',(113.610006855633,2.95,48.5972666207005));
#201046=CARTESIAN_POINT('',(113.119193353083,2.95,48.5018616642512));
#201047=CARTESIAN_POINT('',(113.061950379214,2.95,48.7963497657809));
#201048=CARTESIAN_POINT('',(113.119193353083,2.95,48.5018616642512));
#201049=CARTESIAN_POINT('',(113.552763881763,2.95,48.8917547222302));
#201050=CARTESIAN_POINT('',(113.610006855633,2.95,48.5972666207005));
#201051=CARTESIAN_POINT('Origin',(113.119193353083,2.95,48.5018616642512));
#201052=CARTESIAN_POINT('',(113.061950379214,2.95,48.7963497657809));
#201053=CARTESIAN_POINT('',(113.119193353083,2.95,48.5018616642512));
#201054=CARTESIAN_POINT('Origin',(113.119193353083,2.65,48.5018616642512));
#201055=CARTESIAN_POINT('',(113.610006855633,2.65,48.5972666207005));
#201056=CARTESIAN_POINT('',(113.552763881763,2.65,48.8917547222302));
#201057=CARTESIAN_POINT('',(113.610006855633,2.65,48.5972666207005));
#201058=CARTESIAN_POINT('',(113.061950379214,2.65,48.7963497657809));
#201059=CARTESIAN_POINT('',(113.061950379214,2.65,48.7963497657809));
#201060=CARTESIAN_POINT('',(113.119193353083,2.65,48.5018616642512));
#201061=CARTESIAN_POINT('',(113.119193353083,2.65,48.5018616642512));
#201062=CARTESIAN_POINT('',(113.119193353083,2.65,48.5018616642512));
#201063=CARTESIAN_POINT('Origin',(113.610006855633,2.65,48.5972666207005));
#201064=CARTESIAN_POINT('',(113.610006855633,2.15,48.5972666207005));
#201065=CARTESIAN_POINT('',(113.552763881763,2.15,48.8917547222302));
#201066=CARTESIAN_POINT('',(113.610006855633,2.15,48.5972666207005));
#201067=CARTESIAN_POINT('',(113.552763881763,2.65,48.8917547222302));
#201068=CARTESIAN_POINT('',(113.610006855633,2.65,48.5972666207005));
#201069=CARTESIAN_POINT('Origin',(113.610006855633,2.15,48.5972666207005));
#201070=CARTESIAN_POINT('',(113.119193353083,2.15,48.5018616642512));
#201071=CARTESIAN_POINT('',(113.061950379214,2.15,48.7963497657809));
#201072=CARTESIAN_POINT('',(113.119193353083,2.15,48.5018616642512));
#201073=CARTESIAN_POINT('',(113.552763881763,2.15,48.8917547222302));
#201074=CARTESIAN_POINT('',(113.610006855633,2.15,48.5972666207005));
#201075=CARTESIAN_POINT('Origin',(113.119193353083,2.15,48.5018616642512));
#201076=CARTESIAN_POINT('',(113.061950379214,2.15,48.7963497657809));
#201077=CARTESIAN_POINT('',(113.119193353083,2.15,48.5018616642512));
#201078=CARTESIAN_POINT('Origin',(113.119193353083,1.85,48.5018616642512));
#201079=CARTESIAN_POINT('',(113.610006855633,1.85,48.5972666207005));
#201080=CARTESIAN_POINT('',(113.552763881763,1.85,48.8917547222302));
#201081=CARTESIAN_POINT('',(113.610006855633,1.85,48.5972666207005));
#201082=CARTESIAN_POINT('',(113.061950379214,1.85,48.7963497657809));
#201083=CARTESIAN_POINT('',(113.061950379214,1.85,48.7963497657809));
#201084=CARTESIAN_POINT('',(113.119193353083,1.85,48.5018616642512));
#201085=CARTESIAN_POINT('',(113.119193353083,1.85,48.5018616642512));
#201086=CARTESIAN_POINT('',(113.119193353083,1.85,48.5018616642512));
#201087=CARTESIAN_POINT('Origin',(113.610006855633,1.85,48.5972666207005));
#201088=CARTESIAN_POINT('',(113.610006855633,1.35,48.5972666207005));
#201089=CARTESIAN_POINT('',(113.552763881763,1.35,48.8917547222302));
#201090=CARTESIAN_POINT('',(113.610006855633,1.35,48.5972666207005));
#201091=CARTESIAN_POINT('',(113.552763881763,1.85,48.8917547222302));
#201092=CARTESIAN_POINT('',(113.610006855633,1.85,48.5972666207005));
#201093=CARTESIAN_POINT('Origin',(113.610006855633,1.35,48.5972666207005));
#201094=CARTESIAN_POINT('',(113.119193353083,1.35,48.5018616642512));
#201095=CARTESIAN_POINT('',(113.061950379214,1.35,48.7963497657809));
#201096=CARTESIAN_POINT('',(113.119193353083,1.35,48.5018616642512));
#201097=CARTESIAN_POINT('',(113.552763881763,1.35,48.8917547222302));
#201098=CARTESIAN_POINT('',(113.610006855633,1.35,48.5972666207005));
#201099=CARTESIAN_POINT('Origin',(113.119193353083,1.35,48.5018616642512));
#201100=CARTESIAN_POINT('',(113.061950379214,1.35,48.7963497657809));
#201101=CARTESIAN_POINT('',(113.119193353083,1.35,48.5018616642512));
#201102=CARTESIAN_POINT('Origin',(113.119193353083,1.05,48.5018616642512));
#201103=CARTESIAN_POINT('',(113.610006855633,1.05,48.5972666207005));
#201104=CARTESIAN_POINT('',(113.552763881763,1.05,48.8917547222302));
#201105=CARTESIAN_POINT('',(113.610006855633,1.05,48.5972666207005));
#201106=CARTESIAN_POINT('',(113.061950379214,1.05,48.7963497657809));
#201107=CARTESIAN_POINT('',(113.061950379214,1.05,48.7963497657809));
#201108=CARTESIAN_POINT('',(113.119193353083,1.05,48.5018616642512));
#201109=CARTESIAN_POINT('',(113.119193353083,1.05,48.5018616642512));
#201110=CARTESIAN_POINT('',(113.119193353083,1.05,48.5018616642512));
#201111=CARTESIAN_POINT('Origin',(113.610006855633,1.05,48.5972666207005));
#201112=CARTESIAN_POINT('',(113.610006855633,0.550000000000015,48.5972666207005));
#201113=CARTESIAN_POINT('',(113.552763881763,0.550000000000015,48.8917547222302));
#201114=CARTESIAN_POINT('',(113.610006855633,0.550000000000015,48.5972666207005));
#201115=CARTESIAN_POINT('',(113.552763881763,1.05,48.8917547222302));
#201116=CARTESIAN_POINT('',(113.610006855633,1.05,48.5972666207005));
#201117=CARTESIAN_POINT('Origin',(113.610006855633,0.550000000000015,48.5972666207005));
#201118=CARTESIAN_POINT('',(113.119193353083,0.550000000000015,48.5018616642512));
#201119=CARTESIAN_POINT('',(113.061950379214,0.550000000000015,48.7963497657809));
#201120=CARTESIAN_POINT('',(113.119193353083,0.550000000000015,48.5018616642512));
#201121=CARTESIAN_POINT('',(113.552763881763,0.550000000000015,48.8917547222302));
#201122=CARTESIAN_POINT('',(113.610006855633,0.550000000000015,48.5972666207005));
#201123=CARTESIAN_POINT('Origin',(113.119193353083,0.550000000000015,48.5018616642512));
#201124=CARTESIAN_POINT('',(113.061950379214,0.550000000000015,48.7963497657809));
#201125=CARTESIAN_POINT('',(113.119193353083,0.550000000000015,48.5018616642512));
#201126=CARTESIAN_POINT('Origin',(113.119193353083,0.250000000000015,48.5018616642512));
#201127=CARTESIAN_POINT('',(113.610006855633,0.250000000000015,48.5972666207005));
#201128=CARTESIAN_POINT('',(113.552763881763,0.250000000000015,48.8917547222302));
#201129=CARTESIAN_POINT('',(113.610006855633,0.250000000000015,48.5972666207005));
#201130=CARTESIAN_POINT('',(113.061950379214,0.250000000000015,48.7963497657809));
#201131=CARTESIAN_POINT('',(113.061950379214,0.250000000000015,48.7963497657809));
#201132=CARTESIAN_POINT('',(113.119193353083,0.250000000000015,48.5018616642512));
#201133=CARTESIAN_POINT('',(113.119193353083,0.250000000000015,48.5018616642512));
#201134=CARTESIAN_POINT('',(113.119193353083,0.250000000000015,48.5018616642512));
#201135=CARTESIAN_POINT('Origin',(113.610006855633,0.250000000000015,48.5972666207005));
#201136=CARTESIAN_POINT('',(113.610006855633,-0.249999999999985,48.5972666207005));
#201137=CARTESIAN_POINT('',(113.552763881763,-0.249999999999985,48.8917547222302));
#201138=CARTESIAN_POINT('',(113.610006855633,-0.249999999999985,48.5972666207005));
#201139=CARTESIAN_POINT('',(113.552763881763,0.250000000000015,48.8917547222302));
#201140=CARTESIAN_POINT('',(113.610006855633,0.250000000000015,48.5972666207005));
#201141=CARTESIAN_POINT('Origin',(113.610006855633,-0.249999999999985,48.5972666207005));
#201142=CARTESIAN_POINT('',(113.119193353083,-0.249999999999985,48.5018616642512));
#201143=CARTESIAN_POINT('',(113.061950379214,-0.249999999999985,48.7963497657809));
#201144=CARTESIAN_POINT('',(113.119193353083,-0.249999999999985,48.5018616642512));
#201145=CARTESIAN_POINT('',(113.552763881763,-0.249999999999985,48.8917547222302));
#201146=CARTESIAN_POINT('',(113.610006855633,-0.249999999999985,48.5972666207005));
#201147=CARTESIAN_POINT('Origin',(113.119193353083,-0.249999999999985,48.5018616642512));
#201148=CARTESIAN_POINT('',(113.061950379214,-0.249999999999985,48.7963497657809));
#201149=CARTESIAN_POINT('',(113.119193353083,-0.249999999999985,48.5018616642512));
#201150=CARTESIAN_POINT('Origin',(113.119193353083,-0.549999999999986,48.5018616642512));
#201151=CARTESIAN_POINT('',(113.610006855633,-0.549999999999986,48.5972666207005));
#201152=CARTESIAN_POINT('',(113.552763881763,-0.549999999999986,48.8917547222302));
#201153=CARTESIAN_POINT('',(113.610006855633,-0.549999999999986,48.5972666207005));
#201154=CARTESIAN_POINT('',(113.061950379214,-0.549999999999986,48.7963497657809));
#201155=CARTESIAN_POINT('',(113.061950379214,-0.549999999999986,48.7963497657809));
#201156=CARTESIAN_POINT('',(113.119193353083,-0.549999999999986,48.5018616642512));
#201157=CARTESIAN_POINT('',(113.119193353083,-0.549999999999986,48.5018616642512));
#201158=CARTESIAN_POINT('',(113.119193353083,-0.549999999999986,48.5018616642512));
#201159=CARTESIAN_POINT('Origin',(113.610006855633,-0.549999999999986,48.5972666207005));
#201160=CARTESIAN_POINT('',(113.610006855633,-1.05,48.5972666207005));
#201161=CARTESIAN_POINT('',(113.552763881763,-1.05,48.8917547222302));
#201162=CARTESIAN_POINT('',(113.610006855633,-1.05,48.5972666207005));
#201163=CARTESIAN_POINT('',(113.552763881763,-0.549999999999986,48.8917547222302));
#201164=CARTESIAN_POINT('',(113.610006855633,-0.549999999999986,48.5972666207005));
#201165=CARTESIAN_POINT('Origin',(113.610006855633,-1.05,48.5972666207005));
#201166=CARTESIAN_POINT('',(113.119193353083,-1.05,48.5018616642512));
#201167=CARTESIAN_POINT('',(113.061950379214,-1.05,48.7963497657809));
#201168=CARTESIAN_POINT('',(113.119193353083,-1.05,48.5018616642512));
#201169=CARTESIAN_POINT('',(113.552763881763,-1.05,48.8917547222302));
#201170=CARTESIAN_POINT('',(113.610006855633,-1.05,48.5972666207005));
#201171=CARTESIAN_POINT('Origin',(113.119193353083,-1.05,48.5018616642512));
#201172=CARTESIAN_POINT('',(113.061950379214,-1.05,48.7963497657809));
#201173=CARTESIAN_POINT('',(113.119193353083,-1.05,48.5018616642512));
#201174=CARTESIAN_POINT('Origin',(113.119193353083,-1.35,48.5018616642512));
#201175=CARTESIAN_POINT('',(113.610006855633,-1.35,48.5972666207005));
#201176=CARTESIAN_POINT('',(113.552763881763,-1.35,48.8917547222302));
#201177=CARTESIAN_POINT('',(113.610006855633,-1.35,48.5972666207005));
#201178=CARTESIAN_POINT('',(113.061950379214,-1.35,48.7963497657809));
#201179=CARTESIAN_POINT('',(113.061950379214,-1.35,48.7963497657809));
#201180=CARTESIAN_POINT('',(113.119193353083,-1.35,48.5018616642512));
#201181=CARTESIAN_POINT('',(113.119193353083,-1.35,48.5018616642512));
#201182=CARTESIAN_POINT('',(113.119193353083,-1.35,48.5018616642512));
#201183=CARTESIAN_POINT('Origin',(113.610006855633,-1.35,48.5972666207005));
#201184=CARTESIAN_POINT('',(113.610006855633,-1.85,48.5972666207005));
#201185=CARTESIAN_POINT('',(113.552763881763,-1.85,48.8917547222302));
#201186=CARTESIAN_POINT('',(113.610006855633,-1.85,48.5972666207005));
#201187=CARTESIAN_POINT('',(113.552763881763,-1.35,48.8917547222302));
#201188=CARTESIAN_POINT('',(113.610006855633,-1.35,48.5972666207005));
#201189=CARTESIAN_POINT('Origin',(113.610006855633,-1.85,48.5972666207005));
#201190=CARTESIAN_POINT('',(113.119193353083,-1.85,48.5018616642512));
#201191=CARTESIAN_POINT('',(113.061950379214,-1.85,48.7963497657809));
#201192=CARTESIAN_POINT('',(113.119193353083,-1.85,48.5018616642512));
#201193=CARTESIAN_POINT('',(113.552763881763,-1.85,48.8917547222302));
#201194=CARTESIAN_POINT('',(113.610006855633,-1.85,48.5972666207005));
#201195=CARTESIAN_POINT('Origin',(113.119193353083,-1.85,48.5018616642512));
#201196=CARTESIAN_POINT('',(113.061950379214,-1.85,48.7963497657809));
#201197=CARTESIAN_POINT('',(113.119193353083,-1.85,48.5018616642512));
#201198=CARTESIAN_POINT('Origin',(113.119193353083,-2.15,48.5018616642512));
#201199=CARTESIAN_POINT('',(113.610006855633,-2.15,48.5972666207005));
#201200=CARTESIAN_POINT('',(113.552763881763,-2.15,48.8917547222302));
#201201=CARTESIAN_POINT('',(113.610006855633,-2.15,48.5972666207005));
#201202=CARTESIAN_POINT('',(113.061950379214,-2.15,48.7963497657809));
#201203=CARTESIAN_POINT('',(113.061950379214,-2.15,48.7963497657809));
#201204=CARTESIAN_POINT('',(113.119193353083,-2.15,48.5018616642512));
#201205=CARTESIAN_POINT('',(113.119193353083,-2.15,48.5018616642512));
#201206=CARTESIAN_POINT('',(113.119193353083,-2.15,48.5018616642512));
#201207=CARTESIAN_POINT('Origin',(113.610006855633,-2.15,48.5972666207005));
#201208=CARTESIAN_POINT('',(113.610006855633,-2.65,48.5972666207005));
#201209=CARTESIAN_POINT('',(113.552763881763,-2.65,48.8917547222302));
#201210=CARTESIAN_POINT('',(113.610006855633,-2.65,48.5972666207005));
#201211=CARTESIAN_POINT('',(113.552763881763,-2.15,48.8917547222302));
#201212=CARTESIAN_POINT('',(113.610006855633,-2.15,48.5972666207005));
#201213=CARTESIAN_POINT('Origin',(113.610006855633,-2.65,48.5972666207005));
#201214=CARTESIAN_POINT('',(113.119193353083,-2.65,48.5018616642512));
#201215=CARTESIAN_POINT('',(113.061950379214,-2.65,48.7963497657809));
#201216=CARTESIAN_POINT('',(113.119193353083,-2.65,48.5018616642512));
#201217=CARTESIAN_POINT('',(113.552763881763,-2.65,48.8917547222302));
#201218=CARTESIAN_POINT('',(113.610006855633,-2.65,48.5972666207005));
#201219=CARTESIAN_POINT('Origin',(113.119193353083,-2.65,48.5018616642512));
#201220=CARTESIAN_POINT('',(113.061950379214,-2.65,48.7963497657809));
#201221=CARTESIAN_POINT('',(113.119193353083,-2.65,48.5018616642512));
#201222=CARTESIAN_POINT('Origin',(113.119193353083,-2.95,48.5018616642512));
#201223=CARTESIAN_POINT('',(113.610006855633,-2.95,48.5972666207005));
#201224=CARTESIAN_POINT('',(113.552763881763,-2.95,48.8917547222302));
#201225=CARTESIAN_POINT('',(113.610006855633,-2.95,48.5972666207005));
#201226=CARTESIAN_POINT('',(113.061950379214,-2.95,48.7963497657809));
#201227=CARTESIAN_POINT('',(113.061950379214,-2.95,48.7963497657809));
#201228=CARTESIAN_POINT('',(113.119193353083,-2.95,48.5018616642512));
#201229=CARTESIAN_POINT('',(113.119193353083,-2.95,48.5018616642512));
#201230=CARTESIAN_POINT('',(113.119193353083,-2.95,48.5018616642512));
#201231=CARTESIAN_POINT('Origin',(113.610006855633,-2.95,48.5972666207005));
#201232=CARTESIAN_POINT('',(113.610006855633,-3.45,48.5972666207005));
#201233=CARTESIAN_POINT('',(113.552763881763,-3.45,48.8917547222302));
#201234=CARTESIAN_POINT('',(113.610006855633,-3.45,48.5972666207005));
#201235=CARTESIAN_POINT('',(113.552763881763,-2.95,48.8917547222302));
#201236=CARTESIAN_POINT('',(113.610006855633,-2.95,48.5972666207005));
#201237=CARTESIAN_POINT('Origin',(113.610006855633,-3.45,48.5972666207005));
#201238=CARTESIAN_POINT('',(113.119193353083,-3.45,48.5018616642512));
#201239=CARTESIAN_POINT('',(113.061950379214,-3.45,48.7963497657809));
#201240=CARTESIAN_POINT('',(113.119193353083,-3.45,48.5018616642512));
#201241=CARTESIAN_POINT('',(113.552763881763,-3.45,48.8917547222302));
#201242=CARTESIAN_POINT('',(113.610006855633,-3.45,48.5972666207005));
#201243=CARTESIAN_POINT('Origin',(113.119193353083,-3.45,48.5018616642512));
#201244=CARTESIAN_POINT('',(113.061950379214,-3.45,48.7963497657809));
#201245=CARTESIAN_POINT('',(113.119193353083,-3.45,48.5018616642512));
#201246=CARTESIAN_POINT('Origin',(113.119193353083,-3.75,48.5018616642512));
#201247=CARTESIAN_POINT('',(113.610006855633,-3.75,48.5972666207005));
#201248=CARTESIAN_POINT('',(113.552763881763,-3.75,48.8917547222302));
#201249=CARTESIAN_POINT('',(113.610006855633,-3.75,48.5972666207005));
#201250=CARTESIAN_POINT('',(113.061950379214,-3.75,48.7963497657809));
#201251=CARTESIAN_POINT('',(113.061950379214,-3.75,48.7963497657809));
#201252=CARTESIAN_POINT('',(113.119193353083,-3.75,48.5018616642512));
#201253=CARTESIAN_POINT('',(113.119193353083,-3.75,48.5018616642512));
#201254=CARTESIAN_POINT('',(113.119193353083,-3.75,48.5018616642512));
#201255=CARTESIAN_POINT('Origin',(113.610006855633,-3.75,48.5972666207005));
#201256=CARTESIAN_POINT('',(113.610006855633,-4.25,48.5972666207005));
#201257=CARTESIAN_POINT('',(113.552763881763,-4.25,48.8917547222302));
#201258=CARTESIAN_POINT('',(113.610006855633,-4.25,48.5972666207005));
#201259=CARTESIAN_POINT('',(113.552763881763,-3.75,48.8917547222302));
#201260=CARTESIAN_POINT('',(113.610006855633,-3.75,48.5972666207005));
#201261=CARTESIAN_POINT('Origin',(113.610006855633,-4.25,48.5972666207005));
#201262=CARTESIAN_POINT('',(113.119193353083,-4.25,48.5018616642512));
#201263=CARTESIAN_POINT('',(113.061950379214,-4.25,48.7963497657809));
#201264=CARTESIAN_POINT('',(113.119193353083,-4.25,48.5018616642512));
#201265=CARTESIAN_POINT('',(113.552763881763,-4.25,48.8917547222302));
#201266=CARTESIAN_POINT('',(113.610006855633,-4.25,48.5972666207005));
#201267=CARTESIAN_POINT('Origin',(113.119193353083,-4.25,48.5018616642512));
#201268=CARTESIAN_POINT('',(113.061950379214,-4.25,48.7963497657809));
#201269=CARTESIAN_POINT('',(113.119193353083,-4.25,48.5018616642512));
#201270=CARTESIAN_POINT('Origin',(113.904494957163,-3.75,48.65450959457));
#201271=CARTESIAN_POINT('',(114.395308459712,-3.75,48.7499145510193));
#201272=CARTESIAN_POINT('',(114.338065485842,-3.75,49.044402652549));
#201273=CARTESIAN_POINT('',(114.395308459712,-3.75,48.7499145510193));
#201274=CARTESIAN_POINT('',(113.847251983293,-3.75,48.9489976960997));
#201275=CARTESIAN_POINT('',(113.847251983293,-3.75,48.9489976960997));
#201276=CARTESIAN_POINT('',(113.904494957163,-3.75,48.65450959457));
#201277=CARTESIAN_POINT('',(113.904494957163,-3.75,48.65450959457));
#201278=CARTESIAN_POINT('',(113.904494957163,-3.75,48.65450959457));
#201279=CARTESIAN_POINT('Origin',(114.395308459712,-3.75,48.7499145510193));
#201280=CARTESIAN_POINT('',(114.395308459712,-4.25,48.7499145510193));
#201281=CARTESIAN_POINT('',(114.338065485842,-4.25,49.044402652549));
#201282=CARTESIAN_POINT('',(114.395308459712,-4.25,48.7499145510193));
#201283=CARTESIAN_POINT('',(114.338065485842,-3.75,49.044402652549));
#201284=CARTESIAN_POINT('',(114.395308459712,-3.75,48.7499145510193));
#201285=CARTESIAN_POINT('Origin',(114.395308459712,-4.25,48.7499145510193));
#201286=CARTESIAN_POINT('',(113.904494957163,-4.25,48.65450959457));
#201287=CARTESIAN_POINT('',(113.847251983293,-4.25,48.9489976960997));
#201288=CARTESIAN_POINT('',(113.904494957163,-4.25,48.65450959457));
#201289=CARTESIAN_POINT('',(114.338065485842,-4.25,49.044402652549));
#201290=CARTESIAN_POINT('',(114.395308459712,-4.25,48.7499145510193));
#201291=CARTESIAN_POINT('Origin',(113.904494957163,-4.25,48.65450959457));
#201292=CARTESIAN_POINT('',(113.847251983293,-4.25,48.9489976960997));
#201293=CARTESIAN_POINT('',(113.904494957163,-4.25,48.65450959457));
#201294=CARTESIAN_POINT('Origin',(114.689796561242,-3.75,48.8071575248888));
#201295=CARTESIAN_POINT('',(115.180610063791,-3.75,48.9025624813381));
#201296=CARTESIAN_POINT('',(115.123367089922,-3.75,49.1970505828678));
#201297=CARTESIAN_POINT('',(115.180610063791,-3.75,48.9025624813381));
#201298=CARTESIAN_POINT('',(114.632553587372,-3.75,49.1016456264185));
#201299=CARTESIAN_POINT('',(114.632553587372,-3.75,49.1016456264185));
#201300=CARTESIAN_POINT('',(114.689796561242,-3.75,48.8071575248888));
#201301=CARTESIAN_POINT('',(114.689796561242,-3.75,48.8071575248888));
#201302=CARTESIAN_POINT('',(114.689796561242,-3.75,48.8071575248888));
#201303=CARTESIAN_POINT('Origin',(115.180610063791,-3.75,48.9025624813381));
#201304=CARTESIAN_POINT('',(115.180610063791,-4.25,48.9025624813381));
#201305=CARTESIAN_POINT('',(115.123367089922,-4.25,49.1970505828678));
#201306=CARTESIAN_POINT('',(115.180610063791,-4.25,48.9025624813381));
#201307=CARTESIAN_POINT('',(115.123367089922,-3.75,49.1970505828678));
#201308=CARTESIAN_POINT('',(115.180610063791,-3.75,48.9025624813381));
#201309=CARTESIAN_POINT('Origin',(115.180610063791,-4.25,48.9025624813381));
#201310=CARTESIAN_POINT('',(114.689796561242,-4.25,48.8071575248888));
#201311=CARTESIAN_POINT('',(114.632553587372,-4.25,49.1016456264185));
#201312=CARTESIAN_POINT('',(114.689796561242,-4.25,48.8071575248888));
#201313=CARTESIAN_POINT('',(115.123367089922,-4.25,49.1970505828678));
#201314=CARTESIAN_POINT('',(115.180610063791,-4.25,48.9025624813381));
#201315=CARTESIAN_POINT('Origin',(114.689796561242,-4.25,48.8071575248888));
#201316=CARTESIAN_POINT('',(114.632553587372,-4.25,49.1016456264185));
#201317=CARTESIAN_POINT('',(114.689796561242,-4.25,48.8071575248888));
#201318=CARTESIAN_POINT('Origin',(115.475098165321,-3.75,48.9598054552076));
#201319=CARTESIAN_POINT('',(115.96591166787,-3.75,49.0552104116569));
#201320=CARTESIAN_POINT('',(115.908668694001,-3.75,49.3496985131866));
#201321=CARTESIAN_POINT('',(115.96591166787,-3.75,49.0552104116569));
#201322=CARTESIAN_POINT('',(115.417855191451,-3.75,49.2542935567373));
#201323=CARTESIAN_POINT('',(115.417855191451,-3.75,49.2542935567373));
#201324=CARTESIAN_POINT('',(115.475098165321,-3.75,48.9598054552076));
#201325=CARTESIAN_POINT('',(115.475098165321,-3.75,48.9598054552076));
#201326=CARTESIAN_POINT('',(115.475098165321,-3.75,48.9598054552076));
#201327=CARTESIAN_POINT('Origin',(115.96591166787,-3.75,49.0552104116569));
#201328=CARTESIAN_POINT('',(115.96591166787,-4.25,49.0552104116569));
#201329=CARTESIAN_POINT('',(115.908668694001,-4.25,49.3496985131866));
#201330=CARTESIAN_POINT('',(115.96591166787,-4.25,49.0552104116569));
#201331=CARTESIAN_POINT('',(115.908668694001,-3.75,49.3496985131866));
#201332=CARTESIAN_POINT('',(115.96591166787,-3.75,49.0552104116569));
#201333=CARTESIAN_POINT('Origin',(115.96591166787,-4.25,49.0552104116569));
#201334=CARTESIAN_POINT('',(115.475098165321,-4.25,48.9598054552076));
#201335=CARTESIAN_POINT('',(115.417855191451,-4.25,49.2542935567373));
#201336=CARTESIAN_POINT('',(115.475098165321,-4.25,48.9598054552076));
#201337=CARTESIAN_POINT('',(115.908668694001,-4.25,49.3496985131866));
#201338=CARTESIAN_POINT('',(115.96591166787,-4.25,49.0552104116569));
#201339=CARTESIAN_POINT('Origin',(115.475098165321,-4.25,48.9598054552076));
#201340=CARTESIAN_POINT('',(115.417855191451,-4.25,49.2542935567373));
#201341=CARTESIAN_POINT('',(115.475098165321,-4.25,48.9598054552076));
#201342=CARTESIAN_POINT('Origin',(116.2603997694,-3.75,49.1124533855264));
#201343=CARTESIAN_POINT('',(116.75121327195,-3.75,49.2078583419757));
#201344=CARTESIAN_POINT('',(116.69397029808,-3.75,49.5023464435054));
#201345=CARTESIAN_POINT('',(116.75121327195,-3.75,49.2078583419757));
#201346=CARTESIAN_POINT('',(116.203156795531,-3.75,49.4069414870561));
#201347=CARTESIAN_POINT('',(116.203156795531,-3.75,49.4069414870561));
#201348=CARTESIAN_POINT('',(116.2603997694,-3.75,49.1124533855264));
#201349=CARTESIAN_POINT('',(116.2603997694,-3.75,49.1124533855264));
#201350=CARTESIAN_POINT('',(116.2603997694,-3.75,49.1124533855264));
#201351=CARTESIAN_POINT('Origin',(116.75121327195,-3.75,49.2078583419757));
#201352=CARTESIAN_POINT('',(116.75121327195,-4.25,49.2078583419757));
#201353=CARTESIAN_POINT('',(116.69397029808,-4.25,49.5023464435054));
#201354=CARTESIAN_POINT('',(116.75121327195,-4.25,49.2078583419757));
#201355=CARTESIAN_POINT('',(116.69397029808,-3.75,49.5023464435054));
#201356=CARTESIAN_POINT('',(116.75121327195,-3.75,49.2078583419757));
#201357=CARTESIAN_POINT('Origin',(116.75121327195,-4.25,49.2078583419757));
#201358=CARTESIAN_POINT('',(116.2603997694,-4.25,49.1124533855264));
#201359=CARTESIAN_POINT('',(116.203156795531,-4.25,49.4069414870561));
#201360=CARTESIAN_POINT('',(116.2603997694,-4.25,49.1124533855264));
#201361=CARTESIAN_POINT('',(116.69397029808,-4.25,49.5023464435054));
#201362=CARTESIAN_POINT('',(116.75121327195,-4.25,49.2078583419757));
#201363=CARTESIAN_POINT('Origin',(116.2603997694,-4.25,49.1124533855264));
#201364=CARTESIAN_POINT('',(116.203156795531,-4.25,49.4069414870561));
#201365=CARTESIAN_POINT('',(116.2603997694,-4.25,49.1124533855264));
#201366=CARTESIAN_POINT('Origin',(117.045701373479,-3.75,49.2651013158452));
#201367=CARTESIAN_POINT('',(117.536514876029,-3.75,49.3605062722945));
#201368=CARTESIAN_POINT('',(117.479271902159,-3.75,49.6549943738242));
#201369=CARTESIAN_POINT('',(117.536514876029,-3.75,49.3605062722945));
#201370=CARTESIAN_POINT('',(116.98845839961,-3.75,49.5595894173749));
#201371=CARTESIAN_POINT('',(116.98845839961,-3.75,49.5595894173749));
#201372=CARTESIAN_POINT('',(117.045701373479,-3.75,49.2651013158452));
#201373=CARTESIAN_POINT('',(117.045701373479,-3.75,49.2651013158452));
#201374=CARTESIAN_POINT('',(117.045701373479,-3.75,49.2651013158452));
#201375=CARTESIAN_POINT('Origin',(117.536514876029,-3.75,49.3605062722945));
#201376=CARTESIAN_POINT('',(117.536514876029,-4.25,49.3605062722945));
#201377=CARTESIAN_POINT('',(117.479271902159,-4.25,49.6549943738242));
#201378=CARTESIAN_POINT('',(117.536514876029,-4.25,49.3605062722945));
#201379=CARTESIAN_POINT('',(117.479271902159,-3.75,49.6549943738242));
#201380=CARTESIAN_POINT('',(117.536514876029,-3.75,49.3605062722945));
#201381=CARTESIAN_POINT('Origin',(117.536514876029,-4.25,49.3605062722945));
#201382=CARTESIAN_POINT('',(117.045701373479,-4.25,49.2651013158452));
#201383=CARTESIAN_POINT('',(116.98845839961,-4.25,49.5595894173749));
#201384=CARTESIAN_POINT('',(117.045701373479,-4.25,49.2651013158452));
#201385=CARTESIAN_POINT('',(117.479271902159,-4.25,49.6549943738242));
#201386=CARTESIAN_POINT('',(117.536514876029,-4.25,49.3605062722945));
#201387=CARTESIAN_POINT('Origin',(117.045701373479,-4.25,49.2651013158452));
#201388=CARTESIAN_POINT('',(116.98845839961,-4.25,49.5595894173749));
#201389=CARTESIAN_POINT('',(117.045701373479,-4.25,49.2651013158452));
#201390=CARTESIAN_POINT('Origin',(117.831002977559,-3.75,49.417749246164));
#201391=CARTESIAN_POINT('',(118.321816480108,-3.75,49.5131542026133));
#201392=CARTESIAN_POINT('',(118.264573506239,-3.75,49.807642304143));
#201393=CARTESIAN_POINT('',(118.321816480108,-3.75,49.5131542026133));
#201394=CARTESIAN_POINT('',(117.773760003689,-3.75,49.7122373476937));
#201395=CARTESIAN_POINT('',(117.773760003689,-3.75,49.7122373476937));
#201396=CARTESIAN_POINT('',(117.831002977559,-3.75,49.417749246164));
#201397=CARTESIAN_POINT('',(117.831002977559,-3.75,49.417749246164));
#201398=CARTESIAN_POINT('',(117.831002977559,-3.75,49.417749246164));
#201399=CARTESIAN_POINT('Origin',(118.321816480108,-3.75,49.5131542026133));
#201400=CARTESIAN_POINT('',(118.321816480108,-4.25,49.5131542026133));
#201401=CARTESIAN_POINT('',(118.264573506239,-4.25,49.807642304143));
#201402=CARTESIAN_POINT('',(118.321816480108,-4.25,49.5131542026133));
#201403=CARTESIAN_POINT('',(118.264573506239,-3.75,49.807642304143));
#201404=CARTESIAN_POINT('',(118.321816480108,-3.75,49.5131542026133));
#201405=CARTESIAN_POINT('Origin',(118.321816480108,-4.25,49.5131542026133));
#201406=CARTESIAN_POINT('',(117.831002977559,-4.25,49.417749246164));
#201407=CARTESIAN_POINT('',(117.773760003689,-4.25,49.7122373476937));
#201408=CARTESIAN_POINT('',(117.831002977559,-4.25,49.417749246164));
#201409=CARTESIAN_POINT('',(118.264573506239,-4.25,49.807642304143));
#201410=CARTESIAN_POINT('',(118.321816480108,-4.25,49.5131542026133));
#201411=CARTESIAN_POINT('Origin',(117.831002977559,-4.25,49.417749246164));
#201412=CARTESIAN_POINT('',(117.773760003689,-4.25,49.7122373476937));
#201413=CARTESIAN_POINT('',(117.831002977559,-4.25,49.417749246164));
#201414=CARTESIAN_POINT('Origin',(118.616304581638,-3.75,49.5703971764828));
#201415=CARTESIAN_POINT('',(119.107118084187,-3.75,49.6658021329321));
#201416=CARTESIAN_POINT('',(119.049875110318,-3.75,49.9602902344618));
#201417=CARTESIAN_POINT('',(119.107118084187,-3.75,49.6658021329321));
#201418=CARTESIAN_POINT('',(118.559061607768,-3.75,49.8648852780125));
#201419=CARTESIAN_POINT('',(118.559061607768,-3.75,49.8648852780125));
#201420=CARTESIAN_POINT('',(118.616304581638,-3.75,49.5703971764828));
#201421=CARTESIAN_POINT('',(118.616304581638,-3.75,49.5703971764828));
#201422=CARTESIAN_POINT('',(118.616304581638,-3.75,49.5703971764828));
#201423=CARTESIAN_POINT('Origin',(119.107118084187,-3.75,49.6658021329321));
#201424=CARTESIAN_POINT('',(119.107118084187,-4.25,49.6658021329321));
#201425=CARTESIAN_POINT('',(119.049875110318,-4.25,49.9602902344618));
#201426=CARTESIAN_POINT('',(119.107118084187,-4.25,49.6658021329321));
#201427=CARTESIAN_POINT('',(119.049875110318,-3.75,49.9602902344618));
#201428=CARTESIAN_POINT('',(119.107118084187,-3.75,49.6658021329321));
#201429=CARTESIAN_POINT('Origin',(119.107118084187,-4.25,49.6658021329321));
#201430=CARTESIAN_POINT('',(118.616304581638,-4.25,49.5703971764828));
#201431=CARTESIAN_POINT('',(118.559061607768,-4.25,49.8648852780125));
#201432=CARTESIAN_POINT('',(118.616304581638,-4.25,49.5703971764828));
#201433=CARTESIAN_POINT('',(119.049875110318,-4.25,49.9602902344618));
#201434=CARTESIAN_POINT('',(119.107118084187,-4.25,49.6658021329321));
#201435=CARTESIAN_POINT('Origin',(118.616304581638,-4.25,49.5703971764828));
#201436=CARTESIAN_POINT('',(118.559061607768,-4.25,49.8648852780125));
#201437=CARTESIAN_POINT('',(118.616304581638,-4.25,49.5703971764828));
#201438=CARTESIAN_POINT('Origin',(119.401606185717,-3.75,49.7230451068016));
#201439=CARTESIAN_POINT('',(119.892419688267,-3.75,49.8184500632509));
#201440=CARTESIAN_POINT('',(119.835176714397,-3.75,50.1129381647806));
#201441=CARTESIAN_POINT('',(119.892419688267,-3.75,49.8184500632509));
#201442=CARTESIAN_POINT('',(119.344363211847,-3.75,50.0175332083313));
#201443=CARTESIAN_POINT('',(119.344363211847,-3.75,50.0175332083313));
#201444=CARTESIAN_POINT('',(119.401606185717,-3.75,49.7230451068016));
#201445=CARTESIAN_POINT('',(119.401606185717,-3.75,49.7230451068016));
#201446=CARTESIAN_POINT('',(119.401606185717,-3.75,49.7230451068016));
#201447=CARTESIAN_POINT('Origin',(119.892419688267,-3.75,49.8184500632509));
#201448=CARTESIAN_POINT('',(119.892419688267,-4.25,49.8184500632509));
#201449=CARTESIAN_POINT('',(119.835176714397,-4.25,50.1129381647806));
#201450=CARTESIAN_POINT('',(119.892419688267,-4.25,49.8184500632509));
#201451=CARTESIAN_POINT('',(119.835176714397,-3.75,50.1129381647806));
#201452=CARTESIAN_POINT('',(119.892419688267,-3.75,49.8184500632509));
#201453=CARTESIAN_POINT('Origin',(119.892419688267,-4.25,49.8184500632509));
#201454=CARTESIAN_POINT('',(119.401606185717,-4.25,49.7230451068016));
#201455=CARTESIAN_POINT('',(119.344363211847,-4.25,50.0175332083313));
#201456=CARTESIAN_POINT('',(119.401606185717,-4.25,49.7230451068016));
#201457=CARTESIAN_POINT('',(119.835176714397,-4.25,50.1129381647806));
#201458=CARTESIAN_POINT('',(119.892419688267,-4.25,49.8184500632509));
#201459=CARTESIAN_POINT('Origin',(119.401606185717,-4.25,49.7230451068016));
#201460=CARTESIAN_POINT('',(119.344363211847,-4.25,50.0175332083313));
#201461=CARTESIAN_POINT('',(119.401606185717,-4.25,49.7230451068016));
#201462=CARTESIAN_POINT('Origin',(120.186907789796,-3.75,49.8756930371204));
#201463=CARTESIAN_POINT('',(120.677721292346,-3.75,49.9710979935697));
#201464=CARTESIAN_POINT('',(120.620478318476,-3.75,50.2655860950994));
#201465=CARTESIAN_POINT('',(120.677721292346,-3.75,49.9710979935697));
#201466=CARTESIAN_POINT('',(120.129664815927,-3.75,50.1701811386501));
#201467=CARTESIAN_POINT('',(120.129664815927,-3.75,50.1701811386501));
#201468=CARTESIAN_POINT('',(120.186907789796,-3.75,49.8756930371204));
#201469=CARTESIAN_POINT('',(120.186907789796,-3.75,49.8756930371204));
#201470=CARTESIAN_POINT('',(120.186907789796,-3.75,49.8756930371204));
#201471=CARTESIAN_POINT('Origin',(120.677721292346,-3.75,49.9710979935697));
#201472=CARTESIAN_POINT('',(120.677721292346,-4.25,49.9710979935697));
#201473=CARTESIAN_POINT('',(120.620478318476,-4.25,50.2655860950994));
#201474=CARTESIAN_POINT('',(120.677721292346,-4.25,49.9710979935697));
#201475=CARTESIAN_POINT('',(120.620478318476,-3.75,50.2655860950994));
#201476=CARTESIAN_POINT('',(120.677721292346,-3.75,49.9710979935697));
#201477=CARTESIAN_POINT('Origin',(120.677721292346,-4.25,49.9710979935697));
#201478=CARTESIAN_POINT('',(120.186907789796,-4.25,49.8756930371204));
#201479=CARTESIAN_POINT('',(120.129664815927,-4.25,50.1701811386501));
#201480=CARTESIAN_POINT('',(120.186907789796,-4.25,49.8756930371204));
#201481=CARTESIAN_POINT('',(120.620478318476,-4.25,50.2655860950994));
#201482=CARTESIAN_POINT('',(120.677721292346,-4.25,49.9710979935697));
#201483=CARTESIAN_POINT('Origin',(120.186907789796,-4.25,49.8756930371204));
#201484=CARTESIAN_POINT('',(120.129664815927,-4.25,50.1701811386501));
#201485=CARTESIAN_POINT('',(120.186907789796,-4.25,49.8756930371204));
#201486=CARTESIAN_POINT('Origin',(120.972209393875,-3.75,50.0283409674392));
#201487=CARTESIAN_POINT('',(121.463022896425,-3.75,50.1237459238885));
#201488=CARTESIAN_POINT('',(121.405779922555,-3.75,50.4182340254182));
#201489=CARTESIAN_POINT('',(121.463022896425,-3.75,50.1237459238885));
#201490=CARTESIAN_POINT('',(120.914966420006,-3.75,50.3228290689689));
#201491=CARTESIAN_POINT('',(120.914966420006,-3.75,50.3228290689689));
#201492=CARTESIAN_POINT('',(120.972209393875,-3.75,50.0283409674392));
#201493=CARTESIAN_POINT('',(120.972209393875,-3.75,50.0283409674392));
#201494=CARTESIAN_POINT('',(120.972209393875,-3.75,50.0283409674392));
#201495=CARTESIAN_POINT('Origin',(121.463022896425,-3.75,50.1237459238885));
#201496=CARTESIAN_POINT('',(121.463022896425,-4.25,50.1237459238885));
#201497=CARTESIAN_POINT('',(121.405779922555,-4.25,50.4182340254182));
#201498=CARTESIAN_POINT('',(121.463022896425,-4.25,50.1237459238885));
#201499=CARTESIAN_POINT('',(121.405779922555,-3.75,50.4182340254182));
#201500=CARTESIAN_POINT('',(121.463022896425,-3.75,50.1237459238885));
#201501=CARTESIAN_POINT('Origin',(121.463022896425,-4.25,50.1237459238885));
#201502=CARTESIAN_POINT('',(120.972209393875,-4.25,50.0283409674392));
#201503=CARTESIAN_POINT('',(120.914966420006,-4.25,50.3228290689689));
#201504=CARTESIAN_POINT('',(120.972209393875,-4.25,50.0283409674392));
#201505=CARTESIAN_POINT('',(121.405779922555,-4.25,50.4182340254182));
#201506=CARTESIAN_POINT('',(121.463022896425,-4.25,50.1237459238885));
#201507=CARTESIAN_POINT('Origin',(120.972209393875,-4.25,50.0283409674392));
#201508=CARTESIAN_POINT('',(120.914966420006,-4.25,50.3228290689689));
#201509=CARTESIAN_POINT('',(120.972209393875,-4.25,50.0283409674392));
#201510=CARTESIAN_POINT('Origin',(120.972209393875,-2.95,50.0283409674392));
#201511=CARTESIAN_POINT('',(121.463022896425,-2.95,50.1237459238885));
#201512=CARTESIAN_POINT('',(121.405779922555,-2.95,50.4182340254182));
#201513=CARTESIAN_POINT('',(121.463022896425,-2.95,50.1237459238885));
#201514=CARTESIAN_POINT('',(120.914966420006,-2.95,50.3228290689689));
#201515=CARTESIAN_POINT('',(120.914966420006,-2.95,50.3228290689689));
#201516=CARTESIAN_POINT('',(120.972209393875,-2.95,50.0283409674392));
#201517=CARTESIAN_POINT('',(120.972209393875,-2.95,50.0283409674392));
#201518=CARTESIAN_POINT('',(120.972209393875,-2.95,50.0283409674392));
#201519=CARTESIAN_POINT('Origin',(121.463022896425,-2.95,50.1237459238885));
#201520=CARTESIAN_POINT('',(121.463022896425,-3.45,50.1237459238885));
#201521=CARTESIAN_POINT('',(121.405779922555,-3.45,50.4182340254182));
#201522=CARTESIAN_POINT('',(121.463022896425,-3.45,50.1237459238885));
#201523=CARTESIAN_POINT('',(121.405779922555,-2.95,50.4182340254182));
#201524=CARTESIAN_POINT('',(121.463022896425,-2.95,50.1237459238885));
#201525=CARTESIAN_POINT('Origin',(121.463022896425,-3.45,50.1237459238885));
#201526=CARTESIAN_POINT('',(120.972209393875,-3.45,50.0283409674392));
#201527=CARTESIAN_POINT('',(120.914966420006,-3.45,50.3228290689689));
#201528=CARTESIAN_POINT('',(120.972209393875,-3.45,50.0283409674392));
#201529=CARTESIAN_POINT('',(121.405779922555,-3.45,50.4182340254182));
#201530=CARTESIAN_POINT('',(121.463022896425,-3.45,50.1237459238885));
#201531=CARTESIAN_POINT('Origin',(120.972209393875,-3.45,50.0283409674392));
#201532=CARTESIAN_POINT('',(120.914966420006,-3.45,50.3228290689689));
#201533=CARTESIAN_POINT('',(120.972209393875,-3.45,50.0283409674392));
#201534=CARTESIAN_POINT('Origin',(120.972209393875,-2.15,50.0283409674392));
#201535=CARTESIAN_POINT('',(121.463022896425,-2.15,50.1237459238885));
#201536=CARTESIAN_POINT('',(121.405779922555,-2.15,50.4182340254182));
#201537=CARTESIAN_POINT('',(121.463022896425,-2.15,50.1237459238885));
#201538=CARTESIAN_POINT('',(120.914966420006,-2.15,50.3228290689689));
#201539=CARTESIAN_POINT('',(120.914966420006,-2.15,50.3228290689689));
#201540=CARTESIAN_POINT('',(120.972209393875,-2.15,50.0283409674392));
#201541=CARTESIAN_POINT('',(120.972209393875,-2.15,50.0283409674392));
#201542=CARTESIAN_POINT('',(120.972209393875,-2.15,50.0283409674392));
#201543=CARTESIAN_POINT('Origin',(121.463022896425,-2.15,50.1237459238885));
#201544=CARTESIAN_POINT('',(121.463022896425,-2.65,50.1237459238885));
#201545=CARTESIAN_POINT('',(121.405779922555,-2.65,50.4182340254182));
#201546=CARTESIAN_POINT('',(121.463022896425,-2.65,50.1237459238885));
#201547=CARTESIAN_POINT('',(121.405779922555,-2.15,50.4182340254182));
#201548=CARTESIAN_POINT('',(121.463022896425,-2.15,50.1237459238885));
#201549=CARTESIAN_POINT('Origin',(121.463022896425,-2.65,50.1237459238885));
#201550=CARTESIAN_POINT('',(120.972209393875,-2.65,50.0283409674392));
#201551=CARTESIAN_POINT('',(120.914966420006,-2.65,50.3228290689689));
#201552=CARTESIAN_POINT('',(120.972209393875,-2.65,50.0283409674392));
#201553=CARTESIAN_POINT('',(121.405779922555,-2.65,50.4182340254182));
#201554=CARTESIAN_POINT('',(121.463022896425,-2.65,50.1237459238885));
#201555=CARTESIAN_POINT('Origin',(120.972209393875,-2.65,50.0283409674392));
#201556=CARTESIAN_POINT('',(120.914966420006,-2.65,50.3228290689689));
#201557=CARTESIAN_POINT('',(120.972209393875,-2.65,50.0283409674392));
#201558=CARTESIAN_POINT('Origin',(120.972209393875,-1.35,50.0283409674392));
#201559=CARTESIAN_POINT('',(121.463022896425,-1.35,50.1237459238885));
#201560=CARTESIAN_POINT('',(121.405779922555,-1.35,50.4182340254182));
#201561=CARTESIAN_POINT('',(121.463022896425,-1.35,50.1237459238885));
#201562=CARTESIAN_POINT('',(120.914966420006,-1.35,50.3228290689689));
#201563=CARTESIAN_POINT('',(120.914966420006,-1.35,50.3228290689689));
#201564=CARTESIAN_POINT('',(120.972209393875,-1.35,50.0283409674392));
#201565=CARTESIAN_POINT('',(120.972209393875,-1.35,50.0283409674392));
#201566=CARTESIAN_POINT('',(120.972209393875,-1.35,50.0283409674392));
#201567=CARTESIAN_POINT('Origin',(121.463022896425,-1.35,50.1237459238885));
#201568=CARTESIAN_POINT('',(121.463022896425,-1.85,50.1237459238885));
#201569=CARTESIAN_POINT('',(121.405779922555,-1.85,50.4182340254182));
#201570=CARTESIAN_POINT('',(121.463022896425,-1.85,50.1237459238885));
#201571=CARTESIAN_POINT('',(121.405779922555,-1.35,50.4182340254182));
#201572=CARTESIAN_POINT('',(121.463022896425,-1.35,50.1237459238885));
#201573=CARTESIAN_POINT('Origin',(121.463022896425,-1.85,50.1237459238885));
#201574=CARTESIAN_POINT('',(120.972209393875,-1.85,50.0283409674392));
#201575=CARTESIAN_POINT('',(120.914966420006,-1.85,50.3228290689689));
#201576=CARTESIAN_POINT('',(120.972209393875,-1.85,50.0283409674392));
#201577=CARTESIAN_POINT('',(121.405779922555,-1.85,50.4182340254182));
#201578=CARTESIAN_POINT('',(121.463022896425,-1.85,50.1237459238885));
#201579=CARTESIAN_POINT('Origin',(120.972209393875,-1.85,50.0283409674392));
#201580=CARTESIAN_POINT('',(120.914966420006,-1.85,50.3228290689689));
#201581=CARTESIAN_POINT('',(120.972209393875,-1.85,50.0283409674392));
#201582=CARTESIAN_POINT('Origin',(120.972209393875,-0.549999999999986,50.0283409674392));
#201583=CARTESIAN_POINT('',(121.463022896425,-0.549999999999986,50.1237459238885));
#201584=CARTESIAN_POINT('',(121.405779922555,-0.549999999999986,50.4182340254182));
#201585=CARTESIAN_POINT('',(121.463022896425,-0.549999999999986,50.1237459238885));
#201586=CARTESIAN_POINT('',(120.914966420006,-0.549999999999986,50.3228290689689));
#201587=CARTESIAN_POINT('',(120.914966420006,-0.549999999999986,50.3228290689689));
#201588=CARTESIAN_POINT('',(120.972209393875,-0.549999999999986,50.0283409674392));
#201589=CARTESIAN_POINT('',(120.972209393875,-0.549999999999986,50.0283409674392));
#201590=CARTESIAN_POINT('',(120.972209393875,-0.549999999999986,50.0283409674392));
#201591=CARTESIAN_POINT('Origin',(121.463022896425,-0.549999999999986,50.1237459238885));
#201592=CARTESIAN_POINT('',(121.463022896425,-1.05,50.1237459238885));
#201593=CARTESIAN_POINT('',(121.405779922555,-1.05,50.4182340254182));
#201594=CARTESIAN_POINT('',(121.463022896425,-1.05,50.1237459238885));
#201595=CARTESIAN_POINT('',(121.405779922555,-0.549999999999986,50.4182340254182));
#201596=CARTESIAN_POINT('',(121.463022896425,-0.549999999999986,50.1237459238885));
#201597=CARTESIAN_POINT('Origin',(121.463022896425,-1.05,50.1237459238885));
#201598=CARTESIAN_POINT('',(120.972209393875,-1.05,50.0283409674392));
#201599=CARTESIAN_POINT('',(120.914966420006,-1.05,50.3228290689689));
#201600=CARTESIAN_POINT('',(120.972209393875,-1.05,50.0283409674392));
#201601=CARTESIAN_POINT('',(121.405779922555,-1.05,50.4182340254182));
#201602=CARTESIAN_POINT('',(121.463022896425,-1.05,50.1237459238885));
#201603=CARTESIAN_POINT('Origin',(120.972209393875,-1.05,50.0283409674392));
#201604=CARTESIAN_POINT('',(120.914966420006,-1.05,50.3228290689689));
#201605=CARTESIAN_POINT('',(120.972209393875,-1.05,50.0283409674392));
#201606=CARTESIAN_POINT('Origin',(120.972209393875,0.250000000000015,50.0283409674392));
#201607=CARTESIAN_POINT('',(121.463022896425,0.250000000000015,50.1237459238885));
#201608=CARTESIAN_POINT('',(121.405779922555,0.250000000000015,50.4182340254182));
#201609=CARTESIAN_POINT('',(121.463022896425,0.250000000000015,50.1237459238885));
#201610=CARTESIAN_POINT('',(120.914966420006,0.250000000000015,50.3228290689689));
#201611=CARTESIAN_POINT('',(120.914966420006,0.250000000000015,50.3228290689689));
#201612=CARTESIAN_POINT('',(120.972209393875,0.250000000000015,50.0283409674392));
#201613=CARTESIAN_POINT('',(120.972209393875,0.250000000000015,50.0283409674392));
#201614=CARTESIAN_POINT('',(120.972209393875,0.250000000000015,50.0283409674392));
#201615=CARTESIAN_POINT('Origin',(121.463022896425,0.250000000000015,50.1237459238885));
#201616=CARTESIAN_POINT('',(121.463022896425,-0.249999999999985,50.1237459238885));
#201617=CARTESIAN_POINT('',(121.405779922555,-0.249999999999985,50.4182340254182));
#201618=CARTESIAN_POINT('',(121.463022896425,-0.249999999999985,50.1237459238885));
#201619=CARTESIAN_POINT('',(121.405779922555,0.250000000000015,50.4182340254182));
#201620=CARTESIAN_POINT('',(121.463022896425,0.250000000000015,50.1237459238885));
#201621=CARTESIAN_POINT('Origin',(121.463022896425,-0.249999999999985,50.1237459238885));
#201622=CARTESIAN_POINT('',(120.972209393875,-0.249999999999985,50.0283409674392));
#201623=CARTESIAN_POINT('',(120.914966420006,-0.249999999999985,50.3228290689689));
#201624=CARTESIAN_POINT('',(120.972209393875,-0.249999999999985,50.0283409674392));
#201625=CARTESIAN_POINT('',(121.405779922555,-0.249999999999985,50.4182340254182));
#201626=CARTESIAN_POINT('',(121.463022896425,-0.249999999999985,50.1237459238885));
#201627=CARTESIAN_POINT('Origin',(120.972209393875,-0.249999999999985,50.0283409674392));
#201628=CARTESIAN_POINT('',(120.914966420006,-0.249999999999985,50.3228290689689));
#201629=CARTESIAN_POINT('',(120.972209393875,-0.249999999999985,50.0283409674392));
#201630=CARTESIAN_POINT('Origin',(120.972209393875,1.05,50.0283409674392));
#201631=CARTESIAN_POINT('',(121.463022896425,1.05,50.1237459238885));
#201632=CARTESIAN_POINT('',(121.405779922555,1.05,50.4182340254182));
#201633=CARTESIAN_POINT('',(121.463022896425,1.05,50.1237459238885));
#201634=CARTESIAN_POINT('',(120.914966420006,1.05,50.3228290689689));
#201635=CARTESIAN_POINT('',(120.914966420006,1.05,50.3228290689689));
#201636=CARTESIAN_POINT('',(120.972209393875,1.05,50.0283409674392));
#201637=CARTESIAN_POINT('',(120.972209393875,1.05,50.0283409674392));
#201638=CARTESIAN_POINT('',(120.972209393875,1.05,50.0283409674392));
#201639=CARTESIAN_POINT('Origin',(121.463022896425,1.05,50.1237459238885));
#201640=CARTESIAN_POINT('',(121.463022896425,0.550000000000015,50.1237459238885));
#201641=CARTESIAN_POINT('',(121.405779922555,0.550000000000015,50.4182340254182));
#201642=CARTESIAN_POINT('',(121.463022896425,0.550000000000015,50.1237459238885));
#201643=CARTESIAN_POINT('',(121.405779922555,1.05,50.4182340254182));
#201644=CARTESIAN_POINT('',(121.463022896425,1.05,50.1237459238885));
#201645=CARTESIAN_POINT('Origin',(121.463022896425,0.550000000000015,50.1237459238885));
#201646=CARTESIAN_POINT('',(120.972209393875,0.550000000000015,50.0283409674392));
#201647=CARTESIAN_POINT('',(120.914966420006,0.550000000000015,50.3228290689689));
#201648=CARTESIAN_POINT('',(120.972209393875,0.550000000000015,50.0283409674392));
#201649=CARTESIAN_POINT('',(121.405779922555,0.550000000000015,50.4182340254182));
#201650=CARTESIAN_POINT('',(121.463022896425,0.550000000000015,50.1237459238885));
#201651=CARTESIAN_POINT('Origin',(120.972209393875,0.550000000000015,50.0283409674392));
#201652=CARTESIAN_POINT('',(120.914966420006,0.550000000000015,50.3228290689689));
#201653=CARTESIAN_POINT('',(120.972209393875,0.550000000000015,50.0283409674392));
#201654=CARTESIAN_POINT('Origin',(120.972209393875,1.85,50.0283409674392));
#201655=CARTESIAN_POINT('',(121.463022896425,1.85,50.1237459238885));
#201656=CARTESIAN_POINT('',(121.405779922555,1.85,50.4182340254182));
#201657=CARTESIAN_POINT('',(121.463022896425,1.85,50.1237459238885));
#201658=CARTESIAN_POINT('',(120.914966420006,1.85,50.3228290689689));
#201659=CARTESIAN_POINT('',(120.914966420006,1.85,50.3228290689689));
#201660=CARTESIAN_POINT('',(120.972209393875,1.85,50.0283409674392));
#201661=CARTESIAN_POINT('',(120.972209393875,1.85,50.0283409674392));
#201662=CARTESIAN_POINT('',(120.972209393875,1.85,50.0283409674392));
#201663=CARTESIAN_POINT('Origin',(121.463022896425,1.85,50.1237459238885));
#201664=CARTESIAN_POINT('',(121.463022896425,1.35,50.1237459238885));
#201665=CARTESIAN_POINT('',(121.405779922555,1.35,50.4182340254182));
#201666=CARTESIAN_POINT('',(121.463022896425,1.35,50.1237459238885));
#201667=CARTESIAN_POINT('',(121.405779922555,1.85,50.4182340254182));
#201668=CARTESIAN_POINT('',(121.463022896425,1.85,50.1237459238885));
#201669=CARTESIAN_POINT('Origin',(121.463022896425,1.35,50.1237459238885));
#201670=CARTESIAN_POINT('',(120.972209393875,1.35,50.0283409674392));
#201671=CARTESIAN_POINT('',(120.914966420006,1.35,50.3228290689689));
#201672=CARTESIAN_POINT('',(120.972209393875,1.35,50.0283409674392));
#201673=CARTESIAN_POINT('',(121.405779922555,1.35,50.4182340254182));
#201674=CARTESIAN_POINT('',(121.463022896425,1.35,50.1237459238885));
#201675=CARTESIAN_POINT('Origin',(120.972209393875,1.35,50.0283409674392));
#201676=CARTESIAN_POINT('',(120.914966420006,1.35,50.3228290689689));
#201677=CARTESIAN_POINT('',(120.972209393875,1.35,50.0283409674392));
#201678=CARTESIAN_POINT('Origin',(120.972209393875,2.65,50.0283409674392));
#201679=CARTESIAN_POINT('',(121.463022896425,2.65,50.1237459238885));
#201680=CARTESIAN_POINT('',(121.405779922555,2.65,50.4182340254182));
#201681=CARTESIAN_POINT('',(121.463022896425,2.65,50.1237459238885));
#201682=CARTESIAN_POINT('',(120.914966420006,2.65,50.3228290689689));
#201683=CARTESIAN_POINT('',(120.914966420006,2.65,50.3228290689689));
#201684=CARTESIAN_POINT('',(120.972209393875,2.65,50.0283409674392));
#201685=CARTESIAN_POINT('',(120.972209393875,2.65,50.0283409674392));
#201686=CARTESIAN_POINT('',(120.972209393875,2.65,50.0283409674392));
#201687=CARTESIAN_POINT('Origin',(121.463022896425,2.65,50.1237459238885));
#201688=CARTESIAN_POINT('',(121.463022896425,2.15,50.1237459238885));
#201689=CARTESIAN_POINT('',(121.405779922555,2.15,50.4182340254182));
#201690=CARTESIAN_POINT('',(121.463022896425,2.15,50.1237459238885));
#201691=CARTESIAN_POINT('',(121.405779922555,2.65,50.4182340254182));
#201692=CARTESIAN_POINT('',(121.463022896425,2.65,50.1237459238885));
#201693=CARTESIAN_POINT('Origin',(121.463022896425,2.15,50.1237459238885));
#201694=CARTESIAN_POINT('',(120.972209393875,2.15,50.0283409674392));
#201695=CARTESIAN_POINT('',(120.914966420006,2.15,50.3228290689689));
#201696=CARTESIAN_POINT('',(120.972209393875,2.15,50.0283409674392));
#201697=CARTESIAN_POINT('',(121.405779922555,2.15,50.4182340254182));
#201698=CARTESIAN_POINT('',(121.463022896425,2.15,50.1237459238885));
#201699=CARTESIAN_POINT('Origin',(120.972209393875,2.15,50.0283409674392));
#201700=CARTESIAN_POINT('',(120.914966420006,2.15,50.3228290689689));
#201701=CARTESIAN_POINT('',(120.972209393875,2.15,50.0283409674392));
#201702=CARTESIAN_POINT('Origin',(120.972209393875,3.45,50.0283409674392));
#201703=CARTESIAN_POINT('',(121.463022896425,3.45,50.1237459238885));
#201704=CARTESIAN_POINT('',(121.405779922555,3.45,50.4182340254182));
#201705=CARTESIAN_POINT('',(121.463022896425,3.45,50.1237459238885));
#201706=CARTESIAN_POINT('',(120.914966420006,3.45,50.3228290689689));
#201707=CARTESIAN_POINT('',(120.914966420006,3.45,50.3228290689689));
#201708=CARTESIAN_POINT('',(120.972209393875,3.45,50.0283409674392));
#201709=CARTESIAN_POINT('',(120.972209393875,3.45,50.0283409674392));
#201710=CARTESIAN_POINT('',(120.972209393875,3.45,50.0283409674392));
#201711=CARTESIAN_POINT('Origin',(121.463022896425,3.45,50.1237459238885));
#201712=CARTESIAN_POINT('',(121.463022896425,2.95,50.1237459238885));
#201713=CARTESIAN_POINT('',(121.405779922555,2.95,50.4182340254182));
#201714=CARTESIAN_POINT('',(121.463022896425,2.95,50.1237459238885));
#201715=CARTESIAN_POINT('',(121.405779922555,3.45,50.4182340254182));
#201716=CARTESIAN_POINT('',(121.463022896425,3.45,50.1237459238885));
#201717=CARTESIAN_POINT('Origin',(121.463022896425,2.95,50.1237459238885));
#201718=CARTESIAN_POINT('',(120.972209393875,2.95,50.0283409674392));
#201719=CARTESIAN_POINT('',(120.914966420006,2.95,50.3228290689689));
#201720=CARTESIAN_POINT('',(120.972209393875,2.95,50.0283409674392));
#201721=CARTESIAN_POINT('',(121.405779922555,2.95,50.4182340254182));
#201722=CARTESIAN_POINT('',(121.463022896425,2.95,50.1237459238885));
#201723=CARTESIAN_POINT('Origin',(120.972209393875,2.95,50.0283409674392));
#201724=CARTESIAN_POINT('',(120.914966420006,2.95,50.3228290689689));
#201725=CARTESIAN_POINT('',(120.972209393875,2.95,50.0283409674392));
#201726=CARTESIAN_POINT('Origin',(120.972209393875,4.25,50.0283409674392));
#201727=CARTESIAN_POINT('',(121.463022896425,4.25,50.1237459238885));
#201728=CARTESIAN_POINT('',(121.405779922555,4.25,50.4182340254182));
#201729=CARTESIAN_POINT('',(121.463022896425,4.25,50.1237459238885));
#201730=CARTESIAN_POINT('',(120.914966420006,4.25,50.3228290689689));
#201731=CARTESIAN_POINT('',(120.914966420006,4.25,50.3228290689689));
#201732=CARTESIAN_POINT('',(120.972209393875,4.25,50.0283409674392));
#201733=CARTESIAN_POINT('',(120.972209393875,4.25,50.0283409674392));
#201734=CARTESIAN_POINT('',(120.972209393875,4.25,50.0283409674392));
#201735=CARTESIAN_POINT('Origin',(121.463022896425,4.25,50.1237459238885));
#201736=CARTESIAN_POINT('',(121.463022896425,3.75,50.1237459238885));
#201737=CARTESIAN_POINT('',(121.405779922555,3.75,50.4182340254182));
#201738=CARTESIAN_POINT('',(121.463022896425,3.75,50.1237459238885));
#201739=CARTESIAN_POINT('',(121.405779922555,4.25,50.4182340254182));
#201740=CARTESIAN_POINT('',(121.463022896425,4.25,50.1237459238885));
#201741=CARTESIAN_POINT('Origin',(121.463022896425,3.75,50.1237459238885));
#201742=CARTESIAN_POINT('',(120.972209393875,3.75,50.0283409674392));
#201743=CARTESIAN_POINT('',(120.914966420006,3.75,50.3228290689689));
#201744=CARTESIAN_POINT('',(120.972209393875,3.75,50.0283409674392));
#201745=CARTESIAN_POINT('',(121.405779922555,3.75,50.4182340254182));
#201746=CARTESIAN_POINT('',(121.463022896425,3.75,50.1237459238885));
#201747=CARTESIAN_POINT('Origin',(120.972209393875,3.75,50.0283409674392));
#201748=CARTESIAN_POINT('',(120.914966420006,3.75,50.3228290689689));
#201749=CARTESIAN_POINT('',(120.972209393875,3.75,50.0283409674392));
#201750=CARTESIAN_POINT('Origin',(120.186907789796,4.25,49.8756930371204));
#201751=CARTESIAN_POINT('',(120.677721292346,4.25,49.9710979935697));
#201752=CARTESIAN_POINT('',(120.620478318476,4.25,50.2655860950994));
#201753=CARTESIAN_POINT('',(120.677721292346,4.25,49.9710979935697));
#201754=CARTESIAN_POINT('',(120.129664815927,4.25,50.1701811386501));
#201755=CARTESIAN_POINT('',(120.129664815927,4.25,50.1701811386501));
#201756=CARTESIAN_POINT('',(120.186907789796,4.25,49.8756930371204));
#201757=CARTESIAN_POINT('',(120.186907789796,4.25,49.8756930371204));
#201758=CARTESIAN_POINT('',(120.186907789796,4.25,49.8756930371204));
#201759=CARTESIAN_POINT('Origin',(120.677721292346,4.25,49.9710979935697));
#201760=CARTESIAN_POINT('',(120.677721292346,3.75,49.9710979935697));
#201761=CARTESIAN_POINT('',(120.620478318476,3.75,50.2655860950994));
#201762=CARTESIAN_POINT('',(120.677721292346,3.75,49.9710979935697));
#201763=CARTESIAN_POINT('',(120.620478318476,4.25,50.2655860950994));
#201764=CARTESIAN_POINT('',(120.677721292346,4.25,49.9710979935697));
#201765=CARTESIAN_POINT('Origin',(120.677721292346,3.75,49.9710979935697));
#201766=CARTESIAN_POINT('',(120.186907789796,3.75,49.8756930371204));
#201767=CARTESIAN_POINT('',(120.129664815927,3.75,50.1701811386501));
#201768=CARTESIAN_POINT('',(120.186907789796,3.75,49.8756930371204));
#201769=CARTESIAN_POINT('',(120.620478318476,3.75,50.2655860950994));
#201770=CARTESIAN_POINT('',(120.677721292346,3.75,49.9710979935697));
#201771=CARTESIAN_POINT('Origin',(120.186907789796,3.75,49.8756930371204));
#201772=CARTESIAN_POINT('',(120.129664815927,3.75,50.1701811386501));
#201773=CARTESIAN_POINT('',(120.186907789796,3.75,49.8756930371204));
#201774=CARTESIAN_POINT('Origin',(119.401606185717,4.25,49.7230451068016));
#201775=CARTESIAN_POINT('',(119.892419688267,4.25,49.8184500632509));
#201776=CARTESIAN_POINT('',(119.835176714397,4.25,50.1129381647806));
#201777=CARTESIAN_POINT('',(119.892419688267,4.25,49.8184500632509));
#201778=CARTESIAN_POINT('',(119.344363211847,4.25,50.0175332083313));
#201779=CARTESIAN_POINT('',(119.344363211847,4.25,50.0175332083313));
#201780=CARTESIAN_POINT('',(119.401606185717,4.25,49.7230451068016));
#201781=CARTESIAN_POINT('',(119.401606185717,4.25,49.7230451068016));
#201782=CARTESIAN_POINT('',(119.401606185717,4.25,49.7230451068016));
#201783=CARTESIAN_POINT('Origin',(119.892419688267,4.25,49.8184500632509));
#201784=CARTESIAN_POINT('',(119.892419688267,3.75,49.8184500632509));
#201785=CARTESIAN_POINT('',(119.835176714397,3.75,50.1129381647806));
#201786=CARTESIAN_POINT('',(119.892419688267,3.75,49.8184500632509));
#201787=CARTESIAN_POINT('',(119.835176714397,4.25,50.1129381647806));
#201788=CARTESIAN_POINT('',(119.892419688267,4.25,49.8184500632509));
#201789=CARTESIAN_POINT('Origin',(119.892419688267,3.75,49.8184500632509));
#201790=CARTESIAN_POINT('',(119.401606185717,3.75,49.7230451068016));
#201791=CARTESIAN_POINT('',(119.344363211847,3.75,50.0175332083313));
#201792=CARTESIAN_POINT('',(119.401606185717,3.75,49.7230451068016));
#201793=CARTESIAN_POINT('',(119.835176714397,3.75,50.1129381647806));
#201794=CARTESIAN_POINT('',(119.892419688267,3.75,49.8184500632509));
#201795=CARTESIAN_POINT('Origin',(119.401606185717,3.75,49.7230451068016));
#201796=CARTESIAN_POINT('',(119.344363211847,3.75,50.0175332083313));
#201797=CARTESIAN_POINT('',(119.401606185717,3.75,49.7230451068016));
#201798=CARTESIAN_POINT('Origin',(118.616304581638,4.25,49.5703971764828));
#201799=CARTESIAN_POINT('',(119.107118084187,4.25,49.6658021329321));
#201800=CARTESIAN_POINT('',(119.049875110318,4.25,49.9602902344618));
#201801=CARTESIAN_POINT('',(119.107118084187,4.25,49.6658021329321));
#201802=CARTESIAN_POINT('',(118.559061607768,4.25,49.8648852780125));
#201803=CARTESIAN_POINT('',(118.559061607768,4.25,49.8648852780125));
#201804=CARTESIAN_POINT('',(118.616304581638,4.25,49.5703971764828));
#201805=CARTESIAN_POINT('',(118.616304581638,4.25,49.5703971764828));
#201806=CARTESIAN_POINT('',(118.616304581638,4.25,49.5703971764828));
#201807=CARTESIAN_POINT('Origin',(119.107118084187,4.25,49.6658021329321));
#201808=CARTESIAN_POINT('',(119.107118084187,3.75,49.6658021329321));
#201809=CARTESIAN_POINT('',(119.049875110318,3.75,49.9602902344618));
#201810=CARTESIAN_POINT('',(119.107118084187,3.75,49.6658021329321));
#201811=CARTESIAN_POINT('',(119.049875110318,4.25,49.9602902344618));
#201812=CARTESIAN_POINT('',(119.107118084187,4.25,49.6658021329321));
#201813=CARTESIAN_POINT('Origin',(119.107118084187,3.75,49.6658021329321));
#201814=CARTESIAN_POINT('',(118.616304581638,3.75,49.5703971764828));
#201815=CARTESIAN_POINT('',(118.559061607768,3.75,49.8648852780125));
#201816=CARTESIAN_POINT('',(118.616304581638,3.75,49.5703971764828));
#201817=CARTESIAN_POINT('',(119.049875110318,3.75,49.9602902344618));
#201818=CARTESIAN_POINT('',(119.107118084187,3.75,49.6658021329321));
#201819=CARTESIAN_POINT('Origin',(118.616304581638,3.75,49.5703971764828));
#201820=CARTESIAN_POINT('',(118.559061607768,3.75,49.8648852780125));
#201821=CARTESIAN_POINT('',(118.616304581638,3.75,49.5703971764828));
#201822=CARTESIAN_POINT('Origin',(117.831002977559,4.25,49.417749246164));
#201823=CARTESIAN_POINT('',(118.321816480108,4.25,49.5131542026133));
#201824=CARTESIAN_POINT('',(118.264573506239,4.25,49.807642304143));
#201825=CARTESIAN_POINT('',(118.321816480108,4.25,49.5131542026133));
#201826=CARTESIAN_POINT('',(117.773760003689,4.25,49.7122373476937));
#201827=CARTESIAN_POINT('',(117.773760003689,4.25,49.7122373476937));
#201828=CARTESIAN_POINT('',(117.831002977559,4.25,49.417749246164));
#201829=CARTESIAN_POINT('',(117.831002977559,4.25,49.417749246164));
#201830=CARTESIAN_POINT('',(117.831002977559,4.25,49.417749246164));
#201831=CARTESIAN_POINT('Origin',(118.321816480108,4.25,49.5131542026133));
#201832=CARTESIAN_POINT('',(118.321816480108,3.75,49.5131542026133));
#201833=CARTESIAN_POINT('',(118.264573506239,3.75,49.807642304143));
#201834=CARTESIAN_POINT('',(118.321816480108,3.75,49.5131542026133));
#201835=CARTESIAN_POINT('',(118.264573506239,4.25,49.807642304143));
#201836=CARTESIAN_POINT('',(118.321816480108,4.25,49.5131542026133));
#201837=CARTESIAN_POINT('Origin',(118.321816480108,3.75,49.5131542026133));
#201838=CARTESIAN_POINT('',(117.831002977559,3.75,49.417749246164));
#201839=CARTESIAN_POINT('',(117.773760003689,3.75,49.7122373476937));
#201840=CARTESIAN_POINT('',(117.831002977559,3.75,49.417749246164));
#201841=CARTESIAN_POINT('',(118.264573506239,3.75,49.807642304143));
#201842=CARTESIAN_POINT('',(118.321816480108,3.75,49.5131542026133));
#201843=CARTESIAN_POINT('Origin',(117.831002977559,3.75,49.417749246164));
#201844=CARTESIAN_POINT('',(117.773760003689,3.75,49.7122373476937));
#201845=CARTESIAN_POINT('',(117.831002977559,3.75,49.417749246164));
#201846=CARTESIAN_POINT('Origin',(117.045701373479,4.25,49.2651013158452));
#201847=CARTESIAN_POINT('',(117.536514876029,4.25,49.3605062722945));
#201848=CARTESIAN_POINT('',(117.479271902159,4.25,49.6549943738242));
#201849=CARTESIAN_POINT('',(117.536514876029,4.25,49.3605062722945));
#201850=CARTESIAN_POINT('',(116.98845839961,4.25,49.5595894173749));
#201851=CARTESIAN_POINT('',(116.98845839961,4.25,49.5595894173749));
#201852=CARTESIAN_POINT('',(117.045701373479,4.25,49.2651013158452));
#201853=CARTESIAN_POINT('',(117.045701373479,4.25,49.2651013158452));
#201854=CARTESIAN_POINT('',(117.045701373479,4.25,49.2651013158452));
#201855=CARTESIAN_POINT('Origin',(117.536514876029,4.25,49.3605062722945));
#201856=CARTESIAN_POINT('',(117.536514876029,3.75,49.3605062722945));
#201857=CARTESIAN_POINT('',(117.479271902159,3.75,49.6549943738242));
#201858=CARTESIAN_POINT('',(117.536514876029,3.75,49.3605062722945));
#201859=CARTESIAN_POINT('',(117.479271902159,4.25,49.6549943738242));
#201860=CARTESIAN_POINT('',(117.536514876029,4.25,49.3605062722945));
#201861=CARTESIAN_POINT('Origin',(117.536514876029,3.75,49.3605062722945));
#201862=CARTESIAN_POINT('',(117.045701373479,3.75,49.2651013158452));
#201863=CARTESIAN_POINT('',(116.98845839961,3.75,49.5595894173749));
#201864=CARTESIAN_POINT('',(117.045701373479,3.75,49.2651013158452));
#201865=CARTESIAN_POINT('',(117.479271902159,3.75,49.6549943738242));
#201866=CARTESIAN_POINT('',(117.536514876029,3.75,49.3605062722945));
#201867=CARTESIAN_POINT('Origin',(117.045701373479,3.75,49.2651013158452));
#201868=CARTESIAN_POINT('',(116.98845839961,3.75,49.5595894173749));
#201869=CARTESIAN_POINT('',(117.045701373479,3.75,49.2651013158452));
#201870=CARTESIAN_POINT('Origin',(116.2603997694,4.25,49.1124533855264));
#201871=CARTESIAN_POINT('',(116.75121327195,4.25,49.2078583419757));
#201872=CARTESIAN_POINT('',(116.69397029808,4.25,49.5023464435054));
#201873=CARTESIAN_POINT('',(116.75121327195,4.25,49.2078583419757));
#201874=CARTESIAN_POINT('',(116.203156795531,4.25,49.4069414870561));
#201875=CARTESIAN_POINT('',(116.203156795531,4.25,49.4069414870561));
#201876=CARTESIAN_POINT('',(116.2603997694,4.25,49.1124533855264));
#201877=CARTESIAN_POINT('',(116.2603997694,4.25,49.1124533855264));
#201878=CARTESIAN_POINT('',(116.2603997694,4.25,49.1124533855264));
#201879=CARTESIAN_POINT('Origin',(116.75121327195,4.25,49.2078583419757));
#201880=CARTESIAN_POINT('',(116.75121327195,3.75,49.2078583419757));
#201881=CARTESIAN_POINT('',(116.69397029808,3.75,49.5023464435054));
#201882=CARTESIAN_POINT('',(116.75121327195,3.75,49.2078583419757));
#201883=CARTESIAN_POINT('',(116.69397029808,4.25,49.5023464435054));
#201884=CARTESIAN_POINT('',(116.75121327195,4.25,49.2078583419757));
#201885=CARTESIAN_POINT('Origin',(116.75121327195,3.75,49.2078583419757));
#201886=CARTESIAN_POINT('',(116.2603997694,3.75,49.1124533855264));
#201887=CARTESIAN_POINT('',(116.203156795531,3.75,49.4069414870561));
#201888=CARTESIAN_POINT('',(116.2603997694,3.75,49.1124533855264));
#201889=CARTESIAN_POINT('',(116.69397029808,3.75,49.5023464435054));
#201890=CARTESIAN_POINT('',(116.75121327195,3.75,49.2078583419757));
#201891=CARTESIAN_POINT('Origin',(116.2603997694,3.75,49.1124533855264));
#201892=CARTESIAN_POINT('',(116.203156795531,3.75,49.4069414870561));
#201893=CARTESIAN_POINT('',(116.2603997694,3.75,49.1124533855264));
#201894=CARTESIAN_POINT('Origin',(115.475098165321,4.25,48.9598054552076));
#201895=CARTESIAN_POINT('',(115.96591166787,4.25,49.0552104116569));
#201896=CARTESIAN_POINT('',(115.908668694001,4.25,49.3496985131866));
#201897=CARTESIAN_POINT('',(115.96591166787,4.25,49.0552104116569));
#201898=CARTESIAN_POINT('',(115.417855191451,4.25,49.2542935567373));
#201899=CARTESIAN_POINT('',(115.417855191451,4.25,49.2542935567373));
#201900=CARTESIAN_POINT('',(115.475098165321,4.25,48.9598054552076));
#201901=CARTESIAN_POINT('',(115.475098165321,4.25,48.9598054552076));
#201902=CARTESIAN_POINT('',(115.475098165321,4.25,48.9598054552076));
#201903=CARTESIAN_POINT('Origin',(115.96591166787,4.25,49.0552104116569));
#201904=CARTESIAN_POINT('',(115.96591166787,3.75,49.0552104116569));
#201905=CARTESIAN_POINT('',(115.908668694001,3.75,49.3496985131866));
#201906=CARTESIAN_POINT('',(115.96591166787,3.75,49.0552104116569));
#201907=CARTESIAN_POINT('',(115.908668694001,4.25,49.3496985131866));
#201908=CARTESIAN_POINT('',(115.96591166787,4.25,49.0552104116569));
#201909=CARTESIAN_POINT('Origin',(115.96591166787,3.75,49.0552104116569));
#201910=CARTESIAN_POINT('',(115.475098165321,3.75,48.9598054552076));
#201911=CARTESIAN_POINT('',(115.417855191451,3.75,49.2542935567373));
#201912=CARTESIAN_POINT('',(115.475098165321,3.75,48.9598054552076));
#201913=CARTESIAN_POINT('',(115.908668694001,3.75,49.3496985131866));
#201914=CARTESIAN_POINT('',(115.96591166787,3.75,49.0552104116569));
#201915=CARTESIAN_POINT('Origin',(115.475098165321,3.75,48.9598054552076));
#201916=CARTESIAN_POINT('',(115.417855191451,3.75,49.2542935567373));
#201917=CARTESIAN_POINT('',(115.475098165321,3.75,48.9598054552076));
#201918=CARTESIAN_POINT('Origin',(114.689796561242,4.25,48.8071575248888));
#201919=CARTESIAN_POINT('',(115.180610063791,4.25,48.9025624813381));
#201920=CARTESIAN_POINT('',(115.123367089922,4.25,49.1970505828678));
#201921=CARTESIAN_POINT('',(115.180610063791,4.25,48.9025624813381));
#201922=CARTESIAN_POINT('',(114.632553587372,4.25,49.1016456264185));
#201923=CARTESIAN_POINT('',(114.632553587372,4.25,49.1016456264185));
#201924=CARTESIAN_POINT('',(114.689796561242,4.25,48.8071575248888));
#201925=CARTESIAN_POINT('',(114.689796561242,4.25,48.8071575248888));
#201926=CARTESIAN_POINT('',(114.689796561242,4.25,48.8071575248888));
#201927=CARTESIAN_POINT('Origin',(115.180610063791,4.25,48.9025624813381));
#201928=CARTESIAN_POINT('',(115.180610063791,3.75,48.9025624813381));
#201929=CARTESIAN_POINT('',(115.123367089922,3.75,49.1970505828678));
#201930=CARTESIAN_POINT('',(115.180610063791,3.75,48.9025624813381));
#201931=CARTESIAN_POINT('',(115.123367089922,4.25,49.1970505828678));
#201932=CARTESIAN_POINT('',(115.180610063791,4.25,48.9025624813381));
#201933=CARTESIAN_POINT('Origin',(115.180610063791,3.75,48.9025624813381));
#201934=CARTESIAN_POINT('',(114.689796561242,3.75,48.8071575248888));
#201935=CARTESIAN_POINT('',(114.632553587372,3.75,49.1016456264185));
#201936=CARTESIAN_POINT('',(114.689796561242,3.75,48.8071575248888));
#201937=CARTESIAN_POINT('',(115.123367089922,3.75,49.1970505828678));
#201938=CARTESIAN_POINT('',(115.180610063791,3.75,48.9025624813381));
#201939=CARTESIAN_POINT('Origin',(114.689796561242,3.75,48.8071575248888));
#201940=CARTESIAN_POINT('',(114.632553587372,3.75,49.1016456264185));
#201941=CARTESIAN_POINT('',(114.689796561242,3.75,48.8071575248888));
#201942=CARTESIAN_POINT('Origin',(113.904494957163,4.25,48.65450959457));
#201943=CARTESIAN_POINT('',(114.395308459712,4.25,48.7499145510193));
#201944=CARTESIAN_POINT('',(114.338065485842,4.25,49.044402652549));
#201945=CARTESIAN_POINT('',(114.395308459712,4.25,48.7499145510193));
#201946=CARTESIAN_POINT('',(113.847251983293,4.25,48.9489976960997));
#201947=CARTESIAN_POINT('',(113.847251983293,4.25,48.9489976960997));
#201948=CARTESIAN_POINT('',(113.904494957163,4.25,48.65450959457));
#201949=CARTESIAN_POINT('',(113.904494957163,4.25,48.65450959457));
#201950=CARTESIAN_POINT('',(113.904494957163,4.25,48.65450959457));
#201951=CARTESIAN_POINT('Origin',(114.395308459712,4.25,48.7499145510193));
#201952=CARTESIAN_POINT('',(114.395308459712,3.75,48.7499145510193));
#201953=CARTESIAN_POINT('',(114.338065485842,3.75,49.044402652549));
#201954=CARTESIAN_POINT('',(114.395308459712,3.75,48.7499145510193));
#201955=CARTESIAN_POINT('',(114.338065485842,4.25,49.044402652549));
#201956=CARTESIAN_POINT('',(114.395308459712,4.25,48.7499145510193));
#201957=CARTESIAN_POINT('Origin',(114.395308459712,3.75,48.7499145510193));
#201958=CARTESIAN_POINT('',(113.904494957163,3.75,48.65450959457));
#201959=CARTESIAN_POINT('',(113.847251983293,3.75,48.9489976960997));
#201960=CARTESIAN_POINT('',(113.904494957163,3.75,48.65450959457));
#201961=CARTESIAN_POINT('',(114.338065485842,3.75,49.044402652549));
#201962=CARTESIAN_POINT('',(114.395308459712,3.75,48.7499145510193));
#201963=CARTESIAN_POINT('Origin',(113.904494957163,3.75,48.65450959457));
#201964=CARTESIAN_POINT('',(113.847251983293,3.75,48.9489976960997));
#201965=CARTESIAN_POINT('',(113.904494957163,3.75,48.65450959457));
#201966=CARTESIAN_POINT('Origin',(113.904494957163,3.45,48.65450959457));
#201967=CARTESIAN_POINT('',(114.395308459712,3.45,48.7499145510193));
#201968=CARTESIAN_POINT('',(114.338065485842,3.45,49.044402652549));
#201969=CARTESIAN_POINT('',(114.395308459712,3.45,48.7499145510193));
#201970=CARTESIAN_POINT('',(113.847251983293,3.45,48.9489976960997));
#201971=CARTESIAN_POINT('',(113.847251983293,3.45,48.9489976960997));
#201972=CARTESIAN_POINT('',(113.904494957163,3.45,48.65450959457));
#201973=CARTESIAN_POINT('',(113.904494957163,3.45,48.65450959457));
#201974=CARTESIAN_POINT('',(113.904494957163,3.45,48.65450959457));
#201975=CARTESIAN_POINT('Origin',(114.395308459712,3.45,48.7499145510193));
#201976=CARTESIAN_POINT('',(114.395308459712,2.95,48.7499145510193));
#201977=CARTESIAN_POINT('',(114.338065485842,2.95,49.044402652549));
#201978=CARTESIAN_POINT('',(114.395308459712,2.95,48.7499145510193));
#201979=CARTESIAN_POINT('',(114.338065485842,3.45,49.044402652549));
#201980=CARTESIAN_POINT('',(114.395308459712,3.45,48.7499145510193));
#201981=CARTESIAN_POINT('Origin',(114.395308459712,2.95,48.7499145510193));
#201982=CARTESIAN_POINT('',(113.904494957163,2.95,48.65450959457));
#201983=CARTESIAN_POINT('',(113.847251983293,2.95,48.9489976960997));
#201984=CARTESIAN_POINT('',(113.904494957163,2.95,48.65450959457));
#201985=CARTESIAN_POINT('',(114.338065485842,2.95,49.044402652549));
#201986=CARTESIAN_POINT('',(114.395308459712,2.95,48.7499145510193));
#201987=CARTESIAN_POINT('Origin',(113.904494957163,2.95,48.65450959457));
#201988=CARTESIAN_POINT('',(113.847251983293,2.95,48.9489976960997));
#201989=CARTESIAN_POINT('',(113.904494957163,2.95,48.65450959457));
#201990=CARTESIAN_POINT('Origin',(113.904494957163,2.65,48.65450959457));
#201991=CARTESIAN_POINT('',(114.395308459712,2.65,48.7499145510193));
#201992=CARTESIAN_POINT('',(114.338065485842,2.65,49.044402652549));
#201993=CARTESIAN_POINT('',(114.395308459712,2.65,48.7499145510193));
#201994=CARTESIAN_POINT('',(113.847251983293,2.65,48.9489976960997));
#201995=CARTESIAN_POINT('',(113.847251983293,2.65,48.9489976960997));
#201996=CARTESIAN_POINT('',(113.904494957163,2.65,48.65450959457));
#201997=CARTESIAN_POINT('',(113.904494957163,2.65,48.65450959457));
#201998=CARTESIAN_POINT('',(113.904494957163,2.65,48.65450959457));
#201999=CARTESIAN_POINT('Origin',(114.395308459712,2.65,48.7499145510193));
#202000=CARTESIAN_POINT('',(114.395308459712,2.15,48.7499145510193));
#202001=CARTESIAN_POINT('',(114.338065485842,2.15,49.044402652549));
#202002=CARTESIAN_POINT('',(114.395308459712,2.15,48.7499145510193));
#202003=CARTESIAN_POINT('',(114.338065485842,2.65,49.044402652549));
#202004=CARTESIAN_POINT('',(114.395308459712,2.65,48.7499145510193));
#202005=CARTESIAN_POINT('Origin',(114.395308459712,2.15,48.7499145510193));
#202006=CARTESIAN_POINT('',(113.904494957163,2.15,48.65450959457));
#202007=CARTESIAN_POINT('',(113.847251983293,2.15,48.9489976960997));
#202008=CARTESIAN_POINT('',(113.904494957163,2.15,48.65450959457));
#202009=CARTESIAN_POINT('',(114.338065485842,2.15,49.044402652549));
#202010=CARTESIAN_POINT('',(114.395308459712,2.15,48.7499145510193));
#202011=CARTESIAN_POINT('Origin',(113.904494957163,2.15,48.65450959457));
#202012=CARTESIAN_POINT('',(113.847251983293,2.15,48.9489976960997));
#202013=CARTESIAN_POINT('',(113.904494957163,2.15,48.65450959457));
#202014=CARTESIAN_POINT('Origin',(113.904494957163,1.85,48.65450959457));
#202015=CARTESIAN_POINT('',(114.395308459712,1.85,48.7499145510193));
#202016=CARTESIAN_POINT('',(114.338065485842,1.85,49.044402652549));
#202017=CARTESIAN_POINT('',(114.395308459712,1.85,48.7499145510193));
#202018=CARTESIAN_POINT('',(113.847251983293,1.85,48.9489976960997));
#202019=CARTESIAN_POINT('',(113.847251983293,1.85,48.9489976960997));
#202020=CARTESIAN_POINT('',(113.904494957163,1.85,48.65450959457));
#202021=CARTESIAN_POINT('',(113.904494957163,1.85,48.65450959457));
#202022=CARTESIAN_POINT('',(113.904494957163,1.85,48.65450959457));
#202023=CARTESIAN_POINT('Origin',(114.395308459712,1.85,48.7499145510193));
#202024=CARTESIAN_POINT('',(114.395308459712,1.35,48.7499145510193));
#202025=CARTESIAN_POINT('',(114.338065485842,1.35,49.044402652549));
#202026=CARTESIAN_POINT('',(114.395308459712,1.35,48.7499145510193));
#202027=CARTESIAN_POINT('',(114.338065485842,1.85,49.044402652549));
#202028=CARTESIAN_POINT('',(114.395308459712,1.85,48.7499145510193));
#202029=CARTESIAN_POINT('Origin',(114.395308459712,1.35,48.7499145510193));
#202030=CARTESIAN_POINT('',(113.904494957163,1.35,48.65450959457));
#202031=CARTESIAN_POINT('',(113.847251983293,1.35,48.9489976960997));
#202032=CARTESIAN_POINT('',(113.904494957163,1.35,48.65450959457));
#202033=CARTESIAN_POINT('',(114.338065485842,1.35,49.044402652549));
#202034=CARTESIAN_POINT('',(114.395308459712,1.35,48.7499145510193));
#202035=CARTESIAN_POINT('Origin',(113.904494957163,1.35,48.65450959457));
#202036=CARTESIAN_POINT('',(113.847251983293,1.35,48.9489976960997));
#202037=CARTESIAN_POINT('',(113.904494957163,1.35,48.65450959457));
#202038=CARTESIAN_POINT('Origin',(113.904494957163,1.05,48.65450959457));
#202039=CARTESIAN_POINT('',(114.395308459712,1.05,48.7499145510193));
#202040=CARTESIAN_POINT('',(114.338065485842,1.05,49.044402652549));
#202041=CARTESIAN_POINT('',(114.395308459712,1.05,48.7499145510193));
#202042=CARTESIAN_POINT('',(113.847251983293,1.05,48.9489976960997));
#202043=CARTESIAN_POINT('',(113.847251983293,1.05,48.9489976960997));
#202044=CARTESIAN_POINT('',(113.904494957163,1.05,48.65450959457));
#202045=CARTESIAN_POINT('',(113.904494957163,1.05,48.65450959457));
#202046=CARTESIAN_POINT('',(113.904494957163,1.05,48.65450959457));
#202047=CARTESIAN_POINT('Origin',(114.395308459712,1.05,48.7499145510193));
#202048=CARTESIAN_POINT('',(114.395308459712,0.550000000000015,48.7499145510193));
#202049=CARTESIAN_POINT('',(114.338065485842,0.550000000000015,49.044402652549));
#202050=CARTESIAN_POINT('',(114.395308459712,0.550000000000015,48.7499145510193));
#202051=CARTESIAN_POINT('',(114.338065485842,1.05,49.044402652549));
#202052=CARTESIAN_POINT('',(114.395308459712,1.05,48.7499145510193));
#202053=CARTESIAN_POINT('Origin',(114.395308459712,0.550000000000015,48.7499145510193));
#202054=CARTESIAN_POINT('',(113.904494957163,0.550000000000015,48.65450959457));
#202055=CARTESIAN_POINT('',(113.847251983293,0.550000000000015,48.9489976960997));
#202056=CARTESIAN_POINT('',(113.904494957163,0.550000000000015,48.65450959457));
#202057=CARTESIAN_POINT('',(114.338065485842,0.550000000000015,49.044402652549));
#202058=CARTESIAN_POINT('',(114.395308459712,0.550000000000015,48.7499145510193));
#202059=CARTESIAN_POINT('Origin',(113.904494957163,0.550000000000015,48.65450959457));
#202060=CARTESIAN_POINT('',(113.847251983293,0.550000000000015,48.9489976960997));
#202061=CARTESIAN_POINT('',(113.904494957163,0.550000000000015,48.65450959457));
#202062=CARTESIAN_POINT('Origin',(113.904494957163,0.250000000000015,48.65450959457));
#202063=CARTESIAN_POINT('',(114.395308459712,0.250000000000015,48.7499145510193));
#202064=CARTESIAN_POINT('',(114.338065485842,0.250000000000015,49.044402652549));
#202065=CARTESIAN_POINT('',(114.395308459712,0.250000000000015,48.7499145510193));
#202066=CARTESIAN_POINT('',(113.847251983293,0.250000000000015,48.9489976960997));
#202067=CARTESIAN_POINT('',(113.847251983293,0.250000000000015,48.9489976960997));
#202068=CARTESIAN_POINT('',(113.904494957163,0.250000000000015,48.65450959457));
#202069=CARTESIAN_POINT('',(113.904494957163,0.250000000000015,48.65450959457));
#202070=CARTESIAN_POINT('',(113.904494957163,0.250000000000015,48.65450959457));
#202071=CARTESIAN_POINT('Origin',(114.395308459712,0.250000000000015,48.7499145510193));
#202072=CARTESIAN_POINT('',(114.395308459712,-0.249999999999985,48.7499145510193));
#202073=CARTESIAN_POINT('',(114.338065485842,-0.249999999999985,49.044402652549));
#202074=CARTESIAN_POINT('',(114.395308459712,-0.249999999999985,48.7499145510193));
#202075=CARTESIAN_POINT('',(114.338065485842,0.250000000000015,49.044402652549));
#202076=CARTESIAN_POINT('',(114.395308459712,0.250000000000015,48.7499145510193));
#202077=CARTESIAN_POINT('Origin',(114.395308459712,-0.249999999999985,48.7499145510193));
#202078=CARTESIAN_POINT('',(113.904494957163,-0.249999999999985,48.65450959457));
#202079=CARTESIAN_POINT('',(113.847251983293,-0.249999999999985,48.9489976960997));
#202080=CARTESIAN_POINT('',(113.904494957163,-0.249999999999985,48.65450959457));
#202081=CARTESIAN_POINT('',(114.338065485842,-0.249999999999985,49.044402652549));
#202082=CARTESIAN_POINT('',(114.395308459712,-0.249999999999985,48.7499145510193));
#202083=CARTESIAN_POINT('Origin',(113.904494957163,-0.249999999999985,48.65450959457));
#202084=CARTESIAN_POINT('',(113.847251983293,-0.249999999999985,48.9489976960997));
#202085=CARTESIAN_POINT('',(113.904494957163,-0.249999999999985,48.65450959457));
#202086=CARTESIAN_POINT('Origin',(113.904494957163,-0.549999999999986,48.65450959457));
#202087=CARTESIAN_POINT('',(114.395308459712,-0.549999999999986,48.7499145510193));
#202088=CARTESIAN_POINT('',(114.338065485842,-0.549999999999986,49.044402652549));
#202089=CARTESIAN_POINT('',(114.395308459712,-0.549999999999986,48.7499145510193));
#202090=CARTESIAN_POINT('',(113.847251983293,-0.549999999999986,48.9489976960997));
#202091=CARTESIAN_POINT('',(113.847251983293,-0.549999999999986,48.9489976960997));
#202092=CARTESIAN_POINT('',(113.904494957163,-0.549999999999986,48.65450959457));
#202093=CARTESIAN_POINT('',(113.904494957163,-0.549999999999986,48.65450959457));
#202094=CARTESIAN_POINT('',(113.904494957163,-0.549999999999986,48.65450959457));
#202095=CARTESIAN_POINT('Origin',(114.395308459712,-0.549999999999986,48.7499145510193));
#202096=CARTESIAN_POINT('',(114.395308459712,-1.05,48.7499145510193));
#202097=CARTESIAN_POINT('',(114.338065485842,-1.05,49.044402652549));
#202098=CARTESIAN_POINT('',(114.395308459712,-1.05,48.7499145510193));
#202099=CARTESIAN_POINT('',(114.338065485842,-0.549999999999986,49.044402652549));
#202100=CARTESIAN_POINT('',(114.395308459712,-0.549999999999986,48.7499145510193));
#202101=CARTESIAN_POINT('Origin',(114.395308459712,-1.05,48.7499145510193));
#202102=CARTESIAN_POINT('',(113.904494957163,-1.05,48.65450959457));
#202103=CARTESIAN_POINT('',(113.847251983293,-1.05,48.9489976960997));
#202104=CARTESIAN_POINT('',(113.904494957163,-1.05,48.65450959457));
#202105=CARTESIAN_POINT('',(114.338065485842,-1.05,49.044402652549));
#202106=CARTESIAN_POINT('',(114.395308459712,-1.05,48.7499145510193));
#202107=CARTESIAN_POINT('Origin',(113.904494957163,-1.05,48.65450959457));
#202108=CARTESIAN_POINT('',(113.847251983293,-1.05,48.9489976960997));
#202109=CARTESIAN_POINT('',(113.904494957163,-1.05,48.65450959457));
#202110=CARTESIAN_POINT('Origin',(113.904494957163,-1.35,48.65450959457));
#202111=CARTESIAN_POINT('',(114.395308459712,-1.35,48.7499145510193));
#202112=CARTESIAN_POINT('',(114.338065485842,-1.35,49.044402652549));
#202113=CARTESIAN_POINT('',(114.395308459712,-1.35,48.7499145510193));
#202114=CARTESIAN_POINT('',(113.847251983293,-1.35,48.9489976960997));
#202115=CARTESIAN_POINT('',(113.847251983293,-1.35,48.9489976960997));
#202116=CARTESIAN_POINT('',(113.904494957163,-1.35,48.65450959457));
#202117=CARTESIAN_POINT('',(113.904494957163,-1.35,48.65450959457));
#202118=CARTESIAN_POINT('',(113.904494957163,-1.35,48.65450959457));
#202119=CARTESIAN_POINT('Origin',(114.395308459712,-1.35,48.7499145510193));
#202120=CARTESIAN_POINT('',(114.395308459712,-1.85,48.7499145510193));
#202121=CARTESIAN_POINT('',(114.338065485842,-1.85,49.044402652549));
#202122=CARTESIAN_POINT('',(114.395308459712,-1.85,48.7499145510193));
#202123=CARTESIAN_POINT('',(114.338065485842,-1.35,49.044402652549));
#202124=CARTESIAN_POINT('',(114.395308459712,-1.35,48.7499145510193));
#202125=CARTESIAN_POINT('Origin',(114.395308459712,-1.85,48.7499145510193));
#202126=CARTESIAN_POINT('',(113.904494957163,-1.85,48.65450959457));
#202127=CARTESIAN_POINT('',(113.847251983293,-1.85,48.9489976960997));
#202128=CARTESIAN_POINT('',(113.904494957163,-1.85,48.65450959457));
#202129=CARTESIAN_POINT('',(114.338065485842,-1.85,49.044402652549));
#202130=CARTESIAN_POINT('',(114.395308459712,-1.85,48.7499145510193));
#202131=CARTESIAN_POINT('Origin',(113.904494957163,-1.85,48.65450959457));
#202132=CARTESIAN_POINT('',(113.847251983293,-1.85,48.9489976960997));
#202133=CARTESIAN_POINT('',(113.904494957163,-1.85,48.65450959457));
#202134=CARTESIAN_POINT('Origin',(113.904494957163,-2.15,48.65450959457));
#202135=CARTESIAN_POINT('',(114.395308459712,-2.15,48.7499145510193));
#202136=CARTESIAN_POINT('',(114.338065485842,-2.15,49.044402652549));
#202137=CARTESIAN_POINT('',(114.395308459712,-2.15,48.7499145510193));
#202138=CARTESIAN_POINT('',(113.847251983293,-2.15,48.9489976960997));
#202139=CARTESIAN_POINT('',(113.847251983293,-2.15,48.9489976960997));
#202140=CARTESIAN_POINT('',(113.904494957163,-2.15,48.65450959457));
#202141=CARTESIAN_POINT('',(113.904494957163,-2.15,48.65450959457));
#202142=CARTESIAN_POINT('',(113.904494957163,-2.15,48.65450959457));
#202143=CARTESIAN_POINT('Origin',(114.395308459712,-2.15,48.7499145510193));
#202144=CARTESIAN_POINT('',(114.395308459712,-2.65,48.7499145510193));
#202145=CARTESIAN_POINT('',(114.338065485842,-2.65,49.044402652549));
#202146=CARTESIAN_POINT('',(114.395308459712,-2.65,48.7499145510193));
#202147=CARTESIAN_POINT('',(114.338065485842,-2.15,49.044402652549));
#202148=CARTESIAN_POINT('',(114.395308459712,-2.15,48.7499145510193));
#202149=CARTESIAN_POINT('Origin',(114.395308459712,-2.65,48.7499145510193));
#202150=CARTESIAN_POINT('',(113.904494957163,-2.65,48.65450959457));
#202151=CARTESIAN_POINT('',(113.847251983293,-2.65,48.9489976960997));
#202152=CARTESIAN_POINT('',(113.904494957163,-2.65,48.65450959457));
#202153=CARTESIAN_POINT('',(114.338065485842,-2.65,49.044402652549));
#202154=CARTESIAN_POINT('',(114.395308459712,-2.65,48.7499145510193));
#202155=CARTESIAN_POINT('Origin',(113.904494957163,-2.65,48.65450959457));
#202156=CARTESIAN_POINT('',(113.847251983293,-2.65,48.9489976960997));
#202157=CARTESIAN_POINT('',(113.904494957163,-2.65,48.65450959457));
#202158=CARTESIAN_POINT('Origin',(113.904494957163,-2.95,48.65450959457));
#202159=CARTESIAN_POINT('',(114.395308459712,-2.95,48.7499145510193));
#202160=CARTESIAN_POINT('',(114.338065485842,-2.95,49.044402652549));
#202161=CARTESIAN_POINT('',(114.395308459712,-2.95,48.7499145510193));
#202162=CARTESIAN_POINT('',(113.847251983293,-2.95,48.9489976960997));
#202163=CARTESIAN_POINT('',(113.847251983293,-2.95,48.9489976960997));
#202164=CARTESIAN_POINT('',(113.904494957163,-2.95,48.65450959457));
#202165=CARTESIAN_POINT('',(113.904494957163,-2.95,48.65450959457));
#202166=CARTESIAN_POINT('',(113.904494957163,-2.95,48.65450959457));
#202167=CARTESIAN_POINT('Origin',(114.395308459712,-2.95,48.7499145510193));
#202168=CARTESIAN_POINT('',(114.395308459712,-3.45,48.7499145510193));
#202169=CARTESIAN_POINT('',(114.338065485842,-3.45,49.044402652549));
#202170=CARTESIAN_POINT('',(114.395308459712,-3.45,48.7499145510193));
#202171=CARTESIAN_POINT('',(114.338065485842,-2.95,49.044402652549));
#202172=CARTESIAN_POINT('',(114.395308459712,-2.95,48.7499145510193));
#202173=CARTESIAN_POINT('Origin',(114.395308459712,-3.45,48.7499145510193));
#202174=CARTESIAN_POINT('',(113.904494957163,-3.45,48.65450959457));
#202175=CARTESIAN_POINT('',(113.847251983293,-3.45,48.9489976960997));
#202176=CARTESIAN_POINT('',(113.904494957163,-3.45,48.65450959457));
#202177=CARTESIAN_POINT('',(114.338065485842,-3.45,49.044402652549));
#202178=CARTESIAN_POINT('',(114.395308459712,-3.45,48.7499145510193));
#202179=CARTESIAN_POINT('Origin',(113.904494957163,-3.45,48.65450959457));
#202180=CARTESIAN_POINT('',(113.847251983293,-3.45,48.9489976960997));
#202181=CARTESIAN_POINT('',(113.904494957163,-3.45,48.65450959457));
#202182=CARTESIAN_POINT('Origin',(114.689796561242,-2.95,48.8071575248888));
#202183=CARTESIAN_POINT('',(115.180610063791,-2.95,48.9025624813381));
#202184=CARTESIAN_POINT('',(115.123367089922,-2.95,49.1970505828678));
#202185=CARTESIAN_POINT('',(115.180610063791,-2.95,48.9025624813381));
#202186=CARTESIAN_POINT('',(114.632553587372,-2.95,49.1016456264185));
#202187=CARTESIAN_POINT('',(114.632553587372,-2.95,49.1016456264185));
#202188=CARTESIAN_POINT('',(114.689796561242,-2.95,48.8071575248888));
#202189=CARTESIAN_POINT('',(114.689796561242,-2.95,48.8071575248888));
#202190=CARTESIAN_POINT('',(114.689796561242,-2.95,48.8071575248888));
#202191=CARTESIAN_POINT('Origin',(115.180610063791,-2.95,48.9025624813381));
#202192=CARTESIAN_POINT('',(115.180610063791,-3.45,48.9025624813381));
#202193=CARTESIAN_POINT('',(115.123367089922,-3.45,49.1970505828678));
#202194=CARTESIAN_POINT('',(115.180610063791,-3.45,48.9025624813381));
#202195=CARTESIAN_POINT('',(115.123367089922,-2.95,49.1970505828678));
#202196=CARTESIAN_POINT('',(115.180610063791,-2.95,48.9025624813381));
#202197=CARTESIAN_POINT('Origin',(115.180610063791,-3.45,48.9025624813381));
#202198=CARTESIAN_POINT('',(114.689796561242,-3.45,48.8071575248888));
#202199=CARTESIAN_POINT('',(114.632553587372,-3.45,49.1016456264185));
#202200=CARTESIAN_POINT('',(114.689796561242,-3.45,48.8071575248888));
#202201=CARTESIAN_POINT('',(115.123367089922,-3.45,49.1970505828678));
#202202=CARTESIAN_POINT('',(115.180610063791,-3.45,48.9025624813381));
#202203=CARTESIAN_POINT('Origin',(114.689796561242,-3.45,48.8071575248888));
#202204=CARTESIAN_POINT('',(114.632553587372,-3.45,49.1016456264185));
#202205=CARTESIAN_POINT('',(114.689796561242,-3.45,48.8071575248888));
#202206=CARTESIAN_POINT('Origin',(115.475098165321,-2.95,48.9598054552076));
#202207=CARTESIAN_POINT('',(115.96591166787,-2.95,49.0552104116569));
#202208=CARTESIAN_POINT('',(115.908668694001,-2.95,49.3496985131866));
#202209=CARTESIAN_POINT('',(115.96591166787,-2.95,49.0552104116569));
#202210=CARTESIAN_POINT('',(115.417855191451,-2.95,49.2542935567373));
#202211=CARTESIAN_POINT('',(115.417855191451,-2.95,49.2542935567373));
#202212=CARTESIAN_POINT('',(115.475098165321,-2.95,48.9598054552076));
#202213=CARTESIAN_POINT('',(115.475098165321,-2.95,48.9598054552076));
#202214=CARTESIAN_POINT('',(115.475098165321,-2.95,48.9598054552076));
#202215=CARTESIAN_POINT('Origin',(115.96591166787,-2.95,49.0552104116569));
#202216=CARTESIAN_POINT('',(115.96591166787,-3.45,49.0552104116569));
#202217=CARTESIAN_POINT('',(115.908668694001,-3.45,49.3496985131866));
#202218=CARTESIAN_POINT('',(115.96591166787,-3.45,49.0552104116569));
#202219=CARTESIAN_POINT('',(115.908668694001,-2.95,49.3496985131866));
#202220=CARTESIAN_POINT('',(115.96591166787,-2.95,49.0552104116569));
#202221=CARTESIAN_POINT('Origin',(115.96591166787,-3.45,49.0552104116569));
#202222=CARTESIAN_POINT('',(115.475098165321,-3.45,48.9598054552076));
#202223=CARTESIAN_POINT('',(115.417855191451,-3.45,49.2542935567373));
#202224=CARTESIAN_POINT('',(115.475098165321,-3.45,48.9598054552076));
#202225=CARTESIAN_POINT('',(115.908668694001,-3.45,49.3496985131866));
#202226=CARTESIAN_POINT('',(115.96591166787,-3.45,49.0552104116569));
#202227=CARTESIAN_POINT('Origin',(115.475098165321,-3.45,48.9598054552076));
#202228=CARTESIAN_POINT('',(115.417855191451,-3.45,49.2542935567373));
#202229=CARTESIAN_POINT('',(115.475098165321,-3.45,48.9598054552076));
#202230=CARTESIAN_POINT('Origin',(116.2603997694,-2.95,49.1124533855264));
#202231=CARTESIAN_POINT('',(116.75121327195,-2.95,49.2078583419757));
#202232=CARTESIAN_POINT('',(116.69397029808,-2.95,49.5023464435054));
#202233=CARTESIAN_POINT('',(116.75121327195,-2.95,49.2078583419757));
#202234=CARTESIAN_POINT('',(116.203156795531,-2.95,49.4069414870561));
#202235=CARTESIAN_POINT('',(116.203156795531,-2.95,49.4069414870561));
#202236=CARTESIAN_POINT('',(116.2603997694,-2.95,49.1124533855264));
#202237=CARTESIAN_POINT('',(116.2603997694,-2.95,49.1124533855264));
#202238=CARTESIAN_POINT('',(116.2603997694,-2.95,49.1124533855264));
#202239=CARTESIAN_POINT('Origin',(116.75121327195,-2.95,49.2078583419757));
#202240=CARTESIAN_POINT('',(116.75121327195,-3.45,49.2078583419757));
#202241=CARTESIAN_POINT('',(116.69397029808,-3.45,49.5023464435054));
#202242=CARTESIAN_POINT('',(116.75121327195,-3.45,49.2078583419757));
#202243=CARTESIAN_POINT('',(116.69397029808,-2.95,49.5023464435054));
#202244=CARTESIAN_POINT('',(116.75121327195,-2.95,49.2078583419757));
#202245=CARTESIAN_POINT('Origin',(116.75121327195,-3.45,49.2078583419757));
#202246=CARTESIAN_POINT('',(116.2603997694,-3.45,49.1124533855264));
#202247=CARTESIAN_POINT('',(116.203156795531,-3.45,49.4069414870561));
#202248=CARTESIAN_POINT('',(116.2603997694,-3.45,49.1124533855264));
#202249=CARTESIAN_POINT('',(116.69397029808,-3.45,49.5023464435054));
#202250=CARTESIAN_POINT('',(116.75121327195,-3.45,49.2078583419757));
#202251=CARTESIAN_POINT('Origin',(116.2603997694,-3.45,49.1124533855264));
#202252=CARTESIAN_POINT('',(116.203156795531,-3.45,49.4069414870561));
#202253=CARTESIAN_POINT('',(116.2603997694,-3.45,49.1124533855264));
#202254=CARTESIAN_POINT('Origin',(117.045701373479,-2.95,49.2651013158452));
#202255=CARTESIAN_POINT('',(117.536514876029,-2.95,49.3605062722945));
#202256=CARTESIAN_POINT('',(117.479271902159,-2.95,49.6549943738242));
#202257=CARTESIAN_POINT('',(117.536514876029,-2.95,49.3605062722945));
#202258=CARTESIAN_POINT('',(116.98845839961,-2.95,49.5595894173749));
#202259=CARTESIAN_POINT('',(116.98845839961,-2.95,49.5595894173749));
#202260=CARTESIAN_POINT('',(117.045701373479,-2.95,49.2651013158452));
#202261=CARTESIAN_POINT('',(117.045701373479,-2.95,49.2651013158452));
#202262=CARTESIAN_POINT('',(117.045701373479,-2.95,49.2651013158452));
#202263=CARTESIAN_POINT('Origin',(117.536514876029,-2.95,49.3605062722945));
#202264=CARTESIAN_POINT('',(117.536514876029,-3.45,49.3605062722945));
#202265=CARTESIAN_POINT('',(117.479271902159,-3.45,49.6549943738242));
#202266=CARTESIAN_POINT('',(117.536514876029,-3.45,49.3605062722945));
#202267=CARTESIAN_POINT('',(117.479271902159,-2.95,49.6549943738242));
#202268=CARTESIAN_POINT('',(117.536514876029,-2.95,49.3605062722945));
#202269=CARTESIAN_POINT('Origin',(117.536514876029,-3.45,49.3605062722945));
#202270=CARTESIAN_POINT('',(117.045701373479,-3.45,49.2651013158452));
#202271=CARTESIAN_POINT('',(116.98845839961,-3.45,49.5595894173749));
#202272=CARTESIAN_POINT('',(117.045701373479,-3.45,49.2651013158452));
#202273=CARTESIAN_POINT('',(117.479271902159,-3.45,49.6549943738242));
#202274=CARTESIAN_POINT('',(117.536514876029,-3.45,49.3605062722945));
#202275=CARTESIAN_POINT('Origin',(117.045701373479,-3.45,49.2651013158452));
#202276=CARTESIAN_POINT('',(116.98845839961,-3.45,49.5595894173749));
#202277=CARTESIAN_POINT('',(117.045701373479,-3.45,49.2651013158452));
#202278=CARTESIAN_POINT('Origin',(117.831002977559,-2.95,49.417749246164));
#202279=CARTESIAN_POINT('',(118.321816480108,-2.95,49.5131542026133));
#202280=CARTESIAN_POINT('',(118.264573506239,-2.95,49.807642304143));
#202281=CARTESIAN_POINT('',(118.321816480108,-2.95,49.5131542026133));
#202282=CARTESIAN_POINT('',(117.773760003689,-2.95,49.7122373476937));
#202283=CARTESIAN_POINT('',(117.773760003689,-2.95,49.7122373476937));
#202284=CARTESIAN_POINT('',(117.831002977559,-2.95,49.417749246164));
#202285=CARTESIAN_POINT('',(117.831002977559,-2.95,49.417749246164));
#202286=CARTESIAN_POINT('',(117.831002977559,-2.95,49.417749246164));
#202287=CARTESIAN_POINT('Origin',(118.321816480108,-2.95,49.5131542026133));
#202288=CARTESIAN_POINT('',(118.321816480108,-3.45,49.5131542026133));
#202289=CARTESIAN_POINT('',(118.264573506239,-3.45,49.807642304143));
#202290=CARTESIAN_POINT('',(118.321816480108,-3.45,49.5131542026133));
#202291=CARTESIAN_POINT('',(118.264573506239,-2.95,49.807642304143));
#202292=CARTESIAN_POINT('',(118.321816480108,-2.95,49.5131542026133));
#202293=CARTESIAN_POINT('Origin',(118.321816480108,-3.45,49.5131542026133));
#202294=CARTESIAN_POINT('',(117.831002977559,-3.45,49.417749246164));
#202295=CARTESIAN_POINT('',(117.773760003689,-3.45,49.7122373476937));
#202296=CARTESIAN_POINT('',(117.831002977559,-3.45,49.417749246164));
#202297=CARTESIAN_POINT('',(118.264573506239,-3.45,49.807642304143));
#202298=CARTESIAN_POINT('',(118.321816480108,-3.45,49.5131542026133));
#202299=CARTESIAN_POINT('Origin',(117.831002977559,-3.45,49.417749246164));
#202300=CARTESIAN_POINT('',(117.773760003689,-3.45,49.7122373476937));
#202301=CARTESIAN_POINT('',(117.831002977559,-3.45,49.417749246164));
#202302=CARTESIAN_POINT('Origin',(118.616304581638,-2.95,49.5703971764828));
#202303=CARTESIAN_POINT('',(119.107118084187,-2.95,49.6658021329321));
#202304=CARTESIAN_POINT('',(119.049875110318,-2.95,49.9602902344618));
#202305=CARTESIAN_POINT('',(119.107118084187,-2.95,49.6658021329321));
#202306=CARTESIAN_POINT('',(118.559061607768,-2.95,49.8648852780125));
#202307=CARTESIAN_POINT('',(118.559061607768,-2.95,49.8648852780125));
#202308=CARTESIAN_POINT('',(118.616304581638,-2.95,49.5703971764828));
#202309=CARTESIAN_POINT('',(118.616304581638,-2.95,49.5703971764828));
#202310=CARTESIAN_POINT('',(118.616304581638,-2.95,49.5703971764828));
#202311=CARTESIAN_POINT('Origin',(119.107118084187,-2.95,49.6658021329321));
#202312=CARTESIAN_POINT('',(119.107118084187,-3.45,49.6658021329321));
#202313=CARTESIAN_POINT('',(119.049875110318,-3.45,49.9602902344618));
#202314=CARTESIAN_POINT('',(119.107118084187,-3.45,49.6658021329321));
#202315=CARTESIAN_POINT('',(119.049875110318,-2.95,49.9602902344618));
#202316=CARTESIAN_POINT('',(119.107118084187,-2.95,49.6658021329321));
#202317=CARTESIAN_POINT('Origin',(119.107118084187,-3.45,49.6658021329321));
#202318=CARTESIAN_POINT('',(118.616304581638,-3.45,49.5703971764828));
#202319=CARTESIAN_POINT('',(118.559061607768,-3.45,49.8648852780125));
#202320=CARTESIAN_POINT('',(118.616304581638,-3.45,49.5703971764828));
#202321=CARTESIAN_POINT('',(119.049875110318,-3.45,49.9602902344618));
#202322=CARTESIAN_POINT('',(119.107118084187,-3.45,49.6658021329321));
#202323=CARTESIAN_POINT('Origin',(118.616304581638,-3.45,49.5703971764828));
#202324=CARTESIAN_POINT('',(118.559061607768,-3.45,49.8648852780125));
#202325=CARTESIAN_POINT('',(118.616304581638,-3.45,49.5703971764828));
#202326=CARTESIAN_POINT('Origin',(119.401606185717,-2.95,49.7230451068016));
#202327=CARTESIAN_POINT('',(119.892419688267,-2.95,49.8184500632509));
#202328=CARTESIAN_POINT('',(119.835176714397,-2.95,50.1129381647806));
#202329=CARTESIAN_POINT('',(119.892419688267,-2.95,49.8184500632509));
#202330=CARTESIAN_POINT('',(119.344363211847,-2.95,50.0175332083313));
#202331=CARTESIAN_POINT('',(119.344363211847,-2.95,50.0175332083313));
#202332=CARTESIAN_POINT('',(119.401606185717,-2.95,49.7230451068016));
#202333=CARTESIAN_POINT('',(119.401606185717,-2.95,49.7230451068016));
#202334=CARTESIAN_POINT('',(119.401606185717,-2.95,49.7230451068016));
#202335=CARTESIAN_POINT('Origin',(119.892419688267,-2.95,49.8184500632509));
#202336=CARTESIAN_POINT('',(119.892419688267,-3.45,49.8184500632509));
#202337=CARTESIAN_POINT('',(119.835176714397,-3.45,50.1129381647806));
#202338=CARTESIAN_POINT('',(119.892419688267,-3.45,49.8184500632509));
#202339=CARTESIAN_POINT('',(119.835176714397,-2.95,50.1129381647806));
#202340=CARTESIAN_POINT('',(119.892419688267,-2.95,49.8184500632509));
#202341=CARTESIAN_POINT('Origin',(119.892419688267,-3.45,49.8184500632509));
#202342=CARTESIAN_POINT('',(119.401606185717,-3.45,49.7230451068016));
#202343=CARTESIAN_POINT('',(119.344363211847,-3.45,50.0175332083313));
#202344=CARTESIAN_POINT('',(119.401606185717,-3.45,49.7230451068016));
#202345=CARTESIAN_POINT('',(119.835176714397,-3.45,50.1129381647806));
#202346=CARTESIAN_POINT('',(119.892419688267,-3.45,49.8184500632509));
#202347=CARTESIAN_POINT('Origin',(119.401606185717,-3.45,49.7230451068016));
#202348=CARTESIAN_POINT('',(119.344363211847,-3.45,50.0175332083313));
#202349=CARTESIAN_POINT('',(119.401606185717,-3.45,49.7230451068016));
#202350=CARTESIAN_POINT('Origin',(120.186907789796,-2.95,49.8756930371204));
#202351=CARTESIAN_POINT('',(120.677721292346,-2.95,49.9710979935697));
#202352=CARTESIAN_POINT('',(120.620478318476,-2.95,50.2655860950994));
#202353=CARTESIAN_POINT('',(120.677721292346,-2.95,49.9710979935697));
#202354=CARTESIAN_POINT('',(120.129664815927,-2.95,50.1701811386501));
#202355=CARTESIAN_POINT('',(120.129664815927,-2.95,50.1701811386501));
#202356=CARTESIAN_POINT('',(120.186907789796,-2.95,49.8756930371204));
#202357=CARTESIAN_POINT('',(120.186907789796,-2.95,49.8756930371204));
#202358=CARTESIAN_POINT('',(120.186907789796,-2.95,49.8756930371204));
#202359=CARTESIAN_POINT('Origin',(120.677721292346,-2.95,49.9710979935697));
#202360=CARTESIAN_POINT('',(120.677721292346,-3.45,49.9710979935697));
#202361=CARTESIAN_POINT('',(120.620478318476,-3.45,50.2655860950994));
#202362=CARTESIAN_POINT('',(120.677721292346,-3.45,49.9710979935697));
#202363=CARTESIAN_POINT('',(120.620478318476,-2.95,50.2655860950994));
#202364=CARTESIAN_POINT('',(120.677721292346,-2.95,49.9710979935697));
#202365=CARTESIAN_POINT('Origin',(120.677721292346,-3.45,49.9710979935697));
#202366=CARTESIAN_POINT('',(120.186907789796,-3.45,49.8756930371204));
#202367=CARTESIAN_POINT('',(120.129664815927,-3.45,50.1701811386501));
#202368=CARTESIAN_POINT('',(120.186907789796,-3.45,49.8756930371204));
#202369=CARTESIAN_POINT('',(120.620478318476,-3.45,50.2655860950994));
#202370=CARTESIAN_POINT('',(120.677721292346,-3.45,49.9710979935697));
#202371=CARTESIAN_POINT('Origin',(120.186907789796,-3.45,49.8756930371204));
#202372=CARTESIAN_POINT('',(120.129664815927,-3.45,50.1701811386501));
#202373=CARTESIAN_POINT('',(120.186907789796,-3.45,49.8756930371204));
#202374=CARTESIAN_POINT('Origin',(120.186907789796,-2.15,49.8756930371204));
#202375=CARTESIAN_POINT('',(120.677721292346,-2.15,49.9710979935697));
#202376=CARTESIAN_POINT('',(120.620478318476,-2.15,50.2655860950994));
#202377=CARTESIAN_POINT('',(120.677721292346,-2.15,49.9710979935697));
#202378=CARTESIAN_POINT('',(120.129664815927,-2.15,50.1701811386501));
#202379=CARTESIAN_POINT('',(120.129664815927,-2.15,50.1701811386501));
#202380=CARTESIAN_POINT('',(120.186907789796,-2.15,49.8756930371204));
#202381=CARTESIAN_POINT('',(120.186907789796,-2.15,49.8756930371204));
#202382=CARTESIAN_POINT('',(120.186907789796,-2.15,49.8756930371204));
#202383=CARTESIAN_POINT('Origin',(120.677721292346,-2.15,49.9710979935697));
#202384=CARTESIAN_POINT('',(120.677721292346,-2.65,49.9710979935697));
#202385=CARTESIAN_POINT('',(120.620478318476,-2.65,50.2655860950994));
#202386=CARTESIAN_POINT('',(120.677721292346,-2.65,49.9710979935697));
#202387=CARTESIAN_POINT('',(120.620478318476,-2.15,50.2655860950994));
#202388=CARTESIAN_POINT('',(120.677721292346,-2.15,49.9710979935697));
#202389=CARTESIAN_POINT('Origin',(120.677721292346,-2.65,49.9710979935697));
#202390=CARTESIAN_POINT('',(120.186907789796,-2.65,49.8756930371204));
#202391=CARTESIAN_POINT('',(120.129664815927,-2.65,50.1701811386501));
#202392=CARTESIAN_POINT('',(120.186907789796,-2.65,49.8756930371204));
#202393=CARTESIAN_POINT('',(120.620478318476,-2.65,50.2655860950994));
#202394=CARTESIAN_POINT('',(120.677721292346,-2.65,49.9710979935697));
#202395=CARTESIAN_POINT('Origin',(120.186907789796,-2.65,49.8756930371204));
#202396=CARTESIAN_POINT('',(120.129664815927,-2.65,50.1701811386501));
#202397=CARTESIAN_POINT('',(120.186907789796,-2.65,49.8756930371204));
#202398=CARTESIAN_POINT('Origin',(120.186907789796,-1.35,49.8756930371204));
#202399=CARTESIAN_POINT('',(120.677721292346,-1.35,49.9710979935697));
#202400=CARTESIAN_POINT('',(120.620478318476,-1.35,50.2655860950994));
#202401=CARTESIAN_POINT('',(120.677721292346,-1.35,49.9710979935697));
#202402=CARTESIAN_POINT('',(120.129664815927,-1.35,50.1701811386501));
#202403=CARTESIAN_POINT('',(120.129664815927,-1.35,50.1701811386501));
#202404=CARTESIAN_POINT('',(120.186907789796,-1.35,49.8756930371204));
#202405=CARTESIAN_POINT('',(120.186907789796,-1.35,49.8756930371204));
#202406=CARTESIAN_POINT('',(120.186907789796,-1.35,49.8756930371204));
#202407=CARTESIAN_POINT('Origin',(120.677721292346,-1.35,49.9710979935697));
#202408=CARTESIAN_POINT('',(120.677721292346,-1.85,49.9710979935697));
#202409=CARTESIAN_POINT('',(120.620478318476,-1.85,50.2655860950994));
#202410=CARTESIAN_POINT('',(120.677721292346,-1.85,49.9710979935697));
#202411=CARTESIAN_POINT('',(120.620478318476,-1.35,50.2655860950994));
#202412=CARTESIAN_POINT('',(120.677721292346,-1.35,49.9710979935697));
#202413=CARTESIAN_POINT('Origin',(120.677721292346,-1.85,49.9710979935697));
#202414=CARTESIAN_POINT('',(120.186907789796,-1.85,49.8756930371204));
#202415=CARTESIAN_POINT('',(120.129664815927,-1.85,50.1701811386501));
#202416=CARTESIAN_POINT('',(120.186907789796,-1.85,49.8756930371204));
#202417=CARTESIAN_POINT('',(120.620478318476,-1.85,50.2655860950994));
#202418=CARTESIAN_POINT('',(120.677721292346,-1.85,49.9710979935697));
#202419=CARTESIAN_POINT('Origin',(120.186907789796,-1.85,49.8756930371204));
#202420=CARTESIAN_POINT('',(120.129664815927,-1.85,50.1701811386501));
#202421=CARTESIAN_POINT('',(120.186907789796,-1.85,49.8756930371204));
#202422=CARTESIAN_POINT('Origin',(120.186907789796,-0.549999999999986,49.8756930371204));
#202423=CARTESIAN_POINT('',(120.677721292346,-0.549999999999986,49.9710979935697));
#202424=CARTESIAN_POINT('',(120.620478318476,-0.549999999999986,50.2655860950994));
#202425=CARTESIAN_POINT('',(120.677721292346,-0.549999999999986,49.9710979935697));
#202426=CARTESIAN_POINT('',(120.129664815927,-0.549999999999986,50.1701811386501));
#202427=CARTESIAN_POINT('',(120.129664815927,-0.549999999999986,50.1701811386501));
#202428=CARTESIAN_POINT('',(120.186907789796,-0.549999999999986,49.8756930371204));
#202429=CARTESIAN_POINT('',(120.186907789796,-0.549999999999986,49.8756930371204));
#202430=CARTESIAN_POINT('',(120.186907789796,-0.549999999999986,49.8756930371204));
#202431=CARTESIAN_POINT('Origin',(120.677721292346,-0.549999999999986,49.9710979935697));
#202432=CARTESIAN_POINT('',(120.677721292346,-1.05,49.9710979935697));
#202433=CARTESIAN_POINT('',(120.620478318476,-1.05,50.2655860950994));
#202434=CARTESIAN_POINT('',(120.677721292346,-1.05,49.9710979935697));
#202435=CARTESIAN_POINT('',(120.620478318476,-0.549999999999986,50.2655860950994));
#202436=CARTESIAN_POINT('',(120.677721292346,-0.549999999999986,49.9710979935697));
#202437=CARTESIAN_POINT('Origin',(120.677721292346,-1.05,49.9710979935697));
#202438=CARTESIAN_POINT('',(120.186907789796,-1.05,49.8756930371204));
#202439=CARTESIAN_POINT('',(120.129664815927,-1.05,50.1701811386501));
#202440=CARTESIAN_POINT('',(120.186907789796,-1.05,49.8756930371204));
#202441=CARTESIAN_POINT('',(120.620478318476,-1.05,50.2655860950994));
#202442=CARTESIAN_POINT('',(120.677721292346,-1.05,49.9710979935697));
#202443=CARTESIAN_POINT('Origin',(120.186907789796,-1.05,49.8756930371204));
#202444=CARTESIAN_POINT('',(120.129664815927,-1.05,50.1701811386501));
#202445=CARTESIAN_POINT('',(120.186907789796,-1.05,49.8756930371204));
#202446=CARTESIAN_POINT('Origin',(120.186907789796,0.250000000000015,49.8756930371204));
#202447=CARTESIAN_POINT('',(120.677721292346,0.250000000000015,49.9710979935697));
#202448=CARTESIAN_POINT('',(120.620478318476,0.250000000000015,50.2655860950994));
#202449=CARTESIAN_POINT('',(120.677721292346,0.250000000000015,49.9710979935697));
#202450=CARTESIAN_POINT('',(120.129664815927,0.250000000000015,50.1701811386501));
#202451=CARTESIAN_POINT('',(120.129664815927,0.250000000000015,50.1701811386501));
#202452=CARTESIAN_POINT('',(120.186907789796,0.250000000000015,49.8756930371204));
#202453=CARTESIAN_POINT('',(120.186907789796,0.250000000000015,49.8756930371204));
#202454=CARTESIAN_POINT('',(120.186907789796,0.250000000000015,49.8756930371204));
#202455=CARTESIAN_POINT('Origin',(120.677721292346,0.250000000000015,49.9710979935697));
#202456=CARTESIAN_POINT('',(120.677721292346,-0.249999999999985,49.9710979935697));
#202457=CARTESIAN_POINT('',(120.620478318476,-0.249999999999985,50.2655860950994));
#202458=CARTESIAN_POINT('',(120.677721292346,-0.249999999999985,49.9710979935697));
#202459=CARTESIAN_POINT('',(120.620478318476,0.250000000000015,50.2655860950994));
#202460=CARTESIAN_POINT('',(120.677721292346,0.250000000000015,49.9710979935697));
#202461=CARTESIAN_POINT('Origin',(120.677721292346,-0.249999999999985,49.9710979935697));
#202462=CARTESIAN_POINT('',(120.186907789796,-0.249999999999985,49.8756930371204));
#202463=CARTESIAN_POINT('',(120.129664815927,-0.249999999999985,50.1701811386501));
#202464=CARTESIAN_POINT('',(120.186907789796,-0.249999999999985,49.8756930371204));
#202465=CARTESIAN_POINT('',(120.620478318476,-0.249999999999985,50.2655860950994));
#202466=CARTESIAN_POINT('',(120.677721292346,-0.249999999999985,49.9710979935697));
#202467=CARTESIAN_POINT('Origin',(120.186907789796,-0.249999999999985,49.8756930371204));
#202468=CARTESIAN_POINT('',(120.129664815927,-0.249999999999985,50.1701811386501));
#202469=CARTESIAN_POINT('',(120.186907789796,-0.249999999999985,49.8756930371204));
#202470=CARTESIAN_POINT('Origin',(120.186907789796,1.05,49.8756930371204));
#202471=CARTESIAN_POINT('',(120.677721292346,1.05,49.9710979935697));
#202472=CARTESIAN_POINT('',(120.620478318476,1.05,50.2655860950994));
#202473=CARTESIAN_POINT('',(120.677721292346,1.05,49.9710979935697));
#202474=CARTESIAN_POINT('',(120.129664815927,1.05,50.1701811386501));
#202475=CARTESIAN_POINT('',(120.129664815927,1.05,50.1701811386501));
#202476=CARTESIAN_POINT('',(120.186907789796,1.05,49.8756930371204));
#202477=CARTESIAN_POINT('',(120.186907789796,1.05,49.8756930371204));
#202478=CARTESIAN_POINT('',(120.186907789796,1.05,49.8756930371204));
#202479=CARTESIAN_POINT('Origin',(120.677721292346,1.05,49.9710979935697));
#202480=CARTESIAN_POINT('',(120.677721292346,0.550000000000015,49.9710979935697));
#202481=CARTESIAN_POINT('',(120.620478318476,0.550000000000015,50.2655860950994));
#202482=CARTESIAN_POINT('',(120.677721292346,0.550000000000015,49.9710979935697));
#202483=CARTESIAN_POINT('',(120.620478318476,1.05,50.2655860950994));
#202484=CARTESIAN_POINT('',(120.677721292346,1.05,49.9710979935697));
#202485=CARTESIAN_POINT('Origin',(120.677721292346,0.550000000000015,49.9710979935697));
#202486=CARTESIAN_POINT('',(120.186907789796,0.550000000000015,49.8756930371204));
#202487=CARTESIAN_POINT('',(120.129664815927,0.550000000000015,50.1701811386501));
#202488=CARTESIAN_POINT('',(120.186907789796,0.550000000000015,49.8756930371204));
#202489=CARTESIAN_POINT('',(120.620478318476,0.550000000000015,50.2655860950994));
#202490=CARTESIAN_POINT('',(120.677721292346,0.550000000000015,49.9710979935697));
#202491=CARTESIAN_POINT('Origin',(120.186907789796,0.550000000000015,49.8756930371204));
#202492=CARTESIAN_POINT('',(120.129664815927,0.550000000000015,50.1701811386501));
#202493=CARTESIAN_POINT('',(120.186907789796,0.550000000000015,49.8756930371204));
#202494=CARTESIAN_POINT('Origin',(120.186907789796,1.85,49.8756930371204));
#202495=CARTESIAN_POINT('',(120.677721292346,1.85,49.9710979935697));
#202496=CARTESIAN_POINT('',(120.620478318476,1.85,50.2655860950994));
#202497=CARTESIAN_POINT('',(120.677721292346,1.85,49.9710979935697));
#202498=CARTESIAN_POINT('',(120.129664815927,1.85,50.1701811386501));
#202499=CARTESIAN_POINT('',(120.129664815927,1.85,50.1701811386501));
#202500=CARTESIAN_POINT('',(120.186907789796,1.85,49.8756930371204));
#202501=CARTESIAN_POINT('',(120.186907789796,1.85,49.8756930371204));
#202502=CARTESIAN_POINT('',(120.186907789796,1.85,49.8756930371204));
#202503=CARTESIAN_POINT('Origin',(120.677721292346,1.85,49.9710979935697));
#202504=CARTESIAN_POINT('',(120.677721292346,1.35,49.9710979935697));
#202505=CARTESIAN_POINT('',(120.620478318476,1.35,50.2655860950994));
#202506=CARTESIAN_POINT('',(120.677721292346,1.35,49.9710979935697));
#202507=CARTESIAN_POINT('',(120.620478318476,1.85,50.2655860950994));
#202508=CARTESIAN_POINT('',(120.677721292346,1.85,49.9710979935697));
#202509=CARTESIAN_POINT('Origin',(120.677721292346,1.35,49.9710979935697));
#202510=CARTESIAN_POINT('',(120.186907789796,1.35,49.8756930371204));
#202511=CARTESIAN_POINT('',(120.129664815927,1.35,50.1701811386501));
#202512=CARTESIAN_POINT('',(120.186907789796,1.35,49.8756930371204));
#202513=CARTESIAN_POINT('',(120.620478318476,1.35,50.2655860950994));
#202514=CARTESIAN_POINT('',(120.677721292346,1.35,49.9710979935697));
#202515=CARTESIAN_POINT('Origin',(120.186907789796,1.35,49.8756930371204));
#202516=CARTESIAN_POINT('',(120.129664815927,1.35,50.1701811386501));
#202517=CARTESIAN_POINT('',(120.186907789796,1.35,49.8756930371204));
#202518=CARTESIAN_POINT('Origin',(120.186907789796,2.65,49.8756930371204));
#202519=CARTESIAN_POINT('',(120.677721292346,2.65,49.9710979935697));
#202520=CARTESIAN_POINT('',(120.620478318476,2.65,50.2655860950994));
#202521=CARTESIAN_POINT('',(120.677721292346,2.65,49.9710979935697));
#202522=CARTESIAN_POINT('',(120.129664815927,2.65,50.1701811386501));
#202523=CARTESIAN_POINT('',(120.129664815927,2.65,50.1701811386501));
#202524=CARTESIAN_POINT('',(120.186907789796,2.65,49.8756930371204));
#202525=CARTESIAN_POINT('',(120.186907789796,2.65,49.8756930371204));
#202526=CARTESIAN_POINT('',(120.186907789796,2.65,49.8756930371204));
#202527=CARTESIAN_POINT('Origin',(120.677721292346,2.65,49.9710979935697));
#202528=CARTESIAN_POINT('',(120.677721292346,2.15,49.9710979935697));
#202529=CARTESIAN_POINT('',(120.620478318476,2.15,50.2655860950994));
#202530=CARTESIAN_POINT('',(120.677721292346,2.15,49.9710979935697));
#202531=CARTESIAN_POINT('',(120.620478318476,2.65,50.2655860950994));
#202532=CARTESIAN_POINT('',(120.677721292346,2.65,49.9710979935697));
#202533=CARTESIAN_POINT('Origin',(120.677721292346,2.15,49.9710979935697));
#202534=CARTESIAN_POINT('',(120.186907789796,2.15,49.8756930371204));
#202535=CARTESIAN_POINT('',(120.129664815927,2.15,50.1701811386501));
#202536=CARTESIAN_POINT('',(120.186907789796,2.15,49.8756930371204));
#202537=CARTESIAN_POINT('',(120.620478318476,2.15,50.2655860950994));
#202538=CARTESIAN_POINT('',(120.677721292346,2.15,49.9710979935697));
#202539=CARTESIAN_POINT('Origin',(120.186907789796,2.15,49.8756930371204));
#202540=CARTESIAN_POINT('',(120.129664815927,2.15,50.1701811386501));
#202541=CARTESIAN_POINT('',(120.186907789796,2.15,49.8756930371204));
#202542=CARTESIAN_POINT('Origin',(120.186907789796,3.45,49.8756930371204));
#202543=CARTESIAN_POINT('',(120.677721292346,3.45,49.9710979935697));
#202544=CARTESIAN_POINT('',(120.620478318476,3.45,50.2655860950994));
#202545=CARTESIAN_POINT('',(120.677721292346,3.45,49.9710979935697));
#202546=CARTESIAN_POINT('',(120.129664815927,3.45,50.1701811386501));
#202547=CARTESIAN_POINT('',(120.129664815927,3.45,50.1701811386501));
#202548=CARTESIAN_POINT('',(120.186907789796,3.45,49.8756930371204));
#202549=CARTESIAN_POINT('',(120.186907789796,3.45,49.8756930371204));
#202550=CARTESIAN_POINT('',(120.186907789796,3.45,49.8756930371204));
#202551=CARTESIAN_POINT('Origin',(120.677721292346,3.45,49.9710979935697));
#202552=CARTESIAN_POINT('',(120.677721292346,2.95,49.9710979935697));
#202553=CARTESIAN_POINT('',(120.620478318476,2.95,50.2655860950994));
#202554=CARTESIAN_POINT('',(120.677721292346,2.95,49.9710979935697));
#202555=CARTESIAN_POINT('',(120.620478318476,3.45,50.2655860950994));
#202556=CARTESIAN_POINT('',(120.677721292346,3.45,49.9710979935697));
#202557=CARTESIAN_POINT('Origin',(120.677721292346,2.95,49.9710979935697));
#202558=CARTESIAN_POINT('',(120.186907789796,2.95,49.8756930371204));
#202559=CARTESIAN_POINT('',(120.129664815927,2.95,50.1701811386501));
#202560=CARTESIAN_POINT('',(120.186907789796,2.95,49.8756930371204));
#202561=CARTESIAN_POINT('',(120.620478318476,2.95,50.2655860950994));
#202562=CARTESIAN_POINT('',(120.677721292346,2.95,49.9710979935697));
#202563=CARTESIAN_POINT('Origin',(120.186907789796,2.95,49.8756930371204));
#202564=CARTESIAN_POINT('',(120.129664815927,2.95,50.1701811386501));
#202565=CARTESIAN_POINT('',(120.186907789796,2.95,49.8756930371204));
#202566=CARTESIAN_POINT('Origin',(119.401606185717,3.45,49.7230451068016));
#202567=CARTESIAN_POINT('',(119.892419688267,3.45,49.8184500632509));
#202568=CARTESIAN_POINT('',(119.835176714397,3.45,50.1129381647806));
#202569=CARTESIAN_POINT('',(119.892419688267,3.45,49.8184500632509));
#202570=CARTESIAN_POINT('',(119.344363211847,3.45,50.0175332083313));
#202571=CARTESIAN_POINT('',(119.344363211847,3.45,50.0175332083313));
#202572=CARTESIAN_POINT('',(119.401606185717,3.45,49.7230451068016));
#202573=CARTESIAN_POINT('',(119.401606185717,3.45,49.7230451068016));
#202574=CARTESIAN_POINT('',(119.401606185717,3.45,49.7230451068016));
#202575=CARTESIAN_POINT('Origin',(119.892419688267,3.45,49.8184500632509));
#202576=CARTESIAN_POINT('',(119.892419688267,2.95,49.8184500632509));
#202577=CARTESIAN_POINT('',(119.835176714397,2.95,50.1129381647806));
#202578=CARTESIAN_POINT('',(119.892419688267,2.95,49.8184500632509));
#202579=CARTESIAN_POINT('',(119.835176714397,3.45,50.1129381647806));
#202580=CARTESIAN_POINT('',(119.892419688267,3.45,49.8184500632509));
#202581=CARTESIAN_POINT('Origin',(119.892419688267,2.95,49.8184500632509));
#202582=CARTESIAN_POINT('',(119.401606185717,2.95,49.7230451068016));
#202583=CARTESIAN_POINT('',(119.344363211847,2.95,50.0175332083313));
#202584=CARTESIAN_POINT('',(119.401606185717,2.95,49.7230451068016));
#202585=CARTESIAN_POINT('',(119.835176714397,2.95,50.1129381647806));
#202586=CARTESIAN_POINT('',(119.892419688267,2.95,49.8184500632509));
#202587=CARTESIAN_POINT('Origin',(119.401606185717,2.95,49.7230451068016));
#202588=CARTESIAN_POINT('',(119.344363211847,2.95,50.0175332083313));
#202589=CARTESIAN_POINT('',(119.401606185717,2.95,49.7230451068016));
#202590=CARTESIAN_POINT('Origin',(118.616304581638,3.45,49.5703971764828));
#202591=CARTESIAN_POINT('',(119.107118084187,3.45,49.6658021329321));
#202592=CARTESIAN_POINT('',(119.049875110318,3.45,49.9602902344618));
#202593=CARTESIAN_POINT('',(119.107118084187,3.45,49.6658021329321));
#202594=CARTESIAN_POINT('',(118.559061607768,3.45,49.8648852780125));
#202595=CARTESIAN_POINT('',(118.559061607768,3.45,49.8648852780125));
#202596=CARTESIAN_POINT('',(118.616304581638,3.45,49.5703971764828));
#202597=CARTESIAN_POINT('',(118.616304581638,3.45,49.5703971764828));
#202598=CARTESIAN_POINT('',(118.616304581638,3.45,49.5703971764828));
#202599=CARTESIAN_POINT('Origin',(119.107118084187,3.45,49.6658021329321));
#202600=CARTESIAN_POINT('',(119.107118084187,2.95,49.6658021329321));
#202601=CARTESIAN_POINT('',(119.049875110318,2.95,49.9602902344618));
#202602=CARTESIAN_POINT('',(119.107118084187,2.95,49.6658021329321));
#202603=CARTESIAN_POINT('',(119.049875110318,3.45,49.9602902344618));
#202604=CARTESIAN_POINT('',(119.107118084187,3.45,49.6658021329321));
#202605=CARTESIAN_POINT('Origin',(119.107118084187,2.95,49.6658021329321));
#202606=CARTESIAN_POINT('',(118.616304581638,2.95,49.5703971764828));
#202607=CARTESIAN_POINT('',(118.559061607768,2.95,49.8648852780125));
#202608=CARTESIAN_POINT('',(118.616304581638,2.95,49.5703971764828));
#202609=CARTESIAN_POINT('',(119.049875110318,2.95,49.9602902344618));
#202610=CARTESIAN_POINT('',(119.107118084187,2.95,49.6658021329321));
#202611=CARTESIAN_POINT('Origin',(118.616304581638,2.95,49.5703971764828));
#202612=CARTESIAN_POINT('',(118.559061607768,2.95,49.8648852780125));
#202613=CARTESIAN_POINT('',(118.616304581638,2.95,49.5703971764828));
#202614=CARTESIAN_POINT('Origin',(117.831002977559,3.45,49.417749246164));
#202615=CARTESIAN_POINT('',(118.321816480108,3.45,49.5131542026133));
#202616=CARTESIAN_POINT('',(118.264573506239,3.45,49.807642304143));
#202617=CARTESIAN_POINT('',(118.321816480108,3.45,49.5131542026133));
#202618=CARTESIAN_POINT('',(117.773760003689,3.45,49.7122373476937));
#202619=CARTESIAN_POINT('',(117.773760003689,3.45,49.7122373476937));
#202620=CARTESIAN_POINT('',(117.831002977559,3.45,49.417749246164));
#202621=CARTESIAN_POINT('',(117.831002977559,3.45,49.417749246164));
#202622=CARTESIAN_POINT('',(117.831002977559,3.45,49.417749246164));
#202623=CARTESIAN_POINT('Origin',(118.321816480108,3.45,49.5131542026133));
#202624=CARTESIAN_POINT('',(118.321816480108,2.95,49.5131542026133));
#202625=CARTESIAN_POINT('',(118.264573506239,2.95,49.807642304143));
#202626=CARTESIAN_POINT('',(118.321816480108,2.95,49.5131542026133));
#202627=CARTESIAN_POINT('',(118.264573506239,3.45,49.807642304143));
#202628=CARTESIAN_POINT('',(118.321816480108,3.45,49.5131542026133));
#202629=CARTESIAN_POINT('Origin',(118.321816480108,2.95,49.5131542026133));
#202630=CARTESIAN_POINT('',(117.831002977559,2.95,49.417749246164));
#202631=CARTESIAN_POINT('',(117.773760003689,2.95,49.7122373476937));
#202632=CARTESIAN_POINT('',(117.831002977559,2.95,49.417749246164));
#202633=CARTESIAN_POINT('',(118.264573506239,2.95,49.807642304143));
#202634=CARTESIAN_POINT('',(118.321816480108,2.95,49.5131542026133));
#202635=CARTESIAN_POINT('Origin',(117.831002977559,2.95,49.417749246164));
#202636=CARTESIAN_POINT('',(117.773760003689,2.95,49.7122373476937));
#202637=CARTESIAN_POINT('',(117.831002977559,2.95,49.417749246164));
#202638=CARTESIAN_POINT('Origin',(117.045701373479,3.45,49.2651013158452));
#202639=CARTESIAN_POINT('',(117.536514876029,3.45,49.3605062722945));
#202640=CARTESIAN_POINT('',(117.479271902159,3.45,49.6549943738242));
#202641=CARTESIAN_POINT('',(117.536514876029,3.45,49.3605062722945));
#202642=CARTESIAN_POINT('',(116.98845839961,3.45,49.5595894173749));
#202643=CARTESIAN_POINT('',(116.98845839961,3.45,49.5595894173749));
#202644=CARTESIAN_POINT('',(117.045701373479,3.45,49.2651013158452));
#202645=CARTESIAN_POINT('',(117.045701373479,3.45,49.2651013158452));
#202646=CARTESIAN_POINT('',(117.045701373479,3.45,49.2651013158452));
#202647=CARTESIAN_POINT('Origin',(117.536514876029,3.45,49.3605062722945));
#202648=CARTESIAN_POINT('',(117.536514876029,2.95,49.3605062722945));
#202649=CARTESIAN_POINT('',(117.479271902159,2.95,49.6549943738242));
#202650=CARTESIAN_POINT('',(117.536514876029,2.95,49.3605062722945));
#202651=CARTESIAN_POINT('',(117.479271902159,3.45,49.6549943738242));
#202652=CARTESIAN_POINT('',(117.536514876029,3.45,49.3605062722945));
#202653=CARTESIAN_POINT('Origin',(117.536514876029,2.95,49.3605062722945));
#202654=CARTESIAN_POINT('',(117.045701373479,2.95,49.2651013158452));
#202655=CARTESIAN_POINT('',(116.98845839961,2.95,49.5595894173749));
#202656=CARTESIAN_POINT('',(117.045701373479,2.95,49.2651013158452));
#202657=CARTESIAN_POINT('',(117.479271902159,2.95,49.6549943738242));
#202658=CARTESIAN_POINT('',(117.536514876029,2.95,49.3605062722945));
#202659=CARTESIAN_POINT('Origin',(117.045701373479,2.95,49.2651013158452));
#202660=CARTESIAN_POINT('',(116.98845839961,2.95,49.5595894173749));
#202661=CARTESIAN_POINT('',(117.045701373479,2.95,49.2651013158452));
#202662=CARTESIAN_POINT('Origin',(116.2603997694,3.45,49.1124533855264));
#202663=CARTESIAN_POINT('',(116.75121327195,3.45,49.2078583419757));
#202664=CARTESIAN_POINT('',(116.69397029808,3.45,49.5023464435054));
#202665=CARTESIAN_POINT('',(116.75121327195,3.45,49.2078583419757));
#202666=CARTESIAN_POINT('',(116.203156795531,3.45,49.4069414870561));
#202667=CARTESIAN_POINT('',(116.203156795531,3.45,49.4069414870561));
#202668=CARTESIAN_POINT('',(116.2603997694,3.45,49.1124533855264));
#202669=CARTESIAN_POINT('',(116.2603997694,3.45,49.1124533855264));
#202670=CARTESIAN_POINT('',(116.2603997694,3.45,49.1124533855264));
#202671=CARTESIAN_POINT('Origin',(116.75121327195,3.45,49.2078583419757));
#202672=CARTESIAN_POINT('',(116.75121327195,2.95,49.2078583419757));
#202673=CARTESIAN_POINT('',(116.69397029808,2.95,49.5023464435054));
#202674=CARTESIAN_POINT('',(116.75121327195,2.95,49.2078583419757));
#202675=CARTESIAN_POINT('',(116.69397029808,3.45,49.5023464435054));
#202676=CARTESIAN_POINT('',(116.75121327195,3.45,49.2078583419757));
#202677=CARTESIAN_POINT('Origin',(116.75121327195,2.95,49.2078583419757));
#202678=CARTESIAN_POINT('',(116.2603997694,2.95,49.1124533855264));
#202679=CARTESIAN_POINT('',(116.203156795531,2.95,49.4069414870561));
#202680=CARTESIAN_POINT('',(116.2603997694,2.95,49.1124533855264));
#202681=CARTESIAN_POINT('',(116.69397029808,2.95,49.5023464435054));
#202682=CARTESIAN_POINT('',(116.75121327195,2.95,49.2078583419757));
#202683=CARTESIAN_POINT('Origin',(116.2603997694,2.95,49.1124533855264));
#202684=CARTESIAN_POINT('',(116.203156795531,2.95,49.4069414870561));
#202685=CARTESIAN_POINT('',(116.2603997694,2.95,49.1124533855264));
#202686=CARTESIAN_POINT('Origin',(115.475098165321,3.45,48.9598054552076));
#202687=CARTESIAN_POINT('',(115.96591166787,3.45,49.0552104116569));
#202688=CARTESIAN_POINT('',(115.908668694001,3.45,49.3496985131866));
#202689=CARTESIAN_POINT('',(115.96591166787,3.45,49.0552104116569));
#202690=CARTESIAN_POINT('',(115.417855191451,3.45,49.2542935567373));
#202691=CARTESIAN_POINT('',(115.417855191451,3.45,49.2542935567373));
#202692=CARTESIAN_POINT('',(115.475098165321,3.45,48.9598054552076));
#202693=CARTESIAN_POINT('',(115.475098165321,3.45,48.9598054552076));
#202694=CARTESIAN_POINT('',(115.475098165321,3.45,48.9598054552076));
#202695=CARTESIAN_POINT('Origin',(115.96591166787,3.45,49.0552104116569));
#202696=CARTESIAN_POINT('',(115.96591166787,2.95,49.0552104116569));
#202697=CARTESIAN_POINT('',(115.908668694001,2.95,49.3496985131866));
#202698=CARTESIAN_POINT('',(115.96591166787,2.95,49.0552104116569));
#202699=CARTESIAN_POINT('',(115.908668694001,3.45,49.3496985131866));
#202700=CARTESIAN_POINT('',(115.96591166787,3.45,49.0552104116569));
#202701=CARTESIAN_POINT('Origin',(115.96591166787,2.95,49.0552104116569));
#202702=CARTESIAN_POINT('',(115.475098165321,2.95,48.9598054552076));
#202703=CARTESIAN_POINT('',(115.417855191451,2.95,49.2542935567373));
#202704=CARTESIAN_POINT('',(115.475098165321,2.95,48.9598054552076));
#202705=CARTESIAN_POINT('',(115.908668694001,2.95,49.3496985131866));
#202706=CARTESIAN_POINT('',(115.96591166787,2.95,49.0552104116569));
#202707=CARTESIAN_POINT('Origin',(115.475098165321,2.95,48.9598054552076));
#202708=CARTESIAN_POINT('',(115.417855191451,2.95,49.2542935567373));
#202709=CARTESIAN_POINT('',(115.475098165321,2.95,48.9598054552076));
#202710=CARTESIAN_POINT('Origin',(114.689796561242,3.45,48.8071575248888));
#202711=CARTESIAN_POINT('',(115.180610063791,3.45,48.9025624813381));
#202712=CARTESIAN_POINT('',(115.123367089922,3.45,49.1970505828678));
#202713=CARTESIAN_POINT('',(115.180610063791,3.45,48.9025624813381));
#202714=CARTESIAN_POINT('',(114.632553587372,3.45,49.1016456264185));
#202715=CARTESIAN_POINT('',(114.632553587372,3.45,49.1016456264185));
#202716=CARTESIAN_POINT('',(114.689796561242,3.45,48.8071575248888));
#202717=CARTESIAN_POINT('',(114.689796561242,3.45,48.8071575248888));
#202718=CARTESIAN_POINT('',(114.689796561242,3.45,48.8071575248888));
#202719=CARTESIAN_POINT('Origin',(115.180610063791,3.45,48.9025624813381));
#202720=CARTESIAN_POINT('',(115.180610063791,2.95,48.9025624813381));
#202721=CARTESIAN_POINT('',(115.123367089922,2.95,49.1970505828678));
#202722=CARTESIAN_POINT('',(115.180610063791,2.95,48.9025624813381));
#202723=CARTESIAN_POINT('',(115.123367089922,3.45,49.1970505828678));
#202724=CARTESIAN_POINT('',(115.180610063791,3.45,48.9025624813381));
#202725=CARTESIAN_POINT('Origin',(115.180610063791,2.95,48.9025624813381));
#202726=CARTESIAN_POINT('',(114.689796561242,2.95,48.8071575248888));
#202727=CARTESIAN_POINT('',(114.632553587372,2.95,49.1016456264185));
#202728=CARTESIAN_POINT('',(114.689796561242,2.95,48.8071575248888));
#202729=CARTESIAN_POINT('',(115.123367089922,2.95,49.1970505828678));
#202730=CARTESIAN_POINT('',(115.180610063791,2.95,48.9025624813381));
#202731=CARTESIAN_POINT('Origin',(114.689796561242,2.95,48.8071575248888));
#202732=CARTESIAN_POINT('',(114.632553587372,2.95,49.1016456264185));
#202733=CARTESIAN_POINT('',(114.689796561242,2.95,48.8071575248888));
#202734=CARTESIAN_POINT('Origin',(114.689796561242,2.65,48.8071575248888));
#202735=CARTESIAN_POINT('',(115.180610063791,2.65,48.9025624813381));
#202736=CARTESIAN_POINT('',(115.123367089922,2.65,49.1970505828678));
#202737=CARTESIAN_POINT('',(115.180610063791,2.65,48.9025624813381));
#202738=CARTESIAN_POINT('',(114.632553587372,2.65,49.1016456264185));
#202739=CARTESIAN_POINT('',(114.632553587372,2.65,49.1016456264185));
#202740=CARTESIAN_POINT('',(114.689796561242,2.65,48.8071575248888));
#202741=CARTESIAN_POINT('',(114.689796561242,2.65,48.8071575248888));
#202742=CARTESIAN_POINT('',(114.689796561242,2.65,48.8071575248888));
#202743=CARTESIAN_POINT('Origin',(115.180610063791,2.65,48.9025624813381));
#202744=CARTESIAN_POINT('',(115.180610063791,2.15,48.9025624813381));
#202745=CARTESIAN_POINT('',(115.123367089922,2.15,49.1970505828678));
#202746=CARTESIAN_POINT('',(115.180610063791,2.15,48.9025624813381));
#202747=CARTESIAN_POINT('',(115.123367089922,2.65,49.1970505828678));
#202748=CARTESIAN_POINT('',(115.180610063791,2.65,48.9025624813381));
#202749=CARTESIAN_POINT('Origin',(115.180610063791,2.15,48.9025624813381));
#202750=CARTESIAN_POINT('',(114.689796561242,2.15,48.8071575248888));
#202751=CARTESIAN_POINT('',(114.632553587372,2.15,49.1016456264185));
#202752=CARTESIAN_POINT('',(114.689796561242,2.15,48.8071575248888));
#202753=CARTESIAN_POINT('',(115.123367089922,2.15,49.1970505828678));
#202754=CARTESIAN_POINT('',(115.180610063791,2.15,48.9025624813381));
#202755=CARTESIAN_POINT('Origin',(114.689796561242,2.15,48.8071575248888));
#202756=CARTESIAN_POINT('',(114.632553587372,2.15,49.1016456264185));
#202757=CARTESIAN_POINT('',(114.689796561242,2.15,48.8071575248888));
#202758=CARTESIAN_POINT('Origin',(114.689796561242,1.85,48.8071575248888));
#202759=CARTESIAN_POINT('',(115.180610063791,1.85,48.9025624813381));
#202760=CARTESIAN_POINT('',(115.123367089922,1.85,49.1970505828678));
#202761=CARTESIAN_POINT('',(115.180610063791,1.85,48.9025624813381));
#202762=CARTESIAN_POINT('',(114.632553587372,1.85,49.1016456264185));
#202763=CARTESIAN_POINT('',(114.632553587372,1.85,49.1016456264185));
#202764=CARTESIAN_POINT('',(114.689796561242,1.85,48.8071575248888));
#202765=CARTESIAN_POINT('',(114.689796561242,1.85,48.8071575248888));
#202766=CARTESIAN_POINT('',(114.689796561242,1.85,48.8071575248888));
#202767=CARTESIAN_POINT('Origin',(115.180610063791,1.85,48.9025624813381));
#202768=CARTESIAN_POINT('',(115.180610063791,1.35,48.9025624813381));
#202769=CARTESIAN_POINT('',(115.123367089922,1.35,49.1970505828678));
#202770=CARTESIAN_POINT('',(115.180610063791,1.35,48.9025624813381));
#202771=CARTESIAN_POINT('',(115.123367089922,1.85,49.1970505828678));
#202772=CARTESIAN_POINT('',(115.180610063791,1.85,48.9025624813381));
#202773=CARTESIAN_POINT('Origin',(115.180610063791,1.35,48.9025624813381));
#202774=CARTESIAN_POINT('',(114.689796561242,1.35,48.8071575248888));
#202775=CARTESIAN_POINT('',(114.632553587372,1.35,49.1016456264185));
#202776=CARTESIAN_POINT('',(114.689796561242,1.35,48.8071575248888));
#202777=CARTESIAN_POINT('',(115.123367089922,1.35,49.1970505828678));
#202778=CARTESIAN_POINT('',(115.180610063791,1.35,48.9025624813381));
#202779=CARTESIAN_POINT('Origin',(114.689796561242,1.35,48.8071575248888));
#202780=CARTESIAN_POINT('',(114.632553587372,1.35,49.1016456264185));
#202781=CARTESIAN_POINT('',(114.689796561242,1.35,48.8071575248888));
#202782=CARTESIAN_POINT('Origin',(114.689796561242,1.05,48.8071575248888));
#202783=CARTESIAN_POINT('',(115.180610063791,1.05,48.9025624813381));
#202784=CARTESIAN_POINT('',(115.123367089922,1.05,49.1970505828678));
#202785=CARTESIAN_POINT('',(115.180610063791,1.05,48.9025624813381));
#202786=CARTESIAN_POINT('',(114.632553587372,1.05,49.1016456264185));
#202787=CARTESIAN_POINT('',(114.632553587372,1.05,49.1016456264185));
#202788=CARTESIAN_POINT('',(114.689796561242,1.05,48.8071575248888));
#202789=CARTESIAN_POINT('',(114.689796561242,1.05,48.8071575248888));
#202790=CARTESIAN_POINT('',(114.689796561242,1.05,48.8071575248888));
#202791=CARTESIAN_POINT('Origin',(115.180610063791,1.05,48.9025624813381));
#202792=CARTESIAN_POINT('',(115.180610063791,0.550000000000015,48.9025624813381));
#202793=CARTESIAN_POINT('',(115.123367089922,0.550000000000015,49.1970505828678));
#202794=CARTESIAN_POINT('',(115.180610063791,0.550000000000015,48.9025624813381));
#202795=CARTESIAN_POINT('',(115.123367089922,1.05,49.1970505828678));
#202796=CARTESIAN_POINT('',(115.180610063791,1.05,48.9025624813381));
#202797=CARTESIAN_POINT('Origin',(115.180610063791,0.550000000000015,48.9025624813381));
#202798=CARTESIAN_POINT('',(114.689796561242,0.550000000000015,48.8071575248888));
#202799=CARTESIAN_POINT('',(114.632553587372,0.550000000000015,49.1016456264185));
#202800=CARTESIAN_POINT('',(114.689796561242,0.550000000000015,48.8071575248888));
#202801=CARTESIAN_POINT('',(115.123367089922,0.550000000000015,49.1970505828678));
#202802=CARTESIAN_POINT('',(115.180610063791,0.550000000000015,48.9025624813381));
#202803=CARTESIAN_POINT('Origin',(114.689796561242,0.550000000000015,48.8071575248888));
#202804=CARTESIAN_POINT('',(114.632553587372,0.550000000000015,49.1016456264185));
#202805=CARTESIAN_POINT('',(114.689796561242,0.550000000000015,48.8071575248888));
#202806=CARTESIAN_POINT('Origin',(114.689796561242,0.250000000000015,48.8071575248888));
#202807=CARTESIAN_POINT('',(115.180610063791,0.250000000000015,48.9025624813381));
#202808=CARTESIAN_POINT('',(115.123367089922,0.250000000000015,49.1970505828678));
#202809=CARTESIAN_POINT('',(115.180610063791,0.250000000000015,48.9025624813381));
#202810=CARTESIAN_POINT('',(114.632553587372,0.250000000000015,49.1016456264185));
#202811=CARTESIAN_POINT('',(114.632553587372,0.250000000000015,49.1016456264185));
#202812=CARTESIAN_POINT('',(114.689796561242,0.250000000000015,48.8071575248888));
#202813=CARTESIAN_POINT('',(114.689796561242,0.250000000000015,48.8071575248888));
#202814=CARTESIAN_POINT('',(114.689796561242,0.250000000000015,48.8071575248888));
#202815=CARTESIAN_POINT('Origin',(115.180610063791,0.250000000000015,48.9025624813381));
#202816=CARTESIAN_POINT('',(115.180610063791,-0.249999999999985,48.9025624813381));
#202817=CARTESIAN_POINT('',(115.123367089922,-0.249999999999985,49.1970505828678));
#202818=CARTESIAN_POINT('',(115.180610063791,-0.249999999999985,48.9025624813381));
#202819=CARTESIAN_POINT('',(115.123367089922,0.250000000000015,49.1970505828678));
#202820=CARTESIAN_POINT('',(115.180610063791,0.250000000000015,48.9025624813381));
#202821=CARTESIAN_POINT('Origin',(115.180610063791,-0.249999999999985,48.9025624813381));
#202822=CARTESIAN_POINT('',(114.689796561242,-0.249999999999985,48.8071575248888));
#202823=CARTESIAN_POINT('',(114.632553587372,-0.249999999999985,49.1016456264185));
#202824=CARTESIAN_POINT('',(114.689796561242,-0.249999999999985,48.8071575248888));
#202825=CARTESIAN_POINT('',(115.123367089922,-0.249999999999985,49.1970505828678));
#202826=CARTESIAN_POINT('',(115.180610063791,-0.249999999999985,48.9025624813381));
#202827=CARTESIAN_POINT('Origin',(114.689796561242,-0.249999999999985,48.8071575248888));
#202828=CARTESIAN_POINT('',(114.632553587372,-0.249999999999985,49.1016456264185));
#202829=CARTESIAN_POINT('',(114.689796561242,-0.249999999999985,48.8071575248888));
#202830=CARTESIAN_POINT('Origin',(114.689796561242,-0.549999999999986,48.8071575248888));
#202831=CARTESIAN_POINT('',(115.180610063791,-0.549999999999986,48.9025624813381));
#202832=CARTESIAN_POINT('',(115.123367089922,-0.549999999999986,49.1970505828678));
#202833=CARTESIAN_POINT('',(115.180610063791,-0.549999999999986,48.9025624813381));
#202834=CARTESIAN_POINT('',(114.632553587372,-0.549999999999986,49.1016456264185));
#202835=CARTESIAN_POINT('',(114.632553587372,-0.549999999999986,49.1016456264185));
#202836=CARTESIAN_POINT('',(114.689796561242,-0.549999999999986,48.8071575248888));
#202837=CARTESIAN_POINT('',(114.689796561242,-0.549999999999986,48.8071575248888));
#202838=CARTESIAN_POINT('',(114.689796561242,-0.549999999999986,48.8071575248888));
#202839=CARTESIAN_POINT('Origin',(115.180610063791,-0.549999999999986,48.9025624813381));
#202840=CARTESIAN_POINT('',(115.180610063791,-1.05,48.9025624813381));
#202841=CARTESIAN_POINT('',(115.123367089922,-1.05,49.1970505828678));
#202842=CARTESIAN_POINT('',(115.180610063791,-1.05,48.9025624813381));
#202843=CARTESIAN_POINT('',(115.123367089922,-0.549999999999986,49.1970505828678));
#202844=CARTESIAN_POINT('',(115.180610063791,-0.549999999999986,48.9025624813381));
#202845=CARTESIAN_POINT('Origin',(115.180610063791,-1.05,48.9025624813381));
#202846=CARTESIAN_POINT('',(114.689796561242,-1.05,48.8071575248888));
#202847=CARTESIAN_POINT('',(114.632553587372,-1.05,49.1016456264185));
#202848=CARTESIAN_POINT('',(114.689796561242,-1.05,48.8071575248888));
#202849=CARTESIAN_POINT('',(115.123367089922,-1.05,49.1970505828678));
#202850=CARTESIAN_POINT('',(115.180610063791,-1.05,48.9025624813381));
#202851=CARTESIAN_POINT('Origin',(114.689796561242,-1.05,48.8071575248888));
#202852=CARTESIAN_POINT('',(114.632553587372,-1.05,49.1016456264185));
#202853=CARTESIAN_POINT('',(114.689796561242,-1.05,48.8071575248888));
#202854=CARTESIAN_POINT('Origin',(114.689796561242,-1.35,48.8071575248888));
#202855=CARTESIAN_POINT('',(115.180610063791,-1.35,48.9025624813381));
#202856=CARTESIAN_POINT('',(115.123367089922,-1.35,49.1970505828678));
#202857=CARTESIAN_POINT('',(115.180610063791,-1.35,48.9025624813381));
#202858=CARTESIAN_POINT('',(114.632553587372,-1.35,49.1016456264185));
#202859=CARTESIAN_POINT('',(114.632553587372,-1.35,49.1016456264185));
#202860=CARTESIAN_POINT('',(114.689796561242,-1.35,48.8071575248888));
#202861=CARTESIAN_POINT('',(114.689796561242,-1.35,48.8071575248888));
#202862=CARTESIAN_POINT('',(114.689796561242,-1.35,48.8071575248888));
#202863=CARTESIAN_POINT('Origin',(115.180610063791,-1.35,48.9025624813381));
#202864=CARTESIAN_POINT('',(115.180610063791,-1.85,48.9025624813381));
#202865=CARTESIAN_POINT('',(115.123367089922,-1.85,49.1970505828678));
#202866=CARTESIAN_POINT('',(115.180610063791,-1.85,48.9025624813381));
#202867=CARTESIAN_POINT('',(115.123367089922,-1.35,49.1970505828678));
#202868=CARTESIAN_POINT('',(115.180610063791,-1.35,48.9025624813381));
#202869=CARTESIAN_POINT('Origin',(115.180610063791,-1.85,48.9025624813381));
#202870=CARTESIAN_POINT('',(114.689796561242,-1.85,48.8071575248888));
#202871=CARTESIAN_POINT('',(114.632553587372,-1.85,49.1016456264185));
#202872=CARTESIAN_POINT('',(114.689796561242,-1.85,48.8071575248888));
#202873=CARTESIAN_POINT('',(115.123367089922,-1.85,49.1970505828678));
#202874=CARTESIAN_POINT('',(115.180610063791,-1.85,48.9025624813381));
#202875=CARTESIAN_POINT('Origin',(114.689796561242,-1.85,48.8071575248888));
#202876=CARTESIAN_POINT('',(114.632553587372,-1.85,49.1016456264185));
#202877=CARTESIAN_POINT('',(114.689796561242,-1.85,48.8071575248888));
#202878=CARTESIAN_POINT('Origin',(114.689796561242,-2.15,48.8071575248888));
#202879=CARTESIAN_POINT('',(115.180610063791,-2.15,48.9025624813381));
#202880=CARTESIAN_POINT('',(115.123367089922,-2.15,49.1970505828678));
#202881=CARTESIAN_POINT('',(115.180610063791,-2.15,48.9025624813381));
#202882=CARTESIAN_POINT('',(114.632553587372,-2.15,49.1016456264185));
#202883=CARTESIAN_POINT('',(114.632553587372,-2.15,49.1016456264185));
#202884=CARTESIAN_POINT('',(114.689796561242,-2.15,48.8071575248888));
#202885=CARTESIAN_POINT('',(114.689796561242,-2.15,48.8071575248888));
#202886=CARTESIAN_POINT('',(114.689796561242,-2.15,48.8071575248888));
#202887=CARTESIAN_POINT('Origin',(115.180610063791,-2.15,48.9025624813381));
#202888=CARTESIAN_POINT('',(115.180610063791,-2.65,48.9025624813381));
#202889=CARTESIAN_POINT('',(115.123367089922,-2.65,49.1970505828678));
#202890=CARTESIAN_POINT('',(115.180610063791,-2.65,48.9025624813381));
#202891=CARTESIAN_POINT('',(115.123367089922,-2.15,49.1970505828678));
#202892=CARTESIAN_POINT('',(115.180610063791,-2.15,48.9025624813381));
#202893=CARTESIAN_POINT('Origin',(115.180610063791,-2.65,48.9025624813381));
#202894=CARTESIAN_POINT('',(114.689796561242,-2.65,48.8071575248888));
#202895=CARTESIAN_POINT('',(114.632553587372,-2.65,49.1016456264185));
#202896=CARTESIAN_POINT('',(114.689796561242,-2.65,48.8071575248888));
#202897=CARTESIAN_POINT('',(115.123367089922,-2.65,49.1970505828678));
#202898=CARTESIAN_POINT('',(115.180610063791,-2.65,48.9025624813381));
#202899=CARTESIAN_POINT('Origin',(114.689796561242,-2.65,48.8071575248888));
#202900=CARTESIAN_POINT('',(114.632553587372,-2.65,49.1016456264185));
#202901=CARTESIAN_POINT('',(114.689796561242,-2.65,48.8071575248888));
#202902=CARTESIAN_POINT('Origin',(115.475098165321,-2.15,48.9598054552076));
#202903=CARTESIAN_POINT('',(115.96591166787,-2.15,49.0552104116569));
#202904=CARTESIAN_POINT('',(115.908668694001,-2.15,49.3496985131866));
#202905=CARTESIAN_POINT('',(115.96591166787,-2.15,49.0552104116569));
#202906=CARTESIAN_POINT('',(115.417855191451,-2.15,49.2542935567373));
#202907=CARTESIAN_POINT('',(115.417855191451,-2.15,49.2542935567373));
#202908=CARTESIAN_POINT('',(115.475098165321,-2.15,48.9598054552076));
#202909=CARTESIAN_POINT('',(115.475098165321,-2.15,48.9598054552076));
#202910=CARTESIAN_POINT('',(115.475098165321,-2.15,48.9598054552076));
#202911=CARTESIAN_POINT('Origin',(115.96591166787,-2.15,49.0552104116569));
#202912=CARTESIAN_POINT('',(115.96591166787,-2.65,49.0552104116569));
#202913=CARTESIAN_POINT('',(115.908668694001,-2.65,49.3496985131866));
#202914=CARTESIAN_POINT('',(115.96591166787,-2.65,49.0552104116569));
#202915=CARTESIAN_POINT('',(115.908668694001,-2.15,49.3496985131866));
#202916=CARTESIAN_POINT('',(115.96591166787,-2.15,49.0552104116569));
#202917=CARTESIAN_POINT('Origin',(115.96591166787,-2.65,49.0552104116569));
#202918=CARTESIAN_POINT('',(115.475098165321,-2.65,48.9598054552076));
#202919=CARTESIAN_POINT('',(115.417855191451,-2.65,49.2542935567373));
#202920=CARTESIAN_POINT('',(115.475098165321,-2.65,48.9598054552076));
#202921=CARTESIAN_POINT('',(115.908668694001,-2.65,49.3496985131866));
#202922=CARTESIAN_POINT('',(115.96591166787,-2.65,49.0552104116569));
#202923=CARTESIAN_POINT('Origin',(115.475098165321,-2.65,48.9598054552076));
#202924=CARTESIAN_POINT('',(115.417855191451,-2.65,49.2542935567373));
#202925=CARTESIAN_POINT('',(115.475098165321,-2.65,48.9598054552076));
#202926=CARTESIAN_POINT('Origin',(116.2603997694,-2.15,49.1124533855264));
#202927=CARTESIAN_POINT('',(116.75121327195,-2.15,49.2078583419757));
#202928=CARTESIAN_POINT('',(116.69397029808,-2.15,49.5023464435054));
#202929=CARTESIAN_POINT('',(116.75121327195,-2.15,49.2078583419757));
#202930=CARTESIAN_POINT('',(116.203156795531,-2.15,49.4069414870561));
#202931=CARTESIAN_POINT('',(116.203156795531,-2.15,49.4069414870561));
#202932=CARTESIAN_POINT('',(116.2603997694,-2.15,49.1124533855264));
#202933=CARTESIAN_POINT('',(116.2603997694,-2.15,49.1124533855264));
#202934=CARTESIAN_POINT('',(116.2603997694,-2.15,49.1124533855264));
#202935=CARTESIAN_POINT('Origin',(116.75121327195,-2.15,49.2078583419757));
#202936=CARTESIAN_POINT('',(116.75121327195,-2.65,49.2078583419757));
#202937=CARTESIAN_POINT('',(116.69397029808,-2.65,49.5023464435054));
#202938=CARTESIAN_POINT('',(116.75121327195,-2.65,49.2078583419757));
#202939=CARTESIAN_POINT('',(116.69397029808,-2.15,49.5023464435054));
#202940=CARTESIAN_POINT('',(116.75121327195,-2.15,49.2078583419757));
#202941=CARTESIAN_POINT('Origin',(116.75121327195,-2.65,49.2078583419757));
#202942=CARTESIAN_POINT('',(116.2603997694,-2.65,49.1124533855264));
#202943=CARTESIAN_POINT('',(116.203156795531,-2.65,49.4069414870561));
#202944=CARTESIAN_POINT('',(116.2603997694,-2.65,49.1124533855264));
#202945=CARTESIAN_POINT('',(116.69397029808,-2.65,49.5023464435054));
#202946=CARTESIAN_POINT('',(116.75121327195,-2.65,49.2078583419757));
#202947=CARTESIAN_POINT('Origin',(116.2603997694,-2.65,49.1124533855264));
#202948=CARTESIAN_POINT('',(116.203156795531,-2.65,49.4069414870561));
#202949=CARTESIAN_POINT('',(116.2603997694,-2.65,49.1124533855264));
#202950=CARTESIAN_POINT('Origin',(117.045701373479,-2.15,49.2651013158452));
#202951=CARTESIAN_POINT('',(117.536514876029,-2.15,49.3605062722945));
#202952=CARTESIAN_POINT('',(117.479271902159,-2.15,49.6549943738242));
#202953=CARTESIAN_POINT('',(117.536514876029,-2.15,49.3605062722945));
#202954=CARTESIAN_POINT('',(116.98845839961,-2.15,49.5595894173749));
#202955=CARTESIAN_POINT('',(116.98845839961,-2.15,49.5595894173749));
#202956=CARTESIAN_POINT('',(117.045701373479,-2.15,49.2651013158452));
#202957=CARTESIAN_POINT('',(117.045701373479,-2.15,49.2651013158452));
#202958=CARTESIAN_POINT('',(117.045701373479,-2.15,49.2651013158452));
#202959=CARTESIAN_POINT('Origin',(117.536514876029,-2.15,49.3605062722945));
#202960=CARTESIAN_POINT('',(117.536514876029,-2.65,49.3605062722945));
#202961=CARTESIAN_POINT('',(117.479271902159,-2.65,49.6549943738242));
#202962=CARTESIAN_POINT('',(117.536514876029,-2.65,49.3605062722945));
#202963=CARTESIAN_POINT('',(117.479271902159,-2.15,49.6549943738242));
#202964=CARTESIAN_POINT('',(117.536514876029,-2.15,49.3605062722945));
#202965=CARTESIAN_POINT('Origin',(117.536514876029,-2.65,49.3605062722945));
#202966=CARTESIAN_POINT('',(117.045701373479,-2.65,49.2651013158452));
#202967=CARTESIAN_POINT('',(116.98845839961,-2.65,49.5595894173749));
#202968=CARTESIAN_POINT('',(117.045701373479,-2.65,49.2651013158452));
#202969=CARTESIAN_POINT('',(117.479271902159,-2.65,49.6549943738242));
#202970=CARTESIAN_POINT('',(117.536514876029,-2.65,49.3605062722945));
#202971=CARTESIAN_POINT('Origin',(117.045701373479,-2.65,49.2651013158452));
#202972=CARTESIAN_POINT('',(116.98845839961,-2.65,49.5595894173749));
#202973=CARTESIAN_POINT('',(117.045701373479,-2.65,49.2651013158452));
#202974=CARTESIAN_POINT('Origin',(117.831002977559,-2.15,49.417749246164));
#202975=CARTESIAN_POINT('',(118.321816480108,-2.15,49.5131542026133));
#202976=CARTESIAN_POINT('',(118.264573506239,-2.15,49.807642304143));
#202977=CARTESIAN_POINT('',(118.321816480108,-2.15,49.5131542026133));
#202978=CARTESIAN_POINT('',(117.773760003689,-2.15,49.7122373476937));
#202979=CARTESIAN_POINT('',(117.773760003689,-2.15,49.7122373476937));
#202980=CARTESIAN_POINT('',(117.831002977559,-2.15,49.417749246164));
#202981=CARTESIAN_POINT('',(117.831002977559,-2.15,49.417749246164));
#202982=CARTESIAN_POINT('',(117.831002977559,-2.15,49.417749246164));
#202983=CARTESIAN_POINT('Origin',(118.321816480108,-2.15,49.5131542026133));
#202984=CARTESIAN_POINT('',(118.321816480108,-2.65,49.5131542026133));
#202985=CARTESIAN_POINT('',(118.264573506239,-2.65,49.807642304143));
#202986=CARTESIAN_POINT('',(118.321816480108,-2.65,49.5131542026133));
#202987=CARTESIAN_POINT('',(118.264573506239,-2.15,49.807642304143));
#202988=CARTESIAN_POINT('',(118.321816480108,-2.15,49.5131542026133));
#202989=CARTESIAN_POINT('Origin',(118.321816480108,-2.65,49.5131542026133));
#202990=CARTESIAN_POINT('',(117.831002977559,-2.65,49.417749246164));
#202991=CARTESIAN_POINT('',(117.773760003689,-2.65,49.7122373476937));
#202992=CARTESIAN_POINT('',(117.831002977559,-2.65,49.417749246164));
#202993=CARTESIAN_POINT('',(118.264573506239,-2.65,49.807642304143));
#202994=CARTESIAN_POINT('',(118.321816480108,-2.65,49.5131542026133));
#202995=CARTESIAN_POINT('Origin',(117.831002977559,-2.65,49.417749246164));
#202996=CARTESIAN_POINT('',(117.773760003689,-2.65,49.7122373476937));
#202997=CARTESIAN_POINT('',(117.831002977559,-2.65,49.417749246164));
#202998=CARTESIAN_POINT('Origin',(118.616304581638,-2.15,49.5703971764828));
#202999=CARTESIAN_POINT('',(119.107118084187,-2.15,49.6658021329321));
#203000=CARTESIAN_POINT('',(119.049875110318,-2.15,49.9602902344618));
#203001=CARTESIAN_POINT('',(119.107118084187,-2.15,49.6658021329321));
#203002=CARTESIAN_POINT('',(118.559061607768,-2.15,49.8648852780125));
#203003=CARTESIAN_POINT('',(118.559061607768,-2.15,49.8648852780125));
#203004=CARTESIAN_POINT('',(118.616304581638,-2.15,49.5703971764828));
#203005=CARTESIAN_POINT('',(118.616304581638,-2.15,49.5703971764828));
#203006=CARTESIAN_POINT('',(118.616304581638,-2.15,49.5703971764828));
#203007=CARTESIAN_POINT('Origin',(119.107118084187,-2.15,49.6658021329321));
#203008=CARTESIAN_POINT('',(119.107118084187,-2.65,49.6658021329321));
#203009=CARTESIAN_POINT('',(119.049875110318,-2.65,49.9602902344618));
#203010=CARTESIAN_POINT('',(119.107118084187,-2.65,49.6658021329321));
#203011=CARTESIAN_POINT('',(119.049875110318,-2.15,49.9602902344618));
#203012=CARTESIAN_POINT('',(119.107118084187,-2.15,49.6658021329321));
#203013=CARTESIAN_POINT('Origin',(119.107118084187,-2.65,49.6658021329321));
#203014=CARTESIAN_POINT('',(118.616304581638,-2.65,49.5703971764828));
#203015=CARTESIAN_POINT('',(118.559061607768,-2.65,49.8648852780125));
#203016=CARTESIAN_POINT('',(118.616304581638,-2.65,49.5703971764828));
#203017=CARTESIAN_POINT('',(119.049875110318,-2.65,49.9602902344618));
#203018=CARTESIAN_POINT('',(119.107118084187,-2.65,49.6658021329321));
#203019=CARTESIAN_POINT('Origin',(118.616304581638,-2.65,49.5703971764828));
#203020=CARTESIAN_POINT('',(118.559061607768,-2.65,49.8648852780125));
#203021=CARTESIAN_POINT('',(118.616304581638,-2.65,49.5703971764828));
#203022=CARTESIAN_POINT('Origin',(119.401606185717,-2.15,49.7230451068016));
#203023=CARTESIAN_POINT('',(119.892419688267,-2.15,49.8184500632509));
#203024=CARTESIAN_POINT('',(119.835176714397,-2.15,50.1129381647806));
#203025=CARTESIAN_POINT('',(119.892419688267,-2.15,49.8184500632509));
#203026=CARTESIAN_POINT('',(119.344363211847,-2.15,50.0175332083313));
#203027=CARTESIAN_POINT('',(119.344363211847,-2.15,50.0175332083313));
#203028=CARTESIAN_POINT('',(119.401606185717,-2.15,49.7230451068016));
#203029=CARTESIAN_POINT('',(119.401606185717,-2.15,49.7230451068016));
#203030=CARTESIAN_POINT('',(119.401606185717,-2.15,49.7230451068016));
#203031=CARTESIAN_POINT('Origin',(119.892419688267,-2.15,49.8184500632509));
#203032=CARTESIAN_POINT('',(119.892419688267,-2.65,49.8184500632509));
#203033=CARTESIAN_POINT('',(119.835176714397,-2.65,50.1129381647806));
#203034=CARTESIAN_POINT('',(119.892419688267,-2.65,49.8184500632509));
#203035=CARTESIAN_POINT('',(119.835176714397,-2.15,50.1129381647806));
#203036=CARTESIAN_POINT('',(119.892419688267,-2.15,49.8184500632509));
#203037=CARTESIAN_POINT('Origin',(119.892419688267,-2.65,49.8184500632509));
#203038=CARTESIAN_POINT('',(119.401606185717,-2.65,49.7230451068016));
#203039=CARTESIAN_POINT('',(119.344363211847,-2.65,50.0175332083313));
#203040=CARTESIAN_POINT('',(119.401606185717,-2.65,49.7230451068016));
#203041=CARTESIAN_POINT('',(119.835176714397,-2.65,50.1129381647806));
#203042=CARTESIAN_POINT('',(119.892419688267,-2.65,49.8184500632509));
#203043=CARTESIAN_POINT('Origin',(119.401606185717,-2.65,49.7230451068016));
#203044=CARTESIAN_POINT('',(119.344363211847,-2.65,50.0175332083313));
#203045=CARTESIAN_POINT('',(119.401606185717,-2.65,49.7230451068016));
#203046=CARTESIAN_POINT('Origin',(119.401606185717,-1.35,49.7230451068016));
#203047=CARTESIAN_POINT('',(119.892419688267,-1.35,49.8184500632509));
#203048=CARTESIAN_POINT('',(119.835176714397,-1.35,50.1129381647806));
#203049=CARTESIAN_POINT('',(119.892419688267,-1.35,49.8184500632509));
#203050=CARTESIAN_POINT('',(119.344363211847,-1.35,50.0175332083313));
#203051=CARTESIAN_POINT('',(119.344363211847,-1.35,50.0175332083313));
#203052=CARTESIAN_POINT('',(119.401606185717,-1.35,49.7230451068016));
#203053=CARTESIAN_POINT('',(119.401606185717,-1.35,49.7230451068016));
#203054=CARTESIAN_POINT('',(119.401606185717,-1.35,49.7230451068016));
#203055=CARTESIAN_POINT('Origin',(119.892419688267,-1.35,49.8184500632509));
#203056=CARTESIAN_POINT('',(119.892419688267,-1.85,49.8184500632509));
#203057=CARTESIAN_POINT('',(119.835176714397,-1.85,50.1129381647806));
#203058=CARTESIAN_POINT('',(119.892419688267,-1.85,49.8184500632509));
#203059=CARTESIAN_POINT('',(119.835176714397,-1.35,50.1129381647806));
#203060=CARTESIAN_POINT('',(119.892419688267,-1.35,49.8184500632509));
#203061=CARTESIAN_POINT('Origin',(119.892419688267,-1.85,49.8184500632509));
#203062=CARTESIAN_POINT('',(119.401606185717,-1.85,49.7230451068016));
#203063=CARTESIAN_POINT('',(119.344363211847,-1.85,50.0175332083313));
#203064=CARTESIAN_POINT('',(119.401606185717,-1.85,49.7230451068016));
#203065=CARTESIAN_POINT('',(119.835176714397,-1.85,50.1129381647806));
#203066=CARTESIAN_POINT('',(119.892419688267,-1.85,49.8184500632509));
#203067=CARTESIAN_POINT('Origin',(119.401606185717,-1.85,49.7230451068016));
#203068=CARTESIAN_POINT('',(119.344363211847,-1.85,50.0175332083313));
#203069=CARTESIAN_POINT('',(119.401606185717,-1.85,49.7230451068016));
#203070=CARTESIAN_POINT('Origin',(119.401606185717,-0.549999999999986,49.7230451068016));
#203071=CARTESIAN_POINT('',(119.892419688267,-0.549999999999986,49.8184500632509));
#203072=CARTESIAN_POINT('',(119.835176714397,-0.549999999999986,50.1129381647806));
#203073=CARTESIAN_POINT('',(119.892419688267,-0.549999999999986,49.8184500632509));
#203074=CARTESIAN_POINT('',(119.344363211847,-0.549999999999986,50.0175332083313));
#203075=CARTESIAN_POINT('',(119.344363211847,-0.549999999999986,50.0175332083313));
#203076=CARTESIAN_POINT('',(119.401606185717,-0.549999999999986,49.7230451068016));
#203077=CARTESIAN_POINT('',(119.401606185717,-0.549999999999986,49.7230451068016));
#203078=CARTESIAN_POINT('',(119.401606185717,-0.549999999999986,49.7230451068016));
#203079=CARTESIAN_POINT('Origin',(119.892419688267,-0.549999999999986,49.8184500632509));
#203080=CARTESIAN_POINT('',(119.892419688267,-1.05,49.8184500632509));
#203081=CARTESIAN_POINT('',(119.835176714397,-1.05,50.1129381647806));
#203082=CARTESIAN_POINT('',(119.892419688267,-1.05,49.8184500632509));
#203083=CARTESIAN_POINT('',(119.835176714397,-0.549999999999986,50.1129381647806));
#203084=CARTESIAN_POINT('',(119.892419688267,-0.549999999999986,49.8184500632509));
#203085=CARTESIAN_POINT('Origin',(119.892419688267,-1.05,49.8184500632509));
#203086=CARTESIAN_POINT('',(119.401606185717,-1.05,49.7230451068016));
#203087=CARTESIAN_POINT('',(119.344363211847,-1.05,50.0175332083313));
#203088=CARTESIAN_POINT('',(119.401606185717,-1.05,49.7230451068016));
#203089=CARTESIAN_POINT('',(119.835176714397,-1.05,50.1129381647806));
#203090=CARTESIAN_POINT('',(119.892419688267,-1.05,49.8184500632509));
#203091=CARTESIAN_POINT('Origin',(119.401606185717,-1.05,49.7230451068016));
#203092=CARTESIAN_POINT('',(119.344363211847,-1.05,50.0175332083313));
#203093=CARTESIAN_POINT('',(119.401606185717,-1.05,49.7230451068016));
#203094=CARTESIAN_POINT('Origin',(119.401606185717,0.250000000000015,49.7230451068016));
#203095=CARTESIAN_POINT('',(119.892419688267,0.250000000000015,49.8184500632509));
#203096=CARTESIAN_POINT('',(119.835176714397,0.250000000000015,50.1129381647806));
#203097=CARTESIAN_POINT('',(119.892419688267,0.250000000000015,49.8184500632509));
#203098=CARTESIAN_POINT('',(119.344363211847,0.250000000000015,50.0175332083313));
#203099=CARTESIAN_POINT('',(119.344363211847,0.250000000000015,50.0175332083313));
#203100=CARTESIAN_POINT('',(119.401606185717,0.250000000000015,49.7230451068016));
#203101=CARTESIAN_POINT('',(119.401606185717,0.250000000000015,49.7230451068016));
#203102=CARTESIAN_POINT('',(119.401606185717,0.250000000000015,49.7230451068016));
#203103=CARTESIAN_POINT('Origin',(119.892419688267,0.250000000000015,49.8184500632509));
#203104=CARTESIAN_POINT('',(119.892419688267,-0.249999999999985,49.8184500632509));
#203105=CARTESIAN_POINT('',(119.835176714397,-0.249999999999985,50.1129381647806));
#203106=CARTESIAN_POINT('',(119.892419688267,-0.249999999999985,49.8184500632509));
#203107=CARTESIAN_POINT('',(119.835176714397,0.250000000000015,50.1129381647806));
#203108=CARTESIAN_POINT('',(119.892419688267,0.250000000000015,49.8184500632509));
#203109=CARTESIAN_POINT('Origin',(119.892419688267,-0.249999999999985,49.8184500632509));
#203110=CARTESIAN_POINT('',(119.401606185717,-0.249999999999985,49.7230451068016));
#203111=CARTESIAN_POINT('',(119.344363211847,-0.249999999999985,50.0175332083313));
#203112=CARTESIAN_POINT('',(119.401606185717,-0.249999999999985,49.7230451068016));
#203113=CARTESIAN_POINT('',(119.835176714397,-0.249999999999985,50.1129381647806));
#203114=CARTESIAN_POINT('',(119.892419688267,-0.249999999999985,49.8184500632509));
#203115=CARTESIAN_POINT('Origin',(119.401606185717,-0.249999999999985,49.7230451068016));
#203116=CARTESIAN_POINT('',(119.344363211847,-0.249999999999985,50.0175332083313));
#203117=CARTESIAN_POINT('',(119.401606185717,-0.249999999999985,49.7230451068016));
#203118=CARTESIAN_POINT('Origin',(119.401606185717,1.05,49.7230451068016));
#203119=CARTESIAN_POINT('',(119.892419688267,1.05,49.8184500632509));
#203120=CARTESIAN_POINT('',(119.835176714397,1.05,50.1129381647806));
#203121=CARTESIAN_POINT('',(119.892419688267,1.05,49.8184500632509));
#203122=CARTESIAN_POINT('',(119.344363211847,1.05,50.0175332083313));
#203123=CARTESIAN_POINT('',(119.344363211847,1.05,50.0175332083313));
#203124=CARTESIAN_POINT('',(119.401606185717,1.05,49.7230451068016));
#203125=CARTESIAN_POINT('',(119.401606185717,1.05,49.7230451068016));
#203126=CARTESIAN_POINT('',(119.401606185717,1.05,49.7230451068016));
#203127=CARTESIAN_POINT('Origin',(119.892419688267,1.05,49.8184500632509));
#203128=CARTESIAN_POINT('',(119.892419688267,0.550000000000015,49.8184500632509));
#203129=CARTESIAN_POINT('',(119.835176714397,0.550000000000015,50.1129381647806));
#203130=CARTESIAN_POINT('',(119.892419688267,0.550000000000015,49.8184500632509));
#203131=CARTESIAN_POINT('',(119.835176714397,1.05,50.1129381647806));
#203132=CARTESIAN_POINT('',(119.892419688267,1.05,49.8184500632509));
#203133=CARTESIAN_POINT('Origin',(119.892419688267,0.550000000000015,49.8184500632509));
#203134=CARTESIAN_POINT('',(119.401606185717,0.550000000000015,49.7230451068016));
#203135=CARTESIAN_POINT('',(119.344363211847,0.550000000000015,50.0175332083313));
#203136=CARTESIAN_POINT('',(119.401606185717,0.550000000000015,49.7230451068016));
#203137=CARTESIAN_POINT('',(119.835176714397,0.550000000000015,50.1129381647806));
#203138=CARTESIAN_POINT('',(119.892419688267,0.550000000000015,49.8184500632509));
#203139=CARTESIAN_POINT('Origin',(119.401606185717,0.550000000000015,49.7230451068016));
#203140=CARTESIAN_POINT('',(119.344363211847,0.550000000000015,50.0175332083313));
#203141=CARTESIAN_POINT('',(119.401606185717,0.550000000000015,49.7230451068016));
#203142=CARTESIAN_POINT('Origin',(119.401606185717,1.85,49.7230451068016));
#203143=CARTESIAN_POINT('',(119.892419688267,1.85,49.8184500632509));
#203144=CARTESIAN_POINT('',(119.835176714397,1.85,50.1129381647806));
#203145=CARTESIAN_POINT('',(119.892419688267,1.85,49.8184500632509));
#203146=CARTESIAN_POINT('',(119.344363211847,1.85,50.0175332083313));
#203147=CARTESIAN_POINT('',(119.344363211847,1.85,50.0175332083313));
#203148=CARTESIAN_POINT('',(119.401606185717,1.85,49.7230451068016));
#203149=CARTESIAN_POINT('',(119.401606185717,1.85,49.7230451068016));
#203150=CARTESIAN_POINT('',(119.401606185717,1.85,49.7230451068016));
#203151=CARTESIAN_POINT('Origin',(119.892419688267,1.85,49.8184500632509));
#203152=CARTESIAN_POINT('',(119.892419688267,1.35,49.8184500632509));
#203153=CARTESIAN_POINT('',(119.835176714397,1.35,50.1129381647806));
#203154=CARTESIAN_POINT('',(119.892419688267,1.35,49.8184500632509));
#203155=CARTESIAN_POINT('',(119.835176714397,1.85,50.1129381647806));
#203156=CARTESIAN_POINT('',(119.892419688267,1.85,49.8184500632509));
#203157=CARTESIAN_POINT('Origin',(119.892419688267,1.35,49.8184500632509));
#203158=CARTESIAN_POINT('',(119.401606185717,1.35,49.7230451068016));
#203159=CARTESIAN_POINT('',(119.344363211847,1.35,50.0175332083313));
#203160=CARTESIAN_POINT('',(119.401606185717,1.35,49.7230451068016));
#203161=CARTESIAN_POINT('',(119.835176714397,1.35,50.1129381647806));
#203162=CARTESIAN_POINT('',(119.892419688267,1.35,49.8184500632509));
#203163=CARTESIAN_POINT('Origin',(119.401606185717,1.35,49.7230451068016));
#203164=CARTESIAN_POINT('',(119.344363211847,1.35,50.0175332083313));
#203165=CARTESIAN_POINT('',(119.401606185717,1.35,49.7230451068016));
#203166=CARTESIAN_POINT('Origin',(119.401606185717,2.65,49.7230451068016));
#203167=CARTESIAN_POINT('',(119.892419688267,2.65,49.8184500632509));
#203168=CARTESIAN_POINT('',(119.835176714397,2.65,50.1129381647806));
#203169=CARTESIAN_POINT('',(119.892419688267,2.65,49.8184500632509));
#203170=CARTESIAN_POINT('',(119.344363211847,2.65,50.0175332083313));
#203171=CARTESIAN_POINT('',(119.344363211847,2.65,50.0175332083313));
#203172=CARTESIAN_POINT('',(119.401606185717,2.65,49.7230451068016));
#203173=CARTESIAN_POINT('',(119.401606185717,2.65,49.7230451068016));
#203174=CARTESIAN_POINT('',(119.401606185717,2.65,49.7230451068016));
#203175=CARTESIAN_POINT('Origin',(119.892419688267,2.65,49.8184500632509));
#203176=CARTESIAN_POINT('',(119.892419688267,2.15,49.8184500632509));
#203177=CARTESIAN_POINT('',(119.835176714397,2.15,50.1129381647806));
#203178=CARTESIAN_POINT('',(119.892419688267,2.15,49.8184500632509));
#203179=CARTESIAN_POINT('',(119.835176714397,2.65,50.1129381647806));
#203180=CARTESIAN_POINT('',(119.892419688267,2.65,49.8184500632509));
#203181=CARTESIAN_POINT('Origin',(119.892419688267,2.15,49.8184500632509));
#203182=CARTESIAN_POINT('',(119.401606185717,2.15,49.7230451068016));
#203183=CARTESIAN_POINT('',(119.344363211847,2.15,50.0175332083313));
#203184=CARTESIAN_POINT('',(119.401606185717,2.15,49.7230451068016));
#203185=CARTESIAN_POINT('',(119.835176714397,2.15,50.1129381647806));
#203186=CARTESIAN_POINT('',(119.892419688267,2.15,49.8184500632509));
#203187=CARTESIAN_POINT('Origin',(119.401606185717,2.15,49.7230451068016));
#203188=CARTESIAN_POINT('',(119.344363211847,2.15,50.0175332083313));
#203189=CARTESIAN_POINT('',(119.401606185717,2.15,49.7230451068016));
#203190=CARTESIAN_POINT('Origin',(118.616304581638,2.65,49.5703971764828));
#203191=CARTESIAN_POINT('',(119.107118084187,2.65,49.6658021329321));
#203192=CARTESIAN_POINT('',(119.049875110318,2.65,49.9602902344618));
#203193=CARTESIAN_POINT('',(119.107118084187,2.65,49.6658021329321));
#203194=CARTESIAN_POINT('',(118.559061607768,2.65,49.8648852780125));
#203195=CARTESIAN_POINT('',(118.559061607768,2.65,49.8648852780125));
#203196=CARTESIAN_POINT('',(118.616304581638,2.65,49.5703971764828));
#203197=CARTESIAN_POINT('',(118.616304581638,2.65,49.5703971764828));
#203198=CARTESIAN_POINT('',(118.616304581638,2.65,49.5703971764828));
#203199=CARTESIAN_POINT('Origin',(119.107118084187,2.65,49.6658021329321));
#203200=CARTESIAN_POINT('',(119.107118084187,2.15,49.6658021329321));
#203201=CARTESIAN_POINT('',(119.049875110318,2.15,49.9602902344618));
#203202=CARTESIAN_POINT('',(119.107118084187,2.15,49.6658021329321));
#203203=CARTESIAN_POINT('',(119.049875110318,2.65,49.9602902344618));
#203204=CARTESIAN_POINT('',(119.107118084187,2.65,49.6658021329321));
#203205=CARTESIAN_POINT('Origin',(119.107118084187,2.15,49.6658021329321));
#203206=CARTESIAN_POINT('',(118.616304581638,2.15,49.5703971764828));
#203207=CARTESIAN_POINT('',(118.559061607768,2.15,49.8648852780125));
#203208=CARTESIAN_POINT('',(118.616304581638,2.15,49.5703971764828));
#203209=CARTESIAN_POINT('',(119.049875110318,2.15,49.9602902344618));
#203210=CARTESIAN_POINT('',(119.107118084187,2.15,49.6658021329321));
#203211=CARTESIAN_POINT('Origin',(118.616304581638,2.15,49.5703971764828));
#203212=CARTESIAN_POINT('',(118.559061607768,2.15,49.8648852780125));
#203213=CARTESIAN_POINT('',(118.616304581638,2.15,49.5703971764828));
#203214=CARTESIAN_POINT('Origin',(117.831002977559,2.65,49.417749246164));
#203215=CARTESIAN_POINT('',(118.321816480108,2.65,49.5131542026133));
#203216=CARTESIAN_POINT('',(118.264573506239,2.65,49.807642304143));
#203217=CARTESIAN_POINT('',(118.321816480108,2.65,49.5131542026133));
#203218=CARTESIAN_POINT('',(117.773760003689,2.65,49.7122373476937));
#203219=CARTESIAN_POINT('',(117.773760003689,2.65,49.7122373476937));
#203220=CARTESIAN_POINT('',(117.831002977559,2.65,49.417749246164));
#203221=CARTESIAN_POINT('',(117.831002977559,2.65,49.417749246164));
#203222=CARTESIAN_POINT('',(117.831002977559,2.65,49.417749246164));
#203223=CARTESIAN_POINT('Origin',(118.321816480108,2.65,49.5131542026133));
#203224=CARTESIAN_POINT('',(118.321816480108,2.15,49.5131542026133));
#203225=CARTESIAN_POINT('',(118.264573506239,2.15,49.807642304143));
#203226=CARTESIAN_POINT('',(118.321816480108,2.15,49.5131542026133));
#203227=CARTESIAN_POINT('',(118.264573506239,2.65,49.807642304143));
#203228=CARTESIAN_POINT('',(118.321816480108,2.65,49.5131542026133));
#203229=CARTESIAN_POINT('Origin',(118.321816480108,2.15,49.5131542026133));
#203230=CARTESIAN_POINT('',(117.831002977559,2.15,49.417749246164));
#203231=CARTESIAN_POINT('',(117.773760003689,2.15,49.7122373476937));
#203232=CARTESIAN_POINT('',(117.831002977559,2.15,49.417749246164));
#203233=CARTESIAN_POINT('',(118.264573506239,2.15,49.807642304143));
#203234=CARTESIAN_POINT('',(118.321816480108,2.15,49.5131542026133));
#203235=CARTESIAN_POINT('Origin',(117.831002977559,2.15,49.417749246164));
#203236=CARTESIAN_POINT('',(117.773760003689,2.15,49.7122373476937));
#203237=CARTESIAN_POINT('',(117.831002977559,2.15,49.417749246164));
#203238=CARTESIAN_POINT('Origin',(117.045701373479,2.65,49.2651013158452));
#203239=CARTESIAN_POINT('',(117.536514876029,2.65,49.3605062722945));
#203240=CARTESIAN_POINT('',(117.479271902159,2.65,49.6549943738242));
#203241=CARTESIAN_POINT('',(117.536514876029,2.65,49.3605062722945));
#203242=CARTESIAN_POINT('',(116.98845839961,2.65,49.5595894173749));
#203243=CARTESIAN_POINT('',(116.98845839961,2.65,49.5595894173749));
#203244=CARTESIAN_POINT('',(117.045701373479,2.65,49.2651013158452));
#203245=CARTESIAN_POINT('',(117.045701373479,2.65,49.2651013158452));
#203246=CARTESIAN_POINT('',(117.045701373479,2.65,49.2651013158452));
#203247=CARTESIAN_POINT('Origin',(117.536514876029,2.65,49.3605062722945));
#203248=CARTESIAN_POINT('',(117.536514876029,2.15,49.3605062722945));
#203249=CARTESIAN_POINT('',(117.479271902159,2.15,49.6549943738242));
#203250=CARTESIAN_POINT('',(117.536514876029,2.15,49.3605062722945));
#203251=CARTESIAN_POINT('',(117.479271902159,2.65,49.6549943738242));
#203252=CARTESIAN_POINT('',(117.536514876029,2.65,49.3605062722945));
#203253=CARTESIAN_POINT('Origin',(117.536514876029,2.15,49.3605062722945));
#203254=CARTESIAN_POINT('',(117.045701373479,2.15,49.2651013158452));
#203255=CARTESIAN_POINT('',(116.98845839961,2.15,49.5595894173749));
#203256=CARTESIAN_POINT('',(117.045701373479,2.15,49.2651013158452));
#203257=CARTESIAN_POINT('',(117.479271902159,2.15,49.6549943738242));
#203258=CARTESIAN_POINT('',(117.536514876029,2.15,49.3605062722945));
#203259=CARTESIAN_POINT('Origin',(117.045701373479,2.15,49.2651013158452));
#203260=CARTESIAN_POINT('',(116.98845839961,2.15,49.5595894173749));
#203261=CARTESIAN_POINT('',(117.045701373479,2.15,49.2651013158452));
#203262=CARTESIAN_POINT('Origin',(116.2603997694,2.65,49.1124533855264));
#203263=CARTESIAN_POINT('',(116.75121327195,2.65,49.2078583419757));
#203264=CARTESIAN_POINT('',(116.69397029808,2.65,49.5023464435054));
#203265=CARTESIAN_POINT('',(116.75121327195,2.65,49.2078583419757));
#203266=CARTESIAN_POINT('',(116.203156795531,2.65,49.4069414870561));
#203267=CARTESIAN_POINT('',(116.203156795531,2.65,49.4069414870561));
#203268=CARTESIAN_POINT('',(116.2603997694,2.65,49.1124533855264));
#203269=CARTESIAN_POINT('',(116.2603997694,2.65,49.1124533855264));
#203270=CARTESIAN_POINT('',(116.2603997694,2.65,49.1124533855264));
#203271=CARTESIAN_POINT('Origin',(116.75121327195,2.65,49.2078583419757));
#203272=CARTESIAN_POINT('',(116.75121327195,2.15,49.2078583419757));
#203273=CARTESIAN_POINT('',(116.69397029808,2.15,49.5023464435054));
#203274=CARTESIAN_POINT('',(116.75121327195,2.15,49.2078583419757));
#203275=CARTESIAN_POINT('',(116.69397029808,2.65,49.5023464435054));
#203276=CARTESIAN_POINT('',(116.75121327195,2.65,49.2078583419757));
#203277=CARTESIAN_POINT('Origin',(116.75121327195,2.15,49.2078583419757));
#203278=CARTESIAN_POINT('',(116.2603997694,2.15,49.1124533855264));
#203279=CARTESIAN_POINT('',(116.203156795531,2.15,49.4069414870561));
#203280=CARTESIAN_POINT('',(116.2603997694,2.15,49.1124533855264));
#203281=CARTESIAN_POINT('',(116.69397029808,2.15,49.5023464435054));
#203282=CARTESIAN_POINT('',(116.75121327195,2.15,49.2078583419757));
#203283=CARTESIAN_POINT('Origin',(116.2603997694,2.15,49.1124533855264));
#203284=CARTESIAN_POINT('',(116.203156795531,2.15,49.4069414870561));
#203285=CARTESIAN_POINT('',(116.2603997694,2.15,49.1124533855264));
#203286=CARTESIAN_POINT('Origin',(115.475098165321,2.65,48.9598054552076));
#203287=CARTESIAN_POINT('',(115.96591166787,2.65,49.0552104116569));
#203288=CARTESIAN_POINT('',(115.908668694001,2.65,49.3496985131866));
#203289=CARTESIAN_POINT('',(115.96591166787,2.65,49.0552104116569));
#203290=CARTESIAN_POINT('',(115.417855191451,2.65,49.2542935567373));
#203291=CARTESIAN_POINT('',(115.417855191451,2.65,49.2542935567373));
#203292=CARTESIAN_POINT('',(115.475098165321,2.65,48.9598054552076));
#203293=CARTESIAN_POINT('',(115.475098165321,2.65,48.9598054552076));
#203294=CARTESIAN_POINT('',(115.475098165321,2.65,48.9598054552076));
#203295=CARTESIAN_POINT('Origin',(115.96591166787,2.65,49.0552104116569));
#203296=CARTESIAN_POINT('',(115.96591166787,2.15,49.0552104116569));
#203297=CARTESIAN_POINT('',(115.908668694001,2.15,49.3496985131866));
#203298=CARTESIAN_POINT('',(115.96591166787,2.15,49.0552104116569));
#203299=CARTESIAN_POINT('',(115.908668694001,2.65,49.3496985131866));
#203300=CARTESIAN_POINT('',(115.96591166787,2.65,49.0552104116569));
#203301=CARTESIAN_POINT('Origin',(115.96591166787,2.15,49.0552104116569));
#203302=CARTESIAN_POINT('',(115.475098165321,2.15,48.9598054552076));
#203303=CARTESIAN_POINT('',(115.417855191451,2.15,49.2542935567373));
#203304=CARTESIAN_POINT('',(115.475098165321,2.15,48.9598054552076));
#203305=CARTESIAN_POINT('',(115.908668694001,2.15,49.3496985131866));
#203306=CARTESIAN_POINT('',(115.96591166787,2.15,49.0552104116569));
#203307=CARTESIAN_POINT('Origin',(115.475098165321,2.15,48.9598054552076));
#203308=CARTESIAN_POINT('',(115.417855191451,2.15,49.2542935567373));
#203309=CARTESIAN_POINT('',(115.475098165321,2.15,48.9598054552076));
#203310=CARTESIAN_POINT('Origin',(115.475098165321,1.85,48.9598054552076));
#203311=CARTESIAN_POINT('',(115.96591166787,1.85,49.0552104116569));
#203312=CARTESIAN_POINT('',(115.908668694001,1.85,49.3496985131866));
#203313=CARTESIAN_POINT('',(115.96591166787,1.85,49.0552104116569));
#203314=CARTESIAN_POINT('',(115.417855191451,1.85,49.2542935567373));
#203315=CARTESIAN_POINT('',(115.417855191451,1.85,49.2542935567373));
#203316=CARTESIAN_POINT('',(115.475098165321,1.85,48.9598054552076));
#203317=CARTESIAN_POINT('',(115.475098165321,1.85,48.9598054552076));
#203318=CARTESIAN_POINT('',(115.475098165321,1.85,48.9598054552076));
#203319=CARTESIAN_POINT('Origin',(115.96591166787,1.85,49.0552104116569));
#203320=CARTESIAN_POINT('',(115.96591166787,1.35,49.0552104116569));
#203321=CARTESIAN_POINT('',(115.908668694001,1.35,49.3496985131866));
#203322=CARTESIAN_POINT('',(115.96591166787,1.35,49.0552104116569));
#203323=CARTESIAN_POINT('',(115.908668694001,1.85,49.3496985131866));
#203324=CARTESIAN_POINT('',(115.96591166787,1.85,49.0552104116569));
#203325=CARTESIAN_POINT('Origin',(115.96591166787,1.35,49.0552104116569));
#203326=CARTESIAN_POINT('',(115.475098165321,1.35,48.9598054552076));
#203327=CARTESIAN_POINT('',(115.417855191451,1.35,49.2542935567373));
#203328=CARTESIAN_POINT('',(115.475098165321,1.35,48.9598054552076));
#203329=CARTESIAN_POINT('',(115.908668694001,1.35,49.3496985131866));
#203330=CARTESIAN_POINT('',(115.96591166787,1.35,49.0552104116569));
#203331=CARTESIAN_POINT('Origin',(115.475098165321,1.35,48.9598054552076));
#203332=CARTESIAN_POINT('',(115.417855191451,1.35,49.2542935567373));
#203333=CARTESIAN_POINT('',(115.475098165321,1.35,48.9598054552076));
#203334=CARTESIAN_POINT('Origin',(115.475098165321,1.05,48.9598054552076));
#203335=CARTESIAN_POINT('',(115.96591166787,1.05,49.0552104116569));
#203336=CARTESIAN_POINT('',(115.908668694001,1.05,49.3496985131866));
#203337=CARTESIAN_POINT('',(115.96591166787,1.05,49.0552104116569));
#203338=CARTESIAN_POINT('',(115.417855191451,1.05,49.2542935567373));
#203339=CARTESIAN_POINT('',(115.417855191451,1.05,49.2542935567373));
#203340=CARTESIAN_POINT('',(115.475098165321,1.05,48.9598054552076));
#203341=CARTESIAN_POINT('',(115.475098165321,1.05,48.9598054552076));
#203342=CARTESIAN_POINT('',(115.475098165321,1.05,48.9598054552076));
#203343=CARTESIAN_POINT('Origin',(115.96591166787,1.05,49.0552104116569));
#203344=CARTESIAN_POINT('',(115.96591166787,0.550000000000015,49.0552104116569));
#203345=CARTESIAN_POINT('',(115.908668694001,0.550000000000015,49.3496985131866));
#203346=CARTESIAN_POINT('',(115.96591166787,0.550000000000015,49.0552104116569));
#203347=CARTESIAN_POINT('',(115.908668694001,1.05,49.3496985131866));
#203348=CARTESIAN_POINT('',(115.96591166787,1.05,49.0552104116569));
#203349=CARTESIAN_POINT('Origin',(115.96591166787,0.550000000000015,49.0552104116569));
#203350=CARTESIAN_POINT('',(115.475098165321,0.550000000000015,48.9598054552076));
#203351=CARTESIAN_POINT('',(115.417855191451,0.550000000000015,49.2542935567373));
#203352=CARTESIAN_POINT('',(115.475098165321,0.550000000000015,48.9598054552076));
#203353=CARTESIAN_POINT('',(115.908668694001,0.550000000000015,49.3496985131866));
#203354=CARTESIAN_POINT('',(115.96591166787,0.550000000000015,49.0552104116569));
#203355=CARTESIAN_POINT('Origin',(115.475098165321,0.550000000000015,48.9598054552076));
#203356=CARTESIAN_POINT('',(115.417855191451,0.550000000000015,49.2542935567373));
#203357=CARTESIAN_POINT('',(115.475098165321,0.550000000000015,48.9598054552076));
#203358=CARTESIAN_POINT('Origin',(115.475098165321,0.250000000000015,48.9598054552076));
#203359=CARTESIAN_POINT('',(115.96591166787,0.250000000000015,49.0552104116569));
#203360=CARTESIAN_POINT('',(115.908668694001,0.250000000000015,49.3496985131866));
#203361=CARTESIAN_POINT('',(115.96591166787,0.250000000000015,49.0552104116569));
#203362=CARTESIAN_POINT('',(115.417855191451,0.250000000000015,49.2542935567373));
#203363=CARTESIAN_POINT('',(115.417855191451,0.250000000000015,49.2542935567373));
#203364=CARTESIAN_POINT('',(115.475098165321,0.250000000000015,48.9598054552076));
#203365=CARTESIAN_POINT('',(115.475098165321,0.250000000000015,48.9598054552076));
#203366=CARTESIAN_POINT('',(115.475098165321,0.250000000000015,48.9598054552076));
#203367=CARTESIAN_POINT('Origin',(115.96591166787,0.250000000000015,49.0552104116569));
#203368=CARTESIAN_POINT('',(115.96591166787,-0.249999999999985,49.0552104116569));
#203369=CARTESIAN_POINT('',(115.908668694001,-0.249999999999985,49.3496985131866));
#203370=CARTESIAN_POINT('',(115.96591166787,-0.249999999999985,49.0552104116569));
#203371=CARTESIAN_POINT('',(115.908668694001,0.250000000000015,49.3496985131866));
#203372=CARTESIAN_POINT('',(115.96591166787,0.250000000000015,49.0552104116569));
#203373=CARTESIAN_POINT('Origin',(115.96591166787,-0.249999999999985,49.0552104116569));
#203374=CARTESIAN_POINT('',(115.475098165321,-0.249999999999985,48.9598054552076));
#203375=CARTESIAN_POINT('',(115.417855191451,-0.249999999999985,49.2542935567373));
#203376=CARTESIAN_POINT('',(115.475098165321,-0.249999999999985,48.9598054552076));
#203377=CARTESIAN_POINT('',(115.908668694001,-0.249999999999985,49.3496985131866));
#203378=CARTESIAN_POINT('',(115.96591166787,-0.249999999999985,49.0552104116569));
#203379=CARTESIAN_POINT('Origin',(115.475098165321,-0.249999999999985,48.9598054552076));
#203380=CARTESIAN_POINT('',(115.417855191451,-0.249999999999985,49.2542935567373));
#203381=CARTESIAN_POINT('',(115.475098165321,-0.249999999999985,48.9598054552076));
#203382=CARTESIAN_POINT('Origin',(115.475098165321,-0.549999999999986,48.9598054552076));
#203383=CARTESIAN_POINT('',(115.96591166787,-0.549999999999986,49.0552104116569));
#203384=CARTESIAN_POINT('',(115.908668694001,-0.549999999999986,49.3496985131866));
#203385=CARTESIAN_POINT('',(115.96591166787,-0.549999999999986,49.0552104116569));
#203386=CARTESIAN_POINT('',(115.417855191451,-0.549999999999986,49.2542935567373));
#203387=CARTESIAN_POINT('',(115.417855191451,-0.549999999999986,49.2542935567373));
#203388=CARTESIAN_POINT('',(115.475098165321,-0.549999999999986,48.9598054552076));
#203389=CARTESIAN_POINT('',(115.475098165321,-0.549999999999986,48.9598054552076));
#203390=CARTESIAN_POINT('',(115.475098165321,-0.549999999999986,48.9598054552076));
#203391=CARTESIAN_POINT('Origin',(115.96591166787,-0.549999999999986,49.0552104116569));
#203392=CARTESIAN_POINT('',(115.96591166787,-1.05,49.0552104116569));
#203393=CARTESIAN_POINT('',(115.908668694001,-1.05,49.3496985131866));
#203394=CARTESIAN_POINT('',(115.96591166787,-1.05,49.0552104116569));
#203395=CARTESIAN_POINT('',(115.908668694001,-0.549999999999986,49.3496985131866));
#203396=CARTESIAN_POINT('',(115.96591166787,-0.549999999999986,49.0552104116569));
#203397=CARTESIAN_POINT('Origin',(115.96591166787,-1.05,49.0552104116569));
#203398=CARTESIAN_POINT('',(115.475098165321,-1.05,48.9598054552076));
#203399=CARTESIAN_POINT('',(115.417855191451,-1.05,49.2542935567373));
#203400=CARTESIAN_POINT('',(115.475098165321,-1.05,48.9598054552076));
#203401=CARTESIAN_POINT('',(115.908668694001,-1.05,49.3496985131866));
#203402=CARTESIAN_POINT('',(115.96591166787,-1.05,49.0552104116569));
#203403=CARTESIAN_POINT('Origin',(115.475098165321,-1.05,48.9598054552076));
#203404=CARTESIAN_POINT('',(115.417855191451,-1.05,49.2542935567373));
#203405=CARTESIAN_POINT('',(115.475098165321,-1.05,48.9598054552076));
#203406=CARTESIAN_POINT('Origin',(115.475098165321,-1.35,48.9598054552076));
#203407=CARTESIAN_POINT('',(115.96591166787,-1.35,49.0552104116569));
#203408=CARTESIAN_POINT('',(115.908668694001,-1.35,49.3496985131866));
#203409=CARTESIAN_POINT('',(115.96591166787,-1.35,49.0552104116569));
#203410=CARTESIAN_POINT('',(115.417855191451,-1.35,49.2542935567373));
#203411=CARTESIAN_POINT('',(115.417855191451,-1.35,49.2542935567373));
#203412=CARTESIAN_POINT('',(115.475098165321,-1.35,48.9598054552076));
#203413=CARTESIAN_POINT('',(115.475098165321,-1.35,48.9598054552076));
#203414=CARTESIAN_POINT('',(115.475098165321,-1.35,48.9598054552076));
#203415=CARTESIAN_POINT('Origin',(115.96591166787,-1.35,49.0552104116569));
#203416=CARTESIAN_POINT('',(115.96591166787,-1.85,49.0552104116569));
#203417=CARTESIAN_POINT('',(115.908668694001,-1.85,49.3496985131866));
#203418=CARTESIAN_POINT('',(115.96591166787,-1.85,49.0552104116569));
#203419=CARTESIAN_POINT('',(115.908668694001,-1.35,49.3496985131866));
#203420=CARTESIAN_POINT('',(115.96591166787,-1.35,49.0552104116569));
#203421=CARTESIAN_POINT('Origin',(115.96591166787,-1.85,49.0552104116569));
#203422=CARTESIAN_POINT('',(115.475098165321,-1.85,48.9598054552076));
#203423=CARTESIAN_POINT('',(115.417855191451,-1.85,49.2542935567373));
#203424=CARTESIAN_POINT('',(115.475098165321,-1.85,48.9598054552076));
#203425=CARTESIAN_POINT('',(115.908668694001,-1.85,49.3496985131866));
#203426=CARTESIAN_POINT('',(115.96591166787,-1.85,49.0552104116569));
#203427=CARTESIAN_POINT('Origin',(115.475098165321,-1.85,48.9598054552076));
#203428=CARTESIAN_POINT('',(115.417855191451,-1.85,49.2542935567373));
#203429=CARTESIAN_POINT('',(115.475098165321,-1.85,48.9598054552076));
#203430=CARTESIAN_POINT('Origin',(116.2603997694,-1.35,49.1124533855264));
#203431=CARTESIAN_POINT('',(116.75121327195,-1.35,49.2078583419757));
#203432=CARTESIAN_POINT('',(116.69397029808,-1.35,49.5023464435054));
#203433=CARTESIAN_POINT('',(116.75121327195,-1.35,49.2078583419757));
#203434=CARTESIAN_POINT('',(116.203156795531,-1.35,49.4069414870561));
#203435=CARTESIAN_POINT('',(116.203156795531,-1.35,49.4069414870561));
#203436=CARTESIAN_POINT('',(116.2603997694,-1.35,49.1124533855264));
#203437=CARTESIAN_POINT('',(116.2603997694,-1.35,49.1124533855264));
#203438=CARTESIAN_POINT('',(116.2603997694,-1.35,49.1124533855264));
#203439=CARTESIAN_POINT('Origin',(116.75121327195,-1.35,49.2078583419757));
#203440=CARTESIAN_POINT('',(116.75121327195,-1.85,49.2078583419757));
#203441=CARTESIAN_POINT('',(116.69397029808,-1.85,49.5023464435054));
#203442=CARTESIAN_POINT('',(116.75121327195,-1.85,49.2078583419757));
#203443=CARTESIAN_POINT('',(116.69397029808,-1.35,49.5023464435054));
#203444=CARTESIAN_POINT('',(116.75121327195,-1.35,49.2078583419757));
#203445=CARTESIAN_POINT('Origin',(116.75121327195,-1.85,49.2078583419757));
#203446=CARTESIAN_POINT('',(116.2603997694,-1.85,49.1124533855264));
#203447=CARTESIAN_POINT('',(116.203156795531,-1.85,49.4069414870561));
#203448=CARTESIAN_POINT('',(116.2603997694,-1.85,49.1124533855264));
#203449=CARTESIAN_POINT('',(116.69397029808,-1.85,49.5023464435054));
#203450=CARTESIAN_POINT('',(116.75121327195,-1.85,49.2078583419757));
#203451=CARTESIAN_POINT('Origin',(116.2603997694,-1.85,49.1124533855264));
#203452=CARTESIAN_POINT('',(116.203156795531,-1.85,49.4069414870561));
#203453=CARTESIAN_POINT('',(116.2603997694,-1.85,49.1124533855264));
#203454=CARTESIAN_POINT('Origin',(117.045701373479,-1.35,49.2651013158452));
#203455=CARTESIAN_POINT('',(117.536514876029,-1.35,49.3605062722945));
#203456=CARTESIAN_POINT('',(117.479271902159,-1.35,49.6549943738242));
#203457=CARTESIAN_POINT('',(117.536514876029,-1.35,49.3605062722945));
#203458=CARTESIAN_POINT('',(116.98845839961,-1.35,49.5595894173749));
#203459=CARTESIAN_POINT('',(116.98845839961,-1.35,49.5595894173749));
#203460=CARTESIAN_POINT('',(117.045701373479,-1.35,49.2651013158452));
#203461=CARTESIAN_POINT('',(117.045701373479,-1.35,49.2651013158452));
#203462=CARTESIAN_POINT('',(117.045701373479,-1.35,49.2651013158452));
#203463=CARTESIAN_POINT('Origin',(117.536514876029,-1.35,49.3605062722945));
#203464=CARTESIAN_POINT('',(117.536514876029,-1.85,49.3605062722945));
#203465=CARTESIAN_POINT('',(117.479271902159,-1.85,49.6549943738242));
#203466=CARTESIAN_POINT('',(117.536514876029,-1.85,49.3605062722945));
#203467=CARTESIAN_POINT('',(117.479271902159,-1.35,49.6549943738242));
#203468=CARTESIAN_POINT('',(117.536514876029,-1.35,49.3605062722945));
#203469=CARTESIAN_POINT('Origin',(117.536514876029,-1.85,49.3605062722945));
#203470=CARTESIAN_POINT('',(117.045701373479,-1.85,49.2651013158452));
#203471=CARTESIAN_POINT('',(116.98845839961,-1.85,49.5595894173749));
#203472=CARTESIAN_POINT('',(117.045701373479,-1.85,49.2651013158452));
#203473=CARTESIAN_POINT('',(117.479271902159,-1.85,49.6549943738242));
#203474=CARTESIAN_POINT('',(117.536514876029,-1.85,49.3605062722945));
#203475=CARTESIAN_POINT('Origin',(117.045701373479,-1.85,49.2651013158452));
#203476=CARTESIAN_POINT('',(116.98845839961,-1.85,49.5595894173749));
#203477=CARTESIAN_POINT('',(117.045701373479,-1.85,49.2651013158452));
#203478=CARTESIAN_POINT('Origin',(117.831002977559,-1.35,49.417749246164));
#203479=CARTESIAN_POINT('',(118.321816480108,-1.35,49.5131542026133));
#203480=CARTESIAN_POINT('',(118.264573506239,-1.35,49.807642304143));
#203481=CARTESIAN_POINT('',(118.321816480108,-1.35,49.5131542026133));
#203482=CARTESIAN_POINT('',(117.773760003689,-1.35,49.7122373476937));
#203483=CARTESIAN_POINT('',(117.773760003689,-1.35,49.7122373476937));
#203484=CARTESIAN_POINT('',(117.831002977559,-1.35,49.417749246164));
#203485=CARTESIAN_POINT('',(117.831002977559,-1.35,49.417749246164));
#203486=CARTESIAN_POINT('',(117.831002977559,-1.35,49.417749246164));
#203487=CARTESIAN_POINT('Origin',(118.321816480108,-1.35,49.5131542026133));
#203488=CARTESIAN_POINT('',(118.321816480108,-1.85,49.5131542026133));
#203489=CARTESIAN_POINT('',(118.264573506239,-1.85,49.807642304143));
#203490=CARTESIAN_POINT('',(118.321816480108,-1.85,49.5131542026133));
#203491=CARTESIAN_POINT('',(118.264573506239,-1.35,49.807642304143));
#203492=CARTESIAN_POINT('',(118.321816480108,-1.35,49.5131542026133));
#203493=CARTESIAN_POINT('Origin',(118.321816480108,-1.85,49.5131542026133));
#203494=CARTESIAN_POINT('',(117.831002977559,-1.85,49.417749246164));
#203495=CARTESIAN_POINT('',(117.773760003689,-1.85,49.7122373476937));
#203496=CARTESIAN_POINT('',(117.831002977559,-1.85,49.417749246164));
#203497=CARTESIAN_POINT('',(118.264573506239,-1.85,49.807642304143));
#203498=CARTESIAN_POINT('',(118.321816480108,-1.85,49.5131542026133));
#203499=CARTESIAN_POINT('Origin',(117.831002977559,-1.85,49.417749246164));
#203500=CARTESIAN_POINT('',(117.773760003689,-1.85,49.7122373476937));
#203501=CARTESIAN_POINT('',(117.831002977559,-1.85,49.417749246164));
#203502=CARTESIAN_POINT('Origin',(118.616304581638,-1.35,49.5703971764828));
#203503=CARTESIAN_POINT('',(119.107118084187,-1.35,49.6658021329321));
#203504=CARTESIAN_POINT('',(119.049875110318,-1.35,49.9602902344618));
#203505=CARTESIAN_POINT('',(119.107118084187,-1.35,49.6658021329321));
#203506=CARTESIAN_POINT('',(118.559061607768,-1.35,49.8648852780125));
#203507=CARTESIAN_POINT('',(118.559061607768,-1.35,49.8648852780125));
#203508=CARTESIAN_POINT('',(118.616304581638,-1.35,49.5703971764828));
#203509=CARTESIAN_POINT('',(118.616304581638,-1.35,49.5703971764828));
#203510=CARTESIAN_POINT('',(118.616304581638,-1.35,49.5703971764828));
#203511=CARTESIAN_POINT('Origin',(119.107118084187,-1.35,49.6658021329321));
#203512=CARTESIAN_POINT('',(119.107118084187,-1.85,49.6658021329321));
#203513=CARTESIAN_POINT('',(119.049875110318,-1.85,49.9602902344618));
#203514=CARTESIAN_POINT('',(119.107118084187,-1.85,49.6658021329321));
#203515=CARTESIAN_POINT('',(119.049875110318,-1.35,49.9602902344618));
#203516=CARTESIAN_POINT('',(119.107118084187,-1.35,49.6658021329321));
#203517=CARTESIAN_POINT('Origin',(119.107118084187,-1.85,49.6658021329321));
#203518=CARTESIAN_POINT('',(118.616304581638,-1.85,49.5703971764828));
#203519=CARTESIAN_POINT('',(118.559061607768,-1.85,49.8648852780125));
#203520=CARTESIAN_POINT('',(118.616304581638,-1.85,49.5703971764828));
#203521=CARTESIAN_POINT('',(119.049875110318,-1.85,49.9602902344618));
#203522=CARTESIAN_POINT('',(119.107118084187,-1.85,49.6658021329321));
#203523=CARTESIAN_POINT('Origin',(118.616304581638,-1.85,49.5703971764828));
#203524=CARTESIAN_POINT('',(118.559061607768,-1.85,49.8648852780125));
#203525=CARTESIAN_POINT('',(118.616304581638,-1.85,49.5703971764828));
#203526=CARTESIAN_POINT('Origin',(118.616304581638,-0.549999999999986,49.5703971764828));
#203527=CARTESIAN_POINT('',(119.107118084187,-0.549999999999986,49.6658021329321));
#203528=CARTESIAN_POINT('',(119.049875110318,-0.549999999999986,49.9602902344618));
#203529=CARTESIAN_POINT('',(119.107118084187,-0.549999999999986,49.6658021329321));
#203530=CARTESIAN_POINT('',(118.559061607768,-0.549999999999986,49.8648852780125));
#203531=CARTESIAN_POINT('',(118.559061607768,-0.549999999999986,49.8648852780125));
#203532=CARTESIAN_POINT('',(118.616304581638,-0.549999999999986,49.5703971764828));
#203533=CARTESIAN_POINT('',(118.616304581638,-0.549999999999986,49.5703971764828));
#203534=CARTESIAN_POINT('',(118.616304581638,-0.549999999999986,49.5703971764828));
#203535=CARTESIAN_POINT('Origin',(119.107118084187,-0.549999999999986,49.6658021329321));
#203536=CARTESIAN_POINT('',(119.107118084187,-1.05,49.6658021329321));
#203537=CARTESIAN_POINT('',(119.049875110318,-1.05,49.9602902344618));
#203538=CARTESIAN_POINT('',(119.107118084187,-1.05,49.6658021329321));
#203539=CARTESIAN_POINT('',(119.049875110318,-0.549999999999986,49.9602902344618));
#203540=CARTESIAN_POINT('',(119.107118084187,-0.549999999999986,49.6658021329321));
#203541=CARTESIAN_POINT('Origin',(119.107118084187,-1.05,49.6658021329321));
#203542=CARTESIAN_POINT('',(118.616304581638,-1.05,49.5703971764828));
#203543=CARTESIAN_POINT('',(118.559061607768,-1.05,49.8648852780125));
#203544=CARTESIAN_POINT('',(118.616304581638,-1.05,49.5703971764828));
#203545=CARTESIAN_POINT('',(119.049875110318,-1.05,49.9602902344618));
#203546=CARTESIAN_POINT('',(119.107118084187,-1.05,49.6658021329321));
#203547=CARTESIAN_POINT('Origin',(118.616304581638,-1.05,49.5703971764828));
#203548=CARTESIAN_POINT('',(118.559061607768,-1.05,49.8648852780125));
#203549=CARTESIAN_POINT('',(118.616304581638,-1.05,49.5703971764828));
#203550=CARTESIAN_POINT('Origin',(118.616304581638,0.250000000000015,49.5703971764828));
#203551=CARTESIAN_POINT('',(119.107118084187,0.250000000000015,49.6658021329321));
#203552=CARTESIAN_POINT('',(119.049875110318,0.250000000000015,49.9602902344618));
#203553=CARTESIAN_POINT('',(119.107118084187,0.250000000000015,49.6658021329321));
#203554=CARTESIAN_POINT('',(118.559061607768,0.250000000000015,49.8648852780125));
#203555=CARTESIAN_POINT('',(118.559061607768,0.250000000000015,49.8648852780125));
#203556=CARTESIAN_POINT('',(118.616304581638,0.250000000000015,49.5703971764828));
#203557=CARTESIAN_POINT('',(118.616304581638,0.250000000000015,49.5703971764828));
#203558=CARTESIAN_POINT('',(118.616304581638,0.250000000000015,49.5703971764828));
#203559=CARTESIAN_POINT('Origin',(119.107118084187,0.250000000000015,49.6658021329321));
#203560=CARTESIAN_POINT('',(119.107118084187,-0.249999999999985,49.6658021329321));
#203561=CARTESIAN_POINT('',(119.049875110318,-0.249999999999985,49.9602902344618));
#203562=CARTESIAN_POINT('',(119.107118084187,-0.249999999999985,49.6658021329321));
#203563=CARTESIAN_POINT('',(119.049875110318,0.250000000000015,49.9602902344618));
#203564=CARTESIAN_POINT('',(119.107118084187,0.250000000000015,49.6658021329321));
#203565=CARTESIAN_POINT('Origin',(119.107118084187,-0.249999999999985,49.6658021329321));
#203566=CARTESIAN_POINT('',(118.616304581638,-0.249999999999985,49.5703971764828));
#203567=CARTESIAN_POINT('',(118.559061607768,-0.249999999999985,49.8648852780125));
#203568=CARTESIAN_POINT('',(118.616304581638,-0.249999999999985,49.5703971764828));
#203569=CARTESIAN_POINT('',(119.049875110318,-0.249999999999985,49.9602902344618));
#203570=CARTESIAN_POINT('',(119.107118084187,-0.249999999999985,49.6658021329321));
#203571=CARTESIAN_POINT('Origin',(118.616304581638,-0.249999999999985,49.5703971764828));
#203572=CARTESIAN_POINT('',(118.559061607768,-0.249999999999985,49.8648852780125));
#203573=CARTESIAN_POINT('',(118.616304581638,-0.249999999999985,49.5703971764828));
#203574=CARTESIAN_POINT('Origin',(118.616304581638,1.05,49.5703971764828));
#203575=CARTESIAN_POINT('',(119.107118084187,1.05,49.6658021329321));
#203576=CARTESIAN_POINT('',(119.049875110318,1.05,49.9602902344618));
#203577=CARTESIAN_POINT('',(119.107118084187,1.05,49.6658021329321));
#203578=CARTESIAN_POINT('',(118.559061607768,1.05,49.8648852780125));
#203579=CARTESIAN_POINT('',(118.559061607768,1.05,49.8648852780125));
#203580=CARTESIAN_POINT('',(118.616304581638,1.05,49.5703971764828));
#203581=CARTESIAN_POINT('',(118.616304581638,1.05,49.5703971764828));
#203582=CARTESIAN_POINT('',(118.616304581638,1.05,49.5703971764828));
#203583=CARTESIAN_POINT('Origin',(119.107118084187,1.05,49.6658021329321));
#203584=CARTESIAN_POINT('',(119.107118084187,0.550000000000015,49.6658021329321));
#203585=CARTESIAN_POINT('',(119.049875110318,0.550000000000015,49.9602902344618));
#203586=CARTESIAN_POINT('',(119.107118084187,0.550000000000015,49.6658021329321));
#203587=CARTESIAN_POINT('',(119.049875110318,1.05,49.9602902344618));
#203588=CARTESIAN_POINT('',(119.107118084187,1.05,49.6658021329321));
#203589=CARTESIAN_POINT('Origin',(119.107118084187,0.550000000000015,49.6658021329321));
#203590=CARTESIAN_POINT('',(118.616304581638,0.550000000000015,49.5703971764828));
#203591=CARTESIAN_POINT('',(118.559061607768,0.550000000000015,49.8648852780125));
#203592=CARTESIAN_POINT('',(118.616304581638,0.550000000000015,49.5703971764828));
#203593=CARTESIAN_POINT('',(119.049875110318,0.550000000000015,49.9602902344618));
#203594=CARTESIAN_POINT('',(119.107118084187,0.550000000000015,49.6658021329321));
#203595=CARTESIAN_POINT('Origin',(118.616304581638,0.550000000000015,49.5703971764828));
#203596=CARTESIAN_POINT('',(118.559061607768,0.550000000000015,49.8648852780125));
#203597=CARTESIAN_POINT('',(118.616304581638,0.550000000000015,49.5703971764828));
#203598=CARTESIAN_POINT('Origin',(118.616304581638,1.85,49.5703971764828));
#203599=CARTESIAN_POINT('',(119.107118084187,1.85,49.6658021329321));
#203600=CARTESIAN_POINT('',(119.049875110318,1.85,49.9602902344618));
#203601=CARTESIAN_POINT('',(119.107118084187,1.85,49.6658021329321));
#203602=CARTESIAN_POINT('',(118.559061607768,1.85,49.8648852780125));
#203603=CARTESIAN_POINT('',(118.559061607768,1.85,49.8648852780125));
#203604=CARTESIAN_POINT('',(118.616304581638,1.85,49.5703971764828));
#203605=CARTESIAN_POINT('',(118.616304581638,1.85,49.5703971764828));
#203606=CARTESIAN_POINT('',(118.616304581638,1.85,49.5703971764828));
#203607=CARTESIAN_POINT('Origin',(119.107118084187,1.85,49.6658021329321));
#203608=CARTESIAN_POINT('',(119.107118084187,1.35,49.6658021329321));
#203609=CARTESIAN_POINT('',(119.049875110318,1.35,49.9602902344618));
#203610=CARTESIAN_POINT('',(119.107118084187,1.35,49.6658021329321));
#203611=CARTESIAN_POINT('',(119.049875110318,1.85,49.9602902344618));
#203612=CARTESIAN_POINT('',(119.107118084187,1.85,49.6658021329321));
#203613=CARTESIAN_POINT('Origin',(119.107118084187,1.35,49.6658021329321));
#203614=CARTESIAN_POINT('',(118.616304581638,1.35,49.5703971764828));
#203615=CARTESIAN_POINT('',(118.559061607768,1.35,49.8648852780125));
#203616=CARTESIAN_POINT('',(118.616304581638,1.35,49.5703971764828));
#203617=CARTESIAN_POINT('',(119.049875110318,1.35,49.9602902344618));
#203618=CARTESIAN_POINT('',(119.107118084187,1.35,49.6658021329321));
#203619=CARTESIAN_POINT('Origin',(118.616304581638,1.35,49.5703971764828));
#203620=CARTESIAN_POINT('',(118.559061607768,1.35,49.8648852780125));
#203621=CARTESIAN_POINT('',(118.616304581638,1.35,49.5703971764828));
#203622=CARTESIAN_POINT('Origin',(117.831002977559,1.85,49.417749246164));
#203623=CARTESIAN_POINT('',(118.321816480108,1.85,49.5131542026133));
#203624=CARTESIAN_POINT('',(118.264573506239,1.85,49.807642304143));
#203625=CARTESIAN_POINT('',(118.321816480108,1.85,49.5131542026133));
#203626=CARTESIAN_POINT('',(117.773760003689,1.85,49.7122373476937));
#203627=CARTESIAN_POINT('',(117.773760003689,1.85,49.7122373476937));
#203628=CARTESIAN_POINT('',(117.831002977559,1.85,49.417749246164));
#203629=CARTESIAN_POINT('',(117.831002977559,1.85,49.417749246164));
#203630=CARTESIAN_POINT('',(117.831002977559,1.85,49.417749246164));
#203631=CARTESIAN_POINT('Origin',(118.321816480108,1.85,49.5131542026133));
#203632=CARTESIAN_POINT('',(118.321816480108,1.35,49.5131542026133));
#203633=CARTESIAN_POINT('',(118.264573506239,1.35,49.807642304143));
#203634=CARTESIAN_POINT('',(118.321816480108,1.35,49.5131542026133));
#203635=CARTESIAN_POINT('',(118.264573506239,1.85,49.807642304143));
#203636=CARTESIAN_POINT('',(118.321816480108,1.85,49.5131542026133));
#203637=CARTESIAN_POINT('Origin',(118.321816480108,1.35,49.5131542026133));
#203638=CARTESIAN_POINT('',(117.831002977559,1.35,49.417749246164));
#203639=CARTESIAN_POINT('',(117.773760003689,1.35,49.7122373476937));
#203640=CARTESIAN_POINT('',(117.831002977559,1.35,49.417749246164));
#203641=CARTESIAN_POINT('',(118.264573506239,1.35,49.807642304143));
#203642=CARTESIAN_POINT('',(118.321816480108,1.35,49.5131542026133));
#203643=CARTESIAN_POINT('Origin',(117.831002977559,1.35,49.417749246164));
#203644=CARTESIAN_POINT('',(117.773760003689,1.35,49.7122373476937));
#203645=CARTESIAN_POINT('',(117.831002977559,1.35,49.417749246164));
#203646=CARTESIAN_POINT('Origin',(117.045701373479,1.85,49.2651013158452));
#203647=CARTESIAN_POINT('',(117.536514876029,1.85,49.3605062722945));
#203648=CARTESIAN_POINT('',(117.479271902159,1.85,49.6549943738242));
#203649=CARTESIAN_POINT('',(117.536514876029,1.85,49.3605062722945));
#203650=CARTESIAN_POINT('',(116.98845839961,1.85,49.5595894173749));
#203651=CARTESIAN_POINT('',(116.98845839961,1.85,49.5595894173749));
#203652=CARTESIAN_POINT('',(117.045701373479,1.85,49.2651013158452));
#203653=CARTESIAN_POINT('',(117.045701373479,1.85,49.2651013158452));
#203654=CARTESIAN_POINT('',(117.045701373479,1.85,49.2651013158452));
#203655=CARTESIAN_POINT('Origin',(117.536514876029,1.85,49.3605062722945));
#203656=CARTESIAN_POINT('',(117.536514876029,1.35,49.3605062722945));
#203657=CARTESIAN_POINT('',(117.479271902159,1.35,49.6549943738242));
#203658=CARTESIAN_POINT('',(117.536514876029,1.35,49.3605062722945));
#203659=CARTESIAN_POINT('',(117.479271902159,1.85,49.6549943738242));
#203660=CARTESIAN_POINT('',(117.536514876029,1.85,49.3605062722945));
#203661=CARTESIAN_POINT('Origin',(117.536514876029,1.35,49.3605062722945));
#203662=CARTESIAN_POINT('',(117.045701373479,1.35,49.2651013158452));
#203663=CARTESIAN_POINT('',(116.98845839961,1.35,49.5595894173749));
#203664=CARTESIAN_POINT('',(117.045701373479,1.35,49.2651013158452));
#203665=CARTESIAN_POINT('',(117.479271902159,1.35,49.6549943738242));
#203666=CARTESIAN_POINT('',(117.536514876029,1.35,49.3605062722945));
#203667=CARTESIAN_POINT('Origin',(117.045701373479,1.35,49.2651013158452));
#203668=CARTESIAN_POINT('',(116.98845839961,1.35,49.5595894173749));
#203669=CARTESIAN_POINT('',(117.045701373479,1.35,49.2651013158452));
#203670=CARTESIAN_POINT('Origin',(116.2603997694,1.85,49.1124533855264));
#203671=CARTESIAN_POINT('',(116.75121327195,1.85,49.2078583419757));
#203672=CARTESIAN_POINT('',(116.69397029808,1.85,49.5023464435054));
#203673=CARTESIAN_POINT('',(116.75121327195,1.85,49.2078583419757));
#203674=CARTESIAN_POINT('',(116.203156795531,1.85,49.4069414870561));
#203675=CARTESIAN_POINT('',(116.203156795531,1.85,49.4069414870561));
#203676=CARTESIAN_POINT('',(116.2603997694,1.85,49.1124533855264));
#203677=CARTESIAN_POINT('',(116.2603997694,1.85,49.1124533855264));
#203678=CARTESIAN_POINT('',(116.2603997694,1.85,49.1124533855264));
#203679=CARTESIAN_POINT('Origin',(116.75121327195,1.85,49.2078583419757));
#203680=CARTESIAN_POINT('',(116.75121327195,1.35,49.2078583419757));
#203681=CARTESIAN_POINT('',(116.69397029808,1.35,49.5023464435054));
#203682=CARTESIAN_POINT('',(116.75121327195,1.35,49.2078583419757));
#203683=CARTESIAN_POINT('',(116.69397029808,1.85,49.5023464435054));
#203684=CARTESIAN_POINT('',(116.75121327195,1.85,49.2078583419757));
#203685=CARTESIAN_POINT('Origin',(116.75121327195,1.35,49.2078583419757));
#203686=CARTESIAN_POINT('',(116.2603997694,1.35,49.1124533855264));
#203687=CARTESIAN_POINT('',(116.203156795531,1.35,49.4069414870561));
#203688=CARTESIAN_POINT('',(116.2603997694,1.35,49.1124533855264));
#203689=CARTESIAN_POINT('',(116.69397029808,1.35,49.5023464435054));
#203690=CARTESIAN_POINT('',(116.75121327195,1.35,49.2078583419757));
#203691=CARTESIAN_POINT('Origin',(116.2603997694,1.35,49.1124533855264));
#203692=CARTESIAN_POINT('',(116.203156795531,1.35,49.4069414870561));
#203693=CARTESIAN_POINT('',(116.2603997694,1.35,49.1124533855264));
#203694=CARTESIAN_POINT('Origin',(116.2603997694,1.05,49.1124533855264));
#203695=CARTESIAN_POINT('',(116.75121327195,1.05,49.2078583419757));
#203696=CARTESIAN_POINT('',(116.69397029808,1.05,49.5023464435054));
#203697=CARTESIAN_POINT('',(116.75121327195,1.05,49.2078583419757));
#203698=CARTESIAN_POINT('',(116.203156795531,1.05,49.4069414870561));
#203699=CARTESIAN_POINT('',(116.203156795531,1.05,49.4069414870561));
#203700=CARTESIAN_POINT('',(116.2603997694,1.05,49.1124533855264));
#203701=CARTESIAN_POINT('',(116.2603997694,1.05,49.1124533855264));
#203702=CARTESIAN_POINT('',(116.2603997694,1.05,49.1124533855264));
#203703=CARTESIAN_POINT('Origin',(116.75121327195,1.05,49.2078583419757));
#203704=CARTESIAN_POINT('',(116.75121327195,0.550000000000015,49.2078583419757));
#203705=CARTESIAN_POINT('',(116.69397029808,0.550000000000015,49.5023464435054));
#203706=CARTESIAN_POINT('',(116.75121327195,0.550000000000015,49.2078583419757));
#203707=CARTESIAN_POINT('',(116.69397029808,1.05,49.5023464435054));
#203708=CARTESIAN_POINT('',(116.75121327195,1.05,49.2078583419757));
#203709=CARTESIAN_POINT('Origin',(116.75121327195,0.550000000000015,49.2078583419757));
#203710=CARTESIAN_POINT('',(116.2603997694,0.550000000000015,49.1124533855264));
#203711=CARTESIAN_POINT('',(116.203156795531,0.550000000000015,49.4069414870561));
#203712=CARTESIAN_POINT('',(116.2603997694,0.550000000000015,49.1124533855264));
#203713=CARTESIAN_POINT('',(116.69397029808,0.550000000000015,49.5023464435054));
#203714=CARTESIAN_POINT('',(116.75121327195,0.550000000000015,49.2078583419757));
#203715=CARTESIAN_POINT('Origin',(116.2603997694,0.550000000000015,49.1124533855264));
#203716=CARTESIAN_POINT('',(116.203156795531,0.550000000000015,49.4069414870561));
#203717=CARTESIAN_POINT('',(116.2603997694,0.550000000000015,49.1124533855264));
#203718=CARTESIAN_POINT('Origin',(116.2603997694,0.250000000000015,49.1124533855264));
#203719=CARTESIAN_POINT('',(116.75121327195,0.250000000000015,49.2078583419757));
#203720=CARTESIAN_POINT('',(116.69397029808,0.250000000000015,49.5023464435054));
#203721=CARTESIAN_POINT('',(116.75121327195,0.250000000000015,49.2078583419757));
#203722=CARTESIAN_POINT('',(116.203156795531,0.250000000000015,49.4069414870561));
#203723=CARTESIAN_POINT('',(116.203156795531,0.250000000000015,49.4069414870561));
#203724=CARTESIAN_POINT('',(116.2603997694,0.250000000000015,49.1124533855264));
#203725=CARTESIAN_POINT('',(116.2603997694,0.250000000000015,49.1124533855264));
#203726=CARTESIAN_POINT('',(116.2603997694,0.250000000000015,49.1124533855264));
#203727=CARTESIAN_POINT('Origin',(116.75121327195,0.250000000000015,49.2078583419757));
#203728=CARTESIAN_POINT('',(116.75121327195,-0.249999999999985,49.2078583419757));
#203729=CARTESIAN_POINT('',(116.69397029808,-0.249999999999985,49.5023464435054));
#203730=CARTESIAN_POINT('',(116.75121327195,-0.249999999999985,49.2078583419757));
#203731=CARTESIAN_POINT('',(116.69397029808,0.250000000000015,49.5023464435054));
#203732=CARTESIAN_POINT('',(116.75121327195,0.250000000000015,49.2078583419757));
#203733=CARTESIAN_POINT('Origin',(116.75121327195,-0.249999999999985,49.2078583419757));
#203734=CARTESIAN_POINT('',(116.2603997694,-0.249999999999985,49.1124533855264));
#203735=CARTESIAN_POINT('',(116.203156795531,-0.249999999999985,49.4069414870561));
#203736=CARTESIAN_POINT('',(116.2603997694,-0.249999999999985,49.1124533855264));
#203737=CARTESIAN_POINT('',(116.69397029808,-0.249999999999985,49.5023464435054));
#203738=CARTESIAN_POINT('',(116.75121327195,-0.249999999999985,49.2078583419757));
#203739=CARTESIAN_POINT('Origin',(116.2603997694,-0.249999999999985,49.1124533855264));
#203740=CARTESIAN_POINT('',(116.203156795531,-0.249999999999985,49.4069414870561));
#203741=CARTESIAN_POINT('',(116.2603997694,-0.249999999999985,49.1124533855264));
#203742=CARTESIAN_POINT('Origin',(116.2603997694,-0.549999999999986,49.1124533855264));
#203743=CARTESIAN_POINT('',(116.75121327195,-0.549999999999986,49.2078583419757));
#203744=CARTESIAN_POINT('',(116.69397029808,-0.549999999999986,49.5023464435054));
#203745=CARTESIAN_POINT('',(116.75121327195,-0.549999999999986,49.2078583419757));
#203746=CARTESIAN_POINT('',(116.203156795531,-0.549999999999986,49.4069414870561));
#203747=CARTESIAN_POINT('',(116.203156795531,-0.549999999999986,49.4069414870561));
#203748=CARTESIAN_POINT('',(116.2603997694,-0.549999999999986,49.1124533855264));
#203749=CARTESIAN_POINT('',(116.2603997694,-0.549999999999986,49.1124533855264));
#203750=CARTESIAN_POINT('',(116.2603997694,-0.549999999999986,49.1124533855264));
#203751=CARTESIAN_POINT('Origin',(116.75121327195,-0.549999999999986,49.2078583419757));
#203752=CARTESIAN_POINT('',(116.75121327195,-1.05,49.2078583419757));
#203753=CARTESIAN_POINT('',(116.69397029808,-1.05,49.5023464435054));
#203754=CARTESIAN_POINT('',(116.75121327195,-1.05,49.2078583419757));
#203755=CARTESIAN_POINT('',(116.69397029808,-0.549999999999986,49.5023464435054));
#203756=CARTESIAN_POINT('',(116.75121327195,-0.549999999999986,49.2078583419757));
#203757=CARTESIAN_POINT('Origin',(116.75121327195,-1.05,49.2078583419757));
#203758=CARTESIAN_POINT('',(116.2603997694,-1.05,49.1124533855264));
#203759=CARTESIAN_POINT('',(116.203156795531,-1.05,49.4069414870561));
#203760=CARTESIAN_POINT('',(116.2603997694,-1.05,49.1124533855264));
#203761=CARTESIAN_POINT('',(116.69397029808,-1.05,49.5023464435054));
#203762=CARTESIAN_POINT('',(116.75121327195,-1.05,49.2078583419757));
#203763=CARTESIAN_POINT('Origin',(116.2603997694,-1.05,49.1124533855264));
#203764=CARTESIAN_POINT('',(116.203156795531,-1.05,49.4069414870561));
#203765=CARTESIAN_POINT('',(116.2603997694,-1.05,49.1124533855264));
#203766=CARTESIAN_POINT('Origin',(117.045701373479,-0.549999999999986,49.2651013158452));
#203767=CARTESIAN_POINT('',(117.536514876029,-0.549999999999986,49.3605062722945));
#203768=CARTESIAN_POINT('',(117.479271902159,-0.549999999999986,49.6549943738242));
#203769=CARTESIAN_POINT('',(117.536514876029,-0.549999999999986,49.3605062722945));
#203770=CARTESIAN_POINT('',(116.98845839961,-0.549999999999986,49.5595894173749));
#203771=CARTESIAN_POINT('',(116.98845839961,-0.549999999999986,49.5595894173749));
#203772=CARTESIAN_POINT('',(117.045701373479,-0.549999999999986,49.2651013158452));
#203773=CARTESIAN_POINT('',(117.045701373479,-0.549999999999986,49.2651013158452));
#203774=CARTESIAN_POINT('',(117.045701373479,-0.549999999999986,49.2651013158452));
#203775=CARTESIAN_POINT('Origin',(117.536514876029,-0.549999999999986,49.3605062722945));
#203776=CARTESIAN_POINT('',(117.536514876029,-1.05,49.3605062722945));
#203777=CARTESIAN_POINT('',(117.479271902159,-1.05,49.6549943738242));
#203778=CARTESIAN_POINT('',(117.536514876029,-1.05,49.3605062722945));
#203779=CARTESIAN_POINT('',(117.479271902159,-0.549999999999986,49.6549943738242));
#203780=CARTESIAN_POINT('',(117.536514876029,-0.549999999999986,49.3605062722945));
#203781=CARTESIAN_POINT('Origin',(117.536514876029,-1.05,49.3605062722945));
#203782=CARTESIAN_POINT('',(117.045701373479,-1.05,49.2651013158452));
#203783=CARTESIAN_POINT('',(116.98845839961,-1.05,49.5595894173749));
#203784=CARTESIAN_POINT('',(117.045701373479,-1.05,49.2651013158452));
#203785=CARTESIAN_POINT('',(117.479271902159,-1.05,49.6549943738242));
#203786=CARTESIAN_POINT('',(117.536514876029,-1.05,49.3605062722945));
#203787=CARTESIAN_POINT('Origin',(117.045701373479,-1.05,49.2651013158452));
#203788=CARTESIAN_POINT('',(116.98845839961,-1.05,49.5595894173749));
#203789=CARTESIAN_POINT('',(117.045701373479,-1.05,49.2651013158452));
#203790=CARTESIAN_POINT('Origin',(117.831002977559,-0.549999999999986,49.417749246164));
#203791=CARTESIAN_POINT('',(118.321816480108,-0.549999999999986,49.5131542026133));
#203792=CARTESIAN_POINT('',(118.264573506239,-0.549999999999986,49.807642304143));
#203793=CARTESIAN_POINT('',(118.321816480108,-0.549999999999986,49.5131542026133));
#203794=CARTESIAN_POINT('',(117.773760003689,-0.549999999999986,49.7122373476937));
#203795=CARTESIAN_POINT('',(117.773760003689,-0.549999999999986,49.7122373476937));
#203796=CARTESIAN_POINT('',(117.831002977559,-0.549999999999986,49.417749246164));
#203797=CARTESIAN_POINT('',(117.831002977559,-0.549999999999986,49.417749246164));
#203798=CARTESIAN_POINT('',(117.831002977559,-0.549999999999986,49.417749246164));
#203799=CARTESIAN_POINT('Origin',(118.321816480108,-0.549999999999986,49.5131542026133));
#203800=CARTESIAN_POINT('',(118.321816480108,-1.05,49.5131542026133));
#203801=CARTESIAN_POINT('',(118.264573506239,-1.05,49.807642304143));
#203802=CARTESIAN_POINT('',(118.321816480108,-1.05,49.5131542026133));
#203803=CARTESIAN_POINT('',(118.264573506239,-0.549999999999986,49.807642304143));
#203804=CARTESIAN_POINT('',(118.321816480108,-0.549999999999986,49.5131542026133));
#203805=CARTESIAN_POINT('Origin',(118.321816480108,-1.05,49.5131542026133));
#203806=CARTESIAN_POINT('',(117.831002977559,-1.05,49.417749246164));
#203807=CARTESIAN_POINT('',(117.773760003689,-1.05,49.7122373476937));
#203808=CARTESIAN_POINT('',(117.831002977559,-1.05,49.417749246164));
#203809=CARTESIAN_POINT('',(118.264573506239,-1.05,49.807642304143));
#203810=CARTESIAN_POINT('',(118.321816480108,-1.05,49.5131542026133));
#203811=CARTESIAN_POINT('Origin',(117.831002977559,-1.05,49.417749246164));
#203812=CARTESIAN_POINT('',(117.773760003689,-1.05,49.7122373476937));
#203813=CARTESIAN_POINT('',(117.831002977559,-1.05,49.417749246164));
#203814=CARTESIAN_POINT('Origin',(117.831002977559,0.250000000000015,49.417749246164));
#203815=CARTESIAN_POINT('',(118.321816480108,0.250000000000015,49.5131542026133));
#203816=CARTESIAN_POINT('',(118.264573506239,0.250000000000015,49.807642304143));
#203817=CARTESIAN_POINT('',(118.321816480108,0.250000000000015,49.5131542026133));
#203818=CARTESIAN_POINT('',(117.773760003689,0.250000000000015,49.7122373476937));
#203819=CARTESIAN_POINT('',(117.773760003689,0.250000000000015,49.7122373476937));
#203820=CARTESIAN_POINT('',(117.831002977559,0.250000000000015,49.417749246164));
#203821=CARTESIAN_POINT('',(117.831002977559,0.250000000000015,49.417749246164));
#203822=CARTESIAN_POINT('',(117.831002977559,0.250000000000015,49.417749246164));
#203823=CARTESIAN_POINT('Origin',(118.321816480108,0.250000000000015,49.5131542026133));
#203824=CARTESIAN_POINT('',(118.321816480108,-0.249999999999985,49.5131542026133));
#203825=CARTESIAN_POINT('',(118.264573506239,-0.249999999999985,49.807642304143));
#203826=CARTESIAN_POINT('',(118.321816480108,-0.249999999999985,49.5131542026133));
#203827=CARTESIAN_POINT('',(118.264573506239,0.250000000000015,49.807642304143));
#203828=CARTESIAN_POINT('',(118.321816480108,0.250000000000015,49.5131542026133));
#203829=CARTESIAN_POINT('Origin',(118.321816480108,-0.249999999999985,49.5131542026133));
#203830=CARTESIAN_POINT('',(117.831002977559,-0.249999999999985,49.417749246164));
#203831=CARTESIAN_POINT('',(117.773760003689,-0.249999999999985,49.7122373476937));
#203832=CARTESIAN_POINT('',(117.831002977559,-0.249999999999985,49.417749246164));
#203833=CARTESIAN_POINT('',(118.264573506239,-0.249999999999985,49.807642304143));
#203834=CARTESIAN_POINT('',(118.321816480108,-0.249999999999985,49.5131542026133));
#203835=CARTESIAN_POINT('Origin',(117.831002977559,-0.249999999999985,49.417749246164));
#203836=CARTESIAN_POINT('',(117.773760003689,-0.249999999999985,49.7122373476937));
#203837=CARTESIAN_POINT('',(117.831002977559,-0.249999999999985,49.417749246164));
#203838=CARTESIAN_POINT('Origin',(117.831002977559,1.05,49.417749246164));
#203839=CARTESIAN_POINT('',(118.321816480108,1.05,49.5131542026133));
#203840=CARTESIAN_POINT('',(118.264573506239,1.05,49.807642304143));
#203841=CARTESIAN_POINT('',(118.321816480108,1.05,49.5131542026133));
#203842=CARTESIAN_POINT('',(117.773760003689,1.05,49.7122373476937));
#203843=CARTESIAN_POINT('',(117.773760003689,1.05,49.7122373476937));
#203844=CARTESIAN_POINT('',(117.831002977559,1.05,49.417749246164));
#203845=CARTESIAN_POINT('',(117.831002977559,1.05,49.417749246164));
#203846=CARTESIAN_POINT('',(117.831002977559,1.05,49.417749246164));
#203847=CARTESIAN_POINT('Origin',(118.321816480108,1.05,49.5131542026133));
#203848=CARTESIAN_POINT('',(118.321816480108,0.550000000000015,49.5131542026133));
#203849=CARTESIAN_POINT('',(118.264573506239,0.550000000000015,49.807642304143));
#203850=CARTESIAN_POINT('',(118.321816480108,0.550000000000015,49.5131542026133));
#203851=CARTESIAN_POINT('',(118.264573506239,1.05,49.807642304143));
#203852=CARTESIAN_POINT('',(118.321816480108,1.05,49.5131542026133));
#203853=CARTESIAN_POINT('Origin',(118.321816480108,0.550000000000015,49.5131542026133));
#203854=CARTESIAN_POINT('',(117.831002977559,0.550000000000015,49.417749246164));
#203855=CARTESIAN_POINT('',(117.773760003689,0.550000000000015,49.7122373476937));
#203856=CARTESIAN_POINT('',(117.831002977559,0.550000000000015,49.417749246164));
#203857=CARTESIAN_POINT('',(118.264573506239,0.550000000000015,49.807642304143));
#203858=CARTESIAN_POINT('',(118.321816480108,0.550000000000015,49.5131542026133));
#203859=CARTESIAN_POINT('Origin',(117.831002977559,0.550000000000015,49.417749246164));
#203860=CARTESIAN_POINT('',(117.773760003689,0.550000000000015,49.7122373476937));
#203861=CARTESIAN_POINT('',(117.831002977559,0.550000000000015,49.417749246164));
#203862=CARTESIAN_POINT('Origin',(117.045701373479,1.05,49.2651013158452));
#203863=CARTESIAN_POINT('',(117.536514876029,1.05,49.3605062722945));
#203864=CARTESIAN_POINT('',(117.479271902159,1.05,49.6549943738242));
#203865=CARTESIAN_POINT('',(117.536514876029,1.05,49.3605062722945));
#203866=CARTESIAN_POINT('',(116.98845839961,1.05,49.5595894173749));
#203867=CARTESIAN_POINT('',(116.98845839961,1.05,49.5595894173749));
#203868=CARTESIAN_POINT('',(117.045701373479,1.05,49.2651013158452));
#203869=CARTESIAN_POINT('',(117.045701373479,1.05,49.2651013158452));
#203870=CARTESIAN_POINT('',(117.045701373479,1.05,49.2651013158452));
#203871=CARTESIAN_POINT('Origin',(117.536514876029,1.05,49.3605062722945));
#203872=CARTESIAN_POINT('',(117.536514876029,0.550000000000015,49.3605062722945));
#203873=CARTESIAN_POINT('',(117.479271902159,0.550000000000015,49.6549943738242));
#203874=CARTESIAN_POINT('',(117.536514876029,0.550000000000015,49.3605062722945));
#203875=CARTESIAN_POINT('',(117.479271902159,1.05,49.6549943738242));
#203876=CARTESIAN_POINT('',(117.536514876029,1.05,49.3605062722945));
#203877=CARTESIAN_POINT('Origin',(117.536514876029,0.550000000000015,49.3605062722945));
#203878=CARTESIAN_POINT('',(117.045701373479,0.550000000000015,49.2651013158452));
#203879=CARTESIAN_POINT('',(116.98845839961,0.550000000000015,49.5595894173749));
#203880=CARTESIAN_POINT('',(117.045701373479,0.550000000000015,49.2651013158452));
#203881=CARTESIAN_POINT('',(117.479271902159,0.550000000000015,49.6549943738242));
#203882=CARTESIAN_POINT('',(117.536514876029,0.550000000000015,49.3605062722945));
#203883=CARTESIAN_POINT('Origin',(117.045701373479,0.550000000000015,49.2651013158452));
#203884=CARTESIAN_POINT('',(116.98845839961,0.550000000000015,49.5595894173749));
#203885=CARTESIAN_POINT('',(117.045701373479,0.550000000000015,49.2651013158452));
#203886=CARTESIAN_POINT('Origin',(117.329270107334,1.45439216225896E-14,
49.11647839305));
#203887=CARTESIAN_POINT('Origin',(117.233865150885,1.45439216225896E-14,
49.6072918955995));
#203888=CARTESIAN_POINT('',(116.98845839961,0.250000000000015,49.5595894173749));
#203889=CARTESIAN_POINT('',(117.479271902159,0.250000000000015,49.6549943738242));
#203890=CARTESIAN_POINT('',(116.98845839961,0.250000000000015,49.5595894173749));
#203891=CARTESIAN_POINT('',(117.479271902159,-0.249999999999985,49.6549943738242));
#203892=CARTESIAN_POINT('',(117.479271902159,0.250000000000015,49.6549943738242));
#203893=CARTESIAN_POINT('',(116.98845839961,-0.249999999999985,49.5595894173749));
#203894=CARTESIAN_POINT('',(117.479271902159,-0.249999999999985,49.6549943738242));
#203895=CARTESIAN_POINT('',(116.98845839961,-0.249999999999985,49.5595894173749));
#203896=CARTESIAN_POINT('Origin',(117.045701373479,0.250000000000015,49.2651013158452));
#203897=CARTESIAN_POINT('',(117.536514876029,0.250000000000015,49.3605062722945));
#203898=CARTESIAN_POINT('',(117.536514876029,0.250000000000015,49.3605062722945));
#203899=CARTESIAN_POINT('',(117.045701373479,0.250000000000015,49.2651013158452));
#203900=CARTESIAN_POINT('',(117.045701373479,0.250000000000015,49.2651013158452));
#203901=CARTESIAN_POINT('',(117.045701373479,0.250000000000015,49.2651013158452));
#203902=CARTESIAN_POINT('Origin',(117.536514876029,0.250000000000015,49.3605062722945));
#203903=CARTESIAN_POINT('',(117.536514876029,-0.249999999999985,49.3605062722945));
#203904=CARTESIAN_POINT('',(117.536514876029,-0.249999999999985,49.3605062722945));
#203905=CARTESIAN_POINT('',(117.536514876029,0.250000000000015,49.3605062722945));
#203906=CARTESIAN_POINT('Origin',(117.536514876029,-0.249999999999985,49.3605062722945));
#203907=CARTESIAN_POINT('',(117.045701373479,-0.249999999999985,49.2651013158452));
#203908=CARTESIAN_POINT('',(117.045701373479,-0.249999999999985,49.2651013158452));
#203909=CARTESIAN_POINT('',(117.536514876029,-0.249999999999985,49.3605062722945));
#203910=CARTESIAN_POINT('Origin',(117.045701373479,-0.249999999999985,49.2651013158452));
#203911=CARTESIAN_POINT('',(117.045701373479,-0.249999999999985,49.2651013158452));
#203912=CARTESIAN_POINT('Origin',(117.291108124754,1.45439216225896E-14,
49.3128037940698));
#203913=CARTESIAN_POINT('Origin',(117.386513081203,1.45439216225896E-14,
48.8219902915203));
#203914=CARTESIAN_POINT('Origin',(130.840764973451,4.75,59.7907234006794));
#203915=CARTESIAN_POINT('',(106.028205189486,4.75,54.9676262909074));
#203916=CARTESIAN_POINT('Origin',(130.840764973451,4.75,59.7907234006794));
#203917=CARTESIAN_POINT('',(125.940727510725,4.75,58.8382478507959));
#203918=CARTESIAN_POINT('Origin',(130.554550104103,-4.75,61.2631639083279));
#203919=CARTESIAN_POINT('',(105.741990320138,4.75,56.4400667985559));
#203920=CARTESIAN_POINT('Origin',(130.554550104103,-4.75,61.2631639083279));
#203921=CARTESIAN_POINT('',(125.654512641377,4.75,60.3106883584444));
#203922=CARTESIAN_POINT('Origin',(130.697657538777,4.75,60.5269436545036));
#203923=CARTESIAN_POINT('Origin',(130.697657538777,4.75,60.5269436545036));
#203924=CARTESIAN_POINT('Origin',(120.198385200308,15.3,59.2501193272487));
#203925=CARTESIAN_POINT('',(110.872928651868,10.30824912388,57.4374251547129));
#203926=CARTESIAN_POINT('Origin',(120.198385200308,15.3,59.2501193272487));
#203927=CARTESIAN_POINT('',(110.872928651868,-9.97697348898999,57.4374251547129));
#203928=CARTESIAN_POINT('Origin',(111.159143521215,15.3,55.9649846470644));
#203929=CARTESIAN_POINT('',(111.159143521215,10.30824912388,55.9649846470644));
#203930=CARTESIAN_POINT('Origin',(111.159143521215,15.3,55.9649846470644));
#203931=CARTESIAN_POINT('',(111.159143521215,-9.97697348898999,55.9649846470644));
#203932=CARTESIAN_POINT('Origin',(111.016036086541,15.3,56.7012049008886));
#203933=CARTESIAN_POINT('Origin',(111.016036086541,15.3,56.7012049008886));
#203934=CARTESIAN_POINT('Origin',(114.581607361595,1.45439216225896E-14,
63.2519072664759));
#203935=CARTESIAN_POINT('',(123.565639834831,1.45439216225896E-14,64.998234990541));
#203936=CARTESIAN_POINT('Origin',(114.581607361595,1.45439216225896E-14,
63.2519072664759));
#203937=CARTESIAN_POINT('Origin',(116.959178380441,1.45439216225896E-14,
51.0204257716897));
#203938=CARTESIAN_POINT('',(114.699588927787,0.200000000000015,66.3135202594736));
#203939=CARTESIAN_POINT('',(114.205996738637,0.200000000000015,66.2324103349957));
#203940=CARTESIAN_POINT('Origin',(116.959178380441,0.200000000000015,51.0204257716897));
#203941=CARTESIAN_POINT('',(114.702370237086,0.700000000000015,66.2992117349507));
#203942=CARTESIAN_POINT('Origin',(117.64631728401,1.45439216225896E-14,
51.1539927107186));
#203943=CARTESIAN_POINT('',(114.208775425237,0.700000000000015,66.2181153030243));
#203944=CARTESIAN_POINT('Origin',(116.959178380441,0.700000000000015,51.0204257716897));
#203945=CARTESIAN_POINT('Origin',(117.155503781461,1.45439216225896E-14,
51.0585877542694));
#203946=CARTESIAN_POINT('Origin',(114.720689788746,0.200000000000015,63.5845573505853));
#203947=CARTESIAN_POINT('',(114.642283596451,0.200000000000015,66.6083291607529));
#203948=CARTESIAN_POINT('',(114.699588927787,0.200000000000015,66.3135202594736));
#203949=CARTESIAN_POINT('',(114.148744365364,0.200000000000015,66.5269467920214));
#203950=CARTESIAN_POINT('',(114.205996738637,0.200000000000015,66.2324103349957));
#203951=CARTESIAN_POINT('Origin',(116.959178380441,0.200000000000015,51.0204257716897));
#203952=CARTESIAN_POINT('Origin',(115.211503291295,0.200000000000015,63.6799623070345));
#203953=CARTESIAN_POINT('',(114.64501180044,0.700000000000015,66.5942938380051));
#203954=CARTESIAN_POINT('',(114.702370237086,0.700000000000015,66.2992117349507));
#203955=CARTESIAN_POINT('Origin',(117.64631728401,1.45439216225896E-14,
51.1539927107186));
#203956=CARTESIAN_POINT('Origin',(115.211503291295,0.700000000000015,63.6799623070345));
#203957=CARTESIAN_POINT('',(114.151470093902,0.700000000000015,66.5129242043036));
#203958=CARTESIAN_POINT('',(114.208775425237,0.700000000000015,66.2181153030243));
#203959=CARTESIAN_POINT('Origin',(116.959178380441,0.700000000000015,51.0204257716897));
#203960=CARTESIAN_POINT('Origin',(114.720689788746,0.700000000000015,63.5845573505853));
#203961=CARTESIAN_POINT('Origin',(117.155503781461,1.45439216225896E-14,
51.0585877542694));
#203962=CARTESIAN_POINT('Origin',(116.959178380441,1.45439216225896E-14,
51.0204257716897));
#203963=CARTESIAN_POINT('',(123.604414184892,1.45439216225896E-14,65.3113870623167));
#203964=CARTESIAN_POINT('Origin',(114.524364387726,1.45439216225896E-14,
63.5463953680056));
#203965=CARTESIAN_POINT('Origin',(114.524364387726,1.45439216225896E-14,
63.5463953680056));
#203966=CARTESIAN_POINT('',(0.,0.,0.));
#203967=CARTESIAN_POINT('Origin',(-45.8894114130409,-83.3180213346267,69.5522455184007));
#203968=CARTESIAN_POINT('',(-50.2096235848678,-73.8447192590796,73.4662010349383));
#203969=CARTESIAN_POINT('',(-49.8038356726598,-73.8447192590796,73.4662010349383));
#203970=CARTESIAN_POINT('',(-45.8894114130409,-73.8447192590796,73.4662010349383));
#203971=CARTESIAN_POINT('',(-48.3958698180353,-73.8447192590796,73.4662010349383));
#203972=CARTESIAN_POINT('Ctrl Pts',(-48.3958698180353,-73.8447192590796,
73.4662010349383));
#203973=CARTESIAN_POINT('Ctrl Pts',(-48.4037688023958,-73.7386706426075,
73.2095219351658));
#203974=CARTESIAN_POINT('Ctrl Pts',(-48.4116574949273,-73.6430539000291,
72.9485323067095));
#203975=CARTESIAN_POINT('Ctrl Pts',(-48.4339260978028,-73.4009224543471,
72.1939151829407));
#203976=CARTESIAN_POINT('Ctrl Pts',(-48.4481645682176,-73.2808293376766,
71.6928179235221));
#203977=CARTESIAN_POINT('Ctrl Pts',(-48.480466899021,-73.0972451440741,
70.5549159518891));
#203978=CARTESIAN_POINT('Ctrl Pts',(-48.4985953623062,-73.0546578172561,
69.9168948451602));
#203979=CARTESIAN_POINT('Ctrl Pts',(-48.5346718023404,-73.0884937885025,
68.6477279521232));
#203980=CARTESIAN_POINT('Ctrl Pts',(-48.5522008894746,-73.1636417714324,
68.0192859017049));
#203981=CARTESIAN_POINT('Ctrl Pts',(-48.5881875157042,-73.4338516390347,
66.7600280206718));
#203982=CARTESIAN_POINT('Ctrl Pts',(-48.6067347220618,-73.632875106913,
66.1330034080448));
#203983=CARTESIAN_POINT('Ctrl Pts',(-48.657339605336,-74.331064994807,64.4968207509486));
#203984=CARTESIAN_POINT('Ctrl Pts',(-48.6880625258242,-74.9383023010144,
63.5436661186597));
#203985=CARTESIAN_POINT('Ctrl Pts',(-48.7390155039672,-76.1391472861404,
62.2049346832462));
#203986=CARTESIAN_POINT('Ctrl Pts',(-48.7583174976583,-76.6390544266697,
61.747719387351));
#203987=CARTESIAN_POINT('Ctrl Pts',(-48.7960590212527,-77.7208277256431,
60.938919054492));
#203988=CARTESIAN_POINT('Ctrl Pts',(-48.8147908333194,-78.2999318592946,
60.5891687634112));
#203989=CARTESIAN_POINT('Ctrl Pts',(-48.8432065712902,-79.2059868334308,
60.1574727831644));
#203990=CARTESIAN_POINT('Ctrl Pts',(-48.8525662532641,-79.5094106761401,
60.0304249838887));
#203991=CARTESIAN_POINT('Ctrl Pts',(-48.8912166329455,-80.7871613627979,
59.5662775472869));
#203992=CARTESIAN_POINT('Ctrl Pts',(-48.9194279440347,-81.8034663869601,
59.362498805665));
#203993=CARTESIAN_POINT('Ctrl Pts',(-48.9579250197248,-83.1622898710032,
59.2981281043926));
#203994=CARTESIAN_POINT('Ctrl Pts',(-48.9673076225165,-83.4921415542527,
59.2984239272769));
#203995=CARTESIAN_POINT('Ctrl Pts',(-49.0066694377159,-84.8746715504436,
59.3664025361002));
#203996=CARTESIAN_POINT('Ctrl Pts',(-49.0355301671101,-85.9136649961914,
59.5804252807785));
#203997=CARTESIAN_POINT('Ctrl Pts',(-49.0821868355881,-87.4577419933632,
60.1566345648574));
#203998=CARTESIAN_POINT('Ctrl Pts',(-49.0991802722567,-87.9947530123903,
60.412060635265));
#203999=CARTESIAN_POINT('Ctrl Pts',(-49.130122341021,-88.9451920275598,
60.9699355087346));
#204000=CARTESIAN_POINT('Ctrl Pts',(-49.1441985526236,-89.3639849856817,
61.2596329916114));
#204001=CARTESIAN_POINT('Ctrl Pts',(-49.1763003559444,-90.2547807826329,
61.9793192667773));
#204002=CARTESIAN_POINT('Ctrl Pts',(-49.1943953113045,-90.7116591687776,
62.4246969029591));
#204003=CARTESIAN_POINT('Ctrl Pts',(-49.2304152840414,-91.5332756733942,
63.3902299748733));
#204004=CARTESIAN_POINT('Ctrl Pts',(-49.2479248411482,-91.8970273447589,
63.9076464520963));
#204005=CARTESIAN_POINT('Ctrl Pts',(-49.2838818041742,-92.5368653667999,
65.0239821634796));
#204006=CARTESIAN_POINT('Ctrl Pts',(-49.3024121914913,-92.8075370872142,
65.6226997428383));
#204007=CARTESIAN_POINT('Ctrl Pts',(-49.3595038029608,-93.4554727643574,
67.5222243619057));
#204008=CARTESIAN_POINT('Ctrl Pts',(-49.3964227073141,-93.6345282408168,
68.8750549678309));
#204009=CARTESIAN_POINT('Ctrl Pts',(-49.473309124989,-93.457508738034,71.5719325676014));
#204010=CARTESIAN_POINT('Ctrl Pts',(-49.5102216656477,-93.1032506221796,
72.8895546941323));
#204011=CARTESIAN_POINT('Ctrl Pts',(-49.5748954774791,-92.0944299133281,
74.9269751780849));
#204012=CARTESIAN_POINT('Ctrl Pts',(-49.6003951487874,-91.5755097026235,
75.6944736760051));
#204013=CARTESIAN_POINT('Ctrl Pts',(-49.6510179783252,-90.3743525456944,
77.0386154460731));
#204014=CARTESIAN_POINT('Ctrl Pts',(-49.6762791930195,-89.705601088901,
77.6167589418837));
#204015=CARTESIAN_POINT('Ctrl Pts',(-49.7143859714278,-88.5696143825758,
78.3678616677063));
#204016=CARTESIAN_POINT('Ctrl Pts',(-49.727738082698,-88.1497797203329,
78.6047827076002));
#204017=CARTESIAN_POINT('Ctrl Pts',(-49.7606212091936,-87.0916211277151,
79.1072676497953));
#204018=CARTESIAN_POINT('Ctrl Pts',(-49.7803096541967,-86.4401008290713,
79.3395385943935));
#204019=CARTESIAN_POINT('Ctrl Pts',(-49.8093097839274,-85.4456603226875,
79.5845625524906));
#204020=CARTESIAN_POINT('Ctrl Pts',(-49.8186505287261,-85.1173873690851,
79.6486070096269));
#204021=CARTESIAN_POINT('Ctrl Pts',(-49.8457240773238,-84.1567284833155,
79.7876783315113));
#204022=CARTESIAN_POINT('Ctrl Pts',(-49.8634779845325,-83.5197662041813,
79.8200011829918));
#204023=CARTESIAN_POINT('Ctrl Pts',(-49.8956682408467,-82.3857593300351,
79.7719330243677));
#204024=CARTESIAN_POINT('Ctrl Pts',(-49.9099239632542,-81.8897876487362,
79.7144930808433));
#204025=CARTESIAN_POINT('Ctrl Pts',(-49.9387558076438,-80.8833860201483,
79.522781806287));
#204026=CARTESIAN_POINT('Ctrl Pts',(-49.9532988892753,-80.3751380966072,
79.384767434848));
#204027=CARTESIAN_POINT('Ctrl Pts',(-49.9859711911988,-79.2764357760924,
78.9935480759183));
#204028=CARTESIAN_POINT('Ctrl Pts',(-50.0041557488463,-78.6946047619587,
78.7226660461564));
#204029=CARTESIAN_POINT('Ctrl Pts',(-50.0403294878792,-77.5960381700283,
78.07992568427));
#204030=CARTESIAN_POINT('Ctrl Pts',(-50.057894567962,-77.0809299480628,
77.7107451120727));
#204031=CARTESIAN_POINT('Ctrl Pts',(-50.0939331145918,-76.1062593244605,
76.8656229924851));
#204032=CARTESIAN_POINT('Ctrl Pts',(-50.1125077195411,-75.6520038235377,
76.3879723904082));
#204033=CARTESIAN_POINT('Ctrl Pts',(-50.1577532611068,-74.67166569896,75.1355452763787));
#204034=CARTESIAN_POINT('Ctrl Pts',(-50.1834334662541,-74.2002175935722,
74.3266459469391));
#204035=CARTESIAN_POINT('Ctrl Pts',(-50.2096235848678,-73.8447192590796,
73.4662010349383));
#204036=CARTESIAN_POINT('',(-47.5675364832709,-73.8447192590796,73.4662010349383));
#204037=CARTESIAN_POINT('',(-45.8894114130409,-73.8447192590796,73.4662010349383));
#204038=CARTESIAN_POINT('',(-47.5675364832709,-79.4040658180891,60.0789434428536));
#204039=CARTESIAN_POINT('Origin',(-47.5675364832709,-83.3180213346267,69.5522455184007));
#204040=CARTESIAN_POINT('Origin',(-47.5675364832709,-83.3180213346267,69.5522455184007));
#204041=CARTESIAN_POINT('',(-47.8635970591063,-89.6396660823375,77.6206672715227));
#204042=CARTESIAN_POINT('Ctrl Pts',(-47.8635486253615,-89.639547528851,
77.6207526030934));
#204043=CARTESIAN_POINT('Ctrl Pts',(-47.8770445391941,-89.2585502588736,
77.9192569232619));
#204044=CARTESIAN_POINT('Ctrl Pts',(-47.8905695996721,-88.8568898237617,
78.1903990846767));
#204045=CARTESIAN_POINT('Ctrl Pts',(-47.9176339376232,-88.0279594985981,
78.6683051771889));
#204046=CARTESIAN_POINT('Ctrl Pts',(-47.9311316261011,-87.6024902668963,
78.8758384030079));
#204047=CARTESIAN_POINT('Ctrl Pts',(-47.9711978571694,-86.2919724125154,
79.4063621105855));
#204048=CARTESIAN_POINT('Ctrl Pts',(-47.9969625168339,-85.3752442622018,
79.6376724024459));
#204049=CARTESIAN_POINT('Ctrl Pts',(-48.0398242697937,-83.8709049161899,
79.8033179102035));
#204050=CARTESIAN_POINT('Ctrl Pts',(-48.0562071817464,-83.2976725144938,
79.8181968614348));
#204051=CARTESIAN_POINT('Ctrl Pts',(-48.0866529239232,-82.2155375469544,
79.7556116214413));
#204052=CARTESIAN_POINT('Ctrl Pts',(-48.1008092000048,-81.7077987292351,
79.6878924020851));
#204053=CARTESIAN_POINT('Ctrl Pts',(-48.1330146582569,-80.5833618276912,
79.4512656104272));
#204054=CARTESIAN_POINT('Ctrl Pts',(-48.1511310418103,-79.9730946449028,
79.2620556484616));
#204055=CARTESIAN_POINT('Ctrl Pts',(-48.1871877210263,-78.8013052805535,
78.7750688738245));
#204056=CARTESIAN_POINT('Ctrl Pts',(-48.2047101916097,-78.2418707084766,
78.4793891225225));
#204057=CARTESIAN_POINT('Ctrl Pts',(-48.2406868075071,-77.1638968790423,
77.7753651650062));
#204058=CARTESIAN_POINT('Ctrl Pts',(-48.2592283648658,-76.6503036986312,
77.3647016622442));
#204059=CARTESIAN_POINT('Ctrl Pts',(-48.3097623744413,-75.3754982319245,
76.1275080151719));
#204060=CARTESIAN_POINT('Ctrl Pts',(-48.3404245900448,-74.7048426895327,
75.2206595097633));
#204061=CARTESIAN_POINT('Ctrl Pts',(-48.3800496111431,-74.0674708014668,
73.9757305662848));
#204062=CARTESIAN_POINT('Ctrl Pts',(-48.387963293798,-73.9508691029355,
73.723125144543));
#204063=CARTESIAN_POINT('Ctrl Pts',(-48.3958698180353,-73.8447192590796,
73.4662010349383));
#204064=CARTESIAN_POINT('',(-47.8257920924624,-92.7913239034034,65.6382911956717));
#204065=CARTESIAN_POINT('Ctrl Pts',(-47.8635940884284,-89.6412075243314,
77.6194517516842));
#204066=CARTESIAN_POINT('Ctrl Pts',(-47.8609618681876,-90.29911965049,77.1037712608345));
#204067=CARTESIAN_POINT('Ctrl Pts',(-47.8579335141401,-90.8914872330497,
76.5095387599098));
#204068=CARTESIAN_POINT('Ctrl Pts',(-47.8536397962644,-91.9122995837084,
75.1986881766102));
#204069=CARTESIAN_POINT('Ctrl Pts',(-47.852298616386,-92.3389533405578,
74.4885092324321));
#204070=CARTESIAN_POINT('Ctrl Pts',(-47.8482467829845,-92.9035044699208,
73.2254447666301));
#204071=CARTESIAN_POINT('Ctrl Pts',(-47.8461648680152,-93.0892289316702,
72.6982574235016));
#204072=CARTESIAN_POINT('Ctrl Pts',(-47.840752948818,-93.5123572579288,
71.0889018852209));
#204073=CARTESIAN_POINT('Ctrl Pts',(-47.838841880717,-93.6186069667047,
69.9807652008248));
#204074=CARTESIAN_POINT('Ctrl Pts',(-47.8332362516957,-93.4722739304251,
67.763692091706));
#204075=CARTESIAN_POINT('Ctrl Pts',(-47.828574338379,-93.2174407788572,
66.6696609455417));
#204076=CARTESIAN_POINT('Ctrl Pts',(-47.8257920924624,-92.7913239034034,
65.6382911956717));
#204077=CARTESIAN_POINT('',(-47.8068141272352,-88.0240721664947,60.4464459619263));
#204078=CARTESIAN_POINT('Ctrl Pts',(-47.8257920924624,-92.7913239034034,
65.6382911956717));
#204079=CARTESIAN_POINT('Ctrl Pts',(-47.8243052474299,-92.5636050825149,
65.087122450969));
#204080=CARTESIAN_POINT('Ctrl Pts',(-47.8231856641482,-92.2882261844406,
64.556891664567));
#204081=CARTESIAN_POINT('Ctrl Pts',(-47.8203484488529,-91.6444757055702,
63.5441620336233));
#204082=CARTESIAN_POINT('Ctrl Pts',(-47.8182709902653,-91.2762819077662,
63.0643356310676));
#204083=CARTESIAN_POINT('Ctrl Pts',(-47.8141911238361,-90.4598803479546,
62.1752216331248));
#204084=CARTESIAN_POINT('Ctrl Pts',(-47.8123348538898,-90.0132957742932,
61.7676494127296));
#204085=CARTESIAN_POINT('Ctrl Pts',(-47.8093723566015,-89.0590858823477,
61.0399854921902));
#204086=CARTESIAN_POINT('Ctrl Pts',(-47.8082478401419,-88.5540397942691,
60.7203433366149));
#204087=CARTESIAN_POINT('Ctrl Pts',(-47.8068141268167,-88.0240721666117,
60.446445961702));
#204088=CARTESIAN_POINT('',(-48.1735608262671,-88.0240721664362,60.4464459619211));
#204089=CARTESIAN_POINT('',(-47.8068954859909,-88.0240721666105,60.4464459616985));
#204090=CARTESIAN_POINT('',(-48.5599506281375,-92.7913014568048,65.638236866552));
#204091=CARTESIAN_POINT('Ctrl Pts',(-48.1735608267226,-88.0240721665407,
60.4464459616653));
#204092=CARTESIAN_POINT('Ctrl Pts',(-48.2057390453445,-88.5540323787309,
60.7203395041181));
#204093=CARTESIAN_POINT('Ctrl Pts',(-48.2381635012091,-89.0590731093268,
61.0399772116219));
#204094=CARTESIAN_POINT('Ctrl Pts',(-48.3027869041061,-90.0132657864085,
61.7676250678447));
#204095=CARTESIAN_POINT('Ctrl Pts',(-48.3348415809302,-90.4598486250631,
62.175189981084));
#204096=CARTESIAN_POINT('Ctrl Pts',(-48.3987590450242,-91.2763238760333,
63.0643784397394));
#204097=CARTESIAN_POINT('Ctrl Pts',(-48.4306399072594,-91.6445575518518,
63.5442696368761));
#204098=CARTESIAN_POINT('Ctrl Pts',(-48.4954405792784,-92.2882704723868,
64.5569822372555));
#204099=CARTESIAN_POINT('Ctrl Pts',(-48.5278559888906,-92.5636125815672,
65.0871495574296));
#204100=CARTESIAN_POINT('Ctrl Pts',(-48.5599506281375,-92.7913014568048,
65.638236866552));
#204101=CARTESIAN_POINT('',(-49.2715796128967,-89.6395615474175,77.6207039925155));
#204102=CARTESIAN_POINT('Ctrl Pts',(-48.5599506281375,-92.7913014568048,
65.638236866552));
#204103=CARTESIAN_POINT('Ctrl Pts',(-48.6200116739718,-93.2173923022698,
66.6695268548046));
#204104=CARTESIAN_POINT('Ctrl Pts',(-48.6777501611375,-93.472228091973,
67.7634817707358));
#204105=CARTESIAN_POINT('Ctrl Pts',(-48.7973670931621,-93.6186218586882,
69.9805110412447));
#204106=CARTESIAN_POINT('Ctrl Pts',(-48.8573471180377,-93.5123874190092,
71.0887662129763));
#204107=CARTESIAN_POINT('Ctrl Pts',(-48.945646231306,-93.089241678521,72.6982195125106));
#204108=CARTESIAN_POINT('Ctrl Pts',(-48.9749440674501,-92.903517206451,
73.2254112828409));
#204109=CARTESIAN_POINT('Ctrl Pts',(-49.0488658367833,-92.3389663971347,
74.48848740033));
#204110=CARTESIAN_POINT('Ctrl Pts',(-49.0938910637439,-91.9123107069189,
75.198671314922));
#204111=CARTESIAN_POINT('Ctrl Pts',(-49.1831733484294,-90.8915047968733,
76.509518816451));
#204112=CARTESIAN_POINT('Ctrl Pts',(-49.2270302012072,-90.2991361429743,
77.1037580932684));
#204113=CARTESIAN_POINT('Ctrl Pts',(-49.2714848090302,-89.6412093512397,
77.6194503197283));
#204114=CARTESIAN_POINT('Ctrl Pts',(-49.8038356726598,-73.8447192590796,
73.4662010349383));
#204115=CARTESIAN_POINT('Ctrl Pts',(-49.7973206317714,-73.9339046545335,
73.6820645490462));
#204116=CARTESIAN_POINT('Ctrl Pts',(-49.7908122535838,-74.0304697561549,
73.8948834855084));
#204117=CARTESIAN_POINT('Ctrl Pts',(-49.7750566224764,-74.280725526146,
74.3997763747891));
#204118=CARTESIAN_POINT('Ctrl Pts',(-49.7657933185793,-74.4413676838132,
74.6880306542796));
#204119=CARTESIAN_POINT('Ctrl Pts',(-49.7422829552721,-74.8805252003446,
75.3936935266779));
#204120=CARTESIAN_POINT('Ctrl Pts',(-49.727961661627,-75.1762973368638,
75.79933948665));
#204121=CARTESIAN_POINT('Ctrl Pts',(-49.6954955524956,-75.9185369956801,
76.6745882707689));
#204122=CARTESIAN_POINT('Ctrl Pts',(-49.6776829623546,-76.3821893621727,
77.1268327465661));
#204123=CARTESIAN_POINT('Ctrl Pts',(-49.6333168146343,-77.6135001835875,
78.1193750085976));
#204124=CARTESIAN_POINT('Ctrl Pts',(-49.6064851997932,-78.4185952388004,
78.6039249756669));
#204125=CARTESIAN_POINT('Ctrl Pts',(-49.5660277136841,-79.7486669733972,
79.1743177482119));
#204126=CARTESIAN_POINT('Ctrl Pts',(-49.5518256482393,-80.233605180047,
79.3405518921836));
#204127=CARTESIAN_POINT('Ctrl Pts',(-49.5184093692975,-81.3830672892489,
79.6406306448179));
#204128=CARTESIAN_POINT('Ctrl Pts',(-49.4990777274927,-82.0524924873491,
79.7462625759489));
#204129=CARTESIAN_POINT('Ctrl Pts',(-49.4638379832304,-83.2977325994776,
79.8181320445648));
#204130=CARTESIAN_POINT('Ctrl Pts',(-49.448059778772,-83.8697967280917,
79.8033130035401));
#204131=CARTESIAN_POINT('Ctrl Pts',(-49.4056942010153,-85.3734803820745,
79.6380751530243));
#204132=CARTESIAN_POINT('Ctrl Pts',(-49.3786880403919,-86.2906982588559,
79.4067906991592));
#204133=CARTESIAN_POINT('Ctrl Pts',(-49.3390820081314,-87.6018225060059,
78.8761524780747));
#204134=CARTESIAN_POINT('Ctrl Pts',(-49.3259729344058,-88.0274335519023,
78.6685842401965));
#204135=CARTESIAN_POINT('Ctrl Pts',(-49.2991355767715,-88.8566142472486,
78.1905826735702));
#204136=CARTESIAN_POINT('Ctrl Pts',(-49.285430642252,-89.2583801024993,
77.9193842087995));
#204137=CARTESIAN_POINT('Ctrl Pts',(-49.2716572296686,-89.6394684428446,
77.6208145648924));
#204138=CARTESIAN_POINT('Origin',(-45.8894114130409,-83.3180213346267,69.5522455184007));
#204139=CARTESIAN_POINT('',(-52.0239203182307,-73.8447192573355,73.466201030717));
#204140=CARTESIAN_POINT('',(-51.6180871401245,-73.8447192590796,73.4662010349383));
#204141=CARTESIAN_POINT('',(-45.8894114130409,-73.8447192590796,73.4662010349383));
#204142=CARTESIAN_POINT('Ctrl Pts',(-50.2096235848678,-73.8447192590796,
73.4662010349383));
#204143=CARTESIAN_POINT('Ctrl Pts',(-50.2152587311499,-73.7682291466274,
73.2810650675032));
#204144=CARTESIAN_POINT('Ctrl Pts',(-50.2209205166887,-73.6971066797446,
73.093542991864));
#204145=CARTESIAN_POINT('Ctrl Pts',(-50.2421792944865,-73.4517838938014,
72.384532604673));
#204146=CARTESIAN_POINT('Ctrl Pts',(-50.2579032979112,-73.3141470715678,
71.8515923228509));
#204147=CARTESIAN_POINT('Ctrl Pts',(-50.2878406499025,-73.1314464457096,
70.8021108337474));
#204148=CARTESIAN_POINT('Ctrl Pts',(-50.3021105145613,-73.0814677050922,
70.2880755204298));
#204149=CARTESIAN_POINT('Ctrl Pts',(-50.3344513860217,-73.056673214677,
69.1343003713136));
#204150=CARTESIAN_POINT('Ctrl Pts',(-50.3525860612607,-73.1026014222336,
68.4962506052134));
#204151=CARTESIAN_POINT('Ctrl Pts',(-50.3886731043955,-73.3114457217308,
67.2435798090198));
#204152=CARTESIAN_POINT('Ctrl Pts',(-50.4062059720365,-73.4726928682544,
66.6314572753463));
#204153=CARTESIAN_POINT('Ctrl Pts',(-50.4421982095901,-73.9143301697055,
65.421377238379));
#204154=CARTESIAN_POINT('Ctrl Pts',(-50.4607485014183,-74.1981312827367,
64.8277274844779));
#204155=CARTESIAN_POINT('Ctrl Pts',(-50.5113921507918,-75.1163956227987,
63.3025446990746));
#204156=CARTESIAN_POINT('Ctrl Pts',(-50.5421483544675,-75.8504591731212,
62.4416229161422));
#204157=CARTESIAN_POINT('Ctrl Pts',(-50.5931362890706,-77.2260936162112,
61.2813551912261));
#204158=CARTESIAN_POINT('Ctrl Pts',(-50.6124378411332,-77.7845151191548,
60.8977936531863));
#204159=CARTESIAN_POINT('Ctrl Pts',(-50.6501790766711,-78.9678990253529,
60.2466336853813));
#204160=CARTESIAN_POINT('Ctrl Pts',(-50.6689114356124,-79.5898722357642,
59.9804704590923));
#204161=CARTESIAN_POINT('Ctrl Pts',(-50.702648826188,-80.7262240909296,
59.6218847490626));
#204162=CARTESIAN_POINT('Ctrl Pts',(-50.7174214577686,-81.2300224633969,
59.5038756888092));
#204163=CARTESIAN_POINT('Ctrl Pts',(-50.7413547345326,-82.0681130272073,
59.3733398517201));
#204164=CARTESIAN_POINT('Ctrl Pts',(-50.7505851433636,-82.3979440931124,
59.3382428579476));
#204165=CARTESIAN_POINT('Ctrl Pts',(-50.7975213204536,-84.0782644435076,
59.2415055227305));
#204166=CARTESIAN_POINT('Ctrl Pts',(-50.8360007821808,-85.4297666425667,
59.431481709767));
#204167=CARTESIAN_POINT('Ctrl Pts',(-50.9113416243312,-87.9796635714467,
60.3243343480095));
#204168=CARTESIAN_POINT('Ctrl Pts',(-50.9497759551382,-89.1532807598111,
61.0179025958922));
#204169=CARTESIAN_POINT('Ctrl Pts',(-51.0047808895068,-90.6220228361453,
62.3341359280561));
#204170=CARTESIAN_POINT('Ctrl Pts',(-51.0221410764558,-91.0465650538621,
62.7906518478815));
#204171=CARTESIAN_POINT('Ctrl Pts',(-51.0542450765868,-91.7390711980155,
63.6863618893484));
#204172=CARTESIAN_POINT('Ctrl Pts',(-51.0688308864644,-92.0204998589996,
64.1126185471536));
#204173=CARTESIAN_POINT('Ctrl Pts',(-51.1022187659112,-92.5987553498626,
65.1490151296931));
#204174=CARTESIAN_POINT('Ctrl Pts',(-51.1208774390134,-92.8691501617716,
65.7711860632802));
#204175=CARTESIAN_POINT('Ctrl Pts',(-51.1548729987492,-93.2384272103452,
66.9199684144007));
#204176=CARTESIAN_POINT('Ctrl Pts',(-51.1699759240403,-93.3612329273738,
67.4362989395747));
#204177=CARTESIAN_POINT('Ctrl Pts',(-51.2117835909394,-93.5900395746801,
68.8911604270237));
#204178=CARTESIAN_POINT('Ctrl Pts',(-51.2375992875248,-93.6073154449516,
69.8382887136524));
#204179=CARTESIAN_POINT('Ctrl Pts',(-51.2824202947345,-93.4183243877577,
71.4120497051439));
#204180=CARTESIAN_POINT('Ctrl Pts',(-51.3008195271194,-93.281981828787,
72.0411193268221));
#204181=CARTESIAN_POINT('Ctrl Pts',(-51.332914609746,-92.9358387018392,
73.1316242487575));
#204182=CARTESIAN_POINT('Ctrl Pts',(-51.3468118683534,-92.7490800421751,
73.5981691204317));
#204183=CARTESIAN_POINT('Ctrl Pts',(-51.3702006408016,-92.3831290921145,
74.3477352292558));
#204184=CARTESIAN_POINT('Ctrl Pts',(-51.3795720312957,-92.2229254887043,
74.6390500290059));
#204185=CARTESIAN_POINT('Ctrl Pts',(-51.402509724984,-91.7993587266667,
75.3277306857764));
#204186=CARTESIAN_POINT('Ctrl Pts',(-51.4161202137027,-91.521889929389,
75.7155119559237));
#204187=CARTESIAN_POINT('Ctrl Pts',(-51.4429325966705,-90.9153420781408,
76.4493165723929));
#204188=CARTESIAN_POINT('Ctrl Pts',(-51.4561078238969,-90.5870482648257,
76.7944913293652));
#204189=CARTESIAN_POINT('Ctrl Pts',(-51.48756500931,-89.7569663312927,77.5537380621301));
#204190=CARTESIAN_POINT('Ctrl Pts',(-51.5059390037133,-89.2374296711775,
77.9453668480806));
#204191=CARTESIAN_POINT('Ctrl Pts',(-51.533918319714,-88.3993095355104,
78.4603850334184));
#204192=CARTESIAN_POINT('Ctrl Pts',(-51.5434030417083,-88.105845456195,
78.621489376031));
#204193=CARTESIAN_POINT('Ctrl Pts',(-51.5729128059786,-87.1587681226295,
79.0826086526193));
#204194=CARTESIAN_POINT('Ctrl Pts',(-51.5927914031008,-86.4812026847779,
79.3284127140952));
#204195=CARTESIAN_POINT('Ctrl Pts',(-51.6274224279696,-85.2930522074634,
79.6228502185749));
#204196=CARTESIAN_POINT('Ctrl Pts',(-51.6418592851651,-84.7942755429739,
79.7079580210748));
#204197=CARTESIAN_POINT('Ctrl Pts',(-51.6735664554767,-83.6780138171301,
79.8144286227466));
#204198=CARTESIAN_POINT('Ctrl Pts',(-51.6905597091711,-83.0607405314188,
79.8175173393461));
#204199=CARTESIAN_POINT('Ctrl Pts',(-51.7267421582604,-81.7746480406731,
79.7078230825936));
#204200=CARTESIAN_POINT('Ctrl Pts',(-51.7459449176401,-81.1096667916172,
79.5842398510074));
#204201=CARTESIAN_POINT('Ctrl Pts',(-51.7941678793656,-79.4778033105092,
79.110735851032));
#204202=CARTESIAN_POINT('Ctrl Pts',(-51.822180689247,-78.542268924523,78.6793590613686));
#204203=CARTESIAN_POINT('Ctrl Pts',(-51.8681523662406,-77.1877831947701,
77.7886683778086));
#204204=CARTESIAN_POINT('Ctrl Pts',(-51.8852020986695,-76.7188368099212,
77.4179469190336));
#204205=CARTESIAN_POINT('Ctrl Pts',(-51.9241413640814,-75.7069031604261,
76.4634318958915));
#204206=CARTESIAN_POINT('Ctrl Pts',(-51.9461415253868,-75.1943307168622,
75.8529811569711));
#204207=CARTESIAN_POINT('Ctrl Pts',(-51.9865585514724,-74.4108924845377,
74.6632671062139));
#204208=CARTESIAN_POINT('Ctrl Pts',(-52.0045251918746,-74.1136240030923,
74.1062078376817));
#204209=CARTESIAN_POINT('Ctrl Pts',(-52.0227265417637,-73.8611037358073,
73.5056828137199));
#204210=CARTESIAN_POINT('Ctrl Pts',(-52.0233235296543,-73.8528803082147,
73.4859539635495));
#204211=CARTESIAN_POINT('Ctrl Pts',(-52.0239203182307,-73.8447192555915,
73.4662010264956));
#204212=CARTESIAN_POINT('Ctrl Pts',(-51.6180871401245,-73.8447192590796,
73.4662010349383));
#204213=CARTESIAN_POINT('Ctrl Pts',(-51.6088680289194,-73.9695775786798,
73.7684069678417));
#204214=CARTESIAN_POINT('Ctrl Pts',(-51.5995742687078,-74.1090451023638,
74.0649984361503));
#204215=CARTESIAN_POINT('Ctrl Pts',(-51.5808374449442,-74.4176933519959,
74.6469431862595));
#204216=CARTESIAN_POINT('Ctrl Pts',(-51.5714221024677,-74.5866248525164,
74.9313253023218));
#204217=CARTESIAN_POINT('Ctrl Pts',(-51.5488062304926,-75.0295876819302,
75.6010035997114));
#204218=CARTESIAN_POINT('Ctrl Pts',(-51.535725037155,-75.3170941776685,
75.9764790508954));
#204219=CARTESIAN_POINT('Ctrl Pts',(-51.5132824279099,-75.8479256737056,
76.5785740598815));
#204220=CARTESIAN_POINT('Ctrl Pts',(-51.5040042629682,-76.0782335248933,
76.8156532917978));
#204221=CARTESIAN_POINT('Ctrl Pts',(-51.4804745108094,-76.6859979262158,
77.3836101134934));
#204222=CARTESIAN_POINT('Ctrl Pts',(-51.4661488559317,-77.0770455482743,
77.6986695192962));
#204223=CARTESIAN_POINT('Ctrl Pts',(-51.433710034848,-78.0202762089417,
78.3506896419294));
#204224=CARTESIAN_POINT('Ctrl Pts',(-51.4159271820186,-78.584424246117,
78.6666178546337));
#204225=CARTESIAN_POINT('Ctrl Pts',(-51.3715379735554,-80.0317792974971,
79.3062993131463));
#204226=CARTESIAN_POINT('Ctrl Pts',(-51.3446502820813,-80.9369703855401,
79.5658141301405));
#204227=CARTESIAN_POINT('Ctrl Pts',(-51.304010833661,-82.3760421333811,
79.7719296091203));
#204228=CARTESIAN_POINT('Ctrl Pts',(-51.2896814831992,-82.8921232634512,
79.8064094839421));
#204229=CARTESIAN_POINT('Ctrl Pts',(-51.2561239832045,-84.0848126465833,
79.7958694853764));
#204230=CARTESIAN_POINT('Ctrl Pts',(-51.2367826235284,-84.7587699279815,
79.7229893473125));
#204231=CARTESIAN_POINT('Ctrl Pts',(-51.2020429532851,-85.9627283515491,
79.4706534872351));
#204232=CARTESIAN_POINT('Ctrl Pts',(-51.1867385626414,-86.4947373285883,
79.3132787849589));
#204233=CARTESIAN_POINT('Ctrl Pts',(-51.1397423175928,-88.0607289081945,
78.7083671943219));
#204234=CARTESIAN_POINT('Ctrl Pts',(-51.1075807679138,-89.0361904333139,
78.1330603498034));
#204235=CARTESIAN_POINT('Ctrl Pts',(-51.0578986311202,-90.4020450773067,
76.9893310403567));
#204236=CARTESIAN_POINT('Ctrl Pts',(-51.0395561058025,-90.863790620292,
76.5203866193077));
#204237=CARTESIAN_POINT('Ctrl Pts',(-51.0029816279645,-91.675537924791,
75.5199506099501));
#204238=CARTESIAN_POINT('Ctrl Pts',(-50.9849985245908,-92.0273794945852,
74.9936318724835));
#204239=CARTESIAN_POINT('Ctrl Pts',(-50.949530423408,-92.6329030547024,
73.8769649768003));
#204240=CARTESIAN_POINT('Ctrl Pts',(-50.9317844359032,-92.8841638273681,
73.2884379965072));
#204241=CARTESIAN_POINT('Ctrl Pts',(-50.8990848004757,-93.2367409953333,
72.1882560767215));
#204242=CARTESIAN_POINT('Ctrl Pts',(-50.8843122210643,-93.3570080036304,
71.6849187868307));
#204243=CARTESIAN_POINT('Ctrl Pts',(-50.8543688558147,-93.5248753284648,
70.6377495403507));
#204244=CARTESIAN_POINT('Ctrl Pts',(-50.8393398806685,-93.5680841921314,
70.0948338660248));
#204245=CARTESIAN_POINT('Ctrl Pts',(-50.7920614820175,-93.5678887198971,
68.4056658668837));
#204246=CARTESIAN_POINT('Ctrl Pts',(-50.7593317019474,-93.3757688773966,
67.2683584434087));
#204247=CARTESIAN_POINT('Ctrl Pts',(-50.6897094276442,-92.5559597270763,
64.9101762264595));
#204248=CARTESIAN_POINT('Ctrl Pts',(-50.651244773498,-91.8642330778891,
63.7341197715842));
#204249=CARTESIAN_POINT('Ctrl Pts',(-50.5952993305559,-90.5283527393984,
62.2377214259173));
#204250=CARTESIAN_POINT('Ctrl Pts',(-50.5770222587136,-90.0465525155411,
61.7922196472051));
#204251=CARTESIAN_POINT('Ctrl Pts',(-50.5405414684501,-89.0236613067167,
61.0137450018216));
#204252=CARTESIAN_POINT('Ctrl Pts',(-50.5225693444161,-88.4875600718011,
60.6789031349042));
#204253=CARTESIAN_POINT('Ctrl Pts',(-50.4872101825288,-87.3566336744448,
60.1100214718486));
#204254=CARTESIAN_POINT('Ctrl Pts',(-50.4695694709475,-86.7638732376919,
59.8779451961286));
#204255=CARTESIAN_POINT('Ctrl Pts',(-50.4373797327673,-85.6703517985294,
59.5631628233311));
#204256=CARTESIAN_POINT('Ctrl Pts',(-50.4230182927863,-85.1776707837086,
59.4598259614579));
#204257=CARTESIAN_POINT('Ctrl Pts',(-50.3908246801374,-84.0495941544247,
59.3086580637835));
#204258=CARTESIAN_POINT('Ctrl Pts',(-50.3733051002074,-83.4133024216528,
59.2830095979889));
#204259=CARTESIAN_POINT('Ctrl Pts',(-50.3286408184093,-81.8229071678612,
59.366800535251));
#204260=CARTESIAN_POINT('Ctrl Pts',(-50.3011872547787,-80.8788235245975,
59.5507967074688));
#204261=CARTESIAN_POINT('Ctrl Pts',(-50.2585181496259,-79.4353698362872,
60.0489707053046));
#204262=CARTESIAN_POINT('Ctrl Pts',(-50.2427049380204,-78.9131522289264,
60.2794712754771));
#204263=CARTESIAN_POINT('Ctrl Pts',(-50.2012185078618,-77.6216584887111,
60.98336079612));
#204264=CARTESIAN_POINT('Ctrl Pts',(-50.1754966749369,-76.8908060720885,
61.51699453351));
#204265=CARTESIAN_POINT('Ctrl Pts',(-50.1321267801252,-75.7662093542935,
62.5909022123853));
#204266=CARTESIAN_POINT('Ctrl Pts',(-50.1138751742358,-75.337562903395,
63.0867648717513));
#204267=CARTESIAN_POINT('Ctrl Pts',(-50.0774292702906,-74.5942431474175,
64.1341646722153));
#204268=CARTESIAN_POINT('Ctrl Pts',(-50.0594601022904,-74.2775987983706,
64.6808305870127));
#204269=CARTESIAN_POINT('Ctrl Pts',(-50.0245970747622,-73.7541488071094,
65.8137609433811));
#204270=CARTESIAN_POINT('Ctrl Pts',(-50.0074507095344,-73.5463136479135,
66.396670831945));
#204271=CARTESIAN_POINT('Ctrl Pts',(-49.9762190900313,-73.2706174739045,
67.4666577787987));
#204272=CARTESIAN_POINT('Ctrl Pts',(-49.9623096670931,-73.182831640914,
67.9466531175065));
#204273=CARTESIAN_POINT('Ctrl Pts',(-49.9260721432976,-73.0429598345648,
69.2177099815939));
#204274=CARTESIAN_POINT('Ctrl Pts',(-49.9043390259112,-73.0477888731545,
70.0117339440578));
#204275=CARTESIAN_POINT('Ctrl Pts',(-49.8629742368981,-73.2261677555999,
71.4694146974536));
#204276=CARTESIAN_POINT('Ctrl Pts',(-49.8435831292548,-73.3748234753399,
72.1317511881231));
#204277=CARTESIAN_POINT('Ctrl Pts',(-49.8175643780153,-73.6650694216188,
73.0081948368761));
#204278=CARTESIAN_POINT('Ctrl Pts',(-49.8106963345261,-73.7508026049707,
73.238886025726));
#204279=CARTESIAN_POINT('Ctrl Pts',(-49.8038356726598,-73.8447192590796,
73.4662010349383));
#204280=CARTESIAN_POINT('Origin',(-45.8894114130409,-83.3180213346267,69.5522455184007));
#204281=CARTESIAN_POINT('',(-53.8378263131057,-73.8447192590796,73.4662010349383));
#204282=CARTESIAN_POINT('',(-53.4317936414903,-73.8447192595573,73.4662010360945));
#204283=CARTESIAN_POINT('',(-45.8894114130409,-73.8447192590796,73.4662010349383));
#204284=CARTESIAN_POINT('Ctrl Pts',(-52.0239203182307,-73.8447192555915,
73.4662010264956));
#204285=CARTESIAN_POINT('Ctrl Pts',(-52.0422770133231,-73.5936924086256,
72.858617944282));
#204286=CARTESIAN_POINT('Ctrl Pts',(-52.0605483749575,-73.4016808879974,
72.228248441614));
#204287=CARTESIAN_POINT('Ctrl Pts',(-52.0942628704608,-73.1657213497129,
71.0613550323591));
#204288=CARTESIAN_POINT('Ctrl Pts',(-52.1095099790986,-73.1009902501868,
70.531469726697));
#204289=CARTESIAN_POINT('Ctrl Pts',(-52.1377410759291,-73.0573142951046,
69.5302680403876));
#204290=CARTESIAN_POINT('Ctrl Pts',(-52.1507348460864,-73.0690701400119,
69.060720889055));
#204291=CARTESIAN_POINT('Ctrl Pts',(-52.173186689646,-73.1441802615669,
68.2611238726265));
#204292=CARTESIAN_POINT('Ctrl Pts',(-52.1825655151234,-73.1916465457803,
67.9303426470445));
#204293=CARTESIAN_POINT('Ctrl Pts',(-52.2061708075939,-73.3503948751928,
67.1110373782177));
#204294=CARTESIAN_POINT('Ctrl Pts',(-52.2204692031783,-73.4814864543216,
66.6272407659104));
#204295=CARTESIAN_POINT('Ctrl Pts',(-52.2531015148368,-73.8637581996122,
65.5390745711569));
#204296=CARTESIAN_POINT('Ctrl Pts',(-52.2710912133515,-74.1384598613343,
64.9452632469345));
#204297=CARTESIAN_POINT('Ctrl Pts',(-52.3083462598444,-74.8082876769875,
63.7987580593691));
#204298=CARTESIAN_POINT('Ctrl Pts',(-52.3275847766853,-75.205561491599,
63.2509628073172));
#204299=CARTESIAN_POINT('Ctrl Pts',(-52.3708968886107,-76.2199062240943,
62.1087133425954));
#204300=CARTESIAN_POINT('Ctrl Pts',(-52.3942780319818,-76.8633589762556,
61.544327886537));
#204301=CARTESIAN_POINT('Ctrl Pts',(-52.4439230593988,-78.3198530270727,
60.557645931314));
#204302=CARTESIAN_POINT('Ctrl Pts',(-52.4697754954037,-79.1346429520161,
60.1509757586101));
#204303=CARTESIAN_POINT('Ctrl Pts',(-52.5133928595621,-80.6140705410418,
59.64349633463));
#204304=CARTESIAN_POINT('Ctrl Pts',(-52.5317625923539,-81.2549684453486,
59.4905128716933));
#204305=CARTESIAN_POINT('Ctrl Pts',(-52.5683778176634,-82.532282188248,
59.3128694076042));
#204306=CARTESIAN_POINT('Ctrl Pts',(-52.5863670039881,-83.1652054050903,
59.283902231493));
#204307=CARTESIAN_POINT('Ctrl Pts',(-52.6218833432031,-84.435990751974,
59.3433199942979));
#204308=CARTESIAN_POINT('Ctrl Pts',(-52.6396741231847,-85.0710214742086,
59.4330062849073));
#204309=CARTESIAN_POINT('Ctrl Pts',(-52.6726137453752,-86.2028426545355,
59.7026552256781));
#204310=CARTESIAN_POINT('Ctrl Pts',(-52.6875849700365,-86.7021081484069,
59.8628401268524));
#204311=CARTESIAN_POINT('Ctrl Pts',(-52.7167190063917,-87.65853629047,60.2526874831467));
#204312=CARTESIAN_POINT('Ctrl Pts',(-52.7308076230974,-88.1151488521579,
60.4797915353621));
#204313=CARTESIAN_POINT('Ctrl Pts',(-52.7624829229541,-89.0887049844133,
61.0581310247888));
#204314=CARTESIAN_POINT('Ctrl Pts',(-52.7801173891084,-89.5942839773548,
61.4245592008917));
#204315=CARTESIAN_POINT('Ctrl Pts',(-52.8362453338733,-91.079955018231,
62.7230769619799));
#204316=CARTESIAN_POINT('Ctrl Pts',(-52.8731268851787,-91.9109898122703,
63.8036767077062));
#204317=CARTESIAN_POINT('Ctrl Pts',(-52.9499845296873,-93.1071166812942,
66.2261390180689));
#204318=CARTESIAN_POINT('Ctrl Pts',(-52.986907153841,-93.4599413377088,
67.5445518777276));
#204319=CARTESIAN_POINT('Ctrl Pts',(-53.0347878919167,-93.5681338346198,
69.2242163121293));
#204320=CARTESIAN_POINT('Ctrl Pts',(-53.0442240638684,-93.5733808590658,
69.5558979227205));
#204321=CARTESIAN_POINT('Ctrl Pts',(-53.0681128435813,-93.5456188232973,
70.4048654754654));
#204322=CARTESIAN_POINT('Ctrl Pts',(-53.0824397629106,-93.4894872847451,
70.9204549018704));
#204323=CARTESIAN_POINT('Ctrl Pts',(-53.1266209662051,-93.2006489952452,
72.4707885674772));
#204324=CARTESIAN_POINT('Ctrl Pts',(-53.1569471242125,-92.8464568547865,
73.4756555819651));
#204325=CARTESIAN_POINT('Ctrl Pts',(-53.1956975694565,-92.1884187399158,
74.6988304708029));
#204326=CARTESIAN_POINT('Ctrl Pts',(-53.2048792607579,-92.0182280079635,
74.981581587507));
#204327=CARTESIAN_POINT('Ctrl Pts',(-53.2330373667578,-91.4592599313037,
75.8162701146337));
#204328=CARTESIAN_POINT('Ctrl Pts',(-53.2522385332535,-91.0293762727016,
76.3384637818322));
#204329=CARTESIAN_POINT('Ctrl Pts',(-53.3008563819609,-89.8156874020234,
77.5472951144627));
#204330=CARTESIAN_POINT('Ctrl Pts',(-53.3292423807927,-88.9729888883224,
78.1639715288605));
#204331=CARTESIAN_POINT('Ctrl Pts',(-53.3762905115393,-87.5019766114925,
78.9299701749641));
#204332=CARTESIAN_POINT('Ctrl Pts',(-53.3939907626489,-86.9269766557998,
79.1659159521151));
#204333=CARTESIAN_POINT('Ctrl Pts',(-53.4258660672702,-85.8371802711613,
79.5014547760017));
#204334=CARTESIAN_POINT('Ctrl Pts',(-53.440293462899,-85.3292546008724,
79.6164328858441));
#204335=CARTESIAN_POINT('Ctrl Pts',(-53.473959533795,-84.1456861017741,
79.7911392171768));
#204336=CARTESIAN_POINT('Ctrl Pts',(-53.493308172292,-83.46844100145,79.8234349761715));
#204337=CARTESIAN_POINT('Ctrl Pts',(-53.5276985212792,-82.2519364355357,
79.7610384134673));
#204338=CARTESIAN_POINT('Ctrl Pts',(-53.542672354733,-81.7139511536507,
79.6904382341201));
#204339=CARTESIAN_POINT('Ctrl Pts',(-53.5900109002638,-80.0596313329246,
79.3383093961517));
#204340=CARTESIAN_POINT('Ctrl Pts',(-53.6228577484491,-78.983432082236,
78.9114915684615));
#204341=CARTESIAN_POINT('Ctrl Pts',(-53.6926017569744,-76.8452963902698,
77.6140401558868));
#204342=CARTESIAN_POINT('Ctrl Pts',(-53.7310713831788,-75.8399591963833,
76.691383828323));
#204343=CARTESIAN_POINT('Ctrl Pts',(-53.7870357222705,-74.6559146677685,
75.0712859410944));
#204344=CARTESIAN_POINT('Ctrl Pts',(-53.805332611289,-74.3208843648723,
74.5063768204541));
#204345=CARTESIAN_POINT('Ctrl Pts',(-53.8285582294811,-73.9727193494954,
73.7658432035555));
#204346=CARTESIAN_POINT('Ctrl Pts',(-53.8331925250674,-73.9069169167772,
73.6167436758221));
#204347=CARTESIAN_POINT('Ctrl Pts',(-53.8378263131057,-73.8447192590796,
73.4662010349383));
#204348=CARTESIAN_POINT('Ctrl Pts',(-53.4317936414903,-73.844719260035,
73.4662010372508));
#204349=CARTESIAN_POINT('Ctrl Pts',(-53.4314659960779,-73.8491222862514,
73.4768580815603));
#204350=CARTESIAN_POINT('Ctrl Pts',(-53.4311383816884,-73.8535434612602,
73.4875080972125));
#204351=CARTESIAN_POINT('Ctrl Pts',(-53.4128952710928,-74.1007721347706,
74.0802219304168));
#204352=CARTESIAN_POINT('Ctrl Pts',(-53.3954072228787,-74.3967639325128,
74.6386413478996));
#204353=CARTESIAN_POINT('Ctrl Pts',(-53.3594844786823,-75.1007300517108,
75.7139927044221));
#204354=CARTESIAN_POINT('Ctrl Pts',(-53.3409746455454,-75.5109043610059,
76.226068551973));
#204355=CARTESIAN_POINT('Ctrl Pts',(-53.2839183522462,-76.9087607598518,
77.6645611460637));
#204356=CARTESIAN_POINT('Ctrl Pts',(-53.2470045192626,-78.0328192134182,
78.4379034484896));
#204357=CARTESIAN_POINT('Ctrl Pts',(-53.1760057253269,-80.3261415055106,
79.4224570102882));
#204358=CARTESIAN_POINT('Ctrl Pts',(-53.1446794675631,-81.446073105076,
79.6946439377546));
#204359=CARTESIAN_POINT('Ctrl Pts',(-53.0968240154838,-83.130495291176,
79.8149681958114));
#204360=CARTESIAN_POINT('Ctrl Pts',(-53.0812542410853,-83.6755298664529,
79.8104536842918));
#204361=CARTESIAN_POINT('Ctrl Pts',(-53.0514361457815,-84.7323198864851,
79.7173440421182));
#204362=CARTESIAN_POINT('Ctrl Pts',(-53.0371402952389,-85.2428522259182,
79.6331432599799));
#204363=CARTESIAN_POINT('Ctrl Pts',(-53.0022205705578,-86.4535301974657,
79.3381092417562));
#204364=CARTESIAN_POINT('Ctrl Pts',(-52.9814285047545,-87.1417473880965,
79.0902559042181));
#204365=CARTESIAN_POINT('Ctrl Pts',(-52.9512840399917,-88.0988145283276,
78.6252011401997));
#204366=CARTESIAN_POINT('Ctrl Pts',(-52.941924293927,-88.3924870962548,
78.4642770171724));
#204367=CARTESIAN_POINT('Ctrl Pts',(-52.9143597158262,-89.2348059345622,
77.9475554461033));
#204368=CARTESIAN_POINT('Ctrl Pts',(-52.8961354568488,-89.7578902781713,
77.5533485346869));
#204369=CARTESIAN_POINT('Ctrl Pts',(-52.8641346519024,-90.5899246708746,
76.7915263111902));
#204370=CARTESIAN_POINT('Ctrl Pts',(-52.8505713097731,-90.9172918257617,
76.447087942484));
#204371=CARTESIAN_POINT('Ctrl Pts',(-52.8238139978604,-91.5221729799957,
75.7150387416953));
#204372=CARTESIAN_POINT('Ctrl Pts',(-52.8106602608981,-91.7989167849175,
75.3282771916983));
#204373=CARTESIAN_POINT('Ctrl Pts',(-52.7880664001755,-92.2224186552218,
74.63999416063));
#204374=CARTESIAN_POINT('Ctrl Pts',(-52.7787101072541,-92.3830593056323,
74.347927168135));
#204375=CARTESIAN_POINT('Ctrl Pts',(-52.7550857351594,-92.7494153707999,
73.5974083153159));
#204376=CARTESIAN_POINT('Ctrl Pts',(-52.7407446071526,-92.936195309577,
73.1306895624725));
#204377=CARTESIAN_POINT('Ctrl Pts',(-52.7084130093085,-93.2818563157177,
72.0412732352165));
#204378=CARTESIAN_POINT('Ctrl Pts',(-52.6907451184266,-93.4179637838621,
71.4135437556393));
#204379=CARTESIAN_POINT('Ctrl Pts',(-52.6462484222971,-93.607556126628,
69.8385019542383));
#204380=CARTESIAN_POINT('Ctrl Pts',(-52.6191261781122,-93.5901249332605,
68.8886457121736));
#204381=CARTESIAN_POINT('Ctrl Pts',(-52.577694997278,-93.3590903377669,
67.4244244110862));
#204382=CARTESIAN_POINT('Ctrl Pts',(-52.5628004969001,-93.23389135412,66.9015454393607));
#204383=CARTESIAN_POINT('Ctrl Pts',(-52.5286159492089,-92.8595098718149,
65.7468748805531));
#204384=CARTESIAN_POINT('Ctrl Pts',(-52.5092323715447,-92.5874114302617,
65.1251422778849));
#204385=CARTESIAN_POINT('Ctrl Pts',(-52.4763357891662,-92.0161993105707,
64.1075959626971));
#204386=CARTESIAN_POINT('Ctrl Pts',(-52.4627751968757,-91.7460663408475,
63.6981383524777));
#204387=CARTESIAN_POINT('Ctrl Pts',(-52.4309630398125,-91.0532107862128,
62.7958510848964));
#204388=CARTESIAN_POINT('Ctrl Pts',(-52.412630142182,-90.6109278293944,
62.3206812572907));
#204389=CARTESIAN_POINT('Ctrl Pts',(-52.384692694973,-89.8767155914402,
61.6682144442994));
#204390=CARTESIAN_POINT('Ctrl Pts',(-52.3752083043004,-89.6159179377135,
61.4583639230839));
#204391=CARTESIAN_POINT('Ctrl Pts',(-52.3457945902119,-88.7667206818431,
60.8409941032593));
#204392=CARTESIAN_POINT('Ctrl Pts',(-52.326011970883,-88.1456699508842,
60.4820724973368));
#204393=CARTESIAN_POINT('Ctrl Pts',(-52.2915787964989,-87.0339097740575,
59.986337237425));
#204394=CARTESIAN_POINT('Ctrl Pts',(-52.2772408043858,-86.5611004650484,
59.8158774709484));
#204395=CARTESIAN_POINT('Ctrl Pts',(-52.2448876251276,-85.4596461536221,
59.507953321651));
#204396=CARTESIAN_POINT('Ctrl Pts',(-52.22719657544,-84.8267186286824,59.3935941724937));
#204397=CARTESIAN_POINT('Ctrl Pts',(-52.1827229976503,-83.2468765253718,
59.2591326613441));
#204398=CARTESIAN_POINT('Ctrl Pts',(-52.1556494608471,-82.2999282653714,
59.3093587972093));
#204399=CARTESIAN_POINT('Ctrl Pts',(-52.1143881262755,-80.8505356441113,
59.5894406872827));
#204400=CARTESIAN_POINT('Ctrl Pts',(-52.0996164496285,-80.336457153583,
59.7310317134483));
#204401=CARTESIAN_POINT('Ctrl Pts',(-52.0655683723267,-79.1991284312426,
60.141861162038));
#204402=CARTESIAN_POINT('Ctrl Pts',(-52.046193967924,-78.5868929144694,
60.4342949386094));
#204403=CARTESIAN_POINT('Ctrl Pts',(-52.0129298437869,-77.5780295802241,
61.045327815706));
#204404=CARTESIAN_POINT('Ctrl Pts',(-51.9990216839351,-77.1678265296377,
61.3369998056442));
#204405=CARTESIAN_POINT('Ctrl Pts',(-51.9673054134062,-76.2944334305258,
62.0602316501973));
#204406=CARTESIAN_POINT('Ctrl Pts',(-51.9494382097905,-75.8464292686363,
62.5069380626748));
#204407=CARTESIAN_POINT('Ctrl Pts',(-51.8930940259451,-74.5786579956985,
64.0289113611284));
#204408=CARTESIAN_POINT('Ctrl Pts',(-51.8562261691269,-73.9281584556253,
65.2262591381618));
#204409=CARTESIAN_POINT('Ctrl Pts',(-51.7793863201825,-73.1278341473228,
67.8060293697946));
#204410=CARTESIAN_POINT('Ctrl Pts',(-51.7424659278239,-72.9866121356817,
69.1634381986777));
#204411=CARTESIAN_POINT('Ctrl Pts',(-51.674918110725,-73.2082696381617,
71.527539235845));
#204412=CARTESIAN_POINT('Ctrl Pts',(-51.6468253702287,-73.4555052622732,
72.5241510427503));
#204413=CARTESIAN_POINT('Ctrl Pts',(-51.6180871401245,-73.8447192590796,
73.4662010349383));
#204414=CARTESIAN_POINT('Origin',(-45.8894114130409,-83.3180213346267,69.5522455184007));
#204415=CARTESIAN_POINT('',(-55.6519493945588,-73.8447192590796,73.4662010349383));
#204416=CARTESIAN_POINT('',(-55.2458788381492,-73.8447192608157,73.4662010391402));
#204417=CARTESIAN_POINT('',(-45.8894114130409,-73.8447192590796,73.4662010349383));
#204418=CARTESIAN_POINT('',(-54.9945874883696,-92.4407690432347,74.2253573558264));
#204419=CARTESIAN_POINT('Ctrl Pts',(-54.9945936623312,-92.4407691206747,
74.2253572046497));
#204420=CARTESIAN_POINT('Ctrl Pts',(-55.0066649201741,-92.2433966771307,
74.6106634295504));
#204421=CARTESIAN_POINT('Ctrl Pts',(-55.0187555319245,-92.0218130116692,
74.9830764195218));
#204422=CARTESIAN_POINT('Ctrl Pts',(-55.0429782090374,-91.5373152573875,
75.6911698136988));
#204423=CARTESIAN_POINT('Ctrl Pts',(-55.0550815346248,-91.2756917979126,
76.0267078005093));
#204424=CARTESIAN_POINT('Ctrl Pts',(-55.0899110882135,-90.4637607069585,
76.944205363172));
#204425=CARTESIAN_POINT('Ctrl Pts',(-55.1119688536957,-89.8651910287765,
77.4792395854887));
#204426=CARTESIAN_POINT('Ctrl Pts',(-55.1495375466645,-88.770245468781,
78.248524598755));
#204427=CARTESIAN_POINT('Ctrl Pts',(-55.1648147582145,-88.3063051566961,
78.522698919535));
#204428=CARTESIAN_POINT('Ctrl Pts',(-55.2055978337842,-87.018110709541,
79.1530156806458));
#204429=CARTESIAN_POINT('Ctrl Pts',(-55.2302546487337,-86.1650441718704,
79.4396070179568));
#204430=CARTESIAN_POINT('Ctrl Pts',(-55.2783996876088,-84.4858971272087,
79.7680474707867));
#204431=CARTESIAN_POINT('Ctrl Pts',(-55.3017789764987,-83.6703563978136,
79.8285489547887));
#204432=CARTESIAN_POINT('Ctrl Pts',(-55.3434912289675,-82.1819265079146,
79.761431518673));
#204433=CARTESIAN_POINT('Ctrl Pts',(-55.3621760200869,-81.5122159206528,
79.6644786670884));
#204434=CARTESIAN_POINT('Ctrl Pts',(-55.3999714383141,-80.2140361905615,
79.3433819460147));
#204435=CARTESIAN_POINT('Ctrl Pts',(-55.4189476524304,-79.5880784923225,
79.1224394238562));
#204436=CARTESIAN_POINT('Ctrl Pts',(-55.4515257106814,-78.5351379874725,
78.6316709205173));
#204437=CARTESIAN_POINT('Ctrl Pts',(-55.4653579824756,-78.0984814130689,
78.3878747900162));
#204438=CARTESIAN_POINT('Ctrl Pts',(-55.4993518147926,-77.0860228121406,
77.7212560786378));
#204439=CARTESIAN_POINT('Ctrl Pts',(-55.5196795163116,-76.5332138955025,
77.2682618098607));
#204440=CARTESIAN_POINT('Ctrl Pts',(-55.556419597369,-75.6208619052758,
76.3461951921266));
#204441=CARTESIAN_POINT('Ctrl Pts',(-55.5725755041761,-75.2461089869606,
75.8963961645671));
#204442=CARTESIAN_POINT('Ctrl Pts',(-55.6097438652591,-74.4859060044505,
74.8067753415515));
#204443=CARTESIAN_POINT('Ctrl Pts',(-55.6308775706893,-74.1282814057265,
74.152532256902));
#204444=CARTESIAN_POINT('Ctrl Pts',(-55.6519493945588,-73.8447192590796,
73.4662010349383));
#204445=CARTESIAN_POINT('Ctrl Pts',(-53.8378263131057,-73.8447192590796,
73.4662010349383));
#204446=CARTESIAN_POINT('Ctrl Pts',(-53.8511289913648,-73.6661622292858,
73.034023235829));
#204447=CARTESIAN_POINT('Ctrl Pts',(-53.8643689226581,-73.5173135352037,
72.5899503891903));
#204448=CARTESIAN_POINT('Ctrl Pts',(-53.8952071739069,-73.2388572589834,
71.5214345218071));
#204449=CARTESIAN_POINT('Ctrl Pts',(-53.9128793880311,-73.1360869876221,
70.8921947571121));
#204450=CARTESIAN_POINT('Ctrl Pts',(-53.9452141595788,-73.0574520151227,
69.7520446546323));
#204451=CARTESIAN_POINT('Ctrl Pts',(-53.9596908591394,-73.060116320017,
69.2447001582753));
#204452=CARTESIAN_POINT('Ctrl Pts',(-53.9911563796819,-73.1483514527247,
68.1352280525231));
#204453=CARTESIAN_POINT('Ctrl Pts',(-54.0078860100975,-73.2499536620984,
67.5362743482051));
#204454=CARTESIAN_POINT('Ctrl Pts',(-54.0538873493735,-73.6666986665519,
65.9486543020002));
#204455=CARTESIAN_POINT('Ctrl Pts',(-54.0835374881285,-74.0796424871106,
64.9930500366725));
#204456=CARTESIAN_POINT('Ctrl Pts',(-54.1216000517381,-74.8031229615294,
63.8367233665558));
#204457=CARTESIAN_POINT('Ctrl Pts',(-54.1307538091373,-74.9909046909345,
63.5664443345819));
#204458=CARTESIAN_POINT('Ctrl Pts',(-54.1695655229798,-75.835137602131,
62.4681159636899));
#204459=CARTESIAN_POINT('Ctrl Pts',(-54.199814925981,-76.604543554259,61.7351064166373));
#204460=CARTESIAN_POINT('Ctrl Pts',(-54.2384870978,-77.7431291443887,60.9445863880131));
#204461=CARTESIAN_POINT('Ctrl Pts',(-54.2476655873979,-78.0228892527884,
60.7697177274664));
#204462=CARTESIAN_POINT('Ctrl Pts',(-54.275819493118,-78.8993382745417,
60.2790031422139));
#204463=CARTESIAN_POINT('Ctrl Pts',(-54.2950191884045,-79.5191976094664,
60.0083099722502));
#204464=CARTESIAN_POINT('Ctrl Pts',(-54.3333466588036,-80.803899112053,
59.5924195242559));
#204465=CARTESIAN_POINT('Ctrl Pts',(-54.3520059209203,-81.4656598308053,
59.4483995778347));
#204466=CARTESIAN_POINT('Ctrl Pts',(-54.3898335992285,-82.8072553351873,
59.292751143846));
#204467=CARTESIAN_POINT('Ctrl Pts',(-54.4090163993889,-83.4837877804349,
59.281383272417));
#204468=CARTESIAN_POINT('Ctrl Pts',(-54.4639581430243,-85.4117236740045,
59.4396240734754));
#204469=CARTESIAN_POINT('Ctrl Pts',(-54.4983910906639,-86.6372735668571,
59.7731223727129));
#204470=CARTESIAN_POINT('Ctrl Pts',(-54.5726681292479,-88.98890674642,60.9075822236667));
#204471=CARTESIAN_POINT('Ctrl Pts',(-54.6095885006169,-90.0781160339654,
61.7298248074316));
#204472=CARTESIAN_POINT('Ctrl Pts',(-54.6864723593932,-91.8744273761514,
63.749145864274));
#204473=CARTESIAN_POINT('Ctrl Pts',(-54.7233852421897,-92.5640450374486,
64.9263287131589));
#204474=CARTESIAN_POINT('Ctrl Pts',(-54.7712204353895,-93.113501112805,
66.5157418434284));
#204475=CARTESIAN_POINT('Ctrl Pts',(-54.7806358196329,-93.2063305295844,
66.8332160469199));
#204476=CARTESIAN_POINT('Ctrl Pts',(-54.8032919823625,-93.3944761228066,
67.6152358256552));
#204477=CARTESIAN_POINT('Ctrl Pts',(-54.8164128915059,-93.4732278824495,
68.0829828651234));
#204478=CARTESIAN_POINT('Ctrl Pts',(-54.8568831913935,-93.6141114685972,
69.5234256761779));
#204479=CARTESIAN_POINT('Ctrl Pts',(-54.8847845352893,-93.5703528386626,
70.5009228320982));
#204480=CARTESIAN_POINT('Ctrl Pts',(-54.9256171947155,-93.299580095652,
71.9322540715961));
#204481=CARTESIAN_POINT('Ctrl Pts',(-54.9390015578452,-93.1763120124036,
72.4000628234908));
#204482=CARTESIAN_POINT('Ctrl Pts',(-54.9664446175706,-92.8606052411454,
73.326831632913));
#204483=CARTESIAN_POINT('Ctrl Pts',(-54.9804793163858,-92.6668492605553,
73.7840084525099));
#204484=CARTESIAN_POINT('Ctrl Pts',(-54.9945874883696,-92.4407690432347,
74.2253573558264));
#204485=CARTESIAN_POINT('Ctrl Pts',(-55.2458788381492,-73.8447192625517,
73.4662010433421));
#204486=CARTESIAN_POINT('Ctrl Pts',(-55.2297528696875,-74.0655340732995,
74.0006591869956));
#204487=CARTESIAN_POINT('Ctrl Pts',(-55.2135935927371,-74.3311972775467,
74.5155097397992));
#204488=CARTESIAN_POINT('Ctrl Pts',(-55.183301353506,-74.8996943264174,
75.4203468553558));
#204489=CARTESIAN_POINT('Ctrl Pts',(-55.1692882837076,-75.1899507473671,
75.81621473778));
#204490=CARTESIAN_POINT('Ctrl Pts',(-55.1461364105071,-75.7217303075469,
76.4419764121167));
#204491=CARTESIAN_POINT('Ctrl Pts',(-55.1369251615355,-75.9481322718447,
76.6836385079598));
#204492=CARTESIAN_POINT('Ctrl Pts',(-55.090006389838,-77.1564578517171,
77.8542969941396));
#204493=CARTESIAN_POINT('Ctrl Pts',(-55.0515322837808,-78.3035517458425,
78.5934851025729));
#204494=CARTESIAN_POINT('Ctrl Pts',(-54.9792274053784,-80.7159449267234,
79.54388110746));
#204495=CARTESIAN_POINT('Ctrl Pts',(-54.9438092074083,-81.9440597031267,
79.7853203004272));
#204496=CARTESIAN_POINT('Ctrl Pts',(-54.89027037167,-83.8602625554975,79.8101225522134));
#204497=CARTESIAN_POINT('Ctrl Pts',(-54.8715308620345,-84.534374830482,
79.7521743592111));
#204498=CARTESIAN_POINT('Ctrl Pts',(-54.835980245164,-85.7685029902784,
79.5219286684053));
#204499=CARTESIAN_POINT('Ctrl Pts',(-54.8193640330692,-86.3290526933151,
79.367190176599));
#204500=CARTESIAN_POINT('Ctrl Pts',(-54.7840781959813,-87.5074927108403,
78.9313593608611));
#204501=CARTESIAN_POINT('Ctrl Pts',(-54.7654199970558,-88.116753108433,
78.6347357161773));
#204502=CARTESIAN_POINT('Ctrl Pts',(-54.7254516240248,-89.3235904518117,
77.8916193892214));
#204503=CARTESIAN_POINT('Ctrl Pts',(-54.7041942197188,-89.9107924539841,
77.4356074635136));
#204504=CARTESIAN_POINT('Ctrl Pts',(-54.6696585841749,-90.7969186263016,
76.5786314889983));
#204505=CARTESIAN_POINT('Ctrl Pts',(-54.6560407988341,-91.1251485086316,
76.2120331897269));
#204506=CARTESIAN_POINT('Ctrl Pts',(-54.624771622307,-91.8070700324784,
75.3303838982876));
#204507=CARTESIAN_POINT('Ctrl Pts',(-54.6070471573018,-92.1425801188347,
74.8037196308037));
#204508=CARTESIAN_POINT('Ctrl Pts',(-54.5714386598732,-92.717120542965,
73.6895063011282));
#204509=CARTESIAN_POINT('Ctrl Pts',(-54.5539604063772,-92.9537503793338,
73.1036848450657));
#204510=CARTESIAN_POINT('Ctrl Pts',(-54.5180538921639,-93.3231649468449,
71.8733423618886));
#204511=CARTESIAN_POINT('Ctrl Pts',(-54.4995542665266,-93.4508684858144,
71.2302749514709));
#204512=CARTESIAN_POINT('Ctrl Pts',(-54.4495299901436,-93.6271087478463,
69.4805027022376));
#204513=CARTESIAN_POINT('Ctrl Pts',(-54.4193034082145,-93.5594452055571,
68.370856821029));
#204514=CARTESIAN_POINT('Ctrl Pts',(-54.3720253945435,-93.1916543097974,
66.7428817075923));
#204515=CARTESIAN_POINT('Ctrl Pts',(-54.3558699902278,-93.0219857585303,
66.2034796354675));
#204516=CARTESIAN_POINT('Ctrl Pts',(-54.3255956470203,-92.6149618668774,
65.2056719483687));
#204517=CARTESIAN_POINT('Ctrl Pts',(-54.3113954907581,-92.3857452384584,
64.7457714800481));
#204518=CARTESIAN_POINT('Ctrl Pts',(-54.2704420897157,-91.6377007500768,
63.4905370973475));
#204519=CARTESIAN_POINT('Ctrl Pts',(-54.2432415288258,-91.0416890949028,
62.7473696885035));
#204520=CARTESIAN_POINT('Ctrl Pts',(-54.1978552987443,-89.8614061132386,
61.6338059550811));
#204521=CARTESIAN_POINT('Ctrl Pts',(-54.1791614739977,-89.3262307344683,
61.220439620894));
#204522=CARTESIAN_POINT('Ctrl Pts',(-54.15073098846,-88.4740913422993,60.6873304216285));
#204523=CARTESIAN_POINT('Ctrl Pts',(-54.1413258110868,-88.1855274474128,
60.5256647389317));
#204524=CARTESIAN_POINT('Ctrl Pts',(-54.1063868463423,-87.0860231827504,
59.9777549500284));
#204525=CARTESIAN_POINT('Ctrl Pts',(-54.0816698923603,-86.2332398533938,
59.684610714934));
#204526=CARTESIAN_POINT('Ctrl Pts',(-54.0333045512917,-84.5483186723791,
59.3432627791053));
#204527=CARTESIAN_POINT('Ctrl Pts',(-54.0097425891856,-83.7267279618335,
59.2775227600617));
#204528=CARTESIAN_POINT('Ctrl Pts',(-53.9731695174769,-82.4213334318633,
59.3300217190208));
#204529=CARTESIAN_POINT('Ctrl Pts',(-53.9597184654046,-81.9385320176203,
59.3839162936977));
#204530=CARTESIAN_POINT('Ctrl Pts',(-53.9265872639273,-80.7775262929086,
59.5977546904946));
#204531=CARTESIAN_POINT('Ctrl Pts',(-53.906747086961,-80.1082752639565,
59.7929671092526));
#204532=CARTESIAN_POINT('Ctrl Pts',(-53.8775898556133,-79.1541777096603,
60.1801230406874));
#204533=CARTESIAN_POINT('Ctrl Pts',(-53.8682463598381,-78.8507238093768,
60.320911537634));
#204534=CARTESIAN_POINT('Ctrl Pts',(-53.8411009154114,-77.9889598507366,
60.773190208319));
#204535=CARTESIAN_POINT('Ctrl Pts',(-53.8232780385363,-77.4522311778858,
61.1223459295986));
#204536=CARTESIAN_POINT('Ctrl Pts',(-53.7910712531785,-76.5622674900813,
61.8276764044678));
#204537=CARTESIAN_POINT('Ctrl Pts',(-53.7768719459693,-76.1959593877359,
62.1640513327241));
#204538=CARTESIAN_POINT('Ctrl Pts',(-53.7438427134036,-75.3914487368743,
63.0184756185197));
#204539=CARTESIAN_POINT('Ctrl Pts',(-53.7251832600842,-74.9773718025744,
63.5560568101502));
#204540=CARTESIAN_POINT('Ctrl Pts',(-53.6910623784577,-74.3366115978245,
64.5841032757758));
#204541=CARTESIAN_POINT('Ctrl Pts',(-53.6758314458016,-74.0898149296533,
65.0590998480982));
#204542=CARTESIAN_POINT('Ctrl Pts',(-53.6338431539426,-73.5124670231051,
66.4208153637462));
#204543=CARTESIAN_POINT('Ctrl Pts',(-53.6079792363515,-73.2657260226396,
67.3372712664529));
#204544=CARTESIAN_POINT('Ctrl Pts',(-53.5631322461169,-73.068023389348,
68.9108519644783));
#204545=CARTESIAN_POINT('Ctrl Pts',(-53.5447588669558,-73.0479750547569,
69.553312848836));
#204546=CARTESIAN_POINT('Ctrl Pts',(-53.5126853145242,-73.1194954370545,
70.69441226386));
#204547=CARTESIAN_POINT('Ctrl Pts',(-53.4987850519446,-73.1876555209855,
71.1924183709513));
#204548=CARTESIAN_POINT('Ctrl Pts',(-53.4672275747629,-73.4216606742602,
72.2932815615116));
#204549=CARTESIAN_POINT('Ctrl Pts',(-53.4495081762787,-73.6066644662848,
72.8900153957329));
#204550=CARTESIAN_POINT('Ctrl Pts',(-53.4317936414903,-73.844719260035,
73.4662010372508));
#204551=CARTESIAN_POINT('Origin',(-45.8894114130409,-83.3180213346267,69.5522455184007));
#204552=CARTESIAN_POINT('',(-57.4656305641639,-73.8447192505465,73.4662010142849));
#204553=CARTESIAN_POINT('',(-57.0597576325586,-73.8447192590796,73.4662010349383));
#204554=CARTESIAN_POINT('',(-45.8894114130409,-73.8447192590796,73.4662010349383));
#204555=CARTESIAN_POINT('Ctrl Pts',(-55.6519493945588,-73.8447192590796,
73.4662010349383));
#204556=CARTESIAN_POINT('Ctrl Pts',(-55.6596548633805,-73.7410272723995,
73.2152259003247));
#204557=CARTESIAN_POINT('Ctrl Pts',(-55.6673089420921,-73.6472380756339,
72.9599589662023));
#204558=CARTESIAN_POINT('Ctrl Pts',(-55.693783075687,-73.3563706209773,
72.0588877901198));
#204559=CARTESIAN_POINT('Ctrl Pts',(-55.7124900378615,-73.2130079057446,
71.3979008056047));
#204560=CARTESIAN_POINT('Ctrl Pts',(-55.7490543465984,-73.0648169282569,
70.1141264021171));
#204561=CARTESIAN_POINT('Ctrl Pts',(-55.7667415433354,-73.0495893992716,
69.4954674524715));
#204562=CARTESIAN_POINT('Ctrl Pts',(-55.7982479286604,-73.1233063252767,
68.3752183108468));
#204563=CARTESIAN_POINT('Ctrl Pts',(-55.8122316879438,-73.1936777975706,
67.8743663203349));
#204564=CARTESIAN_POINT('Ctrl Pts',(-55.8465381892149,-73.4529159797878,
66.6784751248108));
#204565=CARTESIAN_POINT('Ctrl Pts',(-55.8670281966967,-73.6785787543878,
65.9941580673973));
#204566=CARTESIAN_POINT('Ctrl Pts',(-55.8968590589922,-74.1114591169312,
65.034098859896));
#204567=CARTESIAN_POINT('Ctrl Pts',(-55.9062138364164,-74.2638300519005,
64.7360168915535));
#204568=CARTESIAN_POINT('Ctrl Pts',(-55.9336509373363,-74.7538575094382,
63.8831286030609));
#204569=CARTESIAN_POINT('Ctrl Pts',(-55.951753234742,-75.1299332157745,
63.3523266230311));
#204570=CARTESIAN_POINT('Ctrl Pts',(-55.9884629980572,-75.9748276848023,
62.3719812270974));
#204571=CARTESIAN_POINT('Ctrl Pts',(-56.0068615798354,-76.4411920836949,
61.9241444889541));
#204572=CARTESIAN_POINT('Ctrl Pts',(-56.0437401783078,-77.4752970866365,
61.1035355941262));
#204573=CARTESIAN_POINT('Ctrl Pts',(-56.0624840712685,-78.0441979459242,
60.7372066610557));
#204574=CARTESIAN_POINT('Ctrl Pts',(-56.0979096502699,-79.1575194967214,
60.1669181507204));
#204575=CARTESIAN_POINT('Ctrl Pts',(-56.1143937075693,-79.691291249844,
59.948028732579));
#204576=CARTESIAN_POINT('Ctrl Pts',(-56.1495554039872,-80.8854448912311,
59.5721617095557));
#204577=CARTESIAN_POINT('Ctrl Pts',(-56.1682134633932,-81.5487757186324,
59.4334867485));
#204578=CARTESIAN_POINT('Ctrl Pts',(-56.2016707642748,-82.7284245294484,
59.3064939682056));
#204579=CARTESIAN_POINT('Ctrl Pts',(-56.2162221770782,-83.2393039312188,
59.2898458278949));
#204580=CARTESIAN_POINT('Ctrl Pts',(-56.2572368274195,-84.6830704364769,
59.3506456915793));
#204581=CARTESIAN_POINT('Ctrl Pts',(-56.2828304154574,-85.6070970828485,
59.517499285441));
#204582=CARTESIAN_POINT('Ctrl Pts',(-56.3275371032007,-87.1103919978489,
60.0076922478935));
#204583=CARTESIAN_POINT('Ctrl Pts',(-56.3460612710478,-87.7047786737991,
60.2658608219851));
#204584=CARTESIAN_POINT('Ctrl Pts',(-56.378260555719,-88.7097868041539,
60.8205394610542));
#204585=CARTESIAN_POINT('Ctrl Pts',(-56.3921434363624,-89.1303370186752,
61.094656321998));
#204586=CARTESIAN_POINT('Ctrl Pts',(-56.4154357382099,-89.7911270975001,
61.5980097340351));
#204587=CARTESIAN_POINT('Ctrl Pts',(-56.4247243732342,-90.0433431070999,
61.8100875413661));
#204588=CARTESIAN_POINT('Ctrl Pts',(-56.452214235767,-90.754116528576,62.4687302659228));
#204589=CARTESIAN_POINT('Ctrl Pts',(-56.4704556899168,-91.1815977372855,
62.9464992597366));
#204590=CARTESIAN_POINT('Ctrl Pts',(-56.5071829360745,-91.9628756085017,
64.0038582558589));
#204591=CARTESIAN_POINT('Ctrl Pts',(-56.525925414791,-92.3093942268284,
64.5850212040973));
#204592=CARTESIAN_POINT('Ctrl Pts',(-56.5613911435208,-92.8416373612569,
65.7186337167351));
#204593=CARTESIAN_POINT('Ctrl Pts',(-56.5779176350843,-93.0424188895371,
66.2610542810256));
#204594=CARTESIAN_POINT('Ctrl Pts',(-56.6084856298555,-93.332806991791,
67.3099887600299));
#204595=CARTESIAN_POINT('Ctrl Pts',(-56.6226291267961,-93.4321298310447,
67.811998230913));
#204596=CARTESIAN_POINT('Ctrl Pts',(-56.6548144418948,-93.5702521925257,
68.9519470315959));
#204597=CARTESIAN_POINT('Ctrl Pts',(-56.6729236665936,-93.5877404272269,
69.5903449546178));
#204598=CARTESIAN_POINT('Ctrl Pts',(-56.7089675415116,-93.5043286909993,
70.8561658371274));
#204599=CARTESIAN_POINT('Ctrl Pts',(-56.7264852422334,-93.4047065420545,
71.4809369788909));
#204600=CARTESIAN_POINT('Ctrl Pts',(-56.762454721504,-93.0856878741423,
72.7279953005713));
#204601=CARTESIAN_POINT('Ctrl Pts',(-56.78099231533,-92.8625183377958,73.3463538705992));
#204602=CARTESIAN_POINT('Ctrl Pts',(-56.8380957305256,-92.0033788889631,
75.1605993844289));
#204603=CARTESIAN_POINT('Ctrl Pts',(-56.8750159211701,-91.1890365629882,
76.2556911510731));
#204604=CARTESIAN_POINT('Ctrl Pts',(-56.9394218654422,-89.5083996664527,
77.7726051826705));
#204605=CARTESIAN_POINT('Ctrl Pts',(-56.9646156137638,-88.7524208614728,
78.2908043918305));
#204606=CARTESIAN_POINT('Ctrl Pts',(-57.0145463896372,-87.1660224735993,
79.0917971309653));
#204607=CARTESIAN_POINT('Ctrl Pts',(-57.0393569399326,-86.3479398257574,
79.3822892230226));
#204608=CARTESIAN_POINT('Ctrl Pts',(-57.0824456155048,-84.8436188663561,
79.7105293118066));
#204609=CARTESIAN_POINT('Ctrl Pts',(-57.1011387504411,-84.1714940580514,
79.7889326366568));
#204610=CARTESIAN_POINT('Ctrl Pts',(-57.1385945747034,-82.8468398370674,
79.8120090611029));
#204611=CARTESIAN_POINT('Ctrl Pts',(-57.1572119729289,-82.1975152551376,
79.7615175035752));
#204612=CARTESIAN_POINT('Ctrl Pts',(-57.1894891839894,-81.0638680605308,
79.5638499525962));
#204613=CARTESIAN_POINT('Ctrl Pts',(-57.2033614830846,-80.5773546512452,
79.4417439633923));
#204614=CARTESIAN_POINT('Ctrl Pts',(-57.237438190015,-79.4234850655456,
79.0604173874403));
#204615=CARTESIAN_POINT('Ctrl Pts',(-57.2578090455034,-78.7705347652535,
78.7659901996338));
#204616=CARTESIAN_POINT('Ctrl Pts',(-57.294600414176,-77.6485276573791,
78.1115176796365));
#204617=CARTESIAN_POINT('Ctrl Pts',(-57.3107631445904,-77.1696568020812,
77.7742837679813));
#204618=CARTESIAN_POINT('Ctrl Pts',(-57.3555562978816,-75.9440543266112,
76.7439374202992));
#204619=CARTESIAN_POINT('Ctrl Pts',(-57.3847050625789,-75.2675824966305,
75.9776838207498));
#204620=CARTESIAN_POINT('Ctrl Pts',(-57.4306208441241,-74.3748318537071,
74.5993556208464));
#204621=CARTESIAN_POINT('Ctrl Pts',(-57.4479646014832,-74.0835506812208,
74.0442664246711));
#204622=CARTESIAN_POINT('Ctrl Pts',(-57.4656305635332,-73.8447192505397,
73.4662010142684));
#204623=CARTESIAN_POINT('',(-56.402691677048,-92.4407740768623,74.2253475292745));
#204624=CARTESIAN_POINT('Ctrl Pts',(-56.402691677048,-92.4407740768623,
74.2253475292745));
#204625=CARTESIAN_POINT('Ctrl Pts',(-56.3905033769764,-92.6400598197725,
73.8363051857964));
#204626=CARTESIAN_POINT('Ctrl Pts',(-56.3782950668991,-92.8142542880859,
73.434915401122));
#204627=CARTESIAN_POINT('Ctrl Pts',(-56.3538404997768,-93.1075649334602,
72.6200352877034));
#204628=CARTESIAN_POINT('Ctrl Pts',(-56.3416239456816,-93.2273594088019,
72.2077141799071));
#204629=CARTESIAN_POINT('Ctrl Pts',(-56.3064251645048,-93.4976065211303,
70.9992048619457));
#204630=CARTESIAN_POINT('Ctrl Pts',(-56.2841306774455,-93.5800601632956,
70.1911577827392));
#204631=CARTESIAN_POINT('Ctrl Pts',(-56.2462056610967,-93.5576184697801,
68.8413324644591));
#204632=CARTESIAN_POINT('Ctrl Pts',(-56.2308430996121,-93.5058840444699,
68.3023686440525));
#204633=CARTESIAN_POINT('Ctrl Pts',(-56.1861214976241,-93.2323654622646,
66.7532673876798));
#204634=CARTESIAN_POINT('Ctrl Pts',(-56.1578623953141,-92.9002472360519,
65.7694620125991));
#204635=CARTESIAN_POINT('Ctrl Pts',(-56.1193148260535,-92.2756548246651,
64.5590576078324));
#204636=CARTESIAN_POINT('Ctrl Pts',(-56.1099340714407,-92.1104824250455,
64.2736330038756));
#204637=CARTESIAN_POINT('Ctrl Pts',(-56.0706362546844,-91.3614570484951,
63.1122829809782));
#204638=CARTESIAN_POINT('Ctrl Pts',(-56.0418346173385,-90.6582563846677,
62.3209985596782));
#204639=CARTESIAN_POINT('Ctrl Pts',(-55.9952001354449,-89.3883262034003,
61.2716708088244));
#204640=CARTESIAN_POINT('Ctrl Pts',(-55.9781648862883,-88.8975221472293,
60.9333305046939));
#204641=CARTESIAN_POINT('Ctrl Pts',(-55.9471894467687,-87.9381682201456,
60.3884524901742));
#204642=CARTESIAN_POINT('Ctrl Pts',(-55.9331194762118,-87.4781282173937,
60.1706478673319));
#204643=CARTESIAN_POINT('Ctrl Pts',(-55.9010251811469,-86.4097959957748,
59.7589459962414));
#204644=CARTESIAN_POINT('Ctrl Pts',(-55.8829313028535,-85.7957245889421,
59.5858640933454));
#204645=CARTESIAN_POINT('Ctrl Pts',(-55.8469130984081,-84.5488417933286,
59.3568591162553));
#204646=CARTESIAN_POINT('Ctrl Pts',(-55.829404124793,-83.9188942874507,
59.3004272451562));
#204647=CARTESIAN_POINT('Ctrl Pts',(-55.7934480639542,-82.6322366741683,
59.3042251232283));
#204648=CARTESIAN_POINT('Ctrl Pts',(-55.7749181977989,-81.9784073585776,
59.3690416053286));
#204649=CARTESIAN_POINT('Ctrl Pts',(-55.7178274654666,-80.0093521796394,
59.7572670969582));
#204650=CARTESIAN_POINT('Ctrl Pts',(-55.6809086679753,-78.7481366318407,
60.2783551802272));
#204651=CARTESIAN_POINT('Ctrl Pts',(-55.6097089193793,-76.6669921704943,
61.6685973025684));
#204652=CARTESIAN_POINT('Ctrl Pts',(-55.5781944556113,-75.8241727682959,
62.464908313525));
#204653=CARTESIAN_POINT('Ctrl Pts',(-55.5315078954419,-74.832900228938,
63.7806558257333));
#204654=CARTESIAN_POINT('Ctrl Pts',(-55.5173291291132,-74.5635846023956,
64.1979608868738));
#204655=CARTESIAN_POINT('Ctrl Pts',(-55.4940067945626,-74.16665515639,64.9235733410436));
#204656=CARTESIAN_POINT('Ctrl Pts',(-55.4847913851266,-74.0219336784218,
65.2215567936392));
#204657=CARTESIAN_POINT('Ctrl Pts',(-55.4378676907604,-73.3610031428395,
66.7689170716168));
#204658=CARTESIAN_POINT('Ctrl Pts',(-55.399391064315,-73.0811505043503,
68.1046266887717));
#204659=CARTESIAN_POINT('Ctrl Pts',(-55.3240281637205,-73.0557992009588,
70.8070225842464));
#204660=CARTESIAN_POINT('Ctrl Pts',(-55.2855668439352,-73.3103358396947,
72.1472223742944));
#204661=CARTESIAN_POINT('Ctrl Pts',(-55.2472197563395,-73.826436129375,
73.4217271981451));
#204662=CARTESIAN_POINT('Ctrl Pts',(-55.2465492717017,-73.8355389359018,
73.4439810648777));
#204663=CARTESIAN_POINT('Ctrl Pts',(-55.2458788381492,-73.8447192625517,
73.4662010433421));
#204664=CARTESIAN_POINT('Ctrl Pts',(-57.0597576325586,-73.8447192590796,
73.4662010349383));
#204665=CARTESIAN_POINT('Ctrl Pts',(-57.0383631309816,-74.1368641142954,
74.173305766094));
#204666=CARTESIAN_POINT('Ctrl Pts',(-57.017120994494,-74.5075970143452,
74.8462899755402));
#204667=CARTESIAN_POINT('Ctrl Pts',(-56.9775517730568,-75.3131405065833,
75.9848714513742));
#204668=CARTESIAN_POINT('Ctrl Pts',(-56.9596411120092,-75.7221508602249,
76.4630748477586));
#204669=CARTESIAN_POINT('Ctrl Pts',(-56.9262735382076,-76.5782428806903,
77.2955277986793));
#204670=CARTESIAN_POINT('Ctrl Pts',(-56.9105628863771,-77.0161437030378,
77.6559096055087));
#204671=CARTESIAN_POINT('Ctrl Pts',(-56.8692274112796,-78.2210699328814,
78.49052611963));
#204672=CARTESIAN_POINT('Ctrl Pts',(-56.8435370700548,-79.0248178896983,
78.9031918397772));
#204673=CARTESIAN_POINT('Ctrl Pts',(-56.8002362825214,-80.4868816128833,
79.4251031806845));
#204674=CARTESIAN_POINT('Ctrl Pts',(-56.782023377819,-81.1212594724405,
79.5853357798321));
#204675=CARTESIAN_POINT('Ctrl Pts',(-56.7456291264912,-82.3892565663906,
79.7795008913734));
#204676=CARTESIAN_POINT('Ctrl Pts',(-56.7276633061683,-83.0194376518196,
79.8172453346938));
#204677=CARTESIAN_POINT('Ctrl Pts',(-56.6910944083757,-84.3275691096218,
79.7749717110202));
#204678=CARTESIAN_POINT('Ctrl Pts',(-56.6722514824881,-85.0021935016001,
79.6856989908197));
#204679=CARTESIAN_POINT('Ctrl Pts',(-56.6380194886854,-86.1789920181178,
79.4091352178211));
#204680=CARTESIAN_POINT('Ctrl Pts',(-56.6228592144546,-86.6847766798411,
79.2480375883778));
#204681=CARTESIAN_POINT('Ctrl Pts',(-56.5944086671809,-87.6200748728344,
78.8680794275189));
#204682=CARTESIAN_POINT('Ctrl Pts',(-56.5811308970273,-88.0511129218097,
78.6566551578047));
#204683=CARTESIAN_POINT('Ctrl Pts',(-56.5404818101695,-89.3082340958285,
77.9265516464997));
#204684=CARTESIAN_POINT('Ctrl Pts',(-56.5125613702138,-90.0766500260617,
77.3196503160365));
#204685=CARTESIAN_POINT('Ctrl Pts',(-56.4717017702708,-91.0808193787086,
76.2630686063062));
#204686=CARTESIAN_POINT('Ctrl Pts',(-56.4583111596744,-91.3886321735106,
75.8895496120529));
#204687=CARTESIAN_POINT('Ctrl Pts',(-56.4308548308858,-91.9566231006264,
75.0914887461845));
#204688=CARTESIAN_POINT('Ctrl Pts',(-56.4168131368927,-92.2145804213453,
74.6669190743884));
#204689=CARTESIAN_POINT('Ctrl Pts',(-56.4026978510105,-92.4407741543022,
74.2253473780977));
#204690=CARTESIAN_POINT('Origin',(-45.8894114130409,-83.3180213346267,69.5522455184007));
#204691=CARTESIAN_POINT('',(-59.2798347108578,-73.8447192567251,73.4662010292395));
#204692=CARTESIAN_POINT('',(-58.8740778711611,-73.8447192590796,73.4662010349383));
#204693=CARTESIAN_POINT('',(-45.8894114130409,-73.8447192590796,73.4662010349383));
#204694=CARTESIAN_POINT('Ctrl Pts',(-57.4656305635332,-73.8447192505397,
73.4662010142684));
#204695=CARTESIAN_POINT('Ctrl Pts',(-57.467015475443,-73.8259962117467,
73.4208839424198));
#204696=CARTESIAN_POINT('Ctrl Pts',(-57.4684018447326,-73.8075955063203,
73.3754256525906));
#204697=CARTESIAN_POINT('Ctrl Pts',(-57.4791268020266,-73.6678971821377,
73.0230533866649));
#204698=CARTESIAN_POINT('Ctrl Pts',(-57.4885180167998,-73.5611619934532,
72.7105833747677));
#204699=CARTESIAN_POINT('Ctrl Pts',(-57.523407156596,-73.2210881588465,
71.531826866936));
#204700=CARTESIAN_POINT('Ctrl Pts',(-57.548081453985,-73.0866520074193,
70.6412316611888));
#204701=CARTESIAN_POINT('Ctrl Pts',(-57.5888899414059,-73.0594451953212,
69.1913900793089));
#204702=CARTESIAN_POINT('Ctrl Pts',(-57.6046512373244,-73.0938694204248,
68.6382921288233));
#204703=CARTESIAN_POINT('Ctrl Pts',(-57.6381300257707,-73.2620038171208,
67.4712027258487));
#204704=CARTESIAN_POINT('Ctrl Pts',(-57.6554659852384,-73.4078004036538,
66.8611954226435));
#204705=CARTESIAN_POINT('Ctrl Pts',(-57.6912072348374,-73.8173648043539,
65.6502278125564));
#204706=CARTESIAN_POINT('Ctrl Pts',(-57.7096703600775,-74.0849436597277,
65.0535258942587));
#204707=CARTESIAN_POINT('Ctrl Pts',(-57.7592658896886,-74.9467254860372,
63.5377100424494));
#204708=CARTESIAN_POINT('Ctrl Pts',(-57.7891281575565,-75.6340776115638,
62.6812739247584));
#204709=CARTESIAN_POINT('Ctrl Pts',(-57.8362286935468,-76.8675816802812,
61.5659286950294));
#204710=CARTESIAN_POINT('Ctrl Pts',(-57.8525941770391,-77.3230367740463,
61.2186032227383));
#204711=CARTESIAN_POINT('Ctrl Pts',(-57.8830343508329,-78.2366472048036,
60.635732430482));
#204712=CARTESIAN_POINT('Ctrl Pts',(-57.8972020710319,-78.6882446648011,
60.3931112276017));
#204713=CARTESIAN_POINT('Ctrl Pts',(-57.9294173301977,-79.7386233211922,
59.9264068339872));
#204714=CARTESIAN_POINT('Ctrl Pts',(-57.9475315653165,-80.3440470263072,
59.7224783147016));
#204715=CARTESIAN_POINT('Ctrl Pts',(-57.9835838838406,-81.5789840879344,
59.431134072273));
#204716=CARTESIAN_POINT('Ctrl Pts',(-58.0011045048751,-82.2055797286569,
59.3432482787389));
#204717=CARTESIAN_POINT('Ctrl Pts',(-58.0370784200417,-83.491556625581,
59.2827403410888));
#204718=CARTESIAN_POINT('Ctrl Pts',(-58.0556185294284,-84.1482869379266,
59.3148877030279));
#204719=CARTESIAN_POINT('Ctrl Pts',(-58.1127259893701,-86.1347912884453,
59.6046365093555));
#204720=CARTESIAN_POINT('Ctrl Pts',(-58.1496465648296,-87.4204709874273,
60.0623024090173));
#204721=CARTESIAN_POINT('Ctrl Pts',(-58.2140602109242,-89.3635408703946,
61.2247457987552));
#204722=CARTESIAN_POINT('Ctrl Pts',(-58.2392619101364,-90.0807132733979,
61.7958566462899));
#204723=CARTESIAN_POINT('Ctrl Pts',(-58.289212135638,-91.3118471784145,
63.078474596357));
#204724=CARTESIAN_POINT('Ctrl Pts',(-58.3140360354744,-91.8295124567072,
63.7759588220253));
#204725=CARTESIAN_POINT('Ctrl Pts',(-58.3571375745626,-92.5841413592949,
65.1186017192531));
#204726=CARTESIAN_POINT('Ctrl Pts',(-58.3758307916147,-92.8559443419004,
65.7382969424522));
#204727=CARTESIAN_POINT('Ctrl Pts',(-58.4132835267388,-93.2659095571014,
66.9980073250782));
#204728=CARTESIAN_POINT('Ctrl Pts',(-58.4318976573724,-93.4077773086004,
67.6335361596171));
#204729=CARTESIAN_POINT('Ctrl Pts',(-58.4641721348258,-93.5507993058548,
68.7752647657367));
#204730=CARTESIAN_POINT('Ctrl Pts',(-58.4780448026798,-93.5765425307035,
69.2762201526045));
#204731=CARTESIAN_POINT('Ctrl Pts',(-58.501263199602,-93.5583826674336,
70.1040382693334));
#204732=CARTESIAN_POINT('Ctrl Pts',(-58.5104876105466,-93.5355624150462,
70.4304981763666));
#204733=CARTESIAN_POINT('Ctrl Pts',(-58.5334900665776,-93.4403878401189,
71.2357751792268));
#204734=CARTESIAN_POINT('Ctrl Pts',(-58.547318724833,-93.3496548816368,
71.7116215901034));
#204735=CARTESIAN_POINT('Ctrl Pts',(-58.574536530198,-93.1018985141553,
72.6460147409128));
#204736=CARTESIAN_POINT('Ctrl Pts',(-58.587905219172,-92.9453145061345,
73.1034273015737));
#204737=CARTESIAN_POINT('Ctrl Pts',(-58.6188859134196,-92.5135392729312,
74.1233723398468));
#204738=CARTESIAN_POINT('Ctrl Pts',(-58.6365653879551,-92.217926162049,
74.6751774283831));
#204739=CARTESIAN_POINT('Ctrl Pts',(-58.6927354152328,-91.1305436805013,
76.3234632986986));
#204740=CARTESIAN_POINT('Ctrl Pts',(-58.7296145133979,-90.1718171794844,
77.2924245070318));
#204741=CARTESIAN_POINT('Ctrl Pts',(-58.8064690912481,-87.932682125596,
78.803961807163));
#204742=CARTESIAN_POINT('Ctrl Pts',(-58.8433913931026,-86.6738345838654,
79.3311957990902));
#204743=CARTESIAN_POINT('Ctrl Pts',(-58.8912730138183,-85.0240359243524,
79.6647104567488));
#204744=CARTESIAN_POINT('Ctrl Pts',(-58.9007099114252,-84.6960500960934,
79.714601179362));
#204745=CARTESIAN_POINT('Ctrl Pts',(-58.9246479319649,-83.8492960797604,
79.8016496087255));
#204746=CARTESIAN_POINT('Ctrl Pts',(-58.9390230634141,-83.3290745763266,
79.8154039115205));
#204747=CARTESIAN_POINT('Ctrl Pts',(-58.983088324147,-81.7582657834689,
79.7374628040006));
#204748=CARTESIAN_POINT('Ctrl Pts',(-59.0132451352954,-80.7207744835811,
79.5234944201013));
#204749=CARTESIAN_POINT('Ctrl Pts',(-59.0518229434533,-79.4253578817725,
79.0400433472406));
#204750=CARTESIAN_POINT('Ctrl Pts',(-59.0609975786727,-79.1223001401009,
78.9099727851408));
#204751=CARTESIAN_POINT('Ctrl Pts',(-59.0991745160973,-77.8979093966226,
78.3130146836009));
#204752=CARTESIAN_POINT('Ctrl Pts',(-59.1287536206049,-77.0434672368736,
77.722843357872));
#204753=CARTESIAN_POINT('Ctrl Pts',(-59.1667441086209,-76.0522700704332,
76.7896127227359));
#204754=CARTESIAN_POINT('Ctrl Pts',(-59.175894985545,-75.8238468424815,
76.5528150534514));
#204755=CARTESIAN_POINT('Ctrl Pts',(-59.2147979782694,-74.90895439182,75.5081892250738));
#204756=CARTESIAN_POINT('Ctrl Pts',(-59.2451433370349,-74.3385626997602,
74.6074410487942));
#204757=CARTESIAN_POINT('Ctrl Pts',(-59.276419405404,-73.8919916490818,
73.5791817223545));
#204758=CARTESIAN_POINT('Ctrl Pts',(-59.2781271442497,-73.8681010896515,
73.522794203641));
#204759=CARTESIAN_POINT('Ctrl Pts',(-59.2798347108578,-73.8447192543706,
73.4662010235407));
#204760=CARTESIAN_POINT('Ctrl Pts',(-58.8740778711611,-73.8447192590796,
73.4662010349383));
#204761=CARTESIAN_POINT('Ctrl Pts',(-58.865480677016,-73.9616231644785,
73.7491541765811));
#204762=CARTESIAN_POINT('Ctrl Pts',(-58.8568298332965,-74.09121168495,74.0268880893285));
#204763=CARTESIAN_POINT('Ctrl Pts',(-58.8302237393543,-74.5252897744171,
74.8577555728255));
#204764=CARTESIAN_POINT('Ctrl Pts',(-58.8122496763533,-74.8684541002789,
75.3888023861618));
#204765=CARTESIAN_POINT('Ctrl Pts',(-58.7768679492777,-75.6511414097794,
76.3849489172506));
#204766=CARTESIAN_POINT('Ctrl Pts',(-58.7592049293814,-76.0897008063705,
76.8473303810519));
#204767=CARTESIAN_POINT('Ctrl Pts',(-58.7269131274484,-76.9486812697864,
77.5989544351491));
#204768=CARTESIAN_POINT('Ctrl Pts',(-58.7124707266324,-77.3531964397123,
77.9032261900877));
#204769=CARTESIAN_POINT('Ctrl Pts',(-58.6807977870372,-78.29566564173,78.5085980364354));
#204770=CARTESIAN_POINT('Ctrl Pts',(-58.6638417859424,-78.8416606190714,
78.7935930503238));
#204771=CARTESIAN_POINT('Ctrl Pts',(-58.627698835136,-80.0336530067509,
79.2852146576557));
#204772=CARTESIAN_POINT('Ctrl Pts',(-58.608496923001,-80.6812934670574,
79.4802570519605));
#204773=CARTESIAN_POINT('Ctrl Pts',(-58.5600660160198,-82.3557729216487,
79.8090010738735));
#204774=CARTESIAN_POINT('Ctrl Pts',(-58.5318567286296,-83.3923970656817,
79.8537709129494));
#204775=CARTESIAN_POINT('Ctrl Pts',(-58.4853312865826,-85.0232559252403,
79.6777124242945));
#204776=CARTESIAN_POINT('Ctrl Pts',(-58.4679508268199,-85.6213368974583,
79.558626364145));
#204777=CARTESIAN_POINT('Ctrl Pts',(-58.4380518470019,-86.646968988707,
79.2575264967924));
#204778=CARTESIAN_POINT('Ctrl Pts',(-58.42528094242,-87.0793893314218,79.0982647335386));
#204779=CARTESIAN_POINT('Ctrl Pts',(-58.3934235862151,-88.1159538346857,
78.6350881133373));
#204780=CARTESIAN_POINT('Ctrl Pts',(-58.3741823220147,-88.7035566415454,
78.2994838844307));
#204781=CARTESIAN_POINT('Ctrl Pts',(-58.3313046014104,-89.9366003987063,
77.4235995634658));
#204782=CARTESIAN_POINT('Ctrl Pts',(-58.3083313497893,-90.5573190559137,
76.8567902276832));
#204783=CARTESIAN_POINT('Ctrl Pts',(-58.2592872983452,-91.6885342963543,
75.5363384200497));
#204784=CARTESIAN_POINT('Ctrl Pts',(-58.2335590056109,-92.1820867856877,
74.777493662248));
#204785=CARTESIAN_POINT('Ctrl Pts',(-58.1901753773432,-92.8515860581853,
73.3734487086653));
#204786=CARTESIAN_POINT('Ctrl Pts',(-58.1719163428853,-93.0759736461244,
72.7573677826434));
#204787=CARTESIAN_POINT('Ctrl Pts',(-58.1354603489394,-93.398315423905,
71.5137992126148));
#204788=CARTESIAN_POINT('Ctrl Pts',(-58.1174903912482,-93.4998675695853,
70.8901716192675));
#204789=CARTESIAN_POINT('Ctrl Pts',(-58.0824142987632,-93.5867158206437,
69.6374893199529));
#204790=CARTESIAN_POINT('Ctrl Pts',(-58.0650557091113,-93.5728043262034,
69.0111571492715));
#204791=CARTESIAN_POINT('Ctrl Pts',(-58.033439441235,-93.446014573542,67.9001845679106));
#204792=CARTESIAN_POINT('Ctrl Pts',(-58.0193633296556,-93.3548473656371,
67.4150341783458));
#204793=CARTESIAN_POINT('Ctrl Pts',(-57.984896436781,-93.0444752203358,
66.2382037502742));
#204794=CARTESIAN_POINT('Ctrl Pts',(-57.964979096147,-92.7861597068894,
65.5596103650216));
#204795=CARTESIAN_POINT('Ctrl Pts',(-57.9256306149137,-92.1527470234762,
64.3113813617936));
#204796=CARTESIAN_POINT('Ctrl Pts',(-57.906324565792,-91.7881652191835,
63.7405605140367));
#204797=CARTESIAN_POINT('Ctrl Pts',(-57.8696146466932,-90.9849265731252,
62.7208107423569));
#204798=CARTESIAN_POINT('Ctrl Pts',(-57.8524474480341,-90.5560339049798,
62.2679395581874));
#204799=CARTESIAN_POINT('Ctrl Pts',(-57.816081258715,-89.5821851003058,
61.4111191668209));
#204800=CARTESIAN_POINT('Ctrl Pts',(-57.7968753902134,-89.0328908418219,
61.0165594991972));
#204801=CARTESIAN_POINT('Ctrl Pts',(-57.7495900455221,-87.5903056963919,
60.1824216424184));
#204802=CARTESIAN_POINT('Ctrl Pts',(-57.7224612188126,-86.6642607996665,
59.813216008457));
#204803=CARTESIAN_POINT('Ctrl Pts',(-57.6786930873766,-85.1618430352934,
59.4542952374702));
#204804=CARTESIAN_POINT('Ctrl Pts',(-57.662870210739,-84.6144877193528,
59.3695416427853));
#204805=CARTESIAN_POINT('Ctrl Pts',(-57.6318897240014,-83.5148596654779,
59.2894106959836));
#204806=CARTESIAN_POINT('Ctrl Pts',(-57.616694018074,-82.9644194841229,
59.29361524856));
#204807=CARTESIAN_POINT('Ctrl Pts',(-57.5823326533279,-81.7445440283663,
59.4012675295343));
#204808=CARTESIAN_POINT('Ctrl Pts',(-57.5630922550812,-81.0796192684715,
59.5268914182743));
#204809=CARTESIAN_POINT('Ctrl Pts',(-57.5200807259351,-79.6238649777219,
59.9540763863877));
#204810=CARTESIAN_POINT('Ctrl Pts',(-57.496981824707,-78.8481281168846,
60.2898647187717));
#204811=CARTESIAN_POINT('Ctrl Pts',(-57.4477592580867,-77.3440856523192,
61.1743283643562));
#204812=CARTESIAN_POINT('Ctrl Pts',(-57.42199881721,-76.6297843294988,61.7327245217374));
#204813=CARTESIAN_POINT('Ctrl Pts',(-57.3785501803015,-75.5392890057419,
62.845304764873));
#204814=CARTESIAN_POINT('Ctrl Pts',(-57.3602576970691,-75.1266074514152,
63.3560804893024));
#204815=CARTESIAN_POINT('Ctrl Pts',(-57.3237553788541,-74.4177483227882,
64.4291868520268));
#204816=CARTESIAN_POINT('Ctrl Pts',(-57.3057811167003,-74.1193365693104,
64.9866343142496));
#204817=CARTESIAN_POINT('Ctrl Pts',(-57.2703971876994,-73.6268660256079,
66.153940148766));
#204818=CARTESIAN_POINT('Ctrl Pts',(-57.252732005662,-73.4347273572782,
66.7616419920649));
#204819=CARTESIAN_POINT('Ctrl Pts',(-57.2204301539975,-73.1931212225111,
67.8775242147072));
#204820=CARTESIAN_POINT('Ctrl Pts',(-57.2059797441725,-73.1228285498709,
68.379072569883));
#204821=CARTESIAN_POINT('Ctrl Pts',(-57.1743559469827,-73.0498849447111,
69.4951367228938));
#204822=CARTESIAN_POINT('Ctrl Pts',(-57.1574534724381,-73.0648239198485,
70.1088705785681));
#204823=CARTESIAN_POINT('Ctrl Pts',(-57.1213672411522,-73.2111942817992,
71.3879527785283));
#204824=CARTESIAN_POINT('Ctrl Pts',(-57.1021665281674,-73.3539131345902,
72.0491045978209));
#204825=CARTESIAN_POINT('Ctrl Pts',(-57.07519652206,-73.6449321917794,72.9536791724396));
#204826=CARTESIAN_POINT('Ctrl Pts',(-57.0674445709045,-73.7397530610107,
73.2121418107528));
#204827=CARTESIAN_POINT('Ctrl Pts',(-57.0597576325586,-73.8447192590796,
73.4662010349383));
#204828=CARTESIAN_POINT('Origin',(-45.8894114130409,-83.3180213346267,69.5522455184007));
#204829=CARTESIAN_POINT('',(-61.0939133588288,-73.8447192590796,73.4662010349383));
#204830=CARTESIAN_POINT('',(-60.6878802914039,-73.844719258044,73.4662010324316));
#204831=CARTESIAN_POINT('',(-45.8894114130409,-73.8447192590796,73.4662010349383));
#204832=CARTESIAN_POINT('Ctrl Pts',(-59.2798347108578,-73.8447192543706,
73.4662010235407));
#204833=CARTESIAN_POINT('Ctrl Pts',(-59.2873239377854,-73.7421687186716,
73.2179886455785));
#204834=CARTESIAN_POINT('Ctrl Pts',(-59.2948125599226,-73.6494041099293,
72.9658202025441));
#204835=CARTESIAN_POINT('Ctrl Pts',(-59.3212550248384,-73.3587591160992,
72.0683661032157));
#204836=CARTESIAN_POINT('Ctrl Pts',(-59.3404565657231,-73.2147647592278,
71.4074966013702));
#204837=CARTESIAN_POINT('Ctrl Pts',(-59.388980080526,-73.0170996645956,
69.7092774270818));
#204838=CARTESIAN_POINT('Ctrl Pts',(-59.4172768982382,-73.0538311498301,
68.6690429747557));
#204839=CARTESIAN_POINT('Ctrl Pts',(-59.4640581669113,-73.3595772879527,
67.0484062054337));
#204840=CARTESIAN_POINT('Ctrl Pts',(-59.4815942395945,-73.5274854184184,
66.4562414312941));
#204841=CARTESIAN_POINT('Ctrl Pts',(-59.5124154215553,-73.9220915867976,
65.4270660511812));
#204842=CARTESIAN_POINT('Ctrl Pts',(-59.5259528039954,-74.1290945036622,
64.9845080489647));
#204843=CARTESIAN_POINT('Ctrl Pts',(-59.5586389489397,-74.695886677548,
63.9685682266536));
#204844=CARTESIAN_POINT('Ctrl Pts',(-59.5779246592963,-75.0824350281104,
63.4127210382677));
#204845=CARTESIAN_POINT('Ctrl Pts',(-59.6160754054652,-75.957435833677,
62.3872808123945));
#204846=CARTESIAN_POINT('Ctrl Pts',(-59.6346024281748,-76.4433492235958,
61.9198262813317));
#204847=CARTESIAN_POINT('Ctrl Pts',(-59.6724351127768,-77.5016643579224,
61.0853546234917));
#204848=CARTESIAN_POINT('Ctrl Pts',(-59.6916891412228,-78.0717858971223,
60.7207537097166));
#204849=CARTESIAN_POINT('Ctrl Pts',(-59.7328542612989,-79.3668808076306,
60.062470759711));
#204850=CARTESIAN_POINT('Ctrl Pts',(-59.7542186855682,-80.0980279749228,
59.790125831768));
#204851=CARTESIAN_POINT('Ctrl Pts',(-59.7951715359065,-81.509865753293,
59.4403143194271));
#204852=CARTESIAN_POINT('Ctrl Pts',(-59.8145446366639,-82.1813180901955,
59.3430109094515));
#204853=CARTESIAN_POINT('Ctrl Pts',(-59.8478622292068,-83.361431778364,
59.289929148128));
#204854=CARTESIAN_POINT('Ctrl Pts',(-59.8618209663203,-83.8664114920447,
59.3044997145979));
#204855=CARTESIAN_POINT('Ctrl Pts',(-59.8935251351027,-84.993946172304,
59.4206409789947));
#204856=CARTESIAN_POINT('Ctrl Pts',(-59.9113264747551,-85.6123672195088,
59.5425453224756));
#204857=CARTESIAN_POINT('Ctrl Pts',(-59.96760981281,-87.5103181489269,60.1019131248088));
#204858=CARTESIAN_POINT('Ctrl Pts',(-60.0044818029743,-88.7169214609657,
60.7354431445205));
#204859=CARTESIAN_POINT('Ctrl Pts',(-60.0813271816948,-90.8167160050427,
62.4347436381659));
#204860=CARTESIAN_POINT('Ctrl Pts',(-60.1182483491901,-91.688878557295,
63.4844612452277));
#204861=CARTESIAN_POINT('Ctrl Pts',(-60.1661320368538,-92.4901236914144,
64.9647587136454));
#204862=CARTESIAN_POINT('Ctrl Pts',(-60.1755708910434,-92.6337496116151,
65.263923404593));
#204863=CARTESIAN_POINT('Ctrl Pts',(-60.1996437446451,-92.9664064236839,
66.0527836900448));
#204864=CARTESIAN_POINT('Ctrl Pts',(-60.2141509106924,-93.1328026992833,
66.550972454217));
#204865=CARTESIAN_POINT('Ctrl Pts',(-60.2579231222864,-93.5126233441831,
68.0660113822973));
#204866=CARTESIAN_POINT('Ctrl Pts',(-60.2876399382542,-93.6106698144504,
69.1048112013147));
#204867=CARTESIAN_POINT('Ctrl Pts',(-60.325770193447,-93.5322403454906,
70.4690205320168));
#204868=CARTESIAN_POINT('Ctrl Pts',(-60.3349266672721,-93.497552757433,
70.7963862117687));
#204869=CARTESIAN_POINT('Ctrl Pts',(-60.3736531787992,-93.2859391199713,
72.1622881970776));
#204870=CARTESIAN_POINT('Ctrl Pts',(-60.4038129149676,-92.965247396422,
73.1720168367747));
#204871=CARTESIAN_POINT('Ctrl Pts',(-60.4423937032275,-92.3496860665155,
74.410246256175));
#204872=CARTESIAN_POINT('Ctrl Pts',(-60.4515684601349,-92.1888099356396,
74.6981417606306));
#204873=CARTESIAN_POINT('Ctrl Pts',(-60.4897418311879,-91.4678567838218,
75.8537211450771));
#204874=CARTESIAN_POINT('Ctrl Pts',(-60.5193171545131,-90.7921521948344,
76.6420825551035));
#204875=CARTESIAN_POINT('Ctrl Pts',(-60.5573038070801,-89.7610650936442,
77.5308299351059));
#204876=CARTESIAN_POINT('Ctrl Pts',(-60.5664545311213,-89.5018137519351,
77.7334027205151));
#204877=CARTESIAN_POINT('Ctrl Pts',(-60.6053623929022,-88.3676161923673,
78.5348760006254));
#204878=CARTESIAN_POINT('Ctrl Pts',(-60.6357128673784,-87.4122867627898,
79.0086219988744));
#204879=CARTESIAN_POINT('Ctrl Pts',(-60.6744881182545,-86.0868170529555,
79.4267115110407));
#204880=CARTESIAN_POINT('Ctrl Pts',(-60.683670824061,-85.7676285026662,
79.5106958294285));
#204881=CARTESIAN_POINT('Ctrl Pts',(-60.7118302698351,-84.7849002375619,
79.7191542008022));
#204882=CARTESIAN_POINT('Ctrl Pts',(-60.7310319109037,-84.1126408753728,
79.7936482022817));
#204883=CARTESIAN_POINT('Ctrl Pts',(-60.7795303438115,-82.4039510736968,
79.8136444435586));
#204884=CARTESIAN_POINT('Ctrl Pts',(-60.8078034529711,-81.374039833783,
79.6692000450616));
#204885=CARTESIAN_POINT('Ctrl Pts',(-60.8545148446357,-79.7961876611496,
79.1976901625094));
#204886=CARTESIAN_POINT('Ctrl Pts',(-60.8720082387315,-79.2260327763903,
78.9699713583507));
#204887=CARTESIAN_POINT('Ctrl Pts',(-60.9025694825878,-78.2514870702418,
78.475431412836));
#204888=CARTESIAN_POINT('Ctrl Pts',(-60.9158896374163,-77.8391334233009,
78.2283508503706));
#204889=CARTESIAN_POINT('Ctrl Pts',(-60.9483391397852,-76.8921846906305,
77.566424912575));
#204890=CARTESIAN_POINT('Ctrl Pts',(-60.9676110033283,-76.3783307299097,
77.1258263425336));
#204891=CARTESIAN_POINT('Ctrl Pts',(-61.0069268347375,-75.4185044007876,
76.1225455087659));
#204892=CARTESIAN_POINT('Ctrl Pts',(-61.0265516412905,-74.9805923799831,
75.5571176972676));
#204893=CARTESIAN_POINT('Ctrl Pts',(-61.0622515558693,-74.3115140978787,
74.4772523777343));
#204894=CARTESIAN_POINT('Ctrl Pts',(-61.07809329045,-74.0572958058767,73.9807193613414));
#204895=CARTESIAN_POINT('Ctrl Pts',(-61.0939133588288,-73.8447192590796,
73.4662010349383));
#204896=CARTESIAN_POINT('Ctrl Pts',(-60.6878802914039,-73.8447192570083,
73.466201029925));
#204897=CARTESIAN_POINT('Ctrl Pts',(-60.6549485354339,-74.2867494945032,
74.5360869688175));
#204898=CARTESIAN_POINT('Ctrl Pts',(-60.6232629605615,-74.9068773164,75.5234704922587));
#204899=CARTESIAN_POINT('Ctrl Pts',(-60.5753209802943,-76.0346255959043,
76.7840831150594));
#204900=CARTESIAN_POINT('Ctrl Pts',(-60.5600539343161,-76.4209829040694,
77.1534423460483));
#204901=CARTESIAN_POINT('Ctrl Pts',(-60.5260316686445,-77.3582558311916,
77.9189217224717));
#204902=CARTESIAN_POINT('Ctrl Pts',(-60.507373814461,-77.9232451295373,
78.293897249308));
#204903=CARTESIAN_POINT('Ctrl Pts',(-60.4735852233983,-78.9827499354831,
78.8549804346847));
#204904=CARTESIAN_POINT('Ctrl Pts',(-60.4586939764479,-79.4624729874221,
79.063827717357));
#204905=CARTESIAN_POINT('Ctrl Pts',(-60.426245377712,-80.5423576065695,
79.4387734459005));
#204906=CARTESIAN_POINT('Ctrl Pts',(-60.4090584186557,-81.14597687462,79.5886775666442));
#204907=CARTESIAN_POINT('Ctrl Pts',(-60.3734714868846,-82.4039286600131,
79.7822078915812));
#204908=CARTESIAN_POINT('Ctrl Pts',(-60.3550172154272,-83.0564048661365,
79.8196325925183));
#204909=CARTESIAN_POINT('Ctrl Pts',(-60.3055240991709,-84.7952387715697,
79.7534292227667));
#204910=CARTESIAN_POINT('Ctrl Pts',(-60.275748624715,-85.8689920193426,
79.5391809450683));
#204911=CARTESIAN_POINT('Ctrl Pts',(-60.2286892275973,-87.4264980060355,
78.9603211413376));
#204912=CARTESIAN_POINT('Ctrl Pts',(-60.2122723783539,-87.9464068033781,
78.7157340011332));
#204913=CARTESIAN_POINT('Ctrl Pts',(-60.181791493603,-88.88621028393,78.1731239021973));
#204914=CARTESIAN_POINT('Ctrl Pts',(-60.1676315602502,-89.3095230772174,
77.8844831166072));
#204915=CARTESIAN_POINT('Ctrl Pts',(-60.1329740426659,-90.2762019116352,
77.1134404337409));
#204916=CARTESIAN_POINT('Ctrl Pts',(-60.1123084476158,-90.7933462710861,
76.6025959711627));
#204917=CARTESIAN_POINT('Ctrl Pts',(-60.0822953265914,-91.464109478671,
75.7824723431725));
#204918=CARTESIAN_POINT('Ctrl Pts',(-60.0729376397771,-91.6631510759079,
75.513226045402));
#204919=CARTESIAN_POINT('Ctrl Pts',(-60.0454258533602,-92.2099444091266,
74.6923694872839));
#204920=CARTESIAN_POINT('Ctrl Pts',(-60.0272520902438,-92.5186744600083,
74.1167986352821));
#204921=CARTESIAN_POINT('Ctrl Pts',(-59.9952901842358,-92.9543870770854,
73.0776794715771));
#204922=CARTESIAN_POINT('Ctrl Pts',(-59.9817127483823,-93.1074215528269,
72.6272857226748));
#204923=CARTESIAN_POINT('Ctrl Pts',(-59.954926432713,-93.350009756936,71.7081280359482));
#204924=CARTESIAN_POINT('Ctrl Pts',(-59.941758434721,-93.4392147721439,
71.24046037876));
#204925=CARTESIAN_POINT('Ctrl Pts',(-59.9191599910848,-93.5351099586427,
70.437872648298));
#204926=CARTESIAN_POINT('Ctrl Pts',(-59.9098138709979,-93.5584749195833,
70.1057288119585));
#204927=CARTESIAN_POINT('Ctrl Pts',(-59.8862018942637,-93.5764556783268,
69.2711961468843));
#204928=CARTESIAN_POINT('Ctrl Pts',(-59.8718628566531,-93.5503896051845,
68.7692382533867));
#204929=CARTESIAN_POINT('Ctrl Pts',(-59.8395168809513,-93.4074846759297,
67.6347664157249));
#204930=CARTESIAN_POINT('Ctrl Pts',(-59.8218335602118,-93.2677443924347,
67.0072485059131));
#204931=CARTESIAN_POINT('Ctrl Pts',(-59.7773523524948,-92.7795652914737,
65.4984210150904));
#204932=CARTESIAN_POINT('Ctrl Pts',(-59.7502626452427,-92.3660787022586,
64.6443974106));
#204933=CARTESIAN_POINT('Ctrl Pts',(-59.7089452485442,-91.545027571265,
63.4151545487212));
#204934=CARTESIAN_POINT('Ctrl Pts',(-59.6941331228762,-91.214270189443,
62.9950532061332));
#204935=CARTESIAN_POINT('Ctrl Pts',(-59.660040108745,-90.3933564921767,
62.1050767579077));
#204936=CARTESIAN_POINT('Ctrl Pts',(-59.6406626778397,-89.8862581147153,
61.654211444381));
#204937=CARTESIAN_POINT('Ctrl Pts',(-59.6075214539216,-88.9350769997471,
60.9639061007698));
#204938=CARTESIAN_POINT('Ctrl Pts',(-59.5937295363488,-88.5109050975766,
60.7009828543388));
#204939=CARTESIAN_POINT('Ctrl Pts',(-59.5619836481251,-87.5051187295114,
60.1748196345809));
#204940=CARTESIAN_POINT('Ctrl Pts',(-59.543963217233,-86.9146733897969,
59.932891031642));
#204941=CARTESIAN_POINT('Ctrl Pts',(-59.5163445956903,-85.9858608325994,
59.6498785785385));
#204942=CARTESIAN_POINT('Ctrl Pts',(-59.5068630286917,-85.6615240423739,
59.5681462488556));
#204943=CARTESIAN_POINT('Ctrl Pts',(-59.4781411725251,-84.6566684099116,
59.3665969175512));
#204944=CARTESIAN_POINT('Ctrl Pts',(-59.459048540038,-83.9675714778447,
59.2995628231034));
#204945=CARTESIAN_POINT('Ctrl Pts',(-59.4259185777449,-82.795074324431,
59.3042570479986));
#204946=CARTESIAN_POINT('Ctrl Pts',(-59.4121692653147,-82.3139001453329,
59.3401703963216));
#204947=CARTESIAN_POINT('Ctrl Pts',(-59.3737534035655,-80.9733775652037,
59.5359101886738));
#204948=CARTESIAN_POINT('Ctrl Pts',(-59.3498274930302,-80.1293491599953,
59.7718212331793));
#204949=CARTESIAN_POINT('Ctrl Pts',(-59.2992816926066,-78.4806782000531,
60.4690792347319));
#204950=CARTESIAN_POINT('Ctrl Pts',(-59.2731736201417,-77.6876573487076,
60.9381396783424));
#204951=CARTESIAN_POINT('Ctrl Pts',(-59.2099049138779,-75.9067319761303,
62.3437746921879));
#204952=CARTESIAN_POINT('Ctrl Pts',(-59.1714264745829,-75.0218245832259,
63.3827736046064));
#204953=CARTESIAN_POINT('Ctrl Pts',(-59.1153877075156,-74.0437887948291,
65.1381830579093));
#204954=CARTESIAN_POINT('Ctrl Pts',(-59.0969999696884,-73.7796585481076,
65.742394789452));
#204955=CARTESIAN_POINT('Ctrl Pts',(-59.0603571635507,-73.3787293450233,
66.9690057963436));
#204956=CARTESIAN_POINT('Ctrl Pts',(-59.0423634327771,-73.2382779305409,
67.5871900361875));
#204957=CARTESIAN_POINT('Ctrl Pts',(-59.0155634689847,-73.1129690606558,
68.5390171613752));
#204958=CARTESIAN_POINT('Ctrl Pts',(-59.0064538880824,-73.0858103549134,
68.8655272988062));
#204959=CARTESIAN_POINT('Ctrl Pts',(-58.9661357929594,-73.0353080704403,
70.3046748358551));
#204960=CARTESIAN_POINT('Ctrl Pts',(-58.9343155934815,-73.1775838491939,
71.4155416553419));
#204961=CARTESIAN_POINT('Ctrl Pts',(-58.8935634968148,-73.5951978839729,
72.8157920654114));
#204962=CARTESIAN_POINT('Ctrl Pts',(-58.8838562465419,-73.7117537529889,
73.1443725421251));
#204963=CARTESIAN_POINT('Ctrl Pts',(-58.8740778711611,-73.8447192590796,
73.4662010349383));
#204964=CARTESIAN_POINT('Origin',(-45.8894114130409,-83.3180213346267,69.5522455184007));
#204965=CARTESIAN_POINT('',(-62.9075068658247,-73.8447192590796,73.4662010349382));
#204966=CARTESIAN_POINT('',(-62.5017927897014,-73.8447192658252,73.4662010512653));
#204967=CARTESIAN_POINT('',(-45.8894114130409,-73.8447192590796,73.4662010349383));
#204968=CARTESIAN_POINT('',(-62.1255498668003,-93.5595364804028,69.970346919323));
#204969=CARTESIAN_POINT('Ctrl Pts',(-62.9075068658247,-73.8447192590795,
73.4662010349381));
#204970=CARTESIAN_POINT('Ctrl Pts',(-62.8890297137548,-74.0941098645064,
74.0698237715866));
#204971=CARTESIAN_POINT('Ctrl Pts',(-62.8709501951455,-74.4006222769129,
74.6482296293146));
#204972=CARTESIAN_POINT('Ctrl Pts',(-62.8346556323582,-75.1175005308676,
75.7357486846773));
#204973=CARTESIAN_POINT('Ctrl Pts',(-62.816127299745,-75.5256433516957,
76.2427667065413));
#204974=CARTESIAN_POINT('Ctrl Pts',(-62.7595831183316,-76.9123795088531,
77.6650712602952));
#204975=CARTESIAN_POINT('Ctrl Pts',(-62.7232980830352,-78.0241240009392,
78.4305795136538));
#204976=CARTESIAN_POINT('Ctrl Pts',(-62.6471481891126,-80.4749509242041,
79.4898561694312));
#204977=CARTESIAN_POINT('Ctrl Pts',(-62.6109576119547,-81.7899614573926,
79.7749756124774));
#204978=CARTESIAN_POINT('Ctrl Pts',(-62.5541063933797,-83.787779249665,
79.8130641293939));
#204979=CARTESIAN_POINT('Ctrl Pts',(-62.5351119019629,-84.4525860097568,
79.760960059608));
#204980=CARTESIAN_POINT('Ctrl Pts',(-62.4978581696944,-85.7602341430177,
79.5290869291398));
#204981=CARTESIAN_POINT('Ctrl Pts',(-62.4796746883654,-86.4000600770917,
79.3503470402618));
#204982=CARTESIAN_POINT('Ctrl Pts',(-62.4424295539205,-87.6317020290275,
78.8735937106281));
#204983=CARTESIAN_POINT('Ctrl Pts',(-62.4235188596297,-88.2209803079372,
78.5775642584995));
#204984=CARTESIAN_POINT('Ctrl Pts',(-62.3861515017277,-89.3406245664244,
77.8728813615582));
#204985=CARTESIAN_POINT('Ctrl Pts',(-62.3677920367359,-89.8676274107198,
77.4647286706258));
#204986=CARTESIAN_POINT('Ctrl Pts',(-62.3306363167816,-90.8357688888216,
76.5514880424947));
#204987=CARTESIAN_POINT('Ctrl Pts',(-62.3115449033513,-91.2744815876631,
76.0484475302656));
#204988=CARTESIAN_POINT('Ctrl Pts',(-62.2644735866283,-92.2367689999472,
74.7000482335409));
#204989=CARTESIAN_POINT('Ctrl Pts',(-62.237467135121,-92.6923052269227,
73.8144878831633));
#204990=CARTESIAN_POINT('Ctrl Pts',(-62.1815044190819,-93.3352043397708,
71.9398912558015));
#204991=CARTESIAN_POINT('Ctrl Pts',(-62.1531555603415,-93.5190613500812,
70.9606701984125));
#204992=CARTESIAN_POINT('Ctrl Pts',(-62.1255316836823,-93.5594905838186,
69.9703455277973));
#204993=CARTESIAN_POINT('Ctrl Pts',(-61.0939133588288,-73.8447192590796,
73.4662010349383));
#204994=CARTESIAN_POINT('Ctrl Pts',(-61.0972755292109,-73.7995412893984,
73.356852691008));
#204995=CARTESIAN_POINT('Ctrl Pts',(-61.1006343640762,-73.7562441228431,
73.2466919441307));
#204996=CARTESIAN_POINT('Ctrl Pts',(-61.1224071184744,-73.4871979595048,
72.5256982249987));
#204997=CARTESIAN_POINT('Ctrl Pts',(-61.1403527106327,-73.3181970944473,
71.8953260594235));
#204998=CARTESIAN_POINT('Ctrl Pts',(-61.1775605622687,-73.098118251332,
70.587507381851));
#204999=CARTESIAN_POINT('Ctrl Pts',(-61.1967979414229,-73.052132641733,
69.9123831679951));
#205000=CARTESIAN_POINT('Ctrl Pts',(-61.2402988666641,-73.0992182659107,
68.3788970089533));
#205001=CARTESIAN_POINT('Ctrl Pts',(-61.2638572963438,-73.2334570554963,
67.5268448741542));
#205002=CARTESIAN_POINT('Ctrl Pts',(-61.3137826779292,-73.7253916735425,
65.8278126755097));
#205003=CARTESIAN_POINT('Ctrl Pts',(-61.3397066335119,-74.0935684710335,
64.9916059948674));
#205004=CARTESIAN_POINT('Ctrl Pts',(-61.4027530430455,-75.2707843617758,
63.0614753140105));
#205005=CARTESIAN_POINT('Ctrl Pts',(-61.4412152659376,-76.1955325584022,
62.0583624016276));
#205006=CARTESIAN_POINT('Ctrl Pts',(-61.4971523997589,-77.8173921947074,
60.8784979180106));
#205007=CARTESIAN_POINT('Ctrl Pts',(-61.5154210351218,-78.3822816998748,
60.5450659144375));
#205008=CARTESIAN_POINT('Ctrl Pts',(-61.5518901541755,-79.5463008162671,
60.0005807093627));
#205009=CARTESIAN_POINT('Ctrl Pts',(-61.5698612016951,-80.1409618991759,
59.7866688915264));
#205010=CARTESIAN_POINT('Ctrl Pts',(-61.6052068932917,-81.3660595803169,
59.4698207635543));
#205011=CARTESIAN_POINT('Ctrl Pts',(-61.6228341737123,-81.9940518549715,
59.3683098329066));
#205012=CARTESIAN_POINT('Ctrl Pts',(-61.6549628277035,-83.1273207365526,
59.2917772992746));
#205013=CARTESIAN_POINT('Ctrl Pts',(-61.6692758998122,-83.6290562963196,
59.2947200422361));
#205014=CARTESIAN_POINT('Ctrl Pts',(-61.7017999922263,-84.77506317455,59.3856271790135));
#205015=CARTESIAN_POINT('Ctrl Pts',(-61.7196746168933,-85.4152409850817,
59.4981532587356));
#205016=CARTESIAN_POINT('Ctrl Pts',(-61.7639923205417,-86.9382214783504,
59.9177370281428));
#205017=CARTESIAN_POINT('Ctrl Pts',(-61.7907068925564,-87.798079577134,
60.2862491473952));
#205018=CARTESIAN_POINT('Ctrl Pts',(-61.8308005140353,-89.0273972914217,
61.0247355433965));
#205019=CARTESIAN_POINT('Ctrl Pts',(-61.8447519131577,-89.4388416258829,
61.3150761380113));
#205020=CARTESIAN_POINT('Ctrl Pts',(-61.877891718036,-90.3493249207702,
62.0635913641212));
#205021=CARTESIAN_POINT('Ctrl Pts',(-61.8972052867198,-90.8276155890008,
62.5433119093223));
#205022=CARTESIAN_POINT('Ctrl Pts',(-61.9334581013333,-91.6389705443853,
63.5362534302575));
#205023=CARTESIAN_POINT('Ctrl Pts',(-61.9501942467327,-91.9802953089516,
64.0390460305397));
#205024=CARTESIAN_POINT('Ctrl Pts',(-61.9931785862009,-92.7259061778884,
65.3792607709462));
#205025=CARTESIAN_POINT('Ctrl Pts',(-62.0197789243641,-93.0646448459485,
66.2468816466174));
#205026=CARTESIAN_POINT('Ctrl Pts',(-62.0588455447749,-93.3920095183979,
67.6036950542001));
#205027=CARTESIAN_POINT('Ctrl Pts',(-62.0718370519845,-93.4705497370475,
68.0662255956203));
#205028=CARTESIAN_POINT('Ctrl Pts',(-62.0984431327042,-93.5649315281472,
69.0102031279554));
#205029=CARTESIAN_POINT('Ctrl Pts',(-62.1120352760041,-93.5790729419953,
69.4906655321689));
#205030=CARTESIAN_POINT('Ctrl Pts',(-62.1256936736043,-93.5594907615313,
69.9703411746549));
#205031=CARTESIAN_POINT('Ctrl Pts',(-62.5017927901943,-73.8447192658304,
73.466201051278));
#205032=CARTESIAN_POINT('Ctrl Pts',(-62.4841847932971,-74.0855314753815,
74.0490607142885));
#205033=CARTESIAN_POINT('Ctrl Pts',(-62.4666545746529,-74.3796576838083,
74.608539247783));
#205034=CARTESIAN_POINT('Ctrl Pts',(-62.4394720039789,-74.9030783441912,
75.4139829192377));
#205035=CARTESIAN_POINT('Ctrl Pts',(-62.4300873205818,-75.0959934428049,
75.6816408449356));
#205036=CARTESIAN_POINT('Ctrl Pts',(-62.3906602265135,-75.9599741494087,
76.7660047698653));
#205037=CARTESIAN_POINT('Ctrl Pts',(-62.3617397936393,-76.7423395887225,
77.4856935935262));
#205038=CARTESIAN_POINT('Ctrl Pts',(-62.3225114354629,-77.8942276034712,
78.2558738490049));
#205039=CARTESIAN_POINT('Ctrl Pts',(-62.3131477738994,-78.1762943169244,
78.4254257130088));
#205040=CARTESIAN_POINT('Ctrl Pts',(-62.2743741082159,-79.3775580116726,
79.0709689990103));
#205041=CARTESIAN_POINT('Ctrl Pts',(-62.2460503879043,-80.3580374681057,
79.4199630804335));
#205042=CARTESIAN_POINT('Ctrl Pts',(-62.2074372133845,-81.6976361070693,
79.6787181434111));
#205043=CARTESIAN_POINT('Ctrl Pts',(-62.1980576697969,-82.0240197146451,
79.7255760830527));
#205044=CARTESIAN_POINT('Ctrl Pts',(-62.1587914746783,-83.3987458291229,
79.8557054367172));
#205045=CARTESIAN_POINT('Ctrl Pts',(-62.1300181568743,-84.4544380023431,
79.7931618537553));
#205046=CARTESIAN_POINT('Ctrl Pts',(-62.0855312849989,-85.9905269512449,
79.4613724502301));
#205047=CARTESIAN_POINT('Ctrl Pts',(-62.0706589776804,-86.4898777562472,
79.3130040452828));
#205048=CARTESIAN_POINT('Ctrl Pts',(-62.0466231600363,-87.28554034407,79.0090542175185));
#205049=CARTESIAN_POINT('Ctrl Pts',(-62.0373902278873,-87.5893541668113,
78.8757724680081));
#205050=CARTESIAN_POINT('Ctrl Pts',(-61.9904527351222,-89.09610785971,78.1256345376654));
#205051=CARTESIAN_POINT('Ctrl Pts',(-61.951973712199,-90.1750339007047,
77.2898589653742));
#205052=CARTESIAN_POINT('Ctrl Pts',(-61.8792605949586,-91.8836561409898,
75.3202275397201));
#205053=CARTESIAN_POINT('Ctrl Pts',(-61.8434485105681,-92.5252913279683,
74.2283448200108));
#205054=CARTESIAN_POINT('Ctrl Pts',(-61.7895069237388,-93.1837604232446,
72.4132391565384));
#205055=CARTESIAN_POINT('Ctrl Pts',(-61.7707654980411,-93.3507060338506,
71.7575408245925));
#205056=CARTESIAN_POINT('Ctrl Pts',(-61.7325189893887,-93.5533519612268,
70.4222640392778));
#205057=CARTESIAN_POINT('Ctrl Pts',(-61.7132059380748,-93.5884366430676,
69.7459250868423));
#205058=CARTESIAN_POINT('Ctrl Pts',(-61.6754557091104,-93.5250454819414,
68.3970701948348));
#205059=CARTESIAN_POINT('Ctrl Pts',(-61.6567438364296,-93.4268963238492,
67.727850414592));
#205060=CARTESIAN_POINT('Ctrl Pts',(-61.6283187645921,-93.1839472020908,
66.7531845002519));
#205061=CARTESIAN_POINT('Ctrl Pts',(-61.6189338943095,-93.0887989606251,
66.4372592869426));
#205062=CARTESIAN_POINT('Ctrl Pts',(-61.5795009251722,-92.6253410740485,
65.1303232177303));
#205063=CARTESIAN_POINT('Ctrl Pts',(-61.5505751177801,-92.1201334356208,
64.194780818897));
#205064=CARTESIAN_POINT('Ctrl Pts',(-61.5113412268191,-91.281979225922,
63.0911267564976));
#205065=CARTESIAN_POINT('Ctrl Pts',(-61.5019777055676,-91.0705636445477,
62.8389179069684));
#205066=CARTESIAN_POINT('Ctrl Pts',(-61.4632083833256,-90.1453340345577,
61.8372699653512));
#205067=CARTESIAN_POINT('Ctrl Pts',(-61.4348886239657,-89.3322286570764,
61.1878947823721));
#205068=CARTESIAN_POINT('Ctrl Pts',(-61.3907373814084,-87.9805507160714,
60.4089783600418));
#205069=CARTESIAN_POINT('Ctrl Pts',(-61.3757161999373,-87.505859075302,
60.1820519947092));
#205070=CARTESIAN_POINT('Ctrl Pts',(-61.3515272274868,-86.7065344518898,
59.8728609480731));
#205071=CARTESIAN_POINT('Ctrl Pts',(-61.3422905309527,-86.3915729733846,
59.7682898692625));
#205072=CARTESIAN_POINT('Ctrl Pts',(-61.2953514805828,-84.7702512509659,
59.3160254008778));
#205073=CARTESIAN_POINT('Ctrl Pts',(-61.2568735915856,-83.4093454335768,
59.2139267594145));
#205074=CARTESIAN_POINT('Ctrl Pts',(-61.1815476021197,-80.7283712650494,
59.5433686192169));
#205075=CARTESIAN_POINT('Ctrl Pts',(-61.1431283745384,-79.4344568146368,
59.9709177871001));
#205076=CARTESIAN_POINT('Ctrl Pts',(-61.0879192659949,-77.7127072891277,
60.9476124636147));
#205077=CARTESIAN_POINT('Ctrl Pts',(-61.070345096222,-77.1946513438504,
61.3082423398081));
#205078=CARTESIAN_POINT('Ctrl Pts',(-61.0381959870421,-76.3277426502109,
62.0387705491118));
#205079=CARTESIAN_POINT('Ctrl Pts',(-61.023791336302,-75.9669566102274,
62.3913690533349));
#205080=CARTESIAN_POINT('Ctrl Pts',(-60.9948506651892,-75.2863030073976,
63.1624605811165));
#205081=CARTESIAN_POINT('Ctrl Pts',(-60.980338142677,-74.9697649554248,
63.5819463534444));
#205082=CARTESIAN_POINT('Ctrl Pts',(-60.9477026164546,-74.341455457925,
64.5628978746868));
#205083=CARTESIAN_POINT('Ctrl Pts',(-60.9295233279679,-74.0474347307934,
65.1331353657493));
#205084=CARTESIAN_POINT('Ctrl Pts',(-60.8933588822817,-73.5725602068601,
66.3136804132178));
#205085=CARTESIAN_POINT('Ctrl Pts',(-60.8757973656961,-73.3913769943919,
66.9208860112263));
#205086=CARTESIAN_POINT('Ctrl Pts',(-60.8397638220275,-73.1382738855007,
68.1856499340229));
#205087=CARTESIAN_POINT('Ctrl Pts',(-60.8211917494364,-73.0715879518112,
68.841309849744));
#205088=CARTESIAN_POINT('Ctrl Pts',(-60.7640366499264,-73.0611151385496,
70.8504175195901));
#205089=CARTESIAN_POINT('Ctrl Pts',(-60.7271143757618,-73.3214825470434,
72.1901587832426));
#205090=CARTESIAN_POINT('Ctrl Pts',(-60.6884024535279,-73.8377218668054,
73.4492323338641));
#205091=CARTESIAN_POINT('Ctrl Pts',(-60.6881413650971,-73.8412149656867,
73.4577192753012));
#205092=CARTESIAN_POINT('Ctrl Pts',(-60.6878802914039,-73.8447192570083,
73.466201029925));
#205093=CARTESIAN_POINT('Origin',(-21.6548258024609,-75.,72.98888938658));
#205094=CARTESIAN_POINT('',(-23.7494631149408,-62.9850802834321,77.9529305028911));
#205095=CARTESIAN_POINT('',(-23.5675316904177,-62.985080294536,77.9529305294611));
#205096=CARTESIAN_POINT('',(-21.6548258024609,-62.9850802944281,77.9529305295057));
#205097=CARTESIAN_POINT('',(-23.5675316903009,-68.1939482861969,84.0648841531478));
#205098=CARTESIAN_POINT('Ctrl Pts',(-23.7494631142981,-62.9850802834266,
77.9529305028778));
#205099=CARTESIAN_POINT('Ctrl Pts',(-23.7335469728175,-63.2572812599135,
78.611763256806));
#205100=CARTESIAN_POINT('Ctrl Pts',(-23.7173356484375,-63.583267752548,
79.2472274989783));
#205101=CARTESIAN_POINT('Ctrl Pts',(-23.6789660693081,-64.4896165551071,
80.7050232770356));
#205102=CARTESIAN_POINT('Ctrl Pts',(-23.6573462260849,-65.1163076778375,
81.4929757686019));
#205103=CARTESIAN_POINT('Ctrl Pts',(-23.6129675706434,-66.5413261017482,
82.9118922601765));
#205104=CARTESIAN_POINT('Ctrl Pts',(-23.5899173818356,-67.3355222961797,
83.5373927807101));
#205105=CARTESIAN_POINT('Ctrl Pts',(-23.5675316903009,-68.1939482861969,
84.0648841531478));
#205106=CARTESIAN_POINT('Origin',(-23.5675316903009,-75.,72.98888938658));
#205107=CARTESIAN_POINT('Origin',(-21.6548258024609,-75.,72.98888938658));
#205108=CARTESIAN_POINT('',(-25.5628518781596,-62.9850802944281,77.9529305295057));
#205109=CARTESIAN_POINT('',(-25.2581222247366,-62.9850802944281,77.9529305295057));
#205110=CARTESIAN_POINT('',(-21.6548258024609,-62.9850802944281,77.9529305295057));
#205111=CARTESIAN_POINT('Ctrl Pts',(-25.5628518781596,-62.9850802944281,
77.9529305295057));
#205112=CARTESIAN_POINT('Ctrl Pts',(-25.5342348853663,-63.4755910199596,
79.1401581958963));
#205113=CARTESIAN_POINT('Ctrl Pts',(-25.5067802221842,-64.1402777289051,
80.2502980014423));
#205114=CARTESIAN_POINT('Ctrl Pts',(-25.4598723099547,-65.4624900254345,
81.8581750998699));
#205115=CARTESIAN_POINT('Ctrl Pts',(-25.4420110595249,-66.0209090968996,
82.4230970114663));
#205116=CARTESIAN_POINT('Ctrl Pts',(-25.4061623457359,-67.2631855963744,
83.468998148917));
#205117=CARTESIAN_POINT('Ctrl Pts',(-25.3882919641257,-67.948955156665,
83.9421414655667));
#205118=CARTESIAN_POINT('Ctrl Pts',(-25.3604186304515,-69.0425151706589,
84.5511188474739));
#205119=CARTESIAN_POINT('Ctrl Pts',(-25.3509160417769,-69.4195525323061,
84.7377352997636));
#205120=CARTESIAN_POINT('Ctrl Pts',(-25.3031624035224,-71.3605130656141,
85.5838769037993));
#205121=CARTESIAN_POINT('Ctrl Pts',(-25.2671492367614,-73.0338876517155,
85.9509106010213));
#205122=CARTESIAN_POINT('Ctrl Pts',(-25.211093783332,-75.5211982206036,
86.0024934260272));
#205123=CARTESIAN_POINT('Ctrl Pts',(-25.1932702125315,-76.3117954672579,
85.9466959719248));
#205124=CARTESIAN_POINT('Ctrl Pts',(-25.1573545097553,-77.9173095201321,
85.6848678053003));
#205125=CARTESIAN_POINT('Ctrl Pts',(-25.1393881007222,-78.7273131421505,
85.4711042328601));
#205126=CARTESIAN_POINT('Ctrl Pts',(-25.1114105692348,-79.905454109883,
85.035186013571));
#205127=CARTESIAN_POINT('Ctrl Pts',(-25.1019084706642,-80.2924279850967,
84.8702591362598));
#205128=CARTESIAN_POINT('Ctrl Pts',(-25.0541466985092,-82.1980757005559,
83.9464752146254));
#205129=CARTESIAN_POINT('Ctrl Pts',(-25.0181261672443,-83.5657348334043,
82.9140686343907));
#205130=CARTESIAN_POINT('Ctrl Pts',(-24.9617637202305,-85.2318804993534,
81.0483612746309));
#205131=CARTESIAN_POINT('Ctrl Pts',(-24.9436507628792,-85.710654373767,
80.4002570731339));
#205132=CARTESIAN_POINT('Ctrl Pts',(-24.9079838183037,-86.5466312994028,
79.0167666311897));
#205133=CARTESIAN_POINT('Ctrl Pts',(-24.8905073373037,-86.9006753634193,
78.2835953282236));
#205134=CARTESIAN_POINT('Ctrl Pts',(-24.8630645895268,-87.3306440284148,
77.1279872899302));
#205135=CARTESIAN_POINT('Ctrl Pts',(-24.8535596220528,-87.4580993038288,
76.7268933833987));
#205136=CARTESIAN_POINT('Ctrl Pts',(-24.8058503480045,-88.0001699063287,
74.6822528929101));
#205137=CARTESIAN_POINT('Ctrl Pts',(-24.7698813216615,-88.1099855999607,
72.9749547963028));
#205138=CARTESIAN_POINT('Ctrl Pts',(-24.7143843430216,-87.7889354780213,
70.5324051813258));
#205139=CARTESIAN_POINT('Ctrl Pts',(-24.6970419222637,-87.6212985854423,
69.7804588734143));
#205140=CARTESIAN_POINT('Ctrl Pts',(-24.6632901642082,-87.1584529888661,
68.3255961552898));
#205141=CARTESIAN_POINT('Ctrl Pts',(-24.6469281069572,-86.8660070905663,
67.6249218798878));
#205142=CARTESIAN_POINT('Ctrl Pts',(-24.6085627568924,-86.0594517133163,
66.0861333089881));
#205143=CARTESIAN_POINT('Ctrl Pts',(-24.586160384182,-85.5081015734761,
65.2727174091092));
#205144=CARTESIAN_POINT('Ctrl Pts',(-24.5478929218035,-84.3881486354314,
63.9660075581999));
#205145=CARTESIAN_POINT('Ctrl Pts',(-24.5317890202234,-83.8583716408209,
63.4453584440213));
#205146=CARTESIAN_POINT('Ctrl Pts',(-24.4786780417851,-81.9915516088788,
61.9008022575739));
#205147=CARTESIAN_POINT('Ctrl Pts',(-24.4404197776329,-80.5002502188647,
61.0903726254298));
#205148=CARTESIAN_POINT('Ctrl Pts',(-24.3944539989605,-78.4940872446607,
60.46016793533));
#205149=CARTESIAN_POINT('Ctrl Pts',(-24.3852625240197,-78.0862384647128,
60.3535169796922));
#205150=CARTESIAN_POINT('Ctrl Pts',(-24.3589735379833,-76.9284736377242,
60.110176267431));
#205151=CARTESIAN_POINT('Ctrl Pts',(-24.3416198348966,-76.170680721155,
60.0193181026919));
#205152=CARTESIAN_POINT('Ctrl Pts',(-24.315347669909,-74.9965402900159,
59.9823322175876));
#205153=CARTESIAN_POINT('Ctrl Pts',(-24.3062012240958,-74.5833920590936,
59.9890054637237));
#205154=CARTESIAN_POINT('Ctrl Pts',(-24.2791962632358,-73.3574014902427,
60.0673205172551));
#205155=CARTESIAN_POINT('Ctrl Pts',(-24.2616122208315,-72.5502449644129,
60.1957750471281));
#205156=CARTESIAN_POINT('Ctrl Pts',(-24.2174452577431,-70.6413697835284,
60.6869544138998));
#205157=CARTESIAN_POINT('Ctrl Pts',(-24.1913574606361,-69.5656309742676,
61.1228465529577));
#205158=CARTESIAN_POINT('Ctrl Pts',(-24.148103015785,-67.8509316396604,
62.1003517955149));
#205159=CARTESIAN_POINT('Ctrl Pts',(-24.1303270077391,-67.1799782752499,
62.5717550113518));
#205160=CARTESIAN_POINT('Ctrl Pts',(-24.0934607218758,-65.9342632283519,
63.6355618776124));
#205161=CARTESIAN_POINT('Ctrl Pts',(-24.0749439293734,-65.3625008128495,
64.2258447186017));
#205162=CARTESIAN_POINT('Ctrl Pts',(-24.0399256256379,-64.3721660207933,
65.4633093764349));
#205163=CARTESIAN_POINT('Ctrl Pts',(-24.0234209550608,-63.9478296127134,
66.1016021098746));
#205164=CARTESIAN_POINT('Ctrl Pts',(-23.9864808616788,-63.1492334947361,
67.5686511770807));
#205165=CARTESIAN_POINT('Ctrl Pts',(-23.9657965863761,-62.8006300155267,
68.4068572518267));
#205166=CARTESIAN_POINT('Ctrl Pts',(-23.928675173025,-62.3247219460287,
70.0030333536306));
#205167=CARTESIAN_POINT('Ctrl Pts',(-23.9121337744945,-62.1718251405703,
70.7492595751274));
#205168=CARTESIAN_POINT('Ctrl Pts',(-23.8584168754266,-61.8917373511402,
73.1862692369497));
#205169=CARTESIAN_POINT('Ctrl Pts',(-23.8198811582598,-62.0287767524375,
74.8896421089106));
#205170=CARTESIAN_POINT('Ctrl Pts',(-23.7736771942405,-62.6026642094907,
76.9237439180875));
#205171=CARTESIAN_POINT('Ctrl Pts',(-23.7645045072629,-62.7364962506747,
77.3228814711087));
#205172=CARTESIAN_POINT('Ctrl Pts',(-23.7532764802333,-62.9205454775805,
77.7945212353098));
#205173=CARTESIAN_POINT('Ctrl Pts',(-23.7513724844866,-62.9524258595896,
77.8738940340813));
#205174=CARTESIAN_POINT('Ctrl Pts',(-23.7494631142981,-62.9850802834266,
77.9529305028778));
#205175=CARTESIAN_POINT('',(-23.5675316904176,-62.0095472178182,72.4907563613072));
#205176=CARTESIAN_POINT('Origin',(-23.5675316903009,-75.,72.98888938658));
#205177=CARTESIAN_POINT('',(-23.5676924422401,-62.0098217648708,72.4836474449556));
#205178=CARTESIAN_POINT('Ctrl Pts',(-23.5675316904176,-62.0095472178182,
72.4907563613072));
#205179=CARTESIAN_POINT('Ctrl Pts',(-23.5675873235413,-62.0095822026889,
72.488392133029));
#205180=CARTESIAN_POINT('Ctrl Pts',(-23.5676429566649,-62.0096178329842,
72.4860278991301));
#205181=CARTESIAN_POINT('Ctrl Pts',(-23.5676985897885,-62.0096541087152,
72.483663659963));
#205182=CARTESIAN_POINT('',(-24.3504740810588,-87.0149185312533,68.0248454013453));
#205183=CARTESIAN_POINT('Ctrl Pts',(-23.5676924422401,-62.0098217648708,
72.4836474449556));
#205184=CARTESIAN_POINT('Ctrl Pts',(-23.579866516381,-62.0307601264892,
71.9453052627917));
#205185=CARTESIAN_POINT('Ctrl Pts',(-23.5921363130452,-62.0851436237892,
71.4087819670163));
#205186=CARTESIAN_POINT('Ctrl Pts',(-23.6163677338717,-62.2602046232303,
70.3453912998643));
#205187=CARTESIAN_POINT('Ctrl Pts',(-23.6283050919866,-62.3807372772904,
69.8195543991636));
#205188=CARTESIAN_POINT('Ctrl Pts',(-23.6548809171447,-62.7250745080482,
68.6550241764099));
#205189=CARTESIAN_POINT('Ctrl Pts',(-23.6693811451348,-62.9667724226921,
68.0232469123233));
#205190=CARTESIAN_POINT('Ctrl Pts',(-23.7137157498716,-63.827887483909,
66.2095881368179));
#205191=CARTESIAN_POINT('Ctrl Pts',(-23.744493151187,-64.5809484779854,
65.1010209222292));
#205192=CARTESIAN_POINT('Ctrl Pts',(-23.7829206451027,-65.7754626425724,
63.8191474354444));
#205193=CARTESIAN_POINT('Ctrl Pts',(-23.7920271109958,-66.0763872068843,
63.5260466635872));
#205194=CARTESIAN_POINT('Ctrl Pts',(-23.8386873210014,-67.6838550110502,
62.1053575149547));
#205195=CARTESIAN_POINT('Ctrl Pts',(-23.8784725722723,-69.1913825338534,
61.2314571897476));
#205196=CARTESIAN_POINT('Ctrl Pts',(-23.9304375078448,-71.4432011399058,
60.4679211891803));
#205197=CARTESIAN_POINT('Ctrl Pts',(-23.944451268879,-72.075814484835,60.3052546592798));
#205198=CARTESIAN_POINT('Ctrl Pts',(-23.9734151603135,-73.3657868000052,
60.0752384248514));
#205199=CARTESIAN_POINT('Ctrl Pts',(-23.9884516930089,-74.021451081523,
60.009079728374));
#205200=CARTESIAN_POINT('Ctrl Pts',(-24.0419614354673,-76.3858270044576,
59.9507329783212));
#205201=CARTESIAN_POINT('Ctrl Pts',(-24.0776364421922,-78.0840502811192,
60.2451583872043));
#205202=CARTESIAN_POINT('Ctrl Pts',(-24.1335183165893,-80.3902635205254,
61.1343653793985));
#205203=CARTESIAN_POINT('Ctrl Pts',(-24.1509196237142,-81.0780618491765,
61.4718643510552));
#205204=CARTESIAN_POINT('Ctrl Pts',(-24.191975435258,-82.6591166877362,
62.4289671184892));
#205205=CARTESIAN_POINT('Ctrl Pts',(-24.2148896691125,-83.5122415194365,
63.1037622587596));
#205206=CARTESIAN_POINT('Ctrl Pts',(-24.253375992345,-84.721255369222,64.33392126898));
#205207=CARTESIAN_POINT('Ctrl Pts',(-24.2680418990414,-85.1363207939457,
64.8239471121187));
#205208=CARTESIAN_POINT('Ctrl Pts',(-24.2940935767868,-85.8152657536147,
65.7574852536921));
#205209=CARTESIAN_POINT('Ctrl Pts',(-24.3055351499505,-86.0921844738963,
66.1898725772783));
#205210=CARTESIAN_POINT('Ctrl Pts',(-24.3281398473406,-86.5941062081981,
67.0862442270561));
#205211=CARTESIAN_POINT('Ctrl Pts',(-24.3392828333263,-86.8185276235538,
67.5495029661639));
#205212=CARTESIAN_POINT('Ctrl Pts',(-24.3504740810588,-87.0149185312533,
68.0248454013453));
#205213=CARTESIAN_POINT('Ctrl Pts',(-25.2581222247366,-62.9850802944281,
77.9529305295057));
#205214=CARTESIAN_POINT('Ctrl Pts',(-25.2371139399055,-63.3447308264597,
78.8234253823906));
#205215=CARTESIAN_POINT('Ctrl Pts',(-25.2154096398342,-63.7981918152589,
79.6529161930109));
#205216=CARTESIAN_POINT('Ctrl Pts',(-25.1819196289562,-64.660700850565,
80.889351340767));
#205217=CARTESIAN_POINT('Ctrl Pts',(-25.1697456138254,-65.0133303636238,
81.3306425360379));
#205218=CARTESIAN_POINT('Ctrl Pts',(-25.1201329901734,-66.5490449435483,
83.0149971167249));
#205219=CARTESIAN_POINT('Ctrl Pts',(-25.0805800079473,-67.9440247118269,
84.0412504740234));
#205220=CARTESIAN_POINT('Ctrl Pts',(-25.0292609529502,-70.0720240720413,
85.0353238642883));
#205221=CARTESIAN_POINT('Ctrl Pts',(-25.0156013108122,-70.6649759484139,
85.2611792869093));
#205222=CARTESIAN_POINT('Ctrl Pts',(-24.9750095399071,-72.4326606250719,
85.790316577514));
#205223=CARTESIAN_POINT('Ctrl Pts',(-24.9470863164347,-73.6361435723789,
85.9737863081481));
#205224=CARTESIAN_POINT('Ctrl Pts',(-24.9074472810636,-75.4215878797593,
85.994728634871));
#205225=CARTESIAN_POINT('Ctrl Pts',(-24.8950686466218,-75.9954684441146,
85.9634276729296));
#205226=CARTESIAN_POINT('Ctrl Pts',(-24.8452804596558,-78.2654540971995,
85.6880829550959));
#205227=CARTESIAN_POINT('Ctrl Pts',(-24.805767495012,-79.9081112242142,
85.1479662718454));
#205228=CARTESIAN_POINT('Ctrl Pts',(-24.7535182298214,-81.9910126324009,
83.9701726844078));
#205229=CARTESIAN_POINT('Ctrl Pts',(-24.7388535666975,-82.5560153403092,
83.5893363069171));
#205230=CARTESIAN_POINT('Ctrl Pts',(-24.69867188384,-83.9815521110443,82.4563454225764));
#205231=CARTESIAN_POINT('Ctrl Pts',(-24.6723892454678,-84.777191987148,
81.632234791459));
#205232=CARTESIAN_POINT('Ctrl Pts',(-24.6343728549608,-85.7938596513943,
80.2564610504218));
#205233=CARTESIAN_POINT('Ctrl Pts',(-24.6220757074884,-86.1021482587485,
79.7761802699739));
#205234=CARTESIAN_POINT('Ctrl Pts',(-24.5723410169992,-87.207375182649,
77.7764145952943));
#205235=CARTESIAN_POINT('Ctrl Pts',(-24.5327923771456,-87.7317495103957,
76.1262380632064));
#205236=CARTESIAN_POINT('Ctrl Pts',(-24.4727154955423,-88.0348717464135,
73.3931830848306));
#205237=CARTESIAN_POINT('Ctrl Pts',(-24.4504231768756,-88.0257007641021,
72.3544900133169));
#205238=CARTESIAN_POINT('Ctrl Pts',(-24.4014705356493,-87.7472570708071,
70.1930457333697));
#205239=CARTESIAN_POINT('Ctrl Pts',(-24.3753730910703,-87.4518616937928,
69.0824179201051));
#205240=CARTESIAN_POINT('Ctrl Pts',(-24.3504740810588,-87.0149185312533,
68.0248454013453));
#205241=CARTESIAN_POINT('Origin',(-21.6548258024609,-75.,72.98888938658));
#205242=CARTESIAN_POINT('',(-27.3772428998354,-62.9850802944281,77.9529305295057));
#205243=CARTESIAN_POINT('',(-27.071820154481,-62.9850802944281,77.9529305295057));
#205244=CARTESIAN_POINT('',(-21.6548258024609,-62.9850802944281,77.9529305295057));
#205245=CARTESIAN_POINT('',(-25.7929126252424,-63.0439273290319,67.8848479330954));
#205246=CARTESIAN_POINT('Ctrl Pts',(-27.3772428998354,-62.9850802944281,
77.9529305295057));
#205247=CARTESIAN_POINT('Ctrl Pts',(-27.3629199848378,-63.2318120975808,
78.5501179254876));
#205248=CARTESIAN_POINT('Ctrl Pts',(-27.3487777117857,-63.522825092598,
79.1283224359325));
#205249=CARTESIAN_POINT('Ctrl Pts',(-27.3167432374599,-64.2661879682576,
80.3659152905382));
#205250=CARTESIAN_POINT('Ctrl Pts',(-27.2988078339567,-64.7385404670655,
81.0099670876734));
#205251=CARTESIAN_POINT('Ctrl Pts',(-27.2639533653288,-65.7802537363062,
82.1864972295272));
#205252=CARTESIAN_POINT('Ctrl Pts',(-27.2470572222126,-66.3443972388745,
82.7192671324979));
#205253=CARTESIAN_POINT('Ctrl Pts',(-27.2168589103768,-67.4082327315602,
83.5577899268292));
#205254=CARTESIAN_POINT('Ctrl Pts',(-27.2038385483791,-67.8874041893299,
83.8860253769056));
#205255=CARTESIAN_POINT('Ctrl Pts',(-27.1718068558823,-69.1270605223102,
84.6184935410882));
#205256=CARTESIAN_POINT('Ctrl Pts',(-27.153075301976,-69.9087850165376,
84.9813302386246));
#205257=CARTESIAN_POINT('Ctrl Pts',(-27.1117001758038,-71.66304607755,85.5928937542637));
#205258=CARTESIAN_POINT('Ctrl Pts',(-27.0893691484628,-72.6402332820879,
85.8118264664918));
#205259=CARTESIAN_POINT('Ctrl Pts',(-27.058137931487,-74.0484977405738,
85.9607580948701));
#205260=CARTESIAN_POINT('Ctrl Pts',(-27.0489528614825,-74.4660695562597,
85.9846445075633));
#205261=CARTESIAN_POINT('Ctrl Pts',(-27.0232634372046,-75.6221972224645,
85.9949554812449));
#205262=CARTESIAN_POINT('Ctrl Pts',(-27.0066641163935,-76.3595533194901,
85.938658020911));
#205263=CARTESIAN_POINT('Ctrl Pts',(-26.9732026303469,-77.8473159642464,
85.6965409593076));
#205264=CARTESIAN_POINT('Ctrl Pts',(-26.9564213215728,-78.5940315824319,
85.5058598959331));
#205265=CARTESIAN_POINT('Ctrl Pts',(-26.9181105876825,-80.2172155340921,
84.9340381390371));
#205266=CARTESIAN_POINT('Ctrl Pts',(-26.8967824074917,-81.0774988763897,
84.5201489840251));
#205267=CARTESIAN_POINT('Ctrl Pts',(-26.8665733823097,-82.2385163399785,
83.7952627014091));
#205268=CARTESIAN_POINT('Ctrl Pts',(-26.8574151612361,-82.581339692512,
83.5575747475936));
#205269=CARTESIAN_POINT('Ctrl Pts',(-26.8292781695803,-83.5889167148567,
82.784705495114));
#205270=CARTESIAN_POINT('Ctrl Pts',(-26.8100732895193,-84.2129557697868,
82.2002385404895));
#205271=CARTESIAN_POINT('Ctrl Pts',(-26.7720941103241,-85.3424817764598,
80.9118601477142));
#205272=CARTESIAN_POINT('Ctrl Pts',(-26.753303317099,-85.8440847764827,
80.2101232663707));
#205273=CARTESIAN_POINT('Ctrl Pts',(-26.7247441938428,-86.4803841279954,
79.1023740556961));
#205274=CARTESIAN_POINT('Ctrl Pts',(-26.7154039726759,-86.6705802017023,
78.7309685675455));
#205275=CARTESIAN_POINT('Ctrl Pts',(-26.687516654797,-87.1869621156996,
77.5905170151558));
#205276=CARTESIAN_POINT('Ctrl Pts',(-26.6692841116462,-87.4572622715524,
76.7985652204479));
#205277=CARTESIAN_POINT('Ctrl Pts',(-26.6330705952091,-87.8335432407178,
75.2105135517567));
#205278=CARTESIAN_POINT('Ctrl Pts',(-26.615132157317,-87.9456009001331,
74.4195782733135));
#205279=CARTESIAN_POINT('Ctrl Pts',(-26.5802741026907,-88.0223050939786,
72.8498560610542));
#205280=CARTESIAN_POINT('Ctrl Pts',(-26.5633772541898,-87.9909070205461,
72.0745076002212));
#205281=CARTESIAN_POINT('Ctrl Pts',(-26.5331691083482,-87.8155575262993,
70.7308942610897));
#205282=CARTESIAN_POINT('Ctrl Pts',(-26.5201397300098,-87.7019475361671,
70.1608885789199));
#205283=CARTESIAN_POINT('Ctrl Pts',(-26.4880993897788,-87.3265303784449,
68.7703861214209));
#205284=CARTESIAN_POINT('Ctrl Pts',(-26.469367816656,-87.0206583434366,
67.9646590272421));
#205285=CARTESIAN_POINT('Ctrl Pts',(-26.4279358786798,-86.1915521415113,
66.2993188834545));
#205286=CARTESIAN_POINT('Ctrl Pts',(-26.4055508421172,-85.6436717340647,
65.4580546557962));
#205287=CARTESIAN_POINT('Ctrl Pts',(-26.3742637420243,-84.7377897463188,
64.3662303866109));
#205288=CARTESIAN_POINT('Ctrl Pts',(-26.3650766230423,-84.4554618402258,
64.0575380091121));
#205289=CARTESIAN_POINT('Ctrl Pts',(-26.3391925499099,-83.6288559059582,
63.2369483463782));
#205290=CARTESIAN_POINT('Ctrl Pts',(-26.3224035255189,-83.0546221804428,
62.7575366580548));
#205291=CARTESIAN_POINT('Ctrl Pts',(-26.288744657427,-81.8110707131792,
61.8892383843992));
#205292=CARTESIAN_POINT('Ctrl Pts',(-26.2719453307364,-81.1418023689104,
61.5053708406699));
#205293=CARTESIAN_POINT('Ctrl Pts',(-26.2323686082621,-79.5281026168419,
60.761456111086));
#205294=CARTESIAN_POINT('Ctrl Pts',(-26.2098478145725,-78.5677958794463,
60.4475697757339));
#205295=CARTESIAN_POINT('Ctrl Pts',(-26.178419829599,-77.170969302484,60.1646211098846));
#205296=CARTESIAN_POINT('Ctrl Pts',(-26.1692271293691,-76.7572395020834,
60.1014120225384));
#205297=CARTESIAN_POINT('Ctrl Pts',(-26.142814409925,-75.5754964523061,
59.9788397979898));
#205298=CARTESIAN_POINT('Ctrl Pts',(-26.1255100904786,-74.8042631984752,
59.9675882242852));
#205299=CARTESIAN_POINT('Ctrl Pts',(-26.0893601842626,-73.1784717009032,
60.0884070018804));
#205300=CARTESIAN_POINT('Ctrl Pts',(-26.0705793196808,-72.3288174455748,
60.237215234787));
#205301=CARTESIAN_POINT('Ctrl Pts',(-26.042047382451,-71.099380616013,60.5808957099613));
#205302=CARTESIAN_POINT('Ctrl Pts',(-26.0327257399638,-70.704253010256,
60.7120943079282));
#205303=CARTESIAN_POINT('Ctrl Pts',(-26.0048113758553,-69.5357311055653,
61.1634258318586));
#205304=CARTESIAN_POINT('Ctrl Pts',(-25.9865326585622,-68.7862798016467,
61.5394572572545));
#205305=CARTESIAN_POINT('Ctrl Pts',(-25.9489134971732,-67.3502583099147,
62.4427544177539));
#205306=CARTESIAN_POINT('Ctrl Pts',(-25.929558754459,-66.6695701650831,
62.9717312372613));
#205307=CARTESIAN_POINT('Ctrl Pts',(-25.8912172492533,-65.414719019039,
64.1638760616071));
#205308=CARTESIAN_POINT('Ctrl Pts',(-25.8721731650173,-64.8451986270309,
64.8256499656624));
#205309=CARTESIAN_POINT('Ctrl Pts',(-25.8427037871473,-64.0902272375414,
65.9053665055431));
#205310=CARTESIAN_POINT('Ctrl Pts',(-25.8327088204804,-63.8533448154717,
66.2843000645008));
#205311=CARTESIAN_POINT('Ctrl Pts',(-25.8127813124671,-63.4181321071454,
67.0675432220405));
#205312=CARTESIAN_POINT('Ctrl Pts',(-25.8028630731624,-63.2203515073318,
67.4714727024354));
#205313=CARTESIAN_POINT('Ctrl Pts',(-25.7929565710457,-63.0438884777109,
67.8848324446381));
#205314=CARTESIAN_POINT('Ctrl Pts',(-25.7925315892805,-63.0438921656051,
67.8848238058572));
#205315=CARTESIAN_POINT('Ctrl Pts',(-25.7738172320668,-62.7100470282805,
68.6668451962005));
#205316=CARTESIAN_POINT('Ctrl Pts',(-25.7554910654483,-62.4537335522494,
69.4797282856584));
#205317=CARTESIAN_POINT('Ctrl Pts',(-25.7174585685912,-62.1044834842583,
71.1393471814885));
#205318=CARTESIAN_POINT('Ctrl Pts',(-25.6982654760424,-62.0114982552743,
71.9819134464724));
#205319=CARTESIAN_POINT('Ctrl Pts',(-25.6580815311061,-61.9889913307642,
73.7950592766215));
#205320=CARTESIAN_POINT('Ctrl Pts',(-25.6373707278172,-62.0850391643306,
74.7609040481865));
#205321=CARTESIAN_POINT('Ctrl Pts',(-25.6073298168377,-62.3662814718529,
76.0762223461048));
#205322=CARTESIAN_POINT('Ctrl Pts',(-25.5988027409165,-62.4612419119342,
76.4417162546856));
#205323=CARTESIAN_POINT('Ctrl Pts',(-25.5810816491096,-62.691769055563,
77.1929608534078));
#205324=CARTESIAN_POINT('Ctrl Pts',(-25.5719178118878,-62.8296852896929,
77.5768138836555));
#205325=CARTESIAN_POINT('Ctrl Pts',(-25.5628518781596,-62.9850802944281,
77.9529305295057));
#205326=CARTESIAN_POINT('Ctrl Pts',(-27.071820154481,-62.9850802944281,
77.9529305295057));
#205327=CARTESIAN_POINT('Ctrl Pts',(-27.0605085630959,-63.1833381622568,
78.4327920565107));
#205328=CARTESIAN_POINT('Ctrl Pts',(-27.049101708122,-63.4103735747692,
78.9008494225221));
#205329=CARTESIAN_POINT('Ctrl Pts',(-27.0197226292045,-64.0551482435365,
80.0489594352128));
#205330=CARTESIAN_POINT('Ctrl Pts',(-27.0015063464426,-64.5081422844583,
80.7060954678677));
#205331=CARTESIAN_POINT('Ctrl Pts',(-26.9591716827354,-65.7149938805126,
82.1524482732041));
#205332=CARTESIAN_POINT('Ctrl Pts',(-26.9361717899996,-66.5135494821474,
82.8965785261809));
#205333=CARTESIAN_POINT('Ctrl Pts',(-26.8941455562996,-68.0553710478556,
84.0086129137462));
#205334=CARTESIAN_POINT('Ctrl Pts',(-26.8756807982664,-68.7585955380911,
84.4216064754456));
#205335=CARTESIAN_POINT('Ctrl Pts',(-26.8189728575791,-71.0278336113285,
85.4821576745034));
#205336=CARTESIAN_POINT('Ctrl Pts',(-26.7836306163197,-72.6849640066519,
85.8923956538304));
#205337=CARTESIAN_POINT('Ctrl Pts',(-26.7312779313272,-75.0002087808532,
86.0039922299509));
#205338=CARTESIAN_POINT('Ctrl Pts',(-26.7169492234306,-75.6276625140699,
85.9888486313766));
#205339=CARTESIAN_POINT('Ctrl Pts',(-26.6742994734323,-77.5315740273115,
85.8046950514129));
#205340=CARTESIAN_POINT('Ctrl Pts',(-26.6471833103362,-78.7861514616839,
85.491643868765));
#205341=CARTESIAN_POINT('Ctrl Pts',(-26.6020301352276,-80.6440099035058,
84.7222013166686));
#205342=CARTESIAN_POINT('Ctrl Pts',(-26.5854317026867,-81.2893519808264,
84.3893059529311));
#205343=CARTESIAN_POINT('Ctrl Pts',(-26.5450219156057,-82.8187606775407,
83.4308013914143));
#205344=CARTESIAN_POINT('Ctrl Pts',(-26.5221896286254,-83.6589081773433,
82.745418781419));
#205345=CARTESIAN_POINT('Ctrl Pts',(-26.4780446566162,-85.0340590756997,
81.3044740726327));
#205346=CARTESIAN_POINT('Ctrl Pts',(-26.4572014070912,-85.5923854343911,
80.580504548093));
#205347=CARTESIAN_POINT('Ctrl Pts',(-26.4036318025543,-86.8409453687443,
78.5523955472661));
#205348=CARTESIAN_POINT('Ctrl Pts',(-26.3728346457446,-87.3936828613449,
77.1790237108958));
#205349=CARTESIAN_POINT('Ctrl Pts',(-26.3244976065549,-87.8482483293957,
75.0816632665241));
#205350=CARTESIAN_POINT('Ctrl Pts',(-26.309023679321,-87.939693929986,74.4106851658523));
#205351=CARTESIAN_POINT('Ctrl Pts',(-26.2641235957008,-88.0551063728715,
72.4048400663272));
#205352=CARTESIAN_POINT('Ctrl Pts',(-26.236068088882,-87.9265379141445,
71.0701429435457));
#205353=CARTESIAN_POINT('Ctrl Pts',(-26.1966699289298,-87.4936517846722,
69.3715812651332));
#205354=CARTESIAN_POINT('Ctrl Pts',(-26.1871415785317,-87.3703257424435,
68.9700224056217));
#205355=CARTESIAN_POINT('Ctrl Pts',(-26.1506331525314,-86.8235764234751,
67.4553166560676));
#205356=CARTESIAN_POINT('Ctrl Pts',(-26.1251170343784,-86.2674471834665,
66.3963153222307));
#205357=CARTESIAN_POINT('Ctrl Pts',(-26.0806649581548,-85.0904635869507,
64.7501647272766));
#205358=CARTESIAN_POINT('Ctrl Pts',(-26.0619069099169,-84.5419049123381,
64.1206280516891));
#205359=CARTESIAN_POINT('Ctrl Pts',(-26.0155474042753,-83.0573098974036,
62.7152958766662));
#205360=CARTESIAN_POINT('Ctrl Pts',(-25.9895183091989,-82.0656527705764,
62.0096573407316));
#205361=CARTESIAN_POINT('Ctrl Pts',(-25.9446017362156,-80.2497908463196,
61.0667794260827));
#205362=CARTESIAN_POINT('Ctrl Pts',(-25.9258205977842,-79.4735168696853,
60.7543225526591));
#205363=CARTESIAN_POINT('Ctrl Pts',(-25.8792531495457,-77.5038511100906,
60.1742348887088));
#205364=CARTESIAN_POINT('Ctrl Pts',(-25.8530429820652,-76.2924140455704,
59.99603259637));
#205365=CARTESIAN_POINT('Ctrl Pts',(-25.7978641992104,-73.7784208884928,
59.9817283532629));
#205366=CARTESIAN_POINT('Ctrl Pts',(-25.7679576827344,-72.4890563234385,
60.1680641200768));
#205367=CARTESIAN_POINT('Ctrl Pts',(-25.7252345790055,-70.6399547469968,
60.7253599424343));
#205368=CARTESIAN_POINT('Ctrl Pts',(-25.7115677709163,-70.0455440165122,
60.9532121513621));
#205369=CARTESIAN_POINT('Ctrl Pts',(-25.6608585552909,-67.943733948015,
61.9410879475899));
#205370=CARTESIAN_POINT('Ctrl Pts',(-25.6219008261576,-66.5714049687478,
62.9487898662649));
#205371=CARTESIAN_POINT('Ctrl Pts',(-25.5674029111497,-64.8778510748112,
64.7908806333424));
#205372=CARTESIAN_POINT('Ctrl Pts',(-25.549760377948,-64.3835663112684,
65.441931124519));
#205373=CARTESIAN_POINT('Ctrl Pts',(-25.5071780938452,-63.377353860841,
67.0636464881761));
#205374=CARTESIAN_POINT('Ctrl Pts',(-25.4819488655821,-62.9205537432864,
68.0612702470938));
#205375=CARTESIAN_POINT('Ctrl Pts',(-25.4375428607864,-62.3153757048581,
69.9939712112621));
#205376=CARTESIAN_POINT('Ctrl Pts',(-25.417562809417,-62.1332992362535,
70.9110885375044));
#205377=CARTESIAN_POINT('Ctrl Pts',(-25.3726675196767,-61.9551318000054,
72.9188124367098));
#205378=CARTESIAN_POINT('Ctrl Pts',(-25.3476385525834,-61.9946232894889,
74.005599743831));
#205379=CARTESIAN_POINT('Ctrl Pts',(-25.3071797422959,-62.289856269085,
75.8216872342338));
#205380=CARTESIAN_POINT('Ctrl Pts',(-25.2909561985297,-62.4762348922606,
76.556496056355));
#205381=CARTESIAN_POINT('Ctrl Pts',(-25.268934758749,-62.8056646343085,
77.5008148037921));
#205382=CARTESIAN_POINT('Ctrl Pts',(-25.2635448812278,-62.8922473331595,
77.7282384805162));
#205383=CARTESIAN_POINT('Ctrl Pts',(-25.2581222247367,-62.9850802944281,
77.9529305295057));
#205384=CARTESIAN_POINT('Origin',(-21.6548258024609,-75.,72.98888938658));
#205385=CARTESIAN_POINT('',(-29.1914736244731,-62.9850802944281,77.9529305295057));
#205386=CARTESIAN_POINT('',(-28.8854250924612,-62.9850802944281,77.9529305295057));
#205387=CARTESIAN_POINT('',(-21.6548258024609,-62.9850802944281,77.9529305295057));
#205388=CARTESIAN_POINT('Ctrl Pts',(-29.1914736244731,-62.9850802944281,
77.9529305295057));
#205389=CARTESIAN_POINT('Ctrl Pts',(-29.1755621721884,-63.2591578354856,
78.6163052989917));
#205390=CARTESIAN_POINT('Ctrl Pts',(-29.1594040788803,-63.5877981516252,
79.2560679492924));
#205391=CARTESIAN_POINT('Ctrl Pts',(-29.1263368716955,-64.3743472329357,
80.5179243315183));
#205392=CARTESIAN_POINT('Ctrl Pts',(-29.1095424566542,-64.8380145192152,
81.1328999266125));
#205393=CARTESIAN_POINT('Ctrl Pts',(-29.0734221104526,-65.9292423739749,
82.3408723417191));
#205394=CARTESIAN_POINT('Ctrl Pts',(-29.054089877859,-66.5669919732695,
82.919781383801));
#205395=CARTESIAN_POINT('Ctrl Pts',(-29.0258111347309,-67.5927591563554,
83.6803490747793));
#205396=CARTESIAN_POINT('Ctrl Pts',(-29.0166214060534,-67.9401399587385,
83.9128494579239));
#205397=CARTESIAN_POINT('Ctrl Pts',(-28.9884263336115,-69.0353829579731,
84.5717936722388));
#205398=CARTESIAN_POINT('Ctrl Pts',(-28.9690997076129,-69.8148721486558,
84.9410760656296));
#205399=CARTESIAN_POINT('Ctrl Pts',(-28.9323737912149,-71.3688686424714,
85.4964360550529));
#205400=CARTESIAN_POINT('Ctrl Pts',(-28.9151159570361,-72.1353086370993,
85.6939031444884));
#205401=CARTESIAN_POINT('Ctrl Pts',(-28.880488831689,-73.6761769729656,
85.9442866240956));
#205402=CARTESIAN_POINT('Ctrl Pts',(-28.8631309851456,-74.4469406872649,
85.9999982835116));
#205403=CARTESIAN_POINT('Ctrl Pts',(-28.8300150987229,-75.9384665632339,
85.9749733885017));
#205404=CARTESIAN_POINT('Ctrl Pts',(-28.8142737633991,-76.6565950375665,
85.9030205174585));
#205405=CARTESIAN_POINT('Ctrl Pts',(-28.7822369910288,-78.0750298881094,
85.6405895141111));
#205406=CARTESIAN_POINT('Ctrl Pts',(-28.7659970656264,-78.7728339413504,
85.4503120997551));
#205407=CARTESIAN_POINT('Ctrl Pts',(-28.7328261718324,-80.175820507993,
84.9390213630989));
#205408=CARTESIAN_POINT('Ctrl Pts',(-28.7159965259154,-80.8754814233276,
84.6110012888045));
#205409=CARTESIAN_POINT('Ctrl Pts',(-28.6812698174062,-82.2249190080084,
83.8251807021196));
#205410=CARTESIAN_POINT('Ctrl Pts',(-28.6635084526963,-82.8702201885422,
83.3659944822798));
#205411=CARTESIAN_POINT('Ctrl Pts',(-28.626929441276,-84.1225480427867,
82.2904716196668));
#205412=CARTESIAN_POINT('Ctrl Pts',(-28.6081295274468,-84.7180178052968,
81.6664721582494));
#205413=CARTESIAN_POINT('Ctrl Pts',(-28.5795486684124,-85.5045511626666,
80.6588937726708));
#205414=CARTESIAN_POINT('Ctrl Pts',(-28.570193195534,-85.7456159824158,
80.3173476616895));
#205415=CARTESIAN_POINT('Ctrl Pts',(-28.5417559073132,-86.4308791313648,
79.2397502921107));
#205416=CARTESIAN_POINT('Ctrl Pts',(-28.523020235589,-86.8189264968287,
78.4707894383435));
#205417=CARTESIAN_POINT('Ctrl Pts',(-28.4867789070654,-87.4058188311497,
76.9499500513124));
#205418=CARTESIAN_POINT('Ctrl Pts',(-28.4694491703824,-87.6188456655288,
76.2074429441466));
#205419=CARTESIAN_POINT('Ctrl Pts',(-28.4332753495974,-87.9277554198034,
74.6055389112504));
#205420=CARTESIAN_POINT('Ctrl Pts',(-28.4144934450725,-88.0063975754321,
73.7465415249287));
#205421=CARTESIAN_POINT('Ctrl Pts',(-28.3859585213444,-87.9963025101264,
72.4698993914055));
#205422=CARTESIAN_POINT('Ctrl Pts',(-28.376634771575,-87.9730259155091,
72.0541011215623));
#205423=CARTESIAN_POINT('Ctrl Pts',(-28.3487236059692,-87.8430715098968,
70.8082898733804));
#205424=CARTESIAN_POINT('Ctrl Pts',(-28.3304501425691,-87.6762258924339,
69.986758647326));
#205425=CARTESIAN_POINT('Ctrl Pts',(-28.2930328738841,-87.1827848282919,
68.3732910096947));
#205426=CARTESIAN_POINT('Ctrl Pts',(-28.2738814873312,-86.8546556479647,
67.5860066595706));
#205427=CARTESIAN_POINT('Ctrl Pts',(-28.2359663672673,-86.0447706375438,
66.0785123439422));
#205428=CARTESIAN_POINT('Ctrl Pts',(-28.2171633117146,-85.5633401429903,
65.3628739021637));
#205429=CARTESIAN_POINT('Ctrl Pts',(-28.1885755944839,-84.7481969832629,
64.3779990500524));
#205430=CARTESIAN_POINT('Ctrl Pts',(-28.1792151542129,-84.4662578931964,
64.0689824667347));
#205431=CARTESIAN_POINT('Ctrl Pts',(-28.1507740214326,-83.560831951342,
63.1679663154694));
#205432=CARTESIAN_POINT('Ctrl Pts',(-28.1320394445061,-82.8931483779347,
62.623727785215));
#205433=CARTESIAN_POINT('Ctrl Pts',(-28.0954542648856,-81.5213277445394,
61.715468453194));
#205434=CARTESIAN_POINT('Ctrl Pts',(-28.0777905124525,-80.8279836820453,
61.3419003843233));
#205435=CARTESIAN_POINT('Ctrl Pts',(-28.0413029644768,-79.3138385090679,
60.6953481352096));
#205436=CARTESIAN_POINT('Ctrl Pts',(-28.0225071271223,-78.4909283062354,
60.4368466474481));
#205437=CARTESIAN_POINT('Ctrl Pts',(-27.993935632166,-77.2398238489032,
60.1764943159538));
#205438=CARTESIAN_POINT('Ctrl Pts',(-27.9845868043934,-76.8272524890396,
60.1111788856647));
#205439=CARTESIAN_POINT('Ctrl Pts',(-27.9567139655793,-75.5831669532874,
59.9752229935156));
#205440=CARTESIAN_POINT('Ctrl Pts',(-27.9385046600024,-74.7472853763196,
59.964615039217));
#205441=CARTESIAN_POINT('Ctrl Pts',(-27.9029475108486,-73.1509483478164,
60.0981690246326));
#205442=CARTESIAN_POINT('Ctrl Pts',(-27.885670168254,-72.3929009548486,
60.2298649264436));
#205443=CARTESIAN_POINT('Ctrl Pts',(-27.8515433038747,-70.9070939213903,
60.6260123463768));
#205444=CARTESIAN_POINT('Ctrl Pts',(-27.8347485680442,-70.1823530868346,
60.8900098978475));
#205445=CARTESIAN_POINT('Ctrl Pts',(-27.7953816908557,-68.5816472958152,
61.639862689273));
#205446=CARTESIAN_POINT('Ctrl Pts',(-27.7730563827175,-67.7297725838768,
62.1657900868321));
#205447=CARTESIAN_POINT('Ctrl Pts',(-27.7418310773711,-66.6183415033926,
63.0429088602213));
#205448=CARTESIAN_POINT('Ctrl Pts',(-27.7326462182551,-66.3028913888067,
63.3175384920493));
#205449=CARTESIAN_POINT('Ctrl Pts',(-27.7069767692208,-65.4691242607782,
64.1172488383875));
#205450=CARTESIAN_POINT('Ctrl Pts',(-27.6903969088421,-64.9814065792122,
64.6719553088264));
#205451=CARTESIAN_POINT('Ctrl Pts',(-27.6569542018304,-64.0863625099057,
65.8836730522086));
#205452=CARTESIAN_POINT('Ctrl Pts',(-27.6401732640537,-63.685186410512,
66.5416750410925));
#205453=CARTESIAN_POINT('Ctrl Pts',(-27.6019784637782,-62.9252502354484,
68.0800545492526));
#205454=CARTESIAN_POINT('Ctrl Pts',(-27.5807611369532,-62.5999289538605,
68.9721117127493));
#205455=CARTESIAN_POINT('Ctrl Pts',(-27.5506635777758,-62.2750570347021,
70.2963863309321));
#205456=CARTESIAN_POINT('Ctrl Pts',(-27.5415074160872,-62.1952730413356,
70.7057528316857));
#205457=CARTESIAN_POINT('Ctrl Pts',(-27.5132372864691,-62.0116317256353,
71.968680244846));
#205458=CARTESIAN_POINT('Ctrl Pts',(-27.493885655565,-61.9726032158218,
72.8292869784305));
#205459=CARTESIAN_POINT('Ctrl Pts',(-27.4557636926057,-62.0650170574753,
74.5466477551924));
#205460=CARTESIAN_POINT('Ctrl Pts',(-27.4369728765414,-62.196445098373,
75.399153925258));
#205461=CARTESIAN_POINT('Ctrl Pts',(-27.4084136951864,-62.5151810677153,
76.6362462977439));
#205462=CARTESIAN_POINT('Ctrl Pts',(-27.3990734339573,-62.6386037251102,
77.0348502593141));
#205463=CARTESIAN_POINT('Ctrl Pts',(-27.3855913578634,-62.8452187583533,
77.6037255106876));
#205464=CARTESIAN_POINT('Ctrl Pts',(-27.3814112768546,-62.9132742983489,
77.7791319544275));
#205465=CARTESIAN_POINT('Ctrl Pts',(-27.3772428998354,-62.9850802944281,
77.9529305295057));
#205466=CARTESIAN_POINT('',(-27.3009674773133,-63.0439273761962,67.8848561928422));
#205467=CARTESIAN_POINT('Ctrl Pts',(-27.3016104665866,-63.0438801073788,
67.8848520519528));
#205468=CARTESIAN_POINT('Ctrl Pts',(-27.2822043952599,-62.7048107611236,
68.6791161785564));
#205469=CARTESIAN_POINT('Ctrl Pts',(-27.2623604194506,-62.4457280137918,
69.5051981159832));
#205470=CARTESIAN_POINT('Ctrl Pts',(-27.2247684323744,-62.0997039577012,
71.1748968405862));
#205471=CARTESIAN_POINT('Ctrl Pts',(-27.2067907395125,-62.0093496555475,
72.0135779289911));
#205472=CARTESIAN_POINT('Ctrl Pts',(-27.1756917833625,-61.9948459983377,
73.4227544982765));
#205473=CARTESIAN_POINT('Ctrl Pts',(-27.1629591529323,-62.0261927256133,
73.9901809827204));
#205474=CARTESIAN_POINT('Ctrl Pts',(-27.1372091243939,-62.1630295671768,
75.1186928323105));
#205475=CARTESIAN_POINT('Ctrl Pts',(-27.1242209431371,-62.2685576332493,
75.6785454171776));
#205476=CARTESIAN_POINT('Ctrl Pts',(-27.0980726651425,-62.5617205545539,
76.8174027048613));
#205477=CARTESIAN_POINT('Ctrl Pts',(-27.0850145343578,-62.7538228583481,
77.3931971498224));
#205478=CARTESIAN_POINT('Ctrl Pts',(-27.071820154481,-62.9850802944281,
77.9529305295057));
#205479=CARTESIAN_POINT('Ctrl Pts',(-28.8854250924612,-62.9850802944281,
77.9529305295057));
#205480=CARTESIAN_POINT('Ctrl Pts',(-28.8824655793347,-63.0358772790107,
78.0758790856261));
#205481=CARTESIAN_POINT('Ctrl Pts',(-28.8795000358553,-63.0885757045039,
78.1980824181724));
#205482=CARTESIAN_POINT('Ctrl Pts',(-28.8672392884279,-63.3138460309727,
78.6991499770645));
#205483=CARTESIAN_POINT('Ctrl Pts',(-28.8579067524138,-63.502667170325,
79.0703865634795));
#205484=CARTESIAN_POINT('Ctrl Pts',(-28.8331156173381,-64.0532943620823,
80.0353275583397));
#205485=CARTESIAN_POINT('Ctrl Pts',(-28.8179202547627,-64.4454316197721,
80.6101584291343));
#205486=CARTESIAN_POINT('Ctrl Pts',(-28.7840050379732,-65.4080639597539,
81.8035269703564));
#205487=CARTESIAN_POINT('Ctrl Pts',(-28.7651855741755,-65.996414212715,
82.4036915784779));
#205488=CARTESIAN_POINT('Ctrl Pts',(-28.7276143167663,-67.2887154577256,
83.4892378536429));
#205489=CARTESIAN_POINT('Ctrl Pts',(-28.7091060250991,-67.9909505633124,
83.9704401572734));
#205490=CARTESIAN_POINT('Ctrl Pts',(-28.6710714995552,-69.489034416249,
84.7943820743572));
#205491=CARTESIAN_POINT('Ctrl Pts',(-28.6517323799731,-70.2823015206987,
85.1331773765378));
#205492=CARTESIAN_POINT('Ctrl Pts',(-28.6235498509551,-71.5008811970346,
85.5160569308502));
#205493=CARTESIAN_POINT('Ctrl Pts',(-28.6143826938631,-71.9043369166701,
85.6218078543965));
#205494=CARTESIAN_POINT('Ctrl Pts',(-28.5866663319979,-73.1293523489743,
85.880680528793));
#205495=CARTESIAN_POINT('Ctrl Pts',(-28.5678985716926,-73.9612676513088,
85.974212703464));
#205496=CARTESIAN_POINT('Ctrl Pts',(-28.531333297673,-75.605680191057,85.9999722142122));
#205497=CARTESIAN_POINT('Ctrl Pts',(-28.5136766214303,-76.4143968440435,
85.9370403358745));
#205498=CARTESIAN_POINT('Ctrl Pts',(-28.4765401100638,-78.059918010105,
85.6529057517265));
#205499=CARTESIAN_POINT('Ctrl Pts',(-28.4571926682296,-78.8912150091837,
85.422668558253));
#205500=CARTESIAN_POINT('Ctrl Pts',(-28.4290213078015,-80.0816420114004,
84.9617761961946));
#205501=CARTESIAN_POINT('Ctrl Pts',(-28.4198731218469,-80.462199939638,
84.793018997335));
#205502=CARTESIAN_POINT('Ctrl Pts',(-28.3921519553204,-81.5816459408153,
84.2308579975198));
#205503=CARTESIAN_POINT('Ctrl Pts',(-28.3733616829992,-82.2912915357417,
83.7841186163781));
#205504=CARTESIAN_POINT('Ctrl Pts',(-28.3356090360205,-83.6337639378527,
82.7458663572929));
#205505=CARTESIAN_POINT('Ctrl Pts',(-28.316851665917,-84.2605066764315,
82.1531406746028));
#205506=CARTESIAN_POINT('Ctrl Pts',(-28.2785424006694,-85.3875212687281,
80.8527031060992));
#205507=CARTESIAN_POINT('Ctrl Pts',(-28.2592282455856,-85.8850413062418,
80.1482225450452));
#205508=CARTESIAN_POINT('Ctrl Pts',(-28.2310242805193,-86.5156813028842,
79.0357238888119));
#205509=CARTESIAN_POINT('Ctrl Pts',(-28.2218167549783,-86.7043522748128,
78.6619186330587));
#205510=CARTESIAN_POINT('Ctrl Pts',(-28.1935087511738,-87.224423088215,
77.494667323832));
#205511=CARTESIAN_POINT('Ctrl Pts',(-28.174165356958,-87.4954779101746,
76.6769212038579));
#205512=CARTESIAN_POINT('Ctrl Pts',(-28.1354288842283,-87.8783888984185,
74.9725128564299));
#205513=CARTESIAN_POINT('Ctrl Pts',(-28.1160379031832,-87.9837419388559,
74.0889426736047));
#205514=CARTESIAN_POINT('Ctrl Pts',(-28.0780343535472,-88.0116076500931,
72.3857529019448));
#205515=CARTESIAN_POINT('Ctrl Pts',(-28.0597797126823,-87.9481231107597,
71.5705006207187));
#205516=CARTESIAN_POINT('Ctrl Pts',(-28.0233789710146,-87.665858585689,
69.9436118868057));
#205517=CARTESIAN_POINT('Ctrl Pts',(-28.004920380141,-87.4440862150033,
69.1363059541179));
#205518=CARTESIAN_POINT('Ctrl Pts',(-27.9768517933053,-86.996931562581,
67.9639966602238));
#205519=CARTESIAN_POINT('Ctrl Pts',(-27.9674592017099,-86.8285779729279,
67.5795770417272));
#205520=CARTESIAN_POINT('Ctrl Pts',(-27.9363387786485,-86.2034007776042,
66.3214313900472));
#205521=CARTESIAN_POINT('Ctrl Pts',(-27.9147711115775,-85.6659305417049,
65.4916152787042));
#205522=CARTESIAN_POINT('Ctrl Pts',(-27.8833998203224,-84.7745594953122,
64.4079550040323));
#205523=CARTESIAN_POINT('Ctrl Pts',(-27.8740344559414,-84.4938395378865,
64.0983629976914));
#205524=CARTESIAN_POINT('Ctrl Pts',(-27.8480890864951,-83.6686900736822,
63.2720783091558));
#205525=CARTESIAN_POINT('Ctrl Pts',(-27.8317104287565,-83.0937338446361,
62.7881989913403));
#205526=CARTESIAN_POINT('Ctrl Pts',(-27.7979650810881,-81.8512099718502,
61.9140300097616));
#205527=CARTESIAN_POINT('Ctrl Pts',(-27.7806504762213,-81.1841122769408,
61.5281589163973));
#205528=CARTESIAN_POINT('Ctrl Pts',(-27.7428609581753,-79.6382848471565,
60.8084786023036));
#205529=CARTESIAN_POINT('Ctrl Pts',(-27.7223959097572,-78.7495511502333,
60.5062226702327));
#205530=CARTESIAN_POINT('Ctrl Pts',(-27.6921817138872,-77.429474847673,
60.211125373953));
#205531=CARTESIAN_POINT('Ctrl Pts',(-27.6828380244843,-77.0187214407476,
60.1398285331527));
#205532=CARTESIAN_POINT('Ctrl Pts',(-27.6544110533982,-75.7525834549773,
59.9822785596287));
#205533=CARTESIAN_POINT('Ctrl Pts',(-27.6356910284017,-74.8914904492901,
59.9609756913596));
#205534=CARTESIAN_POINT('Ctrl Pts',(-27.5974446215772,-73.1765211424777,
60.0886827820958));
#205535=CARTESIAN_POINT('Ctrl Pts',(-27.5780981620778,-72.3268867517458,
60.2376195978667));
#205536=CARTESIAN_POINT('Ctrl Pts',(-27.5499260062608,-71.0974578197744,
60.581498901876));
#205537=CARTESIAN_POINT('Ctrl Pts',(-27.540775909522,-70.7023113279648,
60.712772486862));
#205538=CARTESIAN_POINT('Ctrl Pts',(-27.5130551559875,-69.533893804592,
61.1642803011753));
#205539=CARTESIAN_POINT('Ctrl Pts',(-27.4942668993613,-68.7845696208448,
61.5403913624682));
#205540=CARTESIAN_POINT('Ctrl Pts',(-27.4565944832196,-67.3511627671109,
62.4423309471043));
#205541=CARTESIAN_POINT('Ctrl Pts',(-27.4379095124625,-66.672649402451,
62.9694161330161));
#205542=CARTESIAN_POINT('Ctrl Pts',(-27.3994173835239,-65.4184273779293,
64.1597368892016));
#205543=CARTESIAN_POINT('Ctrl Pts',(-27.3798457176042,-64.8478964836777,
64.822171974088));
#205544=CARTESIAN_POINT('Ctrl Pts',(-27.3507575415468,-64.0916824146765,
65.9030914571655));
#205545=CARTESIAN_POINT('Ctrl Pts',(-27.3409191317284,-63.8544409354465,
66.2824419366119));
#205546=CARTESIAN_POINT('Ctrl Pts',(-27.3210268214252,-63.4186041746793,
67.0665787968306));
#205547=CARTESIAN_POINT('Ctrl Pts',(-27.3109849659766,-63.2205605326239,
67.4709825907912));
#205548=CARTESIAN_POINT('Ctrl Pts',(-27.3009162452285,-63.0438863592108,
67.8848374071685));
#205549=CARTESIAN_POINT('Origin',(-21.6548258024609,-75.,72.98888938658));
#205550=CARTESIAN_POINT('',(-31.0052564152503,-62.9850802944281,77.9529305295057));
#205551=CARTESIAN_POINT('',(-30.6991941617974,-62.9850802944281,77.9529305295057));
#205552=CARTESIAN_POINT('',(-21.6548258024609,-62.9850802944281,77.9529305295057));
#205553=CARTESIAN_POINT('Ctrl Pts',(-31.0052564152503,-62.9850802944281,
77.9529305295057));
#205554=CARTESIAN_POINT('Ctrl Pts',(-30.998890721168,-63.0941305563431,
78.2168747844095));
#205555=CARTESIAN_POINT('Ctrl Pts',(-30.992546634712,-63.211905957649,78.4772925112609));
#205556=CARTESIAN_POINT('Ctrl Pts',(-30.977020603939,-63.5219807092366,
79.1067278389773));
#205557=CARTESIAN_POINT('Ctrl Pts',(-30.9678790268683,-63.7235073326383,
79.470678282968));
#205558=CARTESIAN_POINT('Ctrl Pts',(-30.9397116448984,-64.3945669932255,
80.5562669748228));
#205559=CARTESIAN_POINT('Ctrl Pts',(-30.9203616937345,-64.9185583979383,
81.2414609983222));
#205560=CARTESIAN_POINT('Ctrl Pts',(-30.8821217527453,-66.0933516303725,
82.4972986267386));
#205561=CARTESIAN_POINT('Ctrl Pts',(-30.8634032798322,-66.7410769815901,
83.0650205822738));
#205562=CARTESIAN_POINT('Ctrl Pts',(-30.8349730262052,-67.7789653735092,
83.8069395387207));
#205563=CARTESIAN_POINT('Ctrl Pts',(-30.8256308472951,-68.1293227337512,
84.0327720483039));
#205564=CARTESIAN_POINT('Ctrl Pts',(-30.7955149464664,-69.2964528224528,
84.7080097513539));
#205565=CARTESIAN_POINT('Ctrl Pts',(-30.7751434413671,-70.1508200863168,
85.0865617937747));
#205566=CARTESIAN_POINT('Ctrl Pts',(-30.7452056164092,-71.4373644781035,
85.4982138897057));
#205567=CARTESIAN_POINT('Ctrl Pts',(-30.7358184244919,-71.8423845949013,
85.606537092857));
#205568=CARTESIAN_POINT('Ctrl Pts',(-30.7077965975312,-73.0667863961338,
85.8713481494891));
#205569=CARTESIAN_POINT('Ctrl Pts',(-30.6893835088621,-73.8967163923041,
85.9687904354329));
#205570=CARTESIAN_POINT('Ctrl Pts',(-30.6530238437094,-75.5455739484342,
86.0030124810472));
#205571=CARTESIAN_POINT('Ctrl Pts',(-30.6347672198482,-76.3606887553969,
85.9431769171672));
#205572=CARTESIAN_POINT('Ctrl Pts',(-30.5969613111317,-78.0319612450622,
85.6609303910857));
#205573=CARTESIAN_POINT('Ctrl Pts',(-30.5777484996156,-78.8820214190536,
85.4268680252424));
#205574=CARTESIAN_POINT('Ctrl Pts',(-30.5391876937375,-80.5030966674773,
84.7979716319442));
#205575=CARTESIAN_POINT('Ctrl Pts',(-30.5198459968039,-81.2714860176536,
84.4084764121768));
#205576=CARTESIAN_POINT('Ctrl Pts',(-30.4915427153229,-82.3484255275656,
83.7208822183712));
#205577=CARTESIAN_POINT('Ctrl Pts',(-30.4823380508623,-82.6899721208454,
83.4788539719696));
#205578=CARTESIAN_POINT('Ctrl Pts',(-30.4541354293864,-83.6964098417668,
82.6900575269572));
#205579=CARTESIAN_POINT('Ctrl Pts',(-30.4348190771385,-84.3192090680501,
82.0934233462604));
#205580=CARTESIAN_POINT('Ctrl Pts',(-30.3979038826536,-85.3972083610225,
80.8333015749217));
#205581=CARTESIAN_POINT('Ctrl Pts',(-30.3804678067385,-85.8589996796079,
80.1804721619447));
#205582=CARTESIAN_POINT('Ctrl Pts',(-30.3437108636977,-86.6877136293555,
78.7452595555407));
#205583=CARTESIAN_POINT('Ctrl Pts',(-30.3243708426616,-87.042570297055,
77.9603033557304));
#205584=CARTESIAN_POINT('Ctrl Pts',(-30.2960721159481,-87.451123536123,
76.7498013011091));
#205585=CARTESIAN_POINT('Ctrl Pts',(-30.2868702150667,-87.5656716688902,
76.3472865609622));
#205586=CARTESIAN_POINT('Ctrl Pts',(-30.2586689271407,-87.8559252135777,
75.1020439280308));
#205587=CARTESIAN_POINT('Ctrl Pts',(-30.2393505283487,-87.9675689660564,
74.2468159420369));
#205588=CARTESIAN_POINT('Ctrl Pts',(-30.2024711015591,-88.0182879167508,
72.5908060001859));
#205589=CARTESIAN_POINT('Ctrl Pts',(-30.1850687819595,-87.9694642594319,
71.7942011149537));
#205590=CARTESIAN_POINT('Ctrl Pts',(-30.1483453184102,-87.7170528784014,
70.1578113597426));
#205591=CARTESIAN_POINT('Ctrl Pts',(-30.129005666849,-87.5021665916542,
69.3236095689898));
#205592=CARTESIAN_POINT('Ctrl Pts',(-30.0976361792611,-87.0149633074977,
67.9938113137064));
#205593=CARTESIAN_POINT('Ctrl Pts',(-30.0854255918818,-86.7899758709906,
67.4837449317751));
#205594=CARTESIAN_POINT('Ctrl Pts',(-30.0559991048539,-86.176409896406,
66.3042153825508));
#205595=CARTESIAN_POINT('Ctrl Pts',(-30.038604703564,-85.759443167482,65.6519020193313));
#205596=CARTESIAN_POINT('Ctrl Pts',(-30.0033441253496,-84.789625849535,
64.3967389026165));
#205597=CARTESIAN_POINT('Ctrl Pts',(-29.9856049016184,-84.2328945423459,
63.8010997569562));
#205598=CARTESIAN_POINT('Ctrl Pts',(-29.9582198007299,-83.3120931500439,
62.9847381498667));
#205599=CARTESIAN_POINT('Ctrl Pts',(-29.9488670351272,-82.9868916860702,
62.7232430077088));
#205600=CARTESIAN_POINT('Ctrl Pts',(-29.9181246703679,-81.8746058136736,
61.9137490513676));
#205601=CARTESIAN_POINT('Ctrl Pts',(-29.8971567085003,-81.0395098635633,
61.4371254331555));
#205602=CARTESIAN_POINT('Ctrl Pts',(-29.8568706494704,-79.3706319919682,
60.7154828891975));
#205603=CARTESIAN_POINT('Ctrl Pts',(-29.837515411314,-78.5497294698801,
60.4534055255968));
#205604=CARTESIAN_POINT('Ctrl Pts',(-29.8057525708868,-77.1480165547809,
60.1547552842987));
#205605=CARTESIAN_POINT('Ctrl Pts',(-29.7931778075746,-76.5797519590921,
60.0724906885349));
#205606=CARTESIAN_POINT('Ctrl Pts',(-29.7633617608987,-75.2363492402821,
59.9680193058401));
#205607=CARTESIAN_POINT('Ctrl Pts',(-29.7459400975722,-74.4609644233192,
59.9770349905027));
#205608=CARTESIAN_POINT('Ctrl Pts',(-29.7105146841467,-72.8756579113476,
60.1374783268624));
#205609=CARTESIAN_POINT('Ctrl Pts',(-29.6926466581456,-72.0699435804465,
60.2969092162341));
#205610=CARTESIAN_POINT('Ctrl Pts',(-29.6557636623742,-70.4817919903966,
60.770556621236));
#205611=CARTESIAN_POINT('Ctrl Pts',(-29.6369550883942,-69.7039845516747,
61.0870368054686));
#205612=CARTESIAN_POINT('Ctrl Pts',(-29.6028427678378,-68.3384995671798,
61.8031764171198));
#205613=CARTESIAN_POINT('Ctrl Pts',(-29.5874452410841,-67.7425489572604,
62.1803202522952));
#205614=CARTESIAN_POINT('Ctrl Pts',(-29.5624436415863,-66.8475595708902,
62.8542470383659));
#205615=CARTESIAN_POINT('Ctrl Pts',(-29.5531115347342,-66.5272597426852,
63.1204582288388));
#205616=CARTESIAN_POINT('Ctrl Pts',(-29.5237793391725,-65.5579295318565,
64.0081358404112));
#205617=CARTESIAN_POINT('Ctrl Pts',(-29.5041537322335,-64.9602157775129,
64.6817025881481));
#205618=CARTESIAN_POINT('Ctrl Pts',(-29.4651861012681,-63.9357819911559,
66.1098130782895));
#205619=CARTESIAN_POINT('Ctrl Pts',(-29.4458405951834,-63.5053245953175,
66.856104093393));
#205620=CARTESIAN_POINT('Ctrl Pts',(-29.4175265459778,-62.9794073986883,
68.0209322914322));
#205621=CARTESIAN_POINT('Ctrl Pts',(-29.4083153639602,-62.8256744199076,
68.4105664141887));
#205622=CARTESIAN_POINT('Ctrl Pts',(-29.3801097432522,-62.4142571445577,
69.6215155846038));
#205623=CARTESIAN_POINT('Ctrl Pts',(-29.3607985206994,-62.2190493172461,
70.4615552278131));
#205624=CARTESIAN_POINT('Ctrl Pts',(-29.3224102244011,-61.9969896193244,
72.1714716312305));
#205625=CARTESIAN_POINT('Ctrl Pts',(-29.3035783644143,-61.9714118259082,
73.037208427361));
#205626=CARTESIAN_POINT('Ctrl Pts',(-29.265745472525,-62.0904804272812,
74.7336990427337));
#205627=CARTESIAN_POINT('Ctrl Pts',(-29.2469537725319,-62.2295006742594,
75.5607405632176));
#205628=CARTESIAN_POINT('Ctrl Pts',(-29.2192323662553,-62.5551834904872,
76.7703707735546));
#205629=CARTESIAN_POINT('Ctrl Pts',(-29.2100854648056,-62.6825569506798,
77.1666467030544));
#205630=CARTESIAN_POINT('Ctrl Pts',(-29.1977659444505,-62.8786772013591,
77.6892895044013));
#205631=CARTESIAN_POINT('Ctrl Pts',(-29.1946243175987,-62.9308090557598,
77.8215729206249));
#205632=CARTESIAN_POINT('Ctrl Pts',(-29.1914736244731,-62.9850802944281,
77.9529305295057));
#205633=CARTESIAN_POINT('Ctrl Pts',(-30.6991941617974,-62.9850802944281,
77.9529305295057));
#205634=CARTESIAN_POINT('Ctrl Pts',(-30.6834875022977,-63.2546150961368,
78.6053100942889));
#205635=CARTESIAN_POINT('Ctrl Pts',(-30.6680646534122,-63.5769357250135,
79.2348940795638));
#205636=CARTESIAN_POINT('Ctrl Pts',(-30.6351661799762,-64.3585113190455,
80.4964509355169));
#205637=CARTESIAN_POINT('Ctrl Pts',(-30.617686959713,-64.8265610851101,
81.1194423482921));
#205638=CARTESIAN_POINT('Ctrl Pts',(-30.5812917504611,-65.9230302133756,
82.3348469913923));
#205639=CARTESIAN_POINT('Ctrl Pts',(-30.5625565966539,-66.5604279558448,
82.9142072904607));
#205640=CARTESIAN_POINT('Ctrl Pts',(-30.5341175409341,-67.5858569784203,
83.6755700981386));
#205641=CARTESIAN_POINT('Ctrl Pts',(-30.524759796166,-67.9332224300424,
83.9083818207445));
#205642=CARTESIAN_POINT('Ctrl Pts',(-30.4961757833447,-69.0281749019354,
84.5680775452673));
#205643=CARTESIAN_POINT('Ctrl Pts',(-30.4773744419406,-69.8074164205763,
84.9378379287985));
#205644=CARTESIAN_POINT('Ctrl Pts',(-30.4407631920056,-71.363013246297,
85.49486628652));
#205645=CARTESIAN_POINT('Ctrl Pts',(-30.4229673875379,-72.1314036944881,
85.6931514335511));
#205646=CARTESIAN_POINT('Ctrl Pts',(-30.3882077810968,-73.6741446105418,
85.9440701974626));
#205647=CARTESIAN_POINT('Ctrl Pts',(-30.3713805720921,-74.4447547431935,
85.9998966561631));
#205648=CARTESIAN_POINT('Ctrl Pts',(-30.3381954147462,-75.9384620544506,
85.9751027001332));
#205649=CARTESIAN_POINT('Ctrl Pts',(-30.3219380215226,-76.6589057223357,
85.9028536120398));
#205650=CARTESIAN_POINT('Ctrl Pts',(-30.2898766920797,-78.0783486956509,
85.6397139236142));
#205651=CARTESIAN_POINT('Ctrl Pts',(-30.2741277391873,-78.7749469039115,
85.4496026577444));
#205652=CARTESIAN_POINT('Ctrl Pts',(-30.2410058827323,-80.17670479936,84.9386341964782));
#205653=CARTESIAN_POINT('Ctrl Pts',(-30.2236501801243,-80.8762842245382,
84.6105912010411));
#205654=CARTESIAN_POINT('Ctrl Pts',(-30.1889939369837,-82.2264106548325,
83.8242530979522));
#205655=CARTESIAN_POINT('Ctrl Pts',(-30.1717043987287,-82.8723858416748,
83.3644214828119));
#205656=CARTESIAN_POINT('Ctrl Pts',(-30.1349447443021,-84.1251055584975,
82.2879618490551));
#205657=CARTESIAN_POINT('Ctrl Pts',(-30.1156198528516,-84.720402534393,
81.6638006619738));
#205658=CARTESIAN_POINT('Ctrl Pts',(-30.0874233500389,-85.5067000810964,
80.6559535241312));
#205659=CARTESIAN_POINT('Ctrl Pts',(-30.0782309027172,-85.7477067400808,
80.3142848458829));
#205660=CARTESIAN_POINT('Ctrl Pts',(-30.0499477074069,-86.432701672043,
79.2364185980071));
#205661=CARTESIAN_POINT('Ctrl Pts',(-30.0306136796111,-86.8205316189747,
78.4673298953421));
#205662=CARTESIAN_POINT('Ctrl Pts',(-29.9943582613737,-87.4084050070124,
76.9426142362739));
#205663=CARTESIAN_POINT('Ctrl Pts',(-29.9774277284058,-87.6219691973624,
76.1961243245901));
#205664=CARTESIAN_POINT('Ctrl Pts',(-29.9410515613661,-87.9296922244751,
74.5899724056542));
#205665=CARTESIAN_POINT('Ctrl Pts',(-29.9217091327305,-88.0073005875433,
73.7308796686119));
#205666=CARTESIAN_POINT('Ctrl Pts',(-29.8935307168148,-87.9956649448971,
72.4539048682318));
#205667=CARTESIAN_POINT('Ctrl Pts',(-29.8843706324287,-87.9718515197332,
72.0377932595794));
#205668=CARTESIAN_POINT('Ctrl Pts',(-29.8566521965401,-87.8403258599408,
70.7924099816888));
#205669=CARTESIAN_POINT('Ctrl Pts',(-29.8378757243073,-87.6726051772351,
69.9716799218347));
#205670=CARTESIAN_POINT('Ctrl Pts',(-29.8008659262362,-87.1840607839475,
68.3807326608909));
#205671=CARTESIAN_POINT('Ctrl Pts',(-29.7827974452962,-86.8656900947358,
67.6137753751178));
#205672=CARTESIAN_POINT('Ctrl Pts',(-29.7452214015567,-86.0723171916274,
66.1227272554252));
#205673=CARTESIAN_POINT('Ctrl Pts',(-29.7258844671488,-85.5937076972293,
65.4051068092107));
#205674=CARTESIAN_POINT('Ctrl Pts',(-29.69769942545,-84.7831071765765,64.4177329142406));
#205675=CARTESIAN_POINT('Ctrl Pts',(-29.6885278844453,-84.5031384581846,
64.1083337404917));
#205676=CARTESIAN_POINT('Ctrl Pts',(-29.6608129837716,-83.6194854807112,
63.2215199236546));
#205677=CARTESIAN_POINT('Ctrl Pts',(-29.642050821599,-82.9745871531718,
62.6882592595166));
#205678=CARTESIAN_POINT('Ctrl Pts',(-29.6057630222183,-81.622457439973,
61.7737650850085));
#205679=CARTESIAN_POINT('Ctrl Pts',(-29.5883632773671,-80.9221760565283,
61.3887258931024));
#205680=CARTESIAN_POINT('Ctrl Pts',(-29.5534121049914,-79.4809533117132,
60.761014219963));
#205681=CARTESIAN_POINT('Ctrl Pts',(-29.5359768303154,-78.7446455743179,
60.5158180760146));
#205682=CARTESIAN_POINT('Ctrl Pts',(-29.5059736902797,-77.4249776149149,
60.2038333839358));
#205683=CARTESIAN_POINT('Ctrl Pts',(-29.4932246054559,-76.8507107369019,
60.1081656154282));
#205684=CARTESIAN_POINT('Ctrl Pts',(-29.4612737537624,-75.4163655160643,
59.967146810556));
#205685=CARTESIAN_POINT('Ctrl Pts',(-29.4419130739226,-74.5545228835481,
59.9681102913339));
#205686=CARTESIAN_POINT('Ctrl Pts',(-29.4005791689679,-72.6975463410855,
60.1548729748301));
#205687=CARTESIAN_POINT('Ctrl Pts',(-29.3785386832832,-71.7110658675101,
60.3715921265403));
#205688=CARTESIAN_POINT('Ctrl Pts',(-29.3466721256527,-70.3641054547977,
60.8363818267652));
#205689=CARTESIAN_POINT('Ctrl Pts',(-29.3372957503625,-69.9755182409595,
60.9918254576043));
#205690=CARTESIAN_POINT('Ctrl Pts',(-29.3109609411101,-68.8961026251919,
61.4852749580094));
#205691=CARTESIAN_POINT('Ctrl Pts',(-29.2941686401751,-68.2268157522594,
61.8661788100289));
#205692=CARTESIAN_POINT('Ctrl Pts',(-29.257940853399,-66.8878720503737,
62.7940971908772));
#205693=CARTESIAN_POINT('Ctrl Pts',(-29.2385928281301,-66.2310421640931,
63.3532370354826));
#205694=CARTESIAN_POINT('Ctrl Pts',(-29.2104223633023,-65.3457869125314,
64.2728569247223));
#205695=CARTESIAN_POINT('Ctrl Pts',(-29.2012756705988,-65.0718384593771,
64.5862314377127));
#205696=CARTESIAN_POINT('Ctrl Pts',(-29.1735542263521,-64.2935483120385,
65.5678390535729));
#205697=CARTESIAN_POINT('Ctrl Pts',(-29.1547622954661,-63.8382237515122,
66.2721318653139));
#205698=CARTESIAN_POINT('Ctrl Pts',(-29.1169163552933,-63.0564883780533,
67.7831284393971));
#205699=CARTESIAN_POINT('Ctrl Pts',(-29.0980723811611,-62.7368132410658,
68.5886992064822));
#205700=CARTESIAN_POINT('Ctrl Pts',(-29.0596712387894,-62.2632974701733,
70.2472623241974));
#205701=CARTESIAN_POINT('Ctrl Pts',(-29.0403605035061,-62.1098190770359,
71.0959136064054));
#205702=CARTESIAN_POINT('Ctrl Pts',(-29.0121546226142,-62.0079551746448,
72.370799304808));
#205703=CARTESIAN_POINT('Ctrl Pts',(-29.002942850328,-61.9947894974669,
72.7894815358302));
#205704=CARTESIAN_POINT('Ctrl Pts',(-28.9746278241255,-62.016337702273,
74.067379836155));
#205705=CARTESIAN_POINT('Ctrl Pts',(-28.9552819832539,-62.1160057774037,
74.9231370905748));
#205706=CARTESIAN_POINT('Ctrl Pts',(-28.9192277040408,-62.4629931277269,
76.5118656446705));
#205707=CARTESIAN_POINT('Ctrl Pts',(-28.9024715478143,-62.6924955033703,
77.2447609816684));
#205708=CARTESIAN_POINT('Ctrl Pts',(-28.8854250924612,-62.9850802944281,
77.9529305295057));
#205709=CARTESIAN_POINT('Origin',(-21.6548258024609,-75.,72.98888938658));
#205710=CARTESIAN_POINT('',(-32.819270903196,-62.9850802944281,77.9529305295057));
#205711=CARTESIAN_POINT('',(-32.5134098057851,-62.9850802944281,77.9529305295057));
#205712=CARTESIAN_POINT('',(-21.6548258024609,-62.9850802944281,77.9529305295057));
#205713=CARTESIAN_POINT('',(-31.8032572668915,-84.3357280630092,63.9421119750625));
#205714=CARTESIAN_POINT('Ctrl Pts',(-31.8032572668915,-84.3357280630092,
63.9421119750625));
#205715=CARTESIAN_POINT('Ctrl Pts',(-31.8137268296502,-84.6662804770869,
64.2832221083208));
#205716=CARTESIAN_POINT('Ctrl Pts',(-31.8242105474278,-84.9778883827939,
64.6421916720238));
#205717=CARTESIAN_POINT('Ctrl Pts',(-31.8452661078821,-85.558044034709,
65.3895689566823));
#205718=CARTESIAN_POINT('Ctrl Pts',(-31.8558207746628,-85.8264924884276,
65.7771611941525));
#205719=CARTESIAN_POINT('Ctrl Pts',(-31.8870392024047,-86.5581835076886,
66.9668434036295));
#205720=CARTESIAN_POINT('Ctrl Pts',(-31.9072090633639,-86.9574808246518,
67.804750359145));
#205721=CARTESIAN_POINT('Ctrl Pts',(-31.9438558392689,-87.5045856463217,
69.361228744241));
#205722=CARTESIAN_POINT('Ctrl Pts',(-31.9601457568728,-87.6872416449994,
70.0634020317026));
#205723=CARTESIAN_POINT('Ctrl Pts',(-31.993669338487,-87.9440636466703,
71.5509028311772));
#205724=CARTESIAN_POINT('Ctrl Pts',(-32.0108132108122,-88.007278414284,
72.3352026728299));
#205725=CARTESIAN_POINT('Ctrl Pts',(-32.041413459719,-87.9933581299314,
73.7111701669863));
#205726=CARTESIAN_POINT('Ctrl Pts',(-32.0546718044928,-87.9471161615131,
74.3008439158162));
#205727=CARTESIAN_POINT('Ctrl Pts',(-32.0851344571267,-87.7478091296771,
75.6524738326175));
#205728=CARTESIAN_POINT('Ctrl Pts',(-32.1020536637848,-87.5662736943747,
76.4079661630273));
#205729=CARTESIAN_POINT('Ctrl Pts',(-32.1370010492423,-87.0627838574,77.9010874580178));
#205730=CARTESIAN_POINT('Ctrl Pts',(-32.1550099680091,-86.7375957907177,
78.6341778642299));
#205731=CARTESIAN_POINT('Ctrl Pts',(-32.1912934650356,-85.9396264269875,
80.0614936447038));
#205732=CARTESIAN_POINT('Ctrl Pts',(-32.2095283583469,-85.4629113018594,
80.7493438556071));
#205733=CARTESIAN_POINT('Ctrl Pts',(-32.2401738889961,-84.5742243220643,
81.7994869097814));
#205734=CARTESIAN_POINT('Ctrl Pts',(-32.2523110403474,-84.1995002523804,
82.1900628608691));
#205735=CARTESIAN_POINT('Ctrl Pts',(-32.2737175034811,-83.4924804529018,
82.8404954068366));
#205736=CARTESIAN_POINT('Ctrl Pts',(-32.2829621282018,-83.1698192144293,
83.109680843072));
#205737=CARTESIAN_POINT('Ctrl Pts',(-32.3106727048045,-82.1666891250305,
83.8672771165417));
#205738=CARTESIAN_POINT('Ctrl Pts',(-32.3292499662116,-81.4515148297491,
84.3060753253936));
#205739=CARTESIAN_POINT('Ctrl Pts',(-32.3662481136558,-79.9652516271433,
85.0310242120193));
#205740=CARTESIAN_POINT('Ctrl Pts',(-32.3841858647311,-79.1992642429188,
85.3190523791631));
#205741=CARTESIAN_POINT('Ctrl Pts',(-32.4220642430902,-77.5452463858179,
85.7688466228141));
#205742=CARTESIAN_POINT('Ctrl Pts',(-32.4422074650899,-76.6570952085571,
85.9140432257214));
#205743=CARTESIAN_POINT('Ctrl Pts',(-32.4792994256479,-74.9927441127254,
86.0116521763215));
#205744=CARTESIAN_POINT('Ctrl Pts',(-32.4960937321176,-74.2219013652736,
85.988388222726));
#205745=CARTESIAN_POINT('Ctrl Pts',(-32.529353314226,-72.7348060805604,
85.81070167596));
#205746=CARTESIAN_POINT('Ctrl Pts',(-32.5457254327998,-72.0204897610094,
85.6637655202297));
#205747=CARTESIAN_POINT('Ctrl Pts',(-32.579257934671,-70.5726847695437,
85.2367297597932));
#205748=CARTESIAN_POINT('Ctrl Pts',(-32.5963180037202,-69.8445870749277,
84.9485064312127));
#205749=CARTESIAN_POINT('Ctrl Pts',(-32.6269769784201,-68.6132659357982,
84.3276132039394));
#205750=CARTESIAN_POINT('Ctrl Pts',(-32.6403853306936,-68.0989226873159,
84.0221191075195));
#205751=CARTESIAN_POINT('Ctrl Pts',(-32.6630886340244,-67.2613979801993,
83.4431226889983));
#205752=CARTESIAN_POINT('Ctrl Pts',(-32.6723570558202,-66.9271902569869,
83.187256821882));
#205753=CARTESIAN_POINT('Ctrl Pts',(-32.7088904509961,-65.6616023646648,
82.117080093252));
#205754=CARTESIAN_POINT('Ctrl Pts',(-32.7366344037597,-64.8359994051929,
81.1878295620108));
#205755=CARTESIAN_POINT('Ctrl Pts',(-32.7731968005128,-63.924608112052,
79.8086445818466));
#205756=CARTESIAN_POINT('Ctrl Pts',(-32.7823439576573,-63.7118757009843,
79.450438499197));
#205757=CARTESIAN_POINT('Ctrl Pts',(-32.8007461567169,-63.3213674514892,
78.7145499636195));
#205758=CARTESIAN_POINT('Ctrl Pts',(-32.8099846903507,-63.1439812735294,
78.3375330035928));
#205759=CARTESIAN_POINT('Ctrl Pts',(-32.819270903196,-62.9850802944281,
77.9529305295057));
#205760=CARTESIAN_POINT('Ctrl Pts',(-31.8032546359728,-84.3357281078424,
63.9421120213277));
#205761=CARTESIAN_POINT('Ctrl Pts',(-31.7929017891933,-84.0137418231872,
63.6098416131334));
#205762=CARTESIAN_POINT('Ctrl Pts',(-31.7825782414718,-83.6742452764102,
63.2949969769354));
#205763=CARTESIAN_POINT('Ctrl Pts',(-31.762142865887,-82.9657881833782,
62.7050617455991));
#205764=CARTESIAN_POINT('Ctrl Pts',(-31.7520438876031,-82.5975654591075,
62.4301067000986));
#205765=CARTESIAN_POINT('Ctrl Pts',(-31.7220978906036,-81.4682498818366,
61.6765559885635));
#205766=CARTESIAN_POINT('Ctrl Pts',(-31.701905426842,-80.6712518671031,
61.2567099106229));
#205767=CARTESIAN_POINT('Ctrl Pts',(-31.6687054766057,-79.2851099112889,
60.7010161848905));
#205768=CARTESIAN_POINT('Ctrl Pts',(-31.6556315862844,-78.7183126943624,
60.5177969698974));
#205769=CARTESIAN_POINT('Ctrl Pts',(-31.6235092294182,-77.3059802936444,
60.1661409326779));
#205770=CARTESIAN_POINT('Ctrl Pts',(-31.6041600695629,-76.4524164504797,
60.0416541758202));
#205771=CARTESIAN_POINT('Ctrl Pts',(-31.5670832372624,-74.7868628847689,
59.9656208321883));
#205772=CARTESIAN_POINT('Ctrl Pts',(-31.5494826207861,-73.9792130438151,
60.0039389183364));
#205773=CARTESIAN_POINT('Ctrl Pts',(-31.5129772878929,-72.3534111569085,
60.2337707384166));
#205774=CARTESIAN_POINT('Ctrl Pts',(-31.4942105742096,-71.5396614362397,
60.4300854548566));
#205775=CARTESIAN_POINT('Ctrl Pts',(-31.4664944723401,-70.3564077373968,
60.8393694015009));
#205776=CARTESIAN_POINT('Ctrl Pts',(-31.4573265264178,-69.9692181927887,
60.9945148918131));
#205777=CARTESIAN_POINT('Ctrl Pts',(-31.4291434374201,-68.8077276326911,
61.526072404452));
#205778=CARTESIAN_POINT('Ctrl Pts',(-31.4098046293393,-68.0627862461729,
61.9609491845076));
#205779=CARTESIAN_POINT('Ctrl Pts',(-31.3715448957847,-66.6707011023987,
62.9708420211181));
#205780=CARTESIAN_POINT('Ctrl Pts',(-31.352820942403,-66.026857096905,63.5431921538024));
#205781=CARTESIAN_POINT('Ctrl Pts',(-31.3244008168015,-65.1616248295522,
64.4812402729385));
#205782=CARTESIAN_POINT('Ctrl Pts',(-31.3150537873411,-64.893933566602,
64.801023931398));
#205783=CARTESIAN_POINT('Ctrl Pts',(-31.2846353628715,-64.0711633671607,
65.8858559643348));
#205784=CARTESIAN_POINT('Ctrl Pts',(-31.2639758907107,-63.5840156743489,
66.6985915452734));
#205785=CARTESIAN_POINT('Ctrl Pts',(-31.2239921695654,-62.8300913154623,
68.3378479345733));
#205786=CARTESIAN_POINT('Ctrl Pts',(-31.2046388496943,-62.5492623479359,
69.1524847619243));
#205787=CARTESIAN_POINT('Ctrl Pts',(-31.1763003470951,-62.2541577943955,
70.396740923088));
#205788=CARTESIAN_POINT('Ctrl Pts',(-31.167074447028,-62.1772042064713,
70.8090646931028));
#205789=CARTESIAN_POINT('Ctrl Pts',(-31.1388631048973,-62.0035560249431,
72.0765788918956));
#205790=CARTESIAN_POINT('Ctrl Pts',(-31.119565396247,-61.9716734969528,
72.9382579515243));
#205791=CARTESIAN_POINT('Ctrl Pts',(-31.0808490166685,-62.0797097403603,
74.6734180662941));
#205792=CARTESIAN_POINT('Ctrl Pts',(-31.0617070857034,-62.2230046580078,
75.5423030227853));
#205793=CARTESIAN_POINT('Ctrl Pts',(-31.029900986821,-62.5970165804909,
76.9220559866024));
#205794=CARTESIAN_POINT('Ctrl Pts',(-31.0175294395029,-62.7748319708431,
77.4440474132357));
#205795=CARTESIAN_POINT('Ctrl Pts',(-31.0052564152503,-62.9850802944281,
77.9529305295057));
#205796=CARTESIAN_POINT('Ctrl Pts',(-32.5134098057851,-62.9850802944281,
77.9529305295057));
#205797=CARTESIAN_POINT('Ctrl Pts',(-32.5076053766535,-63.0852617434361,
78.1954087908987));
#205798=CARTESIAN_POINT('Ctrl Pts',(-32.5017802649863,-63.1928105147828,
78.4349197211954));
#205799=CARTESIAN_POINT('Ctrl Pts',(-32.4838237910791,-63.5451785962135,
79.1599913731993));
#205800=CARTESIAN_POINT('Ctrl Pts',(-32.4716239056369,-63.813181450543,
79.6334752954121));
#205801=CARTESIAN_POINT('Ctrl Pts',(-32.442315516669,-64.5315142181605,
80.7352684005586));
#205802=CARTESIAN_POINT('Ctrl Pts',(-32.4254786019266,-65.0097267370101,
81.3429317606586));
#205803=CARTESIAN_POINT('Ctrl Pts',(-32.3909713539776,-66.0764202871788,
82.4748668122886));
#205804=CARTESIAN_POINT('Ctrl Pts',(-32.3733389564417,-66.6642977390282,
82.995392432135));
#205805=CARTESIAN_POINT('Ctrl Pts',(-32.3374292549746,-67.9675929300343,
83.9543629803537));
#205806=CARTESIAN_POINT('Ctrl Pts',(-32.3192073754178,-68.6857914976066,
84.3830607366462));
#205807=CARTESIAN_POINT('Ctrl Pts',(-32.291326621253,-69.8172587654147,
84.918402285109));
#205808=CARTESIAN_POINT('Ctrl Pts',(-32.2819823861496,-70.2027807287757,
85.0785862771025));
#205809=CARTESIAN_POINT('Ctrl Pts',(-32.2534174636685,-71.4048932028122,
85.5114924043552));
#205810=CARTESIAN_POINT('Ctrl Pts',(-32.2346243519322,-72.2413974206223,
85.7219366544957));
#205811=CARTESIAN_POINT('Ctrl Pts',(-32.1970943895163,-73.9163500386038,
85.9703877836411));
#205812=CARTESIAN_POINT('Ctrl Pts',(-32.178350446336,-74.7499965381135,
86.0131394055838));
#205813=CARTESIAN_POINT('Ctrl Pts',(-32.1413374836823,-76.4170147775859,
85.9384356609712));
#205814=CARTESIAN_POINT('Ctrl Pts',(-32.1230775115974,-77.2464955062173,
85.8205668316705));
#205815=CARTESIAN_POINT('Ctrl Pts',(-32.0951739658194,-78.4636969776953,
85.5258852841211));
#205816=CARTESIAN_POINT('Ctrl Pts',(-32.085844592053,-78.8635482433997,
85.4084890933288));
#205817=CARTESIAN_POINT('Ctrl Pts',(-32.0573013444042,-80.0701001412522,
84.9903267017186));
#205818=CARTESIAN_POINT('Ctrl Pts',(-32.0385165171516,-80.8531448342645,
84.6285246885511));
#205819=CARTESIAN_POINT('Ctrl Pts',(-32.0003877748412,-82.3352085699554,
83.7561132100218));
#205820=CARTESIAN_POINT('Ctrl Pts',(-31.9810362370968,-83.0306905604942,
83.2478562689681));
#205821=CARTESIAN_POINT('Ctrl Pts',(-31.9434043043225,-84.2968599059186,
82.1143586018015));
#205822=CARTESIAN_POINT('Ctrl Pts',(-31.9250226552402,-84.8670083633218,
81.4946488408057));
#205823=CARTESIAN_POINT('Ctrl Pts',(-31.8913008487649,-85.7783267450898,
80.2881430609645));
#205824=CARTESIAN_POINT('Ctrl Pts',(-31.8762028643039,-86.1411164443342,
79.7214196296445));
#205825=CARTESIAN_POINT('Ctrl Pts',(-31.8521446795649,-86.6550981991082,
78.7622750048645));
#205826=CARTESIAN_POINT('Ctrl Pts',(-31.8429987285859,-86.8339861382299,
78.3861172138805));
#205827=CARTESIAN_POINT('Ctrl Pts',(-31.8138207580393,-87.3432442577997,
77.1676574911561));
#205828=CARTESIAN_POINT('Ctrl Pts',(-31.793529191697,-87.6039568424936,
76.2991814038458));
#205829=CARTESIAN_POINT('Ctrl Pts',(-31.7542862800609,-87.9325327509782,
74.5663075747454));
#205830=CARTESIAN_POINT('Ctrl Pts',(-31.7355537691597,-88.0085120462363,
73.7081052595353));
#205831=CARTESIAN_POINT('Ctrl Pts',(-31.7071035079715,-87.9947289921439,
72.430020848856));
#205832=CARTESIAN_POINT('Ctrl Pts',(-31.6977308116469,-87.9699889375341,
72.0118011787893));
#205833=CARTESIAN_POINT('Ctrl Pts',(-31.6691269442241,-87.8329027110215,
70.7401793866785));
#205834=CARTESIAN_POINT('Ctrl Pts',(-31.6503158982419,-87.6560195593421,
69.8961139094583));
#205835=CARTESIAN_POINT('Ctrl Pts',(-31.6120804853365,-87.1363994018851,
68.2499349011304));
#205836=CARTESIAN_POINT('Ctrl Pts',(-31.5925892045241,-86.7938770755704,
67.4522536129843));
#205837=CARTESIAN_POINT('Ctrl Pts',(-31.5548346790839,-85.9694660877567,
65.9624419093435));
#205838=CARTESIAN_POINT('Ctrl Pts',(-31.5365502141308,-85.494589124122,
65.2711334018083));
#205839=CARTESIAN_POINT('Ctrl Pts',(-31.5086330202524,-84.6891200693539,
64.3116785261865));
#205840=CARTESIAN_POINT('Ctrl Pts',(-31.4993140041212,-84.4065224252938,
64.0061074697714));
#205841=CARTESIAN_POINT('Ctrl Pts',(-31.4707861257568,-83.4958975907463,
63.1116359011595));
#205842=CARTESIAN_POINT('Ctrl Pts',(-31.4520065931275,-82.8236812233962,
62.5710956883294));
#205843=CARTESIAN_POINT('Ctrl Pts',(-31.4150123713188,-81.4264517085648,
61.6595801380764));
#205844=CARTESIAN_POINT('Ctrl Pts',(-31.3968335975869,-80.7102333464946,
61.2822349818434));
#205845=CARTESIAN_POINT('Ctrl Pts',(-31.3603815270131,-79.1917448914674,
60.6549203171202));
#205846=CARTESIAN_POINT('Ctrl Pts',(-31.3421407050194,-78.3909075940815,
60.4111601434876));
#205847=CARTESIAN_POINT('Ctrl Pts',(-31.3142483880798,-77.1636092287094,
60.1634234396562));
#205848=CARTESIAN_POINT('Ctrl Pts',(-31.3049113604121,-76.7512490389828,
60.1006425146734));
#205849=CARTESIAN_POINT('Ctrl Pts',(-31.2763568826858,-75.480682155363,
59.9693138771131));
#205850=CARTESIAN_POINT('Ctrl Pts',(-31.2575678912659,-74.6181058614249,
59.9660417654655));
#205851=CARTESIAN_POINT('Ctrl Pts',(-31.2212335497617,-72.9864717788575,
60.1221898828707));
#205852=CARTESIAN_POINT('Ctrl Pts',(-31.2037330422133,-72.219625510468,
60.2658489202725));
#205853=CARTESIAN_POINT('Ctrl Pts',(-31.1673159191293,-70.6432895169942,
60.7105594863258));
#205854=CARTESIAN_POINT('Ctrl Pts',(-31.1485808352973,-69.8414825742706,
61.0252771805082));
#205855=CARTESIAN_POINT('Ctrl Pts',(-31.1201415341838,-68.7045718189878,
61.6072261041865));
#205856=CARTESIAN_POINT('Ctrl Pts',(-31.1107834724493,-68.3419367698086,
61.8154893693561));
#205857=CARTESIAN_POINT('Ctrl Pts',(-31.082199021831,-67.2653733681447,
62.5048137772382));
#205858=CARTESIAN_POINT('Ctrl Pts',(-31.0633974799748,-66.5886292737129,
63.0395610118058));
#205859=CARTESIAN_POINT('Ctrl Pts',(-31.0255413684423,-65.3595946174076,
64.2263624187867));
#205860=CARTESIAN_POINT('Ctrl Pts',(-31.0064524824918,-64.8086145122379,
64.8737831689563));
#205861=CARTESIAN_POINT('Ctrl Pts',(-30.9690972310508,-63.8473904397092,
66.2569751884845));
#205862=CARTESIAN_POINT('Ctrl Pts',(-30.9508258173321,-63.4375302189977,
66.9881669649071));
#205863=CARTESIAN_POINT('Ctrl Pts',(-30.9229157934444,-62.9331182219311,
68.1346509919764));
#205864=CARTESIAN_POINT('Ctrl Pts',(-30.9135911765594,-62.7838849288901,
68.5234893095958));
#205865=CARTESIAN_POINT('Ctrl Pts',(-30.8850549659496,-62.3841643947466,
69.7360280741739));
#205866=CARTESIAN_POINT('Ctrl Pts',(-30.8662726182641,-62.1965672448327,
70.5779713737612));
#205867=CARTESIAN_POINT('Ctrl Pts',(-30.8291649365254,-61.9961730712194,
72.239492048222));
#205868=CARTESIAN_POINT('Ctrl Pts',(-30.8108665953323,-61.9747608962482,
73.054081626788));
#205869=CARTESIAN_POINT('Ctrl Pts',(-30.7742958529931,-62.0858921114305,
74.6987386395822));
#205870=CARTESIAN_POINT('Ctrl Pts',(-30.7560509418798,-62.2224047141963,
75.5247984193269));
#205871=CARTESIAN_POINT('Ctrl Pts',(-30.7281561875893,-62.5444063035,76.7348072071708));
#205872=CARTESIAN_POINT('Ctrl Pts',(-30.7188207626434,-62.6708981172921,
77.1321924653583));
#205873=CARTESIAN_POINT('Ctrl Pts',(-30.706059194963,-62.8699996949342,
77.6672262769554));
#205874=CARTESIAN_POINT('Ctrl Pts',(-30.7026204047894,-62.9262841051138,
77.8106207715354));
#205875=CARTESIAN_POINT('Ctrl Pts',(-30.6991941617974,-62.9850802944281,
77.9529305295057));
#205876=CARTESIAN_POINT('Origin',(-21.6548258024609,-75.,72.98888938658));
#205877=CARTESIAN_POINT('',(-34.6333744106366,-62.9850802944281,77.9529305295057));
#205878=CARTESIAN_POINT('',(-34.3273949797549,-62.9850802944281,77.9529305295057));
#205879=CARTESIAN_POINT('',(-21.6548258024609,-62.9850802944281,77.9529305295057));
#205880=CARTESIAN_POINT('Ctrl Pts',(-32.819270903196,-62.9850802944281,
77.9529305295057));
#205881=CARTESIAN_POINT('Ctrl Pts',(-32.8303488181902,-62.7955206140402,
77.4941220156964));
#205882=CARTESIAN_POINT('Ctrl Pts',(-32.8414992495208,-62.6322673893811,
77.0245186000302));
#205883=CARTESIAN_POINT('Ctrl Pts',(-32.8618815752937,-62.3816084436316,
76.1435119333727));
#205884=CARTESIAN_POINT('Ctrl Pts',(-32.8710913751594,-62.2865225690053,
75.7353309164621));
#205885=CARTESIAN_POINT('Ctrl Pts',(-32.9028830983415,-62.0275972955214,
74.3168337901965));
#205886=CARTESIAN_POINT('Ctrl Pts',(-32.9257513877221,-61.9633350804462,
73.2922177203429));
#205887=CARTESIAN_POINT('Ctrl Pts',(-32.9578895657514,-62.0430373705422,
71.8516723340877));
#205888=CARTESIAN_POINT('Ctrl Pts',(-32.9671254965868,-62.0865020708477,
71.433989150719));
#205889=CARTESIAN_POINT('Ctrl Pts',(-32.9948120157051,-62.2768003706303,
70.1925542543176));
#205890=CARTESIAN_POINT('Ctrl Pts',(-33.0133768145488,-62.4829681329178,
69.3801222078165));
#205891=CARTESIAN_POINT('Ctrl Pts',(-33.0503473708614,-63.0417179721099,
67.8250052856451));
#205892=CARTESIAN_POINT('Ctrl Pts',(-33.0682709487124,-63.3894385363193,
67.0845625800919));
#205893=CARTESIAN_POINT('Ctrl Pts',(-33.1060393670685,-64.257983751471,
65.6128504297507));
#205894=CARTESIAN_POINT('Ctrl Pts',(-33.1260757069405,-64.7896612828076,
64.8928516144764));
#205895=CARTESIAN_POINT('Ctrl Pts',(-33.1650532965956,-65.9697286661664,
63.5977881523641));
#205896=CARTESIAN_POINT('Ctrl Pts',(-33.1837862151397,-66.6101315099571,
63.0215078096652));
#205897=CARTESIAN_POINT('Ctrl Pts',(-33.2122343360639,-67.6399968300279,
62.2648258556167));
#205898=CARTESIAN_POINT('Ctrl Pts',(-33.2216040891035,-67.9890639397373,
62.03343596658));
#205899=CARTESIAN_POINT('Ctrl Pts',(-33.2502042061045,-69.0878649514756,
61.3791175769157));
#205900=CARTESIAN_POINT('Ctrl Pts',(-33.2690133164106,-69.8689186312676,
61.0134082367942));
#205901=CARTESIAN_POINT('Ctrl Pts',(-33.3071691200651,-71.4935665018307,
60.4410481577551));
#205902=CARTESIAN_POINT('Ctrl Pts',(-33.3265758030914,-72.3332640196519,
60.2361678442363));
#205903=CARTESIAN_POINT('Ctrl Pts',(-33.3642463882863,-74.0155149179557,
59.9992482292248));
#205904=CARTESIAN_POINT('Ctrl Pts',(-33.3825281393287,-74.8533245389361,
59.9628200418645));
#205905=CARTESIAN_POINT('Ctrl Pts',(-33.4104438619237,-76.1042568462207,
60.0291941259602));
#205906=CARTESIAN_POINT('Ctrl Pts',(-33.419764058336,-76.5184087177558,
60.0711682849701));
#205907=CARTESIAN_POINT('Ctrl Pts',(-33.4482936964434,-77.7807708737798,
60.2606638026717));
#205908=CARTESIAN_POINT('Ctrl Pts',(-33.4670738130376,-78.6169260116809,
60.4725696178896));
#205909=CARTESIAN_POINT('Ctrl Pts',(-33.5040917123383,-80.186566440543,
61.0409253788097));
#205910=CARTESIAN_POINT('Ctrl Pts',(-33.5222954330852,-80.9197737703172,
61.3867091394883));
#205911=CARTESIAN_POINT('Ctrl Pts',(-33.5587722642639,-82.3350289286893,
62.2234390524097));
#205912=CARTESIAN_POINT('Ctrl Pts',(-33.5770139410402,-83.0113491242323,
62.7167978539842));
#205913=CARTESIAN_POINT('Ctrl Pts',(-33.6049067692322,-83.947247329626,
63.5485221842696));
#205914=CARTESIAN_POINT('Ctrl Pts',(-33.6142434632672,-84.2453394212993,
63.8402574857912));
#205915=CARTESIAN_POINT('Ctrl Pts',(-33.6427974541876,-85.1142196463574,
64.7765228903436));
#205916=CARTESIAN_POINT('Ctrl Pts',(-33.6615862595611,-85.6354756538642,
65.4637939289738));
#205917=CARTESIAN_POINT('Ctrl Pts',(-33.6989489121466,-86.5159865149227,
66.9009770269514));
#205918=CARTESIAN_POINT('Ctrl Pts',(-33.7175161856982,-86.8790333380158,
67.6438747237403));
#205919=CARTESIAN_POINT('Ctrl Pts',(-33.7543538268296,-87.4631659122686,
69.1983991735322));
#205920=CARTESIAN_POINT('Ctrl Pts',(-33.7726078625132,-87.6809979278511,
70.0071749752059));
#205921=CARTESIAN_POINT('Ctrl Pts',(-33.8005079783443,-87.8888404294256,
71.2420764442562));
#205922=CARTESIAN_POINT('Ctrl Pts',(-33.809839765355,-87.9381973326846,
71.6559933457568));
#205923=CARTESIAN_POINT('Ctrl Pts',(-33.838386567099,-88.0283126189074,
72.9298890005096));
#205924=CARTESIAN_POINT('Ctrl Pts',(-33.8571726839098,-88.0036620133458,
73.792124332821));
#205925=CARTESIAN_POINT('Ctrl Pts',(-33.8952999643647,-87.7844960111742,
75.4978903978681));
#205926=CARTESIAN_POINT('Ctrl Pts',(-33.9146515604325,-87.5907485760449,
76.3372431692137));
#205927=CARTESIAN_POINT('Ctrl Pts',(-33.9522825945386,-87.0466716428339,
77.9470330997242));
#205928=CARTESIAN_POINT('Ctrl Pts',(-33.9706588111517,-86.7012516996233,
78.7148129789149));
#205929=CARTESIAN_POINT('Ctrl Pts',(-34.0044349709995,-85.9492394717942,
80.0294294550852));
#205930=CARTESIAN_POINT('Ctrl Pts',(-34.0195937256319,-85.5692184286172,
80.5880129405775));
#205931=CARTESIAN_POINT('Ctrl Pts',(-34.043710710229,-84.8873714723516,
81.4395211634468));
#205932=CARTESIAN_POINT('Ctrl Pts',(-34.0528566120177,-84.6117142724853,
81.7517794012562));
#205933=CARTESIAN_POINT('Ctrl Pts',(-34.0820230580383,-83.6915922207639,
82.6983197720169));
#205934=CARTESIAN_POINT('Ctrl Pts',(-34.1023028966374,-82.9957727870719,
83.2789044967711));
#205935=CARTESIAN_POINT('Ctrl Pts',(-34.1415336101152,-81.5318018742164,
84.2616092303533));
#205936=CARTESIAN_POINT('Ctrl Pts',(-34.1602661380666,-80.7724706946262,
84.6686683284463));
#205937=CARTESIAN_POINT('Ctrl Pts',(-34.1887163037608,-79.5917631926907,
85.1581547926365));
#205938=CARTESIAN_POINT('Ctrl Pts',(-34.1980888676959,-79.1974632258503,
85.2997224612759));
#205939=CARTESIAN_POINT('Ctrl Pts',(-34.226692568603,-77.974250045081,85.6732864127809));
#205940=CARTESIAN_POINT('Ctrl Pts',(-34.2455035275443,-77.1285653983452,
85.842266498186));
#205941=CARTESIAN_POINT('Ctrl Pts',(-34.2837353197113,-75.4107807541226,
86.0112103592688));
#205942=CARTESIAN_POINT('Ctrl Pts',(-34.303222750951,-74.5428430101874,
86.0096644763363));
#205943=CARTESIAN_POINT('Ctrl Pts',(-34.3409734567497,-72.8490955860084,
85.8369924859513));
#205944=CARTESIAN_POINT('Ctrl Pts',(-34.3592577985796,-72.0267989571312,
85.6719578850047));
#205945=CARTESIAN_POINT('Ctrl Pts',(-34.387174925936,-70.8280184635038,
85.3082890592474));
#205946=CARTESIAN_POINT('Ctrl Pts',(-34.3964939957936,-70.4359795751436,
85.168493438659));
#205947=CARTESIAN_POINT('Ctrl Pts',(-34.4250219543035,-69.2556313471897,
84.6825903025585));
#205948=CARTESIAN_POINT('Ctrl Pts',(-34.4438015134082,-68.4944285088169,
84.2768454922166));
#205949=CARTESIAN_POINT('Ctrl Pts',(-34.4799213390761,-67.1399896053986,
83.3720786407645));
#205950=CARTESIAN_POINT('Ctrl Pts',(-34.4971936814418,-66.5401658817086,
82.8894741616409));
#205951=CARTESIAN_POINT('Ctrl Pts',(-34.5333759273023,-65.367339869463,
81.7610094243801));
#205952=CARTESIAN_POINT('Ctrl Pts',(-34.5521118107064,-64.808776374574,
81.1053664770553));
#205953=CARTESIAN_POINT('Ctrl Pts',(-34.5805483990371,-64.0808503345902,
80.0561870098963));
#205954=CARTESIAN_POINT('Ctrl Pts',(-34.5899029774752,-63.859392651258,
79.7016676413947));
#205955=CARTESIAN_POINT('Ctrl Pts',(-34.6107233525533,-63.4046850825134,
78.8890800647395));
#205956=CARTESIAN_POINT('Ctrl Pts',(-34.6220712822401,-63.1808895977458,
78.4268655734003));
#205957=CARTESIAN_POINT('Ctrl Pts',(-34.6333744106366,-62.9850802944281,
77.9529305295057));
#205958=CARTESIAN_POINT('',(-33.3112143094267,-84.3357243294104,63.9421081222156));
#205959=CARTESIAN_POINT('Ctrl Pts',(-33.3112143094267,-84.3357243294104,
63.9421081222156));
#205960=CARTESIAN_POINT('Ctrl Pts',(-33.3011567376052,-84.018179448338,
63.6144212482569));
#205961=CARTESIAN_POINT('Ctrl Pts',(-33.2910868185285,-83.6836026922541,
63.3036812712545));
#205962=CARTESIAN_POINT('Ctrl Pts',(-33.270859537395,-82.9856613046251,
62.7207607284952));
#205963=CARTESIAN_POINT('Ctrl Pts',(-33.2607172534439,-82.6229961362875,
62.448719518442));
#205964=CARTESIAN_POINT('Ctrl Pts',(-33.2307972855461,-81.512313296332,
61.7029412195651));
#205965=CARTESIAN_POINT('Ctrl Pts',(-33.2114694583803,-80.7293167802803,
61.2859930717215));
#205966=CARTESIAN_POINT('Ctrl Pts',(-33.1787998006508,-79.3646935367683,
60.7293474205624));
#205967=CARTESIAN_POINT('Ctrl Pts',(-33.1656257625774,-78.8048353287375,
60.5442060876235));
#205968=CARTESIAN_POINT('Ctrl Pts',(-33.1332173327621,-77.4010069115259,
60.1835986577919));
#205969=CARTESIAN_POINT('Ctrl Pts',(-33.1144159002237,-76.5484568928008,
60.0527930603133));
#205970=CARTESIAN_POINT('Ctrl Pts',(-33.0778011775325,-74.8982943026596,
59.9651786904443));
#205971=CARTESIAN_POINT('Ctrl Pts',(-33.0600016200892,-74.1051527881878,
59.9955595269195));
#205972=CARTESIAN_POINT('Ctrl Pts',(-33.0252332862106,-72.5548874686548,
60.1976288909055));
#205973=CARTESIAN_POINT('Ctrl Pts',(-33.0084016440632,-71.8004344901442,
60.3651931764459));
#205974=CARTESIAN_POINT('Ctrl Pts',(-32.975214203434,-70.3764937256837,
60.8173862440033));
#205975=CARTESIAN_POINT('Ctrl Pts',(-32.958959216202,-69.7071313681547,
61.0931828662537));
#205976=CARTESIAN_POINT('Ctrl Pts',(-32.9336299287227,-68.6924594078672,
61.6139391600983));
#205977=CARTESIAN_POINT('Ctrl Pts',(-32.9244502411375,-68.3301624071969,
61.8225189264437));
#205978=CARTESIAN_POINT('Ctrl Pts',(-32.8933811493513,-67.1446714713373,
62.5833361158591));
#205979=CARTESIAN_POINT('Ctrl Pts',(-32.8712073444619,-66.374713381374,
63.2120734643514));
#205980=CARTESIAN_POINT('Ctrl Pts',(-32.8320021167915,-65.1468740655802,
64.4737079533328));
#205981=CARTESIAN_POINT('Ctrl Pts',(-32.8152101770762,-64.6601117225579,
65.0718749085846));
#205982=CARTESIAN_POINT('Ctrl Pts',(-32.7811254811386,-63.8001707228227,
66.34429060657));
#205983=CARTESIAN_POINT('Ctrl Pts',(-32.7638894358816,-63.4281548857308,
67.0156773275925));
#205984=CARTESIAN_POINT('Ctrl Pts',(-32.7283732978745,-62.779158084489,
68.4781778667905));
#205985=CARTESIAN_POINT('Ctrl Pts',(-32.7101654750316,-62.5150246908457,
69.2712427072861));
#205986=CARTESIAN_POINT('Ctrl Pts',(-32.6794071690772,-62.2064347626964,
70.6173912999878));
#205987=CARTESIAN_POINT('Ctrl Pts',(-32.6671274699066,-62.1179749693231,
71.1578394958046));
#205988=CARTESIAN_POINT('Ctrl Pts',(-32.6377330249469,-61.9874232454337,
72.470434962504));
#205989=CARTESIAN_POINT('Ctrl Pts',(-32.6208908717924,-61.9795960428579,
73.2439011138986));
#205990=CARTESIAN_POINT('Ctrl Pts',(-32.5863479185737,-62.1023105176637,
74.7960616240076));
#205991=CARTESIAN_POINT('Ctrl Pts',(-32.5686834978556,-62.2349407008807,
75.5714306412647));
#205992=CARTESIAN_POINT('Ctrl Pts',(-32.5385701469869,-62.5836904218178,
76.8827731080568));
#205993=CARTESIAN_POINT('Ctrl Pts',(-32.5260500510614,-62.7669161892439,
77.4248881279713));
#205994=CARTESIAN_POINT('Ctrl Pts',(-32.5134098057851,-62.9850802944281,
77.9529305295057));
#205995=CARTESIAN_POINT('Ctrl Pts',(-34.3273949797549,-62.9850802944281,
77.9529305295057));
#205996=CARTESIAN_POINT('Ctrl Pts',(-34.322307377864,-63.0729887704614,
78.1657033995463));
#205997=CARTESIAN_POINT('Ctrl Pts',(-34.3172056192574,-63.1665708141729,
78.3761933206329));
#205998=CARTESIAN_POINT('Ctrl Pts',(-34.2949390915263,-63.5977531412717,
79.2804559285437));
#205999=CARTESIAN_POINT('Ctrl Pts',(-34.277572804023,-63.9910798857048,
79.9458085247177));
#206000=CARTESIAN_POINT('Ctrl Pts',(-34.2485826539232,-64.7549730486861,
81.009425030582));
#206001=CARTESIAN_POINT('Ctrl Pts',(-34.2367826841871,-65.0957150793225,
81.4265852338732));
#206002=CARTESIAN_POINT('Ctrl Pts',(-34.2063795532183,-66.0288964681025,
82.4343718864558));
#206003=CARTESIAN_POINT('Ctrl Pts',(-34.187609460991,-66.6542234883961,
82.9911810079837));
#206004=CARTESIAN_POINT('Ctrl Pts',(-34.1509267743499,-67.9861547229964,
83.9647400989129));
#206005=CARTESIAN_POINT('Ctrl Pts',(-34.1331613516227,-68.6873916773296,
84.3824975576726));
#206006=CARTESIAN_POINT('Ctrl Pts',(-34.0959087150043,-70.2003621110454,
85.1010273626399));
#206007=CARTESIAN_POINT('Ctrl Pts',(-34.0765638445927,-71.0123672528302,
85.3920827438407));
#206008=CARTESIAN_POINT('Ctrl Pts',(-34.0483887293973,-72.2510451174338,
85.7017399515547));
#206009=CARTESIAN_POINT('Ctrl Pts',(-34.0392342437792,-72.6595527561254,
85.7832486538415));
#206010=CARTESIAN_POINT('Ctrl Pts',(-34.0115144072217,-73.8981770415323,
85.9690727208953));
#206011=CARTESIAN_POINT('Ctrl Pts',(-33.992731310687,-74.7351255792752,
86.0130592131825));
#206012=CARTESIAN_POINT('Ctrl Pts',(-33.955371706001,-76.4132424902395,
85.9393476777313));
#206013=CARTESIAN_POINT('Ctrl Pts',(-33.9369789651583,-77.2504069684253,
85.8203857576482));
#206014=CARTESIAN_POINT('Ctrl Pts',(-33.8990573661833,-78.9062080321851,
85.4179625902074));
#206015=CARTESIAN_POINT('Ctrl Pts',(-33.8797302592748,-79.7200570759932,
85.1322576993896));
#206016=CARTESIAN_POINT('Ctrl Pts',(-33.8515355843574,-80.8782039104047,
84.5915279003849));
#206017=CARTESIAN_POINT('Ctrl Pts',(-33.8423466167696,-81.2479763059521,
84.3966627677644));
#206018=CARTESIAN_POINT('Ctrl Pts',(-33.8140691160097,-82.3476574494015,
83.7476140687488));
#206019=CARTESIAN_POINT('Ctrl Pts',(-33.794737390197,-83.0424713065999,
83.2386147866756));
#206020=CARTESIAN_POINT('Ctrl Pts',(-33.7586549670554,-84.2527959019681,
82.1526192558822));
#206021=CARTESIAN_POINT('Ctrl Pts',(-33.7418987501866,-84.7771788972721,
81.590921545649));
#206022=CARTESIAN_POINT('Ctrl Pts',(-33.705709722028,-85.7783300496831,
80.3079062206409));
#206023=CARTESIAN_POINT('Ctrl Pts',(-33.6863603081552,-86.239020039698,
79.5786423791186));
#206024=CARTESIAN_POINT('Ctrl Pts',(-33.6581918465749,-86.810452983774,
78.4373873382913));
#206025=CARTESIAN_POINT('Ctrl Pts',(-33.649048647938,-86.9786866665247,
78.056827364037));
#206026=CARTESIAN_POINT('Ctrl Pts',(-33.6213266156159,-87.4296937897356,
76.8880187355971));
#206027=CARTESIAN_POINT('Ctrl Pts',(-33.6025309162896,-87.6548839720965,
76.0799076396883));
#206028=CARTESIAN_POINT('Ctrl Pts',(-33.5644788453735,-87.9531301665975,
74.3957530123024));
#206029=CARTESIAN_POINT('Ctrl Pts',(-33.5454440944437,-88.0183734434914,
73.5225609866536));
#206030=CARTESIAN_POINT('Ctrl Pts',(-33.5068404281006,-87.9731061851425,
71.7895146102885));
#206031=CARTESIAN_POINT('Ctrl Pts',(-33.4875369900912,-87.8653463592952,
70.9339299399998));
#206032=CARTESIAN_POINT('Ctrl Pts',(-33.455659801239,-87.5436039213937,
69.5247130520752));
#206033=CARTESIAN_POINT('Ctrl Pts',(-33.4427790960703,-87.3749552248436,
68.9635945389235));
#206034=CARTESIAN_POINT('Ctrl Pts',(-33.4102418702305,-86.86065891033,67.5950562137833));
#206035=CARTESIAN_POINT('Ctrl Pts',(-33.3905592101602,-86.4700061757207,
66.8076568513819));
#206036=CARTESIAN_POINT('Ctrl Pts',(-33.3613177814963,-85.7637965985004,
65.6852895329601));
#206037=CARTESIAN_POINT('Ctrl Pts',(-33.3514322408723,-85.5049510413509,
65.3176514742272));
#206038=CARTESIAN_POINT('Ctrl Pts',(-33.3314378047931,-84.9482909039063,
64.608183372074));
#206039=CARTESIAN_POINT('Ctrl Pts',(-33.3213410375762,-84.6505963140764,
64.2670367278378));
#206040=CARTESIAN_POINT('Ctrl Pts',(-33.3112169404745,-84.3357242889639,
63.9421080804773));
#206041=CARTESIAN_POINT('Origin',(-21.6548258024609,-75.,72.98888938658));
#206042=CARTESIAN_POINT('',(-36.4473639743914,-62.9850802944281,77.9529305295057));
#206043=CARTESIAN_POINT('',(-36.1412950695185,-62.9850802944281,77.9529305295057));
#206044=CARTESIAN_POINT('',(-21.6548258024609,-62.9850802944281,77.9529305295057));
#206045=CARTESIAN_POINT('Ctrl Pts',(-34.6333744106366,-62.9850802944281,
77.9529305295057));
#206046=CARTESIAN_POINT('Ctrl Pts',(-34.641014498302,-62.8527275341519,
77.6325851210486));
#206047=CARTESIAN_POINT('Ctrl Pts',(-34.648658393585,-62.7331612112141,
77.3068853604773));
#206048=CARTESIAN_POINT('Ctrl Pts',(-34.6738484033682,-62.3844575639027,
76.2249071551718));
#206049=CARTESIAN_POINT('Ctrl Pts',(-34.6915963640586,-62.2112043754734,
75.452710937918));
#206050=CARTESIAN_POINT('Ctrl Pts',(-34.7263102933167,-62.0093905987928,
73.9048043248658));
#206051=CARTESIAN_POINT('Ctrl Pts',(-34.7431409118205,-61.977935394032,
73.132664809404));
#206052=CARTESIAN_POINT('Ctrl Pts',(-34.7762781355656,-62.04983480117,71.6426752969835));
#206053=CARTESIAN_POINT('Ctrl Pts',(-34.7924822107337,-62.1443232499337,
70.9271815436608));
#206054=CARTESIAN_POINT('Ctrl Pts',(-34.8245199273994,-62.4511959471291,
69.5177537052481));
#206055=CARTESIAN_POINT('Ctrl Pts',(-34.8402934076462,-62.6632973062741,
68.826313272693));
#206056=CARTESIAN_POINT('Ctrl Pts',(-34.8734422301294,-63.2184076373919,
67.4401181719159));
#206057=CARTESIAN_POINT('Ctrl Pts',(-34.8907994054739,-63.5682537311863,
66.7511050425069));
#206058=CARTESIAN_POINT('Ctrl Pts',(-34.9254355268895,-64.3960513698163,
65.4270899112198));
#206059=CARTESIAN_POINT('Ctrl Pts',(-34.9427031652233,-64.8752333752963,
64.7965975180037));
#206060=CARTESIAN_POINT('Ctrl Pts',(-34.9794395177757,-65.9894981678966,
63.5787263238995));
#206061=CARTESIAN_POINT('Ctrl Pts',(-34.9987656114795,-66.6318937865852,
63.0031434729509));
#206062=CARTESIAN_POINT('Ctrl Pts',(-35.0269611300522,-67.6636752702301,
62.2486428642757));
#206063=CARTESIAN_POINT('Ctrl Pts',(-35.0361517023118,-68.0126159078625,
62.0184281755644));
#206064=CARTESIAN_POINT('Ctrl Pts',(-35.0644318262356,-69.1111911860981,
61.3673496406319));
#206065=CARTESIAN_POINT('Ctrl Pts',(-35.0837646191923,-69.891955638007,
61.0036431588981));
#206066=CARTESIAN_POINT('Ctrl Pts',(-35.1199264595699,-71.4301373127408,
60.4649172600748));
#206067=CARTESIAN_POINT('Ctrl Pts',(-35.1367626891198,-72.1786144365612,
60.2753694852728));
#206068=CARTESIAN_POINT('Ctrl Pts',(-35.173037667012,-73.7890534336014,
60.0168418106224));
#206069=CARTESIAN_POINT('Ctrl Pts',(-35.1923839804215,-74.6500948468182,
59.9651423694528));
#206070=CARTESIAN_POINT('Ctrl Pts',(-35.2205570259387,-75.9257643229752,
60.015217496338));
#206071=CARTESIAN_POINT('Ctrl Pts',(-35.2297080309738,-76.3405954064536,
60.0515014817868));
#206072=CARTESIAN_POINT('Ctrl Pts',(-35.2574286342686,-77.5817451575349,
60.2204054800453));
#206073=CARTESIAN_POINT('Ctrl Pts',(-35.2762157314665,-78.3976980433205,
60.4129114044301));
#206074=CARTESIAN_POINT('Ctrl Pts',(-35.3137924594775,-79.9969053829984,
60.9573297758994));
#206075=CARTESIAN_POINT('Ctrl Pts',(-35.3323865848766,-80.7753222813578,
61.3109979284769));
#206076=CARTESIAN_POINT('Ctrl Pts',(-35.3705224384596,-82.2580658579586,
62.1694288005398));
#206077=CARTESIAN_POINT('Ctrl Pts',(-35.3898426630841,-82.9580299352939,
62.6733662304289));
#206078=CARTESIAN_POINT('Ctrl Pts',(-35.4180426924495,-83.9165515457928,
63.5194670507581));
#206079=CARTESIAN_POINT('Ctrl Pts',(-35.4272420436857,-84.2165071128488,
63.811152891912));
#206080=CARTESIAN_POINT('Ctrl Pts',(-35.4555365740011,-85.0883345805226,
64.7448662989507));
#206081=CARTESIAN_POINT('Ctrl Pts',(-35.4748750177734,-85.6110660533947,
65.4295455524948));
#206082=CARTESIAN_POINT('Ctrl Pts',(-35.5114915873723,-86.4781358579965,
66.8343076133079));
#206083=CARTESIAN_POINT('Ctrl Pts',(-35.528786138212,-86.8314863636126,
67.5444043405089));
#206084=CARTESIAN_POINT('Ctrl Pts',(-35.5655511241808,-87.4295650057268,
69.0842497084332));
#206085=CARTESIAN_POINT('Ctrl Pts',(-35.5848757378552,-87.6606854241181,
69.9152347545338));
#206086=CARTESIAN_POINT('Ctrl Pts',(-35.613072463526,-87.8795653599801,
71.1746596303435));
#206087=CARTESIAN_POINT('Ctrl Pts',(-35.6222653382204,-87.9312255737478,
71.5895901507472));
#206088=CARTESIAN_POINT('Ctrl Pts',(-35.650549234005,-88.0277575135514,
72.8630698603536));
#206089=CARTESIAN_POINT('Ctrl Pts',(-35.6698835411671,-88.0075990639256,
73.7241801138767));
#206090=CARTESIAN_POINT('Ctrl Pts',(-35.7061605505144,-87.8078514639825,
75.3470532851727));
#206091=CARTESIAN_POINT('Ctrl Pts',(-35.7231128427644,-87.6443181674053,
76.1070974524996));
#206092=CARTESIAN_POINT('Ctrl Pts',(-35.7595123339326,-87.1585564748513,
77.6696917195567));
#206093=CARTESIAN_POINT('Ctrl Pts',(-35.7788538251116,-86.8221704847922,
78.4639876877875));
#206094=CARTESIAN_POINT('Ctrl Pts',(-35.8070334463051,-86.2101080968332,
79.5848778072634));
#206095=CARTESIAN_POINT('Ctrl Pts',(-35.8161955912507,-85.9929688662903,
79.9407396568493));
#206096=CARTESIAN_POINT('Ctrl Pts',(-35.8439134584175,-85.2901079930823,
80.9771252094763));
#206097=CARTESIAN_POINT('Ctrl Pts',(-35.8626874326064,-84.7555150715976,
81.6218578649759));
#206098=CARTESIAN_POINT('Ctrl Pts',(-35.8995680862153,-83.5789696633293,
82.7908559248002));
#206099=CARTESIAN_POINT('Ctrl Pts',(-35.9175169020216,-82.9414147917895,
83.314159654687));
#206100=CARTESIAN_POINT('Ctrl Pts',(-35.9549652882549,-81.5448404094005,
84.2541220410596));
#206101=CARTESIAN_POINT('Ctrl Pts',(-35.9743054945147,-80.7850554546446,
84.6625154958597));
#206102=CARTESIAN_POINT('Ctrl Pts',(-36.0024867155247,-79.6056918100297,
85.1528231393263));
#206103=CARTESIAN_POINT('Ctrl Pts',(-36.0116516105019,-79.213401698831,
85.2942104870982));
#206104=CARTESIAN_POINT('Ctrl Pts',(-36.0393686733256,-78.0163844616726,
85.6616678334622));
#206105=CARTESIAN_POINT('Ctrl Pts',(-36.0581392624687,-77.1960005555216,
85.8292731567654));
#206106=CARTESIAN_POINT('Ctrl Pts',(-36.0948471111402,-75.55421159348,86.0026489499043));
#206107=CARTESIAN_POINT('Ctrl Pts',(-36.1126358407721,-74.7369291072049,
86.0117880164174));
#206108=CARTESIAN_POINT('Ctrl Pts',(-36.1499133610179,-73.0666734822116,
85.8730912847391));
#206109=CARTESIAN_POINT('Ctrl Pts',(-36.1692576616452,-72.218336304354,
85.7169201557518));
#206110=CARTESIAN_POINT('Ctrl Pts',(-36.1974335686496,-70.9916550333374,
85.3625121108948));
#206111=CARTESIAN_POINT('Ctrl Pts',(-36.2065893919981,-70.5974235216031,
85.227790030333));
#206112=CARTESIAN_POINT('Ctrl Pts',(-36.2343089130728,-69.4330841646863,
84.7663449543757));
#206113=CARTESIAN_POINT('Ctrl Pts',(-36.2530904484636,-68.6873616889725,
84.3840459911954));
#206114=CARTESIAN_POINT('Ctrl Pts',(-36.2903665959047,-67.2764011976082,
83.4794373193744));
#206115=CARTESIAN_POINT('Ctrl Pts',(-36.3086819562941,-66.6148714946546,
82.9586035611532));
#206116=CARTESIAN_POINT('Ctrl Pts',(-36.3465211473052,-65.3868126826264,
81.7824650483401));
#206117=CARTESIAN_POINT('Ctrl Pts',(-36.3658507308723,-64.8260169830175,
81.1270970334503));
#206118=CARTESIAN_POINT('Ctrl Pts',(-36.3940432043561,-64.0953648788812,
80.0785506280071));
#206119=CARTESIAN_POINT('Ctrl Pts',(-36.4032280887483,-63.8732812127073,
79.7246515881299));
#206120=CARTESIAN_POINT('Ctrl Pts',(-36.424041948537,-63.4125683625356,
78.9053348831349));
#206121=CARTESIAN_POINT('Ctrl Pts',(-36.4356882557931,-63.1843405800142,
78.4352182992673));
#206122=CARTESIAN_POINT('Ctrl Pts',(-36.4473639743914,-62.9850802944281,
77.9529305295057));
#206123=CARTESIAN_POINT('Ctrl Pts',(-36.1412950695185,-62.9850802944281,
77.9529305295057));
#206124=CARTESIAN_POINT('Ctrl Pts',(-36.1298525502769,-63.1803591218897,
78.425581614498));
#206125=CARTESIAN_POINT('Ctrl Pts',(-36.1184583697945,-63.4034749546776,
78.886580639856));
#206126=CARTESIAN_POINT('Ctrl Pts',(-36.0979502789426,-63.8572044270931,
79.6980294849889));
#206127=CARTESIAN_POINT('Ctrl Pts',(-36.0887627234557,-64.078500159393,
80.0525495582584));
#206128=CARTESIAN_POINT('Ctrl Pts',(-36.0604875345533,-64.8060087068991,
81.1018877758815));
#206129=CARTESIAN_POINT('Ctrl Pts',(-36.0411567591116,-65.3643328811862,
81.7577039564323));
#206130=CARTESIAN_POINT('Ctrl Pts',(-36.0051415928358,-66.5334898549632,
82.8834150934476));
#206131=CARTESIAN_POINT('Ctrl Pts',(-35.9884531675195,-67.1293477687627,
83.3636796870078));
#206132=CARTESIAN_POINT('Ctrl Pts',(-35.9542340750339,-68.4078798433051,
84.220309833931));
#206133=CARTESIAN_POINT('Ctrl Pts',(-35.9367849374942,-69.0891474589492,
84.5933144326596));
#206134=CARTESIAN_POINT('Ctrl Pts',(-35.9065947947129,-70.3398260948869,
85.1392086252321));
#206135=CARTESIAN_POINT('Ctrl Pts',(-35.8936717610195,-70.8954921615821,
85.3379984834587));
#206136=CARTESIAN_POINT('Ctrl Pts',(-35.8631504303883,-72.2199572693316,
85.7125134739772));
#206137=CARTESIAN_POINT('Ctrl Pts',(-35.8454515742033,-72.9950638305585,
85.8574350415196));
#206138=CARTESIAN_POINT('Ctrl Pts',(-35.8119077179018,-74.4986160864227,
85.999339158326));
#206139=CARTESIAN_POINT('Ctrl Pts',(-35.7961055625979,-75.2231526572785,
86.0070843134678));
#206140=CARTESIAN_POINT('Ctrl Pts',(-35.7629303779634,-76.7135634606904,
85.8985059243922));
#206141=CARTESIAN_POINT('Ctrl Pts',(-35.7455770783725,-77.4760531957894,
85.7741799705351));
#206142=CARTESIAN_POINT('Ctrl Pts',(-35.710886806919,-78.9912201978066,
85.3864273889758));
#206143=CARTESIAN_POINT('Ctrl Pts',(-35.693560322958,-79.7398287285188,
85.1199576918447));
#206144=CARTESIAN_POINT('Ctrl Pts',(-35.6567613892564,-81.240323217721,
84.4256128705099));
#206145=CARTESIAN_POINT('Ctrl Pts',(-35.6374385682394,-81.9833735426707,
83.987652175025));
#206146=CARTESIAN_POINT('Ctrl Pts',(-35.609240444434,-83.0150055342737,
83.2326392252354));
#206147=CARTESIAN_POINT('Ctrl Pts',(-35.6000448628727,-83.3402164835095,
82.969646531436));
#206148=CARTESIAN_POINT('Ctrl Pts',(-35.5717565267856,-84.29350749714,82.1195554590688));
#206149=CARTESIAN_POINT('Ctrl Pts',(-35.5524204684057,-84.8765420593404,
81.4854917354083));
#206150=CARTESIAN_POINT('Ctrl Pts',(-35.5160044028697,-85.8626912887872,
80.1731711400995));
#206151=CARTESIAN_POINT('Ctrl Pts',(-35.4989119626645,-86.275235827812,
79.5066367552329));
#206152=CARTESIAN_POINT('Ctrl Pts',(-35.4623624776624,-87.0104486362849,
78.0376025408581));
#206153=CARTESIAN_POINT('Ctrl Pts',(-35.4430274023172,-87.3182033186538,
77.2317962421226));
#206154=CARTESIAN_POINT('Ctrl Pts',(-35.4148403390291,-87.6535935030626,
75.9989728902198));
#206155=CARTESIAN_POINT('Ctrl Pts',(-35.4056652296747,-87.7436649065816,
75.5913950649829));
#206156=CARTESIAN_POINT('Ctrl Pts',(-35.3779516203089,-87.9546667311608,
74.3575301165006));
#206157=CARTESIAN_POINT('Ctrl Pts',(-35.3591941298354,-88.0157992054867,
73.5232336120756));
#206158=CARTESIAN_POINT('Ctrl Pts',(-35.3231332789316,-87.9783573860045,
71.9013534622564));
#206159=CARTESIAN_POINT('Ctrl Pts',(-35.305943613096,-87.8886388157082,
71.1171279053155));
#206160=CARTESIAN_POINT('Ctrl Pts',(-35.2712619772891,-87.57143980227,69.5895381066747));
#206161=CARTESIAN_POINT('Ctrl Pts',(-35.2538720546943,-87.3472935931955,
68.8487163896592));
#206162=CARTESIAN_POINT('Ctrl Pts',(-35.2245121336728,-86.8517196601871,
67.6182549098334));
#206163=CARTESIAN_POINT('Ctrl Pts',(-35.212363976353,-86.6120863114997,
67.1180779594422));
#206164=CARTESIAN_POINT('Ctrl Pts',(-35.1810619928782,-85.9212762507082,
65.885082061825));
#206165=CARTESIAN_POINT('Ctrl Pts',(-35.161725612669,-85.4279893299815,
65.1789353483755));
#206166=CARTESIAN_POINT('Ctrl Pts',(-35.1252832688943,-84.3586469278054,
63.9318707316406));
#206167=CARTESIAN_POINT('Ctrl Pts',(-35.1081643422314,-83.7959127433042,
63.3844224239668));
#206168=CARTESIAN_POINT('Ctrl Pts',(-35.0715865582653,-82.5189577011011,
62.3490750784855));
#206169=CARTESIAN_POINT('Ctrl Pts',(-35.0522527705251,-81.7984371772448,
61.8748605922018));
#206170=CARTESIAN_POINT('Ctrl Pts',(-35.0240643659055,-80.6668092325737,
61.2815674948093));
#206171=CARTESIAN_POINT('Ctrl Pts',(-35.0148868659841,-80.2881379141312,
61.1057201981099));
#206172=CARTESIAN_POINT('Ctrl Pts',(-34.987174173883,-79.1288382149548,
60.6337712453924));
#206173=CARTESIAN_POINT('Ctrl Pts',(-34.968419872004,-78.3275164411888,
60.3942925768916));
#206174=CARTESIAN_POINT('Ctrl Pts',(-34.932511525472,-76.7423163818132,
60.0825130771705));
#206175=CARTESIAN_POINT('Ctrl Pts',(-34.9154629905747,-75.9638072250017,
60.0011529314397));
#206176=CARTESIAN_POINT('Ctrl Pts',(-34.8809560702276,-74.4114376289477,
59.979331990741));
#206177=CARTESIAN_POINT('Ctrl Pts',(-34.8635905575498,-73.6407223218485,
60.0371575924769));
#206178=CARTESIAN_POINT('Ctrl Pts',(-34.8346132052656,-72.3493295968927,
60.2506430475948));
#206179=CARTESIAN_POINT('Ctrl Pts',(-34.8228253346168,-71.8249137096747,
60.3711319717456));
#206180=CARTESIAN_POINT('Ctrl Pts',(-34.7924331535153,-70.5083867782047,
60.7609136513772));
#206181=CARTESIAN_POINT('Ctrl Pts',(-34.7736616693852,-69.7320391158638,
61.0747568939945));
#206182=CARTESIAN_POINT('Ctrl Pts',(-34.7369083697422,-68.2662767014208,
61.838765999511));
#206183=CARTESIAN_POINT('Ctrl Pts',(-34.7190775380642,-67.5786125791408,
62.2841569611463));
#206184=CARTESIAN_POINT('Ctrl Pts',(-34.681755071938,-66.2623542678585,
63.3248345387022));
#206185=CARTESIAN_POINT('Ctrl Pts',(-34.6624118173452,-65.6420146154581,
63.9242035761149));
#206186=CARTESIAN_POINT('Ctrl Pts',(-34.63423449118,-64.816078613799,64.898079971304));
#206187=CARTESIAN_POINT('Ctrl Pts',(-34.6250762620786,-64.5621204161471,
65.2284691985156));
#206188=CARTESIAN_POINT('Ctrl Pts',(-34.5973573387338,-63.8474596197001,
66.2569088915288));
#206189=CARTESIAN_POINT('Ctrl Pts',(-34.5785786450852,-63.4377788028716,
66.9877441412928));
#206190=CARTESIAN_POINT('Ctrl Pts',(-34.5414527763825,-62.765387999806,
68.5157453771292));
#206191=CARTESIAN_POINT('Ctrl Pts',(-34.5232767236405,-62.5038197776782,
69.3091836367251));
#206192=CARTESIAN_POINT('Ctrl Pts',(-34.4855859796664,-62.1302729106898,
70.9614529881757));
#206193=CARTESIAN_POINT('Ctrl Pts',(-34.4662521462287,-62.0243222102277,
71.8174926686515));
#206194=CARTESIAN_POINT('Ctrl Pts',(-34.4380637884215,-61.9937367843572,
73.0948472448445));
#206195=CARTESIAN_POINT('Ctrl Pts',(-34.4288863722571,-62.0038381402737,
73.5122311710028));
#206196=CARTESIAN_POINT('Ctrl Pts',(-34.4011736473037,-62.0942980487042,
74.7606449122937));
#206197=CARTESIAN_POINT('Ctrl Pts',(-34.3824192329003,-62.2345891096477,
75.5851425473809));
#206198=CARTESIAN_POINT('Ctrl Pts',(-34.3516267721921,-62.5970931805737,
76.922270003251));
#206199=CARTESIAN_POINT('Ctrl Pts',(-34.3395609378567,-62.7748651755682,
77.4441277816481));
#206200=CARTESIAN_POINT('Ctrl Pts',(-34.3273949797549,-62.9850802944281,
77.9529305295057));
#206201=CARTESIAN_POINT('Origin',(-21.6548258024609,-75.,72.98888938658));
#206202=CARTESIAN_POINT('',(-39.5675364832709,-62.9850802944281,77.9529305295057));
#206203=CARTESIAN_POINT('',(-39.5675364832709,-70.0359588570743,60.9739696810081));
#206204=CARTESIAN_POINT('Origin',(-39.5675364832709,-75.,72.98888938658));
#206205=CARTESIAN_POINT('Origin',(-39.5675364832709,-75.,72.98888938658));
#206206=CARTESIAN_POINT('',(-39.3655152556871,-62.9850803327788,77.9529306223294));
#206207=CARTESIAN_POINT('',(-21.6548258024609,-62.9850802944281,77.9529305295057));
#206208=CARTESIAN_POINT('',(-39.378281183842,-62.0210675376173,72.249083919906));
#206209=CARTESIAN_POINT('Ctrl Pts',(-39.3655152559408,-62.985080332779,
77.95293062233));
#206210=CARTESIAN_POINT('Ctrl Pts',(-39.367974326097,-62.6134372726655,
77.0534091840336));
#206211=CARTESIAN_POINT('Ctrl Pts',(-39.3710406973607,-62.3439836733896,
76.1149984769994));
#206212=CARTESIAN_POINT('Ctrl Pts',(-39.3753005433957,-62.0195887932955,
74.1956296276191));
#206213=CARTESIAN_POINT('Ctrl Pts',(-39.376513824047,-61.9656804043715,
73.2207797100456));
#206214=CARTESIAN_POINT('Ctrl Pts',(-39.3782811843755,-62.0210675372952,
72.2490839198886));
#206215=CARTESIAN_POINT('',(-38.9114901702032,-62.0210675376382,72.2490839198538));
#206216=CARTESIAN_POINT('',(-38.9115960243709,-62.0210675372924,72.2490839198855));
#206217=CARTESIAN_POINT('',(-38.6651607695592,-62.9850797267618,77.9529291555314));
#206218=CARTESIAN_POINT('Ctrl Pts',(-38.9114901696398,-62.0210675372996,
72.2490839198104));
#206219=CARTESIAN_POINT('Ctrl Pts',(-38.87002296087,-61.9656824369655,73.2207440507031));
#206220=CARTESIAN_POINT('Ctrl Pts',(-38.8281416219942,-62.0195861640916,
74.1955869480229));
#206221=CARTESIAN_POINT('Ctrl Pts',(-38.7459661857041,-62.3439713077193,
76.1149524347908));
#206222=CARTESIAN_POINT('Ctrl Pts',(-38.7059499709518,-62.6134267199739,
77.0533833312218));
#206223=CARTESIAN_POINT('Ctrl Pts',(-38.6651607695592,-62.9850797267618,
77.9529291555314));
#206224=CARTESIAN_POINT('',(-37.9553013365568,-62.9850802944281,77.9529305295057));
#206225=CARTESIAN_POINT('',(-21.6548258024609,-62.9850802944281,77.9529305295057));
#206226=CARTESIAN_POINT('',(-39.3215010433097,-79.7259927877122,85.0994220373138));
#206227=CARTESIAN_POINT('Ctrl Pts',(-39.321506023786,-79.7261416975021,
85.0993635579381));
#206228=CARTESIAN_POINT('Ctrl Pts',(-39.3113482514596,-80.1554579332872,
84.9318218634802));
#206229=CARTESIAN_POINT('Ctrl Pts',(-39.3011776717826,-80.5755604755536,
84.7415702126412));
#206230=CARTESIAN_POINT('Ctrl Pts',(-39.2807471898218,-81.3908301718727,
84.3187887005437));
#206231=CARTESIAN_POINT('Ctrl Pts',(-39.2705028353935,-81.7855868463675,
84.086868401655));
#206232=CARTESIAN_POINT('Ctrl Pts',(-39.2402664687624,-82.9136640432723,
83.341390069044));
#206233=CARTESIAN_POINT('Ctrl Pts',(-39.2207367675194,-83.6071304006881,
82.7724295103021));
#206234=CARTESIAN_POINT('Ctrl Pts',(-39.187736279067,-84.6541971890334,
81.7152027972093));
#206235=CARTESIAN_POINT('Ctrl Pts',(-39.1744557107486,-85.0423775040713,
81.2655263007179));
#206236=CARTESIAN_POINT('Ctrl Pts',(-39.1419599814079,-85.9149008766984,
80.1026338823808));
#206237=CARTESIAN_POINT('Ctrl Pts',(-39.1231751559109,-86.3617101374352,
79.3647788138448));
#206238=CARTESIAN_POINT('Ctrl Pts',(-39.0850463360107,-87.1024487154548,
77.8126986476469));
#206239=CARTESIAN_POINT('Ctrl Pts',(-39.0656944288797,-87.3947616178232,
77.0024020414012));
#206240=CARTESIAN_POINT('Ctrl Pts',(-39.0374375807919,-87.7069281015113,
75.7651521671601));
#206241=CARTESIAN_POINT('Ctrl Pts',(-39.0282836838252,-87.789387623988,
75.356424408735));
#206242=CARTESIAN_POINT('Ctrl Pts',(-38.9983274833698,-87.9935104378332,
74.0149112619828));
#206243=CARTESIAN_POINT('Ctrl Pts',(-38.9772513454028,-88.0336861114053,
73.0727804455865));
#206244=CARTESIAN_POINT('Ctrl Pts',(-38.9371909475701,-87.9154135641783,
71.276891516979));
#206245=CARTESIAN_POINT('Ctrl Pts',(-38.9184592518008,-87.7739999514192,
70.426903035325));
#206246=CARTESIAN_POINT('Ctrl Pts',(-38.8866396546053,-87.4009417144042,
69.046570325221));
#206247=CARTESIAN_POINT('Ctrl Pts',(-38.8738402023574,-87.2160830328018,
68.5064182412333));
#206248=CARTESIAN_POINT('Ctrl Pts',(-38.8517581241255,-86.8344064686362,
67.5922694312997));
#206249=CARTESIAN_POINT('Ctrl Pts',(-38.842500800169,-86.6537393020338,
67.2124680051155));
#206250=CARTESIAN_POINT('Ctrl Pts',(-38.8061998248951,-85.875068985673,
65.7613622926709));
#206251=CARTESIAN_POINT('Ctrl Pts',(-38.7786800607374,-85.1451132647971,
64.768126542228));
#206252=CARTESIAN_POINT('Ctrl Pts',(-38.7423424310481,-83.9954923090845,
63.5945030620776));
#206253=CARTESIAN_POINT('Ctrl Pts',(-38.7331950830006,-83.6899982218031,
63.311218801858));
#206254=CARTESIAN_POINT('Ctrl Pts',(-38.7037868133542,-82.6714131616104,
62.4538702915295));
#206255=CARTESIAN_POINT('Ctrl Pts',(-38.6832615333122,-81.9111407800835,
61.9402098646618));
#206256=CARTESIAN_POINT('Ctrl Pts',(-38.6437753971098,-80.3443935727869,
61.1071315502257));
#206257=CARTESIAN_POINT('Ctrl Pts',(-38.6250431938578,-79.5473707885441,
60.7798707466158));
#206258=CARTESIAN_POINT('Ctrl Pts',(-38.593322866449,-78.1819243201014,
60.3716252262562));
#206259=CARTESIAN_POINT('Ctrl Pts',(-38.5806266647946,-77.6299494353271,
60.245131674304));
#206260=CARTESIAN_POINT('Ctrl Pts',(-38.5507812147664,-76.3080766280265,
60.031770524167));
#206261=CARTESIAN_POINT('Ctrl Pts',(-38.5339097461974,-75.5351845042424,
59.9769113524817));
#206262=CARTESIAN_POINT('Ctrl Pts',(-38.4986388165814,-73.9454075635035,
60.0060198059474));
#206263=CARTESIAN_POINT('Ctrl Pts',(-38.4802511787274,-73.1320287720359,
60.0978945506683));
#206264=CARTESIAN_POINT('Ctrl Pts',(-38.4435802277085,-71.5127828458182,
60.4373529622181));
#206265=CARTESIAN_POINT('Ctrl Pts',(-38.4252687805447,-70.7114301394952,
60.6880794174666));
#206266=CARTESIAN_POINT('Ctrl Pts',(-38.3908818187426,-69.2903855024502,
61.2885760400576));
#206267=CARTESIAN_POINT('Ctrl Pts',(-38.3750346592167,-68.6643789927797,
61.6153699446988));
#206268=CARTESIAN_POINT('Ctrl Pts',(-38.3502514172104,-67.7158356397337,
62.2132591234165));
#206269=CARTESIAN_POINT('Ctrl Pts',(-38.3411059210818,-67.3745706508539,
62.451997730562));
#206270=CARTESIAN_POINT('Ctrl Pts',(-38.3120645038886,-66.3351145766857,
63.2561560128368));
#206271=CARTESIAN_POINT('Ctrl Pts',(-38.2919120963771,-65.6837250195085,
63.8777237668502));
#206272=CARTESIAN_POINT('Ctrl Pts',(-38.2528138845757,-64.5444767098619,
65.2158174645238));
#206273=CARTESIAN_POINT('Ctrl Pts',(-38.2340811610396,-64.0536021176555,
65.9238349903496));
#206274=CARTESIAN_POINT('Ctrl Pts',(-38.2056320505399,-63.4328818764009,
67.0410306554381));
#206275=CARTESIAN_POINT('Ctrl Pts',(-38.1962609427299,-63.247361092142,
67.4165718556594));
#206276=CARTESIAN_POINT('Ctrl Pts',(-38.1676590872137,-62.7369249334442,
68.5892179736311));
#206277=CARTESIAN_POINT('Ctrl Pts',(-38.1488490860104,-62.4727150568358,
69.4101671134101));
#206278=CARTESIAN_POINT('Ctrl Pts',(-38.1106568670412,-62.1096053559418,
71.0957219055625));
#206279=CARTESIAN_POINT('Ctrl Pts',(-38.0912114977267,-62.0123094454613,
71.9562987720156));
#206280=CARTESIAN_POINT('Ctrl Pts',(-38.0535025268716,-61.9902344102795,
73.6567680186461));
#206281=CARTESIAN_POINT('Ctrl Pts',(-38.0352195326587,-62.0601682096371,
74.4924929792126));
#206282=CARTESIAN_POINT('Ctrl Pts',(-38.0073031348116,-62.2843834657231,
75.7249738972242));
#206283=CARTESIAN_POINT('Ctrl Pts',(-37.9979834780239,-62.3784455771531,
76.13045353721));
#206284=CARTESIAN_POINT('Ctrl Pts',(-37.9774552473509,-62.6286908492328,
77.0142109704468));
#206285=CARTESIAN_POINT('Ctrl Pts',(-37.9663643192439,-62.7934308888043,
77.4890640638799));
#206286=CARTESIAN_POINT('Ctrl Pts',(-37.9553013365568,-62.9850802944281,
77.9529305295057));
#206287=CARTESIAN_POINT('Ctrl Pts',(-39.3215011869246,-79.7258751176041,
85.0994675880042));
#206288=CARTESIAN_POINT('Ctrl Pts',(-39.3236712637677,-78.9367247383293,
85.4074154067982));
#206289=CARTESIAN_POINT('Ctrl Pts',(-39.3262569458996,-78.1193599427749,
85.6374944349639));
#206290=CARTESIAN_POINT('Ctrl Pts',(-39.3301175566084,-76.4652632035647,
85.9328892466976));
#206291=CARTESIAN_POINT('Ctrl Pts',(-39.3314200360406,-75.632920357202,
86.0001740554809));
#206292=CARTESIAN_POINT('Ctrl Pts',(-39.3355204404005,-73.1131187980923,
85.9613804639162));
#206293=CARTESIAN_POINT('Ctrl Pts',(-39.3415199539802,-71.4474475515615,
85.6073365102985));
#206294=CARTESIAN_POINT('Ctrl Pts',(-39.3463525919956,-69.1288448774416,
84.6175275196918));
#206295=CARTESIAN_POINT('Ctrl Pts',(-39.3473555822715,-68.395046064557,
84.2169902570332));
#206296=CARTESIAN_POINT('Ctrl Pts',(-39.3513429793926,-66.6498730320518,
83.0337632759551));
#206297=CARTESIAN_POINT('Ctrl Pts',(-39.3558794304813,-65.7059415961714,
82.1673740340386));
#206298=CARTESIAN_POINT('Ctrl Pts',(-39.3612997924157,-64.1112620960786,
80.2011041664734));
#206299=CARTESIAN_POINT('Ctrl Pts',(-39.3623386810063,-63.4651609951521,
79.114913433967));
#206300=CARTESIAN_POINT('Ctrl Pts',(-39.3655152559408,-62.985080332779,
77.95293062233));
#206301=CARTESIAN_POINT('Origin',(-23.4378585958609,-75.,72.98888938658));
#206302=CARTESIAN_POINT('',(-23.3083467243891,-63.2246325280382,77.8539778944304));
#206303=CARTESIAN_POINT('',(-23.4378585958609,-63.1049274015129,77.9034149284856));
#206304=CARTESIAN_POINT('',(-23.5671968062386,-68.218371728628,84.0797707272727));
#206305=CARTESIAN_POINT('Ctrl Pts',(-23.5672140314447,-68.2183351228444,
84.0798326058898));
#206306=CARTESIAN_POINT('Ctrl Pts',(-23.5673199177301,-68.2102006987572,
84.0748587333312));
#206307=CARTESIAN_POINT('Ctrl Pts',(-23.5674258040155,-68.202071746649,
84.06987591173));
#206308=CARTESIAN_POINT('Ctrl Pts',(-23.5675316903009,-68.1939482861969,
84.0648841531478));
#206309=CARTESIAN_POINT('',(-22.5675364824894,-63.000102062494,73.0394432284656));
#206310=CARTESIAN_POINT('Ctrl Pts',(-23.5671139309305,-68.2185478493422,
84.079473011853));
#206311=CARTESIAN_POINT('Ctrl Pts',(-23.5554441969661,-68.9062950368486,
84.4863247226585));
#206312=CARTESIAN_POINT('Ctrl Pts',(-23.5440549453205,-69.6305093949009,
84.8293747514801));
#206313=CARTESIAN_POINT('Ctrl Pts',(-23.5205294743053,-71.1540214987534,
85.3850651834414));
#206314=CARTESIAN_POINT('Ctrl Pts',(-23.5081796031131,-71.9514883296778,
85.5920974487091));
#206315=CARTESIAN_POINT('Ctrl Pts',(-23.4721296505077,-74.35151918976,85.9772996965807));
#206316=CARTESIAN_POINT('Ctrl Pts',(-23.4493257715468,-75.9787816509572,
85.9346245406171));
#206317=CARTESIAN_POINT('Ctrl Pts',(-23.4007516068439,-79.1437407796599,
85.2427926589473));
#206318=CARTESIAN_POINT('Ctrl Pts',(-23.3776454762801,-80.6572582810957,
84.5970625631179));
#206319=CARTESIAN_POINT('Ctrl Pts',(-23.3403526762986,-82.7109372940715,
83.2069683034375));
#206320=CARTESIAN_POINT('Ctrl Pts',(-23.3274897439032,-83.3662661428184,
82.6607486085139));
#206321=CARTESIAN_POINT('Ctrl Pts',(-23.3030014708831,-84.5258213302876,
81.4799624604339));
#206322=CARTESIAN_POINT('Ctrl Pts',(-23.2913605641575,-85.034784190624,
80.8531966773007));
#206323=CARTESIAN_POINT('Ctrl Pts',(-23.2731488040619,-85.70765912193,79.8406857186429));
#206324=CARTESIAN_POINT('Ctrl Pts',(-23.2669076997059,-85.9180739647768,
79.4879801447709));
#206325=CARTESIAN_POINT('Ctrl Pts',(-23.2363418036893,-86.8645556832143,
77.7111294603388));
#206326=CARTESIAN_POINT('Ctrl Pts',(-23.2132436084908,-87.3467226492629,
76.1605022589695));
#206327=CARTESIAN_POINT('Ctrl Pts',(-23.175941245244,-87.6147143249459,
73.7273574819035));
#206328=CARTESIAN_POINT('Ctrl Pts',(-23.1630923328797,-87.6230646296848,
72.8851889496547));
#206329=CARTESIAN_POINT('Ctrl Pts',(-23.1386272326453,-87.4767343480143,
71.2588084415927));
#206330=CARTESIAN_POINT('Ctrl Pts',(-23.1269905153998,-87.3310985127237,
70.4759290443774));
#206331=CARTESIAN_POINT('Ctrl Pts',(-23.1023462125104,-86.8837716791826,
68.9167373502622));
#206332=CARTESIAN_POINT('Ctrl Pts',(-23.0894884991715,-86.5768021364199,
68.1451374417125));
#206333=CARTESIAN_POINT('Ctrl Pts',(-23.0647799643539,-85.829283593617,
66.7003125165248));
#206334=CARTESIAN_POINT('Ctrl Pts',(-23.0529403525711,-85.3948197790364,
66.0267421448464));
#206335=CARTESIAN_POINT('Ctrl Pts',(-23.0283692983425,-84.3849372613321,
64.7498100788465));
#206336=CARTESIAN_POINT('Ctrl Pts',(-23.0154222549053,-83.8071005077573,
64.1532084285903));
#206337=CARTESIAN_POINT('Ctrl Pts',(-22.99053842165,-82.5722329130375,63.1087924579781));
#206338=CARTESIAN_POINT('Ctrl Pts',(-22.9786497998761,-81.9214231764334,
62.6567224664527));
#206339=CARTESIAN_POINT('Ctrl Pts',(-22.9417990983281,-79.7924045565062,
61.461416929723));
#206340=CARTESIAN_POINT('Ctrl Pts',(-22.9159564408366,-78.2107189619208,
60.9523140322316));
#206341=CARTESIAN_POINT('Ctrl Pts',(-22.8848941253731,-76.1771949820816,
60.7213246443215));
#206342=CARTESIAN_POINT('Ctrl Pts',(-22.8788053233581,-75.7757640352971,
60.695510659312));
#206343=CARTESIAN_POINT('Ctrl Pts',(-22.8601629334115,-74.5656541370941,
60.677377622671));
#206344=CARTESIAN_POINT('Ctrl Pts',(-22.8473408710596,-73.7577827747063,
60.745396728485));
#206345=CARTESIAN_POINT('Ctrl Pts',(-22.8226463499019,-72.1947956389624,
61.0335899700935));
#206346=CARTESIAN_POINT('Ctrl Pts',(-22.8107879232795,-71.4409244896018,
61.2483269085628));
#206347=CARTESIAN_POINT('Ctrl Pts',(-22.7739585650263,-69.2056667543144,
62.1240879218911));
#206348=CARTESIAN_POINT('Ctrl Pts',(-22.7483049277877,-67.8343233531809,
63.0075631318264));
#206349=CARTESIAN_POINT('Ctrl Pts',(-22.6985290046577,-65.5116117864563,
65.258515032746));
#206350=CARTESIAN_POINT('Ctrl Pts',(-22.6726909441823,-64.5903204088739,
66.6031378681104));
#206351=CARTESIAN_POINT('Ctrl Pts',(-22.6412225596302,-63.7954162090267,
68.4717174240335));
#206352=CARTESIAN_POINT('Ctrl Pts',(-22.6347891537382,-63.6522165345406,
68.863354422744));
#206353=CARTESIAN_POINT('Ctrl Pts',(-22.6081787237398,-63.1534172450102,
70.484438895471));
#206354=CARTESIAN_POINT('Ctrl Pts',(-22.5874829697694,-62.9747724558953,
71.7617031373275));
#206355=CARTESIAN_POINT('Ctrl Pts',(-22.5675364824894,-63.000102062494,
73.0394432284656));
#206356=CARTESIAN_POINT('',(-22.5675364829333,-75.6109359992393,84.9729941181988));
#206357=CARTESIAN_POINT('Origin',(-22.5675364832709,-75.,72.98888938658));
#206358=CARTESIAN_POINT('Ctrl Pts',(-22.5675364828275,-75.6109290148012,
84.9733322994732));
#206359=CARTESIAN_POINT('Ctrl Pts',(-22.5821246641341,-75.3281574487842,
85.0023542290885));
#206360=CARTESIAN_POINT('Ctrl Pts',(-22.596630345575,-75.043842888071,85.0212811334549));
#206361=CARTESIAN_POINT('Ctrl Pts',(-22.611072664767,-74.7587116498909,
85.0300127005126));
#206362=CARTESIAN_POINT('Ctrl Pts',(-22.6255527714042,-74.47283438326,85.0387671131816));
#206363=CARTESIAN_POINT('Ctrl Pts',(-22.6399691837917,-74.1861364033111,
85.037272755658));
#206364=CARTESIAN_POINT('Ctrl Pts',(-22.654341190157,-73.8993534342203,
85.0254808020076));
#206365=CARTESIAN_POINT('Ctrl Pts',(-22.6687338767193,-73.6121578067898,
85.013671880655));
#206366=CARTESIAN_POINT('Ctrl Pts',(-22.6830820293738,-73.3248771873067,
84.9915357218143));
#206367=CARTESIAN_POINT('Ctrl Pts',(-22.6974050197305,-73.0382505277424,
84.9590756102511));
#206368=CARTESIAN_POINT('Ctrl Pts',(-22.7117584358991,-72.7510149975009,
84.9265465448435));
#206369=CARTESIAN_POINT('Ctrl Pts',(-22.7260865827536,-72.464436447571,
84.8836496437199));
#206370=CARTESIAN_POINT('Ctrl Pts',(-22.7404089556177,-72.1792549800472,
84.8304404268251));
#206371=CARTESIAN_POINT('Ctrl Pts',(-22.7449598340071,-72.0886396755893,
84.8135334046727));
#206372=CARTESIAN_POINT('Ctrl Pts',(-22.7495101294396,-71.9981653826167,
84.7955856168891));
#206373=CARTESIAN_POINT('Ctrl Pts',(-22.7540604673341,-71.9078557089599,
84.7765999369993));
#206374=CARTESIAN_POINT('Ctrl Pts',(-22.7682603128447,-71.6260341291668,
84.7173529695006));
#206375=CARTESIAN_POINT('Ctrl Pts',(-22.7824601583553,-71.3458242246531,
84.6479966081915));
#206376=CARTESIAN_POINT('Ctrl Pts',(-22.7966600038659,-71.0679483801829,
84.5686364662497));
#206377=CARTESIAN_POINT('Ctrl Pts',(-22.8108441312213,-70.7903801232612,
84.4893641699843));
#206378=CARTESIAN_POINT('Ctrl Pts',(-22.8250282585766,-70.515141007826,
84.4001102585464));
#206379=CARTESIAN_POINT('Ctrl Pts',(-22.8392123859319,-70.2429441245523,
84.3010315317623));
#206380=CARTESIAN_POINT('Ctrl Pts',(-22.853385763729,-69.9709535279384,
84.202027892611));
#206381=CARTESIAN_POINT('Ctrl Pts',(-22.8675591415261,-69.7020007974385,
84.0932143694529));
#206382=CARTESIAN_POINT('Ctrl Pts',(-22.8817325193231,-69.4367868456689,
83.9747983265722));
#206383=CARTESIAN_POINT('Ctrl Pts',(-22.8958952491312,-69.1717721403508,
83.8564712457396));
#206384=CARTESIAN_POINT('Ctrl Pts',(-22.9100579789394,-68.9104908376335,
83.7285561304041));
#206385=CARTESIAN_POINT('Ctrl Pts',(-22.9242207087475,-68.653628106899,
83.591309932742));
#206386=CARTESIAN_POINT('Ctrl Pts',(-22.938372891472,-68.3969566636294,
83.4541659432794));
#206387=CARTESIAN_POINT('Ctrl Pts',(-22.9525250741966,-68.144697447945,
83.3077048435254));
#206388=CARTESIAN_POINT('Ctrl Pts',(-22.9666772569212,-67.8975164005641,
83.1522319476065));
#206389=CARTESIAN_POINT('Ctrl Pts',(-22.9808147545176,-67.6505918426178,
82.9969203794091));
#206390=CARTESIAN_POINT('Ctrl Pts',(-22.9949522521141,-67.4087351462392,
82.8326158057185));
#206391=CARTESIAN_POINT('Ctrl Pts',(-23.0090897497105,-67.1725890602893,
82.6596701102742));
#206392=CARTESIAN_POINT('Ctrl Pts',(-23.0232178305834,-66.9366002668442,
82.486839610733));
#206393=CARTESIAN_POINT('Ctrl Pts',(-23.0373459114563,-66.7063146993105,
82.3053796080079));
#206394=CARTESIAN_POINT('Ctrl Pts',(-23.0514739923292,-66.4823493669846,
82.1156872009453));
#206395=CARTESIAN_POINT('Ctrl Pts',(-23.0655889575852,-66.2585919499107,
81.9261708923182));
#206396=CARTESIAN_POINT('Ctrl Pts',(-23.0797039228413,-66.041143249399,
81.7284375853738));
#206397=CARTESIAN_POINT('Ctrl Pts',(-23.0938188880973,-65.830590911148,
81.5229273256862));
#206398=CARTESIAN_POINT('Ctrl Pts',(-23.1038933836672,-65.6803100878887,
81.3762452642536));
#206399=CARTESIAN_POINT('Ctrl Pts',(-23.1139678792372,-65.5335419290588,
81.2256022909387));
#206400=CARTESIAN_POINT('Ctrl Pts',(-23.1240423748071,-65.3904905950289,
81.0711715801781));
#206401=CARTESIAN_POINT('Ctrl Pts',(-23.1381651212176,-65.1899567121992,
80.854685727271));
#206402=CARTESIAN_POINT('Ctrl Pts',(-23.1522876470479,-64.9967312179457,
80.6307580746604));
#206403=CARTESIAN_POINT('Ctrl Pts',(-23.1663998896931,-64.8113536809775,
80.3998921770478));
#206404=CARTESIAN_POINT('Ctrl Pts',(-23.180471970665,-64.62650370524,80.1696832948376));
#206405=CARTESIAN_POINT('Ctrl Pts',(-23.1945338268978,-64.4494572724507,
79.9325757540484));
#206406=CARTESIAN_POINT('Ctrl Pts',(-23.2085754814533,-64.2807160422135,
79.6891085031234));
#206407=CARTESIAN_POINT('Ctrl Pts',(-23.2225931230921,-64.1122633797579,
79.4460576104554));
#206408=CARTESIAN_POINT('Ctrl Pts',(-23.2365906320891,-63.9520877249764,
79.1966688991191));
#206409=CARTESIAN_POINT('Ctrl Pts',(-23.2505580826038,-63.8006520861989,
78.9415158489573));
#206410=CARTESIAN_POINT('Ctrl Pts',(-23.2644919766452,-63.649580268003,
78.6869757980333));
#206411=CARTESIAN_POINT('Ctrl Pts',(-23.2783959564603,-63.5072066914697,
78.426699247846));
#206412=CARTESIAN_POINT('Ctrl Pts',(-23.2922601675768,-63.3739524299285,
78.1612901952514));
#206413=CARTESIAN_POINT('Ctrl Pts',(-23.2975737953982,-63.3228811107241,
78.059568942302));
#206414=CARTESIAN_POINT('Ctrl Pts',(-23.3028815815994,-63.2731489095241,
77.9570941250166));
#206415=CARTESIAN_POINT('Ctrl Pts',(-23.3081829713997,-63.2247779436,77.8539010146614));
#206416=CARTESIAN_POINT('Origin',(-54.462516693425,-83.3223805071439,69.5544896765311));
#206417=CARTESIAN_POINT('',(-55.3469857987243,-91.723644464318,66.083453584911));
#206418=CARTESIAN_POINT('',(-55.5509564659454,-91.7236201228015,66.0833946695129));
#206419=CARTESIAN_POINT('',(-54.462516693425,-91.723644464317,66.0834535849087));
#206420=CARTESIAN_POINT('',(-55.3469876474783,-91.7236667394131,66.0835074998375));
#206421=CARTESIAN_POINT('Ctrl Pts',(-55.3469857987243,-91.7236444643189,
66.0834535849133));
#206422=CARTESIAN_POINT('Ctrl Pts',(-55.346986520562,-91.7236531615995,
66.0834746357314));
#206423=CARTESIAN_POINT('Ctrl Pts',(-55.34698692564,-91.723658042266,66.0834864489593));
#206424=CARTESIAN_POINT('Ctrl Pts',(-55.3469876474783,-91.7236667394131,
66.0835074998375));
#206425=CARTESIAN_POINT('',(-55.5974859706232,-91.412754510303,73.6987840815407));
#206426=CARTESIAN_POINT('Ctrl Pts',(-55.5958816852329,-91.4127370632666,
73.6988181411009));
#206427=CARTESIAN_POINT('Ctrl Pts',(-55.5642543225697,-91.8629650956877,
72.819904863597));
#206428=CARTESIAN_POINT('Ctrl Pts',(-55.5337095641794,-92.1669780783263,
71.8734645115866));
#206429=CARTESIAN_POINT('Ctrl Pts',(-55.4920076933008,-92.3608742713118,
70.5747597609729));
#206430=CARTESIAN_POINT('Ctrl Pts',(-55.4815921437647,-92.3916148160222,
70.2504131744611));
#206431=CARTESIAN_POINT('Ctrl Pts',(-55.4607410660172,-92.4182954809193,
69.5965855223249));
#206432=CARTESIAN_POINT('Ctrl Pts',(-55.4503222021789,-92.4138665426036,
69.2675652529914));
#206433=CARTESIAN_POINT('Ctrl Pts',(-55.4246589713448,-92.3587245966684,
68.4543773063775));
#206434=CARTESIAN_POINT('Ctrl Pts',(-55.409556102247,-92.2869555829917,
67.9726706635948));
#206435=CARTESIAN_POINT('Ctrl Pts',(-55.3785950880418,-92.0647860076726,
67.0155987805646));
#206436=CARTESIAN_POINT('Ctrl Pts',(-55.3627155406804,-91.9131659682807,
66.5421780378772));
#206437=CARTESIAN_POINT('Ctrl Pts',(-55.3469876474783,-91.7236667394131,
66.0835074998375));
#206438=CARTESIAN_POINT('',(-55.7997963168797,-91.4127793742771,73.6987355424395));
#206439=CARTESIAN_POINT('',(-55.7986426798444,-91.4127669427988,73.6987598112127));
#206440=CARTESIAN_POINT('Ctrl Pts',(-55.8013975426224,-91.412796628927,
73.698701857855));
#206441=CARTESIAN_POINT('Ctrl Pts',(-55.7703307595378,-91.8629858380135,
72.8198332392404));
#206442=CARTESIAN_POINT('Ctrl Pts',(-55.738609114948,-92.1669747337267,
71.873445907533));
#206443=CARTESIAN_POINT('Ctrl Pts',(-55.6969348134739,-92.3608675733566,
70.5748181414705));
#206444=CARTESIAN_POINT('Ctrl Pts',(-55.6866939433116,-92.391610150729,
70.250473608271));
#206445=CARTESIAN_POINT('Ctrl Pts',(-55.6660029351568,-92.4182926717337,
69.596708773076));
#206446=CARTESIAN_POINT('Ctrl Pts',(-55.6555661301364,-92.4138699937926,
69.2677545658029));
#206447=CARTESIAN_POINT('Ctrl Pts',(-55.6294909009479,-92.3587621242832,
68.4547261711261));
#206448=CARTESIAN_POINT('Ctrl Pts',(-55.6137725475604,-92.2870277037053,
67.9731075839917));
#206449=CARTESIAN_POINT('Ctrl Pts',(-55.5823353923309,-92.0648910629054,
67.0159225655132));
#206450=CARTESIAN_POINT('Ctrl Pts',(-55.5667469045371,-91.9132233140617,
66.542308496053));
#206451=CARTESIAN_POINT('Ctrl Pts',(-55.5509584931268,-91.7236444643153,
66.0834535849044));
#206452=CARTESIAN_POINT('Origin',(-54.462516693425,-83.3223805071439,69.5544896765311));
#206453=CARTESIAN_POINT('',(-53.7366673713217,-91.723644464317,66.0834535849087));
#206454=CARTESIAN_POINT('Ctrl Pts',(-55.5509564659454,-91.7236201228015,
66.0833946695129));
#206455=CARTESIAN_POINT('Ctrl Pts',(-55.5253406144712,-91.4160335965772,
65.3389298524642));
#206456=CARTESIAN_POINT('Ctrl Pts',(-55.499177208642,-91.0108624303868,
64.6386582185305));
#206457=CARTESIAN_POINT('Ctrl Pts',(-55.4649203412003,-90.3546999993681,
63.7883894770221));
#206458=CARTESIAN_POINT('Ctrl Pts',(-55.4564180486514,-90.1813120932266,
63.5831843472978));
#206459=CARTESIAN_POINT('Ctrl Pts',(-55.4139500320902,-89.2736657850213,
62.6007636815008));
#206460=CARTESIAN_POINT('Ctrl Pts',(-55.3792856629007,-88.4153855626199,
61.9496622562324));
#206461=CARTESIAN_POINT('Ctrl Pts',(-55.3295877163154,-87.0236837526852,
61.2373934801853));
#206462=CARTESIAN_POINT('Ctrl Pts',(-55.3139307707429,-86.5659575586731,
61.0484365270062));
#206463=CARTESIAN_POINT('Ctrl Pts',(-55.2817007715712,-85.6100419548281,
60.7422595286418));
#206464=CARTESIAN_POINT('Ctrl Pts',(-55.2651677518206,-85.1127393687324,
60.6279334855877));
#206465=CARTESIAN_POINT('Ctrl Pts',(-55.2318058404901,-84.0844658784889,
60.4809698156442));
#206466=CARTESIAN_POINT('Ctrl Pts',(-55.2151595260833,-83.5549019378558,
60.4519914605089));
#206467=CARTESIAN_POINT('Ctrl Pts',(-55.1888140433165,-82.7288173444309,
60.4789553904715));
#206468=CARTESIAN_POINT('Ctrl Pts',(-55.1792958474904,-82.432457690611,
60.503209361488));
#206469=CARTESIAN_POINT('Ctrl Pts',(-55.1508190163822,-81.5555431189953,
60.6184660617054));
#206470=CARTESIAN_POINT('Ctrl Pts',(-55.1318383003285,-80.9820421247767,
60.7512479253814));
#206471=CARTESIAN_POINT('Ctrl Pts',(-55.0961446844521,-79.9156960526322,
61.1097895713274));
#206472=CARTESIAN_POINT('Ctrl Pts',(-55.0791754766682,-79.4222373340945,
61.3260426781999));
#206473=CARTESIAN_POINT('Ctrl Pts',(-55.0438935942482,-78.45655296532,61.8557352858212));
#206474=CARTESIAN_POINT('Ctrl Pts',(-55.0256364353789,-77.9885983572908,
62.1722223704164));
#206475=CARTESIAN_POINT('Ctrl Pts',(-54.9915987477152,-77.1614187804716,
62.8516079108152));
#206476=CARTESIAN_POINT('Ctrl Pts',(-54.975718254108,-76.7974323150567,
63.2053850855324));
#206477=CARTESIAN_POINT('Ctrl Pts',(-54.9403850939478,-76.0674404738522,
64.0443477157309));
#206478=CARTESIAN_POINT('Ctrl Pts',(-54.9208907207808,-75.7166775474428,
64.5396028529349));
#206479=CARTESIAN_POINT('Ctrl Pts',(-54.8839584790557,-75.1452993913132,
65.5458567131022));
#206480=CARTESIAN_POINT('Ctrl Pts',(-54.8667561360868,-74.9170969844313,
66.0494924928167));
#206481=CARTESIAN_POINT('Ctrl Pts',(-54.83998383377,-74.6389915050204,66.8497939573887));
#206482=CARTESIAN_POINT('Ctrl Pts',(-54.8306045323765,-74.5556733575306,
67.1334428927245));
#206483=CARTESIAN_POINT('Ctrl Pts',(-54.8021658342044,-74.3464359145047,
67.9998759261224));
#206484=CARTESIAN_POINT('Ctrl Pts',(-54.7830927686022,-74.2638476955701,
68.5914704138563));
#206485=CARTESIAN_POINT('Ctrl Pts',(-54.7469068017329,-74.2172592799442,
69.7425478357616));
#206486=CARTESIAN_POINT('Ctrl Pts',(-54.7295252927433,-74.2458093029776,
70.2991043775261));
#206487=CARTESIAN_POINT('Ctrl Pts',(-54.6965489919458,-74.3938205201781,
71.3274016364934));
#206488=CARTESIAN_POINT('Ctrl Pts',(-54.6810877967896,-74.5005601325604,
71.7990126971426));
#206489=CARTESIAN_POINT('Ctrl Pts',(-54.6493649564325,-74.7992884554055,
72.7572393588683));
#206490=CARTESIAN_POINT('Ctrl Pts',(-54.633222982179,-74.9967973872929,
73.2403241082785));
#206491=CARTESIAN_POINT('Ctrl Pts',(-54.5991420837953,-75.4918730210743,
74.2053133978508));
#206492=CARTESIAN_POINT('Ctrl Pts',(-54.5812202360521,-75.7952380768797,
74.6817818149948));
#206493=CARTESIAN_POINT('Ctrl Pts',(-54.5453238306149,-76.4884066377811,
75.5750969417076));
#206494=CARTESIAN_POINT('Ctrl Pts',(-54.5277297748132,-76.8772124124529,
75.9896059893803));
#206495=CARTESIAN_POINT('Ctrl Pts',(-54.4819257350201,-77.9740545973449,
76.9591547834969));
#206496=CARTESIAN_POINT('Ctrl Pts',(-54.4532575477271,-78.7302245928105,
77.4504226526004));
#206497=CARTESIAN_POINT('Ctrl Pts',(-54.4107330167955,-79.9661825106565,
78.0149052710252));
#206498=CARTESIAN_POINT('Ctrl Pts',(-54.3964014837232,-80.4003698580541,
78.1744984640816));
#206499=CARTESIAN_POINT('Ctrl Pts',(-54.3591923632934,-81.5395675299457,
78.497215353792));
#206500=CARTESIAN_POINT('Ctrl Pts',(-54.3360840119932,-82.2553141229639,
78.6105448520134));
#206501=CARTESIAN_POINT('Ctrl Pts',(-54.2946909823775,-83.5740771167809,
78.6607025923809));
#206502=CARTESIAN_POINT('Ctrl Pts',(-54.2761788315971,-84.172040314975,
78.6244701487551));
#206503=CARTESIAN_POINT('Ctrl Pts',(-54.2388429635918,-85.3389900226743,
78.4372802732549));
#206504=CARTESIAN_POINT('Ctrl Pts',(-54.2201325490364,-85.9056061561151,
78.289341054598));
#206505=CARTESIAN_POINT('Ctrl Pts',(-54.1869301714564,-86.8954795985849,
77.9260696013056));
#206506=CARTESIAN_POINT('Ctrl Pts',(-54.1723247323716,-87.3236339645411,
77.7300851767745));
#206507=CARTESIAN_POINT('Ctrl Pts',(-54.1396768312147,-88.2308002103648,
77.2264331940259));
#206508=CARTESIAN_POINT('Ctrl Pts',(-54.1215896175882,-88.700016029907,
76.9051579967057));
#206509=CARTESIAN_POINT('Ctrl Pts',(-54.0855118501413,-89.570195644652,
76.1811678713697));
#206510=CARTESIAN_POINT('Ctrl Pts',(-54.0679007931629,-89.9696053805803,
75.7804403591979));
#206511=CARTESIAN_POINT('Ctrl Pts',(-54.0318246827696,-90.699775972651,
74.8969280704418));
#206512=CARTESIAN_POINT('Ctrl Pts',(-54.0133105817151,-91.0264078359865,
74.4140740692207));
#206513=CARTESIAN_POINT('Ctrl Pts',(-53.9563753481728,-91.8772605937634,
72.8523420103975));
#206514=CARTESIAN_POINT('Ctrl Pts',(-53.9193773143486,-92.2366885164993,
71.6985282926277));
#206515=CARTESIAN_POINT('Ctrl Pts',(-53.8422853477732,-92.4884677919132,
69.3122004932929));
#206516=CARTESIAN_POINT('Ctrl Pts',(-53.8049835202226,-92.3760370261865,
68.1028845572067));
#206517=CARTESIAN_POINT('Ctrl Pts',(-53.7563177440248,-91.9434278986667,
66.6559697698948));
#206518=CARTESIAN_POINT('Ctrl Pts',(-53.7464297999027,-91.840622165608,
66.3665853414526));
#206519=CARTESIAN_POINT('Ctrl Pts',(-53.7366673713217,-91.723644464317,
66.0834535849086));
#206520=CARTESIAN_POINT('',(-53.5332787937082,-91.723644464317,66.0834535849087));
#206521=CARTESIAN_POINT('',(-54.462516693425,-91.723644464317,66.0834535849087));
#206522=CARTESIAN_POINT('Ctrl Pts',(-53.5332787937083,-91.723644464317,
66.0834535849087));
#206523=CARTESIAN_POINT('Ctrl Pts',(-53.5657195167862,-92.1151475890021,
67.0310441612429));
#206524=CARTESIAN_POINT('Ctrl Pts',(-53.5973634442256,-92.3439610858943,
68.0391740587059));
#206525=CARTESIAN_POINT('Ctrl Pts',(-53.6681363979854,-92.4634382006625,
70.255572182143));
#206526=CARTESIAN_POINT('Ctrl Pts',(-53.7048128836741,-92.2928176317638,
71.4470291134669));
#206527=CARTESIAN_POINT('Ctrl Pts',(-53.7523402620046,-91.7996496083399,
72.8486549360197));
#206528=CARTESIAN_POINT('Ctrl Pts',(-53.7617426504722,-91.688776709542,
73.1208650366088));
#206529=CARTESIAN_POINT('Ctrl Pts',(-53.786786451322,-91.3554824097816,
73.8376344762896));
#206530=CARTESIAN_POINT('Ctrl Pts',(-53.8022949064406,-91.1094803549804,
74.2701164367684));
#206531=CARTESIAN_POINT('Ctrl Pts',(-53.8370000681781,-90.4915686602744,
75.1750728200328));
#206532=CARTESIAN_POINT('Ctrl Pts',(-53.8562507375944,-90.1056750278917,
75.6352062660166));
#206533=CARTESIAN_POINT('Ctrl Pts',(-53.8946704780553,-89.2476479911463,
76.4741486924331));
#206534=CARTESIAN_POINT('Ctrl Pts',(-53.9134537974272,-88.7773537289431,
76.8506354911319));
#206535=CARTESIAN_POINT('Ctrl Pts',(-53.9611704438665,-87.5172814248607,
77.6689760138519));
#206536=CARTESIAN_POINT('Ctrl Pts',(-53.9903650904549,-86.6923511147316,
78.0448008327604));
#206537=CARTESIAN_POINT('Ctrl Pts',(-54.0282062972691,-85.544557337223,
78.373603744593));
#206538=CARTESIAN_POINT('Ctrl Pts',(-54.0374535786892,-85.2597131482222,
78.4405227968045));
#206539=CARTESIAN_POINT('Ctrl Pts',(-54.0785753892556,-83.9888409347452,
78.6750690874694));
#206540=CARTESIAN_POINT('Ctrl Pts',(-54.1109468515645,-82.9823063063651,
78.6930609778407));
#206541=CARTESIAN_POINT('Ctrl Pts',(-54.1802667378603,-80.8218350429073,
78.3737049174265));
#206542=CARTESIAN_POINT('Ctrl Pts',(-54.2185359795977,-79.6955562779002,
77.9733633739001));
#206543=CARTESIAN_POINT('Ctrl Pts',(-54.2745230928638,-78.1805513773695,
77.0728314772297));
#206544=CARTESIAN_POINT('Ctrl Pts',(-54.2928997770395,-77.7127025180204,
76.7305175286025));
#206545=CARTESIAN_POINT('Ctrl Pts',(-54.32985904433,-76.8563102293101,75.9686688065897));
#206546=CARTESIAN_POINT('Ctrl Pts',(-54.348232801788,-76.4683492925215,
75.55232514257));
#206547=CARTESIAN_POINT('Ctrl Pts',(-54.3843160526939,-75.7754913847371,
74.6530862583423));
#206548=CARTESIAN_POINT('Ctrl Pts',(-54.4022512089587,-75.472048291573,
74.172227659856));
#206549=CARTESIAN_POINT('Ctrl Pts',(-54.437648539979,-74.9736500514926,
73.1895548373869));
#206550=CARTESIAN_POINT('Ctrl Pts',(-54.4549919408042,-74.7743974936499,
72.6924811395345));
#206551=CARTESIAN_POINT('Ctrl Pts',(-54.4875469135902,-74.479453168947,
71.715164396541));
#206552=CARTESIAN_POINT('Ctrl Pts',(-54.5028358478436,-74.3765284857388,
71.2390119239194));
#206553=CARTESIAN_POINT('Ctrl Pts',(-54.5349881372755,-74.2429215168278,
70.2378493047272));
#206554=CARTESIAN_POINT('Ctrl Pts',(-54.5518339283031,-74.2186352695932,
69.7137693766174));
#206555=CARTESIAN_POINT('Ctrl Pts',(-54.5878262127692,-74.2634625619525,
68.5950860467173));
#206556=CARTESIAN_POINT('Ctrl Pts',(-54.6065435845373,-74.3458180137023,
68.0034318408713));
#206557=CARTESIAN_POINT('Ctrl Pts',(-54.6347501469436,-74.5547303361902,
67.1368578406274));
#206558=CARTESIAN_POINT('Ctrl Pts',(-54.6441345970218,-74.6379430599501,
66.8531607831728));
#206559=CARTESIAN_POINT('Ctrl Pts',(-54.6711606893686,-74.9153107845357,
66.0539869969008));
#206560=CARTESIAN_POINT('Ctrl Pts',(-54.6889164174018,-75.1426642602809,
65.5514169729881));
#206561=CARTESIAN_POINT('Ctrl Pts',(-54.725247238577,-75.7086005862016,
64.5528422799759));
#206562=CARTESIAN_POINT('Ctrl Pts',(-54.7438770726153,-76.0536243028582,
64.0634688125614));
#206563=CARTESIAN_POINT('Ctrl Pts',(-54.7788210658079,-76.7728794956045,
63.231027367026));
#206564=CARTESIAN_POINT('Ctrl Pts',(-54.7949554163308,-77.1326060662042,
62.8785008434476));
#206565=CARTESIAN_POINT('Ctrl Pts',(-54.830365641688,-77.9899850958522,
62.1674548966518));
#206566=CARTESIAN_POINT('Ctrl Pts',(-54.84930305249,-78.4984758404145,61.8257982800024));
#206567=CARTESIAN_POINT('Ctrl Pts',(-54.8847262838848,-79.4888465396703,
61.2964396989534));
#206568=CARTESIAN_POINT('Ctrl Pts',(-54.9010447988734,-79.9598814487711,
61.0936998418295));
#206569=CARTESIAN_POINT('Ctrl Pts',(-54.9360087087864,-81.0022565798859,
60.7459210379695));
#206570=CARTESIAN_POINT('Ctrl Pts',(-54.9542468382506,-81.5757330457078,
60.6145186004252));
#206571=CARTESIAN_POINT('Ctrl Pts',(-54.9819564822361,-82.4524902379245,
60.5012653520307));
#206572=CARTESIAN_POINT('Ctrl Pts',(-54.9913056516659,-82.7488018448857,
60.4776738507298));
#206573=CARTESIAN_POINT('Ctrl Pts',(-55.0176841874367,-83.5815196074021,
60.4523192208539));
#206574=CARTESIAN_POINT('Ctrl Pts',(-55.0348210866761,-84.1177017372103,
60.48342958032));
#206575=CARTESIAN_POINT('Ctrl Pts',(-55.0705671886528,-85.2440162653569,
60.6494582951026));
#206576=CARTESIAN_POINT('Ctrl Pts',(-55.089200938564,-85.8298129690779,
60.7963474225708));
#206577=CARTESIAN_POINT('Ctrl Pts',(-55.1231960096561,-86.8443013749974,
61.1609466417267));
#206578=CARTESIAN_POINT('Ctrl Pts',(-55.1383443905106,-87.278530347074,
61.3566628218977));
#206579=CARTESIAN_POINT('Ctrl Pts',(-55.1777226776238,-88.3692955365197,
61.9552272237522));
#206580=CARTESIAN_POINT('Ctrl Pts',(-55.2013284446643,-88.9935284884356,
62.4089859390303));
#206581=CARTESIAN_POINT('Ctrl Pts',(-55.2455894770798,-90.0144103447644,
63.3700487284535));
#206582=CARTESIAN_POINT('Ctrl Pts',(-55.2658400124447,-90.4289847484269,
63.8512660279433));
#206583=CARTESIAN_POINT('Ctrl Pts',(-55.3061069537296,-91.1617894580098,
64.9071414971543));
#206584=CARTESIAN_POINT('Ctrl Pts',(-55.3263288657872,-91.4747531335122,
65.4810392879816));
#206585=CARTESIAN_POINT('Ctrl Pts',(-55.3469857987243,-91.7236444643189,
66.0834535849133));
#206586=CARTESIAN_POINT('Origin',(-54.462516693425,-83.3223805071439,69.5544896765311));
#206587=CARTESIAN_POINT('',(-51.719048945098,-91.723644464317,66.0834535849086));
#206588=CARTESIAN_POINT('',(-51.9229031371334,-91.723644464317,66.0834535849087));
#206589=CARTESIAN_POINT('',(-54.462516693425,-91.723644464317,66.0834535849087));
#206590=CARTESIAN_POINT('Ctrl Pts',(-51.719048945098,-91.723644464317,66.0834535849086));
#206591=CARTESIAN_POINT('Ctrl Pts',(-51.7280460948346,-91.8334313256315,
66.3491806982507));
#206592=CARTESIAN_POINT('Ctrl Pts',(-51.7370778457283,-91.9306157095051,
66.6201278091617));
#206593=CARTESIAN_POINT('Ctrl Pts',(-51.7649159822995,-92.188226276821,
67.462244733628));
#206594=CARTESIAN_POINT('Ctrl Pts',(-51.7839197817191,-92.3057665340331,
68.0446929603594));
#206595=CARTESIAN_POINT('Ctrl Pts',(-51.8173273069588,-92.413046642744,
69.0991564993682));
#206596=CARTESIAN_POINT('Ctrl Pts',(-51.8318573841923,-92.4244346559946,
69.566843120823));
#206597=CARTESIAN_POINT('Ctrl Pts',(-51.864463419202,-92.3699133844991,
70.6004128247021));
#206598=CARTESIAN_POINT('Ctrl Pts',(-51.8825878956557,-92.2869251622951,
71.1634435721421));
#206599=CARTESIAN_POINT('Ctrl Pts',(-51.9187219781746,-92.0178233248715,
72.2631931788643));
#206600=CARTESIAN_POINT('Ctrl Pts',(-51.9363519248122,-91.832936819118,
72.7976724134826));
#206601=CARTESIAN_POINT('Ctrl Pts',(-51.9724938200408,-91.3590176540957,
73.8417798068455));
#206602=CARTESIAN_POINT('Ctrl Pts',(-51.9910560470183,-91.0679569868936,
74.3476539661278));
#206603=CARTESIAN_POINT('Ctrl Pts',(-52.0390763812932,-90.1999704828028,
75.5683310544183));
#206604=CARTESIAN_POINT('Ctrl Pts',(-52.0675003869634,-89.5597247088562,
76.230047794052));
#206605=CARTESIAN_POINT('Ctrl Pts',(-52.1125565717711,-88.4385887425772,
77.0842789749737));
#206606=CARTESIAN_POINT('Ctrl Pts',(-52.1285174301459,-88.0219464583443,
77.3511164603119));
#206607=CARTESIAN_POINT('Ctrl Pts',(-52.1536914625528,-87.3265022713049,
77.7204228076833));
#206608=CARTESIAN_POINT('Ctrl Pts',(-52.1629664133898,-87.0607943022757,
77.8454316115363));
#206609=CARTESIAN_POINT('Ctrl Pts',(-52.2097874835752,-85.6932541589566,
78.4096942627259));
#206610=CARTESIAN_POINT('Ctrl Pts',(-52.2480366809078,-84.5190110283137,
78.6431507396296));
#206611=CARTESIAN_POINT('Ctrl Pts',(-52.3040609088526,-82.7530810212965,
78.6452356797767));
#206612=CARTESIAN_POINT('Ctrl Pts',(-52.3224844475056,-82.1743185992721,
78.5904019278873));
#206613=CARTESIAN_POINT('Ctrl Pts',(-52.3594985379059,-81.0469595321664,
78.3734708628753));
#206614=CARTESIAN_POINT('Ctrl Pts',(-52.377865835396,-80.5004550770134,
78.2140925191472));
#206615=CARTESIAN_POINT('Ctrl Pts',(-52.4140204960253,-79.4433398869284,
77.7950159961957));
#206616=CARTESIAN_POINT('Ctrl Pts',(-52.4320383530452,-78.9351414315279,
77.5360534123711));
#206617=CARTESIAN_POINT('Ctrl Pts',(-52.4673467810817,-78.0085664234786,
76.9485093849778));
#206618=CARTESIAN_POINT('Ctrl Pts',(-52.4845077086776,-77.588112981137,
76.6274189899154));
#206619=CARTESIAN_POINT('Ctrl Pts',(-52.5178166694003,-76.8176849777865,
75.9249704882126));
#206620=CARTESIAN_POINT('Ctrl Pts',(-52.5340251926803,-76.4675761418157,
75.546630457846));
#206621=CARTESIAN_POINT('Ctrl Pts',(-52.5660246163178,-75.8522482829902,
74.7567348376003));
#206622=CARTESIAN_POINT('Ctrl Pts',(-52.5817363415229,-75.5844589623201,
74.3493612567707));
#206623=CARTESIAN_POINT('Ctrl Pts',(-52.6167570837017,-75.0627908399065,
73.3972988686499));
#206624=CARTESIAN_POINT('Ctrl Pts',(-52.6356418548615,-74.827614268292,
72.8449236210996));
#206625=CARTESIAN_POINT('Ctrl Pts',(-52.6640308229148,-74.5603214710058,
71.9922158021785));
#206626=CARTESIAN_POINT('Ctrl Pts',(-52.6734291289318,-74.4858967729631,
71.706869928634));
#206627=CARTESIAN_POINT('Ctrl Pts',(-52.7002855574127,-74.3142335361895,
70.8874847239771));
#206628=CARTESIAN_POINT('Ctrl Pts',(-52.7178595812873,-74.2507502221464,
70.3476595574776));
#206629=CARTESIAN_POINT('Ctrl Pts',(-52.752096062351,-74.2210464530811,
69.2719619690269));
#206630=CARTESIAN_POINT('Ctrl Pts',(-52.7688275234276,-74.2533190989187,
68.7382583579621));
#206631=CARTESIAN_POINT('Ctrl Pts',(-52.8016868286785,-74.4059514719878,
67.7172952524294));
#206632=CARTESIAN_POINT('Ctrl Pts',(-52.8177219971952,-74.5201382176993,
67.2310193615866));
#206633=CARTESIAN_POINT('Ctrl Pts',(-52.867566236269,-74.9988198589066,
65.7513459596427));
#206634=CARTESIAN_POINT('Ctrl Pts',(-52.90022275574,-75.4967926656062,64.8104686040742));
#206635=CARTESIAN_POINT('Ctrl Pts',(-52.9434349944675,-76.3254294934196,
63.7442985008549));
#206636=CARTESIAN_POINT('Ctrl Pts',(-52.9528453118307,-76.5168628756349,
63.5212006958766));
#206637=CARTESIAN_POINT('Ctrl Pts',(-52.9767428589438,-77.034707258445,
62.9737704318796));
#206638=CARTESIAN_POINT('Ctrl Pts',(-52.9910699917563,-77.3755367382101,
62.6642244244901));
#206639=CARTESIAN_POINT('Ctrl Pts',(-53.0242260319202,-78.2065432609747,
62.0172722664003));
#206640=CARTESIAN_POINT('Ctrl Pts',(-53.0431193134892,-78.7093350915824,
61.6994762410419));
#206641=CARTESIAN_POINT('Ctrl Pts',(-53.0807685885445,-79.7650676593376,
61.168733962228));
#206642=CARTESIAN_POINT('Ctrl Pts',(-53.0990847605614,-80.3150535149487,
60.9561548028325));
#206643=CARTESIAN_POINT('Ctrl Pts',(-53.1268493395572,-81.1679120998688,
60.7184347319786));
#206644=CARTESIAN_POINT('Ctrl Pts',(-53.1362014375202,-81.45784823377,60.6527416001073));
#206645=CARTESIAN_POINT('Ctrl Pts',(-53.1623121165999,-82.2698361804076,
60.5101806660068));
#206646=CARTESIAN_POINT('Ctrl Pts',(-53.1791828605216,-82.7961449935915,
60.4643601668526));
#206647=CARTESIAN_POINT('Ctrl Pts',(-53.2124636760748,-83.8540302211001,
60.4644846454046));
#206648=CARTESIAN_POINT('Ctrl Pts',(-53.2288874125688,-84.3835885296855,
60.5110010669611));
#206649=CARTESIAN_POINT('Ctrl Pts',(-53.2610378261074,-85.3907108882269,
60.6891878464769));
#206650=CARTESIAN_POINT('Ctrl Pts',(-53.276671043153,-85.8675957484608,
60.81415561908));
#206651=CARTESIAN_POINT('Ctrl Pts',(-53.3108764445405,-86.8846094766451,
61.1710049267115));
#206652=CARTESIAN_POINT('Ctrl Pts',(-53.3290479274024,-87.4171800085415,
61.4178495324768));
#206653=CARTESIAN_POINT('Ctrl Pts',(-53.3566688180232,-88.178992072836,
61.8648066055644));
#206654=CARTESIAN_POINT('Ctrl Pts',(-53.3660137267013,-88.4281347463818,
62.0279251561229));
#206655=CARTESIAN_POINT('Ctrl Pts',(-53.3911629094711,-89.0716763700902,
62.4959452841395));
#206656=CARTESIAN_POINT('Ctrl Pts',(-53.407066244405,-89.4497625944017,
62.8215380421825));
#206657=CARTESIAN_POINT('Ctrl Pts',(-53.4377452891996,-90.1332324938202,
63.5156011965559));
#206658=CARTESIAN_POINT('Ctrl Pts',(-53.4524840198263,-90.4400476533254,
63.8804524211517));
#206659=CARTESIAN_POINT('Ctrl Pts',(-53.4842724605499,-91.0298464419758,
64.7053810477322));
#206660=CARTESIAN_POINT('Ctrl Pts',(-53.5013290324563,-91.303323594756,
65.1700373453449));
#206661=CARTESIAN_POINT('Ctrl Pts',(-53.5234014509498,-91.6010007635352,
65.7970814828092));
#206662=CARTESIAN_POINT('Ctrl Pts',(-53.5283529317896,-91.6641978752785,
65.9395696054042));
#206663=CARTESIAN_POINT('Ctrl Pts',(-53.5332787937083,-91.723644464317,
66.0834535849087));
#206664=CARTESIAN_POINT('Ctrl Pts',(-53.7366673713217,-91.723644464317,
66.0834535849086));
#206665=CARTESIAN_POINT('Ctrl Pts',(-53.7081486511214,-91.3819206498898,
65.2563483950824));
#206666=CARTESIAN_POINT('Ctrl Pts',(-53.6799428389359,-90.9192504983588,
64.4826307592131));
#206667=CARTESIAN_POINT('Ctrl Pts',(-53.6205979136531,-89.7534812546762,
63.061961521807));
#206668=CARTESIAN_POINT('Ctrl Pts',(-53.5911706934458,-89.0485028626822,
62.4324452838763));
#206669=CARTESIAN_POINT('Ctrl Pts',(-53.5444755169724,-87.8271557109556,
61.6423679278073));
#206670=CARTESIAN_POINT('Ctrl Pts',(-53.5277536797414,-87.3716511843474,
61.3998546839219));
#206671=CARTESIAN_POINT('Ctrl Pts',(-53.4943639663923,-86.4161470981597,
60.9910383146938));
#206672=CARTESIAN_POINT('Ctrl Pts',(-53.477868827646,-85.9172934505708,
60.8269172316276));
#206673=CARTESIAN_POINT('Ctrl Pts',(-53.4516685615217,-85.1176832971479,
60.6385142777415));
#206674=CARTESIAN_POINT('Ctrl Pts',(-53.4421396712361,-84.8251140688993,
60.5845666347126));
#206675=CARTESIAN_POINT('Ctrl Pts',(-53.4136787459053,-83.9496869128899,
60.4671831011763));
#206676=CARTESIAN_POINT('Ctrl Pts',(-53.3947130266225,-83.3627652415183,
60.4456456603646));
#206677=CARTESIAN_POINT('Ctrl Pts',(-53.3575363906055,-82.1948539359201,
60.5157322882943));
#206678=CARTESIAN_POINT('Ctrl Pts',(-53.3390801383436,-81.6165748291615,
60.606826546077));
#206679=CARTESIAN_POINT('Ctrl Pts',(-53.3051724791001,-80.5946300775601,
60.8705451302912));
#206680=CARTESIAN_POINT('Ctrl Pts',(-53.2899012688467,-80.1480680465343,
61.023648320535));
#206681=CARTESIAN_POINT('Ctrl Pts',(-53.258092727956,-79.2349494413321,
61.4183846660114));
#206682=CARTESIAN_POINT('Ctrl Pts',(-53.2416775377997,-78.7733335208115,
61.6671913019313));
#206683=CARTESIAN_POINT('Ctrl Pts',(-53.2048870899337,-77.8060578531907,
62.3018490196695));
#206684=CARTESIAN_POINT('Ctrl Pts',(-53.1844570247185,-77.3141925598406,
62.7037762270346));
#206685=CARTESIAN_POINT('Ctrl Pts',(-53.1464175027061,-76.4771458758857,
63.54779452327));
#206686=CARTESIAN_POINT('Ctrl Pts',(-53.1290649933464,-76.123105667652,
63.9770289722223));
#206687=CARTESIAN_POINT('Ctrl Pts',(-53.1021126849508,-75.6438721313054,
64.680339003139));
#206688=CARTESIAN_POINT('Ctrl Pts',(-53.0927016830157,-75.4893308377453,
64.9327836264796));
#206689=CARTESIAN_POINT('Ctrl Pts',(-53.0642539903233,-75.062400958165,
65.7133038623293));
#206690=CARTESIAN_POINT('Ctrl Pts',(-53.0451961493636,-74.829161823644,
66.2609771893408));
#206691=CARTESIAN_POINT('Ctrl Pts',(-53.0099273872458,-74.4931319576961,
67.3294870084385));
#206692=CARTESIAN_POINT('Ctrl Pts',(-52.993448087483,-74.3791499280365,
67.844258133295));
#206693=CARTESIAN_POINT('Ctrl Pts',(-52.9606545795369,-74.2441998094337,
68.8675436550239));
#206694=CARTESIAN_POINT('Ctrl Pts',(-52.9444199327525,-74.2200408829854,
69.3737424775123));
#206695=CARTESIAN_POINT('Ctrl Pts',(-52.9115850000357,-74.2570604093489,
70.4090587406393));
#206696=CARTESIAN_POINT('Ctrl Pts',(-52.8951339010643,-74.3223038731665,
70.9361344387688));
#206697=CARTESIAN_POINT('Ctrl Pts',(-52.8691675386007,-74.4947513726767,
71.7429312181892));
#206698=CARTESIAN_POINT('Ctrl Pts',(-52.8598398246234,-74.5703985491578,
72.0281757097949));
#206699=CARTESIAN_POINT('Ctrl Pts',(-52.831441180149,-74.8411860763033,
72.8796970721193));
#206700=CARTESIAN_POINT('Ctrl Pts',(-52.8123827895505,-75.0785053588338,
73.4308543314911));
#206701=CARTESIAN_POINT('Ctrl Pts',(-52.7779731269084,-75.6110275476858,
74.3934818088159));
#206702=CARTESIAN_POINT('Ctrl Pts',(-52.7623446454619,-75.8896711784268,
74.8114506577758));
#206703=CARTESIAN_POINT('Ctrl Pts',(-52.7308414567282,-76.5093068977027,
75.5924397235683));
#206704=CARTESIAN_POINT('Ctrl Pts',(-52.7150256792488,-76.8484732181349,
75.9547500962502));
#206705=CARTESIAN_POINT('Ctrl Pts',(-52.6828410795849,-77.603471320067,
76.6395301983887));
#206706=CARTESIAN_POINT('Ctrl Pts',(-52.6666477548464,-78.0211694719652,
76.9572517435316));
#206707=CARTESIAN_POINT('Ctrl Pts',(-52.6324118986522,-78.9444518435359,
77.541125514525));
#206708=CARTESIAN_POINT('Ctrl Pts',(-52.6143779457094,-79.4524560329032,
77.7992628054456));
#206709=CARTESIAN_POINT('Ctrl Pts',(-52.5783259604422,-80.5092209315993,
78.2169250335483));
#206710=CARTESIAN_POINT('Ctrl Pts',(-52.5607000542427,-81.0556045471753,
78.3756791360494));
#206711=CARTESIAN_POINT('Ctrl Pts',(-52.5248209603296,-82.1825893786859,
78.5914287432175));
#206712=CARTESIAN_POINT('Ctrl Pts',(-52.5065068731459,-82.7610782936583,
78.6457117134075));
#206713=CARTESIAN_POINT('Ctrl Pts',(-52.4503909217026,-84.526672052444,
78.64213871166));
#206714=CARTESIAN_POINT('Ctrl Pts',(-52.4140519239493,-85.7007150635981,
78.407692612271));
#206715=CARTESIAN_POINT('Ctrl Pts',(-52.3669348165057,-87.0678498890913,
77.8422494937059));
#206716=CARTESIAN_POINT('Ctrl Pts',(-52.3575824285834,-87.3335287584867,
77.716976802084));
#206717=CARTESIAN_POINT('Ctrl Pts',(-52.3314086005314,-88.0664208126591,
77.3269663614386));
#206718=CARTESIAN_POINT('Ctrl Pts',(-52.3147453575165,-88.5169069175132,
77.0334075397887));
#206719=CARTESIAN_POINT('Ctrl Pts',(-52.278844705326,-89.4109679345417,
76.3308417521056));
#206720=CARTESIAN_POINT('Ctrl Pts',(-52.259599526264,-89.8451558968429,
75.9139890291635));
#206721=CARTESIAN_POINT('Ctrl Pts',(-52.2200211865281,-90.6535981838277,
74.9672514545419));
#206722=CARTESIAN_POINT('Ctrl Pts',(-52.200021894855,-91.0188254223797,
74.4339856300373));
#206723=CARTESIAN_POINT('Ctrl Pts',(-52.1605548288282,-91.6091501467412,
73.3384892655007));
#206724=CARTESIAN_POINT('Ctrl Pts',(-52.141237348591,-91.8407471212749,
72.7835176472257));
#206725=CARTESIAN_POINT('Ctrl Pts',(-52.1044422891552,-92.178169658784,
71.6787799226605));
#206726=CARTESIAN_POINT('Ctrl Pts',(-52.0871102535623,-92.291365931404,
71.1340196262976));
#206727=CARTESIAN_POINT('Ctrl Pts',(-52.0424985454643,-92.4502601798141,
69.7378150761446));
#206728=CARTESIAN_POINT('Ctrl Pts',(-52.0149900853586,-92.4274449726464,
68.8839662172004));
#206729=CARTESIAN_POINT('Ctrl Pts',(-51.9700176984552,-92.1917695500525,
67.4837102574374));
#206730=CARTESIAN_POINT('Ctrl Pts',(-51.9520345802026,-92.0445164227658,
66.9317944930678));
#206731=CARTESIAN_POINT('Ctrl Pts',(-51.9301340171887,-91.807517641383,
66.2919126336795));
#206732=CARTESIAN_POINT('Ctrl Pts',(-51.9265206085477,-91.7665388982637,
66.187274879867));
#206733=CARTESIAN_POINT('Ctrl Pts',(-51.9229031371334,-91.723644464317,
66.0834535849086));
#206734=CARTESIAN_POINT('Origin',(-54.462516693425,-83.3223805071439,69.5544896765311));
#206735=CARTESIAN_POINT('',(-49.9050113929448,-91.723644464317,66.0834535849087));
#206736=CARTESIAN_POINT('',(-50.1089321285242,-91.723644464317,66.0834535849087));
#206737=CARTESIAN_POINT('',(-54.462516693425,-91.723644464317,66.0834535849087));
#206738=CARTESIAN_POINT('Ctrl Pts',(-49.9050113929448,-91.723644464317,
66.0834535849087));
#206739=CARTESIAN_POINT('Ctrl Pts',(-49.9147117058398,-91.8403594377234,
66.3659494372877));
#206740=CARTESIAN_POINT('Ctrl Pts',(-49.9244626372976,-91.9428230910478,
66.6543254260075));
#206741=CARTESIAN_POINT('Ctrl Pts',(-49.9517309550091,-92.1890499511924,
67.4768052963225));
#206742=CARTESIAN_POINT('Ctrl Pts',(-49.9688935132306,-92.2989198871257,
68.0194516718644));
#206743=CARTESIAN_POINT('Ctrl Pts',(-50.0043898234736,-92.4215248738981,
69.1433469378638));
#206744=CARTESIAN_POINT('Ctrl Pts',(-50.0227509272814,-92.4292556160134,
69.7226515170119));
#206745=CARTESIAN_POINT('Ctrl Pts',(-50.0700821175691,-92.3078097536682,
71.2009650734095));
#206746=CARTESIAN_POINT('Ctrl Pts',(-50.0980432890603,-92.0993310317001,
72.0870703510565));
#206747=CARTESIAN_POINT('Ctrl Pts',(-50.1425875368639,-91.5798671404784,
73.3869633985969));
#206748=CARTESIAN_POINT('Ctrl Pts',(-50.1584973666223,-91.3591583619826,
73.8304852136159));
#206749=CARTESIAN_POINT('Ctrl Pts',(-50.1835782418007,-90.9516542433398,
74.505221860558));
#206750=CARTESIAN_POINT('Ctrl Pts',(-50.1928159371108,-90.7877440328881,
74.7490941130108));
#206751=CARTESIAN_POINT('Ctrl Pts',(-50.2396278932642,-89.9002769757862,
75.9405196464941));
#206752=CARTESIAN_POINT('Ctrl Pts',(-50.2779141269498,-89.0071221000094,
76.7471110380068));
#206753=CARTESIAN_POINT('Ctrl Pts',(-50.3530205098722,-86.9676506000635,
77.9653378464173));
#206754=CARTESIAN_POINT('Ctrl Pts',(-50.3911527776497,-85.8426406719233,
78.3680389196349));
#206755=CARTESIAN_POINT('Ctrl Pts',(-50.4454549028411,-84.1491389977272,
78.6223152913914));
#206756=CARTESIAN_POINT('Ctrl Pts',(-50.4622048143095,-83.620317206025,
78.6550511697303));
#206757=CARTESIAN_POINT('Ctrl Pts',(-50.4946443774774,-82.6115628902654,
78.6294391630879));
#206758=CARTESIAN_POINT('Ctrl Pts',(-50.5102295271332,-82.133187995805,
78.5792217354898));
#206759=CARTESIAN_POINT('Ctrl Pts',(-50.5416388860715,-81.1692545932663,
78.4000294669564));
#206760=CARTESIAN_POINT('Ctrl Pts',(-50.5573857379669,-80.6858640745953,
78.2681750298379));
#206761=CARTESIAN_POINT('Ctrl Pts',(-50.582839067233,-79.936093350969,77.9955177805239));
#206762=CARTESIAN_POINT('Ctrl Pts',(-50.5923829353959,-79.6615733493138,
77.8801359072546));
#206763=CARTESIAN_POINT('Ctrl Pts',(-50.6208596996984,-78.865131215324,
77.4983677315371));
#206764=CARTESIAN_POINT('Ctrl Pts',(-50.6398117578377,-78.3627405419623,
77.1947944437293));
#206765=CARTESIAN_POINT('Ctrl Pts',(-50.674092270101,-77.4980312629215,
76.5508360117242));
#206766=CARTESIAN_POINT('Ctrl Pts',(-50.6896804164518,-77.1275757909721,
76.2250442796543));
#206767=CARTESIAN_POINT('Ctrl Pts',(-50.7225253822295,-76.4162681619046,
75.4888854656735));
#206768=CARTESIAN_POINT('Ctrl Pts',(-50.7397636875988,-76.0813858709865,
75.075307743088));
#206769=CARTESIAN_POINT('Ctrl Pts',(-50.7737436312742,-75.4894710256001,
74.1970733708151));
#206770=CARTESIAN_POINT('Ctrl Pts',(-50.7903345038232,-75.2331056399603,
73.7344048003945));
#206771=CARTESIAN_POINT('Ctrl Pts',(-50.816619305745,-74.8975005736952,
72.980710162863));
#206772=CARTESIAN_POINT('Ctrl Pts',(-50.8261301328098,-74.7900308770867,
72.7035525028149));
#206773=CARTESIAN_POINT('Ctrl Pts',(-50.8546215199752,-74.510732181035,
71.8632576213085));
#206774=CARTESIAN_POINT('Ctrl Pts',(-50.8736088777131,-74.3797901664283,
71.2881709298883));
#206775=CARTESIAN_POINT('Ctrl Pts',(-50.9110524784387,-74.2302936511775,
70.1159668952692));
#206776=CARTESIAN_POINT('Ctrl Pts',(-50.9297652579409,-74.2130331102534,
69.5215277769831));
#206777=CARTESIAN_POINT('Ctrl Pts',(-50.9680212726247,-74.2950623682846,
68.3309801614858));
#206778=CARTESIAN_POINT('Ctrl Pts',(-50.9873686041531,-74.3954959605317,
67.7378450388702));
#206779=CARTESIAN_POINT('Ctrl Pts',(-51.0224252766225,-74.6877939353173,
66.6679078683688));
#206780=CARTESIAN_POINT('Ctrl Pts',(-51.0384077358017,-74.8629495866275,
66.189007899432));
#206781=CARTESIAN_POINT('Ctrl Pts',(-51.0710032714289,-75.2939730226834,
65.2604331227147));
#206782=CARTESIAN_POINT('Ctrl Pts',(-51.0875646029802,-75.5499389045143,
64.8128238155847));
#206783=CARTESIAN_POINT('Ctrl Pts',(-51.1213167918691,-76.1521548514087,
63.940725506023));
#206784=CARTESIAN_POINT('Ctrl Pts',(-51.1382849145464,-76.501627236609,
63.5209325142995));
#206785=CARTESIAN_POINT('Ctrl Pts',(-51.1648071070228,-77.095135998754,
62.9259189949457));
#206786=CARTESIAN_POINT('Ctrl Pts',(-51.1741696656935,-77.313734766831,
62.7271404034891));
#206787=CARTESIAN_POINT('Ctrl Pts',(-51.2026019892191,-78.0023405478588,
62.1597006176973));
#206788=CARTESIAN_POINT('Ctrl Pts',(-51.2216756010864,-78.4993519598212,
61.8263499545555));
#206789=CARTESIAN_POINT('Ctrl Pts',(-51.2575462095671,-79.5071897115629,
61.2857231149347));
#206790=CARTESIAN_POINT('Ctrl Pts',(-51.2746156182036,-80.0112589861578,
61.0712914152227));
#206791=CARTESIAN_POINT('Ctrl Pts',(-51.3073510376501,-80.9940111643925,
60.7542525107014));
#206792=CARTESIAN_POINT('Ctrl Pts',(-51.3228975014517,-81.4677118574821,
60.6423810585827));
#206793=CARTESIAN_POINT('Ctrl Pts',(-51.3546038077785,-82.4603928963994,
60.4905549578654));
#206794=CARTESIAN_POINT('Ctrl Pts',(-51.3706491520746,-82.9784744867673,
60.4561563234838));
#206795=CARTESIAN_POINT('Ctrl Pts',(-51.4071574905776,-84.1411626825417,
60.4784519058709));
#206796=CARTESIAN_POINT('Ctrl Pts',(-51.4276977631762,-84.7825260302579,
60.5593340711432));
#206797=CARTESIAN_POINT('Ctrl Pts',(-51.465141603421,-85.9348060503362,
60.8312208899268));
#206798=CARTESIAN_POINT('Ctrl Pts',(-51.4818147229151,-86.4476390286903,
61.0015400989278));
#206799=CARTESIAN_POINT('Ctrl Pts',(-51.5074430548604,-87.1981167133596,
61.3273548868817));
#206800=CARTESIAN_POINT('Ctrl Pts',(-51.5162169552698,-87.4486437936567,
61.4501064345573));
#206801=CARTESIAN_POINT('Ctrl Pts',(-51.5439484223193,-88.2171101271034,
61.8715170606771));
#206802=CARTESIAN_POINT('Ctrl Pts',(-51.5629968860554,-88.711485320593,
62.2098310629754));
#206803=CARTESIAN_POINT('Ctrl Pts',(-51.5957845290705,-89.5144903712622,
62.884361891401));
#206804=CARTESIAN_POINT('Ctrl Pts',(-51.6097993152967,-89.8378284318547,
63.1998246909724));
#206805=CARTESIAN_POINT('Ctrl Pts',(-51.6458717535102,-90.5967266573389,
64.0593190861755));
#206806=CARTESIAN_POINT('Ctrl Pts',(-51.6681372105029,-90.9956956352514,
64.6317619870711));
#206807=CARTESIAN_POINT('Ctrl Pts',(-51.6997074378457,-91.4725125845283,
65.5170628329408));
#206808=CARTESIAN_POINT('Ctrl Pts',(-51.7093578146623,-91.6053893697283,
65.7972300373293));
#206809=CARTESIAN_POINT('Ctrl Pts',(-51.7190489450981,-91.723644464317,
66.0834535849086));
#206810=CARTESIAN_POINT('Ctrl Pts',(-51.9229031371334,-91.723644464317,
66.0834535849086));
#206811=CARTESIAN_POINT('Ctrl Pts',(-51.9106399629138,-91.5782329720614,
65.7315009412026));
#206812=CARTESIAN_POINT('Ctrl Pts',(-51.8983152146373,-91.4108065720598,
65.388931473677));
#206813=CARTESIAN_POINT('Ctrl Pts',(-51.8701233880306,-90.9746246996887,
64.6226343007356));
#206814=CARTESIAN_POINT('Ctrl Pts',(-51.8543741618664,-90.6913995856782,
64.2086873870961));
#206815=CARTESIAN_POINT('Ctrl Pts',(-51.8079342398151,-89.7727445766005,
63.0787512514185));
#206816=CARTESIAN_POINT('Ctrl Pts',(-51.7769543255324,-89.0568057887049,
62.4369932458205));
#206817=CARTESIAN_POINT('Ctrl Pts',(-51.7089989440773,-87.2593857639417,
61.276109628659));
#206818=CARTESIAN_POINT('Ctrl Pts',(-51.6707264611623,-86.148627410159,
60.8341728469488));
#206819=CARTESIAN_POINT('Ctrl Pts',(-51.6238049046546,-84.6963343560413,
60.5640814951426));
#206820=CARTESIAN_POINT('Ctrl Pts',(-51.6145142495458,-84.405832334073,
60.5244664165164));
#206821=CARTESIAN_POINT('Ctrl Pts',(-51.5884431318578,-83.5916651291978,
60.4532999788211));
#206822=CARTESIAN_POINT('Ctrl Pts',(-51.5715430527392,-83.0664361370525,
60.4529155628379));
#206823=CARTESIAN_POINT('Ctrl Pts',(-51.535308385102,-81.947820903818,60.5490408300095));
#206824=CARTESIAN_POINT('Ctrl Pts',(-51.5164050182772,-81.3580404309915,
60.6590471765668));
#206825=CARTESIAN_POINT('Ctrl Pts',(-51.4880282358771,-80.500116496568,
60.9086137543441));
#206826=CARTESIAN_POINT('Ctrl Pts',(-51.4786269281836,-80.2210511450564,
61.0047470400078));
#206827=CARTESIAN_POINT('Ctrl Pts',(-51.4523421667,-79.4599662404302,61.3091033972305));
#206828=CARTESIAN_POINT('Ctrl Pts',(-51.4353421259464,-78.9905602503028,
61.54574621155));
#206829=CARTESIAN_POINT('Ctrl Pts',(-51.4032381396794,-78.1343302965438,
62.0748110955611));
#206830=CARTESIAN_POINT('Ctrl Pts',(-51.3881229843155,-77.7452453340655,
62.360254081977));
#206831=CARTESIAN_POINT('Ctrl Pts',(-51.354982436646,-76.955189235919,63.0426378803104));
#206832=CARTESIAN_POINT('Ctrl Pts',(-51.3369374176284,-76.5647631745038,
63.4487599330444));
#206833=CARTESIAN_POINT('Ctrl Pts',(-51.2998470461721,-75.8440821528249,
64.3528310350224));
#206834=CARTESIAN_POINT('Ctrl Pts',(-51.2812367383216,-75.520226204611,
64.8525122607279));
#206835=CARTESIAN_POINT('Ctrl Pts',(-51.2531349279433,-75.1116241412943,
65.6429327668723));
#206836=CARTESIAN_POINT('Ctrl Pts',(-51.2437586862846,-74.9887139169713,
65.9121282087519));
#206837=CARTESIAN_POINT('Ctrl Pts',(-51.2165748688895,-74.6728940874802,
66.7039373935078));
#206838=CARTESIAN_POINT('Ctrl Pts',(-51.1986581480155,-74.5145816307207,
67.238900554646));
#206839=CARTESIAN_POINT('Ctrl Pts',(-51.1608150331806,-74.2811988780267,
68.4148645041512));
#206840=CARTESIAN_POINT('Ctrl Pts',(-51.1408235386528,-74.2232899091996,
69.0562266421446));
#206841=CARTESIAN_POINT('Ctrl Pts',(-51.1035004545141,-74.2418834701496,
70.2311850277702));
#206842=CARTESIAN_POINT('Ctrl Pts',(-51.0864006493592,-74.2971604917727,
70.7622769462743));
#206843=CARTESIAN_POINT('Ctrl Pts',(-51.0531588352697,-74.497848223116,
71.7968903224989));
#206844=CARTESIAN_POINT('Ctrl Pts',(-51.0369912006251,-74.6408351811626,
72.2988488558184));
#206845=CARTESIAN_POINT('Ctrl Pts',(-51.0045451824436,-75.007113482696,
73.2619375189264));
#206846=CARTESIAN_POINT('Ctrl Pts',(-50.9883338827073,-75.2279046094035,
73.7220174218051));
#206847=CARTESIAN_POINT('Ctrl Pts',(-50.9535162065867,-75.7831574417221,
74.6665453786056));
#206848=CARTESIAN_POINT('Ctrl Pts',(-50.9353159240416,-76.1284414515151,
75.1419974076811));
#206849=CARTESIAN_POINT('Ctrl Pts',(-50.9076553343251,-76.7142304625479,
75.8034975351984));
#206850=CARTESIAN_POINT('Ctrl Pts',(-50.8983092076004,-76.922168045955,
76.0163024970541));
#206851=CARTESIAN_POINT('Ctrl Pts',(-50.8724112326359,-77.5224592529502,
76.5731916946453));
#206852=CARTESIAN_POINT('Ctrl Pts',(-50.8557516463148,-77.9345705998867,
76.8942970631852));
#206853=CARTESIAN_POINT('Ctrl Pts',(-50.8237908919568,-78.7877050486375,
77.4482720631052));
#206854=CARTESIAN_POINT('Ctrl Pts',(-50.8084473301634,-79.2248670555909,
77.6837866951273));
#206855=CARTESIAN_POINT('Ctrl Pts',(-50.7771862969671,-80.137596815985,
78.0830881309289));
#206856=CARTESIAN_POINT('Ctrl Pts',(-50.7613140591261,-80.6119298540795,
78.2454785681636));
#206857=CARTESIAN_POINT('Ctrl Pts',(-50.7268304996241,-81.6650034234414,
78.5113515181957));
#206858=CARTESIAN_POINT('Ctrl Pts',(-50.7086164197141,-82.2453277591109,
78.5995013127753));
#206859=CARTESIAN_POINT('Ctrl Pts',(-50.6715587960687,-83.4286575002796,
78.6636813055427));
#206860=CARTESIAN_POINT('Ctrl Pts',(-50.6526148129697,-84.0289673562377,
78.636856509736));
#206861=CARTESIAN_POINT('Ctrl Pts',(-50.5958211608329,-85.7965787181752,
78.3814666021691));
#206862=CARTESIAN_POINT('Ctrl Pts',(-50.5594309811275,-86.9264079236248,
77.9834964909913));
#206863=CARTESIAN_POINT('Ctrl Pts',(-50.4835875375019,-88.9745054927381,
76.7728785011232));
#206864=CARTESIAN_POINT('Ctrl Pts',(-50.4469037372857,-89.8717786780052,
75.9698648153537));
#206865=CARTESIAN_POINT('Ctrl Pts',(-50.3993945748335,-90.7645684248745,
74.7822158909312));
#206866=CARTESIAN_POINT('Ctrl Pts',(-50.3900079168931,-90.9292958464928,
74.5394794443228));
#206867=CARTESIAN_POINT('Ctrl Pts',(-50.3646250050068,-91.346276569298,
73.8560988857613));
#206868=CARTESIAN_POINT('Ctrl Pts',(-50.3487970710957,-91.5738238983745,
73.4016233069964));
#206869=CARTESIAN_POINT('Ctrl Pts',(-50.3040285835809,-92.0990337173014,
72.0886371055357));
#206870=CARTESIAN_POINT('Ctrl Pts',(-50.2747816579962,-92.3079433485688,
71.2010642612718));
#206871=CARTESIAN_POINT('Ctrl Pts',(-50.2278832161795,-92.4292882696803,
69.7211517899185));
#206872=CARTESIAN_POINT('Ctrl Pts',(-50.2096316899784,-92.4214578548965,
69.1417799494627));
#206873=CARTESIAN_POINT('Ctrl Pts',(-50.1733173469438,-92.2985382661797,
68.01686814027));
#206874=CARTESIAN_POINT('Ctrl Pts',(-50.1554343546318,-92.1882849888544,
67.4732789761947));
#206875=CARTESIAN_POINT('Ctrl Pts',(-50.1282000266549,-91.9417963729096,
66.6514363404576));
#206876=CARTESIAN_POINT('Ctrl Pts',(-50.1185905671141,-91.8397738343069,
66.3645320481434));
#206877=CARTESIAN_POINT('Ctrl Pts',(-50.1089321285242,-91.723644464317,
66.0834535849087));
#206878=CARTESIAN_POINT('Origin',(-61.5936228798467,-83.3229197588524,69.5524554490053));
#206879=CARTESIAN_POINT('',(-62.602329162019,-91.7241837160256,66.0814193573896));
#206880=CARTESIAN_POINT('',(-62.8075051404766,-91.7241532646522,66.0813456540805));
#206881=CARTESIAN_POINT('',(-61.5936228798467,-91.7241837160232,66.0814193573838));
#206882=CARTESIAN_POINT('',(-62.6023317437084,-91.724214653637,66.0814942394464));
#206883=CARTESIAN_POINT('Ctrl Pts',(-62.602329162019,-91.724183716028,66.0814193573955));
#206884=CARTESIAN_POINT('Ctrl Pts',(-62.6023301287422,-91.7241953008589,
66.0814473972141));
#206885=CARTESIAN_POINT('Ctrl Pts',(-62.6023307769843,-91.7242030690519,
66.0814661995147));
#206886=CARTESIAN_POINT('Ctrl Pts',(-62.6023317437084,-91.724214653637,
66.0814942394464));
#206887=CARTESIAN_POINT('',(-62.7290132089978,-92.4053664431831,69.9232336695063));
#206888=CARTESIAN_POINT('Ctrl Pts',(-62.7269877844547,-92.4054200988458,
69.9232858703778));
#206889=CARTESIAN_POINT('Ctrl Pts',(-62.7059767167849,-92.4321833496604,
69.2677915511049));
#206890=CARTESIAN_POINT('Ctrl Pts',(-62.6852394928937,-92.3879069276803,
68.6113136984254));
#206891=CARTESIAN_POINT('Ctrl Pts',(-62.6544240531954,-92.2165542002343,
67.6449849877673));
#206892=CARTESIAN_POINT('Ctrl Pts',(-62.6442290356213,-92.1425921867259,
67.3279207418242));
#206893=CARTESIAN_POINT('Ctrl Pts',(-62.6234162513844,-91.959643018198,
66.6984486864254));
#206894=CARTESIAN_POINT('Ctrl Pts',(-62.6128525065425,-91.8502885457368,
66.3866500398474));
#206895=CARTESIAN_POINT('Ctrl Pts',(-62.6023317437084,-91.724214653637,
66.0814942394464));
#206896=CARTESIAN_POINT('',(-62.9304638037219,-92.4054950025943,69.9232129291766));
#206897=CARTESIAN_POINT('',(-62.9299583493521,-92.4054226835952,69.9232225584337));
#206898=CARTESIAN_POINT('Ctrl Pts',(-62.9325038108326,-92.4054252108019,
69.9231606454937));
#206899=CARTESIAN_POINT('Ctrl Pts',(-62.9116762546274,-92.4324227266438,
69.2617048926575));
#206900=CARTESIAN_POINT('Ctrl Pts',(-62.8907033964332,-92.3870813596432,
68.5992795630952));
#206901=CARTESIAN_POINT('Ctrl Pts',(-62.8591164531908,-92.2133065594351,
67.630413397562));
#206902=CARTESIAN_POINT('Ctrl Pts',(-62.8487672428674,-92.1395668305264,
67.3163960992237));
#206903=CARTESIAN_POINT('Ctrl Pts',(-62.8281485913344,-91.9576684801071,
66.6928186370739));
#206904=CARTESIAN_POINT('Ctrl Pts',(-62.8178556351414,-91.8491373548634,
66.3838560001025));
#206905=CARTESIAN_POINT('Ctrl Pts',(-62.8075076622656,-91.7241837160232,
66.0814193573838));
#206906=CARTESIAN_POINT('Origin',(-61.5936228798467,-83.3229197588524,69.5524554490053));
#206907=CARTESIAN_POINT('',(-60.9932785231031,-91.7241837160232,66.0814193573838));
#206908=CARTESIAN_POINT('Ctrl Pts',(-62.8075051404766,-91.7241532646522,
66.0813456540805));
#206909=CARTESIAN_POINT('Ctrl Pts',(-62.782639448844,-91.4238893610732,
65.3546077182715));
#206910=CARTESIAN_POINT('Ctrl Pts',(-62.7573419230597,-91.030597562824,
64.6699048574091));
#206911=CARTESIAN_POINT('Ctrl Pts',(-62.707148163105,-90.0815230164625,
63.4239178672618));
#206912=CARTESIAN_POINT('Ctrl Pts',(-62.6828210378518,-89.5310041730699,
62.8668453774156));
#206913=CARTESIAN_POINT('Ctrl Pts',(-62.6414672514383,-88.5157511700844,
62.0743644731427));
#206914=CARTESIAN_POINT('Ctrl Pts',(-62.6249856508974,-88.0898489339138,
61.7959273286443));
#206915=CARTESIAN_POINT('Ctrl Pts',(-62.5930729332684,-87.2118569051275,
61.3216881943479));
#206916=CARTESIAN_POINT('Ctrl Pts',(-62.5776490581675,-86.7626672683054,
61.1240805190056));
#206917=CARTESIAN_POINT('Ctrl Pts',(-62.5525262949722,-86.0184966553697,
60.8661561273298));
#206918=CARTESIAN_POINT('Ctrl Pts',(-62.5429812228712,-85.7326311968053,
60.7825512578548));
#206919=CARTESIAN_POINT('Ctrl Pts',(-62.514502824905,-84.8736473974892,
60.5765095750246));
#206920=CARTESIAN_POINT('Ctrl Pts',(-62.4955585715648,-84.2922326355718,
60.4952589399396));
#206921=CARTESIAN_POINT('Ctrl Pts',(-62.4614485891902,-83.2202967080181,
60.4499200231851));
#206922=CARTESIAN_POINT('Ctrl Pts',(-62.4460230671324,-82.7326752762972,
60.4684975069705));
#206923=CARTESIAN_POINT('Ctrl Pts',(-62.4159521898034,-81.8022927836982,
60.5792006119913));
#206924=CARTESIAN_POINT('Ctrl Pts',(-62.4013844885234,-81.3602465161134,
60.6654132792302));
#206925=CARTESIAN_POINT('Ctrl Pts',(-62.3687077150992,-80.3823426440256,
60.9326845723041));
#206926=CARTESIAN_POINT('Ctrl Pts',(-62.3509474293283,-79.8533019520944,
61.1316955046727));
#206927=CARTESIAN_POINT('Ctrl Pts',(-62.3111515418468,-78.7293331677781,
61.6785259783383));
#206928=CARTESIAN_POINT('Ctrl Pts',(-62.2889855702203,-78.1484885668729,
62.0474542048791));
#206929=CARTESIAN_POINT('Ctrl Pts',(-62.2490753870823,-77.182021724831,
62.8272944155795));
#206930=CARTESIAN_POINT('Ctrl Pts',(-62.2316233663111,-76.7822923162096,
63.2153729809014));
#206931=CARTESIAN_POINT('Ctrl Pts',(-62.1957585642899,-76.048300806116,
64.0719012677919));
#206932=CARTESIAN_POINT('Ctrl Pts',(-62.177365850264,-75.7179090234939,
64.5404343917883));
#206933=CARTESIAN_POINT('Ctrl Pts',(-62.1407644355438,-75.1524904511458,
65.5282806228294));
#206934=CARTESIAN_POINT('Ctrl Pts',(-62.1229501544509,-74.9177564980146,
66.044873170331));
#206935=CARTESIAN_POINT('Ctrl Pts',(-62.0821006216508,-74.4954880525488,
67.2651918735177));
#206936=CARTESIAN_POINT('Ctrl Pts',(-62.0588399413442,-74.3412146325176,
67.9763609271869));
#206937=CARTESIAN_POINT('Ctrl Pts',(-62.0175905436349,-74.219958136856,
69.2610146368297));
#206938=CARTESIAN_POINT('Ctrl Pts',(-61.9999561766462,-74.2194478550678,
69.8274997616061));
#206939=CARTESIAN_POINT('Ctrl Pts',(-61.9727822537456,-74.2987586045137,
70.6842487011262));
#206940=CARTESIAN_POINT('Ctrl Pts',(-61.9634197903071,-74.3402621771479,
70.9766399771102));
#206941=CARTESIAN_POINT('Ctrl Pts',(-61.9350310385132,-74.5081192292594,
71.8508693468088));
#206942=CARTESIAN_POINT('Ctrl Pts',(-61.9159586366291,-74.677435589082,
72.4228274415055));
#206943=CARTESIAN_POINT('Ctrl Pts',(-61.8816411707454,-75.0884653984842,
73.4344627389694));
#206944=CARTESIAN_POINT('Ctrl Pts',(-61.8661243319853,-75.3129300365894,
73.8786874224392));
#206945=CARTESIAN_POINT('Ctrl Pts',(-61.8333740462486,-75.8534949558486,
74.7607237962095));
#206946=CARTESIAN_POINT('Ctrl Pts',(-61.8161579512294,-76.174532531962,
75.1932816556839));
#206947=CARTESIAN_POINT('Ctrl Pts',(-61.7822899692345,-76.885707966164,
75.9925579573077));
#206948=CARTESIAN_POINT('Ctrl Pts',(-61.7658024137524,-77.2737523608574,
76.3583494761944));
#206949=CARTESIAN_POINT('Ctrl Pts',(-61.7312727699392,-78.1366834708223,
77.0393646593839));
#206950=CARTESIAN_POINT('Ctrl Pts',(-61.713251789691,-78.6136932122976,
77.3482254816014));
#206951=CARTESIAN_POINT('Ctrl Pts',(-61.6772194918282,-79.6195922361186,
77.8733303829382));
#206952=CARTESIAN_POINT('Ctrl Pts',(-61.6595957716167,-80.1463361428618,
78.0883159448589));
#206953=CARTESIAN_POINT('Ctrl Pts',(-61.6237499877836,-81.2430951837849,
78.4202610611445));
#206954=CARTESIAN_POINT('Ctrl Pts',(-61.6054788586489,-81.8112227988724,
78.5345713663026));
#206955=CARTESIAN_POINT('Ctrl Pts',(-61.5495117122661,-83.5640688092825,
78.7161396148171));
#206956=CARTESIAN_POINT('Ctrl Pts',(-61.5132885942868,-84.7543668476728,
78.6068584711006));
#206957=CARTESIAN_POINT('Ctrl Pts',(-61.4439831094195,-86.8469514488567,
77.9907762249617));
#206958=CARTESIAN_POINT('Ctrl Pts',(-61.4133547643517,-87.7508638221166,
77.5535417050547));
#206959=CARTESIAN_POINT('Ctrl Pts',(-61.3725015184426,-88.8045667084337,
76.8096187940016));
#206960=CARTESIAN_POINT('Ctrl Pts',(-61.3631898701075,-89.0352192104166,
76.6294962908981));
#206961=CARTESIAN_POINT('Ctrl Pts',(-61.325135092192,-89.9415011458404,
75.8485398749232));
#206962=CARTESIAN_POINT('Ctrl Pts',(-61.2973272281126,-90.534398211703,
75.1596723383531));
#206963=CARTESIAN_POINT('Ctrl Pts',(-61.2495837013446,-91.3360001075092,
73.8861586684715));
#206964=CARTESIAN_POINT('Ctrl Pts',(-61.2303030811977,-91.6048968722122,
73.3470971633472));
#206965=CARTESIAN_POINT('Ctrl Pts',(-61.1925280821862,-92.031693432208,
72.2255569035656));
#206966=CARTESIAN_POINT('Ctrl Pts',(-61.1738414881785,-92.1888891937034,
71.6459682266556));
#206967=CARTESIAN_POINT('Ctrl Pts',(-61.1385650468259,-92.3722129896584,
70.5522622043069));
#206968=CARTESIAN_POINT('Ctrl Pts',(-61.1221597451864,-92.4140419477611,
70.0431837816635));
#206969=CARTESIAN_POINT('Ctrl Pts',(-61.096633182848,-92.4123489599951,
69.2400668706237));
#206970=CARTESIAN_POINT('Ctrl Pts',(-61.0874154894787,-92.3975428500331,
68.9470408089246));
#206971=CARTESIAN_POINT('Ctrl Pts',(-61.0501135215415,-92.2806775642666,
67.7688067151902));
#206972=CARTESIAN_POINT('Ctrl Pts',(-61.0216496146652,-92.0630968100072,
66.9017215051989));
#206973=CARTESIAN_POINT('Ctrl Pts',(-60.993278523103,-91.7241837160232,
66.0814193573839));
#206974=CARTESIAN_POINT('',(-60.7885639123434,-91.7241837160232,66.0814193573838));
#206975=CARTESIAN_POINT('',(-61.5936228798467,-91.7241837160232,66.0814193573838));
#206976=CARTESIAN_POINT('Ctrl Pts',(-60.7885639123434,-91.7241837160232,
66.0814193573838));
#206977=CARTESIAN_POINT('Ctrl Pts',(-60.8168982940386,-92.0672888336512,
66.9118678408229));
#206978=CARTESIAN_POINT('Ctrl Pts',(-60.8449183666358,-92.2859925617974,
67.7901443518347));
#206979=CARTESIAN_POINT('Ctrl Pts',(-60.8831526417602,-92.3996991184818,
68.9800704653405));
#206980=CARTESIAN_POINT('Ctrl Pts',(-60.8925524312737,-92.4134513972595,
69.2735559243787));
#206981=CARTESIAN_POINT('Ctrl Pts',(-60.9174368238779,-92.412178260678,
70.0588365261411));
#206982=CARTESIAN_POINT('Ctrl Pts',(-60.932787483143,-92.3714961568602,
70.5496070916347));
#206983=CARTESIAN_POINT('Ctrl Pts',(-60.9772216077173,-92.1426559184543,
71.9342410667884));
#206984=CARTESIAN_POINT('Ctrl Pts',(-61.0066354455244,-91.859482771096,
72.8063366536296));
#206985=CARTESIAN_POINT('Ctrl Pts',(-61.0537067591269,-91.192463652668,
74.1387394063432));
#206986=CARTESIAN_POINT('Ctrl Pts',(-61.0719689223178,-90.8848502493925,
74.6299470984856));
#206987=CARTESIAN_POINT('Ctrl Pts',(-61.1084338963099,-90.1929855909006,
75.5309673059974));
#206988=CARTESIAN_POINT('Ctrl Pts',(-61.126453524327,-89.8133021587206,
75.9411452521602));
#206989=CARTESIAN_POINT('Ctrl Pts',(-61.1633331215782,-88.949042409027,
76.7177232860578));
#206990=CARTESIAN_POINT('Ctrl Pts',(-61.1823779849551,-88.4605252890634,
77.0757078145086));
#206991=CARTESIAN_POINT('Ctrl Pts',(-61.2177278849416,-87.5125851856134,
77.6346813099218));
#206992=CARTESIAN_POINT('Ctrl Pts',(-61.2338320906311,-87.065121092545,
77.8513468946674));
#206993=CARTESIAN_POINT('Ctrl Pts',(-61.2656591486748,-86.1374434006063,
78.210175460382));
#206994=CARTESIAN_POINT('Ctrl Pts',(-61.2813449294374,-85.6586735055382,
78.3514280757492));
#206995=CARTESIAN_POINT('Ctrl Pts',(-61.3282500250971,-84.2192145915512,
78.650280335433));
#206996=CARTESIAN_POINT('Ctrl Pts',(-61.3597500356822,-83.2421341316582,
78.6939673325073));
#206997=CARTESIAN_POINT('Ctrl Pts',(-61.4282604264901,-81.0994589239397,
78.4457233733748));
#206998=CARTESIAN_POINT('Ctrl Pts',(-61.4665642768093,-79.9601101687614,
78.0803809269989));
#206999=CARTESIAN_POINT('Ctrl Pts',(-61.522559094674,-78.4165826313906,
77.2265761144129));
#207000=CARTESIAN_POINT('Ctrl Pts',(-61.5409287851939,-77.9380660966484,
76.8987208995993));
#207001=CARTESIAN_POINT('Ctrl Pts',(-61.5778530834986,-77.0582196363352,
76.1634578159226));
#207002=CARTESIAN_POINT('Ctrl Pts',(-61.596197134465,-76.6575364845791,
75.7592663609613));
#207003=CARTESIAN_POINT('Ctrl Pts',(-61.6322253585681,-75.9369036013822,
74.8814793368301));
#207004=CARTESIAN_POINT('Ctrl Pts',(-61.6501362005052,-75.6185290195753,
74.4098303908081));
#207005=CARTESIAN_POINT('Ctrl Pts',(-61.685821083523,-75.0845934510683,
73.4327905100171));
#207006=CARTESIAN_POINT('Ctrl Pts',(-61.7034793284167,-74.8665827823663,
72.9314187521735));
#207007=CARTESIAN_POINT('Ctrl Pts',(-61.73766044682,-74.5279868859487,71.9103238811904));
#207008=CARTESIAN_POINT('Ctrl Pts',(-61.7542661143291,-74.4054643287565,
71.3934826317876));
#207009=CARTESIAN_POINT('Ctrl Pts',(-61.7870276962639,-74.2562332221558,
70.3739160308934));
#207010=CARTESIAN_POINT('Ctrl Pts',(-61.8030966748672,-74.224769053084,
69.8737800427072));
#207011=CARTESIAN_POINT('Ctrl Pts',(-61.8522336467114,-74.2549710778356,
68.339027595969));
#207012=CARTESIAN_POINT('Ctrl Pts',(-61.8841769905295,-74.4518406136614,
67.3154811640129));
#207013=CARTESIAN_POINT('Ctrl Pts',(-61.9266147416522,-74.920079758707,
66.0728677985675));
#207014=CARTESIAN_POINT('Ctrl Pts',(-61.9359959635896,-75.0366477392345,
65.8037293725427));
#207015=CARTESIAN_POINT('Ctrl Pts',(-61.961424997767,-75.3904247045107,
65.084413189159));
#207016=CARTESIAN_POINT('Ctrl Pts',(-61.9772286572875,-75.6527247350318,
64.6477646308985));
#207017=CARTESIAN_POINT('Ctrl Pts',(-62.0115532880872,-76.2906467555519,
63.7632151083716));
#207018=CARTESIAN_POINT('Ctrl Pts',(-62.030089516706,-76.6757007497917,
63.3248849222721));
#207019=CARTESIAN_POINT('Ctrl Pts',(-62.0672816227846,-77.5277871877005,
62.5246413934834));
#207020=CARTESIAN_POINT('Ctrl Pts',(-62.0855140631312,-77.9934688737491,
62.1652578218559));
#207021=CARTESIAN_POINT('Ctrl Pts',(-62.1132208604885,-78.7421310016436,
61.6953605940876));
#207022=CARTESIAN_POINT('Ctrl Pts',(-62.1225699390672,-79.0013151489718,
61.5498747991622));
#207023=CARTESIAN_POINT('Ctrl Pts',(-62.1490053150776,-79.7484642844835,
61.1773832461642));
#207024=CARTESIAN_POINT('Ctrl Pts',(-62.1661982830379,-80.2501233601518,
60.9806122286629));
#207025=CARTESIAN_POINT('Ctrl Pts',(-62.2023613358389,-81.3556147788107,
60.656599334447));
#207026=CARTESIAN_POINT('Ctrl Pts',(-62.2213588160481,-81.9609934442741,
60.5440312316192));
#207027=CARTESIAN_POINT('Ctrl Pts',(-62.255885581863,-83.0515275727582,
60.4537659964282));
#207028=CARTESIAN_POINT('Ctrl Pts',(-62.2711863732942,-83.5323530737995,
60.452129250671));
#207029=CARTESIAN_POINT('Ctrl Pts',(-62.3077598618603,-84.6857142422267,
60.5396914991162));
#207030=CARTESIAN_POINT('Ctrl Pts',(-62.3285833453382,-85.3525521243088,
60.6660772370334));
#207031=CARTESIAN_POINT('Ctrl Pts',(-62.3643327853757,-86.4378214880229,
61.0004153008872));
#207032=CARTESIAN_POINT('Ctrl Pts',(-62.3789269779372,-86.8656055716723,
61.1685795365253));
#207033=CARTESIAN_POINT('Ctrl Pts',(-62.4281880966457,-88.2631528070393,
61.8441065846855));
#207034=CARTESIAN_POINT('Ctrl Pts',(-62.4616915558082,-89.1535935708666,
62.4935761900372));
#207035=CARTESIAN_POINT('Ctrl Pts',(-62.505365522961,-90.0996337652386,
63.4875327634942));
#207036=CARTESIAN_POINT('Ctrl Pts',(-62.5142515770287,-90.2825476536875,
63.6983354789032));
#207037=CARTESIAN_POINT('Ctrl Pts',(-62.5495766311797,-90.9763664269183,
64.5765062365734));
#207038=CARTESIAN_POINT('Ctrl Pts',(-62.5755554219838,-91.4033377225375,
65.3048466540976));
#207039=CARTESIAN_POINT('Ctrl Pts',(-62.602329162019,-91.724183716028,66.0814193573955));
#207040=CARTESIAN_POINT('Origin',(-61.5936228798467,-83.3229197588524,69.5524554490053));
#207041=CARTESIAN_POINT('',(-58.9742739887231,-91.7241837277703,66.0814193858164));
#207042=CARTESIAN_POINT('',(-59.1795703763519,-91.724183709737,66.0814193421689));
#207043=CARTESIAN_POINT('',(-61.5936228798467,-91.7241837160232,66.0814193573838));
#207044=CARTESIAN_POINT('Ctrl Pts',(-58.9742739877562,-91.7241837277819,
66.0814193858445));
#207045=CARTESIAN_POINT('Ctrl Pts',(-58.9908808498526,-91.9257346557453,
66.5692514101137));
#207046=CARTESIAN_POINT('Ctrl Pts',(-59.0076733421077,-92.0844500731938,
67.0738026638248));
#207047=CARTESIAN_POINT('Ctrl Pts',(-59.0627053178923,-92.4564321249842,
68.7556131068187));
#207048=CARTESIAN_POINT('Ctrl Pts',(-59.0995452584485,-92.4820027230901,
69.9613478729627));
#207049=CARTESIAN_POINT('Ctrl Pts',(-59.1763294497039,-92.0644174996969,
72.3194970018555));
#207050=CARTESIAN_POINT('Ctrl Pts',(-59.2134839228635,-91.6230232950485,
73.4484250669953));
#207051=CARTESIAN_POINT('Ctrl Pts',(-59.2798185920197,-90.5099699736407,
75.1843447045194));
#207052=CARTESIAN_POINT('Ctrl Pts',(-59.306794647372,-89.9440543097349,
75.8399395522327));
#207053=CARTESIAN_POINT('Ctrl Pts',(-59.3564437320649,-88.7716315751605,
76.8614591888738));
#207054=CARTESIAN_POINT('Ctrl Pts',(-59.3789666017369,-88.19851752829,77.2556070377854));
#207055=CARTESIAN_POINT('Ctrl Pts',(-59.4103427162114,-87.3288255032696,
77.717439476316));
#207056=CARTESIAN_POINT('Ctrl Pts',(-59.4195600296134,-87.0650332141483,
77.8416552162396));
#207057=CARTESIAN_POINT('Ctrl Pts',(-59.4475024480258,-86.2518958119344,
78.1778092999195));
#207058=CARTESIAN_POINT('Ctrl Pts',(-59.4663513373701,-85.6875172834469,
78.3492898145992));
#207059=CARTESIAN_POINT('Ctrl Pts',(-59.4949052382847,-84.8210363152403,
78.5230831823793));
#207060=CARTESIAN_POINT('Ctrl Pts',(-59.5044493027401,-84.5288673025814,
78.5670108106814));
#207061=CARTESIAN_POINT('Ctrl Pts',(-59.5293097555489,-83.7554968885733,
78.6450096573948));
#207062=CARTESIAN_POINT('Ctrl Pts',(-59.5445018264202,-83.2728265380557,
78.6551561549891));
#207063=CARTESIAN_POINT('Ctrl Pts',(-59.5914450836271,-81.804689052566,
78.5692008948062));
#207064=CARTESIAN_POINT('Ctrl Pts',(-59.6234634814916,-80.8337513441777,
78.3507943668341));
#207065=CARTESIAN_POINT('Ctrl Pts',(-59.6925162025095,-78.8173947877068,
77.5359692864206));
#207066=CARTESIAN_POINT('Ctrl Pts',(-59.7308228499329,-77.8152015027179,
76.8805721756744));
#207067=CARTESIAN_POINT('Ctrl Pts',(-59.7868686029272,-76.5512780269444,
75.644469479372));
#207068=CARTESIAN_POINT('Ctrl Pts',(-59.8053313153152,-76.175373566138,
75.1987234472925));
#207069=CARTESIAN_POINT('Ctrl Pts',(-59.8423698013046,-75.5208578315081,
74.2515572404954));
#207070=CARTESIAN_POINT('Ctrl Pts',(-59.8607019474952,-75.2418141424838,
73.753583441467));
#207071=CARTESIAN_POINT('Ctrl Pts',(-59.8968475291039,-74.7793631392255,
72.7091753358789));
#207072=CARTESIAN_POINT('Ctrl Pts',(-59.9148988032172,-74.5975143782169,
72.1648370032571));
#207073=CARTESIAN_POINT('Ctrl Pts',(-59.9513262035449,-74.3403231442999,
71.0563865840875));
#207074=CARTESIAN_POINT('Ctrl Pts',(-59.9695581868124,-74.2641988474479,
70.4950264196888));
#207075=CARTESIAN_POINT('Ctrl Pts',(-59.9998818133706,-74.224344760623,
69.5369023379722));
#207076=CARTESIAN_POINT('Ctrl Pts',(-60.0122259831535,-74.2335529429989,
69.1429180003753));
#207077=CARTESIAN_POINT('Ctrl Pts',(-60.0426641604663,-74.3184251587381,
68.1843228824391));
#207078=CARTESIAN_POINT('Ctrl Pts',(-60.060855089267,-74.4216222036621,
67.6238288611412));
#207079=CARTESIAN_POINT('Ctrl Pts',(-60.0978940207412,-74.7373164118713,
66.5085492889639));
#207080=CARTESIAN_POINT('Ctrl Pts',(-60.1163146125923,-74.9530998485078,
65.9574494391708));
#207081=CARTESIAN_POINT('Ctrl Pts',(-60.1442198768137,-75.3551635481451,
65.1670227820366));
#207082=CARTESIAN_POINT('Ctrl Pts',(-60.1535820856437,-75.5023665671669,
64.9096002063616));
#207083=CARTESIAN_POINT('Ctrl Pts',(-60.1806193446042,-75.9603345015432,
64.192498313495));
#207084=CARTESIAN_POINT('Ctrl Pts',(-60.1984003506664,-76.300928257504,
63.7534514050396));
#207085=CARTESIAN_POINT('Ctrl Pts',(-60.2365623844928,-77.1290347265396,
62.8667173025896));
#207086=CARTESIAN_POINT('Ctrl Pts',(-60.2570033883428,-77.6296757264703,
62.4355541959524));
#207087=CARTESIAN_POINT('Ctrl Pts',(-60.2949589766168,-78.6167558613648,
61.7568137992786));
#207088=CARTESIAN_POINT('Ctrl Pts',(-60.3122068434638,-79.0873098862241,
61.4914614798484));
#207089=CARTESIAN_POINT('Ctrl Pts',(-60.3480980487767,-80.1284570197993,
61.0208166362793));
#207090=CARTESIAN_POINT('Ctrl Pts',(-60.3667716031957,-80.7017004728976,
60.8276249116441));
#207091=CARTESIAN_POINT('Ctrl Pts',(-60.4009777322731,-81.7584940110668,
60.5851205443442));
#207092=CARTESIAN_POINT('Ctrl Pts',(-60.4163005490733,-82.2349326014184,
60.5149335199254));
#207093=CARTESIAN_POINT('Ctrl Pts',(-60.4544002950272,-83.4363346628987,
60.4343638274107));
#207094=CARTESIAN_POINT('Ctrl Pts',(-60.4766346105869,-84.1611907855992,
60.4722703326291));
#207095=CARTESIAN_POINT('Ctrl Pts',(-60.5140715722796,-85.3315789469087,
60.6749332528192));
#207096=CARTESIAN_POINT('Ctrl Pts',(-60.5288590170102,-85.7825443673847,
60.7891596011839));
#207097=CARTESIAN_POINT('Ctrl Pts',(-60.5624892309632,-86.788494743557,
61.1277659142991));
#207098=CARTESIAN_POINT('Ctrl Pts',(-60.5809396243979,-87.334063076315,
61.373437511639));
#207099=CARTESIAN_POINT('Ctrl Pts',(-60.6160219879483,-88.3040433443999,
61.9307745522433));
#207100=CARTESIAN_POINT('Ctrl Pts',(-60.63256472669,-88.7332559569293,62.2292140725272));
#207101=CARTESIAN_POINT('Ctrl Pts',(-60.6868217004815,-90.0451762610977,
63.320015613818));
#207102=CARTESIAN_POINT('Ctrl Pts',(-60.7231579565889,-90.7991641832008,
64.2479484416805));
#207103=CARTESIAN_POINT('Ctrl Pts',(-60.7701879850551,-91.4900992769741,
65.5510848102547));
#207104=CARTESIAN_POINT('Ctrl Pts',(-60.7794317860479,-91.6136014806138,
65.8137671278693));
#207105=CARTESIAN_POINT('Ctrl Pts',(-60.7885639123434,-91.7241837160232,
66.0814193573838));
#207106=CARTESIAN_POINT('Ctrl Pts',(-60.9932785231031,-91.7241837160232,
66.0814193573838));
#207107=CARTESIAN_POINT('Ctrl Pts',(-60.9836585589429,-91.609266325186,
65.8032743573871));
#207108=CARTESIAN_POINT('Ctrl Pts',(-60.9741358332696,-91.4803992918137,
65.5305050330448));
#207109=CARTESIAN_POINT('Ctrl Pts',(-60.9270802992573,-90.7781059031341,
64.2178840124118));
#207110=CARTESIAN_POINT('Ctrl Pts',(-60.8888532890121,-90.018802447874,
63.2912571558181));
#207111=CARTESIAN_POINT('Ctrl Pts',(-60.8322357517563,-88.6403280280915,
62.1555791049752));
#207112=CARTESIAN_POINT('Ctrl Pts',(-60.8132185571498,-88.1411463147246,
61.8211363998287));
#207113=CARTESIAN_POINT('Ctrl Pts',(-60.7750249259248,-87.0963265378314,
61.2618727704026));
#207114=CARTESIAN_POINT('Ctrl Pts',(-60.7561225370917,-86.5544443622508,
61.0360228755365));
#207115=CARTESIAN_POINT('Ctrl Pts',(-60.7218376982587,-85.5228478084517,
60.7188124525034));
#207116=CARTESIAN_POINT('Ctrl Pts',(-60.7062001797163,-85.0400554744152,
60.6124121799593));
#207117=CARTESIAN_POINT('Ctrl Pts',(-60.6738110596239,-84.0410208393284,
60.476189995232));
#207118=CARTESIAN_POINT('Ctrl Pts',(-60.6570942186559,-83.5260382871465,
60.4500930059206));
#207119=CARTESIAN_POINT('Ctrl Pts',(-60.6240319181291,-82.4963631963837,
60.485375516262));
#207120=CARTESIAN_POINT('Ctrl Pts',(-60.607805525829,-81.9835353091829,
60.5468356453021));
#207121=CARTESIAN_POINT('Ctrl Pts',(-60.5818679147074,-81.1874236998583,
60.7117845706479));
#207122=CARTESIAN_POINT('Ctrl Pts',(-60.572331013593,-80.8992978184601,
60.7863924901967));
#207123=CARTESIAN_POINT('Ctrl Pts',(-60.5438463993114,-80.0556438168937,
61.0496319669537));
#207124=CARTESIAN_POINT('Ctrl Pts',(-60.5248819043189,-79.5141369426373,
61.2780195740827));
#207125=CARTESIAN_POINT('Ctrl Pts',(-60.4896608844245,-78.5388903663837,
61.805500198871));
#207126=CARTESIAN_POINT('Ctrl Pts',(-60.4731466910582,-78.1016574196566,
62.0931880403867));
#207127=CARTESIAN_POINT('Ctrl Pts',(-60.4428068374976,-77.3590790196944,
62.6792229000049));
#207128=CARTESIAN_POINT('Ctrl Pts',(-60.4291140884938,-77.0453418691813,
62.9645320115567));
#207129=CARTESIAN_POINT('Ctrl Pts',(-60.3973440712632,-76.3625499688621,
63.6786809142309));
#207130=CARTESIAN_POINT('Ctrl Pts',(-60.3796211692993,-76.0113096533257,
64.1221391847533));
#207131=CARTESIAN_POINT('Ctrl Pts',(-60.3401220321253,-75.332753475204,
65.1651220201054));
#207132=CARTESIAN_POINT('Ctrl Pts',(-60.3182288784822,-75.0271241498172,
65.7747303146124));
#207133=CARTESIAN_POINT('Ctrl Pts',(-60.2784676608396,-74.5982230652185,
66.9400288655615));
#207134=CARTESIAN_POINT('Ctrl Pts',(-60.2609024862143,-74.4534436343785,
67.4842435611604));
#207135=CARTESIAN_POINT('Ctrl Pts',(-60.2222462640891,-74.2500905920886,
68.6880250243619));
#207136=CARTESIAN_POINT('Ctrl Pts',(-60.2010843280752,-74.2113042729708,
69.3477242652848));
#207137=CARTESIAN_POINT('Ctrl Pts',(-60.1621998069781,-74.2720875747106,
70.5650207586457));
#207138=CARTESIAN_POINT('Ctrl Pts',(-60.1447617133219,-74.3516232954627,
71.1204776505044));
#207139=CARTESIAN_POINT('Ctrl Pts',(-60.1091224794885,-74.6141256441802,
72.2190288625099));
#207140=CARTESIAN_POINT('Ctrl Pts',(-60.0909495045359,-74.7982626855029,
72.7593104905246));
#207141=CARTESIAN_POINT('Ctrl Pts',(-60.0546575572412,-75.2646446818146,
73.7970213248205));
#207142=CARTESIAN_POINT('Ctrl Pts',(-60.0369334088695,-75.5456277540114,
74.2922729755054));
#207143=CARTESIAN_POINT('Ctrl Pts',(-60.0008984975686,-76.2031526972008,
75.2335343312809));
#207144=CARTESIAN_POINT('Ctrl Pts',(-59.9825249930449,-76.5800517774161,
75.67613568403));
#207145=CARTESIAN_POINT('Ctrl Pts',(-59.926268923334,-77.8486967939239,
76.9057230471662));
#207146=CARTESIAN_POINT('Ctrl Pts',(-59.88990758121,-78.8544070034193,77.5568326873641));
#207147=CARTESIAN_POINT('Ctrl Pts',(-59.8225565777777,-80.8228582751085,
78.3415586035183));
#207148=CARTESIAN_POINT('Ctrl Pts',(-59.7938700528801,-81.7369363317453,
78.5515283314669));
#207149=CARTESIAN_POINT('Ctrl Pts',(-59.7478086174076,-83.1932161265221,
78.656903910119));
#207150=CARTESIAN_POINT('Ctrl Pts',(-59.7309667738328,-83.7218631284607,
78.6490835953509));
#207151=CARTESIAN_POINT('Ctrl Pts',(-59.7050208595486,-84.5403896371845,
78.5654554400883));
#207152=CARTESIAN_POINT('Ctrl Pts',(-59.6958264696521,-84.8323098346971,
78.5211869299153));
#207153=CARTESIAN_POINT('Ctrl Pts',(-59.6682566882164,-85.6983688636324,
78.346364362918));
#207154=CARTESIAN_POINT('Ctrl Pts',(-59.6498248806209,-86.262504943039,
78.1741966346491));
#207155=CARTESIAN_POINT('Ctrl Pts',(-59.6218885903569,-87.075242244736,
77.8370407378287));
#207156=CARTESIAN_POINT('Ctrl Pts',(-59.61260781306,-87.3389308468233,77.7124758292482));
#207157=CARTESIAN_POINT('Ctrl Pts',(-59.581961560223,-88.1937331512077,
77.2571860473787));
#207158=CARTESIAN_POINT('Ctrl Pts',(-59.5610948666435,-88.7538620560443,
76.8731497224859));
#207159=CARTESIAN_POINT('Ctrl Pts',(-59.512533068949,-89.9186687394956,
75.8666562474787));
#207160=CARTESIAN_POINT('Ctrl Pts',(-59.4850147781052,-90.4876529920233,
75.2128126897288));
#207161=CARTESIAN_POINT('Ctrl Pts',(-59.4204113195225,-91.6076307263067,
73.4809461880866));
#207162=CARTESIAN_POINT('Ctrl Pts',(-59.3821093262288,-92.0533420830907,
72.3540966318594));
#207163=CARTESIAN_POINT('Ctrl Pts',(-59.3068946430571,-92.4800760647086,
69.9991812669454));
#207164=CARTESIAN_POINT('Ctrl Pts',(-59.2686837525913,-92.4595902367898,
68.7946120083655));
#207165=CARTESIAN_POINT('Ctrl Pts',(-59.2139666988862,-92.0924482424603,
67.0993407838807));
#207166=CARTESIAN_POINT('Ctrl Pts',(-59.1969005346458,-91.9308425416561,
66.5816144831256));
#207167=CARTESIAN_POINT('Ctrl Pts',(-59.1795703768785,-91.7241837097306,
66.0814193421533));
#207168=CARTESIAN_POINT('Origin',(-61.5936228798467,-83.3229197588524,69.5524554490053));
#207169=CARTESIAN_POINT('',(-57.1603612091034,-91.7241837160232,66.0814193573838));
#207170=CARTESIAN_POINT('',(-57.3654750299524,-91.7241837160232,66.0814193573838));
#207171=CARTESIAN_POINT('',(-61.5936228798467,-91.7241837160232,66.0814193573838));
#207172=CARTESIAN_POINT('Ctrl Pts',(-57.1603612091034,-91.7241837160232,
66.0814193573838));
#207173=CARTESIAN_POINT('Ctrl Pts',(-57.1643075550946,-91.7714348510752,
66.1957855717848));
#207174=CARTESIAN_POINT('Ctrl Pts',(-57.1682592739096,-91.8163636829924,
66.3111480666542));
#207175=CARTESIAN_POINT('Ctrl Pts',(-57.201192711216,-92.1711758057006,
67.2803207234912));
#207176=CARTESIAN_POINT('Ctrl Pts',(-57.2292447649847,-92.3538340628692,
68.1752032550547));
#207177=CARTESIAN_POINT('Ctrl Pts',(-57.2738634620999,-92.4263624913974,
69.5754015843189));
#207178=CARTESIAN_POINT('Ctrl Pts',(-57.2897494762442,-92.4116774206205,
70.0698297406882));
#207179=CARTESIAN_POINT('Ctrl Pts',(-57.3148029097305,-92.3243440725679,
70.8524170008992));
#207180=CARTESIAN_POINT('Ctrl Pts',(-57.3240386954911,-92.2776603112734,
71.1424750414258));
#207181=CARTESIAN_POINT('Ctrl Pts',(-57.3708522755525,-91.9708346583543,
72.5961177973874));
#207182=CARTESIAN_POINT('Ctrl Pts',(-57.4091414904654,-91.4976074282449,
73.7027303808055));
#207183=CARTESIAN_POINT('Ctrl Pts',(-57.4842609382672,-90.1556475234844,
75.6635087704191));
#207184=CARTESIAN_POINT('Ctrl Pts',(-57.5224045134595,-89.3024498332601,
76.5005747389649));
#207185=CARTESIAN_POINT('Ctrl Pts',(-57.5764701266048,-87.8772559016594,
77.4365450251894));
#207186=CARTESIAN_POINT('Ctrl Pts',(-57.5929747042321,-87.4179231028032,
77.6846008445442));
#207187=CARTESIAN_POINT('Ctrl Pts',(-57.6258046815346,-86.4808254539663,
78.0910343755753));
#207188=CARTESIAN_POINT('Ctrl Pts',(-57.6420496562794,-86.0061165722681,
78.2518895028104));
#207189=CARTESIAN_POINT('Ctrl Pts',(-57.6738803754007,-85.0410300778121,
78.4923480219708));
#207190=CARTESIAN_POINT('Ctrl Pts',(-57.689444972188,-84.552521939159,78.5725256397523));
#207191=CARTESIAN_POINT('Ctrl Pts',(-57.7147177339823,-83.7631994761432,
78.6367335376223));
#207192=CARTESIAN_POINT('Ctrl Pts',(-57.7242681745868,-83.4654719202352,
78.6462792625143));
#207193=CARTESIAN_POINT('Ctrl Pts',(-57.7527572734999,-82.582197358887,
78.6312057289093));
#207194=CARTESIAN_POINT('Ctrl Pts',(-57.7717005025127,-81.9989056263173,
78.564634914755));
#207195=CARTESIAN_POINT('Ctrl Pts',(-57.8063909285601,-80.9316833242889,
78.3369232520953));
#207196=CARTESIAN_POINT('Ctrl Pts',(-57.8223966429801,-80.4469472315054,
78.1903756694889));
#207197=CARTESIAN_POINT('Ctrl Pts',(-57.8551886855639,-79.4974135420679,
77.8144641304721));
#207198=CARTESIAN_POINT('Ctrl Pts',(-57.8719273494801,-79.0349383175548,
77.5841735694151));
#207199=CARTESIAN_POINT('Ctrl Pts',(-57.9053131805234,-78.1458942510517,
77.0426909799553));
#207200=CARTESIAN_POINT('Ctrl Pts',(-57.9218204048192,-77.7218183928645,
76.7310966467465));
#207201=CARTESIAN_POINT('Ctrl Pts',(-57.9480233051002,-77.1037071145463,
76.1886444468371));
#207202=CARTESIAN_POINT('Ctrl Pts',(-57.9575365520924,-76.8901308045856,
75.9818282628259));
#207203=CARTESIAN_POINT('Ctrl Pts',(-57.9860324136145,-76.2849042509406,
75.335355439972));
#207204=CARTESIAN_POINT('Ctrl Pts',(-58.0050161401071,-75.9253960484828,
74.8677404488049));
#207205=CARTESIAN_POINT('Ctrl Pts',(-58.0424643676744,-75.2991679759306,
73.8653373491247));
#207206=CARTESIAN_POINT('Ctrl Pts',(-58.0611869392659,-75.0347731329829,
73.332424320369));
#207207=CARTESIAN_POINT('Ctrl Pts',(-58.0994464373814,-74.6113738282244,
72.2166936412776));
#207208=CARTESIAN_POINT('Ctrl Pts',(-58.1187827973433,-74.4545756367208,
71.6361270713852));
#207209=CARTESIAN_POINT('Ctrl Pts',(-58.1539312084072,-74.2720434637819,
70.5390498261329));
#207210=CARTESIAN_POINT('Ctrl Pts',(-58.1700167669714,-74.2308340851803,
70.0275421600996));
#207211=CARTESIAN_POINT('Ctrl Pts',(-58.2025959350043,-74.2350161326039,
69.0045550257246));
#207212=CARTESIAN_POINT('Ctrl Pts',(-58.2190306716271,-74.2801456199829,
68.4949023500349));
#207213=CARTESIAN_POINT('Ctrl Pts',(-58.2526122598165,-74.4612172411427,
67.4559438035145));
#207214=CARTESIAN_POINT('Ctrl Pts',(-58.2695416633615,-74.6024966871704,
66.9296025601453));
#207215=CARTESIAN_POINT('Ctrl Pts',(-58.296026273235,-74.8917708654786,
66.1418450920097));
#207216=CARTESIAN_POINT('Ctrl Pts',(-58.3053899012604,-75.0070129209366,
65.8697626281372));
#207217=CARTESIAN_POINT('Ctrl Pts',(-58.3338234479444,-75.3946205761399,
65.0660544878458));
#207218=CARTESIAN_POINT('Ctrl Pts',(-58.3528949851174,-75.7062949711908,
64.5551796005247));
#207219=CARTESIAN_POINT('Ctrl Pts',(-58.3882935170328,-76.385959503553,
63.6541018030826));
#207220=CARTESIAN_POINT('Ctrl Pts',(-58.4048943856861,-76.7427391072376,
63.258552577647));
#207221=CARTESIAN_POINT('Ctrl Pts',(-58.4346675241699,-77.4307444764585,
62.6186240690943));
#207222=CARTESIAN_POINT('Ctrl Pts',(-58.4476894679638,-77.7478164010396,
62.3612130182685));
#207223=CARTESIAN_POINT('Ctrl Pts',(-58.4785830619273,-78.5430493842177,
61.7999155307737));
#207224=CARTESIAN_POINT('Ctrl Pts',(-58.4960997564441,-79.0344094502668,
61.517673738298));
#207225=CARTESIAN_POINT('Ctrl Pts',(-58.5227363605971,-79.8073762245133,
61.1649009892014));
#207226=CARTESIAN_POINT('Ctrl Pts',(-58.5316852592252,-80.0713441764505,
61.0590832791401));
#207227=CARTESIAN_POINT('Ctrl Pts',(-58.5499140211205,-80.6151976913719,
60.870143207617));
#207228=CARTESIAN_POINT('Ctrl Pts',(-58.5591861949119,-80.8950037782894,
60.7877804476541));
#207229=CARTESIAN_POINT('Ctrl Pts',(-58.586539844,-81.7320777528774,60.5845505790919));
#207230=CARTESIAN_POINT('Ctrl Pts',(-58.6042602292198,-82.2972917414937,
60.5024726813504));
#207231=CARTESIAN_POINT('Ctrl Pts',(-58.6402273616741,-83.4466785572209,
60.4446832682405));
#207232=CARTESIAN_POINT('Ctrl Pts',(-58.658555460935,-84.028352856961,60.4712010325149));
#207233=CARTESIAN_POINT('Ctrl Pts',(-58.7072359978959,-85.5457853012357,
60.6871252311085));
#207234=CARTESIAN_POINT('Ctrl Pts',(-58.7364641284295,-86.4611958779166,
60.9683745048571));
#207235=CARTESIAN_POINT('Ctrl Pts',(-58.7832132337006,-87.7898683092187,
61.6181193945942));
#207236=CARTESIAN_POINT('Ctrl Pts',(-58.8000677246322,-88.2424648842144,
61.8905109661702));
#207237=CARTESIAN_POINT('Ctrl Pts',(-58.8318378019263,-89.0585758868051,
62.4839532076096));
#207238=CARTESIAN_POINT('Ctrl Pts',(-58.8467750324505,-89.4251153555413,
62.7978504449456));
#207239=CARTESIAN_POINT('Ctrl Pts',(-58.8797498752602,-90.1657642790579,
63.5418471455463));
#207240=CARTESIAN_POINT('Ctrl Pts',(-58.8978198322272,-90.5278717659411,
63.9810474409389));
#207241=CARTESIAN_POINT('Ctrl Pts',(-58.9338810151096,-91.1638608214093,
64.919040118221));
#207242=CARTESIAN_POINT('Ctrl Pts',(-58.9514883722586,-91.436767839919,
65.4155040937725));
#207243=CARTESIAN_POINT('Ctrl Pts',(-58.9709199352701,-91.6830246161798,
65.9830269473587));
#207244=CARTESIAN_POINT('Ctrl Pts',(-58.9725963370137,-91.7038227431489,
66.0321378446976));
#207245=CARTESIAN_POINT('Ctrl Pts',(-58.9742739877562,-91.7241837277819,
66.0814193858445));
#207246=CARTESIAN_POINT('Ctrl Pts',(-59.1795703768785,-91.7241837097306,
66.0814193421533));
#207247=CARTESIAN_POINT('Ctrl Pts',(-59.1783553620991,-91.7096948898098,
66.0463507353326));
#207248=CARTESIAN_POINT('Ctrl Pts',(-59.1771393902312,-91.6949846120067,
66.0113682909168));
#207249=CARTESIAN_POINT('Ctrl Pts',(-59.1580018344277,-91.4601655241754,
65.4625917852046));
#207250=CARTESIAN_POINT('Ctrl Pts',(-59.1399701168292,-91.1933449814746,
64.9700791141866));
#207251=CARTESIAN_POINT('Ctrl Pts',(-59.1045759997665,-90.5733648370307,
64.0414382185356));
#207252=CARTESIAN_POINT('Ctrl Pts',(-59.0870138155532,-90.2217326564725,
63.6071511480886));
#207253=CARTESIAN_POINT('Ctrl Pts',(-59.0544365075591,-89.5121086859036,
62.8790740543585));
#207254=CARTESIAN_POINT('Ctrl Pts',(-59.039582980177,-89.1672431070907,
62.5750662830142));
#207255=CARTESIAN_POINT('Ctrl Pts',(-59.0012843085679,-88.2159243714361,
61.8566666686836));
#207256=CARTESIAN_POINT('Ctrl Pts',(-58.978371995284,-87.5796644716814,
61.4872967016084));
#207257=CARTESIAN_POINT('Ctrl Pts',(-58.9401170374322,-86.4836038562859,
61.0171976259968));
#207258=CARTESIAN_POINT('Ctrl Pts',(-58.9252306844584,-86.0480941308018,
60.8683337116299));
#207259=CARTESIAN_POINT('Ctrl Pts',(-58.8910256424108,-85.0202121023796,
60.6019676932172));
#207260=CARTESIAN_POINT('Ctrl Pts',(-58.8720962206822,-84.4236506082263,
60.5092024127063));
#207261=CARTESIAN_POINT('Ctrl Pts',(-58.8212772660278,-82.8338578869889,
60.4217304057643));
#207262=CARTESIAN_POINT('Ctrl Pts',(-58.7892143585532,-81.8431288331944,
60.5291775535275));
#207263=CARTESIAN_POINT('Ctrl Pts',(-58.7201202500558,-79.7466171406805,
61.1117228620778));
#207264=CARTESIAN_POINT('Ctrl Pts',(-58.6818139625381,-78.6770244949825,
61.6498248259125));
#207265=CARTESIAN_POINT('Ctrl Pts',(-58.6257691208861,-77.2819454248588,
62.7352552474275));
#207266=CARTESIAN_POINT('Ctrl Pts',(-58.6073090915348,-76.8582525937609,
63.1356291190726));
#207267=CARTESIAN_POINT('Ctrl Pts',(-58.5702707919224,-76.1011351515366,
64.0027244590353));
#207268=CARTESIAN_POINT('Ctrl Pts',(-58.5519348061948,-75.7676859893879,
64.4659884950895));
#207269=CARTESIAN_POINT('Ctrl Pts',(-58.5157889379326,-75.190422212679,
65.4513000243091));
#207270=CARTESIAN_POINT('Ctrl Pts',(-58.497741483714,-74.9483624597392,
65.9714250761848));
#207271=CARTESIAN_POINT('Ctrl Pts',(-58.4613134672743,-74.567679016852,
67.0435448969656));
#207272=CARTESIAN_POINT('Ctrl Pts',(-58.4430756291629,-74.4286308850337,
67.5927330918716));
#207273=CARTESIAN_POINT('Ctrl Pts',(-58.4010649321468,-74.2239027487931,
68.9050171394925));
#207274=CARTESIAN_POINT('Ctrl Pts',(-58.3771770643042,-74.2016623822086,
69.6705738966716));
#207275=CARTESIAN_POINT('Ctrl Pts',(-58.3434224302482,-74.3035131501736,
70.7208207861201));
#207276=CARTESIAN_POINT('Ctrl Pts',(-58.3340499251273,-74.345746037725,
71.0102364882732));
#207277=CARTESIAN_POINT('Ctrl Pts',(-58.3049108446301,-74.5213858130833,
71.9083465114184));
#207278=CARTESIAN_POINT('Ctrl Pts',(-58.2855881226413,-74.7034237654515,
72.5056765036959));
#207279=CARTESIAN_POINT('Ctrl Pts',(-58.2498238969358,-75.1426564471019,
73.5489337250016));
#207280=CARTESIAN_POINT('Ctrl Pts',(-58.2335687564081,-75.3792911537745,
74.0007476823246));
#207281=CARTESIAN_POINT('Ctrl Pts',(-58.1982641757421,-75.9740987793751,
74.9360718971259));
#207282=CARTESIAN_POINT('Ctrl Pts',(-58.1796408263271,-76.3449207690453,
75.4087366445883));
#207283=CARTESIAN_POINT('Ctrl Pts',(-58.151516698401,-76.9647666172548,
76.0556234234973));
#207284=CARTESIAN_POINT('Ctrl Pts',(-58.142166017743,-77.1803356554583,
76.2596131085063));
#207285=CARTESIAN_POINT('Ctrl Pts',(-58.1148962857639,-77.8331707004816,
76.8194639086075));
#207286=CARTESIAN_POINT('Ctrl Pts',(-58.0968869088407,-78.2940299198404,
77.1456785032234));
#207287=CARTESIAN_POINT('Ctrl Pts',(-58.066637450632,-79.1300272859004,
77.6277430013837));
#207288=CARTESIAN_POINT('Ctrl Pts',(-58.0541568621049,-79.4908505879974,
77.8050831100247));
#207289=CARTESIAN_POINT('Ctrl Pts',(-58.0244492458845,-80.3665371628115,
78.1656188149886));
#207290=CARTESIAN_POINT('Ctrl Pts',(-58.0071473291945,-80.8885205324986,
78.3274466919687));
#207291=CARTESIAN_POINT('Ctrl Pts',(-57.9712424764974,-81.9945996455441,
78.5640006805048));
#207292=CARTESIAN_POINT('Ctrl Pts',(-57.9530557583684,-82.5778544662228,
78.6308509025772));
#207293=CARTESIAN_POINT('Ctrl Pts',(-57.9254352831612,-83.4611402262249,
78.6463464595879));
#207294=CARTESIAN_POINT('Ctrl Pts',(-57.9160908551431,-83.7588790637174,
78.6369420233036));
#207295=CARTESIAN_POINT('Ctrl Pts',(-57.8911014063756,-84.54722380647,78.5731907277357));
#207296=CARTESIAN_POINT('Ctrl Pts',(-57.8753600356538,-85.0347775998973,
78.4934914589621));
#207297=CARTESIAN_POINT('Ctrl Pts',(-57.8438473079412,-86.0050026187064,
78.2525863985289));
#207298=CARTESIAN_POINT('Ctrl Pts',(-57.8281804590448,-86.4854956150931,
78.0896660951154));
#207299=CARTESIAN_POINT('Ctrl Pts',(-57.796090447364,-87.4237074244127,
77.6814070912102));
#207300=CARTESIAN_POINT('Ctrl Pts',(-57.7797091837313,-87.879057086696,
77.435216223302));
#207301=CARTESIAN_POINT('Ctrl Pts',(-57.7256290096773,-89.3009349475064,
76.5019029960134));
#207302=CARTESIAN_POINT('Ctrl Pts',(-57.6893062427029,-90.1544163486836,
75.6649122163779));
#207303=CARTESIAN_POINT('Ctrl Pts',(-57.6135547941334,-91.496853693898,
73.7042292352895));
#207304=CARTESIAN_POINT('Ctrl Pts',(-57.5768874335455,-91.9702984067784,
72.5976583239647));
#207305=CARTESIAN_POINT('Ctrl Pts',(-57.5293772120705,-92.2773810073057,
71.1440437792263));
#207306=CARTESIAN_POINT('Ctrl Pts',(-57.5199805450081,-92.3241136417869,
70.8540086098186));
#207307=CARTESIAN_POINT('Ctrl Pts',(-57.4950210105062,-92.411628831952,
70.0710582791185));
#207308=CARTESIAN_POINT('Ctrl Pts',(-57.4795946638747,-92.4263817599483,
69.5762355380885));
#207309=CARTESIAN_POINT('Ctrl Pts',(-57.4351904996613,-92.3538893553277,
68.1754221232929));
#207310=CARTESIAN_POINT('Ctrl Pts',(-57.4058892022752,-92.1711981468918,
67.2803188469568));
#207311=CARTESIAN_POINT('Ctrl Pts',(-57.3732874320217,-91.8163112081297,
66.3110133090398));
#207312=CARTESIAN_POINT('Ctrl Pts',(-57.3693826819263,-91.7714071541859,
66.1957185344876));
#207313=CARTESIAN_POINT('Ctrl Pts',(-57.3654750299524,-91.7241837160232,
66.0814193573838));
#207314=CARTESIAN_POINT('Origin',(-64.4265543961493,-83.3237128444373,69.5530424137804));
#207315=CARTESIAN_POINT('',(-64.4174334691588,-91.7227797420331,66.0829140514164));
#207316=CARTESIAN_POINT('',(-64.5675364832717,-91.7227797420325,66.082914051415));
#207317=CARTESIAN_POINT('',(-64.4265543961493,-91.7227797420325,66.082914051415));
#207318=CARTESIAN_POINT('',(-64.4174351716144,-91.722800105991,66.0829633405634));
#207319=CARTESIAN_POINT('Ctrl Pts',(-64.4174351716144,-91.722800105991,
66.0829633405634));
#207320=CARTESIAN_POINT('Ctrl Pts',(-64.4174346041292,-91.7227933180531,
66.0829469108273));
#207321=CARTESIAN_POINT('Ctrl Pts',(-64.417434036644,-91.7227865300673,
66.0829304811121));
#207322=CARTESIAN_POINT('Ctrl Pts',(-64.4174334691588,-91.7227797420337,
66.0829140514177));
#207323=CARTESIAN_POINT('',(-64.5666618780602,-92.3407155670729,70.6707464084894));
#207324=CARTESIAN_POINT('Ctrl Pts',(-64.5657843992066,-92.3423880036114,
70.6709037535128));
#207325=CARTESIAN_POINT('Ctrl Pts',(-64.5410292714247,-92.4385150622132,
69.895370434019));
#207326=CARTESIAN_POINT('Ctrl Pts',(-64.5157599537561,-92.4342089172065,
69.1106652271105));
#207327=CARTESIAN_POINT('Ctrl Pts',(-64.4664991786972,-92.2249846832541,
67.5621750022409));
#207328=CARTESIAN_POINT('Ctrl Pts',(-64.4423690633479,-92.0210452715925,
66.8048452107943));
#207329=CARTESIAN_POINT('Ctrl Pts',(-64.4174351716144,-91.722800105991,
66.0829633405634));
#207330=CARTESIAN_POINT('Origin',(-64.5675364832709,-83.3237128444373,69.5530424137804));
#207331=CARTESIAN_POINT('Origin',(-27.5423496375577,-74.9965420974961,72.9903965241317));
#207332=CARTESIAN_POINT('',(-30.7042591052869,-85.9391496438337,68.4693880411367));
#207333=CARTESIAN_POINT('',(-31.000413750398,-85.9391496391482,68.4693880297961));
#207334=CARTESIAN_POINT('',(-27.5423496375574,-85.9391496391482,68.4693880297962));
#207335=CARTESIAN_POINT('',(-32.4074704173708,-83.5021837654764,64.7498540653718));
#207336=CARTESIAN_POINT('Ctrl Pts',(-30.7042591049895,-85.9391496438364,
68.4693880411434));
#207337=CARTESIAN_POINT('Ctrl Pts',(-30.7071432045293,-85.9845654573861,
68.5793120605169));
#207338=CARTESIAN_POINT('Ctrl Pts',(-30.7100298765835,-86.0283279638993,
68.6899278133005));
#207339=CARTESIAN_POINT('Ctrl Pts',(-30.7314903820352,-86.3407926437295,
69.5159082856428));
#207340=CARTESIAN_POINT('Ctrl Pts',(-30.7502951478004,-86.5413372287112,
70.2551118645619));
#207341=CARTESIAN_POINT('Ctrl Pts',(-30.7880170308652,-86.8001841891141,
71.7796052353538));
#207342=CARTESIAN_POINT('Ctrl Pts',(-30.8067253105562,-86.85437986065,72.5618279359104));
#207343=CARTESIAN_POINT('Ctrl Pts',(-30.8440099841418,-86.8087314383416,
74.0910619682391));
#207344=CARTESIAN_POINT('Ctrl Pts',(-30.8623820857554,-86.7156689921332,
74.8346731455419));
#207345=CARTESIAN_POINT('Ctrl Pts',(-30.8896034539907,-86.4706684462532,
75.9346034566644));
#207346=CARTESIAN_POINT('Ctrl Pts',(-30.8987267060841,-86.3705077421378,
76.3005076268647));
#207347=CARTESIAN_POINT('Ctrl Pts',(-30.9264312686469,-86.0155656347624,
77.3889953031016));
#207348=CARTESIAN_POINT('Ctrl Pts',(-30.9452013262935,-85.7080997144869,
78.0922659739933));
#207349=CARTESIAN_POINT('Ctrl Pts',(-30.9827961460176,-84.9539398590874,
79.4434068326821));
#207350=CARTESIAN_POINT('Ctrl Pts',(-31.0014229555361,-84.5063398186325,
80.0865127085207));
#207351=CARTESIAN_POINT('Ctrl Pts',(-31.0385706158449,-83.5129783442073,
81.2493039530921));
#207352=CARTESIAN_POINT('Ctrl Pts',(-31.0568842446479,-82.9745504758854,
81.7705235161812));
#207353=CARTESIAN_POINT('Ctrl Pts',(-31.0840397115793,-82.0940878563685,
82.4745480719511));
#207354=CARTESIAN_POINT('Ctrl Pts',(-31.0931509110187,-81.7863701512867,
82.6972251189293));
#207355=CARTESIAN_POINT('Ctrl Pts',(-31.1208199817104,-80.8266619512405,
83.3237097366427));
#207356=CARTESIAN_POINT('Ctrl Pts',(-31.1395731345786,-80.1456699616022,
83.6793688182087));
#207357=CARTESIAN_POINT('Ctrl Pts',(-31.1771138492042,-78.7106922779752,
84.2596399069424));
#207358=CARTESIAN_POINT('Ctrl Pts',(-31.1957146935657,-77.9590595147694,
84.4801421190806));
#207359=CARTESIAN_POINT('Ctrl Pts',(-31.2328274046535,-76.4566786725149,
84.7635396778024));
#207360=CARTESIAN_POINT('Ctrl Pts',(-31.2511279433087,-75.7106803106599,
84.83222551326));
#207361=CARTESIAN_POINT('Ctrl Pts',(-31.2782920461113,-74.583085824835,
84.8290501767478));
#207362=CARTESIAN_POINT('Ctrl Pts',(-31.2874188282591,-74.2032428467766,
84.8096749532239));
#207363=CARTESIAN_POINT('Ctrl Pts',(-31.3151023748541,-73.0629186209356,
84.6962828941739));
#207364=CARTESIAN_POINT('Ctrl Pts',(-31.3338604399769,-72.3099991999214,
84.5467432309358));
#207365=CARTESIAN_POINT('Ctrl Pts',(-31.3714457980926,-70.8282886952565,
84.0997228727802));
#207366=CARTESIAN_POINT('Ctrl Pts',(-31.3900936106412,-70.1039676831453,
83.8003081359218));
#207367=CARTESIAN_POINT('Ctrl Pts',(-31.4272909824107,-68.7557241837118,
83.0795160541388));
#207368=CARTESIAN_POINT('Ctrl Pts',(-31.4456248131496,-68.1317858942723,
82.6657916817774));
#207369=CARTESIAN_POINT('Ctrl Pts',(-31.4728631723181,-67.2552269288479,
81.9568297101897));
#207370=CARTESIAN_POINT('Ctrl Pts',(-31.4820258659373,-66.9711566313225,
81.7034942829615));
#207371=CARTESIAN_POINT('Ctrl Pts',(-31.5097623070298,-66.1547977137663,
80.9016098999437));
#207372=CARTESIAN_POINT('Ctrl Pts',(-31.5285400473232,-65.6629099285718,
80.3148103292199));
#207373=CARTESIAN_POINT('Ctrl Pts',(-31.5691339998758,-64.7213617714676,
78.9413008663864));
#207374=CARTESIAN_POINT('Ctrl Pts',(-31.5907096984462,-64.2982909971383,
78.14209755223));
#207375=CARTESIAN_POINT('Ctrl Pts',(-31.6221007543298,-63.8317068315534,
76.9490340134588));
#207376=CARTESIAN_POINT('Ctrl Pts',(-31.6314437729075,-63.7105012176045,
76.5889570999271));
#207377=CARTESIAN_POINT('Ctrl Pts',(-31.6560197121624,-63.4364098802596,
75.6234286894173));
#207378=CARTESIAN_POINT('Ctrl Pts',(-31.671033899748,-63.3137297869777,
75.0106470624251));
#207379=CARTESIAN_POINT('Ctrl Pts',(-31.7047776140326,-63.1497607691003,
73.6343535167224));
#207380=CARTESIAN_POINT('Ctrl Pts',(-31.7235895909336,-63.1328760920988,
72.870715232101));
#207381=CARTESIAN_POINT('Ctrl Pts',(-31.7649870414119,-63.2584445617294,
71.1852285472259));
#207382=CARTESIAN_POINT('Ctrl Pts',(-31.7872985139579,-63.4359874023173,
70.2709946279799));
#207383=CARTESIAN_POINT('Ctrl Pts',(-31.8195010241203,-63.834104995451,
69.0249778555225));
#207384=CARTESIAN_POINT('Ctrl Pts',(-31.8288900534836,-63.9671030559063,
68.6688202399193));
#207385=CARTESIAN_POINT('Ctrl Pts',(-31.8646424176768,-64.5411922652769,
67.3315896995405));
#207386=CARTESIAN_POINT('Ctrl Pts',(-31.8905243214653,-65.0980260916543,
66.4058830810216));
#207387=CARTESIAN_POINT('Ctrl Pts',(-31.926533878651,-66.0122618544706,
65.2696696427136));
#207388=CARTESIAN_POINT('Ctrl Pts',(-31.9359982523297,-66.2667454965785,
64.9830518186356));
#207389=CARTESIAN_POINT('Ctrl Pts',(-31.9585712997858,-66.9120174586244,
64.3236960593822));
#207390=CARTESIAN_POINT('Ctrl Pts',(-31.971650016924,-67.3152732029544,
63.9643594386768));
#207391=CARTESIAN_POINT('Ctrl Pts',(-32.003365826438,-68.3383236131057,
63.1711085216078));
#207392=CARTESIAN_POINT('Ctrl Pts',(-32.022120836258,-68.9779125267418,
62.7665821034246));
#207393=CARTESIAN_POINT('Ctrl Pts',(-32.0616663025437,-70.4166592161241,
62.0386895278778));
#207394=CARTESIAN_POINT('Ctrl Pts',(-32.082393915655,-71.2214500334388,
61.7358906506367));
#207395=CARTESIAN_POINT('Ctrl Pts',(-32.1129240666703,-72.4200404170053,
61.4281167610066));
#207396=CARTESIAN_POINT('Ctrl Pts',(-32.1223373183744,-72.7925622453359,
61.3513610459618));
#207397=CARTESIAN_POINT('Ctrl Pts',(-32.1461140581556,-73.7462800711484,
61.2022903378908));
#207398=CARTESIAN_POINT('Ctrl Pts',(-32.1602847045135,-74.3303337149976,
61.1549087977211));
#207399=CARTESIAN_POINT('Ctrl Pts',(-32.1932425150503,-75.6787881761831,
61.1456775751533));
#207400=CARTESIAN_POINT('Ctrl Pts',(-32.2121296952263,-76.4408037420532,
61.2142799287779));
#207401=CARTESIAN_POINT('Ctrl Pts',(-32.2501673639803,-77.9602656117201,
61.5008568215757));
#207402=CARTESIAN_POINT('Ctrl Pts',(-32.2690290690518,-78.7133570885059,
61.7219242033699));
#207403=CARTESIAN_POINT('Ctrl Pts',(-32.3081937252706,-80.1928731399112,
62.3208321709841));
#207404=CARTESIAN_POINT('Ctrl Pts',(-32.3283181484142,-80.9132149042037,
62.7028091759389));
#207405=CARTESIAN_POINT('Ctrl Pts',(-32.3582225934137,-81.9343183651991,
63.3872432828824));
#207406=CARTESIAN_POINT('Ctrl Pts',(-32.368315847494,-82.2674785607088,
63.6369600267938));
#207407=CARTESIAN_POINT('Ctrl Pts',(-32.3886344788051,-82.9058716239084,
64.1702193176143));
#207408=CARTESIAN_POINT('Ctrl Pts',(-32.3988458781379,-83.2106814012253,
64.4533636048996));
#207409=CARTESIAN_POINT('Ctrl Pts',(-32.4090802221679,-83.4999635122087,
64.7519499557376));
#207410=CARTESIAN_POINT('',(-32.7070018384414,-83.5021837802876,64.7498540510208));
#207411=CARTESIAN_POINT('Origin',(-32.5572357904921,-87.0216635390508,61.3397527098387));
#207412=CARTESIAN_POINT('Ctrl Pts',(-32.7053886803439,-83.5000181996321,
64.7520064024586));
#207413=CARTESIAN_POINT('Ctrl Pts',(-32.6955235775403,-83.2159761503953,
64.4588247562857));
#207414=CARTESIAN_POINT('Ctrl Pts',(-32.6856518412961,-82.9169615816791,
64.180528821265));
#207415=CARTESIAN_POINT('Ctrl Pts',(-32.6657614829319,-82.29100434518,63.6556208137225));
#207416=CARTESIAN_POINT('Ctrl Pts',(-32.6557559698928,-81.9644490912632,
63.4094003432205));
#207417=CARTESIAN_POINT('Ctrl Pts',(-32.6262473116798,-80.9649493872972,
62.7339598779866));
#207418=CARTESIAN_POINT('Ctrl Pts',(-32.607154849764,-80.2606397788824,
62.355282177213));
#207419=CARTESIAN_POINT('Ctrl Pts',(-32.5688597261284,-78.7997606767584,
61.7507608422622));
#207420=CARTESIAN_POINT('Ctrl Pts',(-32.5496201108103,-78.0479541535455,
61.5238032313802));
#207421=CARTESIAN_POINT('Ctrl Pts',(-32.5122282763324,-76.5325989865272,
61.2260547705057));
#207422=CARTESIAN_POINT('Ctrl Pts',(-32.4940526186921,-75.773527879885,
61.1516674041786));
#207423=CARTESIAN_POINT('Ctrl Pts',(-32.4663243767396,-74.6331304636974,
61.1501222475673));
#207424=CARTESIAN_POINT('Ctrl Pts',(-32.457055363824,-74.2538716297711,
61.1678501491844));
#207425=CARTESIAN_POINT('Ctrl Pts',(-32.4296082716827,-73.1326137434058,
61.2744352894935));
#207426=CARTESIAN_POINT('Ctrl Pts',(-32.411791311583,-72.3974612467249,
61.4153044453678));
#207427=CARTESIAN_POINT('Ctrl Pts',(-32.374796683084,-70.9279543662837,
61.8440388478007));
#207428=CARTESIAN_POINT('Ctrl Pts',(-32.3555785938572,-70.1990824339427,
62.1377898829238));
#207429=CARTESIAN_POINT('Ctrl Pts',(-32.3274200720563,-69.1673891423799,
62.6779746001249));
#207430=CARTESIAN_POINT('Ctrl Pts',(-32.3182936882276,-68.8388796045901,
62.8706996944416));
#207431=CARTESIAN_POINT('Ctrl Pts',(-32.2876159549682,-67.7723110391946,
63.5676121662592));
#207432=CARTESIAN_POINT('Ctrl Pts',(-32.2657942501253,-67.082116790659,
64.1393949651531));
#207433=CARTESIAN_POINT('Ctrl Pts',(-32.2348495530599,-66.1980778729565,
65.0586200074079));
#207434=CARTESIAN_POINT('Ctrl Pts',(-32.2256816351913,-65.9468053524882,
65.3465547554137));
#207435=CARTESIAN_POINT('Ctrl Pts',(-32.1982389607735,-65.2397576912024,
66.2405999387672));
#207436=CARTESIAN_POINT('Ctrl Pts',(-32.1798483429023,-64.8277936767111,
66.8788386288624));
#207437=CARTESIAN_POINT('Ctrl Pts',(-32.1431185151747,-64.1366904307863,
68.2153197596488));
#207438=CARTESIAN_POINT('Ctrl Pts',(-32.1252230237423,-63.8572237084219,
68.909547941657));
#207439=CARTESIAN_POINT('Ctrl Pts',(-32.0875515299678,-63.4144500316063,
70.4032333095941));
#207440=CARTESIAN_POINT('Ctrl Pts',(-32.0676381394455,-63.2644413265768,
71.2026424779196));
#207441=CARTESIAN_POINT('Ctrl Pts',(-32.0294863562713,-63.1346017963956,
72.767003299345));
#207442=CARTESIAN_POINT('Ctrl Pts',(-32.011341711395,-63.1446488920153,
73.5272085810173));
#207443=CARTESIAN_POINT('Ctrl Pts',(-31.979994086474,-63.2848186274647,
74.8052249267449));
#207444=CARTESIAN_POINT('Ctrl Pts',(-31.9670359017254,-63.3772231735677,
75.3248116631135));
#207445=CARTESIAN_POINT('Ctrl Pts',(-31.9448400569064,-63.5957909022094,
76.2073889445845));
#207446=CARTESIAN_POINT('Ctrl Pts',(-31.9356130023789,-63.7055382814396,
76.5736075478546));
#207447=CARTESIAN_POINT('Ctrl Pts',(-31.9079011677942,-64.0869137846266,
77.6532568640312));
#207448=CARTESIAN_POINT('Ctrl Pts',(-31.889304744203,-64.4099659372064,
78.3463885023222));
#207449=CARTESIAN_POINT('Ctrl Pts',(-31.8522258789601,-65.1766905039656,
79.6468430874556));
#207450=CARTESIAN_POINT('Ctrl Pts',(-31.8341947001364,-65.6159391447516,
80.2527692827694));
#207451=CARTESIAN_POINT('Ctrl Pts',(-31.7954188454572,-66.6691730346643,
81.4493010415083));
#207452=CARTESIAN_POINT('Ctrl Pts',(-31.7744776665257,-67.2956839939467,
82.0233865657951));
#207453=CARTESIAN_POINT('Ctrl Pts',(-31.7350939690592,-68.593099193836,
82.9783528899875));
#207454=CARTESIAN_POINT('Ctrl Pts',(-31.7166927358616,-69.2504763472443,
83.3704778726981));
#207455=CARTESIAN_POINT('Ctrl Pts',(-31.6854023968601,-70.4027780984813,
83.9146022665282));
#207456=CARTESIAN_POINT('Ctrl Pts',(-31.6727694345795,-70.8781549672121,
84.1025441246547));
#207457=CARTESIAN_POINT('Ctrl Pts',(-31.6508516949256,-71.7274663599358,
84.3763095166132));
#207458=CARTESIAN_POINT('Ctrl Pts',(-31.6415772192522,-72.0962065035156,
84.4757752603689));
#207459=CARTESIAN_POINT('Ctrl Pts',(-31.6063238889962,-73.5105054038661,
84.7848089382225));
#207460=CARTESIAN_POINT('Ctrl Pts',(-31.5799383761504,-74.57788002886,84.8706817215814));
#207461=CARTESIAN_POINT('Ctrl Pts',(-31.5350170352657,-76.4108734893557,
84.7705654121244));
#207462=CARTESIAN_POINT('Ctrl Pts',(-31.5163791767883,-77.1735670391079,
84.6537270219544));
#207463=CARTESIAN_POINT('Ctrl Pts',(-31.4785596195015,-78.6606251574944,
84.2748805738338));
#207464=CARTESIAN_POINT('Ctrl Pts',(-31.4596683080806,-79.3817144600273,
84.0147041477492));
#207465=CARTESIAN_POINT('Ctrl Pts',(-31.4127643992252,-81.1193900753321,
83.1900685887214));
#207466=CARTESIAN_POINT('Ctrl Pts',(-31.3841098156622,-82.0875618085936,
82.5423602128335));
#207467=CARTESIAN_POINT('Ctrl Pts',(-31.3464639612025,-83.2281269792472,
81.5089614646173));
#207468=CARTESIAN_POINT('Ctrl Pts',(-31.3372185144437,-83.4976051329108,
81.2400550818893));
#207469=CARTESIAN_POINT('Ctrl Pts',(-31.3097513713876,-84.2546823859785,
80.4080249033765));
#207470=CARTESIAN_POINT('Ctrl Pts',(-31.2913800401256,-84.7026497717221,
79.8113813780443));
#207471=CARTESIAN_POINT('Ctrl Pts',(-31.2545593096663,-85.483193428776,
78.5376459511404));
#207472=CARTESIAN_POINT('Ctrl Pts',(-31.2364814300193,-85.8132163418888,
77.8629104229391));
#207473=CARTESIAN_POINT('Ctrl Pts',(-31.1990043821139,-86.3527121201128,
76.4297261704076));
#207474=CARTESIAN_POINT('Ctrl Pts',(-31.1796109525616,-86.5550121217493,
75.6724401148098));
#207475=CARTESIAN_POINT('Ctrl Pts',(-31.1512319426453,-86.7425971277642,
74.525085894939));
#207476=CARTESIAN_POINT('Ctrl Pts',(-31.1420081022768,-86.7858641947752,
74.1466688461417));
#207477=CARTESIAN_POINT('Ctrl Pts',(-31.1145807181722,-86.8597638973797,
73.0221985032259));
#207478=CARTESIAN_POINT('Ctrl Pts',(-31.0962362007859,-86.8381924195305,
72.274610871309));
#207479=CARTESIAN_POINT('Ctrl Pts',(-31.0595156209465,-86.6543553234396,
70.7914046819641));
#207480=CARTESIAN_POINT('Ctrl Pts',(-31.0415259441024,-86.4921070713351,
70.0591576044501));
#207481=CARTESIAN_POINT('Ctrl Pts',(-31.0156884375958,-86.1658214882129,
69.0502525285244));
#207482=CARTESIAN_POINT('Ctrl Pts',(-31.0080604245923,-86.0581626590963,
68.7574460529718));
#207483=CARTESIAN_POINT('Ctrl Pts',(-31.000413750398,-85.9391496391482,
68.4693880297961));
#207484=CARTESIAN_POINT('Origin',(-27.5423496375577,-74.9965420974961,72.9903965241317));
#207485=CARTESIAN_POINT('',(-28.8902889611216,-85.9391496391482,68.4693880297961));
#207486=CARTESIAN_POINT('',(-29.1863798856002,-85.9391496391482,68.4693880297961));
#207487=CARTESIAN_POINT('',(-27.5423496375574,-85.9391496391482,68.4693880297962));
#207488=CARTESIAN_POINT('Ctrl Pts',(-28.8902889611216,-85.9391496391482,
68.4693880297961));
#207489=CARTESIAN_POINT('Ctrl Pts',(-28.8995283211901,-86.0828659887593,
68.817237765775));
#207490=CARTESIAN_POINT('Ctrl Pts',(-28.9087847558972,-86.2099969740892,
69.1719428377128));
#207491=CARTESIAN_POINT('Ctrl Pts',(-28.9365166337169,-86.5427728456659,
70.2616199806556));
#207492=CARTESIAN_POINT('Ctrl Pts',(-28.9548136351524,-86.6945173551246,
71.0107379450507));
#207493=CARTESIAN_POINT('Ctrl Pts',(-28.9826977064045,-86.8122987634401,
72.1465922017969));
#207494=CARTESIAN_POINT('Ctrl Pts',(-28.9920030101979,-86.8332684586263,
72.5256173699335));
#207495=CARTESIAN_POINT('Ctrl Pts',(-29.0195714954137,-86.8413959006649,
73.652315710583));
#207496=CARTESIAN_POINT('Ctrl Pts',(-29.0374679912989,-86.7760169187804,
74.3984708422766));
#207497=CARTESIAN_POINT('Ctrl Pts',(-29.0745754429211,-86.4989551491749,
75.9038615842204));
#207498=CARTESIAN_POINT('Ctrl Pts',(-29.0938293857601,-86.2810628959108,
76.6582800598336));
#207499=CARTESIAN_POINT('Ctrl Pts',(-29.1312567660433,-85.7078102381637,
78.0921471338613));
#207500=CARTESIAN_POINT('Ctrl Pts',(-29.1494411374351,-85.3578996415665,
78.7697910615343));
#207501=CARTESIAN_POINT('Ctrl Pts',(-29.1834627613708,-84.5997096230225,
79.9449582163071));
#207502=CARTESIAN_POINT('Ctrl Pts',(-29.1990955263269,-84.2113052693821,
80.4519580931511));
#207503=CARTESIAN_POINT('Ctrl Pts',(-29.223663925763,-83.5292890863697,
81.2072584288094));
#207504=CARTESIAN_POINT('Ctrl Pts',(-29.2327815354917,-83.2611762405944,
81.4768807104254));
#207505=CARTESIAN_POINT('Ctrl Pts',(-29.2598230591689,-82.4330918413416,
82.2331011690959));
#207506=CARTESIAN_POINT('Ctrl Pts',(-29.2778991984299,-81.8398692406232,
82.6805318777052));
#207507=CARTESIAN_POINT('Ctrl Pts',(-29.3141450695314,-80.5721043557795,
83.4619063847497));
#207508=CARTESIAN_POINT('Ctrl Pts',(-29.3319583185975,-79.8997463284145,
83.7930814781586));
#207509=CARTESIAN_POINT('Ctrl Pts',(-29.3672593369409,-78.5355352643541,
84.311258612612));
#207510=CARTESIAN_POINT('Ctrl Pts',(-29.3846907415346,-77.8489968223934,
84.5034276010871));
#207511=CARTESIAN_POINT('Ctrl Pts',(-29.4197344489482,-76.4262357244761,
84.7665150256504));
#207512=CARTESIAN_POINT('Ctrl Pts',(-29.4372673189812,-75.6922061657539,
84.8325690467404));
#207513=CARTESIAN_POINT('Ctrl Pts',(-29.4732775397643,-74.2086489955821,
84.8275898494527));
#207514=CARTESIAN_POINT('Ctrl Pts',(-29.4916136494817,-73.4624104466234,
84.7541701221947));
#207515=CARTESIAN_POINT('Ctrl Pts',(-29.5187968234955,-72.3559276941455,
84.5381724100144));
#207516=CARTESIAN_POINT('Ctrl Pts',(-29.5279055210172,-71.9874554292504,
84.447681096201));
#207517=CARTESIAN_POINT('Ctrl Pts',(-29.5556043148239,-70.8887031839507,
84.1211728614577));
#207518=CARTESIAN_POINT('Ctrl Pts',(-29.5743943838771,-70.176419571956,
83.8317491779264));
#207519=CARTESIAN_POINT('Ctrl Pts',(-29.6166217713601,-68.6389933094776,
83.0253745443578));
#207520=CARTESIAN_POINT('Ctrl Pts',(-29.6397325088142,-67.8393284889846,
82.4716152789057));
#207521=CARTESIAN_POINT('Ctrl Pts',(-29.6727251199189,-66.83227203796,81.5734915450803));
#207522=CARTESIAN_POINT('Ctrl Pts',(-29.6820549697602,-66.5607898095081,
81.3068205885803));
#207523=CARTESIAN_POINT('Ctrl Pts',(-29.7135942094719,-65.6818272063981,
80.3560312107896));
#207524=CARTESIAN_POINT('Ctrl Pts',(-29.7354604200767,-65.1409273570892,
79.6148476331426));
#207525=CARTESIAN_POINT('Ctrl Pts',(-29.7671521443193,-64.5037619811568,
78.4882150363556));
#207526=CARTESIAN_POINT('Ctrl Pts',(-29.7764893851431,-64.3328021039724,
78.1487966704457));
#207527=CARTESIAN_POINT('Ctrl Pts',(-29.8140374973234,-63.7088234368817,
76.7458116307822));
#207528=CARTESIAN_POINT('Ctrl Pts',(-29.8417315397632,-63.3963174211873,
75.6267801525121));
#207529=CARTESIAN_POINT('Ctrl Pts',(-29.8890836023462,-63.1539811167698,
73.7163291010924));
#207530=CARTESIAN_POINT('Ctrl Pts',(-29.9076924443221,-63.131840415978,
72.9447162553307));
#207531=CARTESIAN_POINT('Ctrl Pts',(-29.9450550017397,-63.2372823510437,
71.4145964340451));
#207532=CARTESIAN_POINT('Ctrl Pts',(-29.9639085109905,-63.3633654104137,
70.6596194303905));
#207533=CARTESIAN_POINT('Ctrl Pts',(-30.0085207959319,-63.8343849018536,
68.9041877426353));
#207534=CARTESIAN_POINT('Ctrl Pts',(-30.0338703028542,-64.2421911750197,
67.9273150329408));
#207535=CARTESIAN_POINT('Ctrl Pts',(-30.0693099484831,-64.9667602581611,
66.6872345673202));
#207536=CARTESIAN_POINT('Ctrl Pts',(-30.0787578858061,-65.1755346487063,
66.3666370547101));
#207537=CARTESIAN_POINT('Ctrl Pts',(-30.1002166176163,-65.6890186467851,
65.6559118241576));
#207538=CARTESIAN_POINT('Ctrl Pts',(-30.1122017028276,-66.0034048638451,
65.2736521907534));
#207539=CARTESIAN_POINT('Ctrl Pts',(-30.1428913209674,-66.8597673107173,
64.3560645921094));
#207540=CARTESIAN_POINT('Ctrl Pts',(-30.1617406158681,-67.4311487764751,
63.8512717027624));
#207541=CARTESIAN_POINT('Ctrl Pts',(-30.1997217089976,-68.6816661592658,
62.94464768289));
#207542=CARTESIAN_POINT('Ctrl Pts',(-30.2186374492105,-69.3604796340118,
62.5486757851087));
#207543=CARTESIAN_POINT('Ctrl Pts',(-30.2562923496927,-70.7525956015514,
61.9121843293235));
#207544=CARTESIAN_POINT('Ctrl Pts',(-30.2748246328103,-71.4596214643,61.6666132054406));
#207545=CARTESIAN_POINT('Ctrl Pts',(-30.3023184544787,-72.5535867528755,
61.3991895158625));
#207546=CARTESIAN_POINT('Ctrl Pts',(-30.3115464992686,-72.9262373699216,
61.3268657950991));
#207547=CARTESIAN_POINT('Ctrl Pts',(-30.339443138637,-74.0548196951778,
61.163631644942));
#207548=CARTESIAN_POINT('Ctrl Pts',(-30.3583002721842,-74.8166679009763,
61.1275620744038));
#207549=CARTESIAN_POINT('Ctrl Pts',(-30.3962660247664,-76.3592346568466,
61.2032381620261));
#207550=CARTESIAN_POINT('Ctrl Pts',(-30.4151558405309,-77.1360426787338,
61.3192108467647));
#207551=CARTESIAN_POINT('Ctrl Pts',(-30.4527658357012,-78.6202333891019,
61.6940477278681));
#207552=CARTESIAN_POINT('Ctrl Pts',(-30.4712817497197,-79.3258368571948,
61.9452233127894));
#207553=CARTESIAN_POINT('Ctrl Pts',(-30.4987258026978,-80.346572414155,
62.4215242683615));
#207554=CARTESIAN_POINT('Ctrl Pts',(-30.5079261447506,-80.682203796793,
62.5982294610262));
#207555=CARTESIAN_POINT('Ctrl Pts',(-30.5357819144917,-81.6654910615277,
63.1778322987453));
#207556=CARTESIAN_POINT('Ctrl Pts',(-30.5546220355387,-82.2832805489083,
63.6274521458031));
#207557=CARTESIAN_POINT('Ctrl Pts',(-30.592489021526,-83.4391975601457,
64.6528521833681));
#207558=CARTESIAN_POINT('Ctrl Pts',(-30.6112994776759,-83.9718815960666,
65.229187676426));
#207559=CARTESIAN_POINT('Ctrl Pts',(-30.6487654182889,-84.8944066472866,
66.4504123203477));
#207560=CARTESIAN_POINT('Ctrl Pts',(-30.6672176269276,-85.2875297772593,
67.0883037849678));
#207561=CARTESIAN_POINT('Ctrl Pts',(-30.6916666439696,-85.7327469846333,
67.9922290522817));
#207562=CARTESIAN_POINT('Ctrl Pts',(-30.697956103958,-85.8398965092981,
68.2291566628825));
#207563=CARTESIAN_POINT('Ctrl Pts',(-30.7042591049895,-85.9391496438364,
68.4693880411434));
#207564=CARTESIAN_POINT('Ctrl Pts',(-31.000413750398,-85.9391496391482,
68.4693880297961));
#207565=CARTESIAN_POINT('Ctrl Pts',(-30.9894496914595,-85.7685047637428,
68.0563607366832));
#207566=CARTESIAN_POINT('Ctrl Pts',(-30.9784421937568,-85.5745171272631,
67.6530957880328));
#207567=CARTESIAN_POINT('Ctrl Pts',(-30.9489866478898,-84.9890409660733,
66.594169209003));
#207568=CARTESIAN_POINT('Ctrl Pts',(-30.9306856427922,-84.5564200349675,
65.9639821729572));
#207569=CARTESIAN_POINT('Ctrl Pts',(-30.9027964530365,-83.8223434458471,
65.0891727552971));
#207570=CARTESIAN_POINT('Ctrl Pts',(-30.8934900606079,-83.5646509049784,
64.8104443704195));
#207571=CARTESIAN_POINT('Ctrl Pts',(-30.8659179058485,-82.7609049498348,
64.0208156210601));
#207572=CARTESIAN_POINT('Ctrl Pts',(-30.8480189088652,-82.1793932751416,
63.5487143241095));
#207573=CARTESIAN_POINT('Ctrl Pts',(-30.8109072016306,-80.9052198210213,
62.7005335637446));
#207574=CARTESIAN_POINT('Ctrl Pts',(-30.7916515937246,-80.2117021199372,
62.332261004331));
#207575=CARTESIAN_POINT('Ctrl Pts',(-30.7542197255713,-78.7828348739039,
61.7465901526257));
#207576=CARTESIAN_POINT('Ctrl Pts',(-30.7360324761767,-78.0525681585849,
61.5265443642416));
#207577=CARTESIAN_POINT('Ctrl Pts',(-30.7082843972894,-76.933941270481,
61.3040471830111));
#207578=CARTESIAN_POINT('Ctrl Pts',(-30.6990064480223,-76.5582851223548,
61.2479421620343));
#207579=CARTESIAN_POINT('Ctrl Pts',(-30.6715352727106,-75.4373726781259,
61.1352798449406));
#207580=CARTESIAN_POINT('Ctrl Pts',(-30.6537045516274,-74.6887582132883,
61.1310797784556));
#207581=CARTESIAN_POINT('Ctrl Pts',(-30.616698716733,-73.1639679461412,
61.2670725895126));
#207582=CARTESIAN_POINT('Ctrl Pts',(-30.5974786207648,-72.3920292877713,
61.4140776340297));
#207583=CARTESIAN_POINT('Ctrl Pts',(-30.560137270925,-70.9114610705807,
61.8517288591366));
#207584=CARTESIAN_POINT('Ctrl Pts',(-30.5420056666565,-70.2050537507344,
62.1368510124088));
#207585=CARTESIAN_POINT('Ctrl Pts',(-30.5143121197003,-69.1938492896317,
62.66308946839));
#207586=CARTESIAN_POINT('Ctrl Pts',(-30.5050377464032,-68.865473614258,
62.8545929909763));
#207587=CARTESIAN_POINT('Ctrl Pts',(-30.4775977068192,-67.9209001963202,
63.4681772825442));
#207588=CARTESIAN_POINT('Ctrl Pts',(-30.4597881945804,-67.3347815885907,
63.9330903691818));
#207589=CARTESIAN_POINT('Ctrl Pts',(-30.422795492168,-66.2307352813139,
64.9931677445109));
#207590=CARTESIAN_POINT('Ctrl Pts',(-30.4035642681644,-65.7204745552141,
65.5910991910053));
#207591=CARTESIAN_POINT('Ctrl Pts',(-30.3661762005337,-64.839223198782,
66.8595510439525));
#207592=CARTESIAN_POINT('Ctrl Pts',(-30.3480147272345,-64.4665326441387,
67.5243833155983));
#207593=CARTESIAN_POINT('Ctrl Pts',(-30.3173044032287,-63.9580353402467,
68.6795630671376));
#207594=CARTESIAN_POINT('Ctrl Pts',(-30.3050081691236,-63.7852893419021,
69.1511613747627));
#207595=CARTESIAN_POINT('Ctrl Pts',(-30.2835062850145,-63.5345902378565,
69.9987605562438));
#207596=CARTESIAN_POINT('Ctrl Pts',(-30.2743102969878,-63.4440046693556,
70.3702618705647));
#207597=CARTESIAN_POINT('Ctrl Pts',(-30.2467410043588,-63.2273042486643,
71.4924223775198));
#207598=CARTESIAN_POINT('Ctrl Pts',(-30.2282552016501,-63.1553881146373,
72.251514331098));
#207599=CARTESIAN_POINT('Ctrl Pts',(-30.1913586400014,-63.1581686717972,
73.7590405717097));
#207600=CARTESIAN_POINT('Ctrl Pts',(-30.1733966847103,-63.2302014472502,
74.5040444931853));
#207601=CARTESIAN_POINT('Ctrl Pts',(-30.1353420038036,-63.5281125145034,
76.0453335219479));
#207602=CARTESIAN_POINT('Ctrl Pts',(-30.1150845932192,-63.7681252329433,
76.8348930486754));
#207603=CARTESIAN_POINT('Ctrl Pts',(-30.0857305276213,-64.236120142187,
77.9440350629426));
#207604=CARTESIAN_POINT('Ctrl Pts',(-30.0765347506166,-64.4010163055766,
78.2875702886592));
#207605=CARTESIAN_POINT('Ctrl Pts',(-30.0428586837917,-65.061971816687,
79.5097345229102));
#207606=CARTESIAN_POINT('Ctrl Pts',(-30.0179927316207,-65.6531656500806,
80.3319735496283));
#207607=CARTESIAN_POINT('Ctrl Pts',(-29.9841355838376,-66.6007529654551,
81.3471537236086));
#207608=CARTESIAN_POINT('Ctrl Pts',(-29.9749379466294,-66.8733574698408,
81.6123764882092));
#207609=CARTESIAN_POINT('Ctrl Pts',(-29.9427149566515,-67.8667577154263,
82.4898713783317));
#207610=CARTESIAN_POINT('Ctrl Pts',(-29.919341186383,-68.6476753332647,
83.0286095885551));
#207611=CARTESIAN_POINT('Ctrl Pts',(-29.8774996552032,-70.1627104857593,
83.8256098816011));
#207612=CARTESIAN_POINT('Ctrl Pts',(-29.8589967844682,-70.8741735942729,
84.11576661727));
#207613=CARTESIAN_POINT('Ctrl Pts',(-29.8308165594556,-71.9723342870696,
84.4437098691336));
#207614=CARTESIAN_POINT('Ctrl Pts',(-29.8214390084931,-72.341004740389,
84.5347605157055));
#207615=CARTESIAN_POINT('Ctrl Pts',(-29.793644439547,-73.44727190563,84.7521691218095));
#207616=CARTESIAN_POINT('Ctrl Pts',(-29.7755815110613,-74.1931497677014,
84.8265316423652));
#207617=CARTESIAN_POINT('Ctrl Pts',(-29.7391907940018,-75.6794620293426,
84.8334988644618));
#207618=CARTESIAN_POINT('Ctrl Pts',(-29.7208679422351,-76.4165826127964,
84.7678719069554));
#207619=CARTESIAN_POINT('Ctrl Pts',(-29.6850838483618,-77.8499336465015,
84.5036674362128));
#207620=CARTESIAN_POINT('Ctrl Pts',(-29.6677084140173,-78.5437558307006,
84.3091655361343));
#207621=CARTESIAN_POINT('Ctrl Pts',(-29.6316592996847,-79.9141711786744,
83.7865084938981));
#207622=CARTESIAN_POINT('Ctrl Pts',(-29.6130886579637,-80.5859096273871,
83.4545299006682));
#207623=CARTESIAN_POINT('Ctrl Pts',(-29.5766865576896,-81.8532708661213,
82.6711241673343));
#207624=CARTESIAN_POINT('Ctrl Pts',(-29.5586589112364,-82.446591262627,
82.2222968715369));
#207625=CARTESIAN_POINT('Ctrl Pts',(-29.5309788247761,-83.2742408827129,
81.4641411954743));
#207626=CARTESIAN_POINT('Ctrl Pts',(-29.5215695524635,-83.5419880701921,
81.1940541730913));
#207627=CARTESIAN_POINT('Ctrl Pts',(-29.497077497559,-84.2072318305858,
80.4550248991315));
#207628=CARTESIAN_POINT('Ctrl Pts',(-29.4822163965591,-84.5820327648268,
79.9672046446882));
#207629=CARTESIAN_POINT('Ctrl Pts',(-29.4485768052743,-85.3333166045812,
78.8138212269672));
#207630=CARTESIAN_POINT('Ctrl Pts',(-29.4297129690653,-85.6866920038498,
78.136449853645));
#207631=CARTESIAN_POINT('Ctrl Pts',(-29.3917545451188,-86.2661187543358,
76.7038891394555));
#207632=CARTESIAN_POINT('Ctrl Pts',(-29.3729028524161,-86.4869973251195,
75.9506039495689));
#207633=CARTESIAN_POINT('Ctrl Pts',(-29.3353572175053,-86.7702323688165,
74.4462388093395));
#207634=CARTESIAN_POINT('Ctrl Pts',(-29.3168550496728,-86.8386605925247,
73.699972782897));
#207635=CARTESIAN_POINT('Ctrl Pts',(-29.280503388481,-86.833846342415,72.2056509893591));
#207636=CARTESIAN_POINT('Ctrl Pts',(-29.2624303820932,-86.7608265292928,
71.4609495908793));
#207637=CARTESIAN_POINT('Ctrl Pts',(-29.2347456172494,-86.5454194912509,
70.3543832744611));
#207638=CARTESIAN_POINT('Ctrl Pts',(-29.2253655360832,-86.4546865015407,
69.9843922351259));
#207639=CARTESIAN_POINT('Ctrl Pts',(-29.2060769114763,-86.2303559646516,
69.229094147064));
#207640=CARTESIAN_POINT('Ctrl Pts',(-29.1962359460246,-86.0944395319839,
68.845250263768));
#207641=CARTESIAN_POINT('Ctrl Pts',(-29.1863798856002,-85.9391496391482,
68.4693880297961));
#207642=CARTESIAN_POINT('Origin',(-27.5423496375577,-74.9965420974961,72.9903965241317));
#207643=CARTESIAN_POINT('',(-27.0763524854127,-85.9391496391482,68.4693880297962));
#207644=CARTESIAN_POINT('',(-27.3723203523406,-85.9391496418573,68.4693880363532));
#207645=CARTESIAN_POINT('',(-27.5423496375574,-85.9391496391482,68.4693880297962));
#207646=CARTESIAN_POINT('Ctrl Pts',(-27.0763524854127,-85.9391496391482,
68.4693880297962));
#207647=CARTESIAN_POINT('Ctrl Pts',(-27.0854958243982,-86.0832420586906,
68.8181480019916));
#207648=CARTESIAN_POINT('Ctrl Pts',(-27.0946269738679,-86.2106594560495,
69.1737926277716));
#207649=CARTESIAN_POINT('Ctrl Pts',(-27.1228582600314,-86.5493155510614,
70.283709893587));
#207650=CARTESIAN_POINT('Ctrl Pts',(-27.1421585225472,-86.7029336633776,
71.053098990638));
#207651=CARTESIAN_POINT('Ctrl Pts',(-27.17041855609,-86.8167726463045,72.2110433942339));
#207652=CARTESIAN_POINT('Ctrl Pts',(-27.1795935858813,-86.8357252283469,
72.5916666797719));
#207653=CARTESIAN_POINT('Ctrl Pts',(-27.2077451655468,-86.8374804134635,
73.7554635391027));
#207654=CARTESIAN_POINT('Ctrl Pts',(-27.2268821242396,-86.7609998238509,
74.5365753507185));
#207655=CARTESIAN_POINT('Ctrl Pts',(-27.2642716278407,-86.4617074378826,
76.0384000127796));
#207656=CARTESIAN_POINT('Ctrl Pts',(-27.2821489972801,-86.2461607100747,
76.7568834329032));
#207657=CARTESIAN_POINT('Ctrl Pts',(-27.3152541188379,-85.7317463330596,
78.0219489283277));
#207658=CARTESIAN_POINT('Ctrl Pts',(-27.3303623796387,-85.4549018410693,
78.5746454022493));
#207659=CARTESIAN_POINT('Ctrl Pts',(-27.3636484640859,-84.7492010731034,
79.7452307442853));
#207660=CARTESIAN_POINT('Ctrl Pts',(-27.3815147552166,-84.3020647535182,
80.3490235437407));
#207661=CARTESIAN_POINT('Ctrl Pts',(-27.414094271405,-83.4029500332305,
81.3490243729791));
#207662=CARTESIAN_POINT('Ctrl Pts',(-27.42864906318,-82.9722483421988,81.7609414970286));
#207663=CARTESIAN_POINT('Ctrl Pts',(-27.4524654145557,-82.215525696821,
82.3826318433475));
#207664=CARTESIAN_POINT('Ctrl Pts',(-27.4617059544625,-81.9069456727931,
82.6119416897413));
#207665=CARTESIAN_POINT('Ctrl Pts',(-27.4975499411919,-80.6692153515452,
83.4414062209669));
#207666=CARTESIAN_POINT('Ctrl Pts',(-27.5245562214543,-79.6689475592958,
83.9252692475761));
#207667=CARTESIAN_POINT('Ctrl Pts',(-27.5604332604563,-78.2542686781622,
84.3795080463537));
#207668=CARTESIAN_POINT('Ctrl Pts',(-27.569546337496,-77.8869933492492,
84.4782133806877));
#207669=CARTESIAN_POINT('Ctrl Pts',(-27.5996011291581,-76.6680617310802,
84.743634102178));
#207670=CARTESIAN_POINT('Ctrl Pts',(-27.6208060446094,-75.8028037754163,
84.8344875628036));
#207671=CARTESIAN_POINT('Ctrl Pts',(-27.6601660945229,-74.1802254319195,
84.8261111357782));
#207672=CARTESIAN_POINT('Ctrl Pts',(-27.678163838067,-73.4271326307702,
84.7499659232919));
#207673=CARTESIAN_POINT('Ctrl Pts',(-27.7096512555339,-72.155460078534,
84.4969827358799));
#207674=CARTESIAN_POINT('Ctrl Pts',(-27.722910279037,-71.6323539700395,
84.3550570407994));
#207675=CARTESIAN_POINT('Ctrl Pts',(-27.7453913084619,-70.7591413854709,
84.0525441104013));
#207676=CARTESIAN_POINT('Ctrl Pts',(-27.7546006665861,-70.4037705024483,
83.9097886059322));
#207677=CARTESIAN_POINT('Ctrl Pts',(-27.782192090083,-69.3635283837108,
83.4321325338603));
#207678=CARTESIAN_POINT('Ctrl Pts',(-27.8006798026253,-68.7034257213282,
83.0480985277529));
#207679=CARTESIAN_POINT('Ctrl Pts',(-27.8375958582695,-67.4779572579048,
82.1669823762717));
#207680=CARTESIAN_POINT('Ctrl Pts',(-27.8555730354232,-66.9137755313285,
81.6741592142469));
#207681=CARTESIAN_POINT('Ctrl Pts',(-27.8943775210409,-65.8118876914272,
80.5105983339386));
#207682=CARTESIAN_POINT('Ctrl Pts',(-27.9154171071773,-65.2929316034503,
79.8278842459823));
#207683=CARTESIAN_POINT('Ctrl Pts',(-27.9547657332123,-64.4593718710948,
78.4427521309384));
#207684=CARTESIAN_POINT('Ctrl Pts',(-27.9730378279666,-64.1305677171517,
77.7538769334039));
#207685=CARTESIAN_POINT('Ctrl Pts',(-28.0009792322269,-63.7399154047799,
76.6800802198003));
#207686=CARTESIAN_POINT('Ctrl Pts',(-28.0103472509272,-63.6269930873546,
76.3158686007264));
#207687=CARTESIAN_POINT('Ctrl Pts',(-28.0380276306472,-63.3454586317787,
75.2241170171683));
#207688=CARTESIAN_POINT('Ctrl Pts',(-28.0559933115398,-63.2278430736962,
74.4853807791906));
#207689=CARTESIAN_POINT('Ctrl Pts',(-28.0906017774928,-63.1378619891058,
73.0679641596003));
#207690=CARTESIAN_POINT('Ctrl Pts',(-28.1072138532676,-63.1526649094277,
72.3930065568334));
#207691=CARTESIAN_POINT('Ctrl Pts',(-28.1430018502095,-63.3086502028039,
70.9442050877484));
#207692=CARTESIAN_POINT('Ctrl Pts',(-28.1618386467817,-63.4695746651608,
70.1756605434761));
#207693=CARTESIAN_POINT('Ctrl Pts',(-28.1951719525807,-63.8788966067122,
68.8780392101065));
#207694=CARTESIAN_POINT('Ctrl Pts',(-28.209451321217,-64.0926259071167,
68.3408662960563));
#207695=CARTESIAN_POINT('Ctrl Pts',(-28.2330434613466,-64.5115675363652,
67.477538743212));
#207696=CARTESIAN_POINT('Ctrl Pts',(-28.2423403980979,-64.6950042239373,
67.1419257611867));
#207697=CARTESIAN_POINT('Ctrl Pts',(-28.2782575692713,-65.4642324921899,
65.8834052913237));
#207698=CARTESIAN_POINT('Ctrl Pts',(-28.3052940638149,-66.1604550120399,
65.0344049615902));
#207699=CARTESIAN_POINT('Ctrl Pts',(-28.350874467331,-67.5289153598374,
63.7704257229028));
#207700=CARTESIAN_POINT('Ctrl Pts',(-28.3695263041074,-68.1443016492391,
63.3043181251833));
#207701=CARTESIAN_POINT('Ctrl Pts',(-28.4073533634817,-69.452036387946,
62.5012072138239));
#207702=CARTESIAN_POINT('Ctrl Pts',(-28.4262322373492,-70.1407193831999,
62.1651652551974));
#207703=CARTESIAN_POINT('Ctrl Pts',(-28.4729977225934,-71.9374544942296,
61.4946502189513));
#207704=CARTESIAN_POINT('Ctrl Pts',(-28.5015233185326,-73.0710745963116,
61.2514541564332));
#207705=CARTESIAN_POINT('Ctrl Pts',(-28.539037728165,-74.6015318743609,
61.1511013483145));
#207706=CARTESIAN_POINT('Ctrl Pts',(-28.5482828840261,-74.9821772154139,
61.1445222323692));
#207707=CARTESIAN_POINT('Ctrl Pts',(-28.5757505360324,-76.1066502335183,
61.1792932576915));
#207708=CARTESIAN_POINT('Ctrl Pts',(-28.5941223390068,-76.8469945147195,
61.2724481329931));
#207709=CARTESIAN_POINT('Ctrl Pts',(-28.6309417874922,-78.3050861885961,
61.597622529213));
#207710=CARTESIAN_POINT('Ctrl Pts',(-28.649017256776,-79.0193697578069,
61.829813117216));
#207711=CARTESIAN_POINT('Ctrl Pts',(-28.6864894041204,-80.424296898995,
62.439041713671));
#207712=CARTESIAN_POINT('Ctrl Pts',(-28.705881136776,-81.1091114536378,
62.8204354895673));
#207713=CARTESIAN_POINT('Ctrl Pts',(-28.7342580491699,-82.0639475914451,
63.4837217852691));
#207714=CARTESIAN_POINT('Ctrl Pts',(-28.7434809356145,-82.3659292479492,
63.7158496889855));
#207715=CARTESIAN_POINT('Ctrl Pts',(-28.7709065316449,-83.2252871348818,
64.4449357595009));
#207716=CARTESIAN_POINT('Ctrl Pts',(-28.7892499602592,-83.7474465205768,
64.9804773629521));
#207717=CARTESIAN_POINT('Ctrl Pts',(-28.8259669934294,-84.6852208613554,
66.1442567743271));
#207718=CARTESIAN_POINT('Ctrl Pts',(-28.8439536997745,-85.0984403092417,
66.7701248636407));
#207719=CARTESIAN_POINT('Ctrl Pts',(-28.8715192371081,-85.6297322719695,
67.76907056115));
#207720=CARTESIAN_POINT('Ctrl Pts',(-28.8808941381578,-85.7930150961074,
68.1156853205936));
#207721=CARTESIAN_POINT('Ctrl Pts',(-28.8902889611216,-85.9391496391482,
68.4693880297961));
#207722=CARTESIAN_POINT('Ctrl Pts',(-29.1863798856002,-85.9391496391482,
68.4693880297961));
#207723=CARTESIAN_POINT('Ctrl Pts',(-29.1772971019885,-85.7960433235432,
68.1230148145369));
#207724=CARTESIAN_POINT('Ctrl Pts',(-29.1681963644014,-85.6364843713224,
67.783420036426));
#207725=CARTESIAN_POINT('Ctrl Pts',(-29.1407582807521,-85.1107337065779,
66.7900910423739));
#207726=CARTESIAN_POINT('Ctrl Pts',(-29.1223061210748,-84.6985425981529,
66.1631089736439));
#207727=CARTESIAN_POINT('Ctrl Pts',(-29.086126866369,-83.7636903125962,
64.9983969503919));
#207728=CARTESIAN_POINT('Ctrl Pts',(-29.0681898763684,-83.2436912315594,
64.4628250181062));
#207729=CARTESIAN_POINT('Ctrl Pts',(-29.0406822288947,-82.3871745438409,
63.7327731941406));
#207730=CARTESIAN_POINT('Ctrl Pts',(-29.0313471682672,-82.085776424672,
63.4999911451696));
#207731=CARTESIAN_POINT('Ctrl Pts',(-28.9963513666028,-80.9090654919775,
62.6785523534647));
#207732=CARTESIAN_POINT('Ctrl Pts',(-28.9712333862021,-79.9676695700785,
62.1931766210143));
#207733=CARTESIAN_POINT('Ctrl Pts',(-28.936153491432,-78.6150149385664,
61.7106575674738));
#207734=CARTESIAN_POINT('Ctrl Pts',(-28.9268151025791,-78.2495315632111,
61.5998777430556));
#207735=CARTESIAN_POINT('Ctrl Pts',(-28.8986232865437,-77.1209857350694,
61.3165687150427));
#207736=CARTESIAN_POINT('Ctrl Pts',(-28.8799524364902,-76.3456378895604,
61.2017806270506));
#207737=CARTESIAN_POINT('Ctrl Pts',(-28.84277626314,-74.8190565486453,61.1284459314675));
#207738=CARTESIAN_POINT('Ctrl Pts',(-28.8245393308923,-74.0717378243645,
61.1632193222358));
#207739=CARTESIAN_POINT('Ctrl Pts',(-28.7973642074776,-72.9538852843799,
61.3218872134568));
#207740=CARTESIAN_POINT('Ctrl Pts',(-28.7881723804377,-72.5779165325592,
61.3939830133214));
#207741=CARTESIAN_POINT('Ctrl Pts',(-28.7605398889809,-71.467218577826,
61.6633444746261));
#207742=CARTESIAN_POINT('Ctrl Pts',(-28.7419026733009,-70.7473162378985,
61.9132892231419));
#207743=CARTESIAN_POINT('Ctrl Pts',(-28.7024162991224,-69.2638670363202,
62.5943845610187));
#207744=CARTESIAN_POINT('Ctrl Pts',(-28.6816183984185,-68.5139859753697,
63.0446887362641));
#207745=CARTESIAN_POINT('Ctrl Pts',(-28.6511205513814,-67.5178540827379,
63.8037720930618));
#207746=CARTESIAN_POINT('Ctrl Pts',(-28.6418249490305,-67.2266154303546,
64.0487477735725));
#207747=CARTESIAN_POINT('Ctrl Pts',(-28.6070570797181,-66.1770088413486,
65.0216909239259));
#207748=CARTESIAN_POINT('Ctrl Pts',(-28.5820663180276,-65.5048692407564,
65.8354971531125));
#207749=CARTESIAN_POINT('Ctrl Pts',(-28.5471143481036,-64.7472228277439,
67.0509431605125));
#207750=CARTESIAN_POINT('Ctrl Pts',(-28.5377911110625,-64.5612176840882,
67.3841804834701));
#207751=CARTESIAN_POINT('Ctrl Pts',(-28.5057992212909,-63.9736707187411,
68.5677290036345));
#207752=CARTESIAN_POINT('Ctrl Pts',(-28.4833135156324,-63.6574612378688,
69.4564278876824));
#207753=CARTESIAN_POINT('Ctrl Pts',(-28.4510316098729,-63.3654362439088,
70.7447832160995));
#207754=CARTESIAN_POINT('Ctrl Pts',(-28.4416982050555,-63.299187330961,
71.1202907801755));
#207755=CARTESIAN_POINT('Ctrl Pts',(-28.4111483995126,-63.1405535562565,
72.3690450414608));
#207756=CARTESIAN_POINT('Ctrl Pts',(-28.3901404343418,-63.1271069850738,
73.2493573598642));
#207757=CARTESIAN_POINT('Ctrl Pts',(-28.3593818012442,-63.247423227447,
74.5012803414066));
#207758=CARTESIAN_POINT('Ctrl Pts',(-28.3500533854523,-63.3019615544363,
74.8775504441455));
#207759=CARTESIAN_POINT('Ctrl Pts',(-28.3145658838677,-63.5795131831366,
76.3047652862547));
#207760=CARTESIAN_POINT('Ctrl Pts',(-28.2888790660904,-63.9270181929924,
77.3262045619693));
#207761=CARTESIAN_POINT('Ctrl Pts',(-28.253128170771,-64.5784613645797,
78.6286525642252));
#207762=CARTESIAN_POINT('Ctrl Pts',(-28.2437350477626,-64.7659425711944,
78.9620942217622));
#207763=CARTESIAN_POINT('Ctrl Pts',(-28.2210603974966,-65.261384644195,
79.751223920991));
#207764=CARTESIAN_POINT('Ctrl Pts',(-28.2078117545108,-65.5855813581234,
80.1956652425472));
#207765=CARTESIAN_POINT('Ctrl Pts',(-28.1753370399049,-66.4432887600706,
81.2143830534427));
#207766=CARTESIAN_POINT('Ctrl Pts',(-28.1559792817018,-67.0051748741336,
81.7613796200071));
#207767=CARTESIAN_POINT('Ctrl Pts',(-28.1238826824113,-68.0341112928614,
82.581507257976));
#207768=CARTESIAN_POINT('Ctrl Pts',(-28.1109884955671,-68.4733393884123,
82.8854799455036));
#207769=CARTESIAN_POINT('Ctrl Pts',(-28.0794727435621,-69.5815716782739,
83.5464889931359));
#207770=CARTESIAN_POINT('Ctrl Pts',(-28.0607239664772,-70.2672509867591,
83.8709658275296));
#207771=CARTESIAN_POINT('Ctrl Pts',(-28.0217455610983,-71.7645473977778,
84.4110543225423));
#207772=CARTESIAN_POINT('Ctrl Pts',(-28.0016036491204,-72.5776705248003,
84.6104775775714));
#207773=CARTESIAN_POINT('Ctrl Pts',(-27.9626090655067,-74.1466431912166,
84.8233178847389));
#207774=CARTESIAN_POINT('Ctrl Pts',(-27.944140686824,-74.8961773583242,
84.8533764503368));
#207775=CARTESIAN_POINT('Ctrl Pts',(-27.9073466166383,-76.4035714098902,
84.7708829331443));
#207776=CARTESIAN_POINT('Ctrl Pts',(-27.8887394009146,-77.1578438435078,
84.6560880138918));
#207777=CARTESIAN_POINT('Ctrl Pts',(-27.8604553618274,-78.2675743292867,
84.3758045125257));
#207778=CARTESIAN_POINT('Ctrl Pts',(-27.8509778381277,-78.6345156666761,
84.2639194082339));
#207779=CARTESIAN_POINT('Ctrl Pts',(-27.8282952642196,-79.5066990884764,
83.9509517373548));
#207780=CARTESIAN_POINT('Ctrl Pts',(-27.8151196182559,-80.0047829154031,
83.7325011740936));
#207781=CARTESIAN_POINT('Ctrl Pts',(-27.7833096066947,-81.1546297060221,
83.1307836630291));
#207782=CARTESIAN_POINT('Ctrl Pts',(-27.7645629968101,-81.7881823980881,
82.7178376662782));
#207783=CARTESIAN_POINT('Ctrl Pts',(-27.724612867408,-83.0623235968154,
81.7018345949151));
#207784=CARTESIAN_POINT('Ctrl Pts',(-27.7034548636324,-83.6839390151742,
81.082066834104));
#207785=CARTESIAN_POINT('Ctrl Pts',(-27.672478627145,-84.4697558964199,
80.1025887706415));
#207786=CARTESIAN_POINT('Ctrl Pts',(-27.6630586456205,-84.6934918862971,
79.7943823483294));
#207787=CARTESIAN_POINT('Ctrl Pts',(-27.6344430041026,-85.3309789543933,
78.8207398754691));
#207788=CARTESIAN_POINT('Ctrl Pts',(-27.6155741924473,-85.6939013615658,
78.1245952783084));
#207789=CARTESIAN_POINT('Ctrl Pts',(-27.5779950692029,-86.2637759448029,
76.7037178938473));
#207790=CARTESIAN_POINT('Ctrl Pts',(-27.559469337933,-86.4757554127163,
75.9848889626256));
#207791=CARTESIAN_POINT('Ctrl Pts',(-27.5230989687509,-86.7608444447559,
74.5191435707775));
#207792=CARTESIAN_POINT('Ctrl Pts',(-27.5050372303059,-86.8337435163221,
73.775596407627));
#207793=CARTESIAN_POINT('Ctrl Pts',(-27.4773527021625,-86.83752431961,72.6495276199141));
#207794=CARTESIAN_POINT('Ctrl Pts',(-27.4679637405674,-86.8204473139073,
72.2690664875133));
#207795=CARTESIAN_POINT('Ctrl Pts',(-27.4394453805095,-86.7123543098441,
71.1109723305979));
#207796=CARTESIAN_POINT('Ctrl Pts',(-27.420664768781,-86.5625736543532,
70.3409800383466));
#207797=CARTESIAN_POINT('Ctrl Pts',(-27.3918260336057,-86.2238438127127,
69.2107403412772));
#207798=CARTESIAN_POINT('Ctrl Pts',(-27.3820680337574,-86.0907277246481,
68.836266240543));
#207799=CARTESIAN_POINT('Ctrl Pts',(-27.3723203523406,-85.9391496445663,
68.4693880429103));
#207800=CARTESIAN_POINT('Origin',(-33.5526503323277,-74.999949493375,72.9851176492631));
#207801=CARTESIAN_POINT('',(-37.9576288901553,-85.9425570350205,68.4641091549305));
#207802=CARTESIAN_POINT('',(-38.2588681851947,-85.9425518661828,68.4640966443435));
#207803=CARTESIAN_POINT('',(-33.5526503323277,-85.9425570350204,68.4641091549303));
#207804=CARTESIAN_POINT('',(-37.9576293742551,-85.9425645971074,68.4641274581797));
#207805=CARTESIAN_POINT('Ctrl Pts',(-37.9576288901553,-85.9425570350206,
68.4641091549307));
#207806=CARTESIAN_POINT('Ctrl Pts',(-37.9576291329799,-85.9425608281721,
68.4641183358399));
#207807=CARTESIAN_POINT('Ctrl Pts',(-37.9576293758044,-85.9425646213122,
68.4641275167542));
#207808=CARTESIAN_POINT('Ctrl Pts',(-37.9576296186288,-85.9425684144409,
68.4641366976736));
#207809=CARTESIAN_POINT('',(-38.4180624217171,-79.3025708087853,84.0154429842386));
#207810=CARTESIAN_POINT('Ctrl Pts',(-37.9576293742551,-85.9425645971074,
68.4641274581797));
#207811=CARTESIAN_POINT('Ctrl Pts',(-37.9743923969875,-86.2044180485594,
69.0979181570568));
#207812=CARTESIAN_POINT('Ctrl Pts',(-37.9910143369726,-86.4107141752036,
69.7532621342486));
#207813=CARTESIAN_POINT('Ctrl Pts',(-38.0246878627216,-86.706819364395,
71.0890404319913));
#207814=CARTESIAN_POINT('Ctrl Pts',(-38.0416261577221,-86.7966319325827,
71.7668394250167));
#207815=CARTESIAN_POINT('Ctrl Pts',(-38.0694126443366,-86.8481623115025,
72.9028136493742));
#207816=CARTESIAN_POINT('Ctrl Pts',(-38.0804609652665,-86.8425840969132,
73.3578466519687));
#207817=CARTESIAN_POINT('Ctrl Pts',(-38.1107350188431,-86.7563114151496,
74.5909878161061));
#207818=CARTESIAN_POINT('Ctrl Pts',(-38.1301458593981,-86.624726229738,
75.3632308311965));
#207819=CARTESIAN_POINT('Ctrl Pts',(-38.1586472131736,-86.3172838441829,
76.4841413512661));
#207820=CARTESIAN_POINT('Ctrl Pts',(-38.1679026264474,-86.1988822198968,
76.8463520170879));
#207821=CARTESIAN_POINT('Ctrl Pts',(-38.1865718755565,-85.9263093144659,
77.5614275235112));
#207822=CARTESIAN_POINT('Ctrl Pts',(-38.1959758908047,-85.7719763124514,
77.9137470500015));
#207823=CARTESIAN_POINT('Ctrl Pts',(-38.2228550042187,-85.2855496534766,
78.8916927030285));
#207824=CARTESIAN_POINT('Ctrl Pts',(-38.2403936750185,-84.9141192185452,
79.495912358085));
#207825=CARTESIAN_POINT('Ctrl Pts',(-38.2709383730497,-84.1652783971981,
80.500014999148));
#207826=CARTESIAN_POINT('Ctrl Pts',(-38.2841616945643,-83.8098556447903,
80.9137044893147));
#207827=CARTESIAN_POINT('Ctrl Pts',(-38.3176332551114,-82.8513592357023,
81.8849868252109));
#207828=CARTESIAN_POINT('Ctrl Pts',(-38.3379297369795,-82.216444701061,
82.4071404513844));
#207829=CARTESIAN_POINT('Ctrl Pts',(-38.368073150965,-81.1831583171694,
83.0907477405221));
#207830=CARTESIAN_POINT('Ctrl Pts',(-38.3782385943083,-80.8215881332394,
83.3032741780965));
#207831=CARTESIAN_POINT('Ctrl Pts',(-38.3987282946612,-80.0768318302408,
83.6894003568694));
#207832=CARTESIAN_POINT('Ctrl Pts',(-38.4090386083604,-79.6941400064729,
83.8626621797839));
#207833=CARTESIAN_POINT('Ctrl Pts',(-38.4193726539769,-79.3030589811838,
84.0152321705287));
#207834=CARTESIAN_POINT('',(-38.7170569083159,-79.302583977372,84.0154504430313));
#207835=CARTESIAN_POINT('',(-38.4175364832709,-79.30270960864,84.0153684626757));
#207836=CARTESIAN_POINT('Ctrl Pts',(-38.2588685144218,-85.9425570350203,
68.4641091549302));
#207837=CARTESIAN_POINT('Ctrl Pts',(-38.2753921140801,-86.2019757173487,
69.0920037570412));
#207838=CARTESIAN_POINT('Ctrl Pts',(-38.2919909110401,-86.4068721094222,
69.7410687161471));
#207839=CARTESIAN_POINT('Ctrl Pts',(-38.3247086479941,-86.7021386154924,
71.062960663399));
#207840=CARTESIAN_POINT('Ctrl Pts',(-38.3408123281424,-86.7926840996756,
71.7331880602675));
#207841=CARTESIAN_POINT('Ctrl Pts',(-38.368176471662,-86.847564808067,72.8567104434098));
#207842=CARTESIAN_POINT('Ctrl Pts',(-38.3791668041158,-86.8438920145194,
73.3068378553918));
#207843=CARTESIAN_POINT('Ctrl Pts',(-38.404419780308,-86.7762256212567,
74.3443579761178));
#207844=CARTESIAN_POINT('Ctrl Pts',(-38.4185812414996,-86.6938852844249,
74.9293606887009));
#207845=CARTESIAN_POINT('Ctrl Pts',(-38.4507641769267,-86.4092982467322,
76.235443956933));
#207846=CARTESIAN_POINT('Ctrl Pts',(-38.4690337585595,-86.1816326587067,
76.9484258103896));
#207847=CARTESIAN_POINT('Ctrl Pts',(-38.5056409803773,-85.5900645712485,
78.3336123336522));
#207848=CARTESIAN_POINT('Ctrl Pts',(-38.5237690303284,-85.2252868599235,
79.0017114320046));
#207849=CARTESIAN_POINT('Ctrl Pts',(-38.5602504821626,-84.3803056288327,
80.2477433922791));
#207850=CARTESIAN_POINT('Ctrl Pts',(-38.5785684555978,-83.9041334058414,
80.8242712373526));
#207851=CARTESIAN_POINT('Ctrl Pts',(-38.616219007985,-82.8062023510351,
81.9235023377032));
#207852=CARTESIAN_POINT('Ctrl Pts',(-38.6355332715926,-82.1785627775367,
82.4349754727978));
#207853=CARTESIAN_POINT('Ctrl Pts',(-38.6653949765361,-81.1583426766389,
83.1056540435057));
#207854=CARTESIAN_POINT('Ctrl Pts',(-38.6755171178595,-80.8012577923637,
83.3144877599883));
#207855=CARTESIAN_POINT('Ctrl Pts',(-38.6956648674306,-80.066181046409,
83.6942191651638));
#207856=CARTESIAN_POINT('Ctrl Pts',(-38.7056764744094,-79.6886661336525,
83.8648002743088));
#207857=CARTESIAN_POINT('Ctrl Pts',(-38.7156810426872,-79.3029942695161,
84.0152574158675));
#207858=CARTESIAN_POINT('Origin',(-33.5526503323277,-74.999949493375,72.9851176492631));
#207859=CARTESIAN_POINT('',(-36.4450710296185,-85.9425570350204,68.4641091549303));
#207860=CARTESIAN_POINT('Ctrl Pts',(-38.2588681851947,-85.9425518661828,
68.4640966443435));
#207861=CARTESIAN_POINT('Ctrl Pts',(-38.2416125443476,-85.6716394289052,
67.8083847872759));
#207862=CARTESIAN_POINT('Ctrl Pts',(-38.2246992567495,-85.3423424744358,
67.178359752856));
#207863=CARTESIAN_POINT('Ctrl Pts',(-38.1907913902441,-84.5847639064926,
66.0001810544474));
#207864=CARTESIAN_POINT('Ctrl Pts',(-38.1738496662569,-84.1607033288119,
65.4526156031358));
#207865=CARTESIAN_POINT('Ctrl Pts',(-38.1458700494748,-83.3784173735093,
64.6069461298567));
#207866=CARTESIAN_POINT('Ctrl Pts',(-38.1348186763153,-83.0460512346096,
64.2872598648431));
#207867=CARTESIAN_POINT('Ctrl Pts',(-38.1012115696759,-81.9879336323315,
63.382191774255));
#207868=CARTESIAN_POINT('Ctrl Pts',(-38.0783453797895,-81.2109640053625,
62.8623023649894));
#207869=CARTESIAN_POINT('Ctrl Pts',(-38.0372470656261,-79.7022677703556,
62.0924956090233));
#207870=CARTESIAN_POINT('Ctrl Pts',(-38.0189916508675,-78.9915459718726,
61.8124646475773));
#207871=CARTESIAN_POINT('Ctrl Pts',(-37.9851891809974,-77.6600567554545,
61.4312455378352));
#207872=CARTESIAN_POINT('Ctrl Pts',(-37.9698558123282,-77.0486597540841,
61.3073215263093));
#207873=CARTESIAN_POINT('Ctrl Pts',(-37.9455221116277,-76.0534310284601,
61.1861967898652));
#207874=CARTESIAN_POINT('Ctrl Pts',(-37.9363633125234,-75.6745141071768,
61.1584816112066));
#207875=CARTESIAN_POINT('Ctrl Pts',(-37.9052919782341,-74.3934819972736,
61.1265564688018));
#207876=CARTESIAN_POINT('Ctrl Pts',(-37.8830606873922,-73.4924271033512,
61.2071451995449));
#207877=CARTESIAN_POINT('Ctrl Pts',(-37.842452469934,-71.8611039360052,
61.543465613656));
#207878=CARTESIAN_POINT('Ctrl Pts',(-37.8240751982879,-71.1295998622464,
61.7697642269712));
#207879=CARTESIAN_POINT('Ctrl Pts',(-37.796023696184,-70.0741530811529,
62.211937365696));
#207880=CARTESIAN_POINT('Ctrl Pts',(-37.7866509684566,-69.7305847509062,
62.3757501858922));
#207881=CARTESIAN_POINT('Ctrl Pts',(-37.7589211397404,-68.7375101769051,
62.9094039216394));
#207882=CARTESIAN_POINT('Ctrl Pts',(-37.7409140989774,-68.1144577391385,
63.3244676823421));
#207883=CARTESIAN_POINT('Ctrl Pts',(-37.7035748245326,-66.9278199909356,
64.2884395531698));
#207884=CARTESIAN_POINT('Ctrl Pts',(-37.6841954035802,-66.3712896182925,
64.8403214554513));
#207885=CARTESIAN_POINT('Ctrl Pts',(-37.6463117908446,-65.3853821197504,
66.0333703196312));
#207886=CARTESIAN_POINT('Ctrl Pts',(-37.6278172025649,-64.9559563641628,
66.6696679463548));
#207887=CARTESIAN_POINT('Ctrl Pts',(-37.5996252819912,-64.4098558886715,
67.6771441788257));
#207888=CARTESIAN_POINT('Ctrl Pts',(-37.5902278724741,-64.2449134677174,
68.0198518845031));
#207889=CARTESIAN_POINT('Ctrl Pts',(-37.5624044606299,-63.8053665947533,
69.0582574537565));
#207890=CARTESIAN_POINT('Ctrl Pts',(-37.5443334318455,-63.5798328803693,
69.7726645123915));
#207891=CARTESIAN_POINT('Ctrl Pts',(-37.5068934288594,-63.2593820722814,
71.2676036407564));
#207892=CARTESIAN_POINT('Ctrl Pts',(-37.4874816554964,-63.17164387106,72.0459921353528));
#207893=CARTESIAN_POINT('Ctrl Pts',(-37.4495292111963,-63.1510148244988,
73.5937510368514));
#207894=CARTESIAN_POINT('Ctrl Pts',(-37.4309908956369,-63.2152494585919,
74.3593589166442));
#207895=CARTESIAN_POINT('Ctrl Pts',(-37.4027658154795,-63.4212676048063,
75.4867988277926));
#207896=CARTESIAN_POINT('Ctrl Pts',(-37.3933733120741,-63.5074246657974,
75.8567296161491));
#207897=CARTESIAN_POINT('Ctrl Pts',(-37.3655429605183,-63.8156143655937,
76.9411140168159));
#207898=CARTESIAN_POINT('Ctrl Pts',(-37.3474663305294,-64.0876986611687,
77.6393676233608));
#207899=CARTESIAN_POINT('Ctrl Pts',(-37.3100234317308,-64.7751675108902,
79.0054966869767));
#207900=CARTESIAN_POINT('Ctrl Pts',(-37.2906186537663,-65.1948023495195,
79.6671992307357));
#207901=CARTESIAN_POINT('Ctrl Pts',(-37.2527293925608,-66.1485614315836,
80.8857195033305));
#207902=CARTESIAN_POINT('Ctrl Pts',(-37.2342357545949,-66.6779437734176,
81.4415239738006));
#207903=CARTESIAN_POINT('Ctrl Pts',(-37.2060940265001,-67.5441090173429,
82.1902448480956));
#207904=CARTESIAN_POINT('Ctrl Pts',(-37.1967331731798,-67.8426842846673,
82.4242636898797));
#207905=CARTESIAN_POINT('Ctrl Pts',(-37.1689807489343,-68.7619521988769,
83.0760387798127));
#207906=CARTESIAN_POINT('Ctrl Pts',(-37.1509553911568,-69.4115327090771,
83.449767619805));
#207907=CARTESIAN_POINT('Ctrl Pts',(-37.1136099924952,-70.8038262478118,
84.0839709447713));
#207908=CARTESIAN_POINT('Ctrl Pts',(-37.0942546423633,-71.5460236827676,
84.3368746469189));
#207909=CARTESIAN_POINT('Ctrl Pts',(-37.0565352279133,-73.051858134729,
84.6884955663936));
#207910=CARTESIAN_POINT('Ctrl Pts',(-37.0381506453932,-73.8110757932122,
84.789807429784));
#207911=CARTESIAN_POINT('Ctrl Pts',(-37.010166306195,-74.9534477350529,
84.8308601815569));
#207912=CARTESIAN_POINT('Ctrl Pts',(-37.0008486703605,-75.3325853469066,
84.8262802307058));
#207913=CARTESIAN_POINT('Ctrl Pts',(-36.9732219453808,-76.4571279179261,
84.7586369880659));
#207914=CARTESIAN_POINT('Ctrl Pts',(-36.9552807147453,-77.1974784827877,
84.6431618483784));
#207915=CARTESIAN_POINT('Ctrl Pts',(-36.918216632995,-78.67545719408,84.266756192141));
#207916=CARTESIAN_POINT('Ctrl Pts',(-36.8990633551225,-79.4081973934672,
84.0011092457016));
#207917=CARTESIAN_POINT('Ctrl Pts',(-36.861678037431,-80.7968427730354,
83.3367662934791));
#207918=CARTESIAN_POINT('Ctrl Pts',(-36.843434072982,-81.450762252324,82.9424075977943));
#207919=CARTESIAN_POINT('Ctrl Pts',(-36.8156208183404,-82.3667480570503,
82.2616680953195));
#207920=CARTESIAN_POINT('Ctrl Pts',(-36.8063331633932,-82.6601959543437,
82.0208651388703));
#207921=CARTESIAN_POINT('Ctrl Pts',(-36.7788204255325,-83.4957607368464,
81.2651954505709));
#207922=CARTESIAN_POINT('Ctrl Pts',(-36.7609605030719,-84.0012571101229,
80.71266317542));
#207923=CARTESIAN_POINT('Ctrl Pts',(-36.7239099388123,-84.9232542401603,
79.4906702030789));
#207924=CARTESIAN_POINT('Ctrl Pts',(-36.7046775421896,-85.3319454568592,
78.8198451706126));
#207925=CARTESIAN_POINT('Ctrl Pts',(-36.6673068359652,-86.0007663416384,
77.4281497084285));
#207926=CARTESIAN_POINT('Ctrl Pts',(-36.6491525986536,-86.2633684645749,
76.7125705098767));
#207927=CARTESIAN_POINT('Ctrl Pts',(-36.6214428496755,-86.5514603764109,
75.6094128012789));
#207928=CARTESIAN_POINT('Ctrl Pts',(-36.612172041046,-86.6296694441817,
75.2376588382518));
#207929=CARTESIAN_POINT('Ctrl Pts',(-36.5847295931906,-86.8083033491122,
74.1255289639083));
#207930=CARTESIAN_POINT('Ctrl Pts',(-36.5669174831325,-86.8567129957862,
73.3787156042629));
#207931=CARTESIAN_POINT('Ctrl Pts',(-36.5299300095861,-86.8111017792754,
71.848643033187));
#207932=CARTESIAN_POINT('Ctrl Pts',(-36.5107101518215,-86.709953528322,
71.0692126138227));
#207933=CARTESIAN_POINT('Ctrl Pts',(-36.4761290010132,-86.3863504026881,
69.6764751873896));
#207934=CARTESIAN_POINT('Ctrl Pts',(-36.4607107367829,-86.1890117344204,
69.0606258515277));
#207935=CARTESIAN_POINT('Ctrl Pts',(-36.4450710296185,-85.9425570350204,
68.4641091549303));
#207936=CARTESIAN_POINT('',(-36.143425535889,-85.9425570350204,68.4641091549303));
#207937=CARTESIAN_POINT('',(-33.5526503323277,-85.9425570350204,68.4641091549303));
#207938=CARTESIAN_POINT('Ctrl Pts',(-36.143425535889,-85.9425570350204,
68.4641091549303));
#207939=CARTESIAN_POINT('Ctrl Pts',(-36.148238507304,-86.0174834758539,
68.6454604259047));
#207940=CARTESIAN_POINT('Ctrl Pts',(-36.1530665592699,-86.0879280851577,
68.8287383180261));
#207941=CARTESIAN_POINT('Ctrl Pts',(-36.167266731233,-86.281155707984,69.371435524502));
#207942=CARTESIAN_POINT('Ctrl Pts',(-36.1766643368532,-86.3912228849641,
69.7350096114226));
#207943=CARTESIAN_POINT('Ctrl Pts',(-36.2030542231982,-86.6518386352883,
70.7735096421015));
#207944=CARTESIAN_POINT('Ctrl Pts',(-36.2197568716503,-86.7610399882958,
71.4572166260671));
#207945=CARTESIAN_POINT('Ctrl Pts',(-36.2552103712041,-86.8635398875244,
72.9007540960301));
#207946=CARTESIAN_POINT('Ctrl Pts',(-36.2739887581872,-86.8447212800773,
73.6583681292809));
#207947=CARTESIAN_POINT('Ctrl Pts',(-36.3103716158341,-86.6664108020393,
75.1302890120472));
#207948=CARTESIAN_POINT('Ctrl Pts',(-36.3279354581554,-86.5128221102881,
75.8420129729576));
#207949=CARTESIAN_POINT('Ctrl Pts',(-36.3641725418675,-86.0709158492975,
77.2480084534117));
#207950=CARTESIAN_POINT('Ctrl Pts',(-36.3827138424614,-85.7798828500403,
77.9380541339613));
#207951=CARTESIAN_POINT('Ctrl Pts',(-36.4191576989442,-85.072124697069,
79.2531561708606));
#207952=CARTESIAN_POINT('Ctrl Pts',(-36.4372829124874,-84.6571567029495,
79.8753547680538));
#207953=CARTESIAN_POINT('Ctrl Pts',(-36.4650541363608,-83.9463039397956,
80.7496371837122));
#207954=CARTESIAN_POINT('Ctrl Pts',(-36.4744653456105,-83.6921109467192,
81.0331826818526));
#207955=CARTESIAN_POINT('Ctrl Pts',(-36.5030580974817,-82.8746401466155,
81.8610580580722));
#207956=CARTESIAN_POINT('Ctrl Pts',(-36.5219004939314,-82.2706782802858,
82.3621948471306));
#207957=CARTESIAN_POINT('Ctrl Pts',(-36.5594359775069,-81.0014393595734,
83.2185000153491));
#207958=CARTESIAN_POINT('Ctrl Pts',(-36.5779561060125,-80.3429151466602,
83.5772242458362));
#207959=CARTESIAN_POINT('Ctrl Pts',(-36.6142671885997,-78.9707546081985,
84.1639642071798));
#207960=CARTESIAN_POINT('Ctrl Pts',(-36.6322663079185,-78.2604946666755,
84.3913768263397));
#207961=CARTESIAN_POINT('Ctrl Pts',(-36.6598749832277,-77.1618598961551,
84.6320549198793));
#207962=CARTESIAN_POINT('Ctrl Pts',(-36.6692493346064,-76.7864044560539,
84.6955225510577));
#207963=CARTESIAN_POINT('Ctrl Pts',(-36.6977320732928,-75.6317722112526,
84.8338736460224));
#207964=CARTESIAN_POINT('Ctrl Pts',(-36.7164809648073,-74.8476831316937,
84.8497303991984));
#207965=CARTESIAN_POINT('Ctrl Pts',(-36.7538592000449,-73.3205657064729,
84.7291228904894));
#207966=CARTESIAN_POINT('Ctrl Pts',(-36.7723383793587,-72.5806394466273,
84.5992872690723));
#207967=CARTESIAN_POINT('Ctrl Pts',(-36.8094626036945,-71.1035223093137,
84.1927196477861));
#207968=CARTESIAN_POINT('Ctrl Pts',(-36.8282950950502,-70.3715189689159,
83.9107809543057));
#207969=CARTESIAN_POINT('Ctrl Pts',(-36.856734308558,-69.3326466704178,
83.3873696220951));
#207970=CARTESIAN_POINT('Ctrl Pts',(-36.8660725857096,-69.0010560135803,
83.1997368064791));
#207971=CARTESIAN_POINT('Ctrl Pts',(-36.8943966804287,-68.0179528155365,
82.5790341463043));
#207972=CARTESIAN_POINT('Ctrl Pts',(-36.9130538277333,-67.3997932428991,
82.0971503431833));
#207973=CARTESIAN_POINT('Ctrl Pts',(-36.9502644985451,-66.2915970856974,
81.0414966619182));
#207974=CARTESIAN_POINT('Ctrl Pts',(-36.9686368114208,-65.7997256006237,
80.4748795771567));
#207975=CARTESIAN_POINT('Ctrl Pts',(-37.0047206435837,-64.9305165687805,
79.2576607293675));
#207976=CARTESIAN_POINT('Ctrl Pts',(-37.0226503340936,-64.5548889939857,
78.6099719727269));
#207977=CARTESIAN_POINT('Ctrl Pts',(-37.0501221059068,-64.0838323661145,
77.5854841283829));
#207978=CARTESIAN_POINT('Ctrl Pts',(-37.0594257097561,-63.9416231268765,
77.2322817378447));
#207979=CARTESIAN_POINT('Ctrl Pts',(-37.0944558615515,-63.4683337741028,
75.8708371110155));
#207980=CARTESIAN_POINT('Ctrl Pts',(-37.1196682747815,-63.2562408457119,
74.8265431874806));
#207981=CARTESIAN_POINT('Ctrl Pts',(-37.1548355702015,-63.1608567503633,
73.3872393056425));
#207982=CARTESIAN_POINT('Ctrl Pts',(-37.1641520237652,-63.1540469129996,
73.005445881158));
#207983=CARTESIAN_POINT('Ctrl Pts',(-37.1960864508945,-63.194341250831,
71.6849857454238));
#207984=CARTESIAN_POINT('Ctrl Pts',(-37.2185220904404,-63.3346533868927,
70.7527189972505));
#207985=CARTESIAN_POINT('Ctrl Pts',(-37.2507210153804,-63.6847111884255,
69.4792801883886));
#207986=CARTESIAN_POINT('Ctrl Pts',(-37.2600339386413,-63.8034555614583,
69.1167795582661));
#207987=CARTESIAN_POINT('Ctrl Pts',(-37.2905721356825,-64.2537199352495,
67.93790366409));
#207988=CARTESIAN_POINT('Ctrl Pts',(-37.3115906708213,-64.6587791099737,
67.1527919767579));
#207989=CARTESIAN_POINT('Ctrl Pts',(-37.3423292207609,-65.357995683196,
66.1034389200866));
#207990=CARTESIAN_POINT('Ctrl Pts',(-37.3516320206513,-65.5839750211042,
65.797336342476));
#207991=CARTESIAN_POINT('Ctrl Pts',(-37.3856258642121,-66.467624739571,
64.7137289705806));
#207992=CARTESIAN_POINT('Ctrl Pts',(-37.4098726886797,-67.2100234473301,
64.0110721617912));
#207993=CARTESIAN_POINT('Ctrl Pts',(-37.4440566413501,-68.3410826462592,
63.1879365471086));
#207994=CARTESIAN_POINT('Ctrl Pts',(-37.4533880966028,-68.6596995598004,
62.9787947945492));
#207995=CARTESIAN_POINT('Ctrl Pts',(-37.4830414748069,-69.7116943037478,
62.3587099843057));
#207996=CARTESIAN_POINT('Ctrl Pts',(-37.5031438140031,-70.4789133305202,
62.010309049287));
#207997=CARTESIAN_POINT('Ctrl Pts',(-37.5329543904772,-71.636968187707,
61.6266533792021));
#207998=CARTESIAN_POINT('Ctrl Pts',(-37.5422743339172,-72.0029436119635,
61.5246504221834));
#207999=CARTESIAN_POINT('Ctrl Pts',(-37.5694744519505,-73.087747807898,
61.2778252619525));
#208000=CARTESIAN_POINT('Ctrl Pts',(-37.5870320088167,-73.8158612059384,
61.1819339459102));
#208001=CARTESIAN_POINT('Ctrl Pts',(-37.6239248535313,-75.3301887145771,
61.1241062397469));
#208002=CARTESIAN_POINT('Ctrl Pts',(-37.6432534817882,-76.1132600710327,
61.1718543800873));
#208003=CARTESIAN_POINT('Ctrl Pts',(-37.6766178299039,-77.4672112260184,
61.3903106970509));
#208004=CARTESIAN_POINT('Ctrl Pts',(-37.6908179431224,-78.0407413815151,
61.5273467136123));
#208005=CARTESIAN_POINT('Ctrl Pts',(-37.7243121371928,-79.3470851552171,
61.9445169355828));
#208006=CARTESIAN_POINT('Ctrl Pts',(-37.7436781430201,-80.0670499423904,
62.2558609425313));
#208007=CARTESIAN_POINT('Ctrl Pts',(-37.7784709687326,-81.3158038597836,
62.9497977401581));
#208008=CARTESIAN_POINT('Ctrl Pts',(-37.7940996341551,-81.8539485181105,
63.3093562021165));
#208009=CARTESIAN_POINT('Ctrl Pts',(-37.8221659870852,-82.7499128002765,
64.020411671817));
#208010=CARTESIAN_POINT('Ctrl Pts',(-37.8344691414043,-83.1198651551587,
64.3540776172099));
#208011=CARTESIAN_POINT('Ctrl Pts',(-37.86522554667,-83.9940875726504,65.2486559849823));
#208012=CARTESIAN_POINT('Ctrl Pts',(-37.8833718986528,-84.4678644238347,
65.8362753272456));
#208013=CARTESIAN_POINT('Ctrl Pts',(-37.9203741409185,-85.2989408740914,
67.0959335227594));
#208014=CARTESIAN_POINT('Ctrl Pts',(-37.9391486654917,-85.6538782424784,
67.7653936501169));
#208015=CARTESIAN_POINT('Ctrl Pts',(-37.9576288901553,-85.9425570350206,
68.4641091549307));
#208016=CARTESIAN_POINT('Origin',(-33.5526503323277,-74.999949493375,72.9851176492631));
#208017=CARTESIAN_POINT('',(-34.329622639475,-85.9425570350204,68.4641091549303));
#208018=CARTESIAN_POINT('',(-34.6308727573024,-85.9425570350204,68.4641091549303));
#208019=CARTESIAN_POINT('',(-33.5526503323277,-85.9425570350204,68.4641091549303));
#208020=CARTESIAN_POINT('Ctrl Pts',(-34.329622639475,-85.9425570350204,
68.4641091549303));
#208021=CARTESIAN_POINT('Ctrl Pts',(-34.3331454855336,-85.9971435846138,
68.5962299394856));
#208022=CARTESIAN_POINT('Ctrl Pts',(-34.3366615064198,-86.0493527669876,
68.7293767663076));
#208023=CARTESIAN_POINT('Ctrl Pts',(-34.3589661420323,-86.3663168730277,
69.582934301803));
#208024=CARTESIAN_POINT('Ctrl Pts',(-34.3775289583419,-86.5628967428812,
70.3266565489548));
#208025=CARTESIAN_POINT('Ctrl Pts',(-34.4117140406206,-86.785736124185,
71.6965614893729));
#208026=CARTESIAN_POINT('Ctrl Pts',(-34.4271139387984,-86.8370621353701,
72.3158541704069));
#208027=CARTESIAN_POINT('Ctrl Pts',(-34.4515943340047,-86.8411879378932,
73.3166789929037));
#208028=CARTESIAN_POINT('Ctrl Pts',(-34.460840960197,-86.824425079426,73.6969031311766));
#208029=CARTESIAN_POINT('Ctrl Pts',(-34.4882992586455,-86.7209055734037,
74.816013838025));
#208030=CARTESIAN_POINT('Ctrl Pts',(-34.5066650536923,-86.5828342577236,
75.5482721060436));
#208031=CARTESIAN_POINT('Ctrl Pts',(-34.5435021566419,-86.1693837093553,
76.983421397808));
#208032=CARTESIAN_POINT('Ctrl Pts',(-34.5616096469221,-85.8937474926455,
77.6827616992859));
#208033=CARTESIAN_POINT('Ctrl Pts',(-34.5991461705954,-85.1995290142402,
79.0481026945294));
#208034=CARTESIAN_POINT('Ctrl Pts',(-34.6185603487462,-84.7771069687462,
79.7080934417855));
#208035=CARTESIAN_POINT('Ctrl Pts',(-34.6469680849255,-84.0569094913357,
80.6203317292538));
#208036=CARTESIAN_POINT('Ctrl Pts',(-34.6562049432673,-83.806817852358,
80.9074966497412));
#208037=CARTESIAN_POINT('Ctrl Pts',(-34.6836624447065,-83.0271662173277,
81.7200941635885));
#208038=CARTESIAN_POINT('Ctrl Pts',(-34.7020276571441,-82.4613395161597,
82.2081144724638));
#208039=CARTESIAN_POINT('Ctrl Pts',(-34.7388066803891,-81.242820807903,
83.0731006593034));
#208040=CARTESIAN_POINT('Ctrl Pts',(-34.7568400152815,-80.5925035909137,
83.4476308918892));
#208041=CARTESIAN_POINT('Ctrl Pts',(-34.7942258548029,-79.1995047284768,
84.0826697742791));
#208042=CARTESIAN_POINT('Ctrl Pts',(-34.8135838749069,-78.4574257329447,
84.3357909980717));
#208043=CARTESIAN_POINT('Ctrl Pts',(-34.841917391454,-77.3250717421524,
84.6005797464628));
#208044=CARTESIAN_POINT('Ctrl Pts',(-34.8511227011814,-76.9503498702266,
84.6693417411533));
#208045=CARTESIAN_POINT('Ctrl Pts',(-34.8793707315971,-75.7972408508684,
84.8239127022759));
#208046=CARTESIAN_POINT('Ctrl Pts',(-34.8985781208994,-75.0131129118346,
84.8507215233565));
#208047=CARTESIAN_POINT('Ctrl Pts',(-34.9361050064331,-73.4841460455405,
84.7513541681887));
#208048=CARTESIAN_POINT('Ctrl Pts',(-34.9540641051862,-72.7424940300257,
84.6318286806867));
#208049=CARTESIAN_POINT('Ctrl Pts',(-34.9896687620346,-71.3260212041991,
84.2630799997661));
#208050=CARTESIAN_POINT('Ctrl Pts',(-35.0072527034101,-70.6526056524081,
84.0210036619251));
#208051=CARTESIAN_POINT('Ctrl Pts',(-35.0430839339609,-69.3159397063232,
83.3990514534641));
#208052=CARTESIAN_POINT('Ctrl Pts',(-35.0612722237815,-68.6592371791954,
83.0127474950601));
#208053=CARTESIAN_POINT('Ctrl Pts',(-35.0959719163052,-67.5063999244693,
82.1757879512153));
#208054=CARTESIAN_POINT('Ctrl Pts',(-35.1122898947841,-67.0025037569717,
81.7408343349271));
#208055=CARTESIAN_POINT('Ctrl Pts',(-35.1468602730768,-66.0020639810478,
80.7184797408343));
#208056=CARTESIAN_POINT('Ctrl Pts',(-35.1652217936896,-65.5207497281352,
80.1203545918229));
#208057=CARTESIAN_POINT('Ctrl Pts',(-35.1931558519464,-64.8918673622647,
79.1618177588344));
#208058=CARTESIAN_POINT('Ctrl Pts',(-35.2024619063936,-64.6986035695765,
78.8338115681298));
#208059=CARTESIAN_POINT('Ctrl Pts',(-35.2263409482913,-64.2417323022475,
77.9652779921287));
#208060=CARTESIAN_POINT('Ctrl Pts',(-35.2407033747601,-64.0028852075868,
77.4129627151134));
#208061=CARTESIAN_POINT('Ctrl Pts',(-35.2737592115932,-63.5563632386513,
76.1181001861888));
#208062=CARTESIAN_POINT('Ctrl Pts',(-35.2925525979034,-63.3771186653348,
75.3686101024677));
#208063=CARTESIAN_POINT('Ctrl Pts',(-35.3301955770658,-63.1647543079954,
73.8330157568421));
#208064=CARTESIAN_POINT('Ctrl Pts',(-35.3487882818884,-63.1345993688963,
73.050276214966));
#208065=CARTESIAN_POINT('Ctrl Pts',(-35.3859053287861,-63.2269862620111,
71.5228495536105));
#208066=CARTESIAN_POINT('Ctrl Pts',(-35.4042500264341,-63.3430018964623,
70.7813772379834));
#208067=CARTESIAN_POINT('Ctrl Pts',(-35.4403055803372,-63.7132183521813,
69.331527780735));
#208068=CARTESIAN_POINT('Ctrl Pts',(-35.4582331517031,-63.9663547939685,
68.6263557777856));
#208069=CARTESIAN_POINT('Ctrl Pts',(-35.4857043494334,-64.445988734284,
67.605651120122));
#208070=CARTESIAN_POINT('Ctrl Pts',(-35.4950012797736,-64.624177266005,
67.269516336227));
#208071=CARTESIAN_POINT('Ctrl Pts',(-35.5311899500532,-65.3837890589454,
65.9895734885102));
#208072=CARTESIAN_POINT('Ctrl Pts',(-35.5575682690911,-66.0803483339916,
65.1207108285158));
#208073=CARTESIAN_POINT('Ctrl Pts',(-35.5939937242823,-67.1662192011089,
64.0992137072605));
#208074=CARTESIAN_POINT('Ctrl Pts',(-35.6033388806798,-67.4574982581706,
63.8506745030953));
#208075=CARTESIAN_POINT('Ctrl Pts',(-35.6279078702261,-68.2611781331839,
63.2296149644293));
#208076=CARTESIAN_POINT('Ctrl Pts',(-35.643092677736,-68.7922891015213,
62.8833442566644));
#208077=CARTESIAN_POINT('Ctrl Pts',(-35.6775470584763,-70.0365630454112,
62.2074533387053));
#208078=CARTESIAN_POINT('Ctrl Pts',(-35.6967970925699,-70.759980699616,
61.9028829891663));
#208079=CARTESIAN_POINT('Ctrl Pts',(-35.7249389510534,-71.8715815101032,
61.5597880547802));
#208080=CARTESIAN_POINT('Ctrl Pts',(-35.7341115011194,-72.2402065668481,
61.4651931106097));
#208081=CARTESIAN_POINT('Ctrl Pts',(-35.7618677759948,-73.3604526520311,
61.2345862663303));
#208082=CARTESIAN_POINT('Ctrl Pts',(-35.7806552631901,-74.1212918052034,
61.1533432880975));
#208083=CARTESIAN_POINT('Ctrl Pts',(-35.8215037729031,-75.794586805878,
61.1370451384279));
#208084=CARTESIAN_POINT('Ctrl Pts',(-35.8433144636235,-76.7025343150823,
61.2331185731713));
#208085=CARTESIAN_POINT('Ctrl Pts',(-35.8749641583077,-77.9610258826306,
61.5153134448595));
#208086=CARTESIAN_POINT('Ctrl Pts',(-35.8843204616723,-78.3273548386835,
61.6161794722982));
#208087=CARTESIAN_POINT('Ctrl Pts',(-35.9082821378525,-79.2562739356596,
61.9207031895175));
#208088=CARTESIAN_POINT('Ctrl Pts',(-35.9226926456173,-79.8094247629693,
62.1496890346621));
#208089=CARTESIAN_POINT('Ctrl Pts',(-35.9558505891654,-81.0238912889785,
62.7638346708611));
#208090=CARTESIAN_POINT('Ctrl Pts',(-35.9746959834488,-81.6699859002282,
63.1732319549594));
#208091=CARTESIAN_POINT('Ctrl Pts',(-36.0183948795527,-83.0752451939547,
64.2670087383948));
#208092=CARTESIAN_POINT('Ctrl Pts',(-36.0428739043318,-83.7943899375482,
64.9930187511748));
#208093=CARTESIAN_POINT('Ctrl Pts',(-36.0773872760601,-84.6432282252551,
66.105229667036));
#208094=CARTESIAN_POINT('Ctrl Pts',(-36.0868193645644,-84.8598640899545,
66.4194669793043));
#208095=CARTESIAN_POINT('Ctrl Pts',(-36.1119948092705,-85.4014006277824,
67.2923975823855));
#208096=CARTESIAN_POINT('Ctrl Pts',(-36.1276008548743,-85.6962046419724,
67.8678400796899));
#208097=CARTESIAN_POINT('Ctrl Pts',(-36.143425535889,-85.9425570350204,
68.4641091549303));
#208098=CARTESIAN_POINT('Ctrl Pts',(-36.4450710296185,-85.9425570350204,
68.4641091549303));
#208099=CARTESIAN_POINT('Ctrl Pts',(-36.4423012432504,-85.8989099986937,
68.3584662680661));
#208100=CARTESIAN_POINT('Ctrl Pts',(-36.4395263830693,-85.8537224637666,
68.2534296903723));
#208101=CARTESIAN_POINT('Ctrl Pts',(-36.4214766063348,-85.5503858269364,
67.5755721521631));
#208102=CARTESIAN_POINT('Ctrl Pts',(-36.4060778793579,-85.2485270709375,
67.0234440471119));
#208103=CARTESIAN_POINT('Ctrl Pts',(-36.3817313446517,-84.6962406003481,
66.1802449180317));
#208104=CARTESIAN_POINT('Ctrl Pts',(-36.3726172947798,-84.4730327659579,
65.8728010050208));
#208105=CARTESIAN_POINT('Ctrl Pts',(-36.345519548382,-83.7702764260099,
64.9967402335534));
#208106=CARTESIAN_POINT('Ctrl Pts',(-36.3273777496255,-83.2515338997932,
64.4619638613415));
#208107=CARTESIAN_POINT('Ctrl Pts',(-36.2901603729948,-82.0909634028798,
63.4714504751788));
#208108=CARTESIAN_POINT('Ctrl Pts',(-36.271485138386,-81.446953432645,63.0237682451142));
#208109=CARTESIAN_POINT('Ctrl Pts',(-36.2334585080771,-80.0790776588067,
62.2614727233239));
#208110=CARTESIAN_POINT('Ctrl Pts',(-36.2141711485334,-79.3584738918224,
61.9489330039573));
#208111=CARTESIAN_POINT('Ctrl Pts',(-36.185995790235,-78.2508598472694,
61.5940770740617));
#208112=CARTESIAN_POINT('Ctrl Pts',(-36.1768518249844,-77.8840634175721,
61.4957264208434));
#208113=CARTESIAN_POINT('Ctrl Pts',(-36.1464433664546,-76.6574615990018,
61.2292836392938));
#208114=CARTESIAN_POINT('Ctrl Pts',(-36.1248802104232,-75.7837662242147,
61.138911762691));
#208115=CARTESIAN_POINT('Ctrl Pts',(-36.0849816876455,-74.1456047686891,
61.1516163766496));
#208116=CARTESIAN_POINT('Ctrl Pts',(-36.0666663650914,-73.3854313170334,
61.2311823622453));
#208117=CARTESIAN_POINT('Ctrl Pts',(-36.0386798573186,-72.2650520565091,
61.4592542871392));
#208118=CARTESIAN_POINT('Ctrl Pts',(-36.0293101717141,-71.8957823513543,
61.5531740009475));
#208119=CARTESIAN_POINT('Ctrl Pts',(-36.0016109162129,-70.817837671739,
61.8834274650834));
#208120=CARTESIAN_POINT('Ctrl Pts',(-35.9836295193508,-70.1262781175103,
62.1691612478175));
#208121=CARTESIAN_POINT('Ctrl Pts',(-35.9491086987731,-68.8750423125115,
62.830665325642));
#208122=CARTESIAN_POINT('Ctrl Pts',(-35.932609906165,-68.3113836752578,
63.1927497777215));
#208123=CARTESIAN_POINT('Ctrl Pts',(-35.9067635571126,-67.4778069486584,
63.833933339976));
#208124=CARTESIAN_POINT('Ctrl Pts',(-35.8974498608685,-67.1857983076346,
64.0819808722953));
#208125=CARTESIAN_POINT('Ctrl Pts',(-35.8609307481193,-66.0900369904637,
65.1082854467731));
#208126=CARTESIAN_POINT('Ctrl Pts',(-35.8332993448451,-65.3861858277439,
65.9846490465808));
#208127=CARTESIAN_POINT('Ctrl Pts',(-35.796660027315,-64.6218662135142,
67.2737141729382));
#208128=CARTESIAN_POINT('Ctrl Pts',(-35.7874270697126,-64.4438167182841,
67.6099149701739));
#208129=CARTESIAN_POINT('Ctrl Pts',(-35.7599128469347,-63.9647069729288,
68.6305736201635));
#208130=CARTESIAN_POINT('Ctrl Pts',(-35.7414774339647,-63.7119206907607,
69.3355937987189));
#208131=CARTESIAN_POINT('Ctrl Pts',(-35.7045641317483,-63.3422378550477,
70.7853929430686));
#208132=CARTESIAN_POINT('Ctrl Pts',(-35.6864703925755,-63.2264664906049,
71.5269927350631));
#208133=CARTESIAN_POINT('Ctrl Pts',(-35.64896276832,-63.1346231584062,73.0545522259459));
#208134=CARTESIAN_POINT('Ctrl Pts',(-35.6295395978061,-63.1650606577362,
73.8372882417922));
#208135=CARTESIAN_POINT('Ctrl Pts',(-35.591570688659,-63.3780004791115,
75.3729507917361));
#208136=CARTESIAN_POINT('Ctrl Pts',(-35.5729545372401,-63.5575613725005,
76.1225058437425));
#208137=CARTESIAN_POINT('Ctrl Pts',(-35.5392581543781,-64.0039247016326,
77.4152470367238));
#208138=CARTESIAN_POINT('Ctrl Pts',(-35.5244078500187,-64.2419660370971,
77.9655197990577));
#208139=CARTESIAN_POINT('Ctrl Pts',(-35.5004693491248,-64.6976848422838,
78.8321932270412));
#208140=CARTESIAN_POINT('Ctrl Pts',(-35.4912269110028,-64.8908981914762,
79.1602315944225));
#208141=CARTESIAN_POINT('Ctrl Pts',(-35.4632432077074,-65.5196493313512,
80.1188959326026));
#208142=CARTESIAN_POINT('Ctrl Pts',(-35.4443344478751,-66.0008935294722,
80.7171201449417));
#208143=CARTESIAN_POINT('Ctrl Pts',(-35.4090628193468,-67.0029332504941,
81.7414152575258));
#208144=CARTESIAN_POINT('Ctrl Pts',(-35.3929634040686,-67.5087898420713,
82.1779161630646));
#208145=CARTESIAN_POINT('Ctrl Pts',(-35.3581139196932,-68.6639077562523,
83.0156867835771));
#208146=CARTESIAN_POINT('Ctrl Pts',(-35.3393112272503,-69.320642967518,
83.401604946994));
#208147=CARTESIAN_POINT('Ctrl Pts',(-35.3033648638821,-70.6522332529131,
84.0204876789463));
#208148=CARTESIAN_POINT('Ctrl Pts',(-35.2863178546542,-71.3201557861807,
84.2608062216495));
#208149=CARTESIAN_POINT('Ctrl Pts',(-35.2506607664019,-72.7309324357505,
84.6295964062637));
#208150=CARTESIAN_POINT('Ctrl Pts',(-35.2321277475721,-73.4726974434984,
84.7498884682277));
#208151=CARTESIAN_POINT('Ctrl Pts',(-35.1977519682759,-74.8843898012942,
84.8429857086929));
#208152=CARTESIAN_POINT('Ctrl Pts',(-35.1817199062326,-75.5504459355787,
84.8307642657437));
#208153=CARTESIAN_POINT('Ctrl Pts',(-35.1472033483399,-76.9550789089867,
84.6862178346176));
#208154=CARTESIAN_POINT('Ctrl Pts',(-35.1288267557659,-77.6893151583641,
84.5395799832117));
#208155=CARTESIAN_POINT('Ctrl Pts',(-35.1015387546173,-78.7693740033933,
84.2152777009895));
#208156=CARTESIAN_POINT('Ctrl Pts',(-35.0923560388029,-79.1284330759511,
84.0883009357928));
#208157=CARTESIAN_POINT('Ctrl Pts',(-35.0646247563223,-80.1862319254944,
83.6558044667905));
#208158=CARTESIAN_POINT('Ctrl Pts',(-35.0458864998912,-80.8622097135662,
83.2999116846659));
#208159=CARTESIAN_POINT('Ctrl Pts',(-35.0089330498868,-82.1327502131304,
82.4655028259929));
#208160=CARTESIAN_POINT('Ctrl Pts',(-34.9908243354338,-82.7248219386633,
81.9896111615221));
#208161=CARTESIAN_POINT('Ctrl Pts',(-34.9541983172375,-83.8024995639809,
80.9383692959569));
#208162=CARTESIAN_POINT('Ctrl Pts',(-34.9358635852369,-84.2870193242917,
80.3668141566195));
#208163=CARTESIAN_POINT('Ctrl Pts',(-34.9086817659159,-84.9313639763156,
79.441992414841));
#208164=CARTESIAN_POINT('Ctrl Pts',(-34.8995626760387,-85.1332290555259,
79.1203332685521));
#208165=CARTESIAN_POINT('Ctrl Pts',(-34.8718816299111,-85.6947918522471,
78.1219625845443));
#208166=CARTESIAN_POINT('Ctrl Pts',(-34.8531275457829,-86.0046212701144,
77.4195302834456));
#208167=CARTESIAN_POINT('Ctrl Pts',(-34.8155821464385,-86.4891036128981,
75.9499447390178));
#208168=CARTESIAN_POINT('Ctrl Pts',(-34.7969745907575,-86.6596990821518,
75.1853692935595));
#208169=CARTESIAN_POINT('Ctrl Pts',(-34.7598582721029,-86.8436520623721,
73.6675037772388));
#208170=CARTESIAN_POINT('Ctrl Pts',(-34.7415620763333,-86.8631076912814,
72.9185736740377));
#208171=CARTESIAN_POINT('Ctrl Pts',(-34.7144123214472,-86.7857495694007,
71.7936797547871));
#208172=CARTESIAN_POINT('Ctrl Pts',(-34.7052924697797,-86.7414362950188,
71.4160111223995));
#208173=CARTESIAN_POINT('Ctrl Pts',(-34.6776234151376,-86.5532565853733,
70.2854655652956));
#208174=CARTESIAN_POINT('Ctrl Pts',(-34.6588754588823,-86.3544340290832,
69.5437961207658));
#208175=CARTESIAN_POINT('Ctrl Pts',(-34.6371431145356,-86.039740020247,
68.7049215467144));
#208176=CARTESIAN_POINT('Ctrl Pts',(-34.634004382883,-85.9921284957838,
68.5840914644261));
#208177=CARTESIAN_POINT('Ctrl Pts',(-34.6308727573024,-85.9425570350204,
68.4641091549303));
#208178=CARTESIAN_POINT('Origin',(-33.5526503323277,-74.999949493375,72.9851176492631));
#208179=CARTESIAN_POINT('',(-32.5154663303127,-85.9425570368316,68.4641091593142));
#208180=CARTESIAN_POINT('',(-32.8170317104293,-85.9425570350204,68.4641091549303));
#208181=CARTESIAN_POINT('',(-33.5526503323277,-85.9425570350204,68.4641091549303));
#208182=CARTESIAN_POINT('Ctrl Pts',(-32.5154663303127,-85.9425570386429,
68.4641091636981));
#208183=CARTESIAN_POINT('Ctrl Pts',(-32.5362001555537,-86.2668363188511,
69.2489917644962));
#208184=CARTESIAN_POINT('Ctrl Pts',(-32.557236083159,-86.5057523881385,
70.0665438105178));
#208185=CARTESIAN_POINT('Ctrl Pts',(-32.5968013922866,-86.7889089507147,
71.6513218766206));
#208186=CARTESIAN_POINT('Ctrl Pts',(-32.615162670662,-86.8502293019532,
72.4111403324576));
#208187=CARTESIAN_POINT('Ctrl Pts',(-32.6432761203485,-86.8322269140453,
73.5541258685461));
#208188=CARTESIAN_POINT('Ctrl Pts',(-32.652734137142,-86.8076621161924,
73.9361595922706));
#208189=CARTESIAN_POINT('Ctrl Pts',(-32.6806312601401,-86.6807210837891,
75.0580105174267));
#208190=CARTESIAN_POINT('Ctrl Pts',(-32.6987270624398,-86.5268492396639,
75.7900945267301));
#208191=CARTESIAN_POINT('Ctrl Pts',(-32.7361038674274,-86.072800945195,
77.2493139389786));
#208192=CARTESIAN_POINT('Ctrl Pts',(-32.7554827092351,-85.7671494755215,
77.970977641766));
#208193=CARTESIAN_POINT('Ctrl Pts',(-32.7933507513484,-85.0286027385363,
79.3241718986652));
#208194=CARTESIAN_POINT('Ctrl Pts',(-32.8116761780355,-84.6012393545235,
79.9545317832694));
#208195=CARTESIAN_POINT('Ctrl Pts',(-32.8433914731719,-83.7772204243217,
80.9489310036303));
#208196=CARTESIAN_POINT('Ctrl Pts',(-32.8565470654291,-83.4108245921608,
81.3349671007405));
#208197=CARTESIAN_POINT('Ctrl Pts',(-32.8881540749963,-82.4647649214919,
82.2060616479441));
#208198=CARTESIAN_POINT('Ctrl Pts',(-32.9063137408051,-81.8622296586511,
82.6628441729054));
#208199=CARTESIAN_POINT('Ctrl Pts',(-32.9386784290198,-80.7376169810788,
83.3572544116666));
#208200=CARTESIAN_POINT('Ctrl Pts',(-32.9526892854524,-80.2340901273826,
83.6202395351201));
#208201=CARTESIAN_POINT('Ctrl Pts',(-32.9760241919647,-79.3619573895282,
83.9987481020109));
#208202=CARTESIAN_POINT('Ctrl Pts',(-32.9853290938375,-79.0030528840064,
84.1342132342873));
#208203=CARTESIAN_POINT('Ctrl Pts',(-33.021684079452,-77.5778963988193,
84.5944182705371));
#208204=CARTESIAN_POINT('Ctrl Pts',(-33.0491279220084,-76.4745400156204,
84.7854247804406));
#208205=CARTESIAN_POINT('Ctrl Pts',(-33.0854694913575,-74.980465276644,
84.8309867661896));
#208206=CARTESIAN_POINT('Ctrl Pts',(-33.0946577552981,-74.5997550705373,
84.8242409289454));
#208207=CARTESIAN_POINT('Ctrl Pts',(-33.1219281605486,-73.4779330231271,
84.7501826497521));
#208208=CARTESIAN_POINT('Ctrl Pts',(-33.1401535735411,-72.7420996480677,
84.6313784846082));
#208209=CARTESIAN_POINT('Ctrl Pts',(-33.1766698348767,-71.2979296906223,
84.2561142083526));
#208210=CARTESIAN_POINT('Ctrl Pts',(-33.1945877072639,-70.5930418352839,
83.9996298991068));
#208211=CARTESIAN_POINT('Ctrl Pts',(-33.2317699618309,-69.2101394892781,
83.3422884929469));
#208212=CARTESIAN_POINT('Ctrl Pts',(-33.2510343398721,-68.5382490198549,
82.9369675079239));
#208213=CARTESIAN_POINT('Ctrl Pts',(-33.2792118147758,-67.6064602754443,
82.2404585606285));
#208214=CARTESIAN_POINT('Ctrl Pts',(-33.288360827012,-67.3127942602629,
81.9980341361255));
#208215=CARTESIAN_POINT('Ctrl Pts',(-33.3155608745428,-66.4796786165661,
81.2399013997123));
#208216=CARTESIAN_POINT('Ctrl Pts',(-33.3337527617114,-65.9767107249673,
80.6869110301534));
#208217=CARTESIAN_POINT('Ctrl Pts',(-33.3701686604761,-65.0806050801455,
79.4924500424553));
#208218=CARTESIAN_POINT('Ctrl Pts',(-33.3880046373794,-64.6897046772445,
78.8534752942746));
#208219=CARTESIAN_POINT('Ctrl Pts',(-33.425040934158,-64.0177777461935,
77.4779861533712));
#208220=CARTESIAN_POINT('Ctrl Pts',(-33.4442621241825,-63.7446205166193,
76.7416494397302));
#208221=CARTESIAN_POINT('Ctrl Pts',(-33.4816087207476,-63.3532977961105,
75.246930029432));
#208222=CARTESIAN_POINT('Ctrl Pts',(-33.4997952030726,-63.2319444456281,
74.4932135551538));
#208223=CARTESIAN_POINT('Ctrl Pts',(-33.5330374949466,-63.145545437588,
73.1283034286607));
#208224=CARTESIAN_POINT('Ctrl Pts',(-33.5478768889659,-63.1537500521688,
72.5214778149435));
#208225=CARTESIAN_POINT('Ctrl Pts',(-33.5716714747802,-63.2426134751784,
71.5395860643369));
#208226=CARTESIAN_POINT('Ctrl Pts',(-33.5807808023606,-63.2950482259868,
71.1630861392373));
#208227=CARTESIAN_POINT('Ctrl Pts',(-33.6078524042025,-63.5033517585942,
70.0591665261869));
#208228=CARTESIAN_POINT('Ctrl Pts',(-33.6259682794434,-63.7097217364428,
69.3431821095985));
#208229=CARTESIAN_POINT('Ctrl Pts',(-33.662268627147,-64.2553500527025,
67.956002829771));
#208230=CARTESIAN_POINT('Ctrl Pts',(-33.6800825137929,-64.5940375698943,
67.2881526140567));
#208231=CARTESIAN_POINT('Ctrl Pts',(-33.7157469632136,-65.3815776410118,
66.042889402939));
#208232=CARTESIAN_POINT('Ctrl Pts',(-33.7335631257147,-65.825410317655,
65.4661129362375));
#208233=CARTESIAN_POINT('Ctrl Pts',(-33.7604159462386,-66.5782982246413,
64.6543886765407));
#208234=CARTESIAN_POINT('Ctrl Pts',(-33.7695669470442,-66.8506431649004,
64.3877888125575));
#208235=CARTESIAN_POINT('Ctrl Pts',(-33.8027431449097,-67.8788358770742,
63.4741163299476));
#208236=CARTESIAN_POINT('Ctrl Pts',(-33.827142276554,-68.702601483181,62.909761785841));
#208237=CARTESIAN_POINT('Ctrl Pts',(-33.8604848528591,-69.9252189508746,
62.2812977763039));
#208238=CARTESIAN_POINT('Ctrl Pts',(-33.8696328599145,-70.2714400569454,
62.1239091781696));
#208239=CARTESIAN_POINT('Ctrl Pts',(-33.9003328092002,-71.4511997282868,
61.6547236603846));
#208240=CARTESIAN_POINT('Ctrl Pts',(-33.9221676751438,-72.312188269407,
61.4201979082925));
#208241=CARTESIAN_POINT('Ctrl Pts',(-33.9531537549127,-73.5680468611588,
61.2260707245608));
#208242=CARTESIAN_POINT('Ctrl Pts',(-33.9623540947932,-73.9474159494766,
61.1860624480864));
#208243=CARTESIAN_POINT('Ctrl Pts',(-33.9965018365887,-75.3555213748371,
61.1060247664143));
#208244=CARTESIAN_POINT('Ctrl Pts',(-34.0218448050146,-76.386231106747,
61.1818348684424));
#208245=CARTESIAN_POINT('Ctrl Pts',(-34.0561679127487,-77.7662903919399,
61.4667855037677));
#208246=CARTESIAN_POINT('Ctrl Pts',(-34.0653565323773,-78.1345758463093,
61.5615133177659));
#208247=CARTESIAN_POINT('Ctrl Pts',(-34.0974356171225,-79.3961546242934,
61.9516218303033));
#208248=CARTESIAN_POINT('Ctrl Pts',(-34.1206717596298,-80.2583404983139,
62.335518771283));
#208249=CARTESIAN_POINT('Ctrl Pts',(-34.1623554485262,-81.723868123819,
63.2098449965164));
#208250=CARTESIAN_POINT('Ctrl Pts',(-34.1808330739508,-82.3421086083129,
63.6652602467367));
#208251=CARTESIAN_POINT('Ctrl Pts',(-34.2089868550122,-83.1944678041097,
64.4309251884236));
#208252=CARTESIAN_POINT('Ctrl Pts',(-34.2183626337148,-83.464557442567,
64.6980946367148));
#208253=CARTESIAN_POINT('Ctrl Pts',(-34.2461425538805,-84.2270339569193,
65.5285647318183));
#208254=CARTESIAN_POINT('Ctrl Pts',(-34.2641935850198,-84.6794134405699,
66.1260180139622));
#208255=CARTESIAN_POINT('Ctrl Pts',(-34.2981159583491,-85.4079851892409,
67.3052775198345));
#208256=CARTESIAN_POINT('Ctrl Pts',(-34.313900770577,-85.6989464536826,
67.874476335635));
#208257=CARTESIAN_POINT('Ctrl Pts',(-34.329622639475,-85.9425570350204,
68.4641091549303));
#208258=CARTESIAN_POINT('Ctrl Pts',(-34.6308727573024,-85.9425570350204,
68.4641091549303));
#208259=CARTESIAN_POINT('Ctrl Pts',(-34.6151647072309,-85.6939094978993,
67.8622849340018));
#208260=CARTESIAN_POINT('Ctrl Pts',(-34.5995663367215,-85.3959511601958,
67.2817919716973));
#208261=CARTESIAN_POINT('Ctrl Pts',(-34.5655837556822,-84.6567913948363,
66.0942658643999));
#208262=CARTESIAN_POINT('Ctrl Pts',(-34.5472770766257,-84.2028031741042,
65.4987349189203));
#208263=CARTESIAN_POINT('Ctrl Pts',(-34.5200847301104,-83.4375414062737,
64.6705548048399));
#208264=CARTESIAN_POINT('Ctrl Pts',(-34.5109387621908,-83.1660354729899,
64.4037452541574));
#208265=CARTESIAN_POINT('Ctrl Pts',(-34.4832349145176,-82.311491216871,
63.6413270748738));
#208266=CARTESIAN_POINT('Ctrl Pts',(-34.4644736135561,-81.6928392277928,
63.1886755374939));
#208267=CARTESIAN_POINT('Ctrl Pts',(-34.4243280928122,-80.2726580978869,
62.3472785062726));
#208268=CARTESIAN_POINT('Ctrl Pts',(-34.4031687356562,-79.4621584529842,
61.9826735535439));
#208269=CARTESIAN_POINT('Ctrl Pts',(-34.3722357835602,-78.2570183909637,
61.5958290693764));
#208270=CARTESIAN_POINT('Ctrl Pts',(-34.3629147924433,-77.8900599117489,
61.497226045264));
#208271=CARTESIAN_POINT('Ctrl Pts',(-34.337168562363,-76.8605944202191,
61.2730627926405));
#208272=CARTESIAN_POINT('Ctrl Pts',(-34.3210092948498,-76.1911532203512,
61.186165893322));
#208273=CARTESIAN_POINT('Ctrl Pts',(-34.2861632365182,-74.7591331587905,
61.1234518467949));
#208274=CARTESIAN_POINT('Ctrl Pts',(-34.267431052308,-73.998867303505,61.1633186959675));
#208275=CARTESIAN_POINT('Ctrl Pts',(-34.2289629584796,-72.4393952168317,
61.396688296194));
#208276=CARTESIAN_POINT('Ctrl Pts',(-34.2093290775955,-71.6458020749369,
61.6010130650712));
#208277=CARTESIAN_POINT('Ctrl Pts',(-34.1709722898193,-70.1796190276928,
62.1452799285413));
#208278=CARTESIAN_POINT('Ctrl Pts',(-34.1525829970362,-69.5057817321438,
62.4707561695213));
#208279=CARTESIAN_POINT('Ctrl Pts',(-34.1159813265182,-68.2174115294735,
63.2509391199804));
#208280=CARTESIAN_POINT('Ctrl Pts',(-34.0974918798712,-67.607089250711,
63.705965598118));
#208281=CARTESIAN_POINT('Ctrl Pts',(-34.0693558525949,-66.7616730010462,
64.4729568089905));
#208282=CARTESIAN_POINT('Ctrl Pts',(-34.0599244964905,-66.4913589481829,
64.7431536343941));
#208283=CARTESIAN_POINT('Ctrl Pts',(-34.0276097484789,-65.6032066065503,
65.7212682687524));
#208284=CARTESIAN_POINT('Ctrl Pts',(-34.0049076937857,-65.0568073308263,
66.4892561927314));
#208285=CARTESIAN_POINT('Ctrl Pts',(-33.9723045829328,-64.424060322569,
67.648783592834));
#208286=CARTESIAN_POINT('Ctrl Pts',(-33.9628625681978,-64.2575194562051,
67.9925139798112));
#208287=CARTESIAN_POINT('Ctrl Pts',(-33.9322576319219,-63.7679958418872,
69.141282453164));
#208288=CARTESIAN_POINT('Ctrl Pts',(-33.9113051902744,-63.5167514112302,
69.9738018899385));
#208289=CARTESIAN_POINT('Ctrl Pts',(-33.8805373415329,-63.2893595333419,
71.1999775036403));
#208290=CARTESIAN_POINT('Ctrl Pts',(-33.871125158333,-63.2380909746136,
71.5768113623866));
#208291=CARTESIAN_POINT('Ctrl Pts',(-33.8344560467218,-63.1085889999484,
73.0602747704319));
#208292=CARTESIAN_POINT('Ctrl Pts',(-33.8077248650607,-63.1678490565414,
74.1731844437304));
#208293=CARTESIAN_POINT('Ctrl Pts',(-33.7708161938028,-63.454971389584,
75.6386756413624));
#208294=CARTESIAN_POINT('Ctrl Pts',(-33.7613251527993,-63.5471871944812,
76.0120184497527));
#208295=CARTESIAN_POINT('Ctrl Pts',(-33.7371337110939,-63.8308436664368,
76.9596755610859));
#208296=CARTESIAN_POINT('Ctrl Pts',(-33.7224675453935,-64.0484396335758,
77.5249930695913));
#208297=CARTESIAN_POINT('Ctrl Pts',(-33.6892264539231,-64.6300104049382,
78.7475375743631));
#208298=CARTESIAN_POINT('Ctrl Pts',(-33.6706288940634,-65.0151972562429,
79.391821109661));
#208299=CARTESIAN_POINT('Ctrl Pts',(-33.636163194024,-65.8508815439249,
80.5292250138947));
#208300=CARTESIAN_POINT('Ctrl Pts',(-33.6201123825181,-66.2872178872439,
81.0292030096662));
#208301=CARTESIAN_POINT('Ctrl Pts',(-33.5854801377261,-67.299745686989,
82.0098175581747));
#208302=CARTESIAN_POINT('Ctrl Pts',(-33.5669967213151,-67.8844164122266,
82.4776171410633));
#208303=CARTESIAN_POINT('Ctrl Pts',(-33.5395581865594,-68.8273062489169,
83.0956700600044));
#208304=CARTESIAN_POINT('Ctrl Pts',(-33.530332062025,-69.1552135967341,
83.2887023103804));
#208305=CARTESIAN_POINT('Ctrl Pts',(-33.5024933750788,-70.1651020687282,
83.8194570842563));
#208306=CARTESIAN_POINT('Ctrl Pts',(-33.4836932287862,-70.8708904003669,
84.1075957813789));
#208307=CARTESIAN_POINT('Ctrl Pts',(-33.447667681666,-72.2815996444594,
84.5305913944526));
#208308=CARTESIAN_POINT('Ctrl Pts',(-33.4305476545864,-72.980848638184,
84.6731725681769));
#208309=CARTESIAN_POINT('Ctrl Pts',(-33.394829336192,-74.4338757657504,
84.8350957688325));
#208310=CARTESIAN_POINT('Ctrl Pts',(-33.3763130781836,-75.1852996757935,
84.8471610513085));
#208311=CARTESIAN_POINT('Ctrl Pts',(-33.3391165478215,-76.7129673545317,
84.7264211013359));
#208312=CARTESIAN_POINT('Ctrl Pts',(-33.3202618390324,-77.4850989654355,
84.5875600682735));
#208313=CARTESIAN_POINT('Ctrl Pts',(-33.2917857623872,-78.6040781646242,
84.2694159652127));
#208314=CARTESIAN_POINT('Ctrl Pts',(-33.2824360030289,-78.9650573931792,
84.1476913381386));
#208315=CARTESIAN_POINT('Ctrl Pts',(-33.254062435625,-80.0476596305296,
83.7234767364529));
#208316=CARTESIAN_POINT('Ctrl Pts',(-33.2353789478727,-80.745720185765,
83.3667290671081));
#208317=CARTESIAN_POINT('Ctrl Pts',(-33.1981196430006,-82.0334725466349,
82.538687540278));
#208318=CARTESIAN_POINT('Ctrl Pts',(-33.1797147752294,-82.6235959920657,
82.0747362894187));
#208319=CARTESIAN_POINT('Ctrl Pts',(-33.1436226430351,-83.7055676849677,
81.0441385737633));
#208320=CARTESIAN_POINT('Ctrl Pts',(-33.1257258711474,-84.1954717050216,
80.4803145839738));
#208321=CARTESIAN_POINT('Ctrl Pts',(-33.0982802356823,-84.8505358131933,
79.5647026712407));
#208322=CARTESIAN_POINT('Ctrl Pts',(-33.0889699029745,-85.0569077586568,
79.2447166974648));
#208323=CARTESIAN_POINT('Ctrl Pts',(-33.0527740201786,-85.802114638911,
77.9569840754069));
#208324=CARTESIAN_POINT('Ctrl Pts',(-33.0264446693192,-86.2195444900787,
76.9255385256059));
#208325=CARTESIAN_POINT('Ctrl Pts',(-32.9901049984065,-86.5801922871778,
75.480014196472));
#208326=CARTESIAN_POINT('Ctrl Pts',(-32.9807775636815,-86.6547558852012,
75.1045569825412));
#208327=CARTESIAN_POINT('Ctrl Pts',(-32.9575906005861,-86.7960016116233,
74.1544662681952));
#208328=CARTESIAN_POINT('Ctrl Pts',(-32.9437648169816,-86.8390166478088,
73.5773273636892));
#208329=CARTESIAN_POINT('Ctrl Pts',(-32.9115049719352,-86.8406196606171,
72.2448080764105));
#208330=CARTESIAN_POINT('Ctrl Pts',(-32.8929994830291,-86.7693936347077,
71.4918945661373));
#208331=CARTESIAN_POINT('Ctrl Pts',(-32.8608659891838,-86.5182184413046,
70.1847600179599));
#208332=CARTESIAN_POINT('Ctrl Pts',(-32.8470745479927,-86.3682277994023,
69.6273248605053));
#208333=CARTESIAN_POINT('Ctrl Pts',(-32.8277666912208,-86.1054186061404,
68.874455678897));
#208334=CARTESIAN_POINT('Ctrl Pts',(-32.8224045352257,-86.0268238377811,
68.6680677523439));
#208335=CARTESIAN_POINT('Ctrl Pts',(-32.8170317104293,-85.9425570350204,
68.4641091549303));
#208336=CARTESIAN_POINT('Origin',(-64.067537349647,-83.3180213346267,69.5522455184007));
#208337=CARTESIAN_POINT('',(-63.567539947994,-92.7913234097594,65.6382900020344));
#208338=CARTESIAN_POINT('',(-64.083662457183,-92.3143114107746,65.8353741883268));
#208339=CARTESIAN_POINT('',(-64.067537349647,-92.3292133594533,65.8292137334027));
#208340=CARTESIAN_POINT('',(-63.5675399484426,-93.4410622313485,71.1605188170969));
#208341=CARTESIAN_POINT('Origin',(-63.5675399484425,-83.3180213346267,69.5522455184007));
#208342=CARTESIAN_POINT('',(-63.5676514812565,-93.4397757524445,71.1683725272602));
#208343=CARTESIAN_POINT('Ctrl Pts',(-63.5675399484426,-93.4410622313485,
71.1605188170969));
#208344=CARTESIAN_POINT('Ctrl Pts',(-63.5675771260472,-93.4406459989832,
71.1631387308018));
#208345=CARTESIAN_POINT('Ctrl Pts',(-63.5676143036518,-93.4402287495399,
71.165758482921));
#208346=CARTESIAN_POINT('Ctrl Pts',(-63.5676514812565,-93.4398104831443,
71.1683780726647));
#208347=CARTESIAN_POINT('',(-64.0597104235077,-74.2995962206461,73.2782678282931));
#208348=CARTESIAN_POINT('Ctrl Pts',(-64.0597104235077,-74.2995962206461,
73.2782678282931));
#208349=CARTESIAN_POINT('Ctrl Pts',(-64.0451218652925,-74.5739578485729,
73.9805348271195));
#208350=CARTESIAN_POINT('Ctrl Pts',(-64.0303356772116,-74.9290239136475,
74.6495330209371));
#208351=CARTESIAN_POINT('Ctrl Pts',(-64.0010809330892,-75.7845158441104,
75.8907572272979));
#208352=CARTESIAN_POINT('Ctrl Pts',(-63.986792125037,-76.2828351876858,
76.4599526620537));
#208353=CARTESIAN_POINT('Ctrl Pts',(-63.9624118992683,-77.2155184999461,
77.3072526411669));
#208354=CARTESIAN_POINT('Ctrl Pts',(-63.9525239575834,-77.616940046916,
77.6190644691922));
#208355=CARTESIAN_POINT('Ctrl Pts',(-63.9304794831546,-78.5750656316906,
78.2509947667963));
#208356=CARTESIAN_POINT('Ctrl Pts',(-63.9183841578929,-79.1431948790861,
78.5508027796503));
#208357=CARTESIAN_POINT('Ctrl Pts',(-63.8936864137597,-80.3346488432265,
79.0391399714275));
#208358=CARTESIAN_POINT('Ctrl Pts',(-63.88113511846,-80.9569483078014,79.225797709248));
#208359=CARTESIAN_POINT('Ctrl Pts',(-63.856575596689,-82.2254688239188,
79.4740442805028));
#208360=CARTESIAN_POINT('Ctrl Pts',(-63.8444614159778,-82.8688166971958,
79.5360061975211));
#208361=CARTESIAN_POINT('Ctrl Pts',(-63.8259893536362,-83.8370504105001,
79.5355609346259));
#208362=CARTESIAN_POINT('Ctrl Pts',(-63.8197844751297,-84.160856180335,
79.5196743975064));
#208363=CARTESIAN_POINT('Ctrl Pts',(-63.8012616880294,-85.1257740309717,
79.4251632815208));
#208364=CARTESIAN_POINT('Ctrl Pts',(-63.7892155220507,-85.7599874091987,
79.3000344343668));
#208365=CARTESIAN_POINT('Ctrl Pts',(-63.7646866488347,-87.0084179082139,
78.9263816821825));
#208366=CARTESIAN_POINT('Ctrl Pts',(-63.7521500622743,-87.6198341036269,
78.6758456951227));
#208367=CARTESIAN_POINT('Ctrl Pts',(-63.7273750610242,-88.7762305561875,
78.0635093820405));
#208368=CARTESIAN_POINT('Ctrl Pts',(-63.7153700975349,-89.319391665153,
77.7044378425474));
#208369=CARTESIAN_POINT('Ctrl Pts',(-63.6918930293161,-90.2944582379416,
76.9159481552165));
#208370=CARTESIAN_POINT('Ctrl Pts',(-63.6804420652402,-90.7303042794259,
76.4937784653884));
#208371=CARTESIAN_POINT('Ctrl Pts',(-63.6520134359374,-91.7183627032395,
75.3484072926959));
#208372=CARTESIAN_POINT('Ctrl Pts',(-63.6354546893578,-92.2159813549411,
74.5842894596791));
#208373=CARTESIAN_POINT('Ctrl Pts',(-63.6099369967653,-92.8025924540037,
73.3532428180121));
#208374=CARTESIAN_POINT('Ctrl Pts',(-63.6013230942664,-92.9716293745234,
72.9269478107908));
#208375=CARTESIAN_POINT('Ctrl Pts',(-63.5843894744831,-93.2500904940269,
72.0578394046302));
#208376=CARTESIAN_POINT('Ctrl Pts',(-63.5760671502839,-93.3597171145667,
71.6159185090164));
#208377=CARTESIAN_POINT('Ctrl Pts',(-63.5676866568907,-93.439665725756,
71.1683542085753));
#208378=CARTESIAN_POINT('',(-64.5675364832709,-89.3666968340079,62.5539864962095));
#208379=CARTESIAN_POINT('Ctrl Pts',(-64.5675364837199,-89.3660909400407,
62.5534304824205));
#208380=CARTESIAN_POINT('Ctrl Pts',(-64.5559053154293,-88.9428563528895,
62.1723173071129));
#208381=CARTESIAN_POINT('Ctrl Pts',(-64.5443683788522,-88.4849430424168,
61.8309194745762));
#208382=CARTESIAN_POINT('Ctrl Pts',(-64.5208921017017,-87.5084101659867,
61.2336544858132));
#208383=CARTESIAN_POINT('Ctrl Pts',(-64.5090141235672,-86.9904281121737,
60.9793895503546));
#208384=CARTESIAN_POINT('Ctrl Pts',(-64.4895980530762,-86.0950101000261,
60.6390797274405));
#208385=CARTESIAN_POINT('Ctrl Pts',(-64.4819115658727,-85.7300076639216,
60.5255089913026));
#208386=CARTESIAN_POINT('Ctrl Pts',(-64.4637503035837,-84.8594397842324,
60.3120024769304));
#208387=CARTESIAN_POINT('Ctrl Pts',(-64.4532397072825,-84.3501047911803,
60.2307861428219));
#208388=CARTESIAN_POINT('Ctrl Pts',(-64.430296409186,-83.2270828504902,
60.1455432302508));
#208389=CARTESIAN_POINT('Ctrl Pts',(-64.4181229662858,-82.6146651702382,
60.1593209414688));
#208390=CARTESIAN_POINT('Ctrl Pts',(-64.393582019433,-81.4022762304732,
60.3048983612713));
#208391=CARTESIAN_POINT('Ctrl Pts',(-64.3811840907539,-80.8041396635978,
60.4364493233302));
#208392=CARTESIAN_POINT('Ctrl Pts',(-64.3626497400445,-79.930308439577,
60.7197347739201));
#208393=CARTESIAN_POINT('Ctrl Pts',(-64.3565059984246,-79.6422585301218,
60.8290195178736));
#208394=CARTESIAN_POINT('Ctrl Pts',(-64.3381789619652,-78.7985985588575,
61.1971140003165));
#208395=CARTESIAN_POINT('Ctrl Pts',(-64.3259769456409,-78.2617699565947,
61.496240439733));
#208396=CARTESIAN_POINT('Ctrl Pts',(-64.3074536245922,-77.5038467125482,
62.0201534087068));
#208397=CARTESIAN_POINT('Ctrl Pts',(-64.3012371111907,-77.2585003728539,
62.208028559282));
#208398=CARTESIAN_POINT('Ctrl Pts',(-64.2828087450528,-76.5537998802924,
62.8043768560138));
#208399=CARTESIAN_POINT('Ctrl Pts',(-64.2707866092118,-76.1242782080949,
63.2460995920489));
#208400=CARTESIAN_POINT('Ctrl Pts',(-64.2461815857642,-75.3497322038532,
64.2130030553009));
#208401=CARTESIAN_POINT('Ctrl Pts',(-64.2336243377818,-75.0072579412108,
64.7383397323998));
#208402=CARTESIAN_POINT('Ctrl Pts',(-64.2090209000687,-74.432058347237,
65.8442881461345));
#208403=CARTESIAN_POINT('Ctrl Pts',(-64.1969313758394,-74.1995909324638,
66.4223889606873));
#208404=CARTESIAN_POINT('Ctrl Pts',(-64.1741708575269,-73.8745334008848,
67.5280676131163));
#208405=CARTESIAN_POINT('Ctrl Pts',(-64.1635849873021,-73.7669170707043,
68.0497086663743));
#208406=CARTESIAN_POINT('Ctrl Pts',(-64.1375350595926,-73.6071678749721,
69.3669952652943));
#208407=CARTESIAN_POINT('Ctrl Pts',(-64.1221954863727,-73.6095231841362,
70.1665095515026));
#208408=CARTESIAN_POINT('Ctrl Pts',(-64.0986553233582,-73.75923543564,71.3543811017856));
#208409=CARTESIAN_POINT('Ctrl Pts',(-64.0907263636134,-73.8341657884656,
71.7497160050924));
#208410=CARTESIAN_POINT('Ctrl Pts',(-64.075116934318,-74.0319672483831,
72.5260089561058));
#208411=CARTESIAN_POINT('Ctrl Pts',(-64.0674339216932,-74.1543432419635,
72.9064724931334));
#208412=CARTESIAN_POINT('Ctrl Pts',(-64.0597104235077,-74.2995962206461,
73.2782678282931));
#208413=CARTESIAN_POINT('',(-64.5675364836265,-91.7950063492917,73.2537214834819));
#208414=CARTESIAN_POINT('Origin',(-64.5675364832709,-83.3180213346267,69.5522455184007));
#208415=CARTESIAN_POINT('Ctrl Pts',(-64.567536483719,-91.7951280360208,
73.2537614015208));
#208416=CARTESIAN_POINT('Ctrl Pts',(-64.5522519075793,-91.9023782991883,
73.0463357077703));
#208417=CARTESIAN_POINT('Ctrl Pts',(-64.5369913991239,-92.0019950641991,
72.8343190083415));
#208418=CARTESIAN_POINT('Ctrl Pts',(-64.5217503919341,-92.0936164747453,
72.6182897831504));
#208419=CARTESIAN_POINT('Ctrl Pts',(-64.5065149014817,-92.1852047213892,
72.4023387533511));
#208420=CARTESIAN_POINT('Ctrl Pts',(-64.4912988981798,-92.2688032584661,
72.182378323606));
#208421=CARTESIAN_POINT('Ctrl Pts',(-64.4760978205663,-92.3440946948215,
71.9590140988965));
#208422=CARTESIAN_POINT('Ctrl Pts',(-64.4609038574466,-92.4193508928554,
71.7357544143678));
#208423=CARTESIAN_POINT('Ctrl Pts',(-64.4457248060474,-92.4863076401705,
71.5090943516248));
#208424=CARTESIAN_POINT('Ctrl Pts',(-64.4305561113083,-92.5446940249905,
71.2796630007527));
#208425=CARTESIAN_POINT('Ctrl Pts',(-64.4153929780723,-92.6030590028226,
71.0503157693915));
#208426=CARTESIAN_POINT('Ctrl Pts',(-64.4002401939035,-92.6528597945351,
70.8181995207348));
#208427=CARTESIAN_POINT('Ctrl Pts',(-64.3850932087498,-92.6938735308666,
70.5839634489218));
#208428=CARTESIAN_POINT('Ctrl Pts',(-64.3699531840988,-92.7348684201324,
70.3498350157449));
#208429=CARTESIAN_POINT('Ctrl Pts',(-64.3548189531346,-92.7670842400402,
70.113588953226));
#208430=CARTESIAN_POINT('Ctrl Pts',(-64.3396859720749,-92.7903475986798,
69.8758907034768));
#208431=CARTESIAN_POINT('Ctrl Pts',(-64.334832339477,-92.797808904247,69.7996532477571));
#208432=CARTESIAN_POINT('Ctrl Pts',(-64.3299788354556,-92.8043496620271,
69.7232665234059));
#208433=CARTESIAN_POINT('Ctrl Pts',(-64.3251253100959,-92.809965244465,
69.6467527948062));
#208434=CARTESIAN_POINT('Ctrl Pts',(-64.3100488689152,-92.8274088533978,
69.4090792187455));
#208435=CARTESIAN_POINT('Ctrl Pts',(-64.2949725167306,-92.8359213053789,
69.1701838191067));
#208436=CARTESIAN_POINT('Ctrl Pts',(-64.2798981906764,-92.8353917560586,
68.9307425222424));
#208437=CARTESIAN_POINT('Ctrl Pts',(-64.2648429722307,-92.8348628779736,
68.6916047315219));
#208438=CARTESIAN_POINT('Ctrl Pts',(-64.2497897747822,-92.8253148473759,
68.4519226836682));
#208439=CARTESIAN_POINT('Ctrl Pts',(-64.2347405281082,-92.8066882622084,
68.2123797226621));
#208440=CARTESIAN_POINT('Ctrl Pts',(-64.2197180065402,-92.7880947549398,
67.9732621524508));
#208441=CARTESIAN_POINT('Ctrl Pts',(-64.2046994217271,-92.7604548736204,
67.7342834363879));
#208442=CARTESIAN_POINT('Ctrl Pts',(-64.1896866931837,-92.723761103761,
67.4961293606001));
#208443=CARTESIAN_POINT('Ctrl Pts',(-64.1746906332506,-92.6871080749401,
67.2582397069306));
#208444=CARTESIAN_POINT('Ctrl Pts',(-64.1597004165899,-92.641421230613,
67.0211731258062));
#208445=CARTESIAN_POINT('Ctrl Pts',(-64.1447179563298,-92.5867450112611,
66.7856152711169));
#208446=CARTESIAN_POINT('Ctrl Pts',(-64.1297582205193,-92.5321517213465,
66.550414695709));
#208447=CARTESIAN_POINT('Ctrl Pts',(-64.1148062175984,-92.4685963074583,
66.3167185364763));
#208448=CARTESIAN_POINT('Ctrl Pts',(-64.099863852003,-92.3961749399324,
66.0852075409147));
#208449=CARTESIAN_POINT('Ctrl Pts',(-64.0944699454781,-92.3700322194679,
66.0016365252302));
#208450=CARTESIAN_POINT('Ctrl Pts',(-64.0890772947653,-92.3427346928514,
65.9183502156652));
#208451=CARTESIAN_POINT('Ctrl Pts',(-64.0836859894461,-92.3142885460423,
65.8353804738359));
#208452=CARTESIAN_POINT('Origin',(-64.067537349647,-83.3180213346267,69.5522455184007));
#208453=CARTESIAN_POINT('',(-63.567539947994,-86.5649230506972,59.8300991896837));
#208454=CARTESIAN_POINT('Ctrl Pts',(-64.0833825702184,-92.3145833582915,
65.8352994300243));
#208455=CARTESIAN_POINT('Ctrl Pts',(-64.0619309619701,-92.2034972449534,
65.5102458841647));
#208456=CARTESIAN_POINT('Ctrl Pts',(-64.0405438036779,-92.0753868183421,
65.1915387606872));
#208457=CARTESIAN_POINT('Ctrl Pts',(-63.9975780848989,-91.7816127980817,
64.5599055048843));
#208458=CARTESIAN_POINT('Ctrl Pts',(-63.9760783705587,-91.6154651381155,
64.2483770552222));
#208459=CARTESIAN_POINT('Ctrl Pts',(-63.911488627533,-91.061916651673,63.3334815420053));
#208460=CARTESIAN_POINT('Ctrl Pts',(-63.8686493908154,-90.6225744631808,
62.7604124769523));
#208461=CARTESIAN_POINT('Ctrl Pts',(-63.803886666834,-89.8898307925944,
61.9886376949778));
#208462=CARTESIAN_POINT('Ctrl Pts',(-63.7825040517021,-89.6341955601574,
61.7463822267544));
#208463=CARTESIAN_POINT('Ctrl Pts',(-63.6782847466946,-88.314927314397,
60.6228146595869));
#208464=CARTESIAN_POINT('Ctrl Pts',(-63.6137547901258,-87.2878515244266,
60.1202593968735));
#208465=CARTESIAN_POINT('Ctrl Pts',(-63.567539947994,-86.5649230506972,
59.8300991896837));
#208466=CARTESIAN_POINT('Origin',(-63.5675399484425,-83.3180213346267,69.5522455184007));
#208467=CARTESIAN_POINT('Origin',(-33.9082782203809,-78.4305456687161,71.5715374392095));
#208468=CARTESIAN_POINT('',(-48.5675364832709,-86.6057727049752,68.1938899513175));
#208469=CARTESIAN_POINT('Origin',(-48.5675364832709,-82.0608411004817,70.0716575959921));
#208470=CARTESIAN_POINT('',(-38.5675364832709,-84.1293203724861,69.217052117043));
#208471=CARTESIAN_POINT('',(-32.6788877561441,-82.6710245849397,69.8195563755257));
#208472=CARTESIAN_POINT('Origin',(-38.5675364832709,-79.5843887679945,71.0948197617183));
#208473=CARTESIAN_POINT('Origin',(-33.5526503323277,-74.999949493375,72.9851176492631));
#208474=CARTESIAN_POINT('Ctrl Pts',(-32.8170317104293,-85.9425570350204,
68.4641091549303));
#208475=CARTESIAN_POINT('Ctrl Pts',(-32.8017220003837,-85.7024411991933,
67.8829349856529));
#208476=CARTESIAN_POINT('Ctrl Pts',(-32.7863496420861,-85.4162708021334,
67.3214853189258));
#208477=CARTESIAN_POINT('Ctrl Pts',(-32.7608347605554,-84.8617909280881,
66.4194041046769));
#208478=CARTESIAN_POINT('Ctrl Pts',(-32.7505255297521,-84.6172361447456,
66.0661359314734));
#208479=CARTESIAN_POINT('Ctrl Pts',(-32.7296708098251,-84.0889065869639,
65.3852438569607));
#208480=CARTESIAN_POINT('Ctrl Pts',(-32.7191392839043,-83.8052559543857,
65.0583404901236));
#208481=CARTESIAN_POINT('Ctrl Pts',(-32.7085755548516,-83.5043603266795,
64.7476924450699));
#208482=CARTESIAN_POINT('Ctrl Pts',(-32.405898694983,-83.5044136926724,
64.7477475410809));
#208483=CARTESIAN_POINT('Ctrl Pts',(-32.4327410348547,-84.2718992350309,
65.5401185566776));
#208484=CARTESIAN_POINT('Ctrl Pts',(-32.4600251083934,-84.9248984032721,
66.4358827107567));
#208485=CARTESIAN_POINT('Ctrl Pts',(-32.4959705871775,-85.6172563043794,
67.7327251559588));
#208486=CARTESIAN_POINT('Ctrl Pts',(-32.5048857483552,-85.7749346554537,
68.0642918789659));
#208487=CARTESIAN_POINT('Ctrl Pts',(-32.5143827756658,-85.9255506318068,
68.4231104132923));
#208488=CARTESIAN_POINT('Ctrl Pts',(-32.5149245145407,-85.9340829810812,
68.4435986323621));
#208489=CARTESIAN_POINT('Ctrl Pts',(-32.5154663303127,-85.9425570386429,
68.4641091636981));
#208490=CARTESIAN_POINT('Origin',(-27.5423496375577,-74.9965420974961,72.9903965241317));
#208491=CARTESIAN_POINT('',(-26.6969350937309,-64.1107405695911,68.3402735649356));
#208492=CARTESIAN_POINT('Ctrl Pts',(-27.3723203523406,-85.9391496445663,
68.4693880429103));
#208493=CARTESIAN_POINT('Ctrl Pts',(-27.3636996501605,-85.8050962805345,
68.1449265076006));
#208494=CARTESIAN_POINT('Ctrl Pts',(-27.3551097818568,-85.656602913772,
67.8264054854172));
#208495=CARTESIAN_POINT('Ctrl Pts',(-27.328549170573,-85.1502905081774,
66.8557319008512));
#208496=CARTESIAN_POINT('Ctrl Pts',(-27.3106304021217,-84.7452160106694,
66.230509408506));
#208497=CARTESIAN_POINT('Ctrl Pts',(-27.2831300851529,-84.0481868827491,
65.3488832284206));
#208498=CARTESIAN_POINT('Ctrl Pts',(-27.2737850478675,-83.7979132654584,
65.0619121673232));
#208499=CARTESIAN_POINT('Ctrl Pts',(-27.2366922027447,-82.7456789989978,
63.9667298171809));
#208500=CARTESIAN_POINT('Ctrl Pts',(-27.2095390063064,-81.8428519134459,
63.2639518915619));
#208501=CARTESIAN_POINT('Ctrl Pts',(-27.172318717458,-80.5203041019529,
62.5111129725245));
#208502=CARTESIAN_POINT('Ctrl Pts',(-27.1629537869745,-80.1778991930004,
62.337656384572));
#208503=CARTESIAN_POINT('Ctrl Pts',(-27.1380744267044,-79.2384073982333,
61.9177563454446));
#208504=CARTESIAN_POINT('Ctrl Pts',(-27.1225970943958,-78.6285864215056,
61.7030125447275));
#208505=CARTESIAN_POINT('Ctrl Pts',(-27.0887288513523,-77.2810534975722,
61.3490746452831));
#208506=CARTESIAN_POINT('Ctrl Pts',(-27.0703984326144,-76.5414194989774,
61.2280527602506));
#208507=CARTESIAN_POINT('Ctrl Pts',(-27.0432293521299,-75.4168264097566,
61.1520074257193));
#208508=CARTESIAN_POINT('Ctrl Pts',(-27.0341195638503,-75.0373145881522,
61.1446195136914));
#208509=CARTESIAN_POINT('Ctrl Pts',(-27.0064444237393,-73.8919104087149,
61.1773740424248));
#208510=CARTESIAN_POINT('Ctrl Pts',(-26.9876862066823,-73.1296576224682,
61.2736375504651));
#208511=CARTESIAN_POINT('Ctrl Pts',(-26.9501334588134,-71.6199605337841,
61.6154471013317));
#208512=CARTESIAN_POINT('Ctrl Pts',(-26.9315328934326,-70.8767923732291,
61.8630228528093));
#208513=CARTESIAN_POINT('Ctrl Pts',(-26.8944219015646,-69.4809320174234,
62.4871971090572));
#208514=CARTESIAN_POINT('Ctrl Pts',(-26.8761197995314,-68.8288518195583,
62.8563569561091));
#208515=CARTESIAN_POINT('Ctrl Pts',(-26.8450525151973,-67.7713377025379,
63.5951446125017));
#208516=CARTESIAN_POINT('Ctrl Pts',(-26.8320439690496,-67.3485935572221,
63.9359379853444));
#208517=CARTESIAN_POINT('Ctrl Pts',(-26.7989683136381,-66.3479106000214,
64.862881895046));
#208518=CARTESIAN_POINT('Ctrl Pts',(-26.7788449346443,-65.8048753902868,
65.482494524121));
#208519=CARTESIAN_POINT('Ctrl Pts',(-26.7490196891172,-65.0898279948038,
66.4934183077934));
#208520=CARTESIAN_POINT('Ctrl Pts',(-26.7390111532609,-64.8673881345169,
66.8459722428458));
#208521=CARTESIAN_POINT('Ctrl Pts',(-26.7187614620685,-64.4589394460568,
67.5760192654688));
#208522=CARTESIAN_POINT('Ctrl Pts',(-26.7085329599487,-64.2735326518323,
67.9531735113464));
#208523=CARTESIAN_POINT('Ctrl Pts',(-26.6982749890421,-64.1085581679634,
68.3393768975646));
#208524=CARTESIAN_POINT('',(-26.3969350937309,-64.1107405695911,68.3402735649356));
#208525=CARTESIAN_POINT('Origin',(-26.5469350937313,-53.5544436394318,63.827825737551));
#208526=CARTESIAN_POINT('Ctrl Pts',(-26.3955978506944,-64.1085838121623,
68.3393168652453));
#208527=CARTESIAN_POINT('Ctrl Pts',(-26.4061671472431,-64.2792160622287,
67.9398748093981));
#208528=CARTESIAN_POINT('Ctrl Pts',(-26.416751543022,-64.4717000818231,
67.5501256478087));
#208529=CARTESIAN_POINT('Ctrl Pts',(-26.4379920407315,-64.8967289793553,
66.7969093671376));
#208530=CARTESIAN_POINT('Ctrl Pts',(-26.4486306576851,-65.1285860795737,
66.4338005620371));
#208531=CARTESIAN_POINT('Ctrl Pts',(-26.4802936890649,-65.8773839632651,
65.391114314244));
#208532=CARTESIAN_POINT('Ctrl Pts',(-26.5008584501326,-66.4485211602495,
64.7539243141916));
#208533=CARTESIAN_POINT('Ctrl Pts',(-26.5358514447633,-67.5086683138891,
63.8013175177357));
#208534=CARTESIAN_POINT('Ctrl Pts',(-26.5500252944045,-67.9613287414215,
63.4503128844906));
#208535=CARTESIAN_POINT('Ctrl Pts',(-26.5826993387652,-69.0658984231094,
62.7153186995669));
#208536=CARTESIAN_POINT('Ctrl Pts',(-26.6009119883849,-69.7327527302829,
62.3582621384974));
#208537=CARTESIAN_POINT('Ctrl Pts',(-26.633610456032,-70.9611934406892,
61.844597299696));
#208538=CARTESIAN_POINT('Ctrl Pts',(-26.6479050391863,-71.5088946671322,
61.6612663526489));
#208539=CARTESIAN_POINT('Ctrl Pts',(-26.6715385593391,-72.4384356559061,
61.423952871691));
#208540=CARTESIAN_POINT('Ctrl Pts',(-26.6808599172737,-72.8134705822262,
61.3473416619736));
#208541=CARTESIAN_POINT('Ctrl Pts',(-26.7171740780291,-74.2854742744447,
61.1202789821206));
#208542=CARTESIAN_POINT('Ctrl Pts',(-26.7445727229865,-75.3976699648159,
61.1057679952971));
#208543=CARTESIAN_POINT('Ctrl Pts',(-26.7809426339764,-76.8730935556046,
61.2940917902757));
#208544=CARTESIAN_POINT('Ctrl Pts',(-26.7901838568864,-77.248031044884,
61.3604443251686));
#208545=CARTESIAN_POINT('Ctrl Pts',(-26.8176517904024,-78.3458986357085,
61.6098232698253));
#208546=CARTESIAN_POINT('Ctrl Pts',(-26.8360248015145,-79.0554657440672,
61.8431652991705));
#208547=CARTESIAN_POINT('Ctrl Pts',(-26.8728273181899,-80.4246542834376,
62.4416171656125));
#208548=CARTESIAN_POINT('Ctrl Pts',(-26.8908787881403,-81.0809298958973,
62.8060274152493));
#208549=CARTESIAN_POINT('Ctrl Pts',(-26.9283004549172,-82.3430537141758,
63.6726441225342));
#208550=CARTESIAN_POINT('Ctrl Pts',(-26.9476729115514,-82.9422950610507,
64.1780896202315));
#208551=CARTESIAN_POINT('Ctrl Pts',(-26.9760265130458,-83.7526521547964,
65.0119463436013));
#208552=CARTESIAN_POINT('Ctrl Pts',(-26.9852398453103,-84.0046681677395,
65.297620929492));
#208553=CARTESIAN_POINT('Ctrl Pts',(-27.0126466015813,-84.7090334743622,
66.1782317810865));
#208554=CARTESIAN_POINT('Ctrl Pts',(-27.0309784936996,-85.1193421781366,
66.804365126236));
#208555=CARTESIAN_POINT('Ctrl Pts',(-27.0583910322376,-85.6407014240736,
67.792404142075));
#208556=CARTESIAN_POINT('Ctrl Pts',(-27.0673916524933,-85.7979333834112,
68.1275894981264));
#208557=CARTESIAN_POINT('Ctrl Pts',(-27.0763524854127,-85.9391496391481,
68.4693880297962));
#208558=CARTESIAN_POINT('Origin',(-49.8209604129909,-85.5885787240481,68.6141501690631));
#208559=CARTESIAN_POINT('',(-47.4206117411878,-74.8936030761356,65.7294283639651));
#208560=CARTESIAN_POINT('',(-47.4206117411893,-80.0485688784053,78.2064603659041));
#208561=CARTESIAN_POINT('Ctrl Pts',(-47.4206117411876,-74.8936030761362,
65.729428363968));
#208562=CARTESIAN_POINT('Ctrl Pts',(-47.4072073505217,-74.5345429245089,
66.753376001073));
#208563=CARTESIAN_POINT('Ctrl Pts',(-47.3965597695574,-74.3257849510905,
67.8789541701247));
#208564=CARTESIAN_POINT('Ctrl Pts',(-47.3802442358666,-74.2939613105297,
70.3818352645528));
#208565=CARTESIAN_POINT('Ctrl Pts',(-47.3761425330335,-74.5723128478446,
71.7610264219768));
#208566=CARTESIAN_POINT('Ctrl Pts',(-47.3761425330335,-75.0680041243238,
72.9607930464209));
#208567=CARTESIAN_POINT('Ctrl Pts',(-47.3761425330335,-75.563695400803,
74.1605596708651));
#208568=CARTESIAN_POINT('Ctrl Pts',(-47.3802442358666,-76.3399893287414,
75.3340227356814));
#208569=CARTESIAN_POINT('Ctrl Pts',(-47.3965597695574,-78.1291388445427,
77.0845570904024));
#208570=CARTESIAN_POINT('Ctrl Pts',(-47.4072073505217,-79.0714850594923,
77.7345491805734));
#208571=CARTESIAN_POINT('Ctrl Pts',(-47.4206117411876,-80.0485688784058,
78.2064603659031));
#208572=CARTESIAN_POINT('',(-40.481003278332,-78.3300079219658,78.9164948483172));
#208573=CARTESIAN_POINT('',(-47.4206117411909,-80.0485688784039,78.2064603659047));
#208574=CARTESIAN_POINT('',(-40.5852420615047,-72.8362530306906,67.7517760446658));
#208575=CARTESIAN_POINT('Ctrl Pts',(-40.4810032783342,-78.3300079219668,
78.9164948483157));
#208576=CARTESIAN_POINT('Ctrl Pts',(-40.5701001577907,-77.3783739218292,
78.4341281348452));
#208577=CARTESIAN_POINT('Ctrl Pts',(-40.6461218070977,-76.4640165146777,
77.7789779463358));
#208578=CARTESIAN_POINT('Ctrl Pts',(-40.7676642501064,-74.7061160640781,
76.0175731138598));
#208579=CARTESIAN_POINT('Ctrl Pts',(-40.8007888323695,-73.936268721286,
74.8355718846972));
#208580=CARTESIAN_POINT('Ctrl Pts',(-40.8007888323695,-73.4396491234305,
73.6335583596984));
#208581=CARTESIAN_POINT('Ctrl Pts',(-40.8007888323695,-72.943029525575,
72.4315448346997));
#208582=CARTESIAN_POINT('Ctrl Pts',(-40.7676642501064,-72.6540848575873,
71.0508555808169));
#208583=CARTESIAN_POINT('Ctrl Pts',(-40.668740252843,-72.6557245993737,
69.0254326994105));
#208584=CARTESIAN_POINT('Ctrl Pts',(-40.6299225890052,-72.7174361037414,
68.3789914813538));
#208585=CARTESIAN_POINT('Ctrl Pts',(-40.5852420615047,-72.8362530306906,
67.7517760446658));
#208586=CARTESIAN_POINT('',(-40.481003278332,-73.1750421196974,66.4394628463787));
#208587=CARTESIAN_POINT('Ctrl Pts',(-40.5852420615047,-72.8362530306906,
67.7517760446658));
#208588=CARTESIAN_POINT('Ctrl Pts',(-40.5532232597647,-72.9213991970445,
67.3023031346757));
#208589=CARTESIAN_POINT('Ctrl Pts',(-40.5182082030456,-73.0357162226427,
66.8626329204887));
#208590=CARTESIAN_POINT('Ctrl Pts',(-40.481003278349,-73.175042119644,66.4394628465471));
#208591=CARTESIAN_POINT('',(-47.4206117411909,-74.8936030761349,65.7294283639646));
#208592=CARTESIAN_POINT('Origin',(-64.4265543961493,-83.3237128444373,69.5530424137804));
#208593=CARTESIAN_POINT('',(-64.5675364832711,-90.9537820568269,64.6166308207583));
#208594=CARTESIAN_POINT('Origin',(-64.5675364832709,-83.3237128444373,69.5530424137804));
#208595=CARTESIAN_POINT('',(-63.7081759237673,-74.9246006814762,73.0230612142441));
#208596=CARTESIAN_POINT('Ctrl Pts',(-64.5675364832717,-90.9537820568266,
64.6166308207584));
#208597=CARTESIAN_POINT('Ctrl Pts',(-64.5460054318702,-90.585927916916,
64.0480492722608));
#208598=CARTESIAN_POINT('Ctrl Pts',(-64.5242151510805,-90.1556468171482,
63.5223301109441));
#208599=CARTESIAN_POINT('Ctrl Pts',(-64.4802433842162,-89.1769113772055,
62.5671481746464));
#208600=CARTESIAN_POINT('Ctrl Pts',(-64.4585326795741,-88.629546564504,
62.142861546234));
#208601=CARTESIAN_POINT('Ctrl Pts',(-64.4216367999337,-87.647267127443,
61.5465778287499));
#208602=CARTESIAN_POINT('Ctrl Pts',(-64.4067804331069,-87.2376250724316,
61.3385500692314));
#208603=CARTESIAN_POINT('Ctrl Pts',(-64.3730365308061,-86.269447621911,
60.9358123869345));
#208604=CARTESIAN_POINT('Ctrl Pts',(-64.3544190590795,-85.7041004997053,
60.7628340472615));
#208605=CARTESIAN_POINT('Ctrl Pts',(-64.3166439831112,-84.5496212266027,
60.529236790111));
#208606=CARTESIAN_POINT('Ctrl Pts',(-64.2975574490637,-83.9632945784081,
60.4688337160353));
#208607=CARTESIAN_POINT('Ctrl Pts',(-64.2597495591603,-82.7850337136813,
60.4621504002003));
#208608=CARTESIAN_POINT('Ctrl Pts',(-64.241099252248,-82.1958827798751,
60.5163118771831));
#208609=CARTESIAN_POINT('Ctrl Pts',(-64.2031978910308,-81.0370119978244,
60.7380099725469));
#208610=CARTESIAN_POINT('Ctrl Pts',(-64.184061183931,-80.47002321394,60.9049062666254));
#208611=CARTESIAN_POINT('Ctrl Pts',(-64.1557944571638,-79.6496879702633,
61.2359124218976));
#208612=CARTESIAN_POINT('Ctrl Pts',(-64.146429116728,-79.3817015131536,
61.3595292794478));
#208613=CARTESIAN_POINT('Ctrl Pts',(-64.1276217352215,-78.8585717954617,
61.632454540492));
#208614=CARTESIAN_POINT('Ctrl Pts',(-64.1181904779767,-78.6037471974636,
61.7816127007718));
#208615=CARTESIAN_POINT('Ctrl Pts',(-64.0897741094685,-77.8630385676629,
62.2650675446127));
#208616=CARTESIAN_POINT('Ctrl Pts',(-64.0707214808186,-77.4019527181837,
62.6344941894086));
#208617=CARTESIAN_POINT('Ctrl Pts',(-64.0332160558767,-76.5577457470272,
63.4575197792184));
#208618=CARTESIAN_POINT('Ctrl Pts',(-64.014559870328,-76.176647047462,63.9091824285621));
#208619=CARTESIAN_POINT('Ctrl Pts',(-63.9767300455895,-75.5073339613555,
64.879936482934));
#208620=CARTESIAN_POINT('Ctrl Pts',(-63.9578042896901,-75.2207011334582,
65.3967325233348));
#208621=CARTESIAN_POINT('Ctrl Pts',(-63.9297910614553,-74.868773083817,
66.2083219024605));
#208622=CARTESIAN_POINT('Ctrl Pts',(-63.9204656552382,-74.7646490456164,
66.4845593731605));
#208623=CARTESIAN_POINT('Ctrl Pts',(-63.8941532883584,-74.5106147379155,
67.2727750530024));
#208624=CARTESIAN_POINT('Ctrl Pts',(-63.8770605769487,-74.3920488100204,
67.7935855420457));
#208625=CARTESIAN_POINT('Ctrl Pts',(-63.8344751232087,-74.2113796600219,
69.1147594772959));
#208626=CARTESIAN_POINT('Ctrl Pts',(-63.80958636877,-74.2081727225401,69.9186094113973));
#208627=CARTESIAN_POINT('Ctrl Pts',(-63.7713711901282,-74.3613121332033,
71.1091500668453));
#208628=CARTESIAN_POINT('Ctrl Pts',(-63.7585739829314,-74.438475725743,
71.5020572684976));
#208629=CARTESIAN_POINT('Ctrl Pts',(-63.7332377069486,-74.6439667049617,
72.2747690093804));
#208630=CARTESIAN_POINT('Ctrl Pts',(-63.7207474086347,-74.772021110162,
72.6537453670004));
#208631=CARTESIAN_POINT('Ctrl Pts',(-63.7081759237673,-74.9246006814762,
73.0230612142441));
#208632=CARTESIAN_POINT('Ctrl Pts',(-63.7081759237673,-74.9246006814762,
73.0230612142441));
#208633=CARTESIAN_POINT('Ctrl Pts',(-63.6875161657485,-75.1753472762659,
73.6299884083669));
#208634=CARTESIAN_POINT('Ctrl Pts',(-63.666633096272,-75.4911431224059,
74.2079528890717));
#208635=CARTESIAN_POINT('Ctrl Pts',(-63.6250338178037,-76.2415525476808,
75.2853977476081));
#208636=CARTESIAN_POINT('Ctrl Pts',(-63.6047129064916,-76.6739032033415,
75.7817602801854));
#208637=CARTESIAN_POINT('Ctrl Pts',(-63.5702347770154,-77.4769637327139,
76.5238902708087));
#208638=CARTESIAN_POINT('Ctrl Pts',(-63.5563499250238,-77.8189848016841,
76.7970165522735));
#208639=CARTESIAN_POINT('Ctrl Pts',(-63.5238782363532,-78.6651834829525,
77.3781042268529));
#208640=CARTESIAN_POINT('Ctrl Pts',(-63.5056266428151,-79.1823446748094,
77.6636872419475));
#208641=CARTESIAN_POINT('Ctrl Pts',(-63.4686546174705,-80.2639002161587,
78.1303410844429));
#208642=CARTESIAN_POINT('Ctrl Pts',(-63.4499671432275,-80.8256634980915,
78.3104533209256));
#208643=CARTESIAN_POINT('Ctrl Pts',(-63.4128436371221,-81.9770369928399,
78.5597118792829));
#208644=CARTESIAN_POINT('Ctrl Pts',(-63.3946215167477,-82.5639656279161,
78.6280860916995));
#208645=CARTESIAN_POINT('Ctrl Pts',(-63.3575823140899,-83.7422255350564,
78.6501758674783));
#208646=CARTESIAN_POINT('Ctrl Pts',(-63.3388446223193,-84.3307600947913,
78.6039452830317));
#208647=CARTESIAN_POINT('Ctrl Pts',(-63.3018702281337,-85.4898411231714,
78.3983799325527));
#208648=CARTESIAN_POINT('Ctrl Pts',(-63.2836465012631,-86.0576752351604,
78.2396736254702));
#208649=CARTESIAN_POINT('Ctrl Pts',(-63.2465196644465,-87.1559936228692,
77.8142404149129));
#208650=CARTESIAN_POINT('Ctrl Pts',(-63.2277373367691,-87.6837798863797,
77.5482653071632));
#208651=CARTESIAN_POINT('Ctrl Pts',(-63.1907483518579,-88.6799825607429,
76.9180689523048));
#208652=CARTESIAN_POINT('Ctrl Pts',(-63.1724068011774,-89.1460822825508,
76.5554173534264));
#208653=CARTESIAN_POINT('Ctrl Pts',(-63.1350988645249,-90.0016677266875,
75.7448462794557));
#208654=CARTESIAN_POINT('Ctrl Pts',(-63.1163171878295,-90.3890983500231,
75.2988106682674));
#208655=CARTESIAN_POINT('Ctrl Pts',(-63.0840698114675,-90.9838957856484,
74.4620982013951));
#208656=CARTESIAN_POINT('Ctrl Pts',(-63.070383528129,-91.2111472462665,
74.0879744284651));
#208657=CARTESIAN_POINT('Ctrl Pts',(-63.03575802426,-91.710095712682,73.1147421819726));
#208658=CARTESIAN_POINT('Ctrl Pts',(-63.0147220449659,-91.9454177103888,
72.499792039988));
#208659=CARTESIAN_POINT('Ctrl Pts',(-62.9836482387311,-92.1959506361543,
71.5473602390956));
#208660=CARTESIAN_POINT('Ctrl Pts',(-62.973330254332,-92.2622035221039,
71.2255528877244));
#208661=CARTESIAN_POINT('Ctrl Pts',(-62.9525789218377,-92.359488578991,
70.576864601696));
#208662=CARTESIAN_POINT('Ctrl Pts',(-62.9421606938526,-92.3905227868185,
70.2504729419997));
#208663=CARTESIAN_POINT('Ctrl Pts',(-62.931689741507,-92.4038646207268,
69.9231225687745));
#208664=CARTESIAN_POINT('',(-63.5151079737573,-74.9246636583587,73.0232136446285));
#208665=CARTESIAN_POINT('Ctrl Pts',(-63.5151079737573,-74.9246636583587,
73.0232136446285));
#208666=CARTESIAN_POINT('Ctrl Pts',(-63.4816571263961,-75.3228894994488,
73.9870618826492));
#208667=CARTESIAN_POINT('Ctrl Pts',(-63.4492397722482,-75.8840734303081,
74.875210590161));
#208668=CARTESIAN_POINT('Ctrl Pts',(-63.3824771659967,-77.266723687465,
76.4040445924905));
#208669=CARTESIAN_POINT('Ctrl Pts',(-63.3506340024212,-78.0719900071899,
77.0392102609248));
#208670=CARTESIAN_POINT('Ctrl Pts',(-63.2990803050339,-79.4817485896302,
77.8096342034867));
#208671=CARTESIAN_POINT('Ctrl Pts',(-63.2798627012716,-80.0239904395514,
78.0409065795314));
#208672=CARTESIAN_POINT('Ctrl Pts',(-63.2420148814413,-81.1452204755426,
78.3953145837462));
#208673=CARTESIAN_POINT('Ctrl Pts',(-63.2234726310312,-81.7215382041962,
78.5176753341718));
#208674=CARTESIAN_POINT('Ctrl Pts',(-63.1860449875657,-82.8898402949109,
78.649388820796));
#208675=CARTESIAN_POINT('Ctrl Pts',(-63.166902594635,-83.4790642592849,
78.6584039746957));
#208676=CARTESIAN_POINT('Ctrl Pts',(-63.1287565369763,-84.654596635391,
78.5621938389019));
#208677=CARTESIAN_POINT('Ctrl Pts',(-63.1099545802623,-85.238071552627,
78.4564857219072));
#208678=CARTESIAN_POINT('Ctrl Pts',(-63.0536399237439,-86.946444137016,
77.9711620727516));
#208679=CARTESIAN_POINT('Ctrl Pts',(-63.0151488836941,-88.0115737252524,
77.427869310999));
#208680=CARTESIAN_POINT('Ctrl Pts',(-62.9590083227095,-89.4046245324071,
76.3320095448116));
#208681=CARTESIAN_POINT('Ctrl Pts',(-62.940472460623,-89.8304017391483,
75.924453235268));
#208682=CARTESIAN_POINT('Ctrl Pts',(-62.9051701193412,-90.5438883000852,
75.0948322057969));
#208683=CARTESIAN_POINT('Ctrl Pts',(-62.8888430717836,-90.841321814152,
74.6841176910583));
#208684=CARTESIAN_POINT('Ctrl Pts',(-62.8485304202398,-91.4962742448335,
73.5995381859555));
#208685=CARTESIAN_POINT('Ctrl Pts',(-62.8249536297514,-91.8062103136783,
72.9014933147706));
#208686=CARTESIAN_POINT('Ctrl Pts',(-62.7883176531253,-92.1355141820709,
71.8077665761614));
#208687=CARTESIAN_POINT('Ctrl Pts',(-62.7760361700276,-92.2223818534238,
71.4359434158888));
#208688=CARTESIAN_POINT('Ctrl Pts',(-62.7516832489389,-92.3488415221792,
70.6837669566824));
#208689=CARTESIAN_POINT('Ctrl Pts',(-62.7396359874419,-92.3883312692993,
70.3041626149918));
#208690=CARTESIAN_POINT('Ctrl Pts',(-62.7276560748581,-92.4038614347471,
69.9232007305413));
#208691=CARTESIAN_POINT('Ctrl Pts',(-64.4174334691588,-91.7227797420337,
66.0829140514177));
#208692=CARTESIAN_POINT('Ctrl Pts',(-64.4028363514007,-91.5481748019053,
65.6603018539285));
#208693=CARTESIAN_POINT('Ctrl Pts',(-64.3882540732041,-91.3419199834527,
65.25146519838));
#208694=CARTESIAN_POINT('Ctrl Pts',(-64.3594594374539,-90.8700985124793,
64.4691034471845));
#208695=CARTESIAN_POINT('Ctrl Pts',(-64.3452859566336,-90.6053241305171,
64.0966231570146));
#208696=CARTESIAN_POINT('Ctrl Pts',(-64.3026020461293,-89.7311263547494,
63.0444153206984));
#208697=CARTESIAN_POINT('Ctrl Pts',(-64.2733419917296,-89.0463574965084,
62.4348613897139));
#208698=CARTESIAN_POINT('Ctrl Pts',(-64.2264360277325,-87.792722421711,
61.6185905971474));
#208699=CARTESIAN_POINT('Ctrl Pts',(-64.2084844170692,-87.2734286352503,
61.3477206114525));
#208700=CARTESIAN_POINT('Ctrl Pts',(-64.1715858830551,-86.1859714638437,
60.9078008299014));
#208701=CARTESIAN_POINT('Ctrl Pts',(-64.1527333829351,-85.620035237133,
60.740571750952));
#208702=CARTESIAN_POINT('Ctrl Pts',(-64.1156388678732,-84.4646051052493,
60.5181037819277));
#208703=CARTESIAN_POINT('Ctrl Pts',(-64.0974824423265,-83.8778773028571,
60.4632320055774));
#208704=CARTESIAN_POINT('Ctrl Pts',(-64.0608178975356,-82.7021876861606,
60.4675969790405));
#208705=CARTESIAN_POINT('Ctrl Pts',(-64.0420536917397,-82.1160066425151,
60.5268008159321));
#208706=CARTESIAN_POINT('Ctrl Pts',(-64.0046823853952,-80.9606971107092,
60.758105192194));
#208707=CARTESIAN_POINT('Ctrl Pts',(-63.9862707238914,-80.3943936764082,
60.9301738347671));
#208708=CARTESIAN_POINT('Ctrl Pts',(-63.9309385982088,-78.7527241764439,
61.6095368533426));
#208709=CARTESIAN_POINT('Ctrl Pts',(-63.8929716043318,-77.7559989133136,
62.2733600379412));
#208710=CARTESIAN_POINT('Ctrl Pts',(-63.8466555962397,-76.7059823331835,
63.3177676912197));
#208711=CARTESIAN_POINT('Ctrl Pts',(-63.837474495331,-76.5072261967547,
63.53569111148));
#208712=CARTESIAN_POINT('Ctrl Pts',(-63.8096802790241,-75.9433278344253,
64.2178338595459));
#208713=CARTESIAN_POINT('Ctrl Pts',(-63.7906821188187,-75.6124659229421,
64.7083354921592));
#208714=CARTESIAN_POINT('Ctrl Pts',(-63.7624535119922,-75.1910566622627,
65.4869514301863));
#208715=CARTESIAN_POINT('Ctrl Pts',(-63.7531028024434,-75.0633219800847,
65.7531559357367));
#208716=CARTESIAN_POINT('Ctrl Pts',(-63.7252693597624,-74.7205177873625,
66.5669362902439));
#208717=CARTESIAN_POINT('Ctrl Pts',(-63.7070369656083,-74.5453935091855,
67.1296354172816));
#208718=CARTESIAN_POINT('Ctrl Pts',(-63.6595559178276,-74.2430232701488,
68.585706164633));
#208719=CARTESIAN_POINT('Ctrl Pts',(-63.6306895989319,-74.1918705736881,
69.4884282042888));
#208720=CARTESIAN_POINT('Ctrl Pts',(-63.587999601034,-74.3156730368305,
70.8368975882274));
#208721=CARTESIAN_POINT('Ctrl Pts',(-63.5736937807602,-74.3912196648846,
71.2861404207558));
#208722=CARTESIAN_POINT('Ctrl Pts',(-63.5444429022993,-74.6089816180539,
72.1696493608413));
#208723=CARTESIAN_POINT('Ctrl Pts',(-63.5297035311655,-74.7509063821301,
72.6026592072826));
#208724=CARTESIAN_POINT('Ctrl Pts',(-63.5151079737573,-74.9246636583587,
73.0232136446285));
#208725=CARTESIAN_POINT('Origin',(-61.5936228798467,-83.3229197588524,69.5524554490053));
#208726=CARTESIAN_POINT('',(-56.4535514884217,-74.9216338018341,73.0234382919193));
#208727=CARTESIAN_POINT('Ctrl Pts',(-57.3654750299524,-91.7241837160232,
66.0814193573838));
#208728=CARTESIAN_POINT('Ctrl Pts',(-57.3511269999552,-91.5507897413691,
65.6617381696345));
#208729=CARTESIAN_POINT('Ctrl Pts',(-57.3367077978504,-91.3461263316519,
65.2554805117783));
#208730=CARTESIAN_POINT('Ctrl Pts',(-57.3043239281533,-90.8258831413671,
64.3908149809122));
#208731=CARTESIAN_POINT('Ctrl Pts',(-57.2864041853605,-90.4970161174915,
63.9427009497785));
#208732=CARTESIAN_POINT('Ctrl Pts',(-57.2496280960837,-89.7290101102497,
63.0750981369921));
#208733=CARTESIAN_POINT('Ctrl Pts',(-57.2305952659493,-89.2845818860741,
62.6638609750959));
#208734=CARTESIAN_POINT('Ctrl Pts',(-57.1954237150673,-88.4107163650698,
62.00361636557));
#208735=CARTESIAN_POINT('Ctrl Pts',(-57.1794898420337,-87.9954101214033,
61.7397429399961));
#208736=CARTESIAN_POINT('Ctrl Pts',(-57.148190326257,-87.1305333422187,
61.2839624331371));
#208737=CARTESIAN_POINT('Ctrl Pts',(-57.1328794922873,-86.6827338480033,
61.0921036329978));
#208738=CARTESIAN_POINT('Ctrl Pts',(-57.1009362166587,-85.7330339675864,
60.7725609603835));
#208739=CARTESIAN_POINT('Ctrl Pts',(-57.0843272617399,-85.2312276240352,
60.6500091943235));
#208740=CARTESIAN_POINT('Ctrl Pts',(-57.0580374834263,-84.4273521006678,
60.5248128591109));
#208741=CARTESIAN_POINT('Ctrl Pts',(-57.0484372892729,-84.1308721435515,
60.493464424947));
#208742=CARTESIAN_POINT('Ctrl Pts',(-57.0160579701305,-83.1170968390338,
60.4364443566522));
#208743=CARTESIAN_POINT('Ctrl Pts',(-56.9934400055393,-82.3985525487146,
60.4810956475757));
#208744=CARTESIAN_POINT('Ctrl Pts',(-56.952011193016,-81.1344679518802,
60.7115248476976));
#208745=CARTESIAN_POINT('Ctrl Pts',(-56.9336416424726,-80.5869234847169,
60.8653549620364));
#208746=CARTESIAN_POINT('Ctrl Pts',(-56.8975866077343,-79.5285546572155,
61.2727739287243));
#208747=CARTESIAN_POINT('Ctrl Pts',(-56.8796783662447,-79.0199942231926,
61.525303890454));
#208748=CARTESIAN_POINT('Ctrl Pts',(-56.844501527484,-78.0889398805368,
62.1016808290221));
#208749=CARTESIAN_POINT('Ctrl Pts',(-56.8273517502541,-77.6647293402901,
62.4184893748666));
#208750=CARTESIAN_POINT('Ctrl Pts',(-56.793853359515,-76.8816904338446,
63.1172871691854));
#208751=CARTESIAN_POINT('Ctrl Pts',(-56.7774870022801,-76.5234790420236,
63.4970084934137));
#208752=CARTESIAN_POINT('Ctrl Pts',(-56.7447381479169,-75.8849848717943,
64.3023881577202));
#208753=CARTESIAN_POINT('Ctrl Pts',(-56.7284256627339,-75.6039484340531,
64.7250797496552));
#208754=CARTESIAN_POINT('Ctrl Pts',(-56.6929753232929,-75.0722101191746,
65.6910700744627));
#208755=CARTESIAN_POINT('Ctrl Pts',(-56.6742621566029,-74.8368586036357,
66.2401636162399));
#208756=CARTESIAN_POINT('Ctrl Pts',(-56.6223104154658,-74.3414220898481,
67.8047577021512));
#208757=CARTESIAN_POINT('Ctrl Pts',(-56.5886870746332,-74.2001051532625,
68.8481768815298));
#208758=CARTESIAN_POINT('Ctrl Pts',(-56.5219062851257,-74.2795067556648,
70.9683983405147));
#208759=CARTESIAN_POINT('Ctrl Pts',(-56.4874132736607,-74.5105716502198,
72.0284893572482));
#208760=CARTESIAN_POINT('Ctrl Pts',(-56.4535514884216,-74.9216338018342,
73.0234382919195));
#208761=CARTESIAN_POINT('Ctrl Pts',(-56.4535514884216,-74.9216338018341,
73.0234382919192));
#208762=CARTESIAN_POINT('Ctrl Pts',(-56.4350025486387,-75.1468070182932,
73.5684552703803));
#208763=CARTESIAN_POINT('Ctrl Pts',(-56.4166167442774,-75.4244814744311,
74.0902687222035));
#208764=CARTESIAN_POINT('Ctrl Pts',(-56.3791654426711,-76.0776033798498,
75.0736682947515));
#208765=CARTESIAN_POINT('Ctrl Pts',(-56.3602283268396,-76.4516830269538,
75.5327997675719));
#208766=CARTESIAN_POINT('Ctrl Pts',(-56.3295967832577,-77.138278850674,
76.2253320098543));
#208767=CARTESIAN_POINT('Ctrl Pts',(-56.317634399164,-77.4259346773961,
76.4808487072807));
#208768=CARTESIAN_POINT('Ctrl Pts',(-56.2894402158142,-78.1341586306357,
77.0337944695028));
#208769=CARTESIAN_POINT('Ctrl Pts',(-56.2731540040184,-78.5655297897047,
77.3152453835778));
#208770=CARTESIAN_POINT('Ctrl Pts',(-56.2191304377677,-80.0620371547784,
78.1198401417049));
#208771=CARTESIAN_POINT('Ctrl Pts',(-56.1828647646033,-81.2054241562849,
78.4715164049074));
#208772=CARTESIAN_POINT('Ctrl Pts',(-56.1075989876639,-83.5623975802335,
78.7162692586896));
#208773=CARTESIAN_POINT('Ctrl Pts',(-56.0713507175757,-84.7533964787986,
78.6070995128668));
#208774=CARTESIAN_POINT('Ctrl Pts',(-56.0244312023155,-86.170417770195,
78.1899669454804));
#208775=CARTESIAN_POINT('Ctrl Pts',(-56.0151271433587,-86.4468088869935,
78.0938936972519));
#208776=CARTESIAN_POINT('Ctrl Pts',(-55.9899598034833,-87.1872017197583,
77.7957799154857));
#208777=CARTESIAN_POINT('Ctrl Pts',(-55.9743076251468,-87.6397370742522,
77.5680755958334));
#208778=CARTESIAN_POINT('Ctrl Pts',(-55.9325391950402,-88.7746966499046,
76.8728703508149));
#208779=CARTESIAN_POINT('Ctrl Pts',(-55.9060931852866,-89.416440799934,
76.3479941666282));
#208780=CARTESIAN_POINT('Ctrl Pts',(-55.8672462315126,-90.2595979929845,
75.4416090357902));
#208781=CARTESIAN_POINT('Ctrl Pts',(-55.8543960475012,-90.5197763975782,
75.1206589210597));
#208782=CARTESIAN_POINT('Ctrl Pts',(-55.8280947721969,-91.0005965893752,
74.4372739798999));
#208783=CARTESIAN_POINT('Ctrl Pts',(-55.8146661895194,-91.2195106834258,
74.0748461106465));
#208784=CARTESIAN_POINT('Ctrl Pts',(-55.8011708396429,-91.4123950525873,
73.6985038205813));
#208785=CARTESIAN_POINT('',(-56.2580209956237,-74.9217169067527,73.0236394350926));
#208786=CARTESIAN_POINT('Ctrl Pts',(-56.2580209956237,-74.9217169067527,
73.0236394350926));
#208787=CARTESIAN_POINT('Ctrl Pts',(-56.2443250754476,-75.0846204163747,
73.4179099304447));
#208788=CARTESIAN_POINT('Ctrl Pts',(-56.2305642181659,-75.2750783558321,
73.8002275282816));
#208789=CARTESIAN_POINT('Ctrl Pts',(-56.2033211069302,-75.7073605527732,
74.5337242263203));
#208790=CARTESIAN_POINT('Ctrl Pts',(-56.1898709563397,-75.9484320247352,
74.8841262966469));
#208791=CARTESIAN_POINT('Ctrl Pts',(-56.1512855608216,-76.707371854651,
75.8368058676944));
#208792=CARTESIAN_POINT('Ctrl Pts',(-56.1256639711523,-77.2807097395701,
76.3898681292522));
#208793=CARTESIAN_POINT('Ctrl Pts',(-56.0833810803596,-78.3407712514973,
77.1736969095166));
#208794=CARTESIAN_POINT('Ctrl Pts',(-56.0667865829977,-78.7893015442435,
77.4487477683126));
#208795=CARTESIAN_POINT('Ctrl Pts',(-56.0320548232101,-79.766401713918,
77.9370958618635));
#208796=CARTESIAN_POINT('Ctrl Pts',(-56.0136903834562,-80.2963550940178,
78.1426188139801));
#208797=CARTESIAN_POINT('Ctrl Pts',(-55.9724037787782,-81.5284216935346,
78.4921548134415));
#208798=CARTESIAN_POINT('Ctrl Pts',(-55.9499103502961,-82.2354030076385,
78.605397131529));
#208799=CARTESIAN_POINT('Ctrl Pts',(-55.903822487772,-83.6793637761405,
78.6649527140371));
#208800=CARTESIAN_POINT('Ctrl Pts',(-55.8800043454388,-84.4113738723253,
78.6067319429833));
#208801=CARTESIAN_POINT('Ctrl Pts',(-55.841858052403,-85.5806198022539,
78.3697661154032));
#208802=CARTESIAN_POINT('Ctrl Pts',(-55.8272928052752,-86.0251498845119,
78.2438378961145));
#208803=CARTESIAN_POINT('Ctrl Pts',(-55.7936110388135,-87.0184892669261,
77.8788240150679));
#208804=CARTESIAN_POINT('Ctrl Pts',(-55.7742461928925,-87.5571384948989,
77.6182491090811));
#208805=CARTESIAN_POINT('Ctrl Pts',(-55.7285410136335,-88.7711700519054,
76.8756090000868));
#208806=CARTESIAN_POINT('Ctrl Pts',(-55.7027970840579,-89.4139326223631,
76.3503647630469));
#208807=CARTESIAN_POINT('Ctrl Pts',(-55.6629912962453,-90.2582430102741,
75.4432276991302));
#208808=CARTESIAN_POINT('Ctrl Pts',(-55.6496589375082,-90.5186999191627,
75.1220745554689));
#208809=CARTESIAN_POINT('Ctrl Pts',(-55.6228882380845,-91.0000718362507,
74.4381366140566));
#208810=CARTESIAN_POINT('Ctrl Pts',(-55.6094895732802,-91.2192478132438,
74.0753471720817));
#208811=CARTESIAN_POINT('Ctrl Pts',(-55.5961206596756,-91.4123422054238,
73.6986069305967));
#208812=CARTESIAN_POINT('Ctrl Pts',(-56.2580209956237,-74.9217169067528,
73.0236394350929));
#208813=CARTESIAN_POINT('Ctrl Pts',(-56.2926073343763,-74.5103362988558,
72.027987245461));
#208814=CARTESIAN_POINT('Ctrl Pts',(-56.3260108520931,-74.2792109946535,
70.9670967281698));
#208815=CARTESIAN_POINT('Ctrl Pts',(-56.3941547954805,-74.2002081594267,
68.8445057035695));
#208816=CARTESIAN_POINT('Ctrl Pts',(-56.4265227223919,-74.3422523522542,
67.799546121765));
#208817=CARTESIAN_POINT('Ctrl Pts',(-56.4789203965196,-74.8393543049745,
66.2337698825305));
#208818=CARTESIAN_POINT('Ctrl Pts',(-56.4979976546502,-75.0751409611987,
65.684805115915));
#208819=CARTESIAN_POINT('Ctrl Pts',(-56.532736048018,-75.6092728256102,
64.7162223172105));
#208820=CARTESIAN_POINT('Ctrl Pts',(-56.5486714524192,-75.8927421873167,
64.291090652088));
#208821=CARTESIAN_POINT('Ctrl Pts',(-56.5812135927908,-76.5323260673472,
63.4874340775086));
#208822=CARTESIAN_POINT('Ctrl Pts',(-56.5977691595269,-76.8882118065885,
63.1110909781267));
#208823=CARTESIAN_POINT('Ctrl Pts',(-56.6308145738522,-77.6680096136265,
62.4159497907822));
#208824=CARTESIAN_POINT('Ctrl Pts',(-56.6471576114214,-78.091689623822,
62.0998077664478));
#208825=CARTESIAN_POINT('Ctrl Pts',(-56.6815228560717,-79.0221041166156,
61.5241819630653));
#208826=CARTESIAN_POINT('Ctrl Pts',(-56.6995260286931,-79.5306161311664,
61.2718387861529));
#208827=CARTESIAN_POINT('Ctrl Pts',(-56.7355244261045,-80.5888864316576,
60.8647416856394));
#208828=CARTESIAN_POINT('Ctrl Pts',(-56.7531344890569,-81.1363977495086,
60.711050953292));
#208829=CARTESIAN_POINT('Ctrl Pts',(-56.79331146269,-82.3999671727881,60.4809925255085));
#208830=CARTESIAN_POINT('Ctrl Pts',(-56.8160841288014,-83.1179966717957,
60.4364660564977));
#208831=CARTESIAN_POINT('Ctrl Pts',(-56.8481932963248,-84.1312184864888,
60.4934959311227));
#208832=CARTESIAN_POINT('Ctrl Pts',(-56.8575101479712,-84.4276804127036,
60.5248533740059));
#208833=CARTESIAN_POINT('Ctrl Pts',(-56.8828739882039,-85.2307648475454,
60.6499554820837));
#208834=CARTESIAN_POINT('Ctrl Pts',(-56.8989249433381,-85.7318063995676,
60.7722709986547));
#208835=CARTESIAN_POINT('Ctrl Pts',(-56.9306247496818,-86.6818969447094,
61.0917059720352));
#208836=CARTESIAN_POINT('Ctrl Pts',(-56.9461926174623,-87.1307544508128,
61.2839971590145));
#208837=CARTESIAN_POINT('Ctrl Pts',(-56.9770159340458,-87.9963784729066,
61.7403358608625));
#208838=CARTESIAN_POINT('Ctrl Pts',(-56.9922216198082,-88.4114715277067,
62.0041393763885));
#208839=CARTESIAN_POINT('Ctrl Pts',(-57.0265860548614,-89.2851086830678,
62.6643175577409));
#208840=CARTESIAN_POINT('Ctrl Pts',(-57.0458060216535,-89.7294982251628,
63.0755829320188));
#208841=CARTESIAN_POINT('Ctrl Pts',(-57.0826057296618,-90.497327911536,
63.9431144140599));
#208842=CARTESIAN_POINT('Ctrl Pts',(-57.0998328662142,-90.8260860586377,
64.3911245878254));
#208843=CARTESIAN_POINT('Ctrl Pts',(-57.1315082096315,-91.3461990421847,
65.2556240251727));
#208844=CARTESIAN_POINT('Ctrl Pts',(-57.1458823024629,-91.5508221368337,
65.6618165793203));
#208845=CARTESIAN_POINT('Ctrl Pts',(-57.1603612091034,-91.7241837160232,
66.0814193573838));
#208846=CARTESIAN_POINT('Origin',(-54.462516693425,-83.3223805071439,69.5544896765311));
#208847=CARTESIAN_POINT('',(-49.1982221066872,-74.9212163133617,73.0257672247191));
#208848=CARTESIAN_POINT('Ctrl Pts',(-50.1089321285242,-91.723644464317,
66.0834535849087));
#208849=CARTESIAN_POINT('Ctrl Pts',(-50.0994336195942,-91.6094380273631,
65.8070293711777));
#208850=CARTESIAN_POINT('Ctrl Pts',(-50.0898876520213,-91.4815881462714,
65.5362396202102));
#208851=CARTESIAN_POINT('Ctrl Pts',(-50.0645523224655,-91.1098859605774,
64.8402840168896));
#208852=CARTESIAN_POINT('Ctrl Pts',(-50.048674965668,-90.8447562790985,
64.4278108302642));
#208853=CARTESIAN_POINT('Ctrl Pts',(-50.0171304476547,-90.2470491828378,
63.6448533458755));
#208854=CARTESIAN_POINT('Ctrl Pts',(-50.0015374739218,-89.9146891796019,
63.276248714982));
#208855=CARTESIAN_POINT('Ctrl Pts',(-49.953823265501,-88.8252169616591,
62.2503795039651));
#208856=CARTESIAN_POINT('Ctrl Pts',(-49.9213980023652,-87.9881259655062,
61.689246247093));
#208857=CARTESIAN_POINT('Ctrl Pts',(-49.851974376817,-85.9975019173158,
60.786550076608));
#208858=CARTESIAN_POINT('Ctrl Pts',(-49.8136784471919,-84.8331530901671,
60.5128852669592));
#208859=CARTESIAN_POINT('Ctrl Pts',(-49.757645753811,-83.0691499064639,
60.4494351506318));
#208860=CARTESIAN_POINT('Ctrl Pts',(-49.7392083102798,-82.4885041654403,
60.4841651943603));
#208861=CARTESIAN_POINT('Ctrl Pts',(-49.7021735698838,-81.3528530603487,
60.6621205125193));
#208862=CARTESIAN_POINT('Ctrl Pts',(-49.6838072996849,-80.8000654677217,
60.8028492188456));
#208863=CARTESIAN_POINT('Ctrl Pts',(-49.6476580471214,-79.7267203638698,
61.1863260386364));
#208864=CARTESIAN_POINT('Ctrl Pts',(-49.6296403007662,-79.2086380689463,
61.4284787014464));
#208865=CARTESIAN_POINT('Ctrl Pts',(-49.5932027578465,-78.2292218191738,
62.0040753822869));
#208866=CARTESIAN_POINT('Ctrl Pts',(-49.5749140332662,-77.7695427425373,
62.335415857715));
#208867=CARTESIAN_POINT('Ctrl Pts',(-49.5342133395524,-76.802880990269,
63.1794756229899));
#208868=CARTESIAN_POINT('Ctrl Pts',(-49.5117063431937,-76.3199648523112,
63.7140396907855));
#208869=CARTESIAN_POINT('Ctrl Pts',(-49.4705593303023,-75.5773352695081,
64.7623231305718));
#208870=CARTESIAN_POINT('Ctrl Pts',(-49.4523615418275,-75.2936591039501,
65.2544623510051));
#208871=CARTESIAN_POINT('Ctrl Pts',(-49.4165436367922,-74.8206065012855,
66.2874806875142));
#208872=CARTESIAN_POINT('Ctrl Pts',(-49.398696196724,-74.6327097900308,
66.8262797100903));
#208873=CARTESIAN_POINT('Ctrl Pts',(-49.3655773179496,-74.3838357000045,
67.8360056556622));
#208874=CARTESIAN_POINT('Ctrl Pts',(-49.3504647070004,-74.306869465203,
68.3009628121704));
#208875=CARTESIAN_POINT('Ctrl Pts',(-49.3198705092816,-74.2235999212939,
69.2619573658559));
#208876=CARTESIAN_POINT('Ctrl Pts',(-49.3045062806606,-74.2211464531685,
69.7567928371245));
#208877=CARTESIAN_POINT('Ctrl Pts',(-49.2588282011871,-74.3320963837926,
71.2039321493425));
#208878=CARTESIAN_POINT('Ctrl Pts',(-49.2281734459348,-74.5556207774409,
72.1409551971163));
#208879=CARTESIAN_POINT('Ctrl Pts',(-49.1982221066872,-74.9212163133618,
73.0257672247193));
#208880=CARTESIAN_POINT('',(-48.6677134573783,-88.926319310838,76.7064654074423));
#208881=CARTESIAN_POINT('Ctrl Pts',(-49.1982221066872,-74.9212163133617,
73.025767224719));
#208882=CARTESIAN_POINT('Ctrl Pts',(-49.1846980474795,-75.086295264689,
73.4252902694153));
#208883=CARTESIAN_POINT('Ctrl Pts',(-49.17120111885,-75.279663006462,73.81252823487));
#208884=CARTESIAN_POINT('Ctrl Pts',(-49.143988944538,-75.7186383315664,
74.554183972483));
#208885=CARTESIAN_POINT('Ctrl Pts',(-49.1303097652266,-75.9633548844277,
74.9078602464795));
#208886=CARTESIAN_POINT('Ctrl Pts',(-49.0903095232135,-76.7519488993082,
75.8907898221601));
#208887=CARTESIAN_POINT('Ctrl Pts',(-49.0648068938641,-77.3580971968119,
76.4643810297756));
#208888=CARTESIAN_POINT('Ctrl Pts',(-49.0230777052332,-78.4328567586469,
77.2332123424207));
#208889=CARTESIAN_POINT('Ctrl Pts',(-49.0074210140729,-78.8545159359737,
77.4859716780431));
#208890=CARTESIAN_POINT('Ctrl Pts',(-48.9742148604392,-79.7976971077219,
77.9521673686708));
#208891=CARTESIAN_POINT('Ctrl Pts',(-48.9568877803953,-80.3228403383812,
78.153742319573));
#208892=CARTESIAN_POINT('Ctrl Pts',(-48.9237288223427,-81.3401391481041,
78.439615953681));
#208893=CARTESIAN_POINT('Ctrl Pts',(-48.908019142487,-81.8272225374683,
78.5344253341945));
#208894=CARTESIAN_POINT('Ctrl Pts',(-48.8736831345182,-82.9016621136855,
78.6536821415626));
#208895=CARTESIAN_POINT('Ctrl Pts',(-48.8554489915002,-83.4886161210103,
78.6618866050423));
#208896=CARTESIAN_POINT('Ctrl Pts',(-48.8094548302731,-84.9538475193705,
78.5405982968361));
#208897=CARTESIAN_POINT('Ctrl Pts',(-48.7811658042173,-85.8200663471706,
78.3393276526718));
#208898=CARTESIAN_POINT('Ctrl Pts',(-48.7396885127796,-87.0478114546505,
77.8574497617519));
#208899=CARTESIAN_POINT('Ctrl Pts',(-48.7261817247739,-87.4402347937579,
77.6699847384728));
#208900=CARTESIAN_POINT('Ctrl Pts',(-48.69851862242,-88.2047631247771,77.2349803582429));
#208901=CARTESIAN_POINT('Ctrl Pts',(-48.6843884534109,-88.5750682105596,
76.9866399293904));
#208902=CARTESIAN_POINT('Ctrl Pts',(-48.6701794005809,-88.9256751617519,
76.7121720277593));
#208903=CARTESIAN_POINT('',(-48.4675099033474,-88.9256126608575,76.7079526484011));
#208904=CARTESIAN_POINT('Ctrl Pts',(-48.6675364832709,-88.925670370627,
76.7064311666085));
#208905=CARTESIAN_POINT('Ctrl Pts',(-48.6008609566297,-88.9257458498605,
76.7121166899682));
#208906=CARTESIAN_POINT('Ctrl Pts',(-48.5341854299886,-88.9257458498605,
76.7121166899682));
#208907=CARTESIAN_POINT('Ctrl Pts',(-48.4675099033474,-88.9256126608575,
76.7079526484011));
#208908=CARTESIAN_POINT('',(-49.0012377727688,-74.9211148625051,73.0255216838241));
#208909=CARTESIAN_POINT('Ctrl Pts',(-49.0012377727688,-74.9211148625051,
73.0255216838241));
#208910=CARTESIAN_POINT('Ctrl Pts',(-48.9869942993802,-75.089699356929,
73.4335626117807));
#208911=CARTESIAN_POINT('Ctrl Pts',(-48.9727665448755,-75.2877888236457,
73.8287836060104));
#208912=CARTESIAN_POINT('Ctrl Pts',(-48.9446794933811,-75.7378818958822,
74.5840306230201));
#208913=CARTESIAN_POINT('Ctrl Pts',(-48.9308529409634,-75.988815789032,
74.943342021598));
#208914=CARTESIAN_POINT('Ctrl Pts',(-48.8896864538057,-76.8041834998098,
75.9478730052195));
#208915=CARTESIAN_POINT('Ctrl Pts',(-48.8618295254185,-77.4349142322651,
76.5330266535213));
#208916=CARTESIAN_POINT('Ctrl Pts',(-48.8153368443144,-78.6323171351225,
77.3643920918584));
#208917=CARTESIAN_POINT('Ctrl Pts',(-48.7964053555968,-79.1593375887011,
77.6575966005903));
#208918=CARTESIAN_POINT('Ctrl Pts',(-48.7622406355031,-80.1315986182241,
78.0784464647309));
#208919=CARTESIAN_POINT('Ctrl Pts',(-48.7474157728212,-80.5648917952641,
78.2283117360319));
#208920=CARTESIAN_POINT('Ctrl Pts',(-48.7035598203036,-81.8874291244707,
78.5765719982373));
#208921=CARTESIAN_POINT('Ctrl Pts',(-48.6750545183272,-82.7970469727182,
78.6748551441189));
#208922=CARTESIAN_POINT('Ctrl Pts',(-48.6306159838848,-84.1726571729396,
78.6167461339182));
#208923=CARTESIAN_POINT('Ctrl Pts',(-48.6156168883726,-84.637081559956,
78.5611000819166));
#208924=CARTESIAN_POINT('Ctrl Pts',(-48.5787691667439,-85.7727895048833,
78.3352724470895));
#208925=CARTESIAN_POINT('Ctrl Pts',(-48.5570481635015,-86.4328395490297,
78.1237188431876));
#208926=CARTESIAN_POINT('Ctrl Pts',(-48.5231754596634,-87.3916298392153,
77.6908842886861));
#208927=CARTESIAN_POINT('Ctrl Pts',(-48.5115549194922,-87.7115877986523,
77.5228376567632));
#208928=CARTESIAN_POINT('Ctrl Pts',(-48.4883063582056,-88.3347227938847,
77.1466111270654));
#208929=CARTESIAN_POINT('Ctrl Pts',(-48.4767027792111,-88.6369798719034,
76.93818233476));
#208930=CARTESIAN_POINT('Ctrl Pts',(-48.4651187514169,-88.9258151777998,
76.7120624158844));
#208931=CARTESIAN_POINT('Ctrl Pts',(-49.0012377727688,-74.9211148625051,
73.0255216838243));
#208932=CARTESIAN_POINT('Ctrl Pts',(-49.0300579383319,-74.5800019255054,
72.1998939187861));
#208933=CARTESIAN_POINT('Ctrl Pts',(-49.0579275328701,-74.3624530212605,
71.3284842431545));
#208934=CARTESIAN_POINT('Ctrl Pts',(-49.1024052105896,-74.2271701161775,
69.9454212245552));
#208935=CARTESIAN_POINT('Ctrl Pts',(-49.1184482023418,-74.2193918386184,
69.4483149280677));
#208936=CARTESIAN_POINT('Ctrl Pts',(-49.148701269016,-74.2819747701981,
68.5044907200461));
#208937=CARTESIAN_POINT('Ctrl Pts',(-49.1628092336948,-74.344955084967,
68.0587394864049));
#208938=CARTESIAN_POINT('Ctrl Pts',(-49.1997883134222,-74.5938130420238,
66.916478032258));
#208939=CARTESIAN_POINT('Ctrl Pts',(-49.2228683860683,-74.8298972452911,
66.2341433446612));
#208940=CARTESIAN_POINT('Ctrl Pts',(-49.2639268800242,-75.3906777671344,
65.0782215789127));
#208941=CARTESIAN_POINT('Ctrl Pts',(-49.2815569067501,-75.6843228254867,
64.5937476630907));
#208942=CARTESIAN_POINT('Ctrl Pts',(-49.3203981633498,-76.4170658727824,
63.6057160228744));
#208943=CARTESIAN_POINT('Ctrl Pts',(-49.3416920089049,-76.8704570668344,
63.1167925672631));
#208944=CARTESIAN_POINT('Ctrl Pts',(-49.3806443144535,-77.7958426459659,
62.3157496485224));
#208945=CARTESIAN_POINT('Ctrl Pts',(-49.3980155450531,-78.2514659505196,
61.9895834962571));
#208946=CARTESIAN_POINT('Ctrl Pts',(-49.4335438607192,-79.2258756161993,
61.419846811469));
#208947=CARTESIAN_POINT('Ctrl Pts',(-49.4516749204165,-79.7435212891671,
61.1791973110947));
#208948=CARTESIAN_POINT('Ctrl Pts',(-49.4879074009792,-80.8161365724487,
60.7982663185702));
#208949=CARTESIAN_POINT('Ctrl Pts',(-49.5056126479794,-81.368685559789,
60.6586599453322));
#208950=CARTESIAN_POINT('Ctrl Pts',(-49.5415855326542,-82.5035879300481,
60.4828280189462));
#208951=CARTESIAN_POINT('Ctrl Pts',(-49.5599179145507,-83.0837029875439,
60.4490798928174));
#208952=CARTESIAN_POINT('Ctrl Pts',(-49.6160241474124,-84.8471661869708,
60.5152178061111));
#208953=CARTESIAN_POINT('Ctrl Pts',(-49.6522879316194,-86.0112414920116,
60.7907328663199));
#208954=CARTESIAN_POINT('Ctrl Pts',(-49.7214250071374,-87.9922109798468,
61.6928355956797));
#208955=CARTESIAN_POINT('Ctrl Pts',(-49.7518751356753,-88.8214775823457,
62.2488159886867));
#208956=CARTESIAN_POINT('Ctrl Pts',(-49.7991169299812,-89.9108243913346,
63.2716368906033));
#208957=CARTESIAN_POINT('Ctrl Pts',(-49.815167059316,-90.2480015101607,
63.6453776917895));
#208958=CARTESIAN_POINT('Ctrl Pts',(-49.8463623528132,-90.8484992053569,
64.4334279320365));
#208959=CARTESIAN_POINT('Ctrl Pts',(-49.8614853611635,-91.1126658038604,
64.8450102511));
#208960=CARTESIAN_POINT('Ctrl Pts',(-49.886164854335,-91.4827887918636,
65.5387831313055));
#208961=CARTESIAN_POINT('Ctrl Pts',(-49.8955642184998,-91.6099752738436,
65.8083297176374));
#208962=CARTESIAN_POINT('Ctrl Pts',(-49.9050113929448,-91.723644464317,
66.0834535849087));
#208963=CARTESIAN_POINT('Ctrl Pts',(-48.6992141518181,-88.6234275459005,
76.9087096781305));
#208964=CARTESIAN_POINT('Ctrl Pts',(-48.6491771284881,-89.9491017707071,
76.0595009463133));
#208965=CARTESIAN_POINT('Ctrl Pts',(-48.5491030818342,-92.1856846035653,
73.6287810246092));
#208966=CARTESIAN_POINT('Ctrl Pts',(-48.3989920118381,-93.3103166936467,
68.6586256876712));
#208967=CARTESIAN_POINT('Ctrl Pts',(-48.2488809418481,-91.7677199889504,
63.6554187246849));
#208968=CARTESIAN_POINT('Ctrl Pts',(-48.1488068951881,-89.1478110606889,
61.2125219408772));
#208969=CARTESIAN_POINT('Ctrl Pts',(-48.0987698718642,-87.5969606882947,
60.3923995585769));
#208970=CARTESIAN_POINT('Ctrl Pts',(-48.6180189895515,-88.6234275459005,
76.9087096781305));
#208971=CARTESIAN_POINT('Ctrl Pts',(-48.5679819662217,-89.9491017707071,
76.0595009463133));
#208972=CARTESIAN_POINT('Ctrl Pts',(-48.4679079195627,-92.1856846035653,
73.6287810246092));
#208973=CARTESIAN_POINT('Ctrl Pts',(-48.3177968495717,-93.3103166936467,
68.6586256876712));
#208974=CARTESIAN_POINT('Ctrl Pts',(-48.1676857795814,-91.7677199889504,
63.6554187246849));
#208975=CARTESIAN_POINT('Ctrl Pts',(-48.0676117329217,-89.1478110606889,
61.2125219408772));
#208976=CARTESIAN_POINT('Ctrl Pts',(-48.0175747095927,-87.5969606882947,
60.3923995585769));
#208977=CARTESIAN_POINT('Ctrl Pts',(-48.536823827284,-88.6234275459005,
76.9087096781305));
#208978=CARTESIAN_POINT('Ctrl Pts',(-48.4867868039552,-89.9491017707071,
76.0595009463133));
#208979=CARTESIAN_POINT('Ctrl Pts',(-48.3867127572953,-92.1856846035653,
73.6287810246092));
#208980=CARTESIAN_POINT('Ctrl Pts',(-48.2366016873052,-93.3103166936467,
68.6586256876712));
#208981=CARTESIAN_POINT('Ctrl Pts',(-48.086490617314,-91.7677199889504,
63.6554187246849));
#208982=CARTESIAN_POINT('Ctrl Pts',(-47.9864165706552,-89.1478110606889,
61.2125219408772));
#208983=CARTESIAN_POINT('Ctrl Pts',(-47.9363795473253,-87.5969606882947,
60.3923995585769));
#208984=CARTESIAN_POINT('Ctrl Pts',(-48.4556286650124,-88.6234275459005,
76.9087096781305));
#208985=CARTESIAN_POINT('Ctrl Pts',(-48.4055916416887,-89.9491017707071,
76.0595009463133));
#208986=CARTESIAN_POINT('Ctrl Pts',(-48.3055175950287,-92.1856846035653,
73.6287810246092));
#208987=CARTESIAN_POINT('Ctrl Pts',(-48.1554065250387,-93.3103166936467,
68.6586256876712));
#208988=CARTESIAN_POINT('Ctrl Pts',(-48.0052954550424,-91.7677199889504,
63.6554187246849));
#208989=CARTESIAN_POINT('Ctrl Pts',(-47.9052214083887,-89.1478110606889,
61.2125219408772));
#208990=CARTESIAN_POINT('Ctrl Pts',(-47.8551843850587,-87.5969606882947,
60.3923995585769));
#208991=CARTESIAN_POINT('',(-48.0901869004046,-87.9505400884526,60.5887241650105));
#208992=CARTESIAN_POINT('Ctrl Pts',(-48.6675364832709,-88.9255866918527,
76.7063115883213));
#208993=CARTESIAN_POINT('Ctrl Pts',(-48.6312818813982,-89.8622753124554,
76.0508334282851));
#208994=CARTESIAN_POINT('Ctrl Pts',(-48.5950272795265,-90.6834819943738,
75.2089926204495));
#208995=CARTESIAN_POINT('Ctrl Pts',(-48.5587726776542,-91.3266685573513,
74.2361378408557));
#208996=CARTESIAN_POINT('Ctrl Pts',(-48.5488391350575,-91.5028978024944,
73.9695814895414));
#208997=CARTESIAN_POINT('Ctrl Pts',(-48.5389055924608,-91.6657627683633,
73.6931898159694));
#208998=CARTESIAN_POINT('Ctrl Pts',(-48.5289720498641,-91.813977577031,
73.4081017822123));
#208999=CARTESIAN_POINT('Ctrl Pts',(-48.4789350265345,-92.5605619669258,
71.9720625789632));
#209000=CARTESIAN_POINT('Ctrl Pts',(-48.4288980032028,-92.9354393302862,
70.3153441333172));
#209001=CARTESIAN_POINT('Ctrl Pts',(-48.378860979872,-92.8657785611838,
68.6531170833298));
#209002=CARTESIAN_POINT('Ctrl Pts',(-48.3288239565412,-92.7961177920813,
66.9908900333425));
#209003=CARTESIAN_POINT('Ctrl Pts',(-48.2787869332112,-92.2819188905158,
65.3231543790137));
#209004=CARTESIAN_POINT('Ctrl Pts',(-48.2287499098812,-91.3698422076677,
63.8785623558974));
#209005=CARTESIAN_POINT('Ctrl Pts',(-48.1929768543094,-90.7177696483925,
62.8457776840203));
#209006=CARTESIAN_POINT('Ctrl Pts',(-48.1572037987375,-89.8623194913236,
61.9270378615952));
#209007=CARTESIAN_POINT('Ctrl Pts',(-48.1214304257687,-88.8608821258745,
61.1874783364655));
#209008=CARTESIAN_POINT('Ctrl Pts',(-48.1110157930562,-88.5693356073277,
60.9721718058239));
#209009=CARTESIAN_POINT('Ctrl Pts',(-48.1006011334425,-88.2654160984107,
60.7720515629503));
#209010=CARTESIAN_POINT('Ctrl Pts',(-48.090186439096,-87.9505401496632,
60.5887240860841));
#209011=CARTESIAN_POINT('',(-47.8901874902887,-87.9505401262583,60.5887240720849));
#209012=CARTESIAN_POINT('',(-48.0901862140809,-87.9505401261674,60.5887240724043));
#209013=CARTESIAN_POINT('Ctrl Pts',(-48.4675451203219,-88.9253730646099,
76.7064610762623));
#209014=CARTESIAN_POINT('Ctrl Pts',(-48.4374727537661,-89.7023621699198,
76.1627715126034));
#209015=CARTESIAN_POINT('Ctrl Pts',(-48.4076478871442,-90.393251570204,
75.4956452737586));
#209016=CARTESIAN_POINT('Ctrl Pts',(-48.3478038746687,-91.5558518713347,
73.9693330989564));
#209017=CARTESIAN_POINT('Ctrl Pts',(-48.3182577310618,-92.0138637347129,
73.1182182398338));
#209018=CARTESIAN_POINT('Ctrl Pts',(-48.2515859642631,-92.7341784031747,
71.0669096930217));
#209019=CARTESIAN_POINT('Ctrl Pts',(-48.2150542464285,-92.9161625724017,
69.8554430328749));
#209020=CARTESIAN_POINT('Ctrl Pts',(-48.1419859937645,-92.8144445035439,
67.4281199427107));
#209021=CARTESIAN_POINT('Ctrl Pts',(-48.1054696631337,-92.5225233986339,
66.2128718196244));
#209022=CARTESIAN_POINT('Ctrl Pts',(-48.0390051710523,-91.6008694441996,
64.1561131800471));
#209023=CARTESIAN_POINT('Ctrl Pts',(-48.0094233078613,-91.040000796683,
63.3004156653558));
#209024=CARTESIAN_POINT('Ctrl Pts',(-47.9496630882316,-89.6603235361633,
61.7718652461384));
#209025=CARTESIAN_POINT('Ctrl Pts',(-47.9198152757014,-88.8463284293892,
61.1102710786235));
#209026=CARTESIAN_POINT('Ctrl Pts',(-47.8901874908167,-87.9505401260834,
60.5887240723554));
#209027=CARTESIAN_POINT('Ctrl Pts',(-63.7104920345709,-92.1934303316092,
74.8099293892526));
#209028=CARTESIAN_POINT('Ctrl Pts',(-63.6718652093945,-92.8968687267479,
73.6224666938168));
#209029=CARTESIAN_POINT('Ctrl Pts',(-63.5946115590417,-93.8203341640412,
70.961991106913));
#209030=CARTESIAN_POINT('Ctrl Pts',(-63.4787310835129,-93.5364438833945,
66.7467220222676));
#209031=CARTESIAN_POINT('Ctrl Pts',(-63.3628506079829,-91.6282348476794,
62.977524645695));
#209032=CARTESIAN_POINT('Ctrl Pts',(-63.2469701324539,-88.3991168492557,
60.25336151795));
#209033=CARTESIAN_POINT('Ctrl Pts',(-63.1310896569249,-84.3623407018535,
59.0072882090149));
#209034=CARTESIAN_POINT('Ctrl Pts',(-63.0152091813959,-80.1595688410345,
59.4373596262817));
#209035=CARTESIAN_POINT('Ctrl Pts',(-62.8993287058659,-76.4588404646688,
61.4752179418164));
#209036=CARTESIAN_POINT('Ctrl Pts',(-62.7834482303369,-73.8483960341625,
64.7969396843518));
#209037=CARTESIAN_POINT('Ctrl Pts',(-62.6675677548079,-72.7431720463215,
68.8745291515197));
#209038=CARTESIAN_POINT('Ctrl Pts',(-62.5516872792779,-73.3188466353806,
73.0598433065361));
#209039=CARTESIAN_POINT('Ctrl Pts',(-62.4358068037489,-75.4839148855997,
76.6876160812524));
#209040=CARTESIAN_POINT('Ctrl Pts',(-62.3199263282199,-78.8942338216446,
79.1812039750164));
#209041=CARTESIAN_POINT('Ctrl Pts',(-62.2040458526899,-83.0077247744123,
80.1442449974989));
#209042=CARTESIAN_POINT('Ctrl Pts',(-62.0881653771609,-87.1705381364528,
79.4236613850277));
#209043=CARTESIAN_POINT('Ctrl Pts',(-61.9722849016309,-90.7209843805715,
77.1339916933007));
#209044=CARTESIAN_POINT('Ctrl Pts',(-61.8564044261019,-93.0947112545776,
73.6391846088869));
#209045=CARTESIAN_POINT('Ctrl Pts',(-61.7405239505729,-93.9144089739031,
69.4947484013197));
#209046=CARTESIAN_POINT('Ctrl Pts',(-61.6246434750429,-93.0497845493678,
65.3594515033776));
#209047=CARTESIAN_POINT('Ctrl Pts',(-61.5087629995139,-90.638272181575,
61.8906096318565));
#209048=CARTESIAN_POINT('Ctrl Pts',(-61.3928825239839,-87.0631877532088,
59.6396038211845));
#209049=CARTESIAN_POINT('Ctrl Pts',(-61.2770020484549,-82.8927998170843,
58.9642370379884));
#209050=CARTESIAN_POINT('Ctrl Pts',(-61.1611215729249,-78.790001897706,
59.9718605105236));
#209051=CARTESIAN_POINT('Ctrl Pts',(-61.0452410973959,-75.4069439184922,
62.5023099842148));
#209052=CARTESIAN_POINT('Ctrl Pts',(-60.9293606218659,-73.2813713510347,
66.1533642278691));
#209053=CARTESIAN_POINT('Ctrl Pts',(-60.8134801463369,-72.7511492362934,
70.3446790977719));
#209054=CARTESIAN_POINT('Ctrl Pts',(-60.6975996708069,-73.9005576968343,
74.4100346812925));
#209055=CARTESIAN_POINT('Ctrl Pts',(-60.5817191952779,-76.5468954019475,
77.7032326073398));
#209056=CARTESIAN_POINT('Ctrl Pts',(-60.4658387197479,-80.2695203981129,
79.7008108830386));
#209057=CARTESIAN_POINT('Ctrl Pts',(-60.3499582442189,-84.4767121926759,
80.0852494781352));
#209058=CARTESIAN_POINT('Ctrl Pts',(-60.2340777686899,-88.4997271963806,
78.7954409227263));
#209059=CARTESIAN_POINT('Ctrl Pts',(-60.1181972931599,-91.6990971784923,
76.0364034914596));
#209060=CARTESIAN_POINT('Ctrl Pts',(-60.0023168176309,-93.566274330974,
72.2466930393405));
#209061=CARTESIAN_POINT('Ctrl Pts',(-59.8864363421009,-93.8044662060933,
68.0286934589439));
#209062=CARTESIAN_POINT('Ctrl Pts',(-59.7705558665719,-92.375811613486,
64.0528662639258));
#209063=CARTESIAN_POINT('Ctrl Pts',(-59.6546753910419,-89.5073987503684,
60.9511790655875));
#209064=CARTESIAN_POINT('Ctrl Pts',(-59.5387949155129,-85.6551689684265,
59.2166527507833));
#209065=CARTESIAN_POINT('Ctrl Pts',(-59.4229144399829,-81.4314437630425,
59.1249945869912));
#209066=CARTESIAN_POINT('Ctrl Pts',(-59.3070339644539,-77.5075947501924,
60.6907738670809));
#209067=CARTESIAN_POINT('Ctrl Pts',(-59.1911534889249,-74.5073274799646,
63.6651060840353));
#209068=CARTESIAN_POINT('Ctrl Pts',(-59.0752730133949,-72.9075418896531,
67.575213741715));
#209069=CARTESIAN_POINT('Ctrl Pts',(-58.9593925378659,-72.9625278737866,
71.7995755125808));
#209070=CARTESIAN_POINT('Ctrl Pts',(-58.8435120623359,-74.6635452735643,
75.6667185969865));
#209071=CARTESIAN_POINT('Ctrl Pts',(-58.7276315868069,-77.740213146816,
78.5619509930675));
#209072=CARTESIAN_POINT('Ctrl Pts',(-58.6117511112779,-81.7034874905648,
80.0250683177526));
#209073=CARTESIAN_POINT('Ctrl Pts',(-58.4958706357479,-85.923396000422,
79.8235044369147));
#209074=CARTESIAN_POINT('Ctrl Pts',(-58.3799901602189,-89.7291737336331,
77.9892984302229));
#209075=CARTESIAN_POINT('Ctrl Pts',(-58.2641096846899,-92.5158828633906,
74.8140018998643));
#209076=CARTESIAN_POINT('Ctrl Pts',(-58.1482292091609,-93.8405690494499,
70.8023361189094));
#209077=CARTESIAN_POINT('Ctrl Pts',(-58.0323487336309,-93.4926701311195,
66.5919653309314));
#209078=CARTESIAN_POINT('Ctrl Pts',(-57.9164682581019,-91.5274855058807,
62.8521384340946));
#209079=CARTESIAN_POINT('Ctrl Pts',(-57.8005877825729,-88.2573861527595,
60.1773102058844));
#209080=CARTESIAN_POINT('Ctrl Pts',(-57.6847073070439,-84.2021624890806,
58.992651239347));
#209081=CARTESIAN_POINT('Ctrl Pts',(-57.5688268315149,-80.0064023920941,
59.4864660203554));
#209082=CARTESIAN_POINT('Ctrl Pts',(-57.4529463559859,-76.3370323543386,
61.5802614638165));
#209083=CARTESIAN_POINT('Ctrl Pts',(-57.3370658804569,-73.7773078604179,
64.9412235766449));
#209084=CARTESIAN_POINT('Ctrl Pts',(-57.2211854049279,-72.7341034791027,
69.0351190986164));
#209085=CARTESIAN_POINT('Ctrl Pts',(-57.1053049293989,-73.3732391374036,
73.2112130953808));
#209086=CARTESIAN_POINT('Ctrl Pts',(-56.9894244538699,-75.5931226397066,
76.8057053079184));
#209087=CARTESIAN_POINT('Ctrl Pts',(-56.8735439783409,-79.0408979677858,
79.2472413050084));
#209088=CARTESIAN_POINT('Ctrl Pts',(-56.7576635028119,-83.1685327406974,
80.1477364670454));
#209089=CARTESIAN_POINT('Ctrl Pts',(-56.6417830272829,-87.3199288790655,
79.3640414392398));
#209090=CARTESIAN_POINT('Ctrl Pts',(-56.5259025517539,-90.8352126833059,
77.0207765453072));
#209091=CARTESIAN_POINT('Ctrl Pts',(-56.4100220762249,-93.155617208859,
73.4902227664913));
#209092=CARTESIAN_POINT('Ctrl Pts',(-56.3327684258729,-93.6600875746688,
70.7195859421521));
#209093=CARTESIAN_POINT('Ctrl Pts',(-56.2941416006959,-93.6316506207481,
69.3397002336783));
#209094=CARTESIAN_POINT('Ctrl Pts',(-63.4863639242949,-91.8230019028041,
74.5904921130553));
#209095=CARTESIAN_POINT('Ctrl Pts',(-63.4477370991189,-92.4970812476076,
73.4525899438658));
#209096=CARTESIAN_POINT('Ctrl Pts',(-63.3704834487659,-93.3820044778794,
70.903153272674));
#209097=CARTESIAN_POINT('Ctrl Pts',(-63.2546029732369,-93.1099627814073,
66.863814728757));
#209098=CARTESIAN_POINT('Ctrl Pts',(-63.1387224977069,-91.2813956951746,
63.2519304250261));
#209099=CARTESIAN_POINT('Ctrl Pts',(-63.0228420221779,-88.1870497514119,
60.6414643074804));
#209100=CARTESIAN_POINT('Ctrl Pts',(-62.9069615466489,-84.3187544758582,
59.4473977261369));
#209101=CARTESIAN_POINT('Ctrl Pts',(-62.7910810711199,-80.2913915654904,
59.8595194715136));
#209102=CARTESIAN_POINT('Ctrl Pts',(-62.6752005955899,-76.7451186061521,
61.8123247315614));
#209103=CARTESIAN_POINT('Ctrl Pts',(-62.5593201200609,-74.2436249664418,
64.9954094640758));
#209104=CARTESIAN_POINT('Ctrl Pts',(-62.4434396445319,-73.1845291497573,
68.9028146546496));
#209105=CARTESIAN_POINT('Ctrl Pts',(-62.3275591690019,-73.7361771014411,
72.9134484825933));
#209106=CARTESIAN_POINT('Ctrl Pts',(-62.2116786934729,-75.8108829998573,
76.3898107511057));
#209107=CARTESIAN_POINT('Ctrl Pts',(-62.0957982179439,-79.0788671899051,
78.7793250358795));
#209108=CARTESIAN_POINT('Ctrl Pts',(-61.9799177424139,-83.0206754640438,
79.7021721052772));
#209109=CARTESIAN_POINT('Ctrl Pts',(-61.8640372668849,-87.0097476031586,
79.0116631243528));
#209110=CARTESIAN_POINT('Ctrl Pts',(-61.7481567913549,-90.4120106791324,
76.8175562113822));
#209111=CARTESIAN_POINT('Ctrl Pts',(-61.6322763158259,-92.6866665225346,
73.468610111819));
#209112=CARTESIAN_POINT('Ctrl Pts',(-61.5163958402969,-93.4721529352706,
69.4971481292357));
#209113=CARTESIAN_POINT('Ctrl Pts',(-61.4005153647669,-92.6436149003541,
65.5344440135603));
#209114=CARTESIAN_POINT('Ctrl Pts',(-61.2846348892379,-90.332750597095,
62.210379430011));
#209115=CARTESIAN_POINT('Ctrl Pts',(-61.1687544137079,-86.9068776482263,
60.0533227033745));
#209116=CARTESIAN_POINT('Ctrl Pts',(-61.0528739381789,-82.9105470711673,
59.4061433599308));
#209117=CARTESIAN_POINT('Ctrl Pts',(-60.9369934626489,-78.9789855407346,
60.3717121643543));
#209118=CARTESIAN_POINT('Ctrl Pts',(-60.8211129871199,-75.7371245308333,
62.7965495560486));
#209119=CARTESIAN_POINT('Ctrl Pts',(-60.7052325115899,-73.7002659039675,
66.2952216066778));
#209120=CARTESIAN_POINT('Ctrl Pts',(-60.5893520360609,-73.192173399811,
70.3116057007245));
#209121=CARTESIAN_POINT('Ctrl Pts',(-60.4734715605309,-74.2936095843438,
74.2072876070263));
#209122=CARTESIAN_POINT('Ctrl Pts',(-60.3575910850019,-76.8294984393236,
77.3630390070701));
#209123=CARTESIAN_POINT('Ctrl Pts',(-60.2417106094719,-80.3967541303873,
79.277245374799));
#209124=CARTESIAN_POINT('Ctrl Pts',(-60.1258301339429,-84.4283525019679,
79.6456388518811));
#209125=CARTESIAN_POINT('Ctrl Pts',(-60.0099496584129,-88.2834609756893,
78.4096623797982));
#209126=CARTESIAN_POINT('Ctrl Pts',(-59.8940691828839,-91.3493004809464,
75.765777489781));
#209127=CARTESIAN_POINT('Ctrl Pts',(-59.7781887073549,-93.13854821078,72.1342362543011));
#209128=CARTESIAN_POINT('Ctrl Pts',(-59.6623082318249,-93.3667987928187,
68.0922811759415));
#209129=CARTESIAN_POINT('Ctrl Pts',(-59.5464277562959,-91.997771229922,
64.282391057355));
#209130=CARTESIAN_POINT('Ctrl Pts',(-59.4305472807659,-89.2490758548062,
61.3101573992296));
#209131=CARTESIAN_POINT('Ctrl Pts',(-59.3146668052369,-85.5576246269588,
59.6480241265653));
#209132=CARTESIAN_POINT('Ctrl Pts',(-59.1987863297069,-81.5101828911056,
59.5601914529124));
#209133=CARTESIAN_POINT('Ctrl Pts',(-59.0829058541779,-77.7501015677444,
61.0606205999848));
#209134=CARTESIAN_POINT('Ctrl Pts',(-58.9670253786489,-74.875054925804,
63.9108146267733));
#209135=CARTESIAN_POINT('Ctrl Pts',(-58.8511449031189,-73.3420387725811,
67.6577281109136));
#209136=CARTESIAN_POINT('Ctrl Pts',(-58.7352644275899,-73.3947298346776,
71.7057798442351));
#209137=CARTESIAN_POINT('Ctrl Pts',(-58.6193839520599,-75.0247527368537,
75.4115219456312));
#209138=CARTESIAN_POINT('Ctrl Pts',(-58.5035034765309,-77.9730112887291,
78.1859175005156));
#209139=CARTESIAN_POINT('Ctrl Pts',(-58.3876230010019,-81.7708724680175,
79.5879694419674));
#209140=CARTESIAN_POINT('Ctrl Pts',(-58.2717425254719,-85.8146568038164,
79.394818130247));
#209141=CARTESIAN_POINT('Ctrl Pts',(-58.1558620499429,-89.4615947284621,
77.6371654462713));
#209142=CARTESIAN_POINT('Ctrl Pts',(-58.0399815744139,-92.1319963973636,
74.5943946513581));
#209143=CARTESIAN_POINT('Ctrl Pts',(-57.9241010988849,-93.4013948301736,
70.7501617236546));
#209144=CARTESIAN_POINT('Ctrl Pts',(-57.8082206233549,-93.0680159919581,
66.7155170386891));
#209145=CARTESIAN_POINT('Ctrl Pts',(-57.6923401478259,-91.1848512773756,
63.1317773939326));
#209146=CARTESIAN_POINT('Ctrl Pts',(-57.5764596722969,-88.0512343968762,
60.568587110321));
#209147=CARTESIAN_POINT('Ctrl Pts',(-57.4605791967679,-84.1652615396361,
59.4333716522234));
#209148=CARTESIAN_POINT('Ctrl Pts',(-57.3446987212389,-80.1446177466814,
59.9065763370039));
#209149=CARTESIAN_POINT('Ctrl Pts',(-57.2288182457099,-76.6283943389352,
61.9129841055395));
#209150=CARTESIAN_POINT('Ctrl Pts',(-57.1129377701809,-74.1755037636287,
65.1336714529826));
#209151=CARTESIAN_POINT('Ctrl Pts',(-56.9970572946509,-73.1758390727135,
69.0567021408465));
#209152=CARTESIAN_POINT('Ctrl Pts',(-56.8811768191219,-73.7882994512876,
73.0585006275909));
#209153=CARTESIAN_POINT('Ctrl Pts',(-56.7652963435929,-75.9155328055053,
76.5029713478119));
#209154=CARTESIAN_POINT('Ctrl Pts',(-56.6494158680649,-79.2194100892149,
78.8426061994354));
#209155=CARTESIAN_POINT('Ctrl Pts',(-56.5335353925359,-83.1747718700718,
79.705517853136));
#209156=CARTESIAN_POINT('Ctrl Pts',(-56.4176549170069,-87.1529033003677,
78.9545315059016));
#209157=CARTESIAN_POINT('Ctrl Pts',(-56.3017744414779,-90.5214714933247,
76.7090662664086));
#209158=CARTESIAN_POINT('Ctrl Pts',(-56.1858939659489,-92.7450304759939,
73.3258654140387));
#209159=CARTESIAN_POINT('Ctrl Pts',(-56.1086403155959,-93.2284460188592,
70.6708652489211));
#209160=CARTESIAN_POINT('Ctrl Pts',(-56.0700134904199,-93.2011959236129,
69.348571128068));
#209161=CARTESIAN_POINT('Ctrl Pts',(-63.2622358140189,-91.452573473999,
74.371054836858));
#209162=CARTESIAN_POINT('Ctrl Pts',(-63.2236089888419,-92.0972937684766,
73.282713193911));
#209163=CARTESIAN_POINT('Ctrl Pts',(-63.1463553384899,-92.9436747917172,
70.8443154384341));
#209164=CARTESIAN_POINT('Ctrl Pts',(-63.0304748629609,-92.6834816794201,
66.9809074352464));
#209165=CARTESIAN_POINT('Ctrl Pts',(-62.9145943874309,-90.9345565426601,
63.5263362043601));
#209166=CARTESIAN_POINT('Ctrl Pts',(-62.7987139119019,-87.9749826535781,
61.0295670970088));
#209167=CARTESIAN_POINT('Ctrl Pts',(-62.6828334363729,-84.2751682498535,
59.8875072432627));
#209168=CARTESIAN_POINT('Ctrl Pts',(-62.5669529608439,-80.4232142899493,
60.2816793167476));
#209169=CARTESIAN_POINT('Ctrl Pts',(-62.4510724853139,-77.0313967476354,
62.1494315213011));
#209170=CARTESIAN_POINT('Ctrl Pts',(-62.3351920097849,-74.6388538987226,
65.1938792437981));
#209171=CARTESIAN_POINT('Ctrl Pts',(-62.2193115342559,-73.6258862531933,
68.9311001577751));
#209172=CARTESIAN_POINT('Ctrl Pts',(-62.1034310587259,-74.1535075675003,
72.7670536586458));
#209173=CARTESIAN_POINT('Ctrl Pts',(-61.9875505831969,-76.137851114111,
76.0920054209541));
#209174=CARTESIAN_POINT('Ctrl Pts',(-61.8716701076679,-79.26350055816,78.3774460967395));
#209175=CARTESIAN_POINT('Ctrl Pts',(-61.7557896321379,-83.0336261536677,
79.2600992130555));
#209176=CARTESIAN_POINT('Ctrl Pts',(-61.6399091566089,-86.8489570698533,
78.5996648636749));
#209177=CARTESIAN_POINT('Ctrl Pts',(-61.5240286810789,-90.1030369776855,
76.5011207294713));
#209178=CARTESIAN_POINT('Ctrl Pts',(-61.4081482055499,-92.2786217904858,
73.2980356147633));
#209179=CARTESIAN_POINT('Ctrl Pts',(-61.2922677300209,-93.0298968966431,
69.4995478571636));
#209180=CARTESIAN_POINT('Ctrl Pts',(-61.1763872544909,-92.2374452513553,
65.7094365237526));
#209181=CARTESIAN_POINT('Ctrl Pts',(-61.0605067789619,-90.0272290126204,
62.5301492281784));
#209182=CARTESIAN_POINT('Ctrl Pts',(-60.9446263034319,-86.7505675432666,
60.4670415855671));
#209183=CARTESIAN_POINT('Ctrl Pts',(-60.8287458279029,-82.9282943252811,
59.8480496818692));
#209184=CARTESIAN_POINT('Ctrl Pts',(-60.7128653523729,-79.1679691837779,
60.7715638181681));
#209185=CARTESIAN_POINT('Ctrl Pts',(-60.5969848768439,-76.0673051431882,
63.0907891278659));
#209186=CARTESIAN_POINT('Ctrl Pts',(-60.4811044013139,-74.1191604569068,
66.4370789854654));
#209187=CARTESIAN_POINT('Ctrl Pts',(-60.3652239257849,-73.6331975633271,
70.2785323036529));
#209188=CARTESIAN_POINT('Ctrl Pts',(-60.2493434502549,-74.6866614718425,
74.004540532737));
#209189=CARTESIAN_POINT('Ctrl Pts',(-60.1334629747259,-77.112101476679,
77.0228454067829));
#209190=CARTESIAN_POINT('Ctrl Pts',(-60.0175824991959,-80.5239878626353,
78.8536798665507));
#209191=CARTESIAN_POINT('Ctrl Pts',(-59.9017020236669,-84.3799928112316,
79.2060282256322));
#209192=CARTESIAN_POINT('Ctrl Pts',(-59.7858215481369,-88.0671947549688,
78.0238838368779));
#209193=CARTESIAN_POINT('Ctrl Pts',(-59.6699410726079,-90.9995037833793,
75.4951514881295));
#209194=CARTESIAN_POINT('Ctrl Pts',(-59.5540605970789,-92.7108220905774,
72.0217794692934));
#209195=CARTESIAN_POINT('Ctrl Pts',(-59.4381801215489,-92.9291313795479,
68.1558688929745));
#209196=CARTESIAN_POINT('Ctrl Pts',(-59.3222996460199,-91.6197308463801,
64.5119158508118));
#209197=CARTESIAN_POINT('Ctrl Pts',(-59.2064191704899,-88.9907529592742,
61.6691357328928));
#209198=CARTESIAN_POINT('Ctrl Pts',(-59.0905386949609,-85.4600802855175,
60.079395502359));
#209199=CARTESIAN_POINT('Ctrl Pts',(-58.9746582194309,-81.5889220192099,
59.9953883188284));
#209200=CARTESIAN_POINT('Ctrl Pts',(-58.8587777439019,-77.9926083853276,
61.4304673328671));
#209201=CARTESIAN_POINT('Ctrl Pts',(-58.7428972683729,-75.2427823716655,
64.1565231694806));
#209202=CARTESIAN_POINT('Ctrl Pts',(-58.6270167928429,-73.7765356555165,
67.7402424800745));
#209203=CARTESIAN_POINT('Ctrl Pts',(-58.5111363173139,-73.8269317955608,
71.6119841758515));
#209204=CARTESIAN_POINT('Ctrl Pts',(-58.3952558417839,-75.3859602001198,
75.1563252942432));
#209205=CARTESIAN_POINT('Ctrl Pts',(-58.2793753662549,-78.2058094306096,
77.8098840079436));
#209206=CARTESIAN_POINT('Ctrl Pts',(-58.1634948907259,-81.8382574454312,
79.1508705661768));
#209207=CARTESIAN_POINT('Ctrl Pts',(-58.0476144151959,-85.7059176071747,
78.9661318235942));
#209208=CARTESIAN_POINT('Ctrl Pts',(-57.9317339396669,-89.1940157232479,
77.2850324623463));
#209209=CARTESIAN_POINT('Ctrl Pts',(-57.8158534641379,-91.7481099313085,
74.3747874028884));
#209210=CARTESIAN_POINT('Ctrl Pts',(-57.6999729886089,-92.9622206108914,
70.6979873284379));
#209211=CARTESIAN_POINT('Ctrl Pts',(-57.5840925130789,-92.6433618528013,
66.8390687464838));
#209212=CARTESIAN_POINT('Ctrl Pts',(-57.4682120375499,-90.8422170489019,
63.4114163537942));
#209213=CARTESIAN_POINT('Ctrl Pts',(-57.3523315620209,-87.8450826410214,
60.9598640147741));
#209214=CARTESIAN_POINT('Ctrl Pts',(-57.2364510864919,-84.1283605902155,
59.8740920651051));
#209215=CARTESIAN_POINT('Ctrl Pts',(-57.1205706109629,-80.2828331013019,
60.3266866536539));
#209216=CARTESIAN_POINT('Ctrl Pts',(-57.0046901354339,-76.9197563235507,
62.2457067472406));
#209217=CARTESIAN_POINT('Ctrl Pts',(-56.8888096599039,-74.5736996668511,
65.326119329296));
#209218=CARTESIAN_POINT('Ctrl Pts',(-56.7729291843749,-73.6175746663254,
69.0782851830545));
#209219=CARTESIAN_POINT('Ctrl Pts',(-56.6570487088459,-74.2033597651635,
72.9057881597824));
#209220=CARTESIAN_POINT('Ctrl Pts',(-56.5411682333169,-76.2379429712918,
76.2002373876932));
#209221=CARTESIAN_POINT('Ctrl Pts',(-56.4252877577879,-79.3979222106296,
78.4379710938565));
#209222=CARTESIAN_POINT('Ctrl Pts',(-56.3094072822599,-83.1810109994346,
79.263299239227));
#209223=CARTESIAN_POINT('Ctrl Pts',(-56.1935268067309,-86.9858777216637,
78.545021572567));
#209224=CARTESIAN_POINT('Ctrl Pts',(-56.0776463312019,-90.2077303033346,
76.3973559875148));
#209225=CARTESIAN_POINT('Ctrl Pts',(-55.9617658556729,-92.3344437431285,
73.1615080615852));
#209226=CARTESIAN_POINT('Ctrl Pts',(-55.8845122053199,-92.7968044630577,
70.6221445556835));
#209227=CARTESIAN_POINT('Ctrl Pts',(-55.8458853801439,-92.7707412264758,
69.357442022453));
#209228=CARTESIAN_POINT('Ctrl Pts',(-63.0381077037429,-91.0821450451938,
74.1516175606607));
#209229=CARTESIAN_POINT('Ctrl Pts',(-62.9994808785659,-91.6975062893363,
73.1128364439599));
#209230=CARTESIAN_POINT('Ctrl Pts',(-62.9222272282139,-92.5053451055553,
70.7854776041952));
#209231=CARTESIAN_POINT('Ctrl Pts',(-62.8063467526839,-92.2570005774417,
67.098000141731));
#209232=CARTESIAN_POINT('Ctrl Pts',(-62.6904662771549,-90.5877173901553,
63.8007419836912));
#209233=CARTESIAN_POINT('Ctrl Pts',(-62.5745858016259,-87.7629155557435,
61.4176698865353));
#209234=CARTESIAN_POINT('Ctrl Pts',(-62.4587053260969,-84.2315820238582,
60.3276167603847));
#209235=CARTESIAN_POINT('Ctrl Pts',(-62.3428248505679,-80.5550370144063,
60.7038391619823));
#209236=CARTESIAN_POINT('Ctrl Pts',(-62.2269443750379,-77.3176748891168,
62.4865383110414));
#209237=CARTESIAN_POINT('Ctrl Pts',(-62.1110638995089,-75.0340828310024,
65.3923490235231));
#209238=CARTESIAN_POINT('Ctrl Pts',(-61.9951834239799,-74.0672433566291,
68.9593856609049));
#209239=CARTESIAN_POINT('Ctrl Pts',(-61.8793029484499,-74.570838033561,
72.620658834703));
#209240=CARTESIAN_POINT('Ctrl Pts',(-61.7634224729209,-76.4648192283687,
75.7942000908074));
#209241=CARTESIAN_POINT('Ctrl Pts',(-61.6475419973919,-79.4481339264209,
77.9755671576036));
#209242=CARTESIAN_POINT('Ctrl Pts',(-61.5316615218619,-83.0465768432993,
78.8180263208338));
#209243=CARTESIAN_POINT('Ctrl Pts',(-61.4157810463329,-86.6881665365578,
78.1876666029972));
#209244=CARTESIAN_POINT('Ctrl Pts',(-61.2999005708029,-89.7940632762463,
76.1846852475528));
#209245=CARTESIAN_POINT('Ctrl Pts',(-61.1840200952739,-91.8705770584431,
73.1274611176964));
#209246=CARTESIAN_POINT('Ctrl Pts',(-61.0681396197439,-92.5876408580107,
69.5019475850796));
#209247=CARTESIAN_POINT('Ctrl Pts',(-60.9522591442149,-91.8312756023416,
65.8844290339352));
#209248=CARTESIAN_POINT('Ctrl Pts',(-60.8363786686859,-89.7217074281312,
62.8499190263368));
#209249=CARTESIAN_POINT('Ctrl Pts',(-60.7204981931559,-86.5942574382841,
60.8807604677571));
#209250=CARTESIAN_POINT('Ctrl Pts',(-60.6046177176269,-82.9460415793733,
60.2899560038079));
#209251=CARTESIAN_POINT('Ctrl Pts',(-60.4887372420969,-79.3569528268042,
61.1714154719932));
#209252=CARTESIAN_POINT('Ctrl Pts',(-60.3728567665679,-76.3974857555292,
63.3850286996998));
#209253=CARTESIAN_POINT('Ctrl Pts',(-60.2569762910379,-74.5380550098396,
66.578936364274));
#209254=CARTESIAN_POINT('Ctrl Pts',(-60.1410958155089,-74.0742217268447,
70.2454589066055));
#209255=CARTESIAN_POINT('Ctrl Pts',(-60.0252153399789,-75.0797133593528,
73.8017934584711));
#209256=CARTESIAN_POINT('Ctrl Pts',(-59.9093348644499,-77.3947045140554,
76.682651806513));
#209257=CARTESIAN_POINT('Ctrl Pts',(-59.7934543889199,-80.65122159491,78.430114358312));
#209258=CARTESIAN_POINT('Ctrl Pts',(-59.6775739133909,-84.3316331205256,
78.7664175993805));
#209259=CARTESIAN_POINT('Ctrl Pts',(-59.5616934378609,-87.850928534276,
77.6381052939461));
#209260=CARTESIAN_POINT('Ctrl Pts',(-59.4458129623319,-90.6497070858334,
75.2245254864509));
#209261=CARTESIAN_POINT('Ctrl Pts',(-59.3299324868019,-92.283095970383,
71.9093226842531));
#209262=CARTESIAN_POINT('Ctrl Pts',(-59.2140520112729,-92.4914639662642,
68.2194566099759));
#209263=CARTESIAN_POINT('Ctrl Pts',(-59.0981715357439,-91.2416904628249,
64.7414406442362));
#209264=CARTESIAN_POINT('Ctrl Pts',(-58.9822910602139,-88.7324300637027,
62.0281140665388));
#209265=CARTESIAN_POINT('Ctrl Pts',(-58.8664105846849,-85.3625359440494,
60.5107668781401));
#209266=CARTESIAN_POINT('Ctrl Pts',(-58.7505301091549,-81.6676611472649,
60.4305851847562));
#209267=CARTESIAN_POINT('Ctrl Pts',(-58.6346496336259,-78.2351152028796,
61.8003140657709));
#209268=CARTESIAN_POINT('Ctrl Pts',(-58.5187691580959,-75.6105098175054,
64.4022317122195));
#209269=CARTESIAN_POINT('Ctrl Pts',(-58.4028886825669,-74.2110325384453,
67.822756849275));
#209270=CARTESIAN_POINT('Ctrl Pts',(-58.2870082070379,-74.259133756452,
71.5181885075058));
#209271=CARTESIAN_POINT('Ctrl Pts',(-58.1711277315079,-75.7471676634089,
74.901128642888));
#209272=CARTESIAN_POINT('Ctrl Pts',(-58.0552472559789,-78.4386075725234,
77.4338505153925));
#209273=CARTESIAN_POINT('Ctrl Pts',(-57.9393667804499,-81.9056424228852,
78.7137716903922));
#209274=CARTESIAN_POINT('Ctrl Pts',(-57.8234863049199,-85.5971784105718,
78.5374455169307));
#209275=CARTESIAN_POINT('Ctrl Pts',(-57.7076058293909,-88.9264367180665,
76.9328994783958));
#209276=CARTESIAN_POINT('Ctrl Pts',(-57.5917253538619,-91.3642234652816,
74.1551801543822));
#209277=CARTESIAN_POINT('Ctrl Pts',(-57.4758448783329,-92.523046391615,
70.6458129331831));
#209278=CARTESIAN_POINT('Ctrl Pts',(-57.3599644028029,-92.2187077136396,
66.9626204542406));
#209279=CARTESIAN_POINT('Ctrl Pts',(-57.2440839272739,-90.4995828203968,
63.6910553136321));
#209280=CARTESIAN_POINT('Ctrl Pts',(-57.1282034517449,-87.6389308851381,
61.3511409192107));
#209281=CARTESIAN_POINT('Ctrl Pts',(-57.0123229762159,-84.091459640771,
60.3148124779814));
#209282=CARTESIAN_POINT('Ctrl Pts',(-56.8964425006869,-80.4210484558933,
60.7467969703094));
#209283=CARTESIAN_POINT('Ctrl Pts',(-56.7805620251579,-77.2111183081457,
62.57842938896));
#209284=CARTESIAN_POINT('Ctrl Pts',(-56.6646815496279,-74.9718955700618,
65.5185672056337));
#209285=CARTESIAN_POINT('Ctrl Pts',(-56.5488010740989,-74.0593102599364,
69.0998682252855));
#209286=CARTESIAN_POINT('Ctrl Pts',(-56.4329205985699,-74.6184200790472,
72.7530756919931));
#209287=CARTESIAN_POINT('Ctrl Pts',(-56.3170401230409,-76.560353137091,
75.8975034275876));
#209288=CARTESIAN_POINT('Ctrl Pts',(-56.2011596475119,-79.5764343320587,
78.0333359882835));
#209289=CARTESIAN_POINT('Ctrl Pts',(-56.0852791719829,-83.18725012881,78.8210806253173));
#209290=CARTESIAN_POINT('Ctrl Pts',(-55.9693986964549,-86.8188521429664,
78.1355116392275));
#209291=CARTESIAN_POINT('Ctrl Pts',(-55.8535182209259,-89.8939891133529,
76.0856457086153));
#209292=CARTESIAN_POINT('Ctrl Pts',(-55.7376377453969,-91.9238570102634,
72.9971507091326));
#209293=CARTESIAN_POINT('Ctrl Pts',(-55.6603840950439,-92.3651629072477,
70.5734238624515));
#209294=CARTESIAN_POINT('Ctrl Pts',(-55.6217572698679,-92.3402865293407,
69.3663129168427));
#209295=CARTESIAN_POINT('',(-63.5337774910882,-93.5594520463458,69.970329252864));
#209296=CARTESIAN_POINT('',(-63.5337571161032,-93.5594128863229,69.970328227734));
#209297=CARTESIAN_POINT('Ctrl Pts',(-63.5337978660732,-93.5594912063686,
69.970330277994));
#209298=CARTESIAN_POINT('Ctrl Pts',(-63.5216568454269,-93.5772513864428,
69.5352741201867));
#209299=CARTESIAN_POINT('Ctrl Pts',(-63.5094960824503,-93.567271818938,
69.0995306219549));
#209300=CARTESIAN_POINT('Ctrl Pts',(-63.4851355856958,-93.4926516929353,
68.2399799410843));
#209301=CARTESIAN_POINT('Ctrl Pts',(-63.4729651705743,-93.4290976072566,
67.8169422519278));
#209302=CARTESIAN_POINT('Ctrl Pts',(-63.4379180895563,-93.1701049116124,
66.6115153529615));
#209303=CARTESIAN_POINT('Ctrl Pts',(-63.4157214108481,-92.9086267996816,
65.8466098604295));
#209304=CARTESIAN_POINT('Ctrl Pts',(-63.3779422794529,-92.3269878674592,
64.6336904127012));
#209305=CARTESIAN_POINT('Ctrl Pts',(-63.3626137085537,-92.0556170188198,
64.1663309373524));
#209306=CARTESIAN_POINT('Ctrl Pts',(-63.3174905710142,-91.1530081274075,
62.8610167967825));
#209307=CARTESIAN_POINT('Ctrl Pts',(-63.2888250790043,-90.4287485210572,
62.0958974953315));
#209308=CARTESIAN_POINT('Ctrl Pts',(-63.2498582130389,-89.3411459094481,
61.2520762780945));
#209309=CARTESIAN_POINT('Ctrl Pts',(-63.2404883841634,-89.0715219048256,
61.0629540782528));
#209310=CARTESIAN_POINT('Ctrl Pts',(-63.2015300107886,-87.9132450973876,
60.3310706918349));
#209311=CARTESIAN_POINT('Ctrl Pts',(-63.1730383758105,-86.9536282367546,
59.9123017459371));
#209312=CARTESIAN_POINT('Ctrl Pts',(-63.134252165677,-85.6291328319174,
59.5607618447651));
#209313=CARTESIAN_POINT('Ctrl Pts',(-63.1248770310096,-85.3069013144664,
59.4916621526057));
#209314=CARTESIAN_POINT('Ctrl Pts',(-63.085746995258,-83.9490150716827,
59.2682734165905));
#209315=CARTESIAN_POINT('Ctrl Pts',(-63.0570979218165,-82.8961668763337,
59.2575730468926));
#209316=CARTESIAN_POINT('Ctrl Pts',(-63.0181490486881,-81.5341877143882,
59.4532947949565));
#209317=CARTESIAN_POINT('Ctrl Pts',(-63.0087782602271,-81.2107874689418,
59.5157903455767));
#209318=CARTESIAN_POINT('Ctrl Pts',(-62.9697840933728,-79.878386152212,
59.8405200251187));
#209319=CARTESIAN_POINT('Ctrl Pts',(-62.9412592415125,-78.9093534753847,
60.2402985218569));
#209320=CARTESIAN_POINT('Ctrl Pts',(-62.896957577525,-77.5697157187439,
61.049717858937));
#209321=CARTESIAN_POINT('Ctrl Pts',(-62.8820052873794,-77.1434642908388,
61.3540239697376));
#209322=CARTESIAN_POINT('Ctrl Pts',(-62.857887191323,-76.4879137579722,
61.9022713082005));
#209323=CARTESIAN_POINT('Ctrl Pts',(-62.8486522391764,-76.2440012611628,
62.1272393924664));
#209324=CARTESIAN_POINT('Ctrl Pts',(-62.8017138500491,-75.063531698435,
63.3270843462837));
#209325=CARTESIAN_POINT('Ctrl Pts',(-62.76323536298,-74.3154953579531,64.468569951771));
#209326=CARTESIAN_POINT('Ctrl Pts',(-62.6904861241906,-73.3407129438074,
66.8883539708659));
#209327=CARTESIAN_POINT('Ctrl Pts',(-62.6546385270754,-73.089478660267,
68.1310048344221));
#209328=CARTESIAN_POINT('Ctrl Pts',(-62.6006605552128,-73.0585228854009,
70.062917874554));
#209329=CARTESIAN_POINT('Ctrl Pts',(-62.5819189575496,-73.1143987731514,
70.7372259394319));
#209330=CARTESIAN_POINT('Ctrl Pts',(-62.543672183343,-73.3580133050627,
72.0656433597821));
#209331=CARTESIAN_POINT('Ctrl Pts',(-62.52435918621,-73.5452782999503,72.7164894035513));
#209332=CARTESIAN_POINT('Ctrl Pts',(-62.5042445607632,-73.8114572910648,
73.3849557517124));
#209333=CARTESIAN_POINT('Ctrl Pts',(-62.503018276399,-73.8279591515225,
73.4256350243488));
#209334=CARTESIAN_POINT('Ctrl Pts',(-62.5017927901943,-73.8447192658304,
73.466201051278));
#209335=CARTESIAN_POINT('',(-56.402655786563,-92.4407016401285,74.2253115652726));
#209336=CARTESIAN_POINT('Ctrl Pts',(-56.5793858481529,-89.1716495247985,
78.0464295027995));
#209337=CARTESIAN_POINT('Ctrl Pts',(-56.5407590229759,-90.3081071926132,
77.2632582583921));
#209338=CARTESIAN_POINT('Ctrl Pts',(-56.4635053726229,-92.2618542008096,
75.2350099031932));
#209339=CARTESIAN_POINT('Ctrl Pts',(-56.3476248970939,-93.7712830739489,
71.289035799845));
#209340=CARTESIAN_POINT('Ctrl Pts',(-56.2317444215639,-93.6190186885821,
67.0670781799152));
#209341=CARTESIAN_POINT('Ctrl Pts',(-56.1158639460339,-91.8294176899935,
63.2401216789652));
#209342=CARTESIAN_POINT('Ctrl Pts',(-55.9999834705049,-88.686900381402,
60.4164989490926));
#209343=CARTESIAN_POINT('Ctrl Pts',(-55.8841029949749,-84.6909887425699,
59.0450242272283));
#209344=CARTESIAN_POINT('Ctrl Pts',(-55.7682225194459,-80.4768398974234,
59.3436988676507));
#209345=CARTESIAN_POINT('Ctrl Pts',(-55.6523420439159,-76.7143040687269,
61.2650472476524));
#209346=CARTESIAN_POINT('Ctrl Pts',(-55.5364615683869,-74.0014454626398,
64.5036664147486));
#209347=CARTESIAN_POINT('Ctrl Pts',(-55.4205810928579,-72.7694797521119,
68.5447697661598));
#209348=CARTESIAN_POINT('Ctrl Pts',(-55.3047006173279,-73.2142309326136,
72.746013893864));
#209349=CARTESIAN_POINT('Ctrl Pts',(-55.1888201417989,-75.2650047030302,
76.4396006022121));
#209350=CARTESIAN_POINT('Ctrl Pts',(-55.0729396662689,-78.5958254759494,
79.0384251072975));
#209351=CARTESIAN_POINT('Ctrl Pts',(-54.9570591907399,-82.6772510137972,
80.1293977965975));
#209352=CARTESIAN_POINT('Ctrl Pts',(-54.8411787152099,-86.8605285862284,
79.5391058504835));
#209353=CARTESIAN_POINT('Ctrl Pts',(-54.7252982396809,-90.4807158290425,
77.3613776404707));
#209354=CARTESIAN_POINT('Ctrl Pts',(-54.6094177641509,-92.9623749849825,
73.9423684764853));
#209355=CARTESIAN_POINT('Ctrl Pts',(-54.4935372886209,-93.9110401651089,
69.8255383602718));
#209356=CARTESIAN_POINT('Ctrl Pts',(-54.3776568130909,-93.1759186818892,
65.6652676678046));
#209357=CARTESIAN_POINT('Ctrl Pts',(-54.2617763375609,-90.8738599216446,
62.1228417625684));
#209358=CARTESIAN_POINT('Ctrl Pts',(-54.1458958620309,-87.3707818441818,
59.7613380439862));
#209359=CARTESIAN_POINT('Ctrl Pts',(-54.0300153865009,-83.2235074139119,
58.956123395707));
#209360=CARTESIAN_POINT('Ctrl Pts',(-53.9141349109709,-79.0912562061879,
59.8351886867613));
#209361=CARTESIAN_POINT('Ctrl Pts',(-53.7982544354409,-75.6308598177706,
62.258804304951));
#209362=CARTESIAN_POINT('Ctrl Pts',(-53.6823739599209,-73.3923568525672,
65.8417305258611));
#209363=CARTESIAN_POINT('Ctrl Pts',(-53.5664934843909,-72.7315629188536,
70.0144523242639));
#209364=CARTESIAN_POINT('Ctrl Pts',(-53.4506130088609,-73.7535128542524,
74.113705202441));
#209365=CARTESIAN_POINT('Ctrl Pts',(-53.3347325333309,-76.2957651773164,
77.487902730087));
#209366=CARTESIAN_POINT('Ctrl Pts',(-53.2188520578009,-79.9542225646198,
79.6007078263948));
#209367=CARTESIAN_POINT('Ctrl Pts',(-53.1029715822709,-84.1473641243655,
80.1162848716646));
#209368=CARTESIAN_POINT('Ctrl Pts',(-52.9870911067409,-88.2086795870379,
78.9526816135227));
#209369=CARTESIAN_POINT('Ctrl Pts',(-52.8712106312109,-91.4926127687853,
76.2948556810079));
#209370=CARTESIAN_POINT('Ctrl Pts',(-52.7553301556809,-93.477174330855,
72.5652751099481));
#209371=CARTESIAN_POINT('Ctrl Pts',(-52.6394496801509,-93.84691328197,68.3567659989079));
#209372=CARTESIAN_POINT('Ctrl Pts',(-52.5235692046209,-92.5430586971659,
64.338281327871));
#209373=CARTESIAN_POINT('Ctrl Pts',(-52.4076887290909,-89.7728615023466,
61.1485692199366));
#209374=CARTESIAN_POINT('Ctrl Pts',(-52.2918082535609,-85.9766514246951,
59.2946423400516));
#209375=CARTESIAN_POINT('Ctrl Pts',(-52.1759277780309,-81.7578454883824,
59.0711869721971));
#209376=CARTESIAN_POINT('Ctrl Pts',(-52.0600473025109,-77.7870333793684,
60.5137219022862));
#209377=CARTESIAN_POINT('Ctrl Pts',(-51.9441668269809,-74.6953855485565,
63.3929526189662));
#209378=CARTESIAN_POINT('Ctrl Pts',(-51.8282863514509,-72.9743271003957,
67.2512182458574));
#209379=CARTESIAN_POINT('Ctrl Pts',(-51.7124058759209,-72.8974245514948,
71.4752378750255));
#209380=CARTESIAN_POINT('Ctrl Pts',(-51.5965254003909,-74.4769017530788,
75.3935930910951));
#209381=CARTESIAN_POINT('Ctrl Pts',(-51.4806449248609,-77.4616968794652,
78.383451596628));
#209382=CARTESIAN_POINT('Ctrl Pts',(-51.3647644493309,-81.3773693290668,
79.9695679533435));
#209383=CARTESIAN_POINT('Ctrl Pts',(-51.2488839738009,-85.6015132368418,
79.8998250253565));
#209384=CARTESIAN_POINT('Ctrl Pts',(-51.1330034982709,-89.462690433018,
78.1853086243629));
#209385=CARTESIAN_POINT('Ctrl Pts',(-51.0171230227409,-92.3471572085029,
75.0985453923105));
#209386=CARTESIAN_POINT('Ctrl Pts',(-50.9012425472109,-93.7964204023591,
71.1301840145485));
#209387=CARTESIAN_POINT('Ctrl Pts',(-50.7853620716809,-93.5801160289695,
66.9110053921681));
#209388=CARTESIAN_POINT('Ctrl Pts',(-50.6694815961509,-91.7326262059582,
63.111658450455));
#209389=CARTESIAN_POINT('Ctrl Pts',(-50.5536011206309,-88.5476140310613,
60.3360588260279));
#209390=CARTESIAN_POINT('Ctrl Pts',(-50.4377206451009,-84.5313451033357,
59.0253949753285));
#209391=CARTESIAN_POINT('Ctrl Pts',(-50.3218401695709,-80.3222153474369,
59.3880001752185));
#209392=CARTESIAN_POINT('Ctrl Pts',(-50.2059596940409,-76.5892763983811,
61.3662374236589));
#209393=CARTESIAN_POINT('Ctrl Pts',(-50.0900792185109,-73.9258881698316,
64.6456610117156));
#209394=CARTESIAN_POINT('Ctrl Pts',(-49.9741987429809,-72.7554028660613,
68.7049983484054));
#209395=CARTESIAN_POINT('Ctrl Pts',(-49.8583182674509,-73.2638719310397,
72.8990079143938));
#209396=CARTESIAN_POINT('Ctrl Pts',(-49.7424377919209,-75.3704733291652,
76.5610405859094));
#209397=CARTESIAN_POINT('Ctrl Pts',(-49.6265573163909,-78.7403560946919,
79.1090104644245));
#209398=CARTESIAN_POINT('Ctrl Pts',(-49.5106768408609,-82.8378743604903,
80.1378991151166));
#209399=CARTESIAN_POINT('Ctrl Pts',(-49.3947963653309,-87.0116973704533,
79.4842080039733));
#209400=CARTESIAN_POINT('Ctrl Pts',(-49.2789158898109,-90.5984604020873,
77.251671755215));
#209401=CARTESIAN_POINT('Ctrl Pts',(-49.2016622394509,-92.2179930301717,
74.9477549101844));
#209402=CARTESIAN_POINT('Ctrl Pts',(-49.1630354142809,-92.7706651531469,
73.6830625549966));
#209403=CARTESIAN_POINT('Ctrl Pts',(-56.3552577378769,-88.9273396238135,
77.6919120683441));
#209404=CARTESIAN_POINT('Ctrl Pts',(-56.3166309126999,-90.0163655362671,
76.9414276436266));
#209405=CARTESIAN_POINT('Ctrl Pts',(-56.2393772623469,-91.8885699997907,
74.9978312579016));
#209406=CARTESIAN_POINT('Ctrl Pts',(-56.1234967868169,-93.335000608173,
71.2165482676822));
#209407=CARTESIAN_POINT('Ctrl Pts',(-56.0076163112879,-93.1890912039718,
67.1708003444751));
#209408=CARTESIAN_POINT('Ctrl Pts',(-55.8917358357579,-91.4741818715764,
63.5035675795474));
#209409=CARTESIAN_POINT('Ctrl Pts',(-55.7758553602289,-88.4628222087298,
60.7977929546752));
#209410=CARTESIAN_POINT('Ctrl Pts',(-55.6599748846989,-84.6336859005426,
59.4835587753601));
#209411=CARTESIAN_POINT('Ctrl Pts',(-55.5440944091699,-80.5954208412564,
59.7697677843112));
#209412=CARTESIAN_POINT('Ctrl Pts',(-55.4282139336399,-76.9899200557673,
61.6109258247081));
#209413=CARTESIAN_POINT('Ctrl Pts',(-55.3123334581109,-74.3902866488067,
64.7143763916865));
#209414=CARTESIAN_POINT('Ctrl Pts',(-55.1964529825809,-73.2097388642188,
68.58681826895));
#209415=CARTESIAN_POINT('Ctrl Pts',(-55.0805725070519,-73.6359276910248,
72.6127172084169));
#209416=CARTESIAN_POINT('Ctrl Pts',(-54.9646920315229,-75.6011093601795,
76.152146567904));
#209417=CARTESIAN_POINT('Ctrl Pts',(-54.8488115559929,-78.7929133614815,
78.6425052571067));
#209418=CARTESIAN_POINT('Ctrl Pts',(-54.7329310804639,-82.7039945186047,
79.687944574445));
#209419=CARTESIAN_POINT('Ctrl Pts',(-54.6170506049339,-86.7126767637781,
79.1222893429069));
#209420=CARTESIAN_POINT('Ctrl Pts',(-54.5011701294009,-90.1817700938727,
77.035451866986));
#209421=CARTESIAN_POINT('Ctrl Pts',(-54.3852896538709,-92.5598535044851,
73.7591401486176));
#209422=CARTESIAN_POINT('Ctrl Pts',(-54.2694091783509,-93.4689247287331,
69.8141320760029));
#209423=CARTESIAN_POINT('Ctrl Pts',(-54.1535287028209,-92.764484636779,
65.8274964843525));
#209424=CARTESIAN_POINT('Ctrl Pts',(-54.0376482272909,-90.5585057315378,
62.4329190064618));
#209425=CARTESIAN_POINT('Ctrl Pts',(-53.9217677517609,-87.2016338411459,
60.1699761668685));
#209426=CARTESIAN_POINT('Ctrl Pts',(-53.8058872762309,-83.2274520933251,
59.3983683526049));
#209427=CARTESIAN_POINT('Ctrl Pts',(-53.6900068007009,-79.2676665514421,
60.2407445429474));
#209428=CARTESIAN_POINT('Ctrl Pts',(-53.5741263251709,-75.9516949661677,
62.5632069494066));
#209429=CARTESIAN_POINT('Ctrl Pts',(-53.4582458496409,-73.8066192600998,
65.9965944019082));
#209430=CARTESIAN_POINT('Ctrl Pts',(-53.3423653741109,-73.1734045465354,
69.9951614340195));
#209431=CARTESIAN_POINT('Ctrl Pts',(-53.2264848985809,-74.15270187753,73.9233258808396));
#209432=CARTESIAN_POINT('Ctrl Pts',(-53.1106044230509,-76.5888495090847,
77.1566962433291));
#209433=CARTESIAN_POINT('Ctrl Pts',(-52.9947239475209,-80.0946157221245,
79.1813202684909));
#209434=CARTESIAN_POINT('Ctrl Pts',(-52.8788434719909,-84.1127502663909,
79.6753789369893));
#209435=CARTESIAN_POINT('Ctrl Pts',(-52.7629629964609,-88.0045606723086,
78.5603403958907));
#209436=CARTESIAN_POINT('Ctrl Pts',(-52.6470825209309,-91.1514340059658,
76.0134427918171));
#209437=CARTESIAN_POINT('Ctrl Pts',(-52.5312020454009,-93.053166932025,
72.4395218271453));
#209438=CARTESIAN_POINT('Ctrl Pts',(-52.4153215698809,-93.4074742766868,
68.4066611192533));
#209439=CARTESIAN_POINT('Ctrl Pts',(-52.2994410943509,-92.1580380071747,
64.5558938980169));
#209440=CARTESIAN_POINT('Ctrl Pts',(-52.1835606188209,-89.5034591229898,
61.4993091811534));
#209441=CARTESIAN_POINT('Ctrl Pts',(-52.0676801432909,-85.8656895335373,
59.7227587040344));
#209442=CARTESIAN_POINT('Ctrl Pts',(-51.9517996677609,-81.8229617537302,
59.5086295791554));
#209443=CARTESIAN_POINT('Ctrl Pts',(-51.8359191922309,-78.0178774090514,
60.8909581629449));
#209444=CARTESIAN_POINT('Ctrl Pts',(-51.7200387167009,-75.0552641104844,
63.6500198923845));
#209445=CARTESIAN_POINT('Ctrl Pts',(-51.6041582411709,-73.4060366029682,
67.3472550501956));
#209446=CARTESIAN_POINT('Ctrl Pts',(-51.4882777656409,-73.3323436966194,
71.3949789216125));
#209447=CARTESIAN_POINT('Ctrl Pts',(-51.3723972901109,-74.8458990620047,
75.1497957399931));
#209448=CARTESIAN_POINT('Ctrl Pts',(-51.2565168145809,-77.7061193131001,
78.0148680425531));
#209449=CARTESIAN_POINT('Ctrl Pts',(-51.1406363390509,-81.4583653342733,
79.534785468025));
#209450=CARTESIAN_POINT('Ctrl Pts',(-51.0247558635209,-85.5062082973436,
79.4679533651301));
#209451=CARTESIAN_POINT('Ctrl Pts',(-50.9088753880009,-89.206233505757,
77.8249948626797));
#209452=CARTESIAN_POINT('Ctrl Pts',(-50.7929949124709,-91.9703127592713,
74.8670622968578));
#209453=CARTESIAN_POINT('Ctrl Pts',(-50.6771144369409,-93.3590887926927,
71.06432639851));
#209454=CARTESIAN_POINT('Ctrl Pts',(-50.5612339614109,-93.1518122048732,
67.0212414872382));
#209455=CARTESIAN_POINT('Ctrl Pts',(-50.4453534858809,-91.3814301244552,
63.3804659554293));
#209456=CARTESIAN_POINT('Ctrl Pts',(-50.3294730103509,-88.3293491819053,
60.7207101200916));
#209457=CARTESIAN_POINT('Ctrl Pts',(-50.2135925348209,-84.4807052266326,
59.4647487795594));
#209458=CARTESIAN_POINT('Ctrl Pts',(-50.0977120592909,-80.447249777423,
59.8122201107395));
#209459=CARTESIAN_POINT('Ctrl Pts',(-49.9818315837609,-76.8701106016706,
61.7078926778295));
#209460=CARTESIAN_POINT('Ctrl Pts',(-49.8659511082309,-74.3178828522775,
64.8504446324207));
#209461=CARTESIAN_POINT('Ctrl Pts',(-49.7500706327009,-73.1962494979973,
68.7403594723971));
#209462=CARTESIAN_POINT('Ctrl Pts',(-49.6341901571709,-73.6834968483606,
72.7593257953695));
#209463=CARTESIAN_POINT('Ctrl Pts',(-49.5183096816509,-75.7021760959367,
76.2685180728017));
#209464=CARTESIAN_POINT('Ctrl Pts',(-49.4024292061209,-78.9314117793381,
78.710144629103));
#209465=CARTESIAN_POINT('Ctrl Pts',(-49.2865487305909,-82.8579140104155,
79.6960910777588));
#209466=CARTESIAN_POINT('Ctrl Pts',(-49.1706682550609,-86.8575362933791,
79.0696827398739));
#209467=CARTESIAN_POINT('Ctrl Pts',(-49.0547877795309,-90.2946004215829,
76.9303247204407));
#209468=CARTESIAN_POINT('Ctrl Pts',(-48.9775341291809,-91.8465394405205,
74.7225652803544));
#209469=CARTESIAN_POINT('Ctrl Pts',(-48.9389073040009,-92.3761449683377,
73.5106567464228));
#209470=CARTESIAN_POINT('Ctrl Pts',(-56.1311296275999,-88.6830297228196,
77.3373946338934));
#209471=CARTESIAN_POINT('Ctrl Pts',(-56.0925028024239,-89.7246238799117,
76.6195970288649));
#209472=CARTESIAN_POINT('Ctrl Pts',(-56.0152491520709,-91.5152857987813,
74.760652612607));
#209473=CARTESIAN_POINT('Ctrl Pts',(-55.8993686765409,-92.8987181423976,
71.1440607355203));
#209474=CARTESIAN_POINT('Ctrl Pts',(-55.7834882010119,-92.7591637193615,
67.274522509035));
#209475=CARTESIAN_POINT('Ctrl Pts',(-55.6676077254819,-91.1189460531508,
63.7670134801353));
#209476=CARTESIAN_POINT('Ctrl Pts',(-55.5517272499529,-88.2387440360669,
61.179086960254));
#209477=CARTESIAN_POINT('Ctrl Pts',(-55.4358467744229,-84.5763830585068,
59.9220933234976));
#209478=CARTESIAN_POINT('Ctrl Pts',(-55.3199662988939,-80.7140017850856,
60.1958367009625));
#209479=CARTESIAN_POINT('Ctrl Pts',(-55.2040858233639,-77.2655360428094,
61.9568044017577));
#209480=CARTESIAN_POINT('Ctrl Pts',(-55.0882053478349,-74.7791278349758,
64.9250863686191));
#209481=CARTESIAN_POINT('Ctrl Pts',(-54.9723248723049,-73.6499979763262,
68.6288667717323));
#209482=CARTESIAN_POINT('Ctrl Pts',(-54.8564443967759,-74.0576244494326,
72.4794205229618));
#209483=CARTESIAN_POINT('Ctrl Pts',(-54.7405639212469,-75.9372140173222,
75.8646925335888));
#209484=CARTESIAN_POINT('Ctrl Pts',(-54.6246834457169,-78.9900012470032,
78.2465854069093));
#209485=CARTESIAN_POINT('Ctrl Pts',(-54.5088029701909,-82.7307380233984,
79.2464913522906));
#209486=CARTESIAN_POINT('Ctrl Pts',(-54.3929224946609,-86.5648249413073,
78.7054728353225));
#209487=CARTESIAN_POINT('Ctrl Pts',(-54.2770420191309,-89.8828243586779,
76.7095260935192));
#209488=CARTESIAN_POINT('Ctrl Pts',(-54.1611615436009,-92.1573320239741,
73.5759118207695));
#209489=CARTESIAN_POINT('Ctrl Pts',(-54.0452810680709,-93.026809292365,
69.8027257917525));
#209490=CARTESIAN_POINT('Ctrl Pts',(-53.9294005925409,-92.353050591669,
65.9897253009272));
#209491=CARTESIAN_POINT('Ctrl Pts',(-53.8135201170109,-90.2431515414503,
62.7429962503755));
#209492=CARTESIAN_POINT('Ctrl Pts',(-53.6976396414809,-87.0324858381458,
60.5786142897588));
#209493=CARTESIAN_POINT('Ctrl Pts',(-53.5817591659509,-83.2313967727705,
59.8406133095025));
#209494=CARTESIAN_POINT('Ctrl Pts',(-53.4658786904209,-79.4440768967273,
60.6463003991196));
#209495=CARTESIAN_POINT('Ctrl Pts',(-53.3499982148909,-76.2725301145909,
62.8676095938363));
#209496=CARTESIAN_POINT('Ctrl Pts',(-53.2341177393609,-74.2208816676457,
66.1514582779195));
#209497=CARTESIAN_POINT('Ctrl Pts',(-53.1182372638309,-73.6152461742155,
69.9758705437336));
#209498=CARTESIAN_POINT('Ctrl Pts',(-53.0023567883009,-74.5518909007893,
73.7329465591992));
#209499=CARTESIAN_POINT('Ctrl Pts',(-52.8864763127809,-76.8819338408193,
76.8254897565407));
#209500=CARTESIAN_POINT('Ctrl Pts',(-52.7705958372509,-80.2350088795841,
78.761932710572));
#209501=CARTESIAN_POINT('Ctrl Pts',(-52.6547153617209,-84.0781364083665,
79.234473002314));
#209502=CARTESIAN_POINT('Ctrl Pts',(-52.5388348861909,-87.8004417575374,
78.167999178288));
#209503=CARTESIAN_POINT('Ctrl Pts',(-52.4229544106609,-90.8102552431185,
75.7320299026639));
#209504=CARTESIAN_POINT('Ctrl Pts',(-52.3070739351309,-92.6291595331741,
72.3137685443966));
#209505=CARTESIAN_POINT('Ctrl Pts',(-52.1911934596009,-92.9680352714057,
68.4565562396562));
#209506=CARTESIAN_POINT('Ctrl Pts',(-52.0753129840709,-91.7730173172237,
64.7735064682078));
#209507=CARTESIAN_POINT('Ctrl Pts',(-51.9594325085409,-89.2340567436806,
61.8500491424068));
#209508=CARTESIAN_POINT('Ctrl Pts',(-51.8435520330109,-85.7547276424399,
60.1508750680323));
#209509=CARTESIAN_POINT('Ctrl Pts',(-51.7276715574809,-81.8880780191402,
59.9460721861074));
#209510=CARTESIAN_POINT('Ctrl Pts',(-51.6117910819509,-78.2487214387897,
61.2681944235775));
#209511=CARTESIAN_POINT('Ctrl Pts',(-51.4959106064209,-75.4151426724483,
63.9070871657534));
#209512=CARTESIAN_POINT('Ctrl Pts',(-51.3800301308909,-73.837746105554,
67.443291854472));
#209513=CARTESIAN_POINT('Ctrl Pts',(-51.2641496553709,-73.7672628417323,
71.3147199681372));
#209514=CARTESIAN_POINT('Ctrl Pts',(-51.1482691798409,-75.2148963708959,
74.9059983888393));
#209515=CARTESIAN_POINT('Ctrl Pts',(-51.0323887043109,-77.9505417466829,
77.6462844884434));
#209516=CARTESIAN_POINT('Ctrl Pts',(-50.9165082287809,-81.5393613394195,
79.1000029826967));
#209517=CARTESIAN_POINT('Ctrl Pts',(-50.8006277532509,-85.4109033577874,
79.0360817049178));
#209518=CARTESIAN_POINT('Ctrl Pts',(-50.6847472777209,-88.9497765784368,
77.4646811010361));
#209519=CARTESIAN_POINT('Ctrl Pts',(-50.5688668021909,-91.5934683099975,
74.6355792014604));
#209520=CARTESIAN_POINT('Ctrl Pts',(-50.4529863266609,-92.9217571830265,
70.9984687825244));
#209521=CARTESIAN_POINT('Ctrl Pts',(-50.3371058511309,-92.7235083807798,
67.1314775823677));
#209522=CARTESIAN_POINT('Ctrl Pts',(-50.2212253756009,-91.0302340429712,
63.6492734604498));
#209523=CARTESIAN_POINT('Ctrl Pts',(-50.1053449000709,-88.1110843328011,
61.105361414176));
#209524=CARTESIAN_POINT('Ctrl Pts',(-49.9894644245409,-84.4300653499657,
59.9041025837992));
#209525=CARTESIAN_POINT('Ctrl Pts',(-49.8735839490209,-80.5722842074503,
60.2364400462553));
#209526=CARTESIAN_POINT('Ctrl Pts',(-49.7577034734909,-77.1509448049911,
62.0495479319753));
#209527=CARTESIAN_POINT('Ctrl Pts',(-49.6418229979609,-74.7098775347402,
65.055228253093));
#209528=CARTESIAN_POINT('Ctrl Pts',(-49.5259425224309,-73.6370961299356,
68.7757205963565));
#209529=CARTESIAN_POINT('Ctrl Pts',(-49.4100620469009,-74.1031217656728,
72.6196436763184));
#209530=CARTESIAN_POINT('Ctrl Pts',(-49.2941815713709,-76.0338788626926,
75.9759955596767));
#209531=CARTESIAN_POINT('Ctrl Pts',(-49.1783010958409,-79.1224674639693,
78.3112787937738));
#209532=CARTESIAN_POINT('Ctrl Pts',(-49.0624206203109,-82.8779536603277,
79.254283040401));
#209533=CARTESIAN_POINT('Ctrl Pts',(-48.9465401447809,-86.7033752162974,
78.6551574757721));
#209534=CARTESIAN_POINT('Ctrl Pts',(-48.8306596692509,-89.9907404410874,
76.6089776856617));
#209535=CARTESIAN_POINT('Ctrl Pts',(-48.7534060189009,-91.4750858508685,
74.4973756505227));
#209536=CARTESIAN_POINT('Ctrl Pts',(-48.7147791937209,-91.9816247835266,
73.3382509378444));
#209537=CARTESIAN_POINT('Ctrl Pts',(-55.9070015173239,-88.4387198218353,
76.9828771994399));
#209538=CARTESIAN_POINT('Ctrl Pts',(-55.8683746921479,-89.4328822235564,
76.2977664141032));
#209539=CARTESIAN_POINT('Ctrl Pts',(-55.7911210417949,-91.1420015977624,
74.5234739673153));
#209540=CARTESIAN_POINT('Ctrl Pts',(-55.6752405662649,-92.4624356766218,
71.0715732033575));
#209541=CARTESIAN_POINT('Ctrl Pts',(-55.5593600907359,-92.32923623476,67.3782446735901));
#209542=CARTESIAN_POINT('Ctrl Pts',(-55.4434796152059,-90.7637102347341,
64.0304593807184));
#209543=CARTESIAN_POINT('Ctrl Pts',(-55.3275991396769,-88.0146658633944,
61.5603809658357));
#209544=CARTESIAN_POINT('Ctrl Pts',(-55.2117186641469,-84.5190802164795,
60.3606278716294));
#209545=CARTESIAN_POINT('Ctrl Pts',(-55.0958381886179,-80.8325827289163,
60.6219056176175));
#209546=CARTESIAN_POINT('Ctrl Pts',(-54.9799577130879,-77.5411520298483,
62.3026829788096));
#209547=CARTESIAN_POINT('Ctrl Pts',(-54.8640772375589,-75.1679690211427,
65.135796345557));
#209548=CARTESIAN_POINT('Ctrl Pts',(-54.7481967620289,-74.0902570884328,
68.6709152745216));
#209549=CARTESIAN_POINT('Ctrl Pts',(-54.6323162864999,-74.4793212078432,
72.3461238375152));
#209550=CARTESIAN_POINT('Ctrl Pts',(-54.5164358109709,-76.2733186744711,
75.5772384992808));
#209551=CARTESIAN_POINT('Ctrl Pts',(-54.4005553354409,-79.1870891325353,
77.8506655567185));
#209552=CARTESIAN_POINT('Ctrl Pts',(-54.2846748599109,-82.7574815282069,
78.8050381301377));
#209553=CARTESIAN_POINT('Ctrl Pts',(-54.1687943843809,-86.416973118854,
78.2886563277362));
#209554=CARTESIAN_POINT('Ctrl Pts',(-54.0529139088509,-89.5838786235081,
76.3836003200345));
#209555=CARTESIAN_POINT('Ctrl Pts',(-53.9370334333209,-91.7548105434674,
73.3926834929055));
#209556=CARTESIAN_POINT('Ctrl Pts',(-53.8211529577909,-92.5846938559892,
69.7913195074835));
#209557=CARTESIAN_POINT('Ctrl Pts',(-53.7052724822609,-91.9416165465586,
66.1519541174746));
#209558=CARTESIAN_POINT('Ctrl Pts',(-53.5893920067309,-89.9277973513432,
63.053073494268));
#209559=CARTESIAN_POINT('Ctrl Pts',(-53.4735115312009,-86.8633378351191,
60.9872524126373));
#209560=CARTESIAN_POINT('Ctrl Pts',(-53.3576310556809,-83.2353414521743,
60.2828582664042));
#209561=CARTESIAN_POINT('Ctrl Pts',(-53.2417505801509,-79.6204872419811,
61.0518562553048));
#209562=CARTESIAN_POINT('Ctrl Pts',(-53.1258701046209,-76.5933652629879,
63.172012238292));
#209563=CARTESIAN_POINT('Ctrl Pts',(-53.0099896290909,-74.6351440751773,
66.306322153967));
#209564=CARTESIAN_POINT('Ctrl Pts',(-52.8941091535609,-74.0570878018971,
69.9565796534892));
#209565=CARTESIAN_POINT('Ctrl Pts',(-52.7782286780309,-74.9510799240673,
73.5425672375985));
#209566=CARTESIAN_POINT('Ctrl Pts',(-52.6623482025009,-77.1750181725883,
76.4942832697836));
#209567=CARTESIAN_POINT('Ctrl Pts',(-52.5464677269709,-80.3754020370897,
78.3425451526677));
#209568=CARTESIAN_POINT('Ctrl Pts',(-52.4305872514409,-84.0435225503917,
78.7935670676356));
#209569=CARTESIAN_POINT('Ctrl Pts',(-52.3147067759109,-87.5963228428119,
77.7756579606599));
#209570=CARTESIAN_POINT('Ctrl Pts',(-52.1988263003809,-90.4690764803083,
75.4506170134693));
#209571=CARTESIAN_POINT('Ctrl Pts',(-52.0829458248509,-92.2051521343437,
72.1880152615928));
#209572=CARTESIAN_POINT('Ctrl Pts',(-51.9670653493209,-92.5285962661224,
68.5064513600015));
#209573=CARTESIAN_POINT('Ctrl Pts',(-51.8511848737909,-91.3879966272414,
64.991119038349));
#209574=CARTESIAN_POINT('Ctrl Pts',(-51.7353043982609,-88.9646543643234,
62.2007891036226));
#209575=CARTESIAN_POINT('Ctrl Pts',(-51.6194239227409,-85.643765751282,
60.5789914320152));
#209576=CARTESIAN_POINT('Ctrl Pts',(-51.5035434472109,-81.9531942844895,
60.3835147930695));
#209577=CARTESIAN_POINT('Ctrl Pts',(-51.3876629716809,-78.479565468472,
61.6454306842398));
#209578=CARTESIAN_POINT('Ctrl Pts',(-51.2717824961509,-75.7750212343761,
64.164154439174));
#209579=CARTESIAN_POINT('Ctrl Pts',(-51.1559020206209,-74.2694556081259,
67.5393286588115));
#209580=CARTESIAN_POINT('Ctrl Pts',(-51.0400215450909,-74.2021819868569,
71.2344610147253));
#209581=CARTESIAN_POINT('Ctrl Pts',(-50.9241410695609,-75.5838936798222,
74.6622010377381));
#209582=CARTESIAN_POINT('Ctrl Pts',(-50.8082605940309,-78.1949641803186,
77.2777009343681));
#209583=CARTESIAN_POINT('Ctrl Pts',(-50.6923801185009,-81.6203573446273,
78.6652204973786));
#209584=CARTESIAN_POINT('Ctrl Pts',(-50.5764996429709,-85.3155984182905,
78.604210044692));
#209585=CARTESIAN_POINT('Ctrl Pts',(-50.4606191674409,-88.6933196511762,
77.1043673393538));
#209586=CARTESIAN_POINT('Ctrl Pts',(-50.3447386919109,-91.2166238607655,
74.4040961060068));
#209587=CARTESIAN_POINT('Ctrl Pts',(-50.2288582163809,-92.484425573369,
70.9326111664812));
#209588=CARTESIAN_POINT('Ctrl Pts',(-50.1129777408609,-92.2952045566739,
67.2417136774408));
#209589=CARTESIAN_POINT('Ctrl Pts',(-49.9970972653309,-90.6790379614674,
63.9180809654222));
#209590=CARTESIAN_POINT('Ctrl Pts',(-49.8812167898009,-87.8928194836539,
61.4900127082349));
#209591=CARTESIAN_POINT('Ctrl Pts',(-49.7653363142709,-84.3794254732619,
60.3434563880282));
#209592=CARTESIAN_POINT('Ctrl Pts',(-49.6494558387409,-80.6973186374278,
60.6606599817841));
#209593=CARTESIAN_POINT('Ctrl Pts',(-49.5335753632109,-77.4317790082792,
62.3912031861476));
#209594=CARTESIAN_POINT('Ctrl Pts',(-49.4176948876809,-75.1018722171853,
65.2600118737984));
#209595=CARTESIAN_POINT('Ctrl Pts',(-49.3018144121509,-74.0779427618718,
68.8110817203492));
#209596=CARTESIAN_POINT('Ctrl Pts',(-49.1859339366209,-74.5227466829941,
72.4799615572945));
#209597=CARTESIAN_POINT('Ctrl Pts',(-49.0700534610909,-76.365581629465,
75.6834730465697));
#209598=CARTESIAN_POINT('Ctrl Pts',(-48.9541729855609,-79.3135231486161,
77.912412958451));
#209599=CARTESIAN_POINT('Ctrl Pts',(-48.8382925100409,-82.8979933102528,
78.8124750030432));
#209600=CARTESIAN_POINT('Ctrl Pts',(-48.7224120345109,-86.5492141392223,
78.2406322116708));
#209601=CARTESIAN_POINT('Ctrl Pts',(-48.6065315589809,-89.686880460583,
76.2876306508874));
#209602=CARTESIAN_POINT('Ctrl Pts',(-48.5292779086209,-91.103632261208,
74.2721860206966));
#209603=CARTESIAN_POINT('Ctrl Pts',(-48.4906510834509,-91.5871045987178,
73.1658451292715));
#209604=CARTESIAN_POINT('Ctrl Pts',(-49.2716875596105,-89.6376853052957,
77.6221314644383));
#209605=CARTESIAN_POINT('Ctrl Pts',(-49.1710275888522,-89.5185411919897,
77.4698472271473));
#209606=CARTESIAN_POINT('Ctrl Pts',(-49.0703675024719,-89.3993929535507,
77.3175659292054));
#209607=CARTESIAN_POINT('Ctrl Pts',(-48.8698648872584,-89.1620562864648,
77.0142463336982));
#209608=CARTESIAN_POINT('Ctrl Pts',(-48.7700220939601,-89.0438676089703,
76.8632075858943));
#209609=CARTESIAN_POINT('Ctrl Pts',(-48.6701794005812,-88.9256751617442,
76.7121720277652));
#209610=CARTESIAN_POINT('Ctrl Pts',(-49.3172045433909,-89.3404582498078,
77.9029428178255));
#209611=CARTESIAN_POINT('Ctrl Pts',(-49.2671675200609,-90.8384471580197,
76.9294625104546));
#209612=CARTESIAN_POINT('Ctrl Pts',(-49.1670934734009,-93.3533237193631,
74.1587488145407));
#209613=CARTESIAN_POINT('Ctrl Pts',(-49.0169824034109,-94.5869930790562,
68.5383989146951));
#209614=CARTESIAN_POINT('Ctrl Pts',(-48.8668713334209,-92.8158926798989,
62.9167841918778));
#209615=CARTESIAN_POINT('Ctrl Pts',(-48.7667972867609,-89.8591099411729,
60.1918250007294));
#209616=CARTESIAN_POINT('Ctrl Pts',(-48.7167602634309,-88.1157743146814,
59.2817848695541));
#209617=CARTESIAN_POINT('Ctrl Pts',(-49.0930764331109,-89.0886145980675,
77.5537369843529));
#209618=CARTESIAN_POINT('Ctrl Pts',(-49.0430394097809,-90.5260811899022,
76.6239047484312));
#209619=CARTESIAN_POINT('Ctrl Pts',(-48.9429653631309,-92.9432122733185,
73.9726075199026));
#209620=CARTESIAN_POINT('Ctrl Pts',(-48.7928542931309,-94.1385843271853,
68.5806263247324));
#209621=CARTESIAN_POINT('Ctrl Pts',(-48.6427432231409,-92.4477415858012,
63.176215785295));
#209622=CARTESIAN_POINT('Ctrl Pts',(-48.5426691764809,-89.609279485427,
60.5503257501768));
#209623=CARTESIAN_POINT('Ctrl Pts',(-48.4926321531609,-87.9335507117994,
59.6718675500254));
#209624=CARTESIAN_POINT('Ctrl Pts',(-48.8689483228409,-88.8367709463283,
77.204531150883));
#209625=CARTESIAN_POINT('Ctrl Pts',(-48.8189112995109,-90.2137152217751,
76.3183469864107));
#209626=CARTESIAN_POINT('Ctrl Pts',(-48.7188372528509,-92.5331008272736,
73.7864662252636));
#209627=CARTESIAN_POINT('Ctrl Pts',(-48.5687261828609,-93.6901755753147,
68.6228537347706));
#209628=CARTESIAN_POINT('Ctrl Pts',(-48.4186151128609,-92.0795904917139,
63.4356473787111));
#209629=CARTESIAN_POINT('Ctrl Pts',(-48.3185410662109,-89.3594490296811,
60.9088264996243));
#209630=CARTESIAN_POINT('Ctrl Pts',(-48.2685040428809,-87.7513271089174,
60.0619502304968));
#209631=CARTESIAN_POINT('Ctrl Pts',(-48.6448202125609,-88.5849272945795,
76.855325317416));
#209632=CARTESIAN_POINT('Ctrl Pts',(-48.5947831892309,-89.9013492536484,
76.0127892243911));
#209633=CARTESIAN_POINT('Ctrl Pts',(-48.4947091425709,-92.1229893812291,
73.6003249306254));
#209634=CARTESIAN_POINT('Ctrl Pts',(-48.3445980725809,-93.2417668234437,
68.6650811448079));
#209635=CARTESIAN_POINT('Ctrl Pts',(-48.1944870025909,-91.7114393976162,
63.6950789721283));
#209636=CARTESIAN_POINT('Ctrl Pts',(-48.0944129559309,-89.1096185739352,
61.2673272490717));
#209637=CARTESIAN_POINT('Ctrl Pts',(-48.0443759326009,-87.5691035060354,
60.4520329109681));
#209638=CARTESIAN_POINT('Ctrl Pts',(-48.173560826516,-88.0240721664226,
60.4464459620599));
#209639=CARTESIAN_POINT('Ctrl Pts',(-48.1596729098132,-88.0118235639595,
60.4701459438197));
#209640=CARTESIAN_POINT('Ctrl Pts',(-48.1457849931372,-87.99957496149,60.4938459255919));
#209641=CARTESIAN_POINT('Ctrl Pts',(-48.1179938256803,-87.9750642324048,
60.5412720571842));
#209642=CARTESIAN_POINT('Ctrl Pts',(-48.1040905748995,-87.9628021057893,
60.5649982070044));
#209643=CARTESIAN_POINT('Ctrl Pts',(-48.0901873241469,-87.9505399791669,
60.5887243568376));
#209644=CARTESIAN_POINT('Origin',(-47.9901862140809,-88.4831990770459,59.5580752732411));
#209645=CARTESIAN_POINT('Ctrl Pts',(-47.890187490573,-87.9505401263848,
60.5887240719836));
#209646=CARTESIAN_POINT('Ctrl Pts',(-47.8762912240803,-87.9627960889656,
60.5650098490354));
#209647=CARTESIAN_POINT('Ctrl Pts',(-47.8623949575891,-87.9750520515467,
60.5412956260866));
#209648=CARTESIAN_POINT('Ctrl Pts',(-47.8346038364013,-87.9995627315646,
60.4938695894352));
#209649=CARTESIAN_POINT('Ctrl Pts',(-47.8207089817047,-88.0118174490013,
60.4701577757326));
#209650=CARTESIAN_POINT('Ctrl Pts',(-47.8068141270095,-88.0240721664383,
60.4464459620294));
#209651=CARTESIAN_POINT('Ctrl Pts',(-48.5133467647509,-88.5849272945888,
76.8553253174122));
#209652=CARTESIAN_POINT('Ctrl Pts',(-48.4633097414209,-89.9013492536481,
76.0127892243902));
#209653=CARTESIAN_POINT('Ctrl Pts',(-48.3632356947609,-92.1229893812287,
73.6003249306245));
#209654=CARTESIAN_POINT('Ctrl Pts',(-48.2131246247709,-93.2417668234433,
68.665081144807));
#209655=CARTESIAN_POINT('Ctrl Pts',(-48.0630135547809,-91.7114393976162,
63.6950789721283));
#209656=CARTESIAN_POINT('Ctrl Pts',(-47.9629395081209,-89.1096185739352,
61.2673272490717));
#209657=CARTESIAN_POINT('Ctrl Pts',(-47.9129024847909,-87.5691035060354,
60.4520329109681));
#209658=CARTESIAN_POINT('Ctrl Pts',(-48.2892186544709,-88.8367709463279,
77.2045311508821));
#209659=CARTESIAN_POINT('Ctrl Pts',(-48.2391816311409,-90.2137152217747,
76.3183469864098));
#209660=CARTESIAN_POINT('Ctrl Pts',(-48.1391075844909,-92.5331008272732,
73.7864662252626));
#209661=CARTESIAN_POINT('Ctrl Pts',(-47.9889965144909,-93.6901755753147,
68.6228537347706));
#209662=CARTESIAN_POINT('Ctrl Pts',(-47.8388854445009,-92.0795904917135,
63.4356473787102));
#209663=CARTESIAN_POINT('Ctrl Pts',(-47.7388113978409,-89.3594490296811,
60.9088264996243));
#209664=CARTESIAN_POINT('Ctrl Pts',(-47.6887743745209,-87.7513271089174,
60.0619502304968));
#209665=CARTESIAN_POINT('Ctrl Pts',(-48.0650905442009,-89.0886145980675,
77.5537369843529));
#209666=CARTESIAN_POINT('Ctrl Pts',(-48.0150535208709,-90.5260811899018,
76.6239047484302));
#209667=CARTESIAN_POINT('Ctrl Pts',(-47.9149794742109,-92.9432122733182,
73.9726075199017));
#209668=CARTESIAN_POINT('Ctrl Pts',(-47.7648684042209,-94.1385843271853,
68.5806263247324));
#209669=CARTESIAN_POINT('Ctrl Pts',(-47.6147573342209,-92.4477415858012,
63.176215785295));
#209670=CARTESIAN_POINT('Ctrl Pts',(-47.5146832875709,-89.609279485427,
60.5503257501768));
#209671=CARTESIAN_POINT('Ctrl Pts',(-47.4646462642409,-87.9335507117994,
59.6718675500254));
#209672=CARTESIAN_POINT('Ctrl Pts',(-47.8409624339209,-89.3404582498171,
77.9029428178217));
#209673=CARTESIAN_POINT('Ctrl Pts',(-47.7909254105909,-90.8384471580193,
76.9294625104536));
#209674=CARTESIAN_POINT('Ctrl Pts',(-47.6908513639309,-93.3533237193627,
74.1587488145398));
#209675=CARTESIAN_POINT('Ctrl Pts',(-47.5407402939409,-94.5869930790562,
68.5383989146951));
#209676=CARTESIAN_POINT('Ctrl Pts',(-47.3906292239509,-92.8158926798989,
62.9167841918778));
#209677=CARTESIAN_POINT('Ctrl Pts',(-47.2905551772909,-89.8591099411729,
60.1918250007294));
#209678=CARTESIAN_POINT('Ctrl Pts',(-47.2405181539609,-88.1157743146814,
59.2817848695541));
#209679=CARTESIAN_POINT('Ctrl Pts',(-48.4651187514177,-88.9258151777763,
76.7120624159033));
#209680=CARTESIAN_POINT('Ctrl Pts',(-48.3651833302526,-89.0441273831064,
76.8632423418457));
#209681=CARTESIAN_POINT('Ctrl Pts',(-48.2652478086818,-89.1624358230597,
77.0144254663974));
#209682=CARTESIAN_POINT('Ctrl Pts',(-48.064741788983,-89.3997965906428,
77.3177584516766));
#209683=CARTESIAN_POINT('Ctrl Pts',(-47.9641710688051,-89.5188491313808,
77.4699086873536));
#209684=CARTESIAN_POINT('Ctrl Pts',(-47.8636004674101,-89.637897562514,
77.6220618559046));
#209685=CARTESIAN_POINT('Ctrl Pts',(-55.7755280695129,-88.4387198218353,
76.9828771994399));
#209686=CARTESIAN_POINT('Ctrl Pts',(-55.7369012443359,-89.4328822235564,
76.2977664141032));
#209687=CARTESIAN_POINT('Ctrl Pts',(-55.6596475939829,-91.1420015977624,
74.5234739673153));
#209688=CARTESIAN_POINT('Ctrl Pts',(-55.5437671184529,-92.4624356766218,
71.0715732033575));
#209689=CARTESIAN_POINT('Ctrl Pts',(-55.4278866429239,-92.32923623476,67.3782446735901));
#209690=CARTESIAN_POINT('Ctrl Pts',(-55.3120061673939,-90.7637102347341,
64.0304593807184));
#209691=CARTESIAN_POINT('Ctrl Pts',(-55.1961256918649,-88.0146658633944,
61.5603809658357));
#209692=CARTESIAN_POINT('Ctrl Pts',(-55.0802452163349,-84.5190802164795,
60.3606278716294));
#209693=CARTESIAN_POINT('Ctrl Pts',(-54.9643647408059,-80.8325827289163,
60.6219056176175));
#209694=CARTESIAN_POINT('Ctrl Pts',(-54.8484842652759,-77.5411520298483,
62.3026829788096));
#209695=CARTESIAN_POINT('Ctrl Pts',(-54.7326037897459,-75.1679690211427,
65.135796345557));
#209696=CARTESIAN_POINT('Ctrl Pts',(-54.6167233142169,-74.0902570884328,
68.6709152745216));
#209697=CARTESIAN_POINT('Ctrl Pts',(-54.5008428386909,-74.4793212078431,
72.3461238375152));
#209698=CARTESIAN_POINT('Ctrl Pts',(-54.3849623631609,-76.2733186744711,
75.5772384992808));
#209699=CARTESIAN_POINT('Ctrl Pts',(-54.2690818876309,-79.1870891325353,
77.8506655567185));
#209700=CARTESIAN_POINT('Ctrl Pts',(-54.1532014121009,-82.7574815282069,
78.8050381301377));
#209701=CARTESIAN_POINT('Ctrl Pts',(-54.0373209365709,-86.416973118854,
78.2886563277362));
#209702=CARTESIAN_POINT('Ctrl Pts',(-53.9214404610409,-89.5838786235081,
76.3836003200345));
#209703=CARTESIAN_POINT('Ctrl Pts',(-53.8055599855109,-91.7548105434674,
73.3926834929055));
#209704=CARTESIAN_POINT('Ctrl Pts',(-53.6896795099809,-92.5846938559892,
69.7913195074835));
#209705=CARTESIAN_POINT('Ctrl Pts',(-53.5737990344509,-91.9416165465586,
66.1519541174746));
#209706=CARTESIAN_POINT('Ctrl Pts',(-53.4579185589209,-89.9277973513432,
63.053073494268));
#209707=CARTESIAN_POINT('Ctrl Pts',(-53.3420380833909,-86.8633378351191,
60.9872524126373));
#209708=CARTESIAN_POINT('Ctrl Pts',(-53.2261576078609,-83.2353414521743,
60.2828582664042));
#209709=CARTESIAN_POINT('Ctrl Pts',(-53.1102771323309,-79.6204872419811,
61.0518562553048));
#209710=CARTESIAN_POINT('Ctrl Pts',(-52.9943966568009,-76.5933652629879,
63.172012238292));
#209711=CARTESIAN_POINT('Ctrl Pts',(-52.8785161812709,-74.6351440751773,
66.306322153967));
#209712=CARTESIAN_POINT('Ctrl Pts',(-52.7626357057409,-74.0570878018971,
69.9565796534892));
#209713=CARTESIAN_POINT('Ctrl Pts',(-52.6467552302109,-74.9510799240673,
73.5425672375985));
#209714=CARTESIAN_POINT('Ctrl Pts',(-52.5308747546809,-77.1750181725883,
76.4942832697836));
#209715=CARTESIAN_POINT('Ctrl Pts',(-52.4149942791509,-80.3754020370897,
78.3425451526677));
#209716=CARTESIAN_POINT('Ctrl Pts',(-52.2991138036209,-84.0435225503917,
78.7935670676356));
#209717=CARTESIAN_POINT('Ctrl Pts',(-52.1832333281009,-87.5963228428119,
77.7756579606599));
#209718=CARTESIAN_POINT('Ctrl Pts',(-52.0673528525709,-90.4690764803083,
75.4506170134693));
#209719=CARTESIAN_POINT('Ctrl Pts',(-51.9514723770409,-92.2051521343437,
72.1880152615928));
#209720=CARTESIAN_POINT('Ctrl Pts',(-51.8355919015109,-92.5285962661224,
68.5064513600015));
#209721=CARTESIAN_POINT('Ctrl Pts',(-51.7197114259809,-91.3879966272414,
64.991119038349));
#209722=CARTESIAN_POINT('Ctrl Pts',(-51.6038309504509,-88.9646543643234,
62.2007891036226));
#209723=CARTESIAN_POINT('Ctrl Pts',(-51.4879504749209,-85.643765751282,
60.5789914320152));
#209724=CARTESIAN_POINT('Ctrl Pts',(-51.3720699993909,-81.9531942844895,
60.3835147930695));
#209725=CARTESIAN_POINT('Ctrl Pts',(-51.2561895238609,-78.479565468472,
61.6454306842398));
#209726=CARTESIAN_POINT('Ctrl Pts',(-51.1403090483309,-75.7750212343761,
64.164154439174));
#209727=CARTESIAN_POINT('Ctrl Pts',(-51.0244285728009,-74.2694556081259,
67.5393286588115));
#209728=CARTESIAN_POINT('Ctrl Pts',(-50.9085480972709,-74.2021819868569,
71.2344610147253));
#209729=CARTESIAN_POINT('Ctrl Pts',(-50.7926676217409,-75.5838936798222,
74.6622010377381));
#209730=CARTESIAN_POINT('Ctrl Pts',(-50.6767871462109,-78.1949641803186,
77.2777009343681));
#209731=CARTESIAN_POINT('Ctrl Pts',(-50.5609066706809,-81.6203573446273,
78.6652204973786));
#209732=CARTESIAN_POINT('Ctrl Pts',(-50.4450261951609,-85.3155984182905,
78.604210044692));
#209733=CARTESIAN_POINT('Ctrl Pts',(-50.3291457196309,-88.6933196511762,
77.1043673393538));
#209734=CARTESIAN_POINT('Ctrl Pts',(-50.2132652441009,-91.2166238607655,
74.4040961060068));
#209735=CARTESIAN_POINT('Ctrl Pts',(-50.0973847685709,-92.484425573369,
70.9326111664812));
#209736=CARTESIAN_POINT('Ctrl Pts',(-49.9815042930409,-92.2952045566739,
67.2417136774408));
#209737=CARTESIAN_POINT('Ctrl Pts',(-49.8656238175109,-90.6790379614674,
63.9180809654222));
#209738=CARTESIAN_POINT('Ctrl Pts',(-49.7497433419809,-87.8928194836539,
61.4900127082349));
#209739=CARTESIAN_POINT('Ctrl Pts',(-49.6338628664509,-84.3794254732619,
60.3434563880282));
#209740=CARTESIAN_POINT('Ctrl Pts',(-49.5179823909209,-80.6973186374278,
60.6606599817841));
#209741=CARTESIAN_POINT('Ctrl Pts',(-49.4021019153909,-77.4317790082792,
62.3912031861476));
#209742=CARTESIAN_POINT('Ctrl Pts',(-49.2862214398709,-75.1018722171853,
65.2600118737984));
#209743=CARTESIAN_POINT('Ctrl Pts',(-49.1703409643409,-74.0779427618718,
68.8110817203492));
#209744=CARTESIAN_POINT('Ctrl Pts',(-49.0544604888109,-74.5227466829941,
72.4799615572945));
#209745=CARTESIAN_POINT('Ctrl Pts',(-48.9385800132809,-76.365581629465,
75.6834730465697));
#209746=CARTESIAN_POINT('Ctrl Pts',(-48.8226995377509,-79.3135231486161,
77.912412958451));
#209747=CARTESIAN_POINT('Ctrl Pts',(-48.7068190622209,-82.8979933102528,
78.8124750030432));
#209748=CARTESIAN_POINT('Ctrl Pts',(-48.5909385866909,-86.5492141392223,
78.2406322116708));
#209749=CARTESIAN_POINT('Ctrl Pts',(-48.4750581111709,-89.686880460583,
76.2876306508874));
#209750=CARTESIAN_POINT('Ctrl Pts',(-48.3978044608109,-91.103632261208,
74.2721860206966));
#209751=CARTESIAN_POINT('Ctrl Pts',(-48.3591776356409,-91.5871045987178,
73.1658451292715));
#209752=CARTESIAN_POINT('Ctrl Pts',(-55.5513999592359,-88.6830297228196,
77.3373946338934));
#209753=CARTESIAN_POINT('Ctrl Pts',(-55.5127731340599,-89.7246238799117,
76.6195970288649));
#209754=CARTESIAN_POINT('Ctrl Pts',(-55.4355194837069,-91.5152857987813,
74.760652612607));
#209755=CARTESIAN_POINT('Ctrl Pts',(-55.3196390081769,-92.8987181423976,
71.1440607355203));
#209756=CARTESIAN_POINT('Ctrl Pts',(-55.2037585326479,-92.7591637193615,
67.274522509035));
#209757=CARTESIAN_POINT('Ctrl Pts',(-55.0878780571179,-91.1189460531508,
63.7670134801353));
#209758=CARTESIAN_POINT('Ctrl Pts',(-54.9719975815889,-88.2387440360669,
61.179086960254));
#209759=CARTESIAN_POINT('Ctrl Pts',(-54.8561171060589,-84.5763830585068,
59.9220933234976));
#209760=CARTESIAN_POINT('Ctrl Pts',(-54.7402366305299,-80.7140017850856,
60.1958367009625));
#209761=CARTESIAN_POINT('Ctrl Pts',(-54.6243561549999,-77.2655360428094,
61.9568044017577));
#209762=CARTESIAN_POINT('Ctrl Pts',(-54.5084756794709,-74.7791278349758,
64.9250863686191));
#209763=CARTESIAN_POINT('Ctrl Pts',(-54.3925952039409,-73.6499979763262,
68.6288667717323));
#209764=CARTESIAN_POINT('Ctrl Pts',(-54.2767147284109,-74.0576244494326,
72.4794205229618));
#209765=CARTESIAN_POINT('Ctrl Pts',(-54.1608342528809,-75.9372140173222,
75.8646925335888));
#209766=CARTESIAN_POINT('Ctrl Pts',(-54.0449537773509,-78.9900012470032,
78.2465854069093));
#209767=CARTESIAN_POINT('Ctrl Pts',(-53.9290733018209,-82.7307380233984,
79.2464913522906));
#209768=CARTESIAN_POINT('Ctrl Pts',(-53.8131928262909,-86.5648249413073,
78.7054728353225));
#209769=CARTESIAN_POINT('Ctrl Pts',(-53.6973123507609,-89.8828243586779,
76.7095260935192));
#209770=CARTESIAN_POINT('Ctrl Pts',(-53.5814318752309,-92.1573320239741,
73.5759118207695));
#209771=CARTESIAN_POINT('Ctrl Pts',(-53.4655513997009,-93.026809292365,
69.8027257917525));
#209772=CARTESIAN_POINT('Ctrl Pts',(-53.3496709241709,-92.353050591669,
65.9897253009272));
#209773=CARTESIAN_POINT('Ctrl Pts',(-53.2337904486409,-90.2431515414503,
62.7429962503755));
#209774=CARTESIAN_POINT('Ctrl Pts',(-53.1179099731109,-87.0324858381458,
60.5786142897588));
#209775=CARTESIAN_POINT('Ctrl Pts',(-53.0020294975809,-83.2313967727705,
59.8406133095025));
#209776=CARTESIAN_POINT('Ctrl Pts',(-52.8861490220609,-79.4440768967273,
60.6463003991196));
#209777=CARTESIAN_POINT('Ctrl Pts',(-52.7702685465309,-76.2725301145905,
62.8676095938354));
#209778=CARTESIAN_POINT('Ctrl Pts',(-52.6543880710009,-74.2208816676457,
66.1514582779195));
#209779=CARTESIAN_POINT('Ctrl Pts',(-52.5385075954709,-73.6152461742155,
69.9758705437336));
#209780=CARTESIAN_POINT('Ctrl Pts',(-52.4226271199409,-74.5518909007893,
73.7329465591992));
#209781=CARTESIAN_POINT('Ctrl Pts',(-52.3067466444109,-76.8819338408192,
76.8254897565408));
#209782=CARTESIAN_POINT('Ctrl Pts',(-52.1908661688809,-80.2350088795841,
78.761932710572));
#209783=CARTESIAN_POINT('Ctrl Pts',(-52.0749856933509,-84.0781364083665,
79.234473002314));
#209784=CARTESIAN_POINT('Ctrl Pts',(-51.9591052178209,-87.8004417575374,
78.167999178288));
#209785=CARTESIAN_POINT('Ctrl Pts',(-51.8432247422909,-90.8102552431185,
75.7320299026639));
#209786=CARTESIAN_POINT('Ctrl Pts',(-51.7273442667609,-92.6291595331741,
72.3137685443966));
#209787=CARTESIAN_POINT('Ctrl Pts',(-51.6114637912309,-92.9680352714057,
68.4565562396562));
#209788=CARTESIAN_POINT('Ctrl Pts',(-51.4955833157009,-91.7730173172237,
64.7735064682078));
#209789=CARTESIAN_POINT('Ctrl Pts',(-51.3797028401709,-89.2340567436806,
61.8500491424068));
#209790=CARTESIAN_POINT('Ctrl Pts',(-51.2638223646409,-85.7547276424399,
60.1508750680323));
#209791=CARTESIAN_POINT('Ctrl Pts',(-51.1479418891109,-81.8880780191402,
59.9460721861074));
#209792=CARTESIAN_POINT('Ctrl Pts',(-51.0320614135809,-78.2487214387897,
61.2681944235775));
#209793=CARTESIAN_POINT('Ctrl Pts',(-50.9161809380509,-75.4151426724483,
63.9070871657534));
#209794=CARTESIAN_POINT('Ctrl Pts',(-50.8003004625309,-73.837746105554,
67.443291854472));
#209795=CARTESIAN_POINT('Ctrl Pts',(-50.6844199870009,-73.7672628417323,
71.3147199681372));
#209796=CARTESIAN_POINT('Ctrl Pts',(-50.5685395114709,-75.2148963708959,
74.9059983888393));
#209797=CARTESIAN_POINT('Ctrl Pts',(-50.4526590359409,-77.9505417466828,
77.6462844884434));
#209798=CARTESIAN_POINT('Ctrl Pts',(-50.3367785604109,-81.5393613394195,
79.1000029826967));
#209799=CARTESIAN_POINT('Ctrl Pts',(-50.2208980848809,-85.4109033577874,
79.0360817049178));
#209800=CARTESIAN_POINT('Ctrl Pts',(-50.1050176093509,-88.9497765784368,
77.4646811010361));
#209801=CARTESIAN_POINT('Ctrl Pts',(-49.9891371338209,-91.5934683099975,
74.6355792014604));
#209802=CARTESIAN_POINT('Ctrl Pts',(-49.8732566582909,-92.9217571830265,
70.9984687825244));
#209803=CARTESIAN_POINT('Ctrl Pts',(-49.7573761827609,-92.7235083807798,
67.1314775823677));
#209804=CARTESIAN_POINT('Ctrl Pts',(-49.6414957072309,-91.0302340429712,
63.6492734604498));
#209805=CARTESIAN_POINT('Ctrl Pts',(-49.5256152317109,-88.1110843328011,
61.105361414176));
#209806=CARTESIAN_POINT('Ctrl Pts',(-49.4097347561809,-84.4300653499657,
59.9041025837992));
#209807=CARTESIAN_POINT('Ctrl Pts',(-49.2938542806509,-80.5722842074503,
60.2364400462553));
#209808=CARTESIAN_POINT('Ctrl Pts',(-49.1779738051209,-77.1509448049911,
62.0495479319753));
#209809=CARTESIAN_POINT('Ctrl Pts',(-49.0620933295909,-74.7098775347402,
65.055228253093));
#209810=CARTESIAN_POINT('Ctrl Pts',(-48.9462128540609,-73.6370961299356,
68.7757205963565));
#209811=CARTESIAN_POINT('Ctrl Pts',(-48.8303323785309,-74.1031217656727,
72.6196436763183));
#209812=CARTESIAN_POINT('Ctrl Pts',(-48.7144519030009,-76.033878862693,
75.9759955596776));
#209813=CARTESIAN_POINT('Ctrl Pts',(-48.5985714274709,-79.1224674639693,
78.3112787937738));
#209814=CARTESIAN_POINT('Ctrl Pts',(-48.4826909519509,-82.8779536603277,
79.254283040401));
#209815=CARTESIAN_POINT('Ctrl Pts',(-48.3668104764209,-86.7033752162974,
78.6551574757721));
#209816=CARTESIAN_POINT('Ctrl Pts',(-48.2509300008909,-89.9907404410874,
76.6089776856617));
#209817=CARTESIAN_POINT('Ctrl Pts',(-48.1736763505409,-91.4750858508685,
74.4973756505227));
#209818=CARTESIAN_POINT('Ctrl Pts',(-48.1350495253609,-91.9816247835266,
73.3382509378444));
#209819=CARTESIAN_POINT('Ctrl Pts',(-55.3272718489599,-88.9273396238135,
77.6919120683441));
#209820=CARTESIAN_POINT('Ctrl Pts',(-55.2886450237839,-90.0163655362671,
76.9414276436266));
#209821=CARTESIAN_POINT('Ctrl Pts',(-55.2113913734309,-91.8885699997907,
74.9978312579016));
#209822=CARTESIAN_POINT('Ctrl Pts',(-55.0955108979009,-93.335000608173,
71.2165482676822));
#209823=CARTESIAN_POINT('Ctrl Pts',(-54.9796304223719,-93.1890912039718,
67.1708003444751));
#209824=CARTESIAN_POINT('Ctrl Pts',(-54.8637499468419,-91.4741818715764,
63.5035675795474));
#209825=CARTESIAN_POINT('Ctrl Pts',(-54.7478694713129,-88.4628222087298,
60.7977929546752));
#209826=CARTESIAN_POINT('Ctrl Pts',(-54.6319889957829,-84.6336859005426,
59.4835587753601));
#209827=CARTESIAN_POINT('Ctrl Pts',(-54.5161085202509,-80.5954208412564,
59.7697677843112));
#209828=CARTESIAN_POINT('Ctrl Pts',(-54.4002280447209,-76.9899200557673,
61.6109258247081));
#209829=CARTESIAN_POINT('Ctrl Pts',(-54.2843475691909,-74.3902866488067,
64.7143763916865));
#209830=CARTESIAN_POINT('Ctrl Pts',(-54.1684670936609,-73.2097388642188,
68.58681826895));
#209831=CARTESIAN_POINT('Ctrl Pts',(-54.0525866181309,-73.6359276910248,
72.6127172084169));
#209832=CARTESIAN_POINT('Ctrl Pts',(-53.9367061426009,-75.6011093601795,
76.152146567904));
#209833=CARTESIAN_POINT('Ctrl Pts',(-53.8208256670709,-78.7929133614815,
78.6425052571067));
#209834=CARTESIAN_POINT('Ctrl Pts',(-53.7049451915509,-82.7039945186047,
79.687944574445));
#209835=CARTESIAN_POINT('Ctrl Pts',(-53.5890647160209,-86.7126767637781,
79.1222893429069));
#209836=CARTESIAN_POINT('Ctrl Pts',(-53.4731842404909,-90.1817700938727,
77.035451866986));
#209837=CARTESIAN_POINT('Ctrl Pts',(-53.3573037649609,-92.5598535044851,
73.7591401486176));
#209838=CARTESIAN_POINT('Ctrl Pts',(-53.2414232894309,-93.4689247287331,
69.8141320760029));
#209839=CARTESIAN_POINT('Ctrl Pts',(-53.1255428139009,-92.764484636779,
65.8274964843525));
#209840=CARTESIAN_POINT('Ctrl Pts',(-53.0096623383709,-90.5585057315378,
62.4329190064618));
#209841=CARTESIAN_POINT('Ctrl Pts',(-52.8937818628409,-87.2016338411459,
60.1699761668685));
#209842=CARTESIAN_POINT('Ctrl Pts',(-52.7779013873109,-83.2274520933251,
59.3983683526049));
#209843=CARTESIAN_POINT('Ctrl Pts',(-52.6620209117809,-79.2676665514421,
60.2407445429474));
#209844=CARTESIAN_POINT('Ctrl Pts',(-52.5461404362509,-75.9516949661677,
62.5632069494066));
#209845=CARTESIAN_POINT('Ctrl Pts',(-52.4302599607209,-73.8066192600998,
65.9965944019082));
#209846=CARTESIAN_POINT('Ctrl Pts',(-52.3143794851909,-73.1734045465354,
69.9951614340195));
#209847=CARTESIAN_POINT('Ctrl Pts',(-52.1984990096609,-74.15270187753,73.9233258808396));
#209848=CARTESIAN_POINT('Ctrl Pts',(-52.0826185341309,-76.5888495090847,
77.1566962433291));
#209849=CARTESIAN_POINT('Ctrl Pts',(-51.9667380586009,-80.0946157221245,
79.1813202684909));
#209850=CARTESIAN_POINT('Ctrl Pts',(-51.8508575830709,-84.1127502663909,
79.6753789369893));
#209851=CARTESIAN_POINT('Ctrl Pts',(-51.7349771075409,-88.0045606723086,
78.5603403958907));
#209852=CARTESIAN_POINT('Ctrl Pts',(-51.6190966320109,-91.1514340059658,
76.0134427918171));
#209853=CARTESIAN_POINT('Ctrl Pts',(-51.5032161564809,-93.053166932025,
72.4395218271453));
#209854=CARTESIAN_POINT('Ctrl Pts',(-51.3873356809509,-93.4074742766868,
68.4066611192533));
#209855=CARTESIAN_POINT('Ctrl Pts',(-51.2714552054309,-92.1580380071747,
64.5558938980169));
#209856=CARTESIAN_POINT('Ctrl Pts',(-51.1555747299009,-89.5034591229898,
61.4993091811534));
#209857=CARTESIAN_POINT('Ctrl Pts',(-51.0396942543709,-85.8656895335373,
59.7227587040344));
#209858=CARTESIAN_POINT('Ctrl Pts',(-50.9238137788409,-81.8229617537302,
59.5086295791554));
#209859=CARTESIAN_POINT('Ctrl Pts',(-50.8079333033109,-78.0178774090514,
60.8909581629449));
#209860=CARTESIAN_POINT('Ctrl Pts',(-50.6920528277809,-75.0552641104844,
63.6500198923845));
#209861=CARTESIAN_POINT('Ctrl Pts',(-50.5761723522509,-73.4060366029682,
67.3472550501956));
#209862=CARTESIAN_POINT('Ctrl Pts',(-50.4602918767209,-73.3323436966194,
71.3949789216125));
#209863=CARTESIAN_POINT('Ctrl Pts',(-50.3444114011909,-74.8458990620047,
75.1497957399931));
#209864=CARTESIAN_POINT('Ctrl Pts',(-50.2285309256609,-77.7061193131001,
78.0148680425531));
#209865=CARTESIAN_POINT('Ctrl Pts',(-50.1126504501309,-81.4583653342733,
79.534785468025));
#209866=CARTESIAN_POINT('Ctrl Pts',(-49.9967699746009,-85.5062082973436,
79.4679533651301));
#209867=CARTESIAN_POINT('Ctrl Pts',(-49.8808894990709,-89.206233505757,
77.8249948626797));
#209868=CARTESIAN_POINT('Ctrl Pts',(-49.7650090235509,-91.9703127592713,
74.8670622968578));
#209869=CARTESIAN_POINT('Ctrl Pts',(-49.6491285480209,-93.3590887926927,
71.06432639851));
#209870=CARTESIAN_POINT('Ctrl Pts',(-49.5332480724909,-93.1518122048732,
67.0212414872382));
#209871=CARTESIAN_POINT('Ctrl Pts',(-49.4173675969609,-91.3814301244552,
63.3804659554293));
#209872=CARTESIAN_POINT('Ctrl Pts',(-49.3014871214309,-88.3293491819053,
60.7207101200916));
#209873=CARTESIAN_POINT('Ctrl Pts',(-49.1856066459009,-84.4807052266326,
59.4647487795594));
#209874=CARTESIAN_POINT('Ctrl Pts',(-49.0697261703709,-80.447249777423,
59.8122201107395));
#209875=CARTESIAN_POINT('Ctrl Pts',(-48.9538456948409,-76.8701106016706,
61.7078926778295));
#209876=CARTESIAN_POINT('Ctrl Pts',(-48.8379652193109,-74.3178828522775,
64.8504446324207));
#209877=CARTESIAN_POINT('Ctrl Pts',(-48.7220847437809,-73.1962494979973,
68.7403594723971));
#209878=CARTESIAN_POINT('Ctrl Pts',(-48.6062042682609,-73.6834968483605,
72.7593257953694));
#209879=CARTESIAN_POINT('Ctrl Pts',(-48.4903237927309,-75.7021760959367,
76.2685180728017));
#209880=CARTESIAN_POINT('Ctrl Pts',(-48.3744433172009,-78.9314117793381,
78.710144629103));
#209881=CARTESIAN_POINT('Ctrl Pts',(-48.2585628416709,-82.8579140104155,
79.6960910777588));
#209882=CARTESIAN_POINT('Ctrl Pts',(-48.1426823661409,-86.8575362933791,
79.0696827398739));
#209883=CARTESIAN_POINT('Ctrl Pts',(-48.0268018906109,-90.2946004215829,
76.9303247204407));
#209884=CARTESIAN_POINT('Ctrl Pts',(-47.9495482402609,-91.8465394405205,
74.7225652803544));
#209885=CARTESIAN_POINT('Ctrl Pts',(-47.9109214150809,-92.3761449683377,
73.5106567464228));
#209886=CARTESIAN_POINT('Ctrl Pts',(-55.1031437386839,-89.1716495247985,
78.0464295027995));
#209887=CARTESIAN_POINT('Ctrl Pts',(-55.0645169135079,-90.3081071926132,
77.2632582583921));
#209888=CARTESIAN_POINT('Ctrl Pts',(-54.9872632631549,-92.2618542008096,
75.2350099031932));
#209889=CARTESIAN_POINT('Ctrl Pts',(-54.8713827876249,-93.7712830739489,
71.289035799845));
#209890=CARTESIAN_POINT('Ctrl Pts',(-54.7555023120959,-93.6190186885821,
67.0670781799152));
#209891=CARTESIAN_POINT('Ctrl Pts',(-54.6396218365659,-91.8294176899935,
63.2401216789652));
#209892=CARTESIAN_POINT('Ctrl Pts',(-54.5237413610409,-88.686900381402,
60.4164989490926));
#209893=CARTESIAN_POINT('Ctrl Pts',(-54.4078608855109,-84.6909887425699,
59.0450242272283));
#209894=CARTESIAN_POINT('Ctrl Pts',(-54.2919804099809,-80.4768398974234,
59.3436988676507));
#209895=CARTESIAN_POINT('Ctrl Pts',(-54.1760999344509,-76.7143040687269,
61.2650472476524));
#209896=CARTESIAN_POINT('Ctrl Pts',(-54.0602194589209,-74.0014454626398,
64.5036664147486));
#209897=CARTESIAN_POINT('Ctrl Pts',(-53.9443389833909,-72.7694797521119,
68.5447697661598));
#209898=CARTESIAN_POINT('Ctrl Pts',(-53.8284585078609,-73.2142309326136,
72.746013893864));
#209899=CARTESIAN_POINT('Ctrl Pts',(-53.7125780323309,-75.2650047030302,
76.4396006022121));
#209900=CARTESIAN_POINT('Ctrl Pts',(-53.5966975568009,-78.5958254759494,
79.0384251072975));
#209901=CARTESIAN_POINT('Ctrl Pts',(-53.4808170812709,-82.6772510137972,
80.1293977965975));
#209902=CARTESIAN_POINT('Ctrl Pts',(-53.3649366057409,-86.8605285862284,
79.5391058504835));
#209903=CARTESIAN_POINT('Ctrl Pts',(-53.2490561302109,-90.4807158290425,
77.3613776404707));
#209904=CARTESIAN_POINT('Ctrl Pts',(-53.1331756546809,-92.9623749849825,
73.9423684764853));
#209905=CARTESIAN_POINT('Ctrl Pts',(-53.0172951791509,-93.9110401651089,
69.8255383602718));
#209906=CARTESIAN_POINT('Ctrl Pts',(-52.9014147036209,-93.1759186818892,
65.6652676678046));
#209907=CARTESIAN_POINT('Ctrl Pts',(-52.7855342280909,-90.8738599216446,
62.1228417625684));
#209908=CARTESIAN_POINT('Ctrl Pts',(-52.6696537525609,-87.3707818441818,
59.7613380439862));
#209909=CARTESIAN_POINT('Ctrl Pts',(-52.5537732770309,-83.2235074139119,
58.956123395707));
#209910=CARTESIAN_POINT('Ctrl Pts',(-52.4378928015009,-79.0912562061879,
59.8351886867613));
#209911=CARTESIAN_POINT('Ctrl Pts',(-52.3220123259709,-75.6308598177706,
62.258804304951));
#209912=CARTESIAN_POINT('Ctrl Pts',(-52.2061318504409,-73.3923568525672,
65.8417305258611));
#209913=CARTESIAN_POINT('Ctrl Pts',(-52.0902513749109,-72.7315629188536,
70.0144523242639));
#209914=CARTESIAN_POINT('Ctrl Pts',(-51.9743708993809,-73.7535128542524,
74.113705202441));
#209915=CARTESIAN_POINT('Ctrl Pts',(-51.8584904238609,-76.2957651773164,
77.487902730087));
#209916=CARTESIAN_POINT('Ctrl Pts',(-51.7426099483309,-79.9542225646198,
79.6007078263948));
#209917=CARTESIAN_POINT('Ctrl Pts',(-51.6267294728009,-84.1473641243655,
80.1162848716646));
#209918=CARTESIAN_POINT('Ctrl Pts',(-51.5108489972709,-88.2086795870379,
78.9526816135227));
#209919=CARTESIAN_POINT('Ctrl Pts',(-51.3949685217409,-91.4926127687853,
76.2948556810079));
#209920=CARTESIAN_POINT('Ctrl Pts',(-51.2790880462109,-93.477174330855,
72.5652751099481));
#209921=CARTESIAN_POINT('Ctrl Pts',(-51.1632075706809,-93.84691328197,68.3567659989079));
#209922=CARTESIAN_POINT('Ctrl Pts',(-51.0473270951509,-92.5430586971659,
64.338281327871));
#209923=CARTESIAN_POINT('Ctrl Pts',(-50.9314466196209,-89.7728615023466,
61.1485692199366));
#209924=CARTESIAN_POINT('Ctrl Pts',(-50.8155661440909,-85.9766514246951,
59.2946423400516));
#209925=CARTESIAN_POINT('Ctrl Pts',(-50.6996856685609,-81.7578454883824,
59.0711869721971));
#209926=CARTESIAN_POINT('Ctrl Pts',(-50.5838051930309,-77.7870333793684,
60.5137219022862));
#209927=CARTESIAN_POINT('Ctrl Pts',(-50.4679247175009,-74.6953855485565,
63.3929526189662));
#209928=CARTESIAN_POINT('Ctrl Pts',(-50.3520442419709,-72.9743271003957,
67.2512182458574));
#209929=CARTESIAN_POINT('Ctrl Pts',(-50.2361637664409,-72.8974245514948,
71.4752378750255));
#209930=CARTESIAN_POINT('Ctrl Pts',(-50.1202832909109,-74.4769017530788,
75.3935930910951));
#209931=CARTESIAN_POINT('Ctrl Pts',(-50.0044028153909,-77.4616968794652,
78.383451596628));
#209932=CARTESIAN_POINT('Ctrl Pts',(-49.8885223398609,-81.3773693290668,
79.9695679533435));
#209933=CARTESIAN_POINT('Ctrl Pts',(-49.7726418643309,-85.6015132368418,
79.8998250253565));
#209934=CARTESIAN_POINT('Ctrl Pts',(-49.6567613888009,-89.462690433018,
78.1853086243629));
#209935=CARTESIAN_POINT('Ctrl Pts',(-49.5408809132709,-92.3471572085029,
75.0985453923105));
#209936=CARTESIAN_POINT('Ctrl Pts',(-49.4250004377409,-93.7964204023591,
71.1301840145485));
#209937=CARTESIAN_POINT('Ctrl Pts',(-49.3091199622109,-93.5801160289695,
66.9110053921681));
#209938=CARTESIAN_POINT('Ctrl Pts',(-49.1932394866809,-91.7326262059582,
63.111658450455));
#209939=CARTESIAN_POINT('Ctrl Pts',(-49.0773590111509,-88.5476140310613,
60.3360588260279));
#209940=CARTESIAN_POINT('Ctrl Pts',(-48.9614785356209,-84.5313451033357,
59.0253949753285));
#209941=CARTESIAN_POINT('Ctrl Pts',(-48.8455980601009,-80.3222153474369,
59.3880001752185));
#209942=CARTESIAN_POINT('Ctrl Pts',(-48.7297175845709,-76.5892763983811,
61.3662374236589));
#209943=CARTESIAN_POINT('Ctrl Pts',(-48.6138371090409,-73.9258881698316,
64.6456610117156));
#209944=CARTESIAN_POINT('Ctrl Pts',(-48.4979566335109,-72.7554028660613,
68.7049983484054));
#209945=CARTESIAN_POINT('Ctrl Pts',(-48.3820761579809,-73.2638719310397,
72.8990079143937));
#209946=CARTESIAN_POINT('Ctrl Pts',(-48.2661956824509,-75.3704733291652,
76.5610405859094));
#209947=CARTESIAN_POINT('Ctrl Pts',(-48.1503152069209,-78.7403560946919,
79.1090104644245));
#209948=CARTESIAN_POINT('Ctrl Pts',(-48.0344347313909,-82.8378743604903,
80.1378991151166));
#209949=CARTESIAN_POINT('Ctrl Pts',(-47.9185542558709,-87.0116973704533,
79.4842080039733));
#209950=CARTESIAN_POINT('Ctrl Pts',(-47.8026737803409,-90.5984604020873,
77.251671755215));
#209951=CARTESIAN_POINT('Ctrl Pts',(-47.7254201299809,-92.2179930301717,
74.9477549101844));
#209952=CARTESIAN_POINT('Ctrl Pts',(-47.6867933048109,-92.7706651531469,
73.6830625549966));
#209953=CARTESIAN_POINT('',(-55.5975553638665,-91.4098880899276,73.6973239050991));
#209954=CARTESIAN_POINT('Ctrl Pts',(-62.9066342559309,-91.0821450451938,
74.1516175606607));
#209955=CARTESIAN_POINT('Ctrl Pts',(-62.8680074307549,-91.6975062893363,
73.1128364439599));
#209956=CARTESIAN_POINT('Ctrl Pts',(-62.7907537804019,-92.5053451055553,
70.7854776041952));
#209957=CARTESIAN_POINT('Ctrl Pts',(-62.6748733048729,-92.2570005774417,
67.098000141731));
#209958=CARTESIAN_POINT('Ctrl Pts',(-62.5589928293429,-90.5877173901553,
63.8007419836912));
#209959=CARTESIAN_POINT('Ctrl Pts',(-62.4431123538139,-87.7629155557435,
61.4176698865353));
#209960=CARTESIAN_POINT('Ctrl Pts',(-62.3272318782849,-84.2315820238582,
60.3276167603847));
#209961=CARTESIAN_POINT('Ctrl Pts',(-62.2113514027559,-80.5550370144063,
60.7038391619823));
#209962=CARTESIAN_POINT('Ctrl Pts',(-62.0954709272259,-77.3176748891168,
62.4865383110414));
#209963=CARTESIAN_POINT('Ctrl Pts',(-61.9795904516969,-75.0340828310024,
65.3923490235231));
#209964=CARTESIAN_POINT('Ctrl Pts',(-61.8637099761679,-74.0672433566291,
68.9593856609049));
#209965=CARTESIAN_POINT('Ctrl Pts',(-61.7478295006379,-74.570838033561,
72.620658834703));
#209966=CARTESIAN_POINT('Ctrl Pts',(-61.6319490251089,-76.4648192283687,
75.7942000908074));
#209967=CARTESIAN_POINT('Ctrl Pts',(-61.5160685495799,-79.4481339264209,
77.9755671576036));
#209968=CARTESIAN_POINT('Ctrl Pts',(-61.4001880740499,-83.0465768432993,
78.8180263208338));
#209969=CARTESIAN_POINT('Ctrl Pts',(-61.2843075985209,-86.6881665365578,
78.1876666029972));
#209970=CARTESIAN_POINT('Ctrl Pts',(-61.1684271229909,-89.7940632762463,
76.1846852475528));
#209971=CARTESIAN_POINT('Ctrl Pts',(-61.0525466474619,-91.8705770584431,
73.1274611176964));
#209972=CARTESIAN_POINT('Ctrl Pts',(-60.9366661719329,-92.5876408580107,
69.5019475850796));
#209973=CARTESIAN_POINT('Ctrl Pts',(-60.8207856964029,-91.8312756023416,
65.8844290339351));
#209974=CARTESIAN_POINT('Ctrl Pts',(-60.7049052208739,-89.7217074281312,
62.8499190263368));
#209975=CARTESIAN_POINT('Ctrl Pts',(-60.5890247453439,-86.5942574382841,
60.8807604677571));
#209976=CARTESIAN_POINT('Ctrl Pts',(-60.4731442698149,-82.9460415793733,
60.2899560038079));
#209977=CARTESIAN_POINT('Ctrl Pts',(-60.3572637942849,-79.3569528268042,
61.1714154719932));
#209978=CARTESIAN_POINT('Ctrl Pts',(-60.2413833187559,-76.3974857555292,
63.3850286996998));
#209979=CARTESIAN_POINT('Ctrl Pts',(-60.1255028432259,-74.5380550098396,
66.578936364274));
#209980=CARTESIAN_POINT('Ctrl Pts',(-60.0096223676969,-74.0742217268447,
70.2454589066055));
#209981=CARTESIAN_POINT('Ctrl Pts',(-59.8937418921669,-75.0797133593528,
73.8017934584711));
#209982=CARTESIAN_POINT('Ctrl Pts',(-59.7778614166379,-77.3947045140553,
76.682651806513));
#209983=CARTESIAN_POINT('Ctrl Pts',(-59.6619809411079,-80.65122159491,78.430114358312));
#209984=CARTESIAN_POINT('Ctrl Pts',(-59.5461004655789,-84.3316331205256,
78.7664175993805));
#209985=CARTESIAN_POINT('Ctrl Pts',(-59.4302199900499,-87.850928534276,
77.6381052939461));
#209986=CARTESIAN_POINT('Ctrl Pts',(-59.3143395145199,-90.6497070858334,
75.2245254864509));
#209987=CARTESIAN_POINT('Ctrl Pts',(-59.1984590389909,-92.283095970383,
71.9093226842531));
#209988=CARTESIAN_POINT('Ctrl Pts',(-59.0825785634609,-92.4914639662642,
68.2194566099759));
#209989=CARTESIAN_POINT('Ctrl Pts',(-58.9666980879319,-91.2416904628249,
64.7414406442362));
#209990=CARTESIAN_POINT('Ctrl Pts',(-58.8508176124019,-88.7324300637027,
62.0281140665388));
#209991=CARTESIAN_POINT('Ctrl Pts',(-58.7349371368729,-85.3625359440494,
60.5107668781401));
#209992=CARTESIAN_POINT('Ctrl Pts',(-58.6190566613429,-81.6676611472649,
60.4305851847562));
#209993=CARTESIAN_POINT('Ctrl Pts',(-58.5031761858139,-78.2351152028786,
61.8003140657713));
#209994=CARTESIAN_POINT('Ctrl Pts',(-58.3872957102849,-75.6105098175054,
64.4022317122195));
#209995=CARTESIAN_POINT('Ctrl Pts',(-58.2714152347549,-74.2110325384453,
67.822756849275));
#209996=CARTESIAN_POINT('Ctrl Pts',(-58.1555347592259,-74.259133756452,
71.5181885075058));
#209997=CARTESIAN_POINT('Ctrl Pts',(-58.0396542836959,-75.7471676634089,
74.901128642888));
#209998=CARTESIAN_POINT('Ctrl Pts',(-57.9237738081669,-78.4386075725234,
77.4338505153925));
#209999=CARTESIAN_POINT('Ctrl Pts',(-57.8078933326379,-81.9056424228852,
78.7137716903922));
#210000=CARTESIAN_POINT('Ctrl Pts',(-57.6920128571079,-85.5971784105718,
78.5374455169307));
#210001=CARTESIAN_POINT('Ctrl Pts',(-57.5761323815789,-88.9264367180665,
76.9328994783958));
#210002=CARTESIAN_POINT('Ctrl Pts',(-57.4602519060499,-91.3642234652816,
74.1551801543822));
#210003=CARTESIAN_POINT('Ctrl Pts',(-57.3443714305209,-92.523046391615,
70.6458129331831));
#210004=CARTESIAN_POINT('Ctrl Pts',(-57.2284909549909,-92.2187077136396,
66.9626204542406));
#210005=CARTESIAN_POINT('Ctrl Pts',(-57.1126104794619,-90.4995828203968,
63.6910553136321));
#210006=CARTESIAN_POINT('Ctrl Pts',(-56.9967300039329,-87.6389308851381,
61.3511409192107));
#210007=CARTESIAN_POINT('Ctrl Pts',(-56.8808495284039,-84.091459640771,
60.3148124779814));
#210008=CARTESIAN_POINT('Ctrl Pts',(-56.7649690528749,-80.4210484558933,
60.7467969703094));
#210009=CARTESIAN_POINT('Ctrl Pts',(-56.6490885773459,-77.2111183081457,
62.57842938896));
#210010=CARTESIAN_POINT('Ctrl Pts',(-56.5332081018169,-74.9718955700618,
65.5185672056337));
#210011=CARTESIAN_POINT('Ctrl Pts',(-56.4173276262869,-74.0593102599364,
69.0998682252855));
#210012=CARTESIAN_POINT('Ctrl Pts',(-56.3014471507579,-74.6184200790472,
72.7530756919932));
#210013=CARTESIAN_POINT('Ctrl Pts',(-56.1855666752289,-76.560353137091,
75.8975034275876));
#210014=CARTESIAN_POINT('Ctrl Pts',(-56.0696861997009,-79.5764343320587,
78.0333359882835));
#210015=CARTESIAN_POINT('Ctrl Pts',(-55.9538057241719,-83.18725012881,78.8210806253173));
#210016=CARTESIAN_POINT('Ctrl Pts',(-55.8379252486429,-86.8188521429654,
78.1355116392279));
#210017=CARTESIAN_POINT('Ctrl Pts',(-55.7220447731139,-89.8939891133529,
76.0856457086153));
#210018=CARTESIAN_POINT('Ctrl Pts',(-55.6061642975849,-91.9238570102634,
72.9971507091326));
#210019=CARTESIAN_POINT('Ctrl Pts',(-55.5289106472319,-92.3651629072477,
70.5734238624515));
#210020=CARTESIAN_POINT('Ctrl Pts',(-55.4902838220559,-92.3402865293407,
69.3663129168427));
#210021=CARTESIAN_POINT('Ctrl Pts',(-62.6825061456549,-91.452573473999,
74.371054836858));
#210022=CARTESIAN_POINT('Ctrl Pts',(-62.6438793204789,-92.0972937684766,
73.282713193911));
#210023=CARTESIAN_POINT('Ctrl Pts',(-62.5666256701259,-92.9436747917172,
70.8443154384341));
#210024=CARTESIAN_POINT('Ctrl Pts',(-62.4507451945969,-92.6834816794201,
66.9809074352464));
#210025=CARTESIAN_POINT('Ctrl Pts',(-62.3348647190669,-90.9345565426601,
63.5263362043601));
#210026=CARTESIAN_POINT('Ctrl Pts',(-62.2189842435379,-87.9749826535781,
61.0295670970088));
#210027=CARTESIAN_POINT('Ctrl Pts',(-62.1031037680089,-84.2751682498535,
59.8875072432627));
#210028=CARTESIAN_POINT('Ctrl Pts',(-61.9872232924799,-80.4232142899493,
60.2816793167476));
#210029=CARTESIAN_POINT('Ctrl Pts',(-61.8713428169499,-77.0313967476354,
62.1494315213011));
#210030=CARTESIAN_POINT('Ctrl Pts',(-61.7554623414209,-74.6388538987226,
65.1938792437981));
#210031=CARTESIAN_POINT('Ctrl Pts',(-61.6395818658919,-73.6258862531933,
68.9311001577751));
#210032=CARTESIAN_POINT('Ctrl Pts',(-61.5237013903619,-74.1535075675003,
72.7670536586458));
#210033=CARTESIAN_POINT('Ctrl Pts',(-61.4078209148329,-76.137851114111,
76.0920054209541));
#210034=CARTESIAN_POINT('Ctrl Pts',(-61.2919404393039,-79.26350055816,78.3774460967395));
#210035=CARTESIAN_POINT('Ctrl Pts',(-61.1760599637739,-83.0336261536677,
79.2600992130555));
#210036=CARTESIAN_POINT('Ctrl Pts',(-61.0601794882449,-86.8489570698533,
78.5996648636749));
#210037=CARTESIAN_POINT('Ctrl Pts',(-60.9442990127149,-90.1030369776855,
76.5011207294713));
#210038=CARTESIAN_POINT('Ctrl Pts',(-60.8284185371859,-92.2786217904858,
73.2980356147633));
#210039=CARTESIAN_POINT('Ctrl Pts',(-60.7125380616569,-93.0298968966431,
69.4995478571636));
#210040=CARTESIAN_POINT('Ctrl Pts',(-60.5966575861269,-92.2374452513553,
65.7094365237526));
#210041=CARTESIAN_POINT('Ctrl Pts',(-60.4807771105979,-90.0272290126208,
62.5301492281794));
#210042=CARTESIAN_POINT('Ctrl Pts',(-60.3648966350679,-86.7505675432666,
60.4670415855671));
#210043=CARTESIAN_POINT('Ctrl Pts',(-60.2490161595389,-82.9282943252811,
59.8480496818692));
#210044=CARTESIAN_POINT('Ctrl Pts',(-60.1331356840089,-79.1679691837779,
60.7715638181681));
#210045=CARTESIAN_POINT('Ctrl Pts',(-60.0172552084799,-76.0673051431882,
63.0907891278659));
#210046=CARTESIAN_POINT('Ctrl Pts',(-59.9013747329499,-74.1191604569068,
66.4370789854654));
#210047=CARTESIAN_POINT('Ctrl Pts',(-59.7854942574209,-73.6331975633271,
70.2785323036529));
#210048=CARTESIAN_POINT('Ctrl Pts',(-59.6696137818909,-74.6866614718425,
74.004540532737));
#210049=CARTESIAN_POINT('Ctrl Pts',(-59.5537333063619,-77.112101476679,
77.0228454067829));
#210050=CARTESIAN_POINT('Ctrl Pts',(-59.4378528308319,-80.5239878626353,
78.8536798665507));
#210051=CARTESIAN_POINT('Ctrl Pts',(-59.3219723553029,-84.3799928112316,
79.2060282256322));
#210052=CARTESIAN_POINT('Ctrl Pts',(-59.2060918797729,-88.0671947549688,
78.0238838368779));
#210053=CARTESIAN_POINT('Ctrl Pts',(-59.0902114042439,-90.9995037833793,
75.4951514881295));
#210054=CARTESIAN_POINT('Ctrl Pts',(-58.9743309287149,-92.7108220905774,
72.0217794692934));
#210055=CARTESIAN_POINT('Ctrl Pts',(-58.8584504531849,-92.9291313795479,
68.1558688929745));
#210056=CARTESIAN_POINT('Ctrl Pts',(-58.7425699776559,-91.6197308463801,
64.5119158508118));
#210057=CARTESIAN_POINT('Ctrl Pts',(-58.6266895021259,-88.9907529592742,
61.6691357328928));
#210058=CARTESIAN_POINT('Ctrl Pts',(-58.5108090265969,-85.4600802855175,
60.079395502359));
#210059=CARTESIAN_POINT('Ctrl Pts',(-58.3949285510669,-81.5889220192099,
59.9953883188284));
#210060=CARTESIAN_POINT('Ctrl Pts',(-58.2790480755379,-77.9926083853276,
61.4304673328671));
#210061=CARTESIAN_POINT('Ctrl Pts',(-58.1631676000089,-75.2427823716655,
64.1565231694806));
#210062=CARTESIAN_POINT('Ctrl Pts',(-58.0472871244789,-73.7765356555165,
67.7402424800745));
#210063=CARTESIAN_POINT('Ctrl Pts',(-57.9314066489499,-73.8269317955608,
71.6119841758515));
#210064=CARTESIAN_POINT('Ctrl Pts',(-57.8155261734199,-75.3859602001198,
75.1563252942432));
#210065=CARTESIAN_POINT('Ctrl Pts',(-57.6996456978909,-78.2058094306096,
77.8098840079436));
#210066=CARTESIAN_POINT('Ctrl Pts',(-57.5837652223619,-81.8382574454312,
79.1508705661768));
#210067=CARTESIAN_POINT('Ctrl Pts',(-57.4678847468319,-85.7059176071747,
78.9661318235942));
#210068=CARTESIAN_POINT('Ctrl Pts',(-57.3520042713029,-89.1940157232479,
77.2850324623463));
#210069=CARTESIAN_POINT('Ctrl Pts',(-57.2361237957739,-91.7481099313085,
74.3747874028884));
#210070=CARTESIAN_POINT('Ctrl Pts',(-57.1202433202449,-92.9622206108914,
70.6979873284379));
#210071=CARTESIAN_POINT('Ctrl Pts',(-57.0043628447149,-92.6433618528013,
66.8390687464838));
#210072=CARTESIAN_POINT('Ctrl Pts',(-56.8884823691859,-90.8422170489019,
63.4114163537942));
#210073=CARTESIAN_POINT('Ctrl Pts',(-56.7726018936569,-87.8450826410214,
60.9598640147741));
#210074=CARTESIAN_POINT('Ctrl Pts',(-56.6567214181279,-84.1283605902155,
59.8740920651051));
#210075=CARTESIAN_POINT('Ctrl Pts',(-56.5408409425989,-80.2828331013019,
60.3266866536539));
#210076=CARTESIAN_POINT('Ctrl Pts',(-56.4249604670699,-76.9197563235507,
62.2457067472406));
#210077=CARTESIAN_POINT('Ctrl Pts',(-56.3090799915409,-74.5736996668511,
65.326119329296));
#210078=CARTESIAN_POINT('Ctrl Pts',(-56.1931995160109,-73.6175746663254,
69.0782851830545));
#210079=CARTESIAN_POINT('Ctrl Pts',(-56.0773190404819,-74.2033597651636,
72.9057881597825));
#210080=CARTESIAN_POINT('Ctrl Pts',(-55.9614385649529,-76.2379429712918,
76.2002373876932));
#210081=CARTESIAN_POINT('Ctrl Pts',(-55.8455580894239,-79.3979222106296,
78.4379710938565));
#210082=CARTESIAN_POINT('Ctrl Pts',(-55.7296776138959,-83.1810109994356,
79.2632992392267));
#210083=CARTESIAN_POINT('Ctrl Pts',(-55.6137971383669,-86.9858777216637,
78.545021572567));
#210084=CARTESIAN_POINT('Ctrl Pts',(-55.4979166628379,-90.2077303033346,
76.3973559875148));
#210085=CARTESIAN_POINT('Ctrl Pts',(-55.3820361873089,-92.3344437431285,
73.1615080615852));
#210086=CARTESIAN_POINT('Ctrl Pts',(-55.3047825369559,-92.7968044630577,
70.6221445556835));
#210087=CARTESIAN_POINT('Ctrl Pts',(-55.2661557117799,-92.7707412264758,
69.357442022453));
#210088=CARTESIAN_POINT('Ctrl Pts',(-62.4583780353789,-91.8230019028041,
74.5904921130553));
#210089=CARTESIAN_POINT('Ctrl Pts',(-62.4197512102019,-92.4970812476076,
73.4525899438658));
#210090=CARTESIAN_POINT('Ctrl Pts',(-62.3424975598499,-93.3820044778794,
70.903153272674));
#210091=CARTESIAN_POINT('Ctrl Pts',(-62.2266170843209,-93.1099627814073,
66.863814728757));
#210092=CARTESIAN_POINT('Ctrl Pts',(-62.1107366087909,-91.2813956951746,
63.2519304250261));
#210093=CARTESIAN_POINT('Ctrl Pts',(-61.9948561332619,-88.1870497514119,
60.6414643074804));
#210094=CARTESIAN_POINT('Ctrl Pts',(-61.8789756577329,-84.3187544758582,
59.4473977261369));
#210095=CARTESIAN_POINT('Ctrl Pts',(-61.7630951822039,-80.2913915654904,
59.8595194715136));
#210096=CARTESIAN_POINT('Ctrl Pts',(-61.6472147066739,-76.7451186061521,
61.8123247315614));
#210097=CARTESIAN_POINT('Ctrl Pts',(-61.5313342311449,-74.2436249664418,
64.9954094640758));
#210098=CARTESIAN_POINT('Ctrl Pts',(-61.4154537556159,-73.1845291497573,
68.9028146546496));
#210099=CARTESIAN_POINT('Ctrl Pts',(-61.2995732800859,-73.7361771014411,
72.9134484825933));
#210100=CARTESIAN_POINT('Ctrl Pts',(-61.1836928045569,-75.8108829998573,
76.3898107511057));
#210101=CARTESIAN_POINT('Ctrl Pts',(-61.0678123290279,-79.0788671899051,
78.7793250358795));
#210102=CARTESIAN_POINT('Ctrl Pts',(-60.9519318534979,-83.0206754640438,
79.7021721052772));
#210103=CARTESIAN_POINT('Ctrl Pts',(-60.8360513779689,-87.0097476031586,
79.0116631243528));
#210104=CARTESIAN_POINT('Ctrl Pts',(-60.7201709024389,-90.4120106791324,
76.8175562113822));
#210105=CARTESIAN_POINT('Ctrl Pts',(-60.6042904269099,-92.6866665225346,
73.468610111819));
#210106=CARTESIAN_POINT('Ctrl Pts',(-60.4884099513809,-93.4721529352706,
69.4971481292357));
#210107=CARTESIAN_POINT('Ctrl Pts',(-60.3725294758509,-92.6436149003541,
65.5344440135603));
#210108=CARTESIAN_POINT('Ctrl Pts',(-60.2566490003219,-90.332750597095,
62.210379430011));
#210109=CARTESIAN_POINT('Ctrl Pts',(-60.1407685247919,-86.9068776482263,
60.0533227033745));
#210110=CARTESIAN_POINT('Ctrl Pts',(-60.0248880492629,-82.9105470711673,
59.4061433599308));
#210111=CARTESIAN_POINT('Ctrl Pts',(-59.9090075737329,-78.9789855407346,
60.3717121643543));
#210112=CARTESIAN_POINT('Ctrl Pts',(-59.7931270982039,-75.7371245308324,
62.796549556049));
#210113=CARTESIAN_POINT('Ctrl Pts',(-59.6772466226739,-73.7002659039675,
66.2952216066778));
#210114=CARTESIAN_POINT('Ctrl Pts',(-59.5613661471449,-73.192173399811,
70.3116057007245));
#210115=CARTESIAN_POINT('Ctrl Pts',(-59.4454856716149,-74.2936095843438,
74.2072876070263));
#210116=CARTESIAN_POINT('Ctrl Pts',(-59.3296051960859,-76.8294984393236,
77.3630390070701));
#210117=CARTESIAN_POINT('Ctrl Pts',(-59.2137247205559,-80.3967541303873,
79.277245374799));
#210118=CARTESIAN_POINT('Ctrl Pts',(-59.0978442450269,-84.4283525019679,
79.6456388518811));
#210119=CARTESIAN_POINT('Ctrl Pts',(-58.9819637694969,-88.2834609756893,
78.4096623797982));
#210120=CARTESIAN_POINT('Ctrl Pts',(-58.8660832939679,-91.3493004809464,
75.765777489781));
#210121=CARTESIAN_POINT('Ctrl Pts',(-58.7502028184379,-93.13854821078,72.1342362543011));
#210122=CARTESIAN_POINT('Ctrl Pts',(-58.6343223429089,-93.3667987928187,
68.0922811759415));
#210123=CARTESIAN_POINT('Ctrl Pts',(-58.5184418673799,-91.997771229922,
64.282391057355));
#210124=CARTESIAN_POINT('Ctrl Pts',(-58.4025613918499,-89.2490758548062,
61.3101573992296));
#210125=CARTESIAN_POINT('Ctrl Pts',(-58.2866809163209,-85.5576246269588,
59.6480241265653));
#210126=CARTESIAN_POINT('Ctrl Pts',(-58.1708004407909,-81.5101828911056,
59.5601914529124));
#210127=CARTESIAN_POINT('Ctrl Pts',(-58.0549199652619,-77.7501015677444,
61.0606205999848));
#210128=CARTESIAN_POINT('Ctrl Pts',(-57.9390394897319,-74.875054925804,
63.9108146267733));
#210129=CARTESIAN_POINT('Ctrl Pts',(-57.8231590142029,-73.3420387725811,
67.6577281109136));
#210130=CARTESIAN_POINT('Ctrl Pts',(-57.7072785386739,-73.3947298346776,
71.7057798442351));
#210131=CARTESIAN_POINT('Ctrl Pts',(-57.5913980631439,-75.0247527368537,
75.4115219456312));
#210132=CARTESIAN_POINT('Ctrl Pts',(-57.4755175876149,-77.9730112887291,
78.1859175005156));
#210133=CARTESIAN_POINT('Ctrl Pts',(-57.3596371120859,-81.7708724680175,
79.5879694419674));
#210134=CARTESIAN_POINT('Ctrl Pts',(-57.2437566365559,-85.8146568038154,
79.3948181302474));
#210135=CARTESIAN_POINT('Ctrl Pts',(-57.1278761610269,-89.4615947284621,
77.6371654462713));
#210136=CARTESIAN_POINT('Ctrl Pts',(-57.0119956854979,-92.1319963973636,
74.5943946513581));
#210137=CARTESIAN_POINT('Ctrl Pts',(-56.8961152099689,-93.4013948301736,
70.7501617236546));
#210138=CARTESIAN_POINT('Ctrl Pts',(-56.7802347344389,-93.0680159919581,
66.7155170386891));
#210139=CARTESIAN_POINT('Ctrl Pts',(-56.6643542589099,-91.1848512773756,
63.1317773939326));
#210140=CARTESIAN_POINT('Ctrl Pts',(-56.5484737833809,-88.0512343968762,
60.568587110321));
#210141=CARTESIAN_POINT('Ctrl Pts',(-56.4325933078519,-84.1652615396361,
59.4333716522234));
#210142=CARTESIAN_POINT('Ctrl Pts',(-56.3167128323229,-80.1446177466814,
59.9065763370039));
#210143=CARTESIAN_POINT('Ctrl Pts',(-56.2008323567939,-76.6283943389352,
61.9129841055395));
#210144=CARTESIAN_POINT('Ctrl Pts',(-56.0849518812639,-74.1755037636287,
65.1336714529826));
#210145=CARTESIAN_POINT('Ctrl Pts',(-55.9690714057349,-73.1758390727135,
69.0567021408465));
#210146=CARTESIAN_POINT('Ctrl Pts',(-55.8531909302059,-73.7882994512876,
73.0585006275909));
#210147=CARTESIAN_POINT('Ctrl Pts',(-55.7373104546769,-75.9155328055053,
76.5029713478119));
#210148=CARTESIAN_POINT('Ctrl Pts',(-55.6214299791479,-79.2194100892149,
78.8426061994354));
#210149=CARTESIAN_POINT('Ctrl Pts',(-55.5055495036199,-83.1747718700718,
79.705517853136));
#210150=CARTESIAN_POINT('Ctrl Pts',(-55.3896690280909,-87.1529033003677,
78.9545315059016));
#210151=CARTESIAN_POINT('Ctrl Pts',(-55.2737885525619,-90.5214714933247,
76.7090662664086));
#210152=CARTESIAN_POINT('Ctrl Pts',(-55.1579080770329,-92.7450304759939,
73.3258654140387));
#210153=CARTESIAN_POINT('Ctrl Pts',(-55.0806544266799,-93.2284460188592,
70.6708652489211));
#210154=CARTESIAN_POINT('Ctrl Pts',(-55.0420276015039,-93.2011959236129,
69.348571128068));
#210155=CARTESIAN_POINT('Ctrl Pts',(-62.2342499251029,-92.1934303316092,
74.8099293892526));
#210156=CARTESIAN_POINT('Ctrl Pts',(-62.1956230999259,-92.8968687267479,
73.6224666938168));
#210157=CARTESIAN_POINT('Ctrl Pts',(-62.1183694495739,-93.8203341640412,
70.961991106913));
#210158=CARTESIAN_POINT('Ctrl Pts',(-62.0024889740439,-93.5364438833945,
66.7467220222676));
#210159=CARTESIAN_POINT('Ctrl Pts',(-61.8866084985149,-91.6282348476794,
62.977524645695));
#210160=CARTESIAN_POINT('Ctrl Pts',(-61.7707280229859,-88.3991168492557,
60.25336151795));
#210161=CARTESIAN_POINT('Ctrl Pts',(-61.6548475474569,-84.3623407018535,
59.0072882090149));
#210162=CARTESIAN_POINT('Ctrl Pts',(-61.5389670719279,-80.1595688410345,
59.4373596262817));
#210163=CARTESIAN_POINT('Ctrl Pts',(-61.4230865963979,-76.4588404646688,
61.4752179418164));
#210164=CARTESIAN_POINT('Ctrl Pts',(-61.3072061208689,-73.8483960341625,
64.7969396843518));
#210165=CARTESIAN_POINT('Ctrl Pts',(-61.1913256453399,-72.7431720463215,
68.8745291515197));
#210166=CARTESIAN_POINT('Ctrl Pts',(-61.0754451698099,-73.3188466353806,
73.0598433065361));
#210167=CARTESIAN_POINT('Ctrl Pts',(-60.9595646942809,-75.4839148855997,
76.6876160812524));
#210168=CARTESIAN_POINT('Ctrl Pts',(-60.8436842187519,-78.8942338216446,
79.1812039750164));
#210169=CARTESIAN_POINT('Ctrl Pts',(-60.7278037432219,-83.0077247744123,
80.1442449974989));
#210170=CARTESIAN_POINT('Ctrl Pts',(-60.6119232676929,-87.1705381364528,
79.4236613850277));
#210171=CARTESIAN_POINT('Ctrl Pts',(-60.4960427921629,-90.7209843805715,
77.1339916933007));
#210172=CARTESIAN_POINT('Ctrl Pts',(-60.3801623166339,-93.0947112545776,
73.6391846088869));
#210173=CARTESIAN_POINT('Ctrl Pts',(-60.2642818411039,-93.9144089739031,
69.4947484013197));
#210174=CARTESIAN_POINT('Ctrl Pts',(-60.1484013655749,-93.0497845493678,
65.3594515033776));
#210175=CARTESIAN_POINT('Ctrl Pts',(-60.0325208900459,-90.638272181575,
61.8906096318565));
#210176=CARTESIAN_POINT('Ctrl Pts',(-59.9166404145159,-87.0631877532088,
59.6396038211845));
#210177=CARTESIAN_POINT('Ctrl Pts',(-59.8007599389869,-82.8927998170843,
58.9642370379884));
#210178=CARTESIAN_POINT('Ctrl Pts',(-59.6848794634569,-78.790001897706,
59.9718605105236));
#210179=CARTESIAN_POINT('Ctrl Pts',(-59.5689989879279,-75.4069439184913,
62.5023099842152));
#210180=CARTESIAN_POINT('Ctrl Pts',(-59.4531185123979,-73.2813713510347,
66.1533642278691));
#210181=CARTESIAN_POINT('Ctrl Pts',(-59.3372380368689,-72.7511492362934,
70.3446790977719));
#210182=CARTESIAN_POINT('Ctrl Pts',(-59.2213575613389,-73.9005576968343,
74.4100346812925));
#210183=CARTESIAN_POINT('Ctrl Pts',(-59.1054770858099,-76.5468954019475,
77.7032326073398));
#210184=CARTESIAN_POINT('Ctrl Pts',(-58.9895966102799,-80.2695203981129,
79.7008108830386));
#210185=CARTESIAN_POINT('Ctrl Pts',(-58.8737161347509,-84.4767121926759,
80.0852494781352));
#210186=CARTESIAN_POINT('Ctrl Pts',(-58.7578356592209,-88.4997271963806,
78.7954409227263));
#210187=CARTESIAN_POINT('Ctrl Pts',(-58.6419551836919,-91.6990971784923,
76.0364034914596));
#210188=CARTESIAN_POINT('Ctrl Pts',(-58.5260747081619,-93.566274330974,
72.2466930393405));
#210189=CARTESIAN_POINT('Ctrl Pts',(-58.4101942326329,-93.8044662060933,
68.0286934589439));
#210190=CARTESIAN_POINT('Ctrl Pts',(-58.2943137571039,-92.375811613486,
64.0528662639258));
#210191=CARTESIAN_POINT('Ctrl Pts',(-58.1784332815739,-89.5073987503684,
60.9511790655875));
#210192=CARTESIAN_POINT('Ctrl Pts',(-58.0625528060449,-85.6551689684265,
59.2166527507833));
#210193=CARTESIAN_POINT('Ctrl Pts',(-57.9466723305149,-81.4314437630425,
59.1249945869912));
#210194=CARTESIAN_POINT('Ctrl Pts',(-57.8307918549859,-77.5075947501924,
60.6907738670809));
#210195=CARTESIAN_POINT('Ctrl Pts',(-57.7149113794559,-74.5073274799646,
63.6651060840353));
#210196=CARTESIAN_POINT('Ctrl Pts',(-57.5990309039269,-72.9075418896531,
67.575213741715));
#210197=CARTESIAN_POINT('Ctrl Pts',(-57.4831504283979,-72.9625278737866,
71.7995755125808));
#210198=CARTESIAN_POINT('Ctrl Pts',(-57.3672699528679,-74.6635452735643,
75.6667185969865));
#210199=CARTESIAN_POINT('Ctrl Pts',(-57.2513894773389,-77.740213146816,
78.5619509930675));
#210200=CARTESIAN_POINT('Ctrl Pts',(-57.1355090018099,-81.7034874905648,
80.0250683177526));
#210201=CARTESIAN_POINT('Ctrl Pts',(-57.0196285262799,-85.923396000422,
79.8235044369147));
#210202=CARTESIAN_POINT('Ctrl Pts',(-56.9037480507509,-89.7291737336331,
77.9892984302229));
#210203=CARTESIAN_POINT('Ctrl Pts',(-56.7878675752219,-92.5158828633906,
74.8140018998643));
#210204=CARTESIAN_POINT('Ctrl Pts',(-56.6719870996929,-93.8405690494495,
70.8023361189084));
#210205=CARTESIAN_POINT('Ctrl Pts',(-56.5561066241629,-93.4926701311195,
66.5919653309314));
#210206=CARTESIAN_POINT('Ctrl Pts',(-56.4402261486339,-91.5274855058807,
62.8521384340946));
#210207=CARTESIAN_POINT('Ctrl Pts',(-56.3243456731049,-88.2573861527595,
60.1773102058844));
#210208=CARTESIAN_POINT('Ctrl Pts',(-56.2084651975759,-84.2021624890806,
58.992651239347));
#210209=CARTESIAN_POINT('Ctrl Pts',(-56.0925847220469,-80.0064023920941,
59.4864660203554));
#210210=CARTESIAN_POINT('Ctrl Pts',(-55.9767042465179,-76.3370323543386,
61.5802614638165));
#210211=CARTESIAN_POINT('Ctrl Pts',(-55.8608237709879,-73.7773078604179,
64.9412235766449));
#210212=CARTESIAN_POINT('Ctrl Pts',(-55.7449432954589,-72.7341034791027,
69.0351190986164));
#210213=CARTESIAN_POINT('Ctrl Pts',(-55.6290628199299,-73.3732391374036,
73.2112130953808));
#210214=CARTESIAN_POINT('Ctrl Pts',(-55.5131823444009,-75.5931226397066,
76.8057053079184));
#210215=CARTESIAN_POINT('Ctrl Pts',(-55.3973018688719,-79.0408979677858,
79.2472413050084));
#210216=CARTESIAN_POINT('Ctrl Pts',(-55.2814213933429,-83.1685327406974,
80.1477364670454));
#210217=CARTESIAN_POINT('Ctrl Pts',(-55.1655409178149,-87.3199288790655,
79.3640414392398));
#210218=CARTESIAN_POINT('Ctrl Pts',(-55.0496604422859,-90.8352126833059,
77.0207765453072));
#210219=CARTESIAN_POINT('Ctrl Pts',(-54.9337799667569,-93.155617208859,
73.4902227664913));
#210220=CARTESIAN_POINT('Ctrl Pts',(-54.8565263164039,-93.6600875746688,
70.7195859421521));
#210221=CARTESIAN_POINT('Ctrl Pts',(-54.8178994912279,-93.6316506207481,
69.3397002336783));
#210222=CARTESIAN_POINT('',(-62.7285891236391,-92.4023459513537,69.9231276410267));
#210223=CARTESIAN_POINT('Ctrl Pts',(-65.2384132905482,-92.5793602293726,
65.0087087433499));
#210224=CARTESIAN_POINT('Ctrl Pts',(-65.2029278919597,-92.020907624565,
63.8703843309197));
#210225=CARTESIAN_POINT('Ctrl Pts',(-65.1319570947826,-90.4796880229805,
61.8024113142918));
#210226=CARTESIAN_POINT('Ctrl Pts',(-65.0255008990171,-87.2049470387258,
59.7419494328986));
#210227=CARTESIAN_POINT('Ctrl Pts',(-64.9190447032515,-83.4077236954013,
59.0003860876845));
#210228=CARTESIAN_POINT('Ctrl Pts',(-64.8125885074859,-79.5984301452028,
59.6773007910861));
#210229=CARTESIAN_POINT('Ctrl Pts',(-64.7061323117203,-76.2891695109715,
61.6817243939745));
#210230=CARTESIAN_POINT('Ctrl Pts',(-64.5996761159548,-73.9248064731438,
64.7441915297996));
#210231=CARTESIAN_POINT('Ctrl Pts',(-64.4932199201892,-72.8231867097155,
68.4530125546885));
#210232=CARTESIAN_POINT('Ctrl Pts',(-64.3867637244237,-73.1324022343814,
72.3096048992952));
#210233=CARTESIAN_POINT('Ctrl Pts',(-64.2803075286581,-74.8108848414099,
75.7955215493427));
#210234=CARTESIAN_POINT('Ctrl Pts',(-64.1738513328926,-77.632993750829,
78.4421459656915));
#210235=CARTESIAN_POINT('Ctrl Pts',(-64.0673951371271,-81.2193488611975,
79.8936880956339));
#210236=CARTESIAN_POINT('Ctrl Pts',(-63.9609389413616,-85.0878315917651,
79.9550174392733));
#210237=CARTESIAN_POINT('Ctrl Pts',(-63.8544827455961,-88.7183957428313,
78.6178806428873));
#210238=CARTESIAN_POINT('Ctrl Pts',(-63.7480265498306,-91.6229818614739,
76.0620635928089));
#210239=CARTESIAN_POINT('Ctrl Pts',(-63.6415703540651,-93.41111347443,72.6310262841576));
#210240=CARTESIAN_POINT('Ctrl Pts',(-63.5705995568881,-93.6986662915826,
70.0679844126328));
#210241=CARTESIAN_POINT('Ctrl Pts',(-63.5351141582999,-93.6066243106656,
68.8033975024123));
#210242=CARTESIAN_POINT('Ctrl Pts',(-65.0142851802722,-92.1928244408197,
65.1983400256205));
#210243=CARTESIAN_POINT('Ctrl Pts',(-64.9787997816837,-91.6576796881873,
64.1075252799263));
#210244=CARTESIAN_POINT('Ctrl Pts',(-64.9078289845066,-90.1807851848182,
62.1258622007476));
#210245=CARTESIAN_POINT('Ctrl Pts',(-64.801372788741,-87.0427203985795,
60.1513967683751));
#210246=CARTESIAN_POINT('Ctrl Pts',(-64.6949165929754,-83.4039798336089,
59.4407836751363));
#210247=CARTESIAN_POINT('Ctrl Pts',(-64.5884603972099,-79.7536728298564,
60.0894463340284));
#210248=CARTESIAN_POINT('Ctrl Pts',(-64.4820042014443,-76.5825291227051,
62.0102123290093));
#210249=CARTESIAN_POINT('Ctrl Pts',(-64.3755480056787,-74.3168463018152,
64.9448628324088));
#210250=CARTESIAN_POINT('Ctrl Pts',(-64.2690918099132,-73.261204281863,
68.4988906815204));
#210251=CARTESIAN_POINT('Ctrl Pts',(-64.1626356141476,-73.5575142355291,
72.1945223939759));
#210252=CARTESIAN_POINT('Ctrl Pts',(-64.0561794183821,-75.1659428681317,
75.5349491147065));
#210253=CARTESIAN_POINT('Ctrl Pts',(-63.9497232226166,-77.8702668541082,
78.0711127145998));
#210254=CARTESIAN_POINT('Ctrl Pts',(-63.843267026851,-81.306940086253,79.4620725693219));
#210255=CARTESIAN_POINT('Ctrl Pts',(-63.7368108310855,-85.013965921681,
79.5208422413552));
#210256=CARTESIAN_POINT('Ctrl Pts',(-63.63035463532,-88.4930030642919,78.2395128430028));
#210257=CARTESIAN_POINT('Ctrl Pts',(-63.5238984395549,-91.2763619501754,
75.7903666285429));
#210258=CARTESIAN_POINT('Ctrl Pts',(-63.4174422437889,-92.989863223953,
72.5025287780578));
#210259=CARTESIAN_POINT('Ctrl Pts',(-63.3464714466119,-93.265414595499,
70.046459280852));
#210260=CARTESIAN_POINT('Ctrl Pts',(-63.3109860480239,-93.1772141238976,
68.834651790985));
#210261=CARTESIAN_POINT('Ctrl Pts',(-64.7901570699962,-91.8062886522624,
65.3879713079068));
#210262=CARTESIAN_POINT('Ctrl Pts',(-64.7546716714076,-91.2944517518238,
64.3446662289411));
#210263=CARTESIAN_POINT('Ctrl Pts',(-64.6837008742306,-89.8818823466701,
62.4493130872115));
#210264=CARTESIAN_POINT('Ctrl Pts',(-64.577244678465,-86.8804937584546,
60.5608441038513));
#210265=CARTESIAN_POINT('Ctrl Pts',(-64.4707884826994,-83.4002359718365,
59.8811812625842));
#210266=CARTESIAN_POINT('Ctrl Pts',(-64.3643322869338,-79.9089155145195,
60.5015918769625));
#210267=CARTESIAN_POINT('Ctrl Pts',(-64.2578760911682,-76.8758887344474,
62.3387002640362));
#210268=CARTESIAN_POINT('Ctrl Pts',(-64.1514198954027,-74.7088861304908,
65.1455341350097));
#210269=CARTESIAN_POINT('Ctrl Pts',(-64.0449636996371,-73.6992218540112,
68.5447688083423));
#210270=CARTESIAN_POINT('Ctrl Pts',(-63.9385075038716,-73.9826262366747,
72.0794398886478));
#210271=CARTESIAN_POINT('Ctrl Pts',(-63.832051308106,-75.5210008948488,
75.2743766800647));
#210272=CARTESIAN_POINT('Ctrl Pts',(-63.7255951123405,-78.1075399573813,
77.7000794635042));
#210273=CARTESIAN_POINT('Ctrl Pts',(-63.619138916575,-81.3945313113022,
79.0304570430103));
#210274=CARTESIAN_POINT('Ctrl Pts',(-63.5126827208099,-84.9401002515923,
79.086667043439));
#210275=CARTESIAN_POINT('Ctrl Pts',(-63.4062265250439,-88.2676103857406,
77.8611450431156));
#210276=CARTESIAN_POINT('Ctrl Pts',(-63.2997703292789,-90.9297420388772,
75.5186696642778));
#210277=CARTESIAN_POINT('Ctrl Pts',(-63.1933141335129,-92.5686129734675,
72.3740312719635));
#210278=CARTESIAN_POINT('Ctrl Pts',(-63.1223433363359,-92.8321628994063,
70.0249341490751));
#210279=CARTESIAN_POINT('Ctrl Pts',(-63.0868579377479,-92.7478039371384,
68.8659060795531));
#210280=CARTESIAN_POINT('Ctrl Pts',(-64.5660289597201,-91.4197528637094,
65.5776025901771));
#210281=CARTESIAN_POINT('Ctrl Pts',(-64.5305435611316,-90.9312238154461,
64.5818071779478));
#210282=CARTESIAN_POINT('Ctrl Pts',(-64.4595727639545,-89.5829795085174,
62.7727639736644));
#210283=CARTESIAN_POINT('Ctrl Pts',(-64.3531165681889,-86.7182671183082,
60.9702914393278));
#210284=CARTESIAN_POINT('Ctrl Pts',(-64.2466603724233,-83.3964921100534,
60.3215788500321));
#210285=CARTESIAN_POINT('Ctrl Pts',(-64.1402041766578,-80.0641581991723,
60.9137374199029));
#210286=CARTESIAN_POINT('Ctrl Pts',(-64.0337479808922,-77.1692483461807,
62.6671881990701));
#210287=CARTESIAN_POINT('Ctrl Pts',(-63.9272917851266,-75.1009259591622,
65.3462054376189));
#210288=CARTESIAN_POINT('Ctrl Pts',(-63.8208355893611,-74.1372394261586,
68.5906469351742));
#210289=CARTESIAN_POINT('Ctrl Pts',(-63.7143793935955,-74.4077382378226,
71.9643573833285));
#210290=CARTESIAN_POINT('Ctrl Pts',(-63.60792319783,-75.8760589215704,75.0138042454286));
#210291=CARTESIAN_POINT('Ctrl Pts',(-63.5014670020649,-78.3448130606606,
77.3290462124125));
#210292=CARTESIAN_POINT('Ctrl Pts',(-63.3950108062989,-81.4821225363578,
78.5988415166983));
#210293=CARTESIAN_POINT('Ctrl Pts',(-63.2885546105339,-84.8662345815091,
78.6524918455205));
#210294=CARTESIAN_POINT('Ctrl Pts',(-63.1820984147679,-88.0422177072,77.4827772432284));
#210295=CARTESIAN_POINT('Ctrl Pts',(-63.0756422190029,-90.5831221275879,
75.2469727000079));
#210296=CARTESIAN_POINT('Ctrl Pts',(-62.9691860232369,-92.1473627229813,
72.2455337658675));
#210297=CARTESIAN_POINT('Ctrl Pts',(-62.8982152260599,-92.3989112033227,
70.0034090172943));
#210298=CARTESIAN_POINT('Ctrl Pts',(-62.8627298274719,-92.3183937503701,
68.8971603681249));
#210299=CARTESIAN_POINT('Ctrl Pts',(-64.5675364832709,-89.3666802039723,
62.5540045030464));
#210300=CARTESIAN_POINT('Ctrl Pts',(-64.5675364832709,-89.6837232097609,
62.8628731621223));
#210301=CARTESIAN_POINT('Ctrl Pts',(-64.5675364832687,-89.9771780606084,
63.1936835736481));
#210302=CARTESIAN_POINT('Ctrl Pts',(-64.5675364832687,-90.5061924891354,
63.8842115791694));
#210303=CARTESIAN_POINT('Ctrl Pts',(-64.5675364832709,-90.7431890489746,
64.2429885299648));
#210304=CARTESIAN_POINT('Ctrl Pts',(-64.5675364832709,-90.9537820568252,
64.6166308207592));
#210305=CARTESIAN_POINT('Ctrl Pts',(-63.5337949169409,-93.5594912036319,
69.9703303450313));
#210306=CARTESIAN_POINT('Ctrl Pts',(-63.5394868426676,-93.551300696559,
70.1709662592206));
#210307=CARTESIAN_POINT('Ctrl Pts',(-63.5451666556007,-93.5372160945861,
70.3713185694425));
#210308=CARTESIAN_POINT('Ctrl Pts',(-63.5564167240733,-93.4975597846317,
70.7682868434331));
#210309=CARTESIAN_POINT('Ctrl Pts',(-63.561985078531,-93.4721513323048,
70.9648330212324));
#210310=CARTESIAN_POINT('Ctrl Pts',(-63.5675399484426,-93.4410622313485,
71.1605188170969));
#210311=CARTESIAN_POINT('Origin',(-49.5265537491909,-84.0265789317952,61.9560808081071));
#210312=CARTESIAN_POINT('',(-47.1840596451126,-83.4464714330094,62.1957559421789));
#210313=CARTESIAN_POINT('',(-39.7523422906826,-81.6060420553333,62.9561411445197));
#210314=CARTESIAN_POINT('',(-47.1840596451109,-83.4464714330093,62.1957559421787));
#210315=CARTESIAN_POINT('',(-47.119731784661,-80.7405384334922,63.3137295174306));
#210316=CARTESIAN_POINT('Origin',(-113.778845940191,-80.7405384334922,63.3137295174306));
#210317=CARTESIAN_POINT('Origin',(-113.778845940191,-80.7405384334922,63.3137295174306));
#210318=CARTESIAN_POINT('Origin',(27.1782499005891,-72.4225170988655,66.75037338561));
#210319=CARTESIAN_POINT('Origin',(27.1782499005891,-75.,72.98888938658));
#210320=CARTESIAN_POINT('Origin',(27.1782499005891,-75.,72.98888938658));
#210321=CARTESIAN_POINT('',(-39.7523422906826,-86.7610078576023,75.4331731464598));
#210322=CARTESIAN_POINT('Origin',(27.1782499005891,-77.5774829011345,79.2274053875501));
#210323=CARTESIAN_POINT('Ctrl Pts',(-39.7523422906848,-81.6060420553332,
62.9561411445199));
#210324=CARTESIAN_POINT('Ctrl Pts',(-39.7281387736131,-82.5738094980375,
63.4318987914185));
#210325=CARTESIAN_POINT('Ctrl Pts',(-39.7067753132048,-83.5053294334335,
64.0835294670284));
#210326=CARTESIAN_POINT('Ctrl Pts',(-39.6724659131911,-85.2832094673282,
65.8377960430231));
#210327=CARTESIAN_POINT('Ctrl Pts',(-39.6628533608352,-86.0573358731186,
67.0147663024293));
#210328=CARTESIAN_POINT('Ctrl Pts',(-39.6628533608352,-87.0495295570505,
69.4162628052949));
#210329=CARTESIAN_POINT('Ctrl Pts',(-39.6724659131911,-87.3318920083316,
70.7964084967982));
#210330=CARTESIAN_POINT('Ctrl Pts',(-39.7067753132048,-87.3106857783487,
73.2939791024836));
#210331=CARTESIAN_POINT('Ctrl Pts',(-39.7281387736131,-87.1107535098341,
74.4130765135442));
#210332=CARTESIAN_POINT('Ctrl Pts',(-39.7523422906848,-86.7610078576022,
75.4331731464597));
#210333=CARTESIAN_POINT('Origin',(-23.4378585958609,-75.,72.98888938658));
#210334=CARTESIAN_POINT('Ctrl Pts',(-23.3090332587941,-63.2240228732978,
77.8543002128611));
#210335=CARTESIAN_POINT('Ctrl Pts',(-23.3534781005806,-62.83121418956,77.0199591890652));
#210336=CARTESIAN_POINT('Ctrl Pts',(-23.3969857639789,-62.5315314215813,
76.148166123812));
#210337=CARTESIAN_POINT('Ctrl Pts',(-23.4821035727885,-62.1231202708912,
74.3427299956358));
#210338=CARTESIAN_POINT('Ctrl Pts',(-23.5241358609361,-62.0176287394905,
73.4125249276314));
#210339=CARTESIAN_POINT('Ctrl Pts',(-23.5675316904176,-62.0095472178182,
72.4907563613072));
#210340=CARTESIAN_POINT('Ctrl Pts',(-38.3758095864366,-79.7336577641993,
83.8196273194874));
#210341=CARTESIAN_POINT('Ctrl Pts',(-38.4258466097666,-77.8912456464383,
84.7194504420196));
#210342=CARTESIAN_POINT('Ctrl Pts',(-38.525920656419,-73.6862797614722,
85.5568522331397));
#210343=CARTESIAN_POINT('Ctrl Pts',(-38.6760317264166,-67.4554874534197,
83.4636401838067));
#210344=CARTESIAN_POINT('Ctrl Pts',(-38.826142796409,-63.0004712968532,
78.4421077647582));
#210345=CARTESIAN_POINT('Ctrl Pts',(-38.9262168430666,-62.0709193802797,
73.9710084799022));
#210346=CARTESIAN_POINT('Ctrl Pts',(-38.9762538663893,-62.2003708352002,
71.7442636422223));
#210347=CARTESIAN_POINT('Ctrl Pts',(-38.4975359461084,-79.7336577641993,
83.8196273194874));
#210348=CARTESIAN_POINT('Ctrl Pts',(-38.5475729694384,-77.8912456464383,
84.7194504420196));
#210349=CARTESIAN_POINT('Ctrl Pts',(-38.647647016096,-73.6862797614722,
85.5568522331397));
#210350=CARTESIAN_POINT('Ctrl Pts',(-38.7977580860884,-67.4554874534197,
83.4636401838067));
#210351=CARTESIAN_POINT('Ctrl Pts',(-38.947869156086,-63.0004712968532,
78.4421077647582));
#210352=CARTESIAN_POINT('Ctrl Pts',(-39.0479432027384,-62.0709193802797,
73.9710084799022));
#210353=CARTESIAN_POINT('Ctrl Pts',(-39.0979802260676,-62.2003708352002,
71.7442636422223));
#210354=CARTESIAN_POINT('Ctrl Pts',(-38.6192623057863,-79.7336577641993,
83.8196273194874));
#210355=CARTESIAN_POINT('Ctrl Pts',(-38.6692993291154,-77.8912456464383,
84.7194504420196));
#210356=CARTESIAN_POINT('Ctrl Pts',(-38.7693733757677,-73.6862797614722,
85.5568522331397));
#210357=CARTESIAN_POINT('Ctrl Pts',(-38.9194844457654,-67.4554874534197,
83.4636401838067));
#210358=CARTESIAN_POINT('Ctrl Pts',(-39.0695955157577,-63.0004712968532,
78.4421077647582));
#210359=CARTESIAN_POINT('Ctrl Pts',(-39.1696695624154,-62.0709193802797,
73.9710084799022));
#210360=CARTESIAN_POINT('Ctrl Pts',(-39.2197065857454,-62.2003708352002,
71.7442636422223));
#210361=CARTESIAN_POINT('Ctrl Pts',(-38.7409886654647,-79.7336577641993,
83.8196273194874));
#210362=CARTESIAN_POINT('Ctrl Pts',(-38.7910256887871,-77.8912456464383,
84.7194504420196));
#210363=CARTESIAN_POINT('Ctrl Pts',(-38.8910997354449,-73.6862797614722,
85.5568522331397));
#210364=CARTESIAN_POINT('Ctrl Pts',(-39.0412108054371,-67.4554874534197,
83.4636401838067));
#210365=CARTESIAN_POINT('Ctrl Pts',(-39.1913218754349,-63.0004712968532,
78.4421077647582));
#210366=CARTESIAN_POINT('Ctrl Pts',(-39.2913959220871,-62.0709193802797,
73.9710084799022));
#210367=CARTESIAN_POINT('Ctrl Pts',(-39.341432945417,-62.2003708352002,
71.7442636422223));
#210368=CARTESIAN_POINT('',(-38.9948861699879,-62.1810067989059,72.2582005417311));
#210369=CARTESIAN_POINT('Ctrl Pts',(-38.4175364832709,-79.3040007179705,
84.018699824741));
#210370=CARTESIAN_POINT('Ctrl Pts',(-38.4515840088404,-78.0242319180911,
84.580297006929));
#210371=CARTESIAN_POINT('Ctrl Pts',(-38.4856315344087,-76.6337365057753,
84.9164019235577));
#210372=CARTESIAN_POINT('Ctrl Pts',(-38.5196790599775,-75.2185063065921,
85.0027014193313));
#210373=CARTESIAN_POINT('Ctrl Pts',(-38.5318196218509,-74.7138678780693,
85.0334738279151));
#210374=CARTESIAN_POINT('Ctrl Pts',(-38.5439601837242,-74.2060847177368,
85.0324846379198));
#210375=CARTESIAN_POINT('Ctrl Pts',(-38.5561007455978,-73.6990558480383,
84.9986331104708));
#210376=CARTESIAN_POINT('Ctrl Pts',(-38.6061377689272,-71.6093489921214,
84.859114883362));
#210377=CARTESIAN_POINT('Ctrl Pts',(-38.6561747922594,-69.5324182227705,
84.1613775335844));
#210378=CARTESIAN_POINT('Ctrl Pts',(-38.7062118155911,-67.7514501453341,
82.9755867888541));
#210379=CARTESIAN_POINT('Ctrl Pts',(-38.7562488389227,-65.9704820678976,
81.7897960441239));
#210380=CARTESIAN_POINT('Ctrl Pts',(-38.8062858622539,-64.4854766823754,
80.115951904441));
#210381=CARTESIAN_POINT('Ctrl Pts',(-38.8563228855836,-63.5105860104709,
78.1612550133856));
#210382=CARTESIAN_POINT('Ctrl Pts',(-38.8900113257437,-62.8542211054953,
76.8452157116171));
#210383=CARTESIAN_POINT('Ctrl Pts',(-38.9236997659031,-62.4290840399959,
75.4018511432914));
#210384=CARTESIAN_POINT('Ctrl Pts',(-38.9573884811954,-62.2608540356083,
73.919597891675));
#210385=CARTESIAN_POINT('Ctrl Pts',(-38.9698878032445,-62.1984366657286,
73.3696463547994));
#210386=CARTESIAN_POINT('Ctrl Pts',(-38.9823871631681,-62.1713843280277,
72.8143415959309));
#210387=CARTESIAN_POINT('Ctrl Pts',(-38.9948865750186,-62.1810067178394,
72.2582005494316));
#210388=CARTESIAN_POINT('',(-39.2948856689521,-62.1810067177622,72.2582005309434));
#210389=CARTESIAN_POINT('',(-38.9948867524609,-62.1810067181578,72.2582005310305));
#210390=CARTESIAN_POINT('Ctrl Pts',(-38.7175257490599,-79.3043967631952,
84.0185260206292));
#210391=CARTESIAN_POINT('Ctrl Pts',(-38.7475365958835,-78.1763594241,84.5135891741795));
#210392=CARTESIAN_POINT('Ctrl Pts',(-38.7773577336901,-76.9698200260516,
84.8302771319025));
#210393=CARTESIAN_POINT('Ctrl Pts',(-38.8371612694423,-74.4971301206813,
85.0901078006421));
#210394=CARTESIAN_POINT('Ctrl Pts',(-38.8666805284219,-73.2491623894031,
85.0253215589554));
#210395=CARTESIAN_POINT('Ctrl Pts',(-38.9333423802022,-70.5016684508897,
84.4457335806271));
#210396=CARTESIAN_POINT('Ctrl Pts',(-38.9699089016275,-69.0435745979185,
83.8358955289173));
#210397=CARTESIAN_POINT('Ctrl Pts',(-39.0430464798089,-66.4403850004115,
82.1026671558932));
#210398=CARTESIAN_POINT('Ctrl Pts',(-39.0796009224146,-65.3002030898782,
80.9726262266062));
#210399=CARTESIAN_POINT('Ctrl Pts',(-39.1461000544407,-63.6601136043194,
78.5958132558447));
#210400=CARTESIAN_POINT('Ctrl Pts',(-39.1756663161435,-63.0966943303126,
77.4163792493374));
#210401=CARTESIAN_POINT('Ctrl Pts',(-39.2353970967561,-62.3417992295227,
74.9007486757214));
#210402=CARTESIAN_POINT('Ctrl Pts',(-39.2652280895187,-62.1581747903836,
73.5778073419933));
#210403=CARTESIAN_POINT('Ctrl Pts',(-39.2948856682995,-62.1810067181595,
72.2582005309356));
#210404=CARTESIAN_POINT('Ctrl Pts',(-22.1107451997509,-75.5739040289331,
84.8149721769878));
#210405=CARTESIAN_POINT('Ctrl Pts',(-22.1554803513709,-73.7414528439281,
84.9038985896114));
#210406=CARTESIAN_POINT('Ctrl Pts',(-22.2449506545909,-70.0361529743874,
84.2144079552725));
#210407=CARTESIAN_POINT('Ctrl Pts',(-22.3791561094309,-65.5303320257027,
80.7979303917428));
#210408=CARTESIAN_POINT('Ctrl Pts',(-22.5133615642709,-63.034536682417,
75.7241832750653));
#210409=CARTESIAN_POINT('Ctrl Pts',(-22.6475670191109,-63.0779852322991,
70.0699504067063));
#210410=CARTESIAN_POINT('Ctrl Pts',(-22.7817724739509,-65.6515761891153,
65.0351802123127));
#210411=CARTESIAN_POINT('Ctrl Pts',(-22.9159779287909,-70.2091042452636,
61.6883646725776));
#210412=CARTESIAN_POINT('Ctrl Pts',(-23.0501833836309,-75.7833689502356,
60.7397722098011));
#210413=CARTESIAN_POINT('Ctrl Pts',(-23.1843888384709,-81.1913848225435,
62.3907153943343));
#210414=CARTESIAN_POINT('Ctrl Pts',(-23.3185942933109,-85.2854509968364,
66.2908272630258));
#210415=CARTESIAN_POINT('Ctrl Pts',(-23.4527997481509,-87.1967152341949,
71.6124171753859));
#210416=CARTESIAN_POINT('Ctrl Pts',(-23.5870052029909,-86.5195647170419,
77.2261251637649));
#210417=CARTESIAN_POINT('Ctrl Pts',(-23.7212106578309,-83.3977058628873,
81.9405972979454));
#210418=CARTESIAN_POINT('Ctrl Pts',(-23.8554161126709,-78.4936666911383,
84.7553175337842));
#210419=CARTESIAN_POINT('Ctrl Pts',(-23.9896215675109,-72.8481935946092,
85.0729395141451));
#210420=CARTESIAN_POINT('Ctrl Pts',(-24.1238270223509,-67.6593817681323,
82.8260567769256));
#210421=CARTESIAN_POINT('Ctrl Pts',(-24.2580324771909,-64.0284127084992,
78.4915079084072));
#210422=CARTESIAN_POINT('Ctrl Pts',(-24.3922379320309,-62.7258589625622,
72.9891807694126));
#210423=CARTESIAN_POINT('Ctrl Pts',(-24.5264433868709,-64.0281514612617,
67.4867917924942));
#210424=CARTESIAN_POINT('Ctrl Pts',(-24.6606488417109,-67.6589147161704,
63.1520705335424));
#210425=CARTESIAN_POINT('Ctrl Pts',(-24.7948542965509,-72.8476198566583,
60.9049414386412));
#210426=CARTESIAN_POINT('Ctrl Pts',(-24.9290597513909,-78.4931080275489,
61.2222953760157));
#210427=CARTESIAN_POINT('Ctrl Pts',(-25.0632652062309,-83.3972808331134,
64.0367827707003));
#210428=CARTESIAN_POINT('Ctrl Pts',(-25.1974706610709,-86.5193635271416,
68.7511066704761));
#210429=CARTESIAN_POINT('Ctrl Pts',(-25.3316761159109,-87.1967805614843,
74.3647825240851));
#210430=CARTESIAN_POINT('Ctrl Pts',(-25.4658815707509,-85.2857690508221,
79.6864630932148));
#210431=CARTESIAN_POINT('Ctrl Pts',(-25.6000870255909,-81.1918878310654,
83.586769647843));
#210432=CARTESIAN_POINT('Ctrl Pts',(-25.7342924804309,-75.7839511863107,
85.2379684505081));
#210433=CARTESIAN_POINT('Ctrl Pts',(-25.8684979352709,-70.2096383289215,
84.2896449343191));
#210434=CARTESIAN_POINT('Ctrl Pts',(-26.0027033901109,-65.6519630192656,
80.9430297969228));
#210435=CARTESIAN_POINT('Ctrl Pts',(-26.1369088449509,-63.0780895580271,
75.9084414716367));
#210436=CARTESIAN_POINT('Ctrl Pts',(-26.2711142997909,-63.0345347478559,
70.2539879752973));
#210437=CARTESIAN_POINT('Ctrl Pts',(-26.3605846030209,-64.6978341565217,
66.8719649808208));
#210438=CARTESIAN_POINT('Ctrl Pts',(-26.4053197546309,-65.8649786513045,
65.456493688071));
#210439=CARTESIAN_POINT('Ctrl Pts',(-22.2602140739609,-75.5739040289331,
84.8149721769878));
#210440=CARTESIAN_POINT('Ctrl Pts',(-22.3049492255709,-73.7414528439281,
84.9038985896114));
#210441=CARTESIAN_POINT('Ctrl Pts',(-22.3944195288009,-70.0361529743874,
84.2144079552725));
#210442=CARTESIAN_POINT('Ctrl Pts',(-22.5286249836409,-65.5303320257027,
80.7979303917428));
#210443=CARTESIAN_POINT('Ctrl Pts',(-22.6628304384809,-63.034536682417,
75.7241832750653));
#210444=CARTESIAN_POINT('Ctrl Pts',(-22.7970358933209,-63.0779852322991,
70.0699504067063));
#210445=CARTESIAN_POINT('Ctrl Pts',(-22.9312413481609,-65.6515761891153,
65.0351802123127));
#210446=CARTESIAN_POINT('Ctrl Pts',(-23.0654468030009,-70.2091042452636,
61.6883646725776));
#210447=CARTESIAN_POINT('Ctrl Pts',(-23.1996522578409,-75.7833689502356,
60.7397722098011));
#210448=CARTESIAN_POINT('Ctrl Pts',(-23.3338577126809,-81.1913848225435,
62.3907153943343));
#210449=CARTESIAN_POINT('Ctrl Pts',(-23.4680631675209,-85.2854509968364,
66.2908272630258));
#210450=CARTESIAN_POINT('Ctrl Pts',(-23.6022686223609,-87.1967152341949,
71.6124171753859));
#210451=CARTESIAN_POINT('Ctrl Pts',(-23.7364740772009,-86.5195647170419,
77.2261251637649));
#210452=CARTESIAN_POINT('Ctrl Pts',(-23.8706795320409,-83.3977058628873,
81.9405972979454));
#210453=CARTESIAN_POINT('Ctrl Pts',(-24.0048849868809,-78.4936666911383,
84.7553175337842));
#210454=CARTESIAN_POINT('Ctrl Pts',(-24.1390904417209,-72.8481935946092,
85.0729395141451));
#210455=CARTESIAN_POINT('Ctrl Pts',(-24.2732958965609,-67.6593817681323,
82.8260567769256));
#210456=CARTESIAN_POINT('Ctrl Pts',(-24.4075013514009,-64.0284127084992,
78.4915079084072));
#210457=CARTESIAN_POINT('Ctrl Pts',(-24.5417068062409,-62.7258589625622,
72.9891807694126));
#210458=CARTESIAN_POINT('Ctrl Pts',(-24.6759122610809,-64.0281514612617,
67.4867917924942));
#210459=CARTESIAN_POINT('Ctrl Pts',(-24.8101177159209,-67.6589147161704,
63.1520705335424));
#210460=CARTESIAN_POINT('Ctrl Pts',(-24.9443231707609,-72.8476198566583,
60.9049414386412));
#210461=CARTESIAN_POINT('Ctrl Pts',(-25.0785286256009,-78.4931080275489,
61.2222953760157));
#210462=CARTESIAN_POINT('Ctrl Pts',(-25.2127340804409,-83.3972808331134,
64.0367827707003));
#210463=CARTESIAN_POINT('Ctrl Pts',(-25.3469395352809,-86.5193635271416,
68.7511066704761));
#210464=CARTESIAN_POINT('Ctrl Pts',(-25.4811449901209,-87.1967805614843,
74.3647825240851));
#210465=CARTESIAN_POINT('Ctrl Pts',(-25.6153504449609,-85.2857690508221,
79.6864630932148));
#210466=CARTESIAN_POINT('Ctrl Pts',(-25.7495558998009,-81.1918878310654,
83.586769647843));
#210467=CARTESIAN_POINT('Ctrl Pts',(-25.8837613546409,-75.7839511863107,
85.2379684505081));
#210468=CARTESIAN_POINT('Ctrl Pts',(-26.0179668094809,-70.2096383289215,
84.2896449343191));
#210469=CARTESIAN_POINT('Ctrl Pts',(-26.1521722643209,-65.6519630192656,
80.9430297969228));
#210470=CARTESIAN_POINT('Ctrl Pts',(-26.2863777191609,-63.0780895580271,
75.9084414716367));
#210471=CARTESIAN_POINT('Ctrl Pts',(-26.4205831740009,-63.0345347478559,
70.2539879752973));
#210472=CARTESIAN_POINT('Ctrl Pts',(-26.5100534772209,-64.6978341565217,
66.8719649808208));
#210473=CARTESIAN_POINT('Ctrl Pts',(-26.5547886288309,-65.8649786513045,
65.456493688071));
#210474=CARTESIAN_POINT('Ctrl Pts',(-22.4096829481609,-75.5739040289331,
84.8149721769878));
#210475=CARTESIAN_POINT('Ctrl Pts',(-22.4544180997809,-73.7414528439281,
84.9038985896114));
#210476=CARTESIAN_POINT('Ctrl Pts',(-22.5438884030009,-70.0361529743874,
84.2144079552725));
#210477=CARTESIAN_POINT('Ctrl Pts',(-22.6780938578409,-65.5303320257027,
80.7979303917428));
#210478=CARTESIAN_POINT('Ctrl Pts',(-22.8122993126809,-63.034536682417,
75.7241832750653));
#210479=CARTESIAN_POINT('Ctrl Pts',(-22.9465047675209,-63.0779852322991,
70.0699504067063));
#210480=CARTESIAN_POINT('Ctrl Pts',(-23.0807102223609,-65.6515761891153,
65.0351802123127));
#210481=CARTESIAN_POINT('Ctrl Pts',(-23.2149156772009,-70.2091042452636,
61.6883646725776));
#210482=CARTESIAN_POINT('Ctrl Pts',(-23.3491211320409,-75.7833689502356,
60.7397722098011));
#210483=CARTESIAN_POINT('Ctrl Pts',(-23.4833265868809,-81.1913848225435,
62.3907153943343));
#210484=CARTESIAN_POINT('Ctrl Pts',(-23.6175320417209,-85.2854509968364,
66.2908272630258));
#210485=CARTESIAN_POINT('Ctrl Pts',(-23.7517374965609,-87.1967152341949,
71.6124171753859));
#210486=CARTESIAN_POINT('Ctrl Pts',(-23.8859429514009,-86.5195647170419,
77.2261251637649));
#210487=CARTESIAN_POINT('Ctrl Pts',(-24.0201484062409,-83.3977058628873,
81.9405972979454));
#210488=CARTESIAN_POINT('Ctrl Pts',(-24.1543538610809,-78.4936666911383,
84.7553175337842));
#210489=CARTESIAN_POINT('Ctrl Pts',(-24.2885593159209,-72.8481935946092,
85.0729395141451));
#210490=CARTESIAN_POINT('Ctrl Pts',(-24.4227647707609,-67.6593817681323,
82.8260567769256));
#210491=CARTESIAN_POINT('Ctrl Pts',(-24.5569702256009,-64.0284127084992,
78.4915079084072));
#210492=CARTESIAN_POINT('Ctrl Pts',(-24.6911756804409,-62.7258589625622,
72.9891807694126));
#210493=CARTESIAN_POINT('Ctrl Pts',(-24.8253811352809,-64.0281514612617,
67.4867917924942));
#210494=CARTESIAN_POINT('Ctrl Pts',(-24.9595865901209,-67.6589147161704,
63.1520705335424));
#210495=CARTESIAN_POINT('Ctrl Pts',(-25.0937920449609,-72.8476198566583,
60.9049414386412));
#210496=CARTESIAN_POINT('Ctrl Pts',(-25.2279974998009,-78.4931080275489,
61.2222953760157));
#210497=CARTESIAN_POINT('Ctrl Pts',(-25.3622029546409,-83.3972808331134,
64.0367827707003));
#210498=CARTESIAN_POINT('Ctrl Pts',(-25.4964084094809,-86.5193635271416,
68.7511066704761));
#210499=CARTESIAN_POINT('Ctrl Pts',(-25.6306138643209,-87.1967805614843,
74.3647825240851));
#210500=CARTESIAN_POINT('Ctrl Pts',(-25.7648193191609,-85.2857690508221,
79.6864630932148));
#210501=CARTESIAN_POINT('Ctrl Pts',(-25.8990247740009,-81.1918878310654,
83.586769647843));
#210502=CARTESIAN_POINT('Ctrl Pts',(-26.0332302288409,-75.7839511863107,
85.2379684505081));
#210503=CARTESIAN_POINT('Ctrl Pts',(-26.1674356836809,-70.2096383289215,
84.2896449343191));
#210504=CARTESIAN_POINT('Ctrl Pts',(-26.3016411385209,-65.6519630192656,
80.9430297969228));
#210505=CARTESIAN_POINT('Ctrl Pts',(-26.4358465933609,-63.0780895580271,
75.9084414716367));
#210506=CARTESIAN_POINT('Ctrl Pts',(-26.5700520482009,-63.0345347478559,
70.2539879752973));
#210507=CARTESIAN_POINT('Ctrl Pts',(-26.6595223514309,-64.6978341565217,
66.8719649808208));
#210508=CARTESIAN_POINT('Ctrl Pts',(-26.7042575030409,-65.8649786513045,
65.456493688071));
#210509=CARTESIAN_POINT('Ctrl Pts',(-22.5591518223709,-75.5739040289331,
84.8149721769878));
#210510=CARTESIAN_POINT('Ctrl Pts',(-22.6038869739809,-73.7414528439281,
84.9038985896114));
#210511=CARTESIAN_POINT('Ctrl Pts',(-22.6933572772109,-70.0361529743874,
84.2144079552725));
#210512=CARTESIAN_POINT('Ctrl Pts',(-22.8275627320509,-65.5303320257027,
80.7979303917428));
#210513=CARTESIAN_POINT('Ctrl Pts',(-22.9617681868909,-63.034536682417,
75.7241832750653));
#210514=CARTESIAN_POINT('Ctrl Pts',(-23.0959736417309,-63.0779852322991,
70.0699504067063));
#210515=CARTESIAN_POINT('Ctrl Pts',(-23.2301790965709,-65.6515761891153,
65.0351802123127));
#210516=CARTESIAN_POINT('Ctrl Pts',(-23.3643845514109,-70.2091042452636,
61.6883646725776));
#210517=CARTESIAN_POINT('Ctrl Pts',(-23.4985900062509,-75.7833689502356,
60.7397722098011));
#210518=CARTESIAN_POINT('Ctrl Pts',(-23.6327954610909,-81.1913848225435,
62.3907153943343));
#210519=CARTESIAN_POINT('Ctrl Pts',(-23.7670009159309,-85.2854509968364,
66.2908272630258));
#210520=CARTESIAN_POINT('Ctrl Pts',(-23.9012063707709,-87.1967152341949,
71.6124171753859));
#210521=CARTESIAN_POINT('Ctrl Pts',(-24.0354118256109,-86.5195647170419,
77.2261251637649));
#210522=CARTESIAN_POINT('Ctrl Pts',(-24.1696172804509,-83.3977058628873,
81.9405972979454));
#210523=CARTESIAN_POINT('Ctrl Pts',(-24.3038227352909,-78.4936666911383,
84.7553175337842));
#210524=CARTESIAN_POINT('Ctrl Pts',(-24.4380281901309,-72.8481935946092,
85.0729395141451));
#210525=CARTESIAN_POINT('Ctrl Pts',(-24.5722336449709,-67.6593817681323,
82.8260567769256));
#210526=CARTESIAN_POINT('Ctrl Pts',(-24.7064390998109,-64.0284127084992,
78.4915079084072));
#210527=CARTESIAN_POINT('Ctrl Pts',(-24.8406445546509,-62.7258589625622,
72.9891807694126));
#210528=CARTESIAN_POINT('Ctrl Pts',(-24.9748500094909,-64.0281514612617,
67.4867917924942));
#210529=CARTESIAN_POINT('Ctrl Pts',(-25.1090554643309,-67.6589147161704,
63.1520705335424));
#210530=CARTESIAN_POINT('Ctrl Pts',(-25.2432609191709,-72.8476198566583,
60.9049414386412));
#210531=CARTESIAN_POINT('Ctrl Pts',(-25.3774663740109,-78.4931080275489,
61.2222953760157));
#210532=CARTESIAN_POINT('Ctrl Pts',(-25.5116718288509,-83.3972808331134,
64.0367827707003));
#210533=CARTESIAN_POINT('Ctrl Pts',(-25.6458772836909,-86.5193635271416,
68.7511066704761));
#210534=CARTESIAN_POINT('Ctrl Pts',(-25.7800827385309,-87.1967805614843,
74.3647825240851));
#210535=CARTESIAN_POINT('Ctrl Pts',(-25.9142881933709,-85.2857690508221,
79.6864630932148));
#210536=CARTESIAN_POINT('Ctrl Pts',(-26.0484936482109,-81.1918878310654,
83.586769647843));
#210537=CARTESIAN_POINT('Ctrl Pts',(-26.1826991030509,-75.7839511863107,
85.2379684505081));
#210538=CARTESIAN_POINT('Ctrl Pts',(-26.3169045578909,-70.2096383289215,
84.2896449343191));
#210539=CARTESIAN_POINT('Ctrl Pts',(-26.4511100127309,-65.6519630192656,
80.9430297969228));
#210540=CARTESIAN_POINT('Ctrl Pts',(-26.5853154675709,-63.0780895580271,
75.9084414716367));
#210541=CARTESIAN_POINT('Ctrl Pts',(-26.7195209224109,-63.0345347478559,
70.2539879752973));
#210542=CARTESIAN_POINT('Ctrl Pts',(-26.8089912256309,-64.6978341565217,
66.8719649808208));
#210543=CARTESIAN_POINT('Ctrl Pts',(-26.8537263772509,-65.8649786513045,
65.456493688071));
#210544=CARTESIAN_POINT('',(-22.5675364832709,-72.2044512501012,84.4927878836045));
#210545=CARTESIAN_POINT('Ctrl Pts',(-22.5675364832709,-72.2044512501012,
84.4927878836045));
#210546=CARTESIAN_POINT('Ctrl Pts',(-22.5702005749792,-72.101381045307,
84.467793838185));
#210547=CARTESIAN_POINT('Ctrl Pts',(-22.5728694662329,-71.9986439061689,
84.4414253512639));
#210548=CARTESIAN_POINT('Ctrl Pts',(-22.5892107893379,-71.3720639244154,
84.2716538950522));
#210549=CARTESIAN_POINT('Ctrl Pts',(-22.6029000964172,-70.857571028858,
84.0937531121258));
#210550=CARTESIAN_POINT('Ctrl Pts',(-22.6289955618953,-69.8696262372289,
83.6729279463958));
#210551=CARTESIAN_POINT('Ctrl Pts',(-22.6413046609066,-69.3967095048034,
83.4319232204433));
#210552=CARTESIAN_POINT('Ctrl Pts',(-22.6599801160594,-68.7147555205797,
83.0250434553367));
#210553=CARTESIAN_POINT('Ctrl Pts',(-22.6662554004773,-68.4915974755653,
82.8815572226386));
#210554=CARTESIAN_POINT('Ctrl Pts',(-22.6893343517786,-67.7056195601597,
82.3383815790085));
#210555=CARTESIAN_POINT('Ctrl Pts',(-22.7069178421115,-67.1716946281647,
81.8966499936456));
#210556=CARTESIAN_POINT('Ctrl Pts',(-22.7321799276305,-66.4561223902797,
81.191081357374));
#210557=CARTESIAN_POINT('Ctrl Pts',(-22.7400417610185,-66.2408487732195,
80.9612051372088));
#210558=CARTESIAN_POINT('Ctrl Pts',(-22.7616713767574,-65.6637270733977,
80.2927579163368));
#210559=CARTESIAN_POINT('Ctrl Pts',(-22.7748837672742,-65.3251316974417,
79.8367065697317));
#210560=CARTESIAN_POINT('Ctrl Pts',(-22.7947609375481,-64.8709906011954,
79.1240614124061));
#210561=CARTESIAN_POINT('Ctrl Pts',(-22.801362841351,-64.7292600705043,
78.8833334005035));
#210562=CARTESIAN_POINT('Ctrl Pts',(-22.8237826878125,-64.2863646376341,
78.066924839321));
#210563=CARTESIAN_POINT('Ctrl Pts',(-22.8402920915749,-64.0231454411833,
77.4705540397267));
#210564=CARTESIAN_POINT('Ctrl Pts',(-22.8648029152467,-63.7043957916297,
76.5509224533803));
#210565=CARTESIAN_POINT('Ctrl Pts',(-22.8729157189747,-63.6109150950584,
76.2407322943046));
#210566=CARTESIAN_POINT('Ctrl Pts',(-22.8959687353885,-63.3777242540699,
75.3320075975269));
#210567=CARTESIAN_POINT('Ctrl Pts',(-22.9102264149049,-63.272832382873,
74.7270547946618));
#210568=CARTESIAN_POINT('Ctrl Pts',(-22.9311662489802,-63.1886126135983,
73.8409316995098));
#210569=CARTESIAN_POINT('Ctrl Pts',(-22.9377614229422,-63.172002102898,
73.5625527585218));
#210570=CARTESIAN_POINT('Ctrl Pts',(-22.9606740564853,-63.1486501868713,
72.6142548128651));
#210571=CARTESIAN_POINT('Ctrl Pts',(-22.9777573547508,-63.1884849523521,
71.9430921224707));
#210572=CARTESIAN_POINT('Ctrl Pts',(-23.0022394040367,-63.3280072789211,
70.9807639026107));
#210573=CARTESIAN_POINT('Ctrl Pts',(-23.009809992206,-63.3828970341615,
70.6830316322857));
#210574=CARTESIAN_POINT('Ctrl Pts',(-23.0313765416433,-63.575741394923,
69.8254004003008));
#210575=CARTESIAN_POINT('Ctrl Pts',(-23.0447944938312,-63.7437455267563,
69.2740313357485));
#210576=CARTESIAN_POINT('Ctrl Pts',(-23.0652537324288,-64.0568737760211,
68.461953897769));
#210577=CARTESIAN_POINT('Ctrl Pts',(-23.072249157524,-64.1737923279692,
68.1895288572785));
#210578=CARTESIAN_POINT('Ctrl Pts',(-23.0965474361077,-64.6054951171437,
67.2786381453301));
#210579=CARTESIAN_POINT('Ctrl Pts',(-23.1147579084745,-64.967843830616,
66.6626023540414));
#210580=CARTESIAN_POINT('Ctrl Pts',(-23.1397715132475,-65.5471606574156,
65.8542689053473));
#210581=CARTESIAN_POINT('Ctrl Pts',(-23.1468311929961,-65.7201277877051,
65.6303568070702));
#210582=CARTESIAN_POINT('Ctrl Pts',(-23.1676747514321,-66.2648908086861,
64.9758232123873));
#210583=CARTESIAN_POINT('Ctrl Pts',(-23.180917910398,-66.6602300549298,
64.5661869645247));
#210584=CARTESIAN_POINT('Ctrl Pts',(-23.2013065948263,-67.3052464719053,
63.98684644309));
#210585=CARTESIAN_POINT('Ctrl Pts',(-23.2083909984657,-67.5358879433693,
63.7949330533718));
#210586=CARTESIAN_POINT('Ctrl Pts',(-23.2324629811764,-68.3265224511962,
63.1858849928527));
#210587=CARTESIAN_POINT('Ctrl Pts',(-23.2503290955488,-68.9170420587356,
62.8082314172963));
#210588=CARTESIAN_POINT('Ctrl Pts',(-23.2748842311724,-69.7822021340986,
62.3572729968318));
#210589=CARTESIAN_POINT('Ctrl Pts',(-23.2818169730817,-70.0327823351848,
62.2376943943266));
#210590=CARTESIAN_POINT('Ctrl Pts',(-23.3035186130697,-70.8455154209485,
61.8849216123275));
#210591=CARTESIAN_POINT('Ctrl Pts',(-23.3176588018285,-71.4219044077756,
61.6868980638871));
#210592=CARTESIAN_POINT('Ctrl Pts',(-23.3388664824507,-72.2933800065435,
61.4600378227875));
#210593=CARTESIAN_POINT('Ctrl Pts',(-23.3458199835052,-72.5801380471361,
61.3966045554723));
#210594=CARTESIAN_POINT('Ctrl Pts',(-23.3682626536341,-73.4930114596429,
61.2296514049232));
#210595=CARTESIAN_POINT('Ctrl Pts',(-23.3844526926435,-74.1263361552216,
61.1651917382816));
#210596=CARTESIAN_POINT('Ctrl Pts',(-23.407684371625,-75.0471740386811,
61.1458073048583));
#210597=CARTESIAN_POINT('Ctrl Pts',(-23.4148695247781,-75.3338716005414,
61.1502002309391));
#210598=CARTESIAN_POINT('Ctrl Pts',(-23.437206134341,-76.2411868293319,
61.1975982391152));
#210599=CARTESIAN_POINT('Ctrl Pts',(-23.4516854993175,-76.8584841699238,
61.2799207344907));
#210600=CARTESIAN_POINT('Ctrl Pts',(-23.4735337262852,-77.7658938973876,
61.4737526344256));
#210601=CARTESIAN_POINT('Ctrl Pts',(-23.4808192690104,-78.0644314250129,
61.5497313157693));
#210602=CARTESIAN_POINT('Ctrl Pts',(-23.5040385331769,-78.985976686343,
61.8225462972605));
#210603=CARTESIAN_POINT('Ctrl Pts',(-23.5207281916305,-79.5972182308479,
62.0593503041271));
#210604=CARTESIAN_POINT('Ctrl Pts',(-23.5441129061001,-80.4314026015402,
62.4648501692533));
#210605=CARTESIAN_POINT('Ctrl Pts',(-23.5509830628018,-80.673910896464,
62.5933714538943));
#210606=CARTESIAN_POINT('Ctrl Pts',(-23.5725188546082,-81.4338200893154,
63.0311669320082));
#210607=CARTESIAN_POINT('Ctrl Pts',(-23.5865887278414,-81.9320304656956,
63.3723514817783));
#210608=CARTESIAN_POINT('Ctrl Pts',(-23.6083405871127,-82.6525232096769,
63.9503037294639));
#210609=CARTESIAN_POINT('Ctrl Pts',(-23.6159578353334,-82.895558722176,
64.1620087200743));
#210610=CARTESIAN_POINT('Ctrl Pts',(-23.6398805770154,-83.6157764881116,
64.8424376056804));
#210611=CARTESIAN_POINT('Ctrl Pts',(-23.6569839558427,-84.0633982830332,
65.3425405823492));
#210612=CARTESIAN_POINT('Ctrl Pts',(-23.6804648193501,-84.6237728802768,
66.0871527080787));
#210613=CARTESIAN_POINT('Ctrl Pts',(-23.6870485851375,-84.7749847799005,
66.3027475337673));
#210614=CARTESIAN_POINT('Ctrl Pts',(-23.7082031998033,-85.2460366915907,
67.025357154534));
#210615=CARTESIAN_POINT('Ctrl Pts',(-23.7222219941297,-85.5344434917129,
67.5526944759278));
#210616=CARTESIAN_POINT('Ctrl Pts',(-23.7441210530633,-85.917699285489,
68.3991972044296));
#210617=CARTESIAN_POINT('Ctrl Pts',(-23.7519297485863,-86.041288304194,
68.7054045196352));
#210618=CARTESIAN_POINT('Ctrl Pts',(-23.7755298190367,-86.3691023964499,
69.6255567349058));
#210619=CARTESIAN_POINT('Ctrl Pts',(-23.7920487902638,-86.536744826011,
70.2525895074464));
#210620=CARTESIAN_POINT('Ctrl Pts',(-23.8151391213079,-86.6998527884554,
71.1537311340575));
#210621=CARTESIAN_POINT('Ctrl Pts',(-23.8218753913192,-86.7387036230601,
71.420093236262));
#210622=CARTESIAN_POINT('Ctrl Pts',(-23.8433555858714,-86.8349025507093,
72.2904016804811));
#210623=CARTESIAN_POINT('Ctrl Pts',(-23.8575579717939,-86.8543681848811,
72.8983416348768));
#210624=CARTESIAN_POINT('Ctrl Pts',(-23.8798554463617,-86.8126009199117,
73.8427727913579));
#210625=CARTESIAN_POINT('Ctrl Pts',(-23.8878816096207,-86.7831869848533,
74.1806799322738));
#210626=CARTESIAN_POINT('Ctrl Pts',(-23.9110847210234,-86.6594162642764,
75.1323771410212));
#210627=CARTESIAN_POINT('Ctrl Pts',(-23.9269053581022,-86.5313769103644,
75.7418298181749));
#210628=CARTESIAN_POINT('Ctrl Pts',(-23.9495459158712,-86.2782593381081,
76.6026846921188));
#210629=CARTESIAN_POINT('Ctrl Pts',(-23.9564812052765,-86.1908829611717,
76.8653374683523));
#210630=CARTESIAN_POINT('Ctrl Pts',(-23.978357349735,-85.87951350085,77.7003660271306));
#210631=CARTESIAN_POINT('Ctrl Pts',(-23.9927641337887,-85.6192994879538,
78.2589304827335));
#210632=CARTESIAN_POINT('Ctrl Pts',(-24.0155119050259,-85.1462650587442,
79.0984245577459));
#210633=CARTESIAN_POINT('Ctrl Pts',(-24.0237891876252,-84.9614493005972,
79.395151667052));
#210634=CARTESIAN_POINT('Ctrl Pts',(-24.0466112890863,-84.4281573134537,
80.1732424407857));
#210635=CARTESIAN_POINT('Ctrl Pts',(-24.0617134596371,-84.0557500977274,
80.6382476573784));
#210636=CARTESIAN_POINT('Ctrl Pts',(-24.0839137958733,-83.455843100956,
81.2812040167729));
#210637=CARTESIAN_POINT('Ctrl Pts',(-24.0910796733786,-83.2534875950334,
81.482882460786));
#210638=CARTESIAN_POINT('Ctrl Pts',(-24.114057595194,-82.5668987389516,
82.1183964911421));
#210639=CARTESIAN_POINT('Ctrl Pts',(-24.1292856506188,-82.0531629663279,
82.5197843027206));
#210640=CARTESIAN_POINT('Ctrl Pts',(-24.1528881185347,-81.2191982476438,
83.0682211280836));
#210641=CARTESIAN_POINT('Ctrl Pts',(-24.1611669801199,-80.9197306683576,
83.2468935918955));
#210642=CARTESIAN_POINT('Ctrl Pts',(-24.1827559596316,-80.1362205425358,
83.6690821495163));
#210643=CARTESIAN_POINT('Ctrl Pts',(-24.1964874148007,-79.6419118838925,
83.8935996769975));
#210644=CARTESIAN_POINT('Ctrl Pts',(-24.2174768257468,-78.8635400001464,
84.1843685432751));
#210645=CARTESIAN_POINT('Ctrl Pts',(-24.2247571552006,-78.5886510660862,
84.2756825250963));
#210646=CARTESIAN_POINT('Ctrl Pts',(-24.2483756982726,-77.6675515482579,
84.5438270605521));
#210647=CARTESIAN_POINT('Ctrl Pts',(-24.2640946299932,-77.0085486087368,
84.6754742522788));
#210648=CARTESIAN_POINT('Ctrl Pts',(-24.2884926428815,-75.9843843113636,
84.7918940227002));
#210649=CARTESIAN_POINT('Ctrl Pts',(-24.2970807599795,-75.6237028793401,
84.8163932788448));
#210650=CARTESIAN_POINT('Ctrl Pts',(-24.3182126869125,-74.753379085836,
84.8359863747897));
#210651=CARTESIAN_POINT('Ctrl Pts',(-24.331086847875,-74.2433492494284,
84.8148743652152));
#210652=CARTESIAN_POINT('Ctrl Pts',(-24.3515180034849,-73.4391621471866,
84.7292196212527));
#210653=CARTESIAN_POINT('Ctrl Pts',(-24.3590613604395,-73.1425132511634,
84.6861535064079));
#210654=CARTESIAN_POINT('Ctrl Pts',(-24.3815384824964,-72.2455386694007,
84.5202236828175));
#210655=CARTESIAN_POINT('Ctrl Pts',(-24.3960069964874,-71.6522821119051,
84.3613414335283));
#210656=CARTESIAN_POINT('Ctrl Pts',(-24.420087747924,-70.6927799935796,
84.0234693101138));
#210657=CARTESIAN_POINT('Ctrl Pts',(-24.4296875364308,-70.3176894943474,
83.8695157327615));
#210658=CARTESIAN_POINT('Ctrl Pts',(-24.4517726454239,-69.492170899461,
83.4806056486045));
#210659=CARTESIAN_POINT('Ctrl Pts',(-24.4645281627022,-69.0467282022266,
83.2349870119561));
#210660=CARTESIAN_POINT('Ctrl Pts',(-24.4851445577002,-68.3588257034976,
82.7956074273213));
#210661=CARTESIAN_POINT('Ctrl Pts',(-24.4929344656444,-68.1050651461329,
82.6191436156437));
#210662=CARTESIAN_POINT('Ctrl Pts',(-24.5153697889196,-67.3800154221781,
82.0707183485821));
#210663=CARTESIAN_POINT('Ctrl Pts',(-24.5295968633418,-66.9295782058471,
81.6718532422255));
#210664=CARTESIAN_POINT('Ctrl Pts',(-24.5540914658925,-66.2096628206234,
80.9304241509229));
#210665=CARTESIAN_POINT('Ctrl Pts',(-24.564365750269,-65.9246307267622,
80.6029215596546));
#210666=CARTESIAN_POINT('Ctrl Pts',(-24.5860905187512,-65.3728346095594,
79.894567924767));
#210667=CARTESIAN_POINT('Ctrl Pts',(-24.5976840511342,-65.1087963504241,
79.511541722129));
#210668=CARTESIAN_POINT('Ctrl Pts',(-24.6172620568231,-64.7068591408205,
78.8479458411513));
#210669=CARTESIAN_POINT('Ctrl Pts',(-24.6251367322929,-64.5560611690603,
78.5751882904969));
#210670=CARTESIAN_POINT('Ctrl Pts',(-24.6472317420048,-64.1564776850288,
77.778450069505));
#210671=CARTESIAN_POINT('Ctrl Pts',(-24.6610648696814,-63.9353368803934,
77.240709445703));
#210672=CARTESIAN_POINT('Ctrl Pts',(-24.6908945637497,-63.5435177201768,
76.0472767679771));
#210673=CARTESIAN_POINT('Ctrl Pts',(-24.7068825789407,-63.3872882704072,
75.3867366115899));
#210674=CARTESIAN_POINT('Ctrl Pts',(-24.7317749488675,-63.2391139871652,
74.3879117013547));
#210675=CARTESIAN_POINT('Ctrl Pts',(-24.7401923448886,-63.204033550018,
74.0559075222267));
#210676=CARTESIAN_POINT('Ctrl Pts',(-24.7610996526955,-63.1520046518361,
73.2283760432204));
#210677=CARTESIAN_POINT('Ctrl Pts',(-24.7733789330876,-63.1523239657399,
72.7345232328324));
#210678=CARTESIAN_POINT('Ctrl Pts',(-24.7975533204228,-63.2163039535267,
71.7369892425429));
#210679=CARTESIAN_POINT('Ctrl Pts',(-24.8094922231537,-63.2808630596704,
71.2360827207114));
#210680=CARTESIAN_POINT('Ctrl Pts',(-24.8351973708289,-63.4864194352961,
70.1752564221956));
#210681=CARTESIAN_POINT('Ctrl Pts',(-24.8489873208506,-63.6371013798287,
69.6171097101316));
#210682=CARTESIAN_POINT('Ctrl Pts',(-24.871569359364,-63.9377876836337,
68.7570415397288));
#210683=CARTESIAN_POINT('Ctrl Pts',(-24.8800360304053,-64.0615447344729,
68.4458729535586));
#210684=CARTESIAN_POINT('Ctrl Pts',(-24.9001649362169,-64.3887688614134,
67.7156793928846));
#210685=CARTESIAN_POINT('Ctrl Pts',(-24.9116058676399,-64.6036307349302,
67.304238822933));
#210686=CARTESIAN_POINT('Ctrl Pts',(-24.936773504184,-65.1398482256562,
66.4104777396577));
#210687=CARTESIAN_POINT('Ctrl Pts',(-24.9504401609289,-65.4735636386861,
65.9367826121286));
#210688=CARTESIAN_POINT('Ctrl Pts',(-24.9762719223671,-66.1587653668953,
65.099986780096));
#210689=CARTESIAN_POINT('Ctrl Pts',(-24.9884096401357,-66.5025277537145,
64.7304245665408));
#210690=CARTESIAN_POINT('Ctrl Pts',(-25.0096077839027,-67.1226339839138,
64.143431275759));
#210691=CARTESIAN_POINT('Ctrl Pts',(-25.0184772157891,-67.3876176298573,
63.9139452540245));
#210692=CARTESIAN_POINT('Ctrl Pts',(-25.0395422051437,-68.0467493322417,
63.3929967902548));
#210693=CARTESIAN_POINT('Ctrl Pts',(-25.051481480533,-68.4488671084499,
63.1146464292296));
#210694=CARTESIAN_POINT('Ctrl Pts',(-25.0840133009887,-69.605829643291,
62.4152363687055));
#210695=CARTESIAN_POINT('Ctrl Pts',(-25.104319479274,-70.3943111889634,
62.0491341885859));
#210696=CARTESIAN_POINT('Ctrl Pts',(-25.1367303308552,-71.6511389741192,
61.623800462803));
#210697=CARTESIAN_POINT('Ctrl Pts',(-25.1483805833471,-72.0982070991733,
61.5009928872146));
#210698=CARTESIAN_POINT('Ctrl Pts',(-25.1736387791001,-73.0833297619818,
61.2922240109905));
#210699=CARTESIAN_POINT('Ctrl Pts',(-25.18690328478,-73.6212370846174,61.2172565919412));
#210700=CARTESIAN_POINT('Ctrl Pts',(-25.2253780352521,-75.2159620477906,
61.1054031807067));
#210701=CARTESIAN_POINT('Ctrl Pts',(-25.2502026720849,-76.280546882193,
61.1724865348266));
#210702=CARTESIAN_POINT('Ctrl Pts',(-25.2868501328567,-77.724738435485,
61.4594462472879));
#210703=CARTESIAN_POINT('Ctrl Pts',(-25.2973866547898,-78.1284078048523,
61.5619808193849));
#210704=CARTESIAN_POINT('Ctrl Pts',(-25.3189006619814,-78.9588852174617,
61.8212918368161));
#210705=CARTESIAN_POINT('Ctrl Pts',(-25.3298740811697,-79.3836100045202,
61.9815962718169));
#210706=CARTESIAN_POINT('Ctrl Pts',(-25.3676607858402,-80.8209660344883,
62.620119032157));
#210707=CARTESIAN_POINT('Ctrl Pts',(-25.3942496696967,-81.7803037275957,
63.2194097958438));
#210708=CARTESIAN_POINT('Ctrl Pts',(-25.4315170012924,-82.9187865576204,
64.1789466500218));
#210709=CARTESIAN_POINT('Ctrl Pts',(-25.4407247650091,-83.1891272839219,
64.4295735366799));
#210710=CARTESIAN_POINT('Ctrl Pts',(-25.4634471275391,-83.8379068478192,
65.091061289566));
#210711=CARTESIAN_POINT('Ctrl Pts',(-25.4768210572136,-84.1994663576492,
65.5163497127943));
#210712=CARTESIAN_POINT('Ctrl Pts',(-25.5082872674835,-84.9777305813297,
66.5732280735895));
#210713=CARTESIAN_POINT('Ctrl Pts',(-25.5263741675259,-85.3681341316777,
67.2244202926804));
#210714=CARTESIAN_POINT('Ctrl Pts',(-25.5565118018322,-85.892517668506,
68.3253303899162));
#210715=CARTESIAN_POINT('Ctrl Pts',(-25.5682319358942,-86.0673700339834,
68.7558528469077));
#210716=CARTESIAN_POINT('Ctrl Pts',(-25.5936707871693,-86.3976332999429,
69.7340864108877));
#210717=CARTESIAN_POINT('Ctrl Pts',(-25.6073488507091,-86.5398957155988,
70.284393827016));
#210718=CARTESIAN_POINT('Ctrl Pts',(-25.6390902685798,-86.7786955465479,
71.5834051319908));
#210719=CARTESIAN_POINT('Ctrl Pts',(-25.6571261045347,-86.8447346260927,
72.3378995205217));
#210720=CARTESIAN_POINT('Ctrl Pts',(-25.6886429549223,-86.8346771541917,
73.6213929423741));
#210721=CARTESIAN_POINT('Ctrl Pts',(-25.7020061921809,-86.795000649475,
74.1509454828671));
#210722=CARTESIAN_POINT('Ctrl Pts',(-25.7309197773289,-86.6269076368682,
75.3136246984158));
#210723=CARTESIAN_POINT('Ctrl Pts',(-25.7464095591912,-86.4825368138157,
75.9421181765224));
#210724=CARTESIAN_POINT('Ctrl Pts',(-25.7802443466448,-86.058468686505,
77.2828736886994));
#210725=CARTESIAN_POINT('Ctrl Pts',(-25.7985939560829,-85.758370917871,
77.9889025693498));
#210726=CARTESIAN_POINT('Ctrl Pts',(-25.831032553874,-85.1291604331345,
79.1443949968908));
#210727=CARTESIAN_POINT('Ctrl Pts',(-25.844811107583,-84.8322918439808,
79.6085218961476));
#210728=CARTESIAN_POINT('Ctrl Pts',(-25.8792602330504,-83.990955503201,
80.7386112650431));
#210729=CARTESIAN_POINT('Ctrl Pts',(-25.8997594340109,-83.4048901794276,
81.3694771722443));
#210730=CARTESIAN_POINT('Ctrl Pts',(-25.9579490738006,-81.5877385699402,
82.9475470254536));
#210731=CARTESIAN_POINT('Ctrl Pts',(-25.9960369474434,-80.2388638266101,
83.7179044612192));
#210732=CARTESIAN_POINT('Ctrl Pts',(-26.0520110212422,-78.0417648515169,
84.4556003538643));
#210733=CARTESIAN_POINT('Ctrl Pts',(-26.0705765621172,-77.288612729029,
84.6300887618639));
#210734=CARTESIAN_POINT('Ctrl Pts',(-26.1000724134121,-76.0986710445967,
84.7856474129164));
#210735=CARTESIAN_POINT('Ctrl Pts',(-26.1107596449467,-75.6697395694068,
84.8178911491601));
#210736=CARTESIAN_POINT('Ctrl Pts',(-26.1480724884064,-74.1490259463417,
84.8475873904511));
#210737=CARTESIAN_POINT('Ctrl Pts',(-26.1742484856788,-73.0566099990662,
84.7171041053917));
#210738=CARTESIAN_POINT('Ctrl Pts',(-26.2193931213824,-71.2585880803683,
84.2478848991978));
#210739=CARTESIAN_POINT('Ctrl Pts',(-26.2384151825556,-70.5337737099665,
83.981778363005));
#210740=CARTESIAN_POINT('Ctrl Pts',(-26.2957251622276,-68.4292285265332,
82.9604600860379));
#210741=CARTESIAN_POINT('Ctrl Pts',(-26.3332502293259,-67.1567131535949,
81.9948919179989));
#210742=CARTESIAN_POINT('Ctrl Pts',(-26.3809156049555,-65.8740149622752,
80.5415543079316));
#210743=CARTESIAN_POINT('Ctrl Pts',(-26.3900399203341,-65.641478463133,
80.2509925078922));
#210744=CARTESIAN_POINT('Ctrl Pts',(-26.4361742047054,-64.5325293841572,
78.7228356001248));
#210745=CARTESIAN_POINT('Ctrl Pts',(-26.4727735230356,-63.8780065946758,
77.3230290806258));
#210746=CARTESIAN_POINT('Ctrl Pts',(-26.5412761300322,-63.2022949315233,
74.611776993663));
#210747=CARTESIAN_POINT('Ctrl Pts',(-26.5723193488738,-63.0981845490051,
73.3221947465108));
#210748=CARTESIAN_POINT('Ctrl Pts',(-26.6346898575196,-63.2994981574995,
70.7677501968342));
#210749=CARTESIAN_POINT('Ctrl Pts',(-26.6657005351421,-63.6077274104244,
69.5203338851136));
#210750=CARTESIAN_POINT('Ctrl Pts',(-26.6970005540986,-64.1119403475322,
68.3407908335599));
#210751=CARTESIAN_POINT('',(-22.5673849603904,-63.669040753613,76.420933693241));
#210752=CARTESIAN_POINT('Ctrl Pts',(-22.5675364832709,-63.6687702444235,
76.4210531081683));
#210753=CARTESIAN_POINT('Ctrl Pts',(-22.5675364832709,-63.7258038321112,
76.6088225515179));
#210754=CARTESIAN_POINT('Ctrl Pts',(-22.5675364832709,-63.7873203078865,
76.7945020356765));
#210755=CARTESIAN_POINT('Ctrl Pts',(-22.5675364832709,-63.8532188980627,
76.9781622505545));
#210756=CARTESIAN_POINT('Ctrl Pts',(-22.5675364832709,-63.9184088764334,
77.1598475552547));
#210757=CARTESIAN_POINT('Ctrl Pts',(-22.5675364832709,-63.9878875599488,
77.33955714555));
#210758=CARTESIAN_POINT('Ctrl Pts',(-22.5675364832709,-64.0616097872864,
77.5173473119477));
#210759=CARTESIAN_POINT('Ctrl Pts',(-22.5675364832709,-64.1355001969537,
77.6955430705995));
#210760=CARTESIAN_POINT('Ctrl Pts',(-22.5675364832709,-64.2136537188044,
77.8718110268248));
#210761=CARTESIAN_POINT('Ctrl Pts',(-22.5675364832709,-64.2960741558206,
78.0461899469697));
#210762=CARTESIAN_POINT('Ctrl Pts',(-22.5675364832709,-64.378330446047,
78.2202215777655));
#210763=CARTESIAN_POINT('Ctrl Pts',(-22.5675364832709,-64.4648368683367,
78.3923720715572));
#210764=CARTESIAN_POINT('Ctrl Pts',(-22.5675364832709,-64.5556433242083,
78.5626563900689));
#210765=CARTESIAN_POINT('Ctrl Pts',(-22.5675364832709,-64.6480925106386,
78.7360212302351));
#210766=CARTESIAN_POINT('Ctrl Pts',(-22.5675364832709,-64.7449987516446,
78.9074522896587));
#210767=CARTESIAN_POINT('Ctrl Pts',(-22.5675364832709,-64.8464610303325,
79.0769339040445));
#210768=CARTESIAN_POINT('Ctrl Pts',(-22.5675364832709,-64.8669864107892,
79.1112193021322));
#210769=CARTESIAN_POINT('Ctrl Pts',(-22.5675364832709,-64.8876983884462,
79.145424805595));
#210770=CARTESIAN_POINT('Ctrl Pts',(-22.5675364832709,-64.9085980057327,
79.1795501013398));
#210771=CARTESIAN_POINT('Ctrl Pts',(-22.5675364832709,-64.9174000338929,
79.1939222216519));
#210772=CARTESIAN_POINT('Ctrl Pts',(-22.5675364832709,-64.9262364572077,
79.2082819116383));
#210773=CARTESIAN_POINT('Ctrl Pts',(-22.5675364832709,-64.9351037869345,
79.222623373272));
#210774=CARTESIAN_POINT('Ctrl Pts',(-22.5675364832709,-65.0375475668251,
79.3883095024868));
#210775=CARTESIAN_POINT('Ctrl Pts',(-22.5675364832709,-65.1436663874556,
79.5508453779689));
#210776=CARTESIAN_POINT('Ctrl Pts',(-22.5675364832709,-65.2534263053612,
79.7102890247438));
#210777=CARTESIAN_POINT('Ctrl Pts',(-22.5675364832709,-65.3633010588936,
79.8698994884356));
#210778=CARTESIAN_POINT('Ctrl Pts',(-22.5675364832709,-65.4768247520306,
80.0264116215346));
#210779=CARTESIAN_POINT('Ctrl Pts',(-22.5675364832709,-65.5940096958059,
80.1798598398312));
#210780=CARTESIAN_POINT('Ctrl Pts',(-22.5675364832709,-65.6823624769175,
80.2955536858692));
#210781=CARTESIAN_POINT('Ctrl Pts',(-22.5675364832709,-65.7727974833994,
80.4095053827246));
#210782=CARTESIAN_POINT('Ctrl Pts',(-22.5675364832709,-65.8653362932692,
80.5217187995515));
#210783=CARTESIAN_POINT('Ctrl Pts',(-22.5675364832709,-65.987966895796,
80.6704218025018));
#210784=CARTESIAN_POINT('Ctrl Pts',(-22.5675364832709,-66.1142907375747,
80.8160736236853));
#210785=CARTESIAN_POINT('Ctrl Pts',(-22.5675364832709,-66.2443103813311,
80.9587217971806));
#210786=CARTESIAN_POINT('Ctrl Pts',(-22.5675364832709,-66.3745137755541,
81.1015715684322));
#210787=CARTESIAN_POINT('Ctrl Pts',(-22.5675364832709,-66.5084237436001,
81.2414094814956));
#210788=CARTESIAN_POINT('Ctrl Pts',(-22.5675364832709,-66.6460788550177,
81.3782455406439));
#210789=CARTESIAN_POINT('Ctrl Pts',(-22.5675364832709,-66.7103748553523,
81.4421589777416));
#210790=CARTESIAN_POINT('Ctrl Pts',(-22.5675364832709,-66.7754883930306,
81.5054169558065));
#210791=CARTESIAN_POINT('Ctrl Pts',(-22.5675364832709,-66.8414257863485,
81.5680174031831));
#210792=CARTESIAN_POINT('Ctrl Pts',(-22.5675364832709,-66.8594783064253,
81.5851563250637));
#210793=CARTESIAN_POINT('Ctrl Pts',(-22.5675364832709,-66.8775970561921,
81.6022500915462));
#210794=CARTESIAN_POINT('Ctrl Pts',(-22.5675364832709,-66.8957572266453,
81.619275372102));
#210795=CARTESIAN_POINT('Ctrl Pts',(-22.5675364832709,-67.0349336946461,
81.7497542363061));
#210796=CARTESIAN_POINT('Ctrl Pts',(-22.5675364832709,-67.1767618191788,
81.8764274620977));
#210797=CARTESIAN_POINT('Ctrl Pts',(-22.5675364832709,-67.3212106845732,
81.9993967091251));
#210798=CARTESIAN_POINT('Ctrl Pts',(-22.5675364832709,-67.4664417640186,
82.1230318545839));
#210799=CARTESIAN_POINT('Ctrl Pts',(-22.5675364832709,-67.6143223758131,
82.2429230597769));
#210800=CARTESIAN_POINT('Ctrl Pts',(-22.5675364832709,-67.7648596939825,
82.3591374576176));
#210801=CARTESIAN_POINT('Ctrl Pts',(-22.5675364832709,-67.9155872738129,
82.4754987369403));
#210802=CARTESIAN_POINT('Ctrl Pts',(-22.5675364832709,-68.0689786215426,
82.5881741648509));
#210803=CARTESIAN_POINT('Ctrl Pts',(-22.5675364832709,-68.2250744281003,
82.6971910903905));
#210804=CARTESIAN_POINT('Ctrl Pts',(-22.5675364832709,-68.3803784145739,
82.8056550107402));
#210805=CARTESIAN_POINT('Ctrl Pts',(-22.5675364832709,-68.538359844291,
82.9104976776817));
#210806=CARTESIAN_POINT('Ctrl Pts',(-22.5675364832709,-68.6990866879562,
83.0117028805195));
#210807=CARTESIAN_POINT('Ctrl Pts',(-22.5675364832709,-68.819631820705,
83.0876067826479));
#210808=CARTESIAN_POINT('Ctrl Pts',(-22.5675364832709,-68.9417218476887,
83.1614637579624));
#210809=CARTESIAN_POINT('Ctrl Pts',(-22.5675364832709,-69.0653940624834,
83.2332496878576));
#210810=CARTESIAN_POINT('Ctrl Pts',(-22.5675364832709,-69.119053375501,
83.2643964065358));
#210811=CARTESIAN_POINT('Ctrl Pts',(-22.5675364832709,-69.1730106287839,
83.2951530451425));
#210812=CARTESIAN_POINT('Ctrl Pts',(-22.5675364832709,-69.2272692395212,
83.3255167097264));
#210813=CARTESIAN_POINT('Ctrl Pts',(-22.5675364832709,-69.2590702189398,
83.3433128578286));
#210814=CARTESIAN_POINT('Ctrl Pts',(-22.5675364832709,-69.2909747226799,
83.3609740033855));
#210815=CARTESIAN_POINT('Ctrl Pts',(-22.5675364832709,-69.3229834710798,
83.3784994710574));
#210816=CARTESIAN_POINT('Ctrl Pts',(-22.5675364832709,-69.3427780357163,
83.389337414431));
#210817=CARTESIAN_POINT('Ctrl Pts',(-22.5675364832709,-69.362616341774,
83.4001255274541));
#210818=CARTESIAN_POINT('Ctrl Pts',(-22.5675364832709,-69.3824732041753,
83.4108500423031));
#210819=CARTESIAN_POINT('Ctrl Pts',(-22.5675364832709,-69.5606622039941,
83.5070883369465));
#210820=CARTESIAN_POINT('Ctrl Pts',(-22.5675364832709,-69.7407061600605,
83.5984099230677));
#210821=CARTESIAN_POINT('Ctrl Pts',(-22.5675364832709,-69.9225805595835,
83.684846614458));
#210822=CARTESIAN_POINT('Ctrl Pts',(-22.5675364832709,-70.0183813516282,
83.730376405999));
#210823=CARTESIAN_POINT('Ctrl Pts',(-22.5675364832709,-70.1146905431934,
83.7745501571491));
#210824=CARTESIAN_POINT('Ctrl Pts',(-22.5675364832709,-70.2115077836584,
83.8173676866023));
#210825=CARTESIAN_POINT('Ctrl Pts',(-22.5675364832709,-70.394853554888,
83.8984525525004));
#210826=CARTESIAN_POINT('Ctrl Pts',(-22.5675364832709,-70.5800199760405,
83.9746766474746));
#210827=CARTESIAN_POINT('Ctrl Pts',(-22.5675364832709,-70.7669764966094,
84.0461131619166));
#210828=CARTESIAN_POINT('Ctrl Pts',(-22.5675364832709,-70.9546509613198,
84.1178240044584));
#210829=CARTESIAN_POINT('Ctrl Pts',(-22.5675364832709,-71.1441297243915,
84.1847105346889));
#210830=CARTESIAN_POINT('Ctrl Pts',(-22.5675364832709,-71.3354013965792,
84.2467978873676));
#210831=CARTESIAN_POINT('Ctrl Pts',(-22.5675364832709,-71.5266286583088,
84.3088708242798));
#210832=CARTESIAN_POINT('Ctrl Pts',(-22.5675364832709,-71.7196484304936,
84.3661469096111));
#210833=CARTESIAN_POINT('Ctrl Pts',(-22.5675364832709,-71.91446234413,84.4186009739624));
#210834=CARTESIAN_POINT('Ctrl Pts',(-22.5675364832709,-72.0106871486104,
84.4445097090839));
#210835=CARTESIAN_POINT('Ctrl Pts',(-22.5675364832709,-72.1073498268638,
84.4692412399597));
#210836=CARTESIAN_POINT('Ctrl Pts',(-22.5675364832709,-72.2044512501012,
84.4927878836045));
#210837=CARTESIAN_POINT('',(-22.5675364837383,-63.6650775904626,76.4088722770809));
#210838=CARTESIAN_POINT('Ctrl Pts',(-22.5673829558621,-63.6690417381459,
76.4209333437237));
#210839=CARTESIAN_POINT('Ctrl Pts',(-22.5674341318949,-63.6677182296578,
76.4169137400222));
#210840=CARTESIAN_POINT('Ctrl Pts',(-22.5674853079278,-63.6663968467197,
76.4128933831604));
#210841=CARTESIAN_POINT('Ctrl Pts',(-22.5675364839606,-63.665077590315,
76.4088722753856));
#210842=CARTESIAN_POINT('Ctrl Pts',(-22.5675364837383,-63.6650775904626,
76.4088722770809));
#210843=CARTESIAN_POINT('Ctrl Pts',(-22.586268085323,-63.4407556184205,
75.6674670848505));
#210844=CARTESIAN_POINT('Ctrl Pts',(-22.6057724255717,-63.2917836040619,
74.9097552024768));
#210845=CARTESIAN_POINT('Ctrl Pts',(-22.6429310858971,-63.1457829357986,
73.4058157535817));
#210846=CARTESIAN_POINT('Ctrl Pts',(-22.6606405257089,-63.1430629241209,
72.6625676820767));
#210847=CARTESIAN_POINT('Ctrl Pts',(-22.6917079591697,-63.2582592579212,
71.3752055764282));
#210848=CARTESIAN_POINT('Ctrl Pts',(-22.7050393165102,-63.3458208703714,
70.8282257981593));
#210849=CARTESIAN_POINT('Ctrl Pts',(-22.7250377762266,-63.5307031732887,
70.0378179720608));
#210850=CARTESIAN_POINT('Ctrl Pts',(-22.7314888115041,-63.5980781301251,
69.7878453758935));
#210851=CARTESIAN_POINT('Ctrl Pts',(-22.7709634204641,-64.0624224972185,
68.2665105161733));
#210852=CARTESIAN_POINT('Ctrl Pts',(-22.8027640999297,-64.6679194849621,
67.0581888191365));
#210853=CARTESIAN_POINT('Ctrl Pts',(-22.8537481998866,-65.9071091201683,
65.3669320568941));
#210854=CARTESIAN_POINT('Ctrl Pts',(-22.8725290298921,-66.4156702435171,
64.7993630234648));
#210855=CARTESIAN_POINT('Ctrl Pts',(-22.9239292449122,-67.9619180596299,
63.3764671688569));
#210856=CARTESIAN_POINT('Ctrl Pts',(-22.9604267297465,-69.2359429638033,
62.5103550986164));
#210857=CARTESIAN_POINT('Ctrl Pts',(-23.0202928869868,-71.5293846545732,
61.6432305647962));
#210858=CARTESIAN_POINT('Ctrl Pts',(-23.0392730866334,-72.2792099810029,
61.441436526952));
#210859=CARTESIAN_POINT('Ctrl Pts',(-23.0930290504121,-74.445504175765,
61.0779603516231));
#210860=CARTESIAN_POINT('Ctrl Pts',(-23.1299594944171,-76.0198431470072,
61.0706562319354));
#210861=CARTESIAN_POINT('Ctrl Pts',(-23.1905021030074,-78.4129038273741,
61.628264893377));
#210862=CARTESIAN_POINT('Ctrl Pts',(-23.2090908068358,-79.130062116161,
61.8685784075949));
#210863=CARTESIAN_POINT('Ctrl Pts',(-23.2410740979783,-80.3384165870843,
62.4056935084503));
#210864=CARTESIAN_POINT('Ctrl Pts',(-23.2545074008345,-80.8422218529907,
62.6745433313161));
#210865=CARTESIAN_POINT('Ctrl Pts',(-23.2863973120796,-81.9507079764464,
63.3759610656578));
#210866=CARTESIAN_POINT('Ctrl Pts',(-23.3048480792465,-82.5381646861957,
63.8305898999235));
#210867=CARTESIAN_POINT('Ctrl Pts',(-23.3350930669854,-83.4322130684856,
64.6654052881871));
#210868=CARTESIAN_POINT('Ctrl Pts',(-23.3469809107225,-83.7657290843186,
65.0169928637771));
#210869=CARTESIAN_POINT('Ctrl Pts',(-23.36893902758,-84.3520862167886,65.7159828751825));
#210870=CARTESIAN_POINT('Ctrl Pts',(-23.3790075514594,-84.609791987786,
66.0593191549823));
#210871=CARTESIAN_POINT('Ctrl Pts',(-23.3969914175803,-85.0270869734603,
66.6842488965303));
#210872=CARTESIAN_POINT('Ctrl Pts',(-23.4048424767611,-85.1948254259029,
66.9596772122972));
#210873=CARTESIAN_POINT('Ctrl Pts',(-23.4296186292686,-85.6824443991078,
67.839468895149));
#210874=CARTESIAN_POINT('Ctrl Pts',(-23.4468326360181,-85.9619375557439,
68.4665319016512));
#210875=CARTESIAN_POINT('Ctrl Pts',(-23.4767056660226,-86.3583903479144,
69.6102254268307));
#210876=CARTESIAN_POINT('Ctrl Pts',(-23.489401765161,-86.4979883598872,
70.1191785115426));
#210877=CARTESIAN_POINT('Ctrl Pts',(-23.5097178004072,-86.6694129472462,
70.9606073814973));
#210878=CARTESIAN_POINT('Ctrl Pts',(-23.5175437050304,-86.7219987057389,
71.2888547719625));
#210879=CARTESIAN_POINT('Ctrl Pts',(-23.5372801291869,-86.8169868755348,
72.1037210969665));
#210880=CARTESIAN_POINT('Ctrl Pts',(-23.5494001670538,-86.8428986535457,
72.5918834219198));
#210881=CARTESIAN_POINT('Ctrl Pts',(-23.5734791553164,-86.8347310175825,
73.555385132888));
#210882=CARTESIAN_POINT('Ctrl Pts',(-23.5854383058721,-86.8020866465661,
74.0310234500652));
#210883=CARTESIAN_POINT('Ctrl Pts',(-23.6099759330426,-86.674778997216,
75.0188565090374));
#210884=CARTESIAN_POINT('Ctrl Pts',(-23.6223585606802,-86.5746198606898,
75.5304187723396));
#210885=CARTESIAN_POINT('Ctrl Pts',(-23.6423017686355,-86.3580165407987,
76.347259459777));
#210886=CARTESIAN_POINT('Ctrl Pts',(-23.64996574602,-86.261790108825,76.65790185941));
#210887=CARTESIAN_POINT('Ctrl Pts',(-23.6713796367493,-85.9633916480115,
77.4955707899585));
#210888=CARTESIAN_POINT('Ctrl Pts',(-23.6855188631017,-85.7356046736506,
78.0123852988445));
#210889=CARTESIAN_POINT('Ctrl Pts',(-23.7091552450762,-85.2958981914814,
78.8448886272851));
#210890=CARTESIAN_POINT('Ctrl Pts',(-23.7186618439811,-85.1029821930297,
79.1713809851606));
#210891=CARTESIAN_POINT('Ctrl Pts',(-23.7427639934682,-84.5651742002068,
79.9901439374166));
#210892=CARTESIAN_POINT('Ctrl Pts',(-23.7568771368581,-84.1974308613908,
80.4674901565153));
#210893=CARTESIAN_POINT('Ctrl Pts',(-23.7781528652288,-83.5953254237176,
81.1368390030137));
#210894=CARTESIAN_POINT('Ctrl Pts',(-23.7852645329272,-83.3865629699947,
81.3518844373689));
#210895=CARTESIAN_POINT('Ctrl Pts',(-23.8051161905733,-82.7938308006642,
81.9171206383192));
#210896=CARTESIAN_POINT('Ctrl Pts',(-23.8181956316299,-82.3943211869376,
82.2499055715468));
#210897=CARTESIAN_POINT('Ctrl Pts',(-23.8397098155051,-81.7028715992346,
82.7532298694108));
#210898=CARTESIAN_POINT('Ctrl Pts',(-23.8481703871649,-81.4220441131709,
82.9399204995204));
#210899=CARTESIAN_POINT('Ctrl Pts',(-23.8711970500663,-80.6219484498624,
83.4243581702032));
#210900=CARTESIAN_POINT('Ctrl Pts',(-23.8852778638192,-80.0867100406283,
83.6958827846338));
#210901=CARTESIAN_POINT('Ctrl Pts',(-23.9073163037075,-79.2263152444547,
84.053440516101));
#210902=CARTESIAN_POINT('Ctrl Pts',(-23.9152294424715,-78.913127485958,
84.1683613902867));
#210903=CARTESIAN_POINT('Ctrl Pts',(-23.9341886438323,-78.167825248394,
84.4061841008917));
#210904=CARTESIAN_POINT('Ctrl Pts',(-23.9454211520972,-77.733419580155,
84.5174767713367));
#210905=CARTESIAN_POINT('Ctrl Pts',(-23.9652782132137,-76.9595352927832,
84.6696729400019));
#210906=CARTESIAN_POINT('Ctrl Pts',(-23.9738842404027,-76.6217327526431,
84.7210490326955));
#210907=CARTESIAN_POINT('Ctrl Pts',(-23.9968051979934,-75.6997099389066,
84.8210702035748));
#210908=CARTESIAN_POINT('Ctrl Pts',(-24.0107033113079,-75.1123315013629,
84.8413692782653));
#210909=CARTESIAN_POINT('Ctrl Pts',(-24.0340122827486,-74.1297607022727,
84.8028056628773));
#210910=CARTESIAN_POINT('Ctrl Pts',(-24.0434324047584,-73.7335916800172,
84.7673381145636));
#210911=CARTESIAN_POINT('Ctrl Pts',(-24.0646309551327,-72.8665015294452,
84.6450363719954));
#210912=CARTESIAN_POINT('Ctrl Pts',(-24.0765713079443,-72.399014171567,
84.5493528448018));
#210913=CARTESIAN_POINT('Ctrl Pts',(-24.0997554081118,-71.5089793165134,
84.310313566701));
#210914=CARTESIAN_POINT('Ctrl Pts',(-24.1108807937167,-71.0858335697661,
84.1706526421816));
#210915=CARTESIAN_POINT('Ctrl Pts',(-24.138533227618,-70.0268835211385,
83.7543074460251));
#210916=CARTESIAN_POINT('Ctrl Pts',(-24.1548409783302,-69.4039225594739,
83.4445873667952));
#210917=CARTESIAN_POINT('Ctrl Pts',(-24.1798141076876,-68.5144527788177,
82.9004178078518));
#210918=CARTESIAN_POINT('Ctrl Pts',(-24.1882658800564,-68.2242060734541,
82.704657018762));
#210919=CARTESIAN_POINT('Ctrl Pts',(-24.2064651621954,-67.6319243272847,
82.2650889548629));
#210920=CARTESIAN_POINT('Ctrl Pts',(-24.2162594926797,-67.3322371454712,
82.0184893106432));
#210921=CARTESIAN_POINT('Ctrl Pts',(-24.2503354667518,-66.3240452924204,
81.1023758653165));
#210922=CARTESIAN_POINT('Ctrl Pts',(-24.2734890978267,-65.6834341645618,
80.3575421127117));
#210923=CARTESIAN_POINT('Ctrl Pts',(-24.3359484974999,-64.2389187654643,
78.1900043195484));
#210924=CARTESIAN_POINT('Ctrl Pts',(-24.3698713517956,-63.7839507079286,
76.9116039690688));
#210925=CARTESIAN_POINT('Ctrl Pts',(-24.4133074766064,-63.3381100240567,
75.1700668662164));
#210926=CARTESIAN_POINT('Ctrl Pts',(-24.4319587440239,-63.2185309075811,
74.3940693434518));
#210927=CARTESIAN_POINT('Ctrl Pts',(-24.4613547807653,-63.1540310279044,
73.1896082034826));
#210928=CARTESIAN_POINT('Ctrl Pts',(-24.471852603356,-63.1544389514483,
72.7660588280706));
#210929=CARTESIAN_POINT('Ctrl Pts',(-24.5046971488066,-63.2278786888342,
71.441152956426));
#210930=CARTESIAN_POINT('Ctrl Pts',(-24.5265462495199,-63.381491704234,
70.5461094578424));
#210931=CARTESIAN_POINT('Ctrl Pts',(-24.5670051429739,-63.848113738075,
68.940460524804));
#210932=CARTESIAN_POINT('Ctrl Pts',(-24.5856817309163,-64.1348934482634,
68.2206283273269));
#210933=CARTESIAN_POINT('Ctrl Pts',(-24.6232006790464,-64.8387020839017,
66.8653478737878));
#210934=CARTESIAN_POINT('Ctrl Pts',(-24.641661123262,-65.2512151410827,
66.2297978498682));
#210935=CARTESIAN_POINT('Ctrl Pts',(-24.688246890458,-66.4376319825064,
64.7326308652929));
#210936=CARTESIAN_POINT('Ctrl Pts',(-24.7260382386131,-67.5561267157986,
63.5847792685608));
#210937=CARTESIAN_POINT('Ctrl Pts',(-24.7917113773772,-69.8951100285009,
62.2801640674082));
#210938=CARTESIAN_POINT('Ctrl Pts',(-24.8105835909978,-70.6016469499005,
61.9711661347996));
#210939=CARTESIAN_POINT('Ctrl Pts',(-24.8476505405662,-72.0487458576382,
61.4982879163503));
#210940=CARTESIAN_POINT('Ctrl Pts',(-24.8656179042792,-72.7881859508202,
61.3322689755976));
#210941=CARTESIAN_POINT('Ctrl Pts',(-24.9052918234948,-74.4024570724264,
61.1330685277049));
#210942=CARTESIAN_POINT('Ctrl Pts',(-24.9268693700248,-75.2747719906355,
61.1221140290983));
#210943=CARTESIAN_POINT('Ctrl Pts',(-24.9577085382441,-76.5262184018719,
61.2424810283113));
#210944=CARTESIAN_POINT('Ctrl Pts',(-24.9672177195347,-76.9128067571203,
61.298875033784));
#210945=CARTESIAN_POINT('Ctrl Pts',(-24.9905520650339,-77.8648755091039,
61.4862146028854));
#210946=CARTESIAN_POINT('Ctrl Pts',(-25.0042103174987,-78.4242489456068,
61.6397751316609));
#210947=CARTESIAN_POINT('Ctrl Pts',(-25.033528821721,-79.5538256273119,
62.0429563473436));
#210948=CARTESIAN_POINT('Ctrl Pts',(-25.04892536006,-80.1189290269644,62.296315326189));
#210949=CARTESIAN_POINT('Ctrl Pts',(-25.0800666050373,-81.2227434998887,
62.8976245618864));
#210950=CARTESIAN_POINT('Ctrl Pts',(-25.0957726872482,-81.759935237262,
63.2487373897805));
#210951=CARTESIAN_POINT('Ctrl Pts',(-25.1193718523509,-82.5435011709395,
63.8566578124951));
#210952=CARTESIAN_POINT('Ctrl Pts',(-25.1276624343038,-82.8120640683606,
64.0849197521116));
#210953=CARTESIAN_POINT('Ctrl Pts',(-25.1454609563522,-83.3545132896373,
64.5900982370671));
#210954=CARTESIAN_POINT('Ctrl Pts',(-25.1550148296105,-83.625759296159,
64.869428342891));
#210955=CARTESIAN_POINT('Ctrl Pts',(-25.1821367707944,-84.3482342239114,
65.6906711368966));
#210956=CARTESIAN_POINT('Ctrl Pts',(-25.1999107406064,-84.7667054739517,
66.2617692430849));
#210957=CARTESIAN_POINT('Ctrl Pts',(-25.2283952223508,-85.3696652829342,
67.2584876520549));
#210958=CARTESIAN_POINT('Ctrl Pts',(-25.2393089263843,-85.5849431538456,
67.665653210413));
#210959=CARTESIAN_POINT('Ctrl Pts',(-25.2610572632069,-85.9669200722996,
68.5030414663968));
#210960=CARTESIAN_POINT('Ctrl Pts',(-25.2719955468722,-86.1331191980178,
68.9323993214247));
#210961=CARTESIAN_POINT('Ctrl Pts',(-25.2937880673866,-86.4034375703859,
69.7767493402283));
#210962=CARTESIAN_POINT('Ctrl Pts',(-25.3044379286781,-86.5109674922512,
70.1883156831867));
#210963=CARTESIAN_POINT('Ctrl Pts',(-25.3293736091068,-86.7108551138341,
71.1638320986707));
#210964=CARTESIAN_POINT('Ctrl Pts',(-25.343638785203,-86.7852594491684,
71.7315450267012));
#210965=CARTESIAN_POINT('Ctrl Pts',(-25.3658368888779,-86.8394224130096,
72.6541834421136));
#210966=CARTESIAN_POINT('Ctrl Pts',(-25.374145029744,-86.8444614999076,
73.0076890856007));
#210967=CARTESIAN_POINT('Ctrl Pts',(-25.3932547504683,-86.8197084010493,
73.8167754615253));
#210968=CARTESIAN_POINT('Ctrl Pts',(-25.4041146979202,-86.7793325444496,
74.2716084565836));
#210969=CARTESIAN_POINT('Ctrl Pts',(-25.424894620039,-86.6553428033959,
75.1053687246365));
#210970=CARTESIAN_POINT('Ctrl Pts',(-25.4345780693059,-86.5799035844431,
75.483491530525));
#210971=CARTESIAN_POINT('Ctrl Pts',(-25.4567619973944,-86.3652872626109,
76.3401422706028));
#210972=CARTESIAN_POINT('Ctrl Pts',(-25.4692500578771,-86.2138979984785,
76.8156577038014));
#210973=CARTESIAN_POINT('Ctrl Pts',(-25.4890094659494,-85.9180320095654,
77.5769828960217));
#210974=CARTESIAN_POINT('Ctrl Pts',(-25.4965644957774,-85.7906708954485,
77.8694937917343));
#210975=CARTESIAN_POINT('Ctrl Pts',(-25.5177272011171,-85.4002237205209,
78.675968320559));
#210976=CARTESIAN_POINT('Ctrl Pts',(-25.5313223378869,-85.1104844963385,
79.1778737046409));
#210977=CARTESIAN_POINT('Ctrl Pts',(-25.5539619675576,-84.5929121635644,
79.93673654874));
#210978=CARTESIAN_POINT('Ctrl Pts',(-25.5624776214518,-84.3898698056711,
80.2082748200738));
#210979=CARTESIAN_POINT('Ctrl Pts',(-25.583850319648,-83.8526286867851,
80.8660090615761));
#210980=CARTESIAN_POINT('Ctrl Pts',(-25.5966963903215,-83.5041146448396,
81.2405495882105));
#210981=CARTESIAN_POINT('Ctrl Pts',(-25.6174987374248,-82.8801328369273,
81.8305356652936));
#210982=CARTESIAN_POINT('Ctrl Pts',(-25.6257626286481,-82.6166528461616,
82.0587208875653));
#210983=CARTESIAN_POINT('Ctrl Pts',(-25.6481489502375,-81.8749389306029,
82.6461857161961));
#210984=CARTESIAN_POINT('Ctrl Pts',(-25.6622524342849,-81.3776042707483,
82.982588201651));
#210985=CARTESIAN_POINT('Ctrl Pts',(-25.6849535707228,-80.5776536122919,
83.4376350608617));
#210986=CARTESIAN_POINT('Ctrl Pts',(-25.6930171765533,-80.2925384126093,
83.5846073202146));
#210987=CARTESIAN_POINT('Ctrl Pts',(-25.7146507220582,-79.5134293397299,
83.9469660150489));
#210988=CARTESIAN_POINT('Ctrl Pts',(-25.7281391359254,-79.0093860434919,
84.1408019798079));
#210989=CARTESIAN_POINT('Ctrl Pts',(-25.7520876074811,-78.0611832160611,
84.4337245706684));
#210990=CARTESIAN_POINT('Ctrl Pts',(-25.7628108659822,-77.6200926928871,
84.5429585790474));
#210991=CARTESIAN_POINT('Ctrl Pts',(-25.7851622316925,-76.6949087349468,
84.7165901495161));
#210992=CARTESIAN_POINT('Ctrl Pts',(-25.7968063426044,-76.209853352635,
84.7770486933715));
#210993=CARTESIAN_POINT('Ctrl Pts',(-25.8166416512073,-75.4074932820353,
84.8260692378726));
#210994=CARTESIAN_POINT('Ctrl Pts',(-25.8245878850808,-75.0915856903094,
84.8324891107674));
#210995=CARTESIAN_POINT('Ctrl Pts',(-25.8461263984118,-74.2351689420447,
84.8155658720594));
#210996=CARTESIAN_POINT('Ctrl Pts',(-25.8595502609578,-73.6951265588063,
84.7677371052758));
#210997=CARTESIAN_POINT('Ctrl Pts',(-25.8870929365112,-72.5668908757251,
84.590167107365));
#210998=CARTESIAN_POINT('Ctrl Pts',(-25.9012958491269,-71.9799307868807,
84.4518600552353));
#210999=CARTESIAN_POINT('Ctrl Pts',(-25.9262597884433,-70.9876187870929,
84.1367233640308));
#211000=CARTESIAN_POINT('Ctrl Pts',(-25.9369484716105,-70.5754337900106,
83.9800739201598));
#211001=CARTESIAN_POINT('Ctrl Pts',(-25.9593084055028,-69.7555554483605,
83.6136503722819));
#211002=CARTESIAN_POINT('Ctrl Pts',(-25.9708645623636,-69.3496943959058,
83.4029204272594));
#211003=CARTESIAN_POINT('Ctrl Pts',(-25.993834366265,-68.5485247822595,
82.9265531223753));
#211004=CARTESIAN_POINT('Ctrl Pts',(-26.0053100341751,-68.1543368512848,
82.6589885236473));
#211005=CARTESIAN_POINT('Ctrl Pts',(-26.0343820127018,-67.1941352451247,
81.9199778940686));
#211006=CARTESIAN_POINT('Ctrl Pts',(-26.0518964723241,-66.6521974956702,
81.4170463576902));
#211007=CARTESIAN_POINT('Ctrl Pts',(-26.0820442935133,-65.834173220253,
80.5001478589804));
#211008=CARTESIAN_POINT('Ctrl Pts',(-26.0944271911147,-65.5306940758781,
80.1129252510169));
#211009=CARTESIAN_POINT('Ctrl Pts',(-26.1225191227804,-64.8854521730426,
79.1752815467207));
#211010=CARTESIAN_POINT('Ctrl Pts',(-26.1381663634804,-64.5620635789478,
78.6116580075701));
#211011=CARTESIAN_POINT('Ctrl Pts',(-26.1721088657882,-63.9623371723801,
77.3370325344058));
#211012=CARTESIAN_POINT('Ctrl Pts',(-26.1904008122124,-63.7041000312099,
76.6173315306627));
#211013=CARTESIAN_POINT('Ctrl Pts',(-26.2163069038114,-63.4471831016142,
75.5971963120756));
#211014=CARTESIAN_POINT('Ctrl Pts',(-26.2235318340176,-63.3868135706353,
75.3127304873911));
#211015=CARTESIAN_POINT('Ctrl Pts',(-26.2587554148368,-63.141968335338,
73.904777802475));
#211016=CARTESIAN_POINT('Ctrl Pts',(-26.2862238156631,-63.1094668467566,
72.754329610765));
#211017=CARTESIAN_POINT('Ctrl Pts',(-26.3415801754294,-63.3707065358412,
70.4878602924608));
#211018=CARTESIAN_POINT('Ctrl Pts',(-26.3693494802877,-63.6652819705078,
69.3856928759218));
#211019=CARTESIAN_POINT('Ctrl Pts',(-26.3971183084764,-64.1119392449378,
68.3407934129424));
#211020=CARTESIAN_POINT('Ctrl Pts',(-31.6489087198709,-79.9040287823937,
60.8783100640841));
#211021=CARTESIAN_POINT('Ctrl Pts',(-31.6814645153009,-81.2696674810732,
61.4313085050615));
#211022=CARTESIAN_POINT('Ctrl Pts',(-31.7465761061609,-83.811729992399,
63.0035716608669));
#211023=CARTESIAN_POINT('Ctrl Pts',(-31.8442434924509,-86.6262501677223,
66.49395799585));
#211024=CARTESIAN_POINT('Ctrl Pts',(-31.9419108787409,-88.1228094499778,
70.7205438274274));
#211025=CARTESIAN_POINT('Ctrl Pts',(-32.0395782650309,-88.1318596833692,
75.2042647157331));
#211026=CARTESIAN_POINT('Ctrl Pts',(-32.1372456513209,-86.6523499320974,
79.4368608152641));
#211027=CARTESIAN_POINT('Ctrl Pts',(-32.2349130376109,-83.8519959181997,
82.9385512545613));
#211028=CARTESIAN_POINT('Ctrl Pts',(-32.3325804239009,-80.0482284232973,
85.3124031224554));
#211029=CARTESIAN_POINT('Ctrl Pts',(-32.4302478101809,-75.6722218896999,
86.2893299487034));
#211030=CARTESIAN_POINT('Ctrl Pts',(-32.5279151964709,-71.2200159883432,
85.7585926810093));
#211031=CARTESIAN_POINT('Ctrl Pts',(-32.6255825827609,-67.1962880910714,
83.7803527627688));
#211032=CARTESIAN_POINT('Ctrl Pts',(-32.7232499690509,-64.0571456387238,
80.5788524819327));
#211033=CARTESIAN_POINT('Ctrl Pts',(-32.8209173553409,-62.1584243900869,
76.5169961329518));
#211034=CARTESIAN_POINT('Ctrl Pts',(-32.9185847416309,-61.7153528413655,
72.0552131952207));
#211035=CARTESIAN_POINT('Ctrl Pts',(-33.0162521279209,-62.7781551230735,
67.6992666057196));
#211036=CARTESIAN_POINT('Ctrl Pts',(-33.1139195142109,-65.2263578703911,
63.9429222806304));
#211037=CARTESIAN_POINT('Ctrl Pts',(-33.2115869005009,-68.7824464151142,
61.2119785531442));
#211038=CARTESIAN_POINT('Ctrl Pts',(-33.3092542867909,-73.0433223072712,
59.8160000388975));
#211039=CARTESIAN_POINT('Ctrl Pts',(-33.4069216730809,-77.5259963169692,
59.9132271101948));
#211040=CARTESIAN_POINT('Ctrl Pts',(-33.5045890593709,-81.7223374113863,
61.4926386461447));
#211041=CARTESIAN_POINT('Ctrl Pts',(-33.6022564456609,-85.1566716669334,
64.3752013257362));
#211042=CARTESIAN_POINT('Ctrl Pts',(-33.6999238319509,-87.43970202375,68.2341638508803));
#211043=CARTESIAN_POINT('Ctrl Pts',(-33.7975912182409,-88.3126368385637,
72.632095659094));
#211044=CARTESIAN_POINT('Ctrl Pts',(-33.8952586045309,-87.6765250683029,
77.0704716229308));
#211045=CARTESIAN_POINT('Ctrl Pts',(-33.9929259908209,-85.6034728108319,
81.0461820900503));
#211046=CARTESIAN_POINT('Ctrl Pts',(-34.0905933771109,-82.3284697580989,
84.1085625995896));
#211047=CARTESIAN_POINT('Ctrl Pts',(-34.1882607634009,-78.2227520696129,
85.9104787028144));
#211048=CARTESIAN_POINT('Ctrl Pts',(-34.2859281496909,-73.7517211029078,
86.2476751965479));
#211049=CARTESIAN_POINT('Ctrl Pts',(-34.3835955359809,-69.4221881001095,
85.0819293587689));
#211050=CARTESIAN_POINT('Ctrl Pts',(-34.4812629222709,-65.7249248799056,
82.545383664097));
#211051=CARTESIAN_POINT('Ctrl Pts',(-34.5789303085609,-63.0790326695276,
78.9255668466803));
#211052=CARTESIAN_POINT('Ctrl Pts',(-34.6765976948509,-61.7844351169188,
74.6328012395937));
#211053=CARTESIAN_POINT('Ctrl Pts',(-34.7742650811409,-61.9878806115566,
70.1536909137268));
#211054=CARTESIAN_POINT('Ctrl Pts',(-34.8719324674309,-63.666307701945,
65.995962942479));
#211055=CARTESIAN_POINT('Ctrl Pts',(-34.9695998537209,-66.6294592136506,
62.6309142802354));
#211056=CARTESIAN_POINT('Ctrl Pts',(-35.0672672400109,-70.5414487461066,
60.4399881567566));
#211057=CARTESIAN_POINT('Ctrl Pts',(-35.1649346263009,-74.9588348897375,
59.6715357908676));
#211058=CARTESIAN_POINT('Ctrl Pts',(-35.2626020125909,-79.3808872816728,
60.4126646754531));
#211059=CARTESIAN_POINT('Ctrl Pts',(-35.3602693988809,-83.3063466190444,
62.5793645557408));
#211060=CARTESIAN_POINT('Ctrl Pts',(-35.4579367851709,-86.2902446299875,
65.9260303652965));
#211061=CARTESIAN_POINT('Ctrl Pts',(-35.5556041714609,-87.994343206,70.0733026524509));
#211062=CARTESIAN_POINT('Ctrl Pts',(-35.6532715577509,-88.2254751955924,
74.5510696611245));
#211063=CARTESIAN_POINT('Ctrl Pts',(-35.7509389440409,-86.9574407599487,
78.8517565888795));
#211064=CARTESIAN_POINT('Ctrl Pts',(-35.8486063303309,-84.3339772411099,
82.4878614479098));
#211065=CARTESIAN_POINT('Ctrl Pts',(-35.9462737166209,-80.6524658951112,
85.0472155832));
#211066=CARTESIAN_POINT('Ctrl Pts',(-36.0439411029109,-76.3302224041847,
86.2397048224279));
#211067=CARTESIAN_POINT('Ctrl Pts',(-36.1416084892009,-71.857192288432,
85.9301552074926));
#211068=CARTESIAN_POINT('Ctrl Pts',(-36.2392758754909,-67.7404134024109,
84.1536555637811));
#211069=CARTESIAN_POINT('Ctrl Pts',(-36.3369432617809,-64.4465409395824,
81.1115800257429));
#211070=CARTESIAN_POINT('Ctrl Pts',(-36.4346106480709,-62.3489499909946,
77.1487613832986));
#211071=CARTESIAN_POINT('Ctrl Pts',(-36.5322780343609,-61.6854118183574,
72.7144027516668));
#211072=CARTESIAN_POINT('Ctrl Pts',(-36.6299454206509,-62.5311414241959,
68.3111584007035));
#211073=CARTESIAN_POINT('Ctrl Pts',(-36.7276128069509,-64.7902715968898,
64.4381556582015));
#211074=CARTESIAN_POINT('Ctrl Pts',(-36.8252801932409,-68.206719885141,
61.534416607706));
#211075=CARTESIAN_POINT('Ctrl Pts',(-36.9229475795309,-72.3932166837339,
59.9290929831488));
#211076=CARTESIAN_POINT('Ctrl Pts',(-37.0206149658209,-76.875203961106,
59.8041553558837));
#211077=CARTESIAN_POINT('Ctrl Pts',(-37.1182823521109,-81.1446285386002,
61.1737659619934));
#211078=CARTESIAN_POINT('Ctrl Pts',(-37.2159497384009,-84.7175321175373,
63.8826733471557));
#211079=CARTESIAN_POINT('Ctrl Pts',(-37.3136171246909,-87.1889103282383,
67.6238108193034));
#211080=CARTESIAN_POINT('Ctrl Pts',(-37.4112845109809,-88.2786209412064,
71.9731037866268));
#211081=CARTESIAN_POINT('Ctrl Pts',(-37.5089518972709,-87.8631423512599,
76.4375406365594));
#211082=CARTESIAN_POINT('Ctrl Pts',(-37.6066192835609,-85.9895636692369,
80.5110572786137));
#211083=CARTESIAN_POINT('Ctrl Pts',(-37.7042866698509,-82.8702903713335,
83.7319036844191));
#211084=CARTESIAN_POINT('Ctrl Pts',(-37.8019540561409,-78.8588051875596,
85.7349781226078));
#211085=CARTESIAN_POINT('Ctrl Pts',(-37.8670656470009,-75.8930709812184,
86.1071526244662));
#211086=CARTESIAN_POINT('Ctrl Pts',(-37.8996214424309,-74.4211620580609,
86.0418804791265));
#211087=CARTESIAN_POINT('Ctrl Pts',(-31.8730368301509,-79.7424307674282,
61.2773790062616));
#211088=CARTESIAN_POINT('Ctrl Pts',(-31.9055926255809,-81.0630688120212,
61.8121549909075));
#211089=CARTESIAN_POINT('Ctrl Pts',(-31.9707042164409,-83.5213650417874,
63.3326087841966));
#211090=CARTESIAN_POINT('Ctrl Pts',(-32.0683716027309,-86.2431408851346,
66.7079795823174));
#211091=CARTESIAN_POINT('Ctrl Pts',(-32.1660389890109,-87.6903854059918,
70.7952905623852));
#211092=CARTESIAN_POINT('Ctrl Pts',(-32.2637063753009,-87.6991374152512,
75.1312634607482));
#211093=CARTESIAN_POINT('Ctrl Pts',(-32.3613737615909,-86.2683806076395,
79.2243866578649));
#211094=CARTESIAN_POINT('Ctrl Pts',(-32.4590411478809,-83.5603041210376,
82.610689066389));
#211095=CARTESIAN_POINT('Ctrl Pts',(-32.5567085341709,-79.8818787282825,
84.9063175455787));
#211096=CARTESIAN_POINT('Ctrl Pts',(-32.6543759204609,-75.6500707711405,
85.8510525877097));
#211097=CARTESIAN_POINT('Ctrl Pts',(-32.7520433067509,-71.3445743749261,
85.3378042240803));
#211098=CARTESIAN_POINT('Ctrl Pts',(-32.8497106930409,-67.4534367355484,
83.4247514525908));
#211099=CARTESIAN_POINT('Ctrl Pts',(-32.9473780793309,-64.4177355988012,
80.3287473083499));
#211100=CARTESIAN_POINT('Ctrl Pts',(-33.0450454656209,-62.5815811902788,
76.400737629567));
#211101=CARTESIAN_POINT('Ctrl Pts',(-33.1427128519109,-62.1531097766604,
72.0859797803774));
#211102=CARTESIAN_POINT('Ctrl Pts',(-33.2403802382009,-63.1808904982033,
67.8735707501784));
#211103=CARTESIAN_POINT('Ctrl Pts',(-33.3380476244909,-65.5484198396858,
64.2410058345145));
#211104=CARTESIAN_POINT('Ctrl Pts',(-33.4357150107809,-68.9873278221854,
61.6000524200778));
#211105=CARTESIAN_POINT('Ctrl Pts',(-33.5333823970709,-73.1077989335492,
60.2500743203519));
#211106=CARTESIAN_POINT('Ctrl Pts',(-33.6310497833609,-77.4427594501453,
60.3440975560973));
#211107=CARTESIAN_POINT('Ctrl Pts',(-33.7287171696509,-81.5008223204608,
61.871464175445));
#211108=CARTESIAN_POINT('Ctrl Pts',(-33.8263845559409,-84.8219880725154,
64.6590403800946));
#211109=CARTESIAN_POINT('Ctrl Pts',(-33.9240519422309,-87.0297877995459,
68.390842011297));
#211110=CARTESIAN_POINT('Ctrl Pts',(-34.0217193285209,-87.8739575847217,
72.6438527593594));
#211111=CARTESIAN_POINT('Ctrl Pts',(-34.1193867148109,-87.2588070289994,
76.9359749434431));
#211112=CARTESIAN_POINT('Ctrl Pts',(-34.2170541010909,-85.2540661833469,
80.7806774275269));
#211113=CARTESIAN_POINT('Ctrl Pts',(-34.3147214873809,-82.0869813374197,
83.7421460881762));
#211114=CARTESIAN_POINT('Ctrl Pts',(-34.4123888736709,-78.1165556420916,
85.4846852834909));
#211115=CARTESIAN_POINT('Ctrl Pts',(-34.5100562599609,-73.7928545058452,
85.8107704468362));
#211116=CARTESIAN_POINT('Ctrl Pts',(-34.6077236462509,-69.6059886793678,
84.6834383749047));
#211117=CARTESIAN_POINT('Ctrl Pts',(-34.7053910325409,-66.0305580224903,
82.2304771711338));
#211118=CARTESIAN_POINT('Ctrl Pts',(-34.8030584188309,-63.4718534996216,
78.729940895939));
#211119=CARTESIAN_POINT('Ctrl Pts',(-34.9007258051209,-62.2199156466047,
74.5786309025152));
#211120=CARTESIAN_POINT('Ctrl Pts',(-34.9983931914109,-62.4166571862875,
70.2471166389011));
#211121=CARTESIAN_POINT('Ctrl Pts',(-35.0960605777009,-64.0397765902539,
66.2263945085208));
#211122=CARTESIAN_POINT('Ctrl Pts',(-35.1937279639909,-66.9052860562882,
62.9722312444263));
#211123=CARTESIAN_POINT('Ctrl Pts',(-35.2913953502809,-70.6883673438916,
60.8535007234066));
#211124=CARTESIAN_POINT('Ctrl Pts',(-35.3890627365809,-74.9601913662926,
60.1103704717333));
#211125=CARTESIAN_POINT('Ctrl Pts',(-35.4867301228709,-79.2365278743448,
60.8270776080123));
#211126=CARTESIAN_POINT('Ctrl Pts',(-35.5843975091609,-83.032635108598,
62.9223801912564));
#211127=CARTESIAN_POINT('Ctrl Pts',(-35.6820648954509,-85.9182074332976,
66.1587663561375));
#211128=CARTESIAN_POINT('Ctrl Pts',(-35.7797322817409,-87.566152393697,
70.1693773391154));
#211129=CARTESIAN_POINT('Ctrl Pts',(-35.8773996680309,-87.7896681003677,
74.4995925506423));
#211130=CARTESIAN_POINT('Ctrl Pts',(-35.9750670543209,-86.5634180540064,
78.6585628406411));
#211131=CARTESIAN_POINT('Ctrl Pts',(-36.0727344406109,-84.0264031503354,
82.1748504323777));
#211132=CARTESIAN_POINT('Ctrl Pts',(-36.1704018269009,-80.4662053104341,
84.6498684909032));
#211133=CARTESIAN_POINT('Ctrl Pts',(-36.2680692131909,-76.2863887911529,
85.8030627132264));
#211134=CARTESIAN_POINT('Ctrl Pts',(-36.3657365994809,-71.9607543820079,
85.5037134061586));
#211135=CARTESIAN_POINT('Ctrl Pts',(-36.4634039857709,-67.9796319787588,
83.7857531448031));
#211136=CARTESIAN_POINT('Ctrl Pts',(-36.5610713720609,-64.7942995092932,
80.8439203643351));
#211137=CARTESIAN_POINT('Ctrl Pts',(-36.6587387583509,-62.7658285737666,
77.0116848923228));
#211138=CARTESIAN_POINT('Ctrl Pts',(-36.7564061446409,-62.1241553730382,
72.723447660932));
#211139=CARTESIAN_POINT('Ctrl Pts',(-36.8540735309309,-62.9420164178251,
68.4652994295259));
#211140=CARTESIAN_POINT('Ctrl Pts',(-36.9517409172209,-65.126703521839,
64.7199202355243));
#211141=CARTESIAN_POINT('Ctrl Pts',(-37.0494083035109,-68.4305726866551,
61.9118654657189));
#211142=CARTESIAN_POINT('Ctrl Pts',(-37.1470756898009,-72.479115651301,
60.359440615331));
#211143=CARTESIAN_POINT('Ctrl Pts',(-37.2447430760909,-76.8134120648424,
60.238619944442));
#211144=CARTESIAN_POINT('Ctrl Pts',(-37.3424104623809,-80.9421501644669,
61.5630990137955));
#211145=CARTESIAN_POINT('Ctrl Pts',(-37.4400778486709,-84.397319090609,
64.1827422295159));
#211146=CARTESIAN_POINT('Ctrl Pts',(-37.5377452349609,-86.7872602154302,
67.8006013898866));
#211147=CARTESIAN_POINT('Ctrl Pts',(-37.6354126212509,-87.8410625823901,
72.0065760486924));
#211148=CARTESIAN_POINT('Ctrl Pts',(-37.7330800075509,-87.4392748817876,
76.3239003581206));
#211149=CARTESIAN_POINT('Ctrl Pts',(-37.8307473938409,-85.6274345396819,
80.2631860989099));
#211150=CARTESIAN_POINT('Ctrl Pts',(-37.9284147801309,-82.6109478271435,
83.3778988728008));
#211151=CARTESIAN_POINT('Ctrl Pts',(-38.0260821664209,-78.7316494782208,
85.3149678148182));
#211152=CARTESIAN_POINT('Ctrl Pts',(-38.0911937572809,-75.8636424227415,
85.6748783876891));
#211153=CARTESIAN_POINT('Ctrl Pts',(-38.1237495527109,-74.4402359800407,
85.6117570961772));
#211154=CARTESIAN_POINT('Ctrl Pts',(-32.0971649404209,-79.5808327524621,
61.6764479484404));
#211155=CARTESIAN_POINT('Ctrl Pts',(-32.1297207358509,-80.8564701429687,
62.1930014767526));
#211156=CARTESIAN_POINT('Ctrl Pts',(-32.1948323267109,-83.2310000911753,
63.6616459075254));
#211157=CARTESIAN_POINT('Ctrl Pts',(-32.2924997130009,-85.8600316025557,
66.9220011687801));
#211158=CARTESIAN_POINT('Ctrl Pts',(-32.3901670992909,-87.2579613620154,
70.8700372973401));
#211159=CARTESIAN_POINT('Ctrl Pts',(-32.4878344855809,-87.2664151471337,
75.0582622057642));
#211160=CARTESIAN_POINT('Ctrl Pts',(-32.5855018718709,-85.8844112831762,
79.0119125004583));
#211161=CARTESIAN_POINT('Ctrl Pts',(-32.6831692581609,-83.2686123238737,
82.2828268782174));
#211162=CARTESIAN_POINT('Ctrl Pts',(-32.7808366444509,-79.7155290332633,
84.5002319687039));
#211163=CARTESIAN_POINT('Ctrl Pts',(-32.8785040307409,-75.6279196525717,
85.412775226709));
#211164=CARTESIAN_POINT('Ctrl Pts',(-32.9761714170309,-71.4691327614987,
84.9170157671447));
#211165=CARTESIAN_POINT('Ctrl Pts',(-33.0738388033209,-67.7105853800127,
83.0691501424084));
#211166=CARTESIAN_POINT('Ctrl Pts',(-33.1715061896109,-64.7783255588649,
80.0786421347598));
#211167=CARTESIAN_POINT('Ctrl Pts',(-33.2691735759009,-63.0047379904651,
76.2844791261684));
#211168=CARTESIAN_POINT('Ctrl Pts',(-33.3668409621909,-62.5908667119491,
72.1167463655193));
#211169=CARTESIAN_POINT('Ctrl Pts',(-33.4645083484809,-63.5836258733412,
68.0478748946176));
#211170=CARTESIAN_POINT('Ctrl Pts',(-33.5621757347709,-65.8704818089924,
64.5390893883721));
#211171=CARTESIAN_POINT('Ctrl Pts',(-33.6598431210609,-69.1922092292778,
61.9881262869918));
#211172=CARTESIAN_POINT('Ctrl Pts',(-33.7575105073509,-73.1722755598568,
60.6841486018049));
#211173=CARTESIAN_POINT('Ctrl Pts',(-33.8551778936409,-77.3595225833569,
60.7749680020175));
#211174=CARTESIAN_POINT('Ctrl Pts',(-33.9528452799309,-81.2793072295691,
62.2502897047617));
#211175=CARTESIAN_POINT('Ctrl Pts',(-34.0505126662209,-84.4873044781106,
64.9428794344855));
#211176=CARTESIAN_POINT('Ctrl Pts',(-34.1481800525109,-86.6198735753575,
68.5475201717516));
#211177=CARTESIAN_POINT('Ctrl Pts',(-34.2458474388009,-87.4352783308858,
72.6556098596655));
#211178=CARTESIAN_POINT('Ctrl Pts',(-34.3435148250909,-86.8410889896759,
76.8014782640016));
#211179=CARTESIAN_POINT('Ctrl Pts',(-34.4411822113809,-84.9046595558289,
80.5151727650388));
#211180=CARTESIAN_POINT('Ctrl Pts',(-34.5388495976709,-81.8454929166992,
83.3757295768015));
#211181=CARTESIAN_POINT('Ctrl Pts',(-34.6365169839609,-78.0103592145147,
85.0588918641796));
#211182=CARTESIAN_POINT('Ctrl Pts',(-34.7341843702509,-73.8339879087212,
85.3738656971173));
#211183=CARTESIAN_POINT('Ctrl Pts',(-34.8318517565409,-69.7897892585688,
84.2849473910144));
#211184=CARTESIAN_POINT('Ctrl Pts',(-34.9295191428309,-66.3361911650335,
81.9155706781227));
#211185=CARTESIAN_POINT('Ctrl Pts',(-35.0271865291209,-63.8646743296805,
78.5343149451387));
#211186=CARTESIAN_POINT('Ctrl Pts',(-35.1248539154109,-62.6553961762831,
74.5244605653661));
#211187=CARTESIAN_POINT('Ctrl Pts',(-35.2225213017009,-62.8454337610229,
70.3405423640074));
#211188=CARTESIAN_POINT('Ctrl Pts',(-35.3201886879909,-64.4132454785962,
66.4568260744839));
#211189=CARTESIAN_POINT('Ctrl Pts',(-35.4178560742809,-67.181112898978,
63.3135482085524));
#211190=CARTESIAN_POINT('Ctrl Pts',(-35.5155234605709,-70.8352859417533,
61.2670132900357));
#211191=CARTESIAN_POINT('Ctrl Pts',(-35.6131908468609,-74.9615478429283,
60.5492051525981));
#211192=CARTESIAN_POINT('Ctrl Pts',(-35.7108582331509,-79.0921684670951,
61.2414905405986));
#211193=CARTESIAN_POINT('Ctrl Pts',(-35.8085256194409,-82.7589235982165,
63.2653958268243));
#211194=CARTESIAN_POINT('Ctrl Pts',(-35.9061930057309,-85.5461702366482,
66.3915023470505));
#211195=CARTESIAN_POINT('Ctrl Pts',(-36.0038603920209,-87.1379615814165,
70.2654520258604));
#211196=CARTESIAN_POINT('Ctrl Pts',(-36.1015277783109,-87.3538610051255,
74.4481154402485));
#211197=CARTESIAN_POINT('Ctrl Pts',(-36.1991951646009,-86.1693953480258,
78.4653690924801));
#211198=CARTESIAN_POINT('Ctrl Pts',(-36.2968625508909,-83.7188290595022,
81.8618394169131));
#211199=CARTESIAN_POINT('Ctrl Pts',(-36.3945299371809,-80.2799447256819,
84.2525213986484));
#211200=CARTESIAN_POINT('Ctrl Pts',(-36.4921973234709,-76.2425551780386,
85.3664206040374));
#211201=CARTESIAN_POINT('Ctrl Pts',(-36.5898647097609,-72.064316475499,
85.0772716047946));
#211202=CARTESIAN_POINT('Ctrl Pts',(-36.6875320960509,-68.2188505550257,
83.4178507257861));
#211203=CARTESIAN_POINT('Ctrl Pts',(-36.7851994823409,-65.1420580789654,
80.57626070286));
#211204=CARTESIAN_POINT('Ctrl Pts',(-36.8828668686309,-63.1827071565181,
76.8746084012712));
#211205=CARTESIAN_POINT('Ctrl Pts',(-36.9805342549209,-62.5628989277203,
72.7324925701221));
#211206=CARTESIAN_POINT('Ctrl Pts',(-37.0782016412109,-63.3528914114806,
68.6194404582811));
#211207=CARTESIAN_POINT('Ctrl Pts',(-37.1758690275009,-65.4631354468294,
65.0016848127869));
#211208=CARTESIAN_POINT('Ctrl Pts',(-37.2735364137909,-68.6544254882255,
62.2893143236977));
#211209=CARTESIAN_POINT('Ctrl Pts',(-37.3712038000809,-72.5650146189264,
60.7897882474999));
#211210=CARTESIAN_POINT('Ctrl Pts',(-37.4688711863709,-76.7516201686318,
60.673084533));
#211211=CARTESIAN_POINT('Ctrl Pts',(-37.5665385726609,-80.7396717903781,
61.9524320656214));
#211212=CARTESIAN_POINT('Ctrl Pts',(-37.6642059589509,-84.0771060637059,
64.482811111911));
#211213=CARTESIAN_POINT('Ctrl Pts',(-37.7618733452409,-86.3856101026459,
67.9773919605015));
#211214=CARTESIAN_POINT('Ctrl Pts',(-37.8595407315309,-87.4035042235849,
72.0400483107849));
#211215=CARTESIAN_POINT('Ctrl Pts',(-37.9572081178209,-87.0154074123175,
76.2102600797002));
#211216=CARTESIAN_POINT('Ctrl Pts',(-38.0548755041109,-85.265305410114,
80.0153149192114));
#211217=CARTESIAN_POINT('Ctrl Pts',(-38.1525428904009,-82.351605282947,
83.0238940611852));
#211218=CARTESIAN_POINT('Ctrl Pts',(-38.2502102766909,-78.60449376888,84.8949575070187));
#211219=CARTESIAN_POINT('Ctrl Pts',(-38.3153218675509,-75.8342138642759,
85.2426041509182));
#211220=CARTESIAN_POINT('Ctrl Pts',(-38.3478776629809,-74.4593099020373,
85.1816337132426));
#211221=CARTESIAN_POINT('Ctrl Pts',(-32.3212930507009,-79.4192347374965,
62.0755168906179));
#211222=CARTESIAN_POINT('Ctrl Pts',(-32.3538488461309,-80.6498714739172,
62.5738479625973));
#211223=CARTESIAN_POINT('Ctrl Pts',(-32.4189604369909,-82.9406351405637,
63.9906830308551));
#211224=CARTESIAN_POINT('Ctrl Pts',(-32.5166278232809,-85.4769223199675,
67.1360227552467));
#211225=CARTESIAN_POINT('Ctrl Pts',(-32.6142952095709,-86.8255373180291,
70.944784032297));
#211226=CARTESIAN_POINT('Ctrl Pts',(-32.7119625958609,-86.8336928790153,
74.9852609507784));
#211227=CARTESIAN_POINT('Ctrl Pts',(-32.8096299821509,-85.5004419587156,
78.7994383430527));
#211228=CARTESIAN_POINT('Ctrl Pts',(-32.9072973684309,-82.9769205267125,
81.9549646900448));
#211229=CARTESIAN_POINT('Ctrl Pts',(-33.0049647547209,-79.5491793382486,
84.0941463918273));
#211230=CARTESIAN_POINT('Ctrl Pts',(-33.1026321410109,-75.6057685340114,
84.9744978657157));
#211231=CARTESIAN_POINT('Ctrl Pts',(-33.2002995273009,-71.5936911480816,
84.4962273102156));
#211232=CARTESIAN_POINT('Ctrl Pts',(-33.2979669135909,-67.9677340244805,
82.7135488322342));
#211233=CARTESIAN_POINT('Ctrl Pts',(-33.3956342998809,-65.1389155189428,
79.8285369611779));
#211234=CARTESIAN_POINT('Ctrl Pts',(-33.4933016861709,-63.4278947906478,
76.1682206227875));
#211235=CARTESIAN_POINT('Ctrl Pts',(-33.5909690724609,-63.0286236472347,
72.1475129506798));
#211236=CARTESIAN_POINT('Ctrl Pts',(-33.6886364587509,-63.9863612484711,
68.2221790390764));
#211237=CARTESIAN_POINT('Ctrl Pts',(-33.7863038450409,-66.1925437782824,
64.8371729422473));
#211238=CARTESIAN_POINT('Ctrl Pts',(-33.8839712313309,-69.397090636349,
62.3762001539254));
#211239=CARTESIAN_POINT('Ctrl Pts',(-33.9816386176209,-73.2367521861339,
61.1182228832598));
#211240=CARTESIAN_POINT('Ctrl Pts',(-34.0793060039109,-77.2762857165359,
61.2058384479296));
#211241=CARTESIAN_POINT('Ctrl Pts',(-34.1769733902009,-81.0577921386458,
62.6291152340621));
#211242=CARTESIAN_POINT('Ctrl Pts',(-34.2746407764909,-84.1526208836926,
65.2267184888439));
#211243=CARTESIAN_POINT('Ctrl Pts',(-34.3723081627809,-86.2099593511533,
68.7041983321678));
#211244=CARTESIAN_POINT('Ctrl Pts',(-34.4699755490709,-86.9965990770434,
72.6673669599299));
#211245=CARTESIAN_POINT('Ctrl Pts',(-34.5676429353609,-86.4233709503677,
76.6669815845159));
#211246=CARTESIAN_POINT('Ctrl Pts',(-34.6653103216509,-84.5552529283401,
80.2496681025061));
#211247=CARTESIAN_POINT('Ctrl Pts',(-34.7629777079409,-81.6040044960209,
83.0093130653876));
#211248=CARTESIAN_POINT('Ctrl Pts',(-34.8606450942309,-77.9041627869953,
84.6330984448553));
#211249=CARTESIAN_POINT('Ctrl Pts',(-34.9583124805209,-73.8751213116633,
84.9369609474145));
#211250=CARTESIAN_POINT('Ctrl Pts',(-35.0559798668109,-69.9735898378284,
83.8864564071507));
#211251=CARTESIAN_POINT('Ctrl Pts',(-35.1536472531009,-66.6418243076185,
81.6006641851604));
#211252=CARTESIAN_POINT('Ctrl Pts',(-35.2513146393909,-64.2574951597656,
78.338688994402));
#211253=CARTESIAN_POINT('Ctrl Pts',(-35.3489820256809,-63.090876705969,
74.4702902282876));
#211254=CARTESIAN_POINT('Ctrl Pts',(-35.4466494119709,-63.2742103357459,
70.433968089186));
#211255=CARTESIAN_POINT('Ctrl Pts',(-35.5443167982609,-64.7867143669015,
66.6872576405196));
#211256=CARTESIAN_POINT('Ctrl Pts',(-35.6419841845509,-67.4569397416147,
63.6548651727437));
#211257=CARTESIAN_POINT('Ctrl Pts',(-35.7396515708509,-70.9822045395409,
61.6805258566954));
#211258=CARTESIAN_POINT('Ctrl Pts',(-35.8373189571409,-74.9629043194786,
60.9880398334549));
#211259=CARTESIAN_POINT('Ctrl Pts',(-35.9349863434309,-78.9478090597658,
61.6559034731573));
#211260=CARTESIAN_POINT('Ctrl Pts',(-36.0326537297209,-82.485212087779,
63.6084114623351));
#211261=CARTESIAN_POINT('Ctrl Pts',(-36.1303211160109,-85.1741330399482,
66.6242383378935));
#211262=CARTESIAN_POINT('Ctrl Pts',(-36.2279885023009,-86.7097707691124,
70.3615267125221));
#211263=CARTESIAN_POINT('Ctrl Pts',(-36.3256558885909,-86.9180539098912,
74.3966383297691));
#211264=CARTESIAN_POINT('Ctrl Pts',(-36.4233232748809,-85.7753726420844,
78.2721753442413));
#211265=CARTESIAN_POINT('Ctrl Pts',(-36.5209906611709,-83.4112549687333,
81.5488284013896));
#211266=CARTESIAN_POINT('Ctrl Pts',(-36.6186580474609,-80.0936841410099,
83.8551743063604));
#211267=CARTESIAN_POINT('Ctrl Pts',(-36.7163254337509,-76.1987215650125,
84.9297784948444));
#211268=CARTESIAN_POINT('Ctrl Pts',(-36.8139928200409,-72.1678785690723,
84.6508298034518));
#211269=CARTESIAN_POINT('Ctrl Pts',(-36.9116602063309,-68.4580691313762,
83.0499483068092));
#211270=CARTESIAN_POINT('Ctrl Pts',(-37.0093275926209,-65.489816648677,
80.3086010414542));
#211271=CARTESIAN_POINT('Ctrl Pts',(-37.1069949789109,-63.5995857392998,
76.7375319102927));
#211272=CARTESIAN_POINT('Ctrl Pts',(-37.2046623652009,-63.0016424824015,
72.7415374793882));
#211273=CARTESIAN_POINT('Ctrl Pts',(-37.3023297514909,-63.7637664051097,
68.7735814871057));
#211274=CARTESIAN_POINT('Ctrl Pts',(-37.3999971377809,-65.7995673717778,
65.2834493901101));
#211275=CARTESIAN_POINT('Ctrl Pts',(-37.4976645240709,-68.8782782897348,
62.6667631817017));
#211276=CARTESIAN_POINT('Ctrl Pts',(-37.5953319103609,-72.6509135864917,
61.2201358796829));
#211277=CARTESIAN_POINT('Ctrl Pts',(-37.6929992966509,-76.6898282723673,
61.1075491215586));
#211278=CARTESIAN_POINT('Ctrl Pts',(-37.7906666829409,-80.5371934162449,
62.3417651174235));
#211279=CARTESIAN_POINT('Ctrl Pts',(-37.8883340692309,-83.7568930367679,
64.7828799942741));
#211280=CARTESIAN_POINT('Ctrl Pts',(-37.9860014555209,-85.9839599898376,
68.1541825310842));
#211281=CARTESIAN_POINT('Ctrl Pts',(-38.0836688418109,-86.9659458647775,
72.0735205728459));
#211282=CARTESIAN_POINT('Ctrl Pts',(-38.1813362281009,-86.5915399428526,
76.0966198012583));
#211283=CARTESIAN_POINT('Ctrl Pts',(-38.2790036143909,-84.9031762805598,
79.7674437395071));
#211284=CARTESIAN_POINT('Ctrl Pts',(-38.3766710006809,-82.092262738757,
82.669889249567));
#211285=CARTESIAN_POINT('Ctrl Pts',(-38.4743383869709,-78.4773380595411,
84.4749471992291));
#211286=CARTESIAN_POINT('Ctrl Pts',(-38.5394499778309,-75.804785305799,
84.8103299141412));
#211287=CARTESIAN_POINT('Ctrl Pts',(-38.5720057732609,-74.4783838240209,
84.7515103303026));
#211288=CARTESIAN_POINT('',(-37.8135594354587,-79.7260345616507,85.0994033094111));
#211289=CARTESIAN_POINT('Ctrl Pts',(-37.8135412566022,-79.7265008243874,
85.0992154535007));
#211290=CARTESIAN_POINT('Ctrl Pts',(-37.9141945917161,-79.656190438583,
84.9191034084108));
#211291=CARTESIAN_POINT('Ctrl Pts',(-38.0148480643992,-79.5858805128641,
84.7389909011183));
#211292=CARTESIAN_POINT('Ctrl Pts',(-38.2164814622351,-79.4450337333417,
84.3781812915445));
#211293=CARTESIAN_POINT('Ctrl Pts',(-38.3174616202436,-79.3744967204846,
84.1974837711852));
#211294=CARTESIAN_POINT('Ctrl Pts',(-38.4184416307607,-79.3039603665244,
84.0167862995282));
#211295=CARTESIAN_POINT('',(-31.8032830015106,-84.3356921461145,63.942145982536));
#211296=CARTESIAN_POINT('Ctrl Pts',(-36.4473639743914,-62.9850802944281,
77.9529305295057));
#211297=CARTESIAN_POINT('Ctrl Pts',(-36.4543241802223,-62.8662959481017,
77.665425985869));
#211298=CARTESIAN_POINT('Ctrl Pts',(-36.4612900402069,-62.7578055866838,
77.3735961326477));
#211299=CARTESIAN_POINT('Ctrl Pts',(-36.485117930428,-62.4205173636423,
76.355723017862));
#211300=CARTESIAN_POINT('Ctrl Pts',(-36.5017296931877,-62.2450550777804,
75.6138349173405));
#211301=CARTESIAN_POINT('Ctrl Pts',(-36.5357274612721,-62.0247013039446,
74.0995341640204));
#211302=CARTESIAN_POINT('Ctrl Pts',(-36.5530476473795,-61.981718828881,
73.329864494191));
#211303=CARTESIAN_POINT('Ctrl Pts',(-36.5916197209741,-62.0390359146387,
71.5897218188896));
#211304=CARTESIAN_POINT('Ctrl Pts',(-36.6128801976632,-62.1798186416409,
70.6251596328269));
#211305=CARTESIAN_POINT('Ctrl Pts',(-36.6439294954884,-62.5328099313688,
69.281688088584));
#211306=CARTESIAN_POINT('Ctrl Pts',(-36.6532881833061,-62.6582388994359,
68.8833927198607));
#211307=CARTESIAN_POINT('Ctrl Pts',(-36.6809267326242,-63.0881923767221,
67.7172302332754));
#211308=CARTESIAN_POINT('Ctrl Pts',(-36.6989314919195,-63.4469139763311,
66.9716008860826));
#211309=CARTESIAN_POINT('Ctrl Pts',(-36.7364395657127,-64.3189605283735,
65.5286083221384));
#211310=CARTESIAN_POINT('Ctrl Pts',(-36.7557782652972,-64.8360286904484,
64.8381780403023));
#211311=CARTESIAN_POINT('Ctrl Pts',(-36.7839612892329,-65.6992197482852,
63.8966248022828));
#211312=CARTESIAN_POINT('Ctrl Pts',(-36.7931293056665,-65.9955511341076,
63.6030655527872));
#211313=CARTESIAN_POINT('Ctrl Pts',(-36.8208453918513,-66.9263589877273,
62.7656896735039));
#211314=CARTESIAN_POINT('Ctrl Pts',(-36.8396120669197,-67.5996227911344,
62.2682600303921));
#211315=CARTESIAN_POINT('Ctrl Pts',(-36.8761230715828,-69.0081416355683,
61.4238997206659));
#211316=CARTESIAN_POINT('Ctrl Pts',(-36.8937294894461,-69.7374966540635,
61.074300943056));
#211317=CARTESIAN_POINT('Ctrl Pts',(-36.9308123211814,-71.3016845990245,
60.4963768345923));
#211318=CARTESIAN_POINT('Ctrl Pts',(-36.9501609036144,-72.1364439111921,
60.2790324585819));
#211319=CARTESIAN_POINT('Ctrl Pts',(-36.978330496994,-73.3974509651564,
60.0813397198586));
#211320=CARTESIAN_POINT('Ctrl Pts',(-36.9874757398909,-73.8112215024371,
60.0366769320551));
#211321=CARTESIAN_POINT('Ctrl Pts',(-37.0151974403007,-75.0617540677333,
59.9621303772785));
#211322=CARTESIAN_POINT('Ctrl Pts',(-37.033990966252,-75.8999419217079,
59.993107255278));
#211323=CARTESIAN_POINT('Ctrl Pts',(-37.0719276034909,-77.5900391620661,
60.2199469355597));
#211324=CARTESIAN_POINT('Ctrl Pts',(-37.0908557950954,-78.4370257822214,
60.4214292563707));
#211325=CARTESIAN_POINT('Ctrl Pts',(-37.1293461869287,-80.0703946238553,
60.9875916109183));
#211326=CARTESIAN_POINT('Ctrl Pts',(-37.1486534495965,-80.8532460091769,
61.3493201333601));
#211327=CARTESIAN_POINT('Ctrl Pts',(-37.176861062698,-81.9555297796532,
61.9981658508267));
#211328=CARTESIAN_POINT('Ctrl Pts',(-37.1860769038382,-82.305971777073,
62.2279333725017));
#211329=CARTESIAN_POINT('Ctrl Pts',(-37.2143986726791,-83.3398725112968,
62.9796324327799));
#211330=CARTESIAN_POINT('Ctrl Pts',(-37.2337467737194,-83.9831984350049,
63.5527441000205));
#211331=CARTESIAN_POINT('Ctrl Pts',(-37.2730206552509,-85.1829821911235,
64.8563039758477));
#211332=CARTESIAN_POINT('Ctrl Pts',(-37.2929574213215,-85.7283677887833,
65.5906324615143));
#211333=CARTESIAN_POINT('Ctrl Pts',(-37.3226165148976,-86.4041788015047,
66.7344460687353));
#211334=CARTESIAN_POINT('Ctrl Pts',(-37.331952372424,-86.5986311571669,
67.1028796803519));
#211335=CARTESIAN_POINT('Ctrl Pts',(-37.3691472807876,-87.3053212567826,
68.6134082064923));
#211336=CARTESIAN_POINT('Ctrl Pts',(-37.3963711391022,-87.6691654605218,
69.8174527414559));
#211337=CARTESIAN_POINT('Ctrl Pts',(-37.4337911968826,-87.9179781646002,
71.4712655513977));
#211338=CARTESIAN_POINT('Ctrl Pts',(-37.4432018905373,-87.9603582315639,
71.8904995638018));
#211339=CARTESIAN_POINT('Ctrl Pts',(-37.4666736267226,-88.0157060709946,
72.9505504624398));
#211340=CARTESIAN_POINT('Ctrl Pts',(-37.4807126142551,-88.0017984756817,
73.591643275133));
#211341=CARTESIAN_POINT('Ctrl Pts',(-37.5120280994412,-87.8673101327979,
74.9949391007185));
#211342=CARTESIAN_POINT('Ctrl Pts',(-37.5293477014922,-87.7260732777811,
75.7527569995565));
#211343=CARTESIAN_POINT('Ctrl Pts',(-37.5673950034065,-87.2631759441533,
77.4061926447705));
#211344=CARTESIAN_POINT('Ctrl Pts',(-37.5881189354855,-86.9086724029588,
78.2880952478141));
#211345=CARTESIAN_POINT('Ctrl Pts',(-37.6177617346494,-86.2825812137115,
79.457820072434));
#211346=CARTESIAN_POINT('Ctrl Pts',(-37.6262594874007,-86.0891590173064,
79.7840534963821));
#211347=CARTESIAN_POINT('Ctrl Pts',(-37.6615797474437,-85.2225597219804,
81.1099098905177));
#211348=CARTESIAN_POINT('Ctrl Pts',(-37.6877898088874,-84.4263406844536,
82.0219288772879));
#211349=CARTESIAN_POINT('Ctrl Pts',(-37.7230062828639,-83.2369419520325,
83.0531423108285));
#211350=CARTESIAN_POINT('Ctrl Pts',(-37.7312775772375,-82.9477112373158,
83.2830764354318));
#211351=CARTESIAN_POINT('Ctrl Pts',(-37.7642212958841,-81.7474044354274,
84.1565247586272));
#211352=CARTESIAN_POINT('Ctrl Pts',(-37.7885929278986,-80.7650329325693,
84.6939292153208));
#211353=CARTESIAN_POINT('Ctrl Pts',(-37.8135449901798,-79.7261875999371,
85.0993456443021));
#211354=CARTESIAN_POINT('Ctrl Pts',(-37.7678684231509,-80.2245721714987,
84.9428528583424));
#211355=CARTESIAN_POINT('Ctrl Pts',(-37.8179054464809,-78.1874891607719,
85.9277583999695));
#211356=CARTESIAN_POINT('Ctrl Pts',(-37.9179794931409,-73.5482212730369,
86.8316803850282));
#211357=CARTESIAN_POINT('Ctrl Pts',(-38.0680905631309,-66.7022463072535,
84.5014189876433));
#211358=CARTESIAN_POINT('Ctrl Pts',(-38.2182016331209,-61.8311972113564,
78.9684584806007));
#211359=CARTESIAN_POINT('Ctrl Pts',(-38.3182756797809,-60.8302931416496,
74.0638248418014));
#211360=CARTESIAN_POINT('Ctrl Pts',(-38.3683127031109,-60.9803062607213,
71.6256255348517));
#211361=CARTESIAN_POINT('Ctrl Pts',(-37.9919965334309,-80.0521476485986,
84.5483408522442));
#211362=CARTESIAN_POINT('Ctrl Pts',(-38.0420335567609,-78.0834391555961,
85.5033627821869));
#211363=CARTESIAN_POINT('Ctrl Pts',(-38.1421076034109,-73.5967117403114,
86.3839207906894));
#211364=CARTESIAN_POINT('Ctrl Pts',(-38.2922186734109,-66.9668082009882,
84.1369185523978));
#211365=CARTESIAN_POINT('Ctrl Pts',(-38.4423297434009,-62.2418829099991,
78.7835876157209));
#211366=CARTESIAN_POINT('Ctrl Pts',(-38.5424037900609,-61.2660399523217,
74.0312248270541));
#211367=CARTESIAN_POINT('Ctrl Pts',(-38.5924408133809,-61.4088311706314,
71.6672949557471));
#211368=CARTESIAN_POINT('Ctrl Pts',(-38.2161246437009,-79.8797231256986,
84.1538288461459));
#211369=CARTESIAN_POINT('Ctrl Pts',(-38.2661616670309,-77.9793891504164,
85.078967164395));
#211370=CARTESIAN_POINT('Ctrl Pts',(-38.3662357136909,-73.645202207582,
85.9361611963413));
#211371=CARTESIAN_POINT('Ctrl Pts',(-38.5163467836809,-67.2313700947256,
83.7724181171587));
#211372=CARTESIAN_POINT('Ctrl Pts',(-38.6664578536809,-62.652568608624,
78.5987167508506));
#211373=CARTESIAN_POINT('Ctrl Pts',(-38.7665319003309,-61.7017867629931,
73.998624812305));
#211374=CARTESIAN_POINT('Ctrl Pts',(-38.8165689236609,-61.8373560805414,
71.7089643766425));
#211375=CARTESIAN_POINT('Ctrl Pts',(-38.4402527539809,-79.7072986027986,
83.7593168400476));
#211376=CARTESIAN_POINT('Ctrl Pts',(-38.4902897773109,-77.8753391452405,
84.6545715466123));
#211377=CARTESIAN_POINT('Ctrl Pts',(-38.5903638239709,-73.6936926748527,
85.4884016019933));
#211378=CARTESIAN_POINT('Ctrl Pts',(-38.7404748939609,-67.49593198846,83.4079176819122));
#211379=CARTESIAN_POINT('Ctrl Pts',(-38.8905859639509,-63.0632543072575,
78.4138458859746));
#211380=CARTESIAN_POINT('Ctrl Pts',(-38.9906600106109,-62.1375335736656,
73.9660247975586));
#211381=CARTESIAN_POINT('Ctrl Pts',(-39.0406970339409,-62.2658809904518,
71.7506337975388));
#211382=CARTESIAN_POINT('Ctrl Pts',(-38.9114901698969,-62.0210675377945,
72.2490839199139));
#211383=CARTESIAN_POINT('Ctrl Pts',(-38.9253796493603,-62.0477053299784,
72.2506022870319));
#211384=CARTESIAN_POINT('Ctrl Pts',(-38.9392691288105,-62.0743431221692,
72.2521206541503));
#211385=CARTESIAN_POINT('Ctrl Pts',(-38.9670676750248,-62.1276562719404,
72.2551595296326));
#211386=CARTESIAN_POINT('Ctrl Pts',(-38.9809767417889,-62.1543316295209,
72.2566800379965));
#211387=CARTESIAN_POINT('Ctrl Pts',(-38.9948858085393,-62.1810069871086,
72.2582005463609));
#211388=CARTESIAN_POINT('Ctrl Pts',(-38.6651607695592,-62.9850797267618,
77.9529291555313));
#211389=CARTESIAN_POINT('Ctrl Pts',(-38.61247162501,-63.4651597069569,79.1149107179876));
#211390=CARTESIAN_POINT('Ctrl Pts',(-38.5579303068348,-64.1112609851083,
80.2010992341744));
#211391=CARTESIAN_POINT('Ctrl Pts',(-38.4509479952484,-65.7059259388704,
82.1673583393617));
#211392=CARTESIAN_POINT('Ctrl Pts',(-38.3992043907891,-66.6498484985761,
83.0337413163219));
#211393=CARTESIAN_POINT('Ctrl Pts',(-38.3094997884852,-68.3950020381939,
84.2169638927091));
#211394=CARTESIAN_POINT('Ctrl Pts',(-38.2735339351584,-69.1287945259406,
84.6175018705529));
#211395=CARTESIAN_POINT('Ctrl Pts',(-38.166422504845,-71.447408923872,85.6073284218056));
#211396=CARTESIAN_POINT('Ctrl Pts',(-38.0982006061265,-73.1130898711673,
85.9613759922044));
#211397=CARTESIAN_POINT('Ctrl Pts',(-37.9903150495058,-75.6328782495681,
86.0001753956267));
#211398=CARTESIAN_POINT('Ctrl Pts',(-37.9546993734579,-76.4652312027286,
85.9328938291295));
#211399=CARTESIAN_POINT('Ctrl Pts',(-37.8839532152002,-78.1193429154257,
85.6374986271243));
#211400=CARTESIAN_POINT('Ctrl Pts',(-37.8490190852945,-78.9367127274665,
85.4074198623626));
#211401=CARTESIAN_POINT('Ctrl Pts',(-37.8135657720877,-79.7258720358075,
85.0994687906041));
#211402=CARTESIAN_POINT('Origin',(-39.1448867524609,-61.0226881170831,72.1921758070624));
#211403=CARTESIAN_POINT('Ctrl Pts',(-39.2948856686008,-62.1810067175759,
72.2582005309974));
#211404=CARTESIAN_POINT('Ctrl Pts',(-39.3087857943346,-62.1543485130583,
72.2566810003664));
#211405=CARTESIAN_POINT('Ctrl Pts',(-39.3226859200676,-62.1276903085403,
72.2551614697354));
#211406=CARTESIAN_POINT('Ctrl Pts',(-39.3504844252439,-62.0743772486039,
72.2521225993737));
#211407=CARTESIAN_POINT('Ctrl Pts',(-39.3643828046871,-62.0477223931856,
72.250603259643));
#211408=CARTESIAN_POINT('Ctrl Pts',(-39.3782811841296,-62.0210675377669,
72.2490839199123));
#211409=CARTESIAN_POINT('Ctrl Pts',(-38.6717262017909,-79.7072986027985,
83.7593168400477));
#211410=CARTESIAN_POINT('Ctrl Pts',(-38.7217632251209,-77.8753391452405,
84.6545715466123));
#211411=CARTESIAN_POINT('Ctrl Pts',(-38.8218372717809,-73.6936926748527,
85.4884016019933));
#211412=CARTESIAN_POINT('Ctrl Pts',(-38.9719483417709,-67.49593198846,83.4079176819122));
#211413=CARTESIAN_POINT('Ctrl Pts',(-39.1220594117609,-63.0632543072574,
78.4138458859745));
#211414=CARTESIAN_POINT('Ctrl Pts',(-39.2221334584209,-62.1375335736652,
73.9660247975577));
#211415=CARTESIAN_POINT('Ctrl Pts',(-39.2721704817509,-62.2658809904518,
71.7506337975388));
#211416=CARTESIAN_POINT('Ctrl Pts',(-38.8958543120709,-79.8797231256985,
84.153828846146));
#211417=CARTESIAN_POINT('Ctrl Pts',(-38.9458913354009,-77.9793891504164,
85.078967164395));
#211418=CARTESIAN_POINT('Ctrl Pts',(-39.0459653820509,-73.645202207582,
85.9361611963413));
#211419=CARTESIAN_POINT('Ctrl Pts',(-39.1960764520509,-67.2313700947253,
83.7724181171577));
#211420=CARTESIAN_POINT('Ctrl Pts',(-39.3461875220409,-62.652568608624,
78.5987167508506));
#211421=CARTESIAN_POINT('Ctrl Pts',(-39.4462615687009,-61.7017867629931,
73.998624812305));
#211422=CARTESIAN_POINT('Ctrl Pts',(-39.4962985920209,-61.8373560805414,
71.7089643766425));
#211423=CARTESIAN_POINT('Ctrl Pts',(-39.1199824223409,-80.0521476485985,
84.5483408522443));
#211424=CARTESIAN_POINT('Ctrl Pts',(-39.1700194456709,-78.0834391555961,
85.5033627821869));
#211425=CARTESIAN_POINT('Ctrl Pts',(-39.2700934923309,-73.5967117403114,
86.3839207906894));
#211426=CARTESIAN_POINT('Ctrl Pts',(-39.4202045623209,-66.9668082009882,
84.1369185523978));
#211427=CARTESIAN_POINT('Ctrl Pts',(-39.5703156323209,-62.241882909999,
78.7835876157208));
#211428=CARTESIAN_POINT('Ctrl Pts',(-39.6703896789709,-61.2660399523217,
74.0312248270541));
#211429=CARTESIAN_POINT('Ctrl Pts',(-39.7204267023009,-61.4088311706314,
71.6672949557471));
#211430=CARTESIAN_POINT('Ctrl Pts',(-39.3441105326209,-80.2245721714985,
84.9428528583425));
#211431=CARTESIAN_POINT('Ctrl Pts',(-39.3941475559509,-78.1874891607719,
85.9277583999695));
#211432=CARTESIAN_POINT('Ctrl Pts',(-39.4942216026109,-73.5482212730369,
86.8316803850282));
#211433=CARTESIAN_POINT('Ctrl Pts',(-39.6443326726009,-66.7022463072535,
84.5014189876433));
#211434=CARTESIAN_POINT('Ctrl Pts',(-39.7944437425909,-61.8311972113564,
78.9684584806006));
#211435=CARTESIAN_POINT('Ctrl Pts',(-39.8945177892509,-60.8302931416493,
74.0638248418005));
#211436=CARTESIAN_POINT('Ctrl Pts',(-39.9445548125809,-60.9803062607213,
71.6256255348517));
#211437=CARTESIAN_POINT('Ctrl Pts',(-38.7166027955228,-79.3038821947565,
84.0168244534335));
#211438=CARTESIAN_POINT('Ctrl Pts',(-38.8175042526392,-79.3743616523911,
84.1973833874513));
#211439=CARTESIAN_POINT('Ctrl Pts',(-38.918405870868,-79.4448417742437,
84.3779423951187));
#211440=CARTESIAN_POINT('Ctrl Pts',(-39.1200383310617,-79.5856838366802,
84.7387543832486));
#211441=CARTESIAN_POINT('Ctrl Pts',(-39.220769502857,-79.6560460057835,
84.9190079546549));
#211442=CARTESIAN_POINT('Ctrl Pts',(-39.3215005357773,-79.7264086317985,
85.0992610619778));
#211443=CARTESIAN_POINT('Ctrl Pts',(-32.5527664985109,-79.4192347374965,
62.0755168906179));
#211444=CARTESIAN_POINT('Ctrl Pts',(-32.5853222939409,-80.6498714739172,
62.5738479625973));
#211445=CARTESIAN_POINT('Ctrl Pts',(-32.6504338848009,-82.9406351405637,
63.9906830308551));
#211446=CARTESIAN_POINT('Ctrl Pts',(-32.7481012710909,-85.4769223199675,
67.1360227552467));
#211447=CARTESIAN_POINT('Ctrl Pts',(-32.8457686573809,-86.8255373180291,
70.944784032297));
#211448=CARTESIAN_POINT('Ctrl Pts',(-32.9434360436709,-86.8336928790153,
74.9852609507784));
#211449=CARTESIAN_POINT('Ctrl Pts',(-33.0411034299609,-85.5004419587156,
78.7994383430527));
#211450=CARTESIAN_POINT('Ctrl Pts',(-33.1387708162509,-82.9769205267125,
81.9549646900448));
#211451=CARTESIAN_POINT('Ctrl Pts',(-33.2364382025409,-79.5491793382486,
84.0941463918273));
#211452=CARTESIAN_POINT('Ctrl Pts',(-33.3341055888209,-75.6057685340114,
84.9744978657157));
#211453=CARTESIAN_POINT('Ctrl Pts',(-33.4317729751109,-71.5936911480816,
84.4962273102156));
#211454=CARTESIAN_POINT('Ctrl Pts',(-33.5294403614009,-67.9677340244805,
82.7135488322342));
#211455=CARTESIAN_POINT('Ctrl Pts',(-33.6271077476909,-65.1389155189428,
79.8285369611779));
#211456=CARTESIAN_POINT('Ctrl Pts',(-33.7247751339809,-63.4278947906478,
76.1682206227875));
#211457=CARTESIAN_POINT('Ctrl Pts',(-33.8224425202709,-63.0286236472347,
72.1475129506798));
#211458=CARTESIAN_POINT('Ctrl Pts',(-33.9201099065609,-63.9863612484711,
68.2221790390764));
#211459=CARTESIAN_POINT('Ctrl Pts',(-34.0177772928509,-66.1925437782824,
64.8371729422473));
#211460=CARTESIAN_POINT('Ctrl Pts',(-34.1154446791409,-69.397090636349,
62.3762001539254));
#211461=CARTESIAN_POINT('Ctrl Pts',(-34.2131120654309,-73.2367521861339,
61.1182228832598));
#211462=CARTESIAN_POINT('Ctrl Pts',(-34.3107794517209,-77.2762857165359,
61.2058384479296));
#211463=CARTESIAN_POINT('Ctrl Pts',(-34.4084468380109,-81.0577921386454,
62.6291152340612));
#211464=CARTESIAN_POINT('Ctrl Pts',(-34.5061142243009,-84.1526208836926,
65.2267184888439));
#211465=CARTESIAN_POINT('Ctrl Pts',(-34.6037816105909,-86.2099593511533,
68.7041983321678));
#211466=CARTESIAN_POINT('Ctrl Pts',(-34.7014489968809,-86.9965990770434,
72.6673669599299));
#211467=CARTESIAN_POINT('Ctrl Pts',(-34.7991163831709,-86.4233709503677,
76.6669815845159));
#211468=CARTESIAN_POINT('Ctrl Pts',(-34.8967837694509,-84.5552529283401,
80.2496681025061));
#211469=CARTESIAN_POINT('Ctrl Pts',(-34.9944511557409,-81.6040044960209,
83.0093130653876));
#211470=CARTESIAN_POINT('Ctrl Pts',(-35.0921185420309,-77.9041627869953,
84.6330984448553));
#211471=CARTESIAN_POINT('Ctrl Pts',(-35.1897859283209,-73.8751213116633,
84.9369609474145));
#211472=CARTESIAN_POINT('Ctrl Pts',(-35.2874533146109,-69.9735898378284,
83.8864564071507));
#211473=CARTESIAN_POINT('Ctrl Pts',(-35.3851207009009,-66.6418243076185,
81.6006641851604));
#211474=CARTESIAN_POINT('Ctrl Pts',(-35.4827880871909,-64.2574951597656,
78.3386889944021));
#211475=CARTESIAN_POINT('Ctrl Pts',(-35.5804554734809,-63.090876705969,
74.4702902282876));
#211476=CARTESIAN_POINT('Ctrl Pts',(-35.6781228597709,-63.2742103357459,
70.433968089186));
#211477=CARTESIAN_POINT('Ctrl Pts',(-35.7757902460609,-64.7867143669015,
66.6872576405196));
#211478=CARTESIAN_POINT('Ctrl Pts',(-35.8734576323509,-67.4569397416147,
63.6548651727437));
#211479=CARTESIAN_POINT('Ctrl Pts',(-35.9711250186409,-70.982204539541,
61.6805258566954));
#211480=CARTESIAN_POINT('Ctrl Pts',(-36.0687924049309,-74.9629043194786,
60.9880398334549));
#211481=CARTESIAN_POINT('Ctrl Pts',(-36.1664597912209,-78.9478090597658,
61.6559034731573));
#211482=CARTESIAN_POINT('Ctrl Pts',(-36.2641271775109,-82.485212087779,
63.6084114623351));
#211483=CARTESIAN_POINT('Ctrl Pts',(-36.3617945638009,-85.1741330399482,
66.6242383378935));
#211484=CARTESIAN_POINT('Ctrl Pts',(-36.4594619500909,-86.7097707691124,
70.3615267125221));
#211485=CARTESIAN_POINT('Ctrl Pts',(-36.5571293363809,-86.9180539098912,
74.3966383297691));
#211486=CARTESIAN_POINT('Ctrl Pts',(-36.6547967226709,-85.7753726420844,
78.2721753442413));
#211487=CARTESIAN_POINT('Ctrl Pts',(-36.7524641089609,-83.4112549687333,
81.5488284013896));
#211488=CARTESIAN_POINT('Ctrl Pts',(-36.8501314952509,-80.0936841410099,
83.8551743063604));
#211489=CARTESIAN_POINT('Ctrl Pts',(-36.9477988815409,-76.1987215650125,
84.9297784948444));
#211490=CARTESIAN_POINT('Ctrl Pts',(-37.0454662678409,-72.1678785690723,
84.6508298034518));
#211491=CARTESIAN_POINT('Ctrl Pts',(-37.1431336541309,-68.4580691313762,
83.0499483068092));
#211492=CARTESIAN_POINT('Ctrl Pts',(-37.2408010404209,-65.489816648677,
80.3086010414542));
#211493=CARTESIAN_POINT('Ctrl Pts',(-37.3384684267109,-63.5995857392998,
76.7375319102927));
#211494=CARTESIAN_POINT('Ctrl Pts',(-37.4361358130009,-63.0016424824015,
72.7415374793882));
#211495=CARTESIAN_POINT('Ctrl Pts',(-37.5338031992909,-63.7637664051097,
68.7735814871057));
#211496=CARTESIAN_POINT('Ctrl Pts',(-37.6314705855809,-65.7995673717778,
65.2834493901101));
#211497=CARTESIAN_POINT('Ctrl Pts',(-37.7291379718709,-68.8782782897348,
62.6667631817017));
#211498=CARTESIAN_POINT('Ctrl Pts',(-37.8268053581609,-72.6509135864917,
61.2201358796829));
#211499=CARTESIAN_POINT('Ctrl Pts',(-37.9244727444509,-76.6898282723673,
61.1075491215586));
#211500=CARTESIAN_POINT('Ctrl Pts',(-38.0221401307409,-80.5371934162449,
62.3417651174235));
#211501=CARTESIAN_POINT('Ctrl Pts',(-38.1198075170309,-83.7568930367679,
64.7828799942741));
#211502=CARTESIAN_POINT('Ctrl Pts',(-38.2174749033309,-85.9839599898376,
68.1541825310842));
#211503=CARTESIAN_POINT('Ctrl Pts',(-38.3151422896209,-86.9659458647775,
72.0735205728459));
#211504=CARTESIAN_POINT('Ctrl Pts',(-38.4128096759109,-86.5915399428526,
76.0966198012583));
#211505=CARTESIAN_POINT('Ctrl Pts',(-38.5104770622009,-84.9031762805598,
79.7674437395071));
#211506=CARTESIAN_POINT('Ctrl Pts',(-38.6081444484909,-82.092262738757,
82.669889249567));
#211507=CARTESIAN_POINT('Ctrl Pts',(-38.7058118347809,-78.4773380595411,
84.4749471992291));
#211508=CARTESIAN_POINT('Ctrl Pts',(-38.7709234256409,-75.804785305799,
84.8103299141412));
#211509=CARTESIAN_POINT('Ctrl Pts',(-38.8034792210709,-74.4783838240209,
84.7515103303026));
#211510=CARTESIAN_POINT('Ctrl Pts',(-32.7768946087909,-79.5808327524621,
61.6764479484404));
#211511=CARTESIAN_POINT('Ctrl Pts',(-32.8094504042209,-80.8564701429687,
62.1930014767526));
#211512=CARTESIAN_POINT('Ctrl Pts',(-32.8745619950809,-83.2310000911753,
63.6616459075254));
#211513=CARTESIAN_POINT('Ctrl Pts',(-32.9722293813709,-85.8600316025557,
66.9220011687801));
#211514=CARTESIAN_POINT('Ctrl Pts',(-33.0698967676509,-87.2579613620154,
70.8700372973401));
#211515=CARTESIAN_POINT('Ctrl Pts',(-33.1675641539409,-87.2664151471337,
75.0582622057642));
#211516=CARTESIAN_POINT('Ctrl Pts',(-33.2652315402309,-85.8844112831762,
79.0119125004583));
#211517=CARTESIAN_POINT('Ctrl Pts',(-33.3628989265209,-83.2686123238737,
82.2828268782174));
#211518=CARTESIAN_POINT('Ctrl Pts',(-33.4605663128109,-79.7155290332633,
84.5002319687039));
#211519=CARTESIAN_POINT('Ctrl Pts',(-33.5582336991009,-75.6279196525717,
85.412775226709));
#211520=CARTESIAN_POINT('Ctrl Pts',(-33.6559010853909,-71.4691327614987,
84.9170157671447));
#211521=CARTESIAN_POINT('Ctrl Pts',(-33.7535684716809,-67.7105853800127,
83.0691501424084));
#211522=CARTESIAN_POINT('Ctrl Pts',(-33.8512358579709,-64.7783255588649,
80.0786421347598));
#211523=CARTESIAN_POINT('Ctrl Pts',(-33.9489032442609,-63.0047379904651,
76.2844791261684));
#211524=CARTESIAN_POINT('Ctrl Pts',(-34.0465706305509,-62.5908667119491,
72.1167463655193));
#211525=CARTESIAN_POINT('Ctrl Pts',(-34.1442380168409,-63.5836258733412,
68.0478748946176));
#211526=CARTESIAN_POINT('Ctrl Pts',(-34.2419054031309,-65.8704818089924,
64.5390893883721));
#211527=CARTESIAN_POINT('Ctrl Pts',(-34.3395727894109,-69.1922092292778,
61.9881262869918));
#211528=CARTESIAN_POINT('Ctrl Pts',(-34.4372401757009,-73.1722755598568,
60.6841486018049));
#211529=CARTESIAN_POINT('Ctrl Pts',(-34.5349075619909,-77.3595225833569,
60.7749680020175));
#211530=CARTESIAN_POINT('Ctrl Pts',(-34.6325749482809,-81.2793072295691,
62.2502897047617));
#211531=CARTESIAN_POINT('Ctrl Pts',(-34.7302423345709,-84.4873044781106,
64.9428794344855));
#211532=CARTESIAN_POINT('Ctrl Pts',(-34.8279097208609,-86.6198735753576,
68.5475201717517));
#211533=CARTESIAN_POINT('Ctrl Pts',(-34.9255771071509,-87.4352783308858,
72.6556098596655));
#211534=CARTESIAN_POINT('Ctrl Pts',(-35.0232444934409,-86.8410889896759,
76.8014782640016));
#211535=CARTESIAN_POINT('Ctrl Pts',(-35.1209118797309,-84.9046595558289,
80.5151727650388));
#211536=CARTESIAN_POINT('Ctrl Pts',(-35.2185792660209,-81.8454929166992,
83.3757295768015));
#211537=CARTESIAN_POINT('Ctrl Pts',(-35.3162466523109,-78.0103592145147,
85.0588918641796));
#211538=CARTESIAN_POINT('Ctrl Pts',(-35.4139140386009,-73.8339879087212,
85.3738656971173));
#211539=CARTESIAN_POINT('Ctrl Pts',(-35.5115814248909,-69.7897892585688,
84.2849473910144));
#211540=CARTESIAN_POINT('Ctrl Pts',(-35.6092488111809,-66.3361911650335,
81.9155706781227));
#211541=CARTESIAN_POINT('Ctrl Pts',(-35.7069161974709,-63.8646743296805,
78.5343149451387));
#211542=CARTESIAN_POINT('Ctrl Pts',(-35.8045835837609,-62.6553961762827,
74.5244605653652));
#211543=CARTESIAN_POINT('Ctrl Pts',(-35.9022509700509,-62.8454337610229,
70.3405423640074));
#211544=CARTESIAN_POINT('Ctrl Pts',(-35.9999183563409,-64.4132454785962,
66.4568260744839));
#211545=CARTESIAN_POINT('Ctrl Pts',(-36.0975857426309,-67.181112898978,
63.3135482085524));
#211546=CARTESIAN_POINT('Ctrl Pts',(-36.1952531289209,-70.8352859417533,
61.2670132900357));
#211547=CARTESIAN_POINT('Ctrl Pts',(-36.2929205152109,-74.9615478429283,
60.5492051525981));
#211548=CARTESIAN_POINT('Ctrl Pts',(-36.3905879015009,-79.0921684670951,
61.2414905405986));
#211549=CARTESIAN_POINT('Ctrl Pts',(-36.4882552877909,-82.7589235982165,
63.2653958268243));
#211550=CARTESIAN_POINT('Ctrl Pts',(-36.5859226740809,-85.5461702366482,
66.3915023470505));
#211551=CARTESIAN_POINT('Ctrl Pts',(-36.6835900603709,-87.1379615814165,
70.2654520258604));
#211552=CARTESIAN_POINT('Ctrl Pts',(-36.7812574466609,-87.3538610051255,
74.4481154402485));
#211553=CARTESIAN_POINT('Ctrl Pts',(-36.8789248329509,-86.1693953480258,
78.4653690924801));
#211554=CARTESIAN_POINT('Ctrl Pts',(-36.9765922192409,-83.7188290595022,
81.8618394169131));
#211555=CARTESIAN_POINT('Ctrl Pts',(-37.0742596055309,-80.2799447256819,
84.2525213986484));
#211556=CARTESIAN_POINT('Ctrl Pts',(-37.1719269918209,-76.2425551780386,
85.3664206040374));
#211557=CARTESIAN_POINT('Ctrl Pts',(-37.2695943781109,-72.064316475499,
85.0772716047946));
#211558=CARTESIAN_POINT('Ctrl Pts',(-37.3672617644009,-68.2188505550257,
83.4178507257861));
#211559=CARTESIAN_POINT('Ctrl Pts',(-37.4649291506909,-65.1420580789654,
80.57626070286));
#211560=CARTESIAN_POINT('Ctrl Pts',(-37.5625965369809,-63.1827071565181,
76.8746084012712));
#211561=CARTESIAN_POINT('Ctrl Pts',(-37.6602639232709,-62.5628989277203,
72.7324925701221));
#211562=CARTESIAN_POINT('Ctrl Pts',(-37.7579313095609,-63.3528914114806,
68.6194404582811));
#211563=CARTESIAN_POINT('Ctrl Pts',(-37.8555986958509,-65.4631354468294,
65.0016848127869));
#211564=CARTESIAN_POINT('Ctrl Pts',(-37.9532660821509,-68.6544254882255,
62.2893143236977));
#211565=CARTESIAN_POINT('Ctrl Pts',(-38.0509334684409,-72.5650146189264,
60.7897882474999));
#211566=CARTESIAN_POINT('Ctrl Pts',(-38.1486008547309,-76.7516201686318,
60.673084533));
#211567=CARTESIAN_POINT('Ctrl Pts',(-38.2462682410209,-80.7396717903781,
61.9524320656214));
#211568=CARTESIAN_POINT('Ctrl Pts',(-38.3439356273109,-84.0771060637059,
64.482811111911));
#211569=CARTESIAN_POINT('Ctrl Pts',(-38.4416030136009,-86.3856101026459,
67.9773919605015));
#211570=CARTESIAN_POINT('Ctrl Pts',(-38.5392703998909,-87.4035042235849,
72.0400483107849));
#211571=CARTESIAN_POINT('Ctrl Pts',(-38.6369377861809,-87.0154074123175,
76.2102600797002));
#211572=CARTESIAN_POINT('Ctrl Pts',(-38.7346051724709,-85.2653054101149,
80.015314919211));
#211573=CARTESIAN_POINT('Ctrl Pts',(-38.8322725587709,-82.351605282947,
83.0238940611852));
#211574=CARTESIAN_POINT('Ctrl Pts',(-38.9299399450609,-78.60449376888,84.8949575070187));
#211575=CARTESIAN_POINT('Ctrl Pts',(-38.9950515359209,-75.8342138642759,
85.2426041509182));
#211576=CARTESIAN_POINT('Ctrl Pts',(-39.0276073313509,-74.4593099020373,
85.1816337132426));
#211577=CARTESIAN_POINT('Ctrl Pts',(-33.0010227190609,-79.7424307674282,
61.2773790062616));
#211578=CARTESIAN_POINT('Ctrl Pts',(-33.0335785144909,-81.0630688120212,
61.8121549909075));
#211579=CARTESIAN_POINT('Ctrl Pts',(-33.0986901053509,-83.5213650417874,
63.3326087841966));
#211580=CARTESIAN_POINT('Ctrl Pts',(-33.1963574916409,-86.2431408851346,
66.7079795823174));
#211581=CARTESIAN_POINT('Ctrl Pts',(-33.2940248779309,-87.6903854059918,
70.7952905623852));
#211582=CARTESIAN_POINT('Ctrl Pts',(-33.3916922642209,-87.6991374152512,
75.1312634607482));
#211583=CARTESIAN_POINT('Ctrl Pts',(-33.4893596505109,-86.2683806076395,
79.2243866578649));
#211584=CARTESIAN_POINT('Ctrl Pts',(-33.5870270368009,-83.5603041210376,
82.610689066389));
#211585=CARTESIAN_POINT('Ctrl Pts',(-33.6846944230909,-79.8818787282825,
84.9063175455787));
#211586=CARTESIAN_POINT('Ctrl Pts',(-33.7823618093809,-75.6500707711405,
85.8510525877097));
#211587=CARTESIAN_POINT('Ctrl Pts',(-33.8800291956709,-71.3445743749261,
85.3378042240803));
#211588=CARTESIAN_POINT('Ctrl Pts',(-33.9776965819609,-67.4534367355484,
83.4247514525908));
#211589=CARTESIAN_POINT('Ctrl Pts',(-34.0753639682509,-64.4177355988012,
80.3287473083499));
#211590=CARTESIAN_POINT('Ctrl Pts',(-34.1730313545409,-62.5815811902788,
76.400737629567));
#211591=CARTESIAN_POINT('Ctrl Pts',(-34.2706987408209,-62.1531097766604,
72.0859797803774));
#211592=CARTESIAN_POINT('Ctrl Pts',(-34.3683661271109,-63.1808904982033,
67.8735707501784));
#211593=CARTESIAN_POINT('Ctrl Pts',(-34.4660335134009,-65.5484198396858,
64.2410058345145));
#211594=CARTESIAN_POINT('Ctrl Pts',(-34.5637008996909,-68.9873278221854,
61.6000524200778));
#211595=CARTESIAN_POINT('Ctrl Pts',(-34.6613682859809,-73.1077989335492,
60.2500743203519));
#211596=CARTESIAN_POINT('Ctrl Pts',(-34.7590356722709,-77.4427594501453,
60.3440975560973));
#211597=CARTESIAN_POINT('Ctrl Pts',(-34.8567030585609,-81.5008223204608,
61.871464175445));
#211598=CARTESIAN_POINT('Ctrl Pts',(-34.9543704448509,-84.8219880725154,
64.6590403800946));
#211599=CARTESIAN_POINT('Ctrl Pts',(-35.0520378311409,-87.0297877995459,
68.390842011297));
#211600=CARTESIAN_POINT('Ctrl Pts',(-35.1497052174309,-87.8739575847217,
72.6438527593594));
#211601=CARTESIAN_POINT('Ctrl Pts',(-35.2473726037209,-87.2588070289994,
76.9359749434431));
#211602=CARTESIAN_POINT('Ctrl Pts',(-35.3450399900109,-85.2540661833469,
80.7806774275269));
#211603=CARTESIAN_POINT('Ctrl Pts',(-35.4427073763009,-82.0869813374197,
83.7421460881762));
#211604=CARTESIAN_POINT('Ctrl Pts',(-35.5403747625909,-78.1165556420916,
85.4846852834909));
#211605=CARTESIAN_POINT('Ctrl Pts',(-35.6380421488809,-73.7928545058452,
85.8107704468362));
#211606=CARTESIAN_POINT('Ctrl Pts',(-35.7357095351709,-69.6059886793678,
84.6834383749047));
#211607=CARTESIAN_POINT('Ctrl Pts',(-35.8333769214609,-66.0305580224903,
82.2304771711338));
#211608=CARTESIAN_POINT('Ctrl Pts',(-35.9310443077509,-63.4718534996216,
78.729940895939));
#211609=CARTESIAN_POINT('Ctrl Pts',(-36.0287116940409,-62.2199156466047,
74.5786309025152));
#211610=CARTESIAN_POINT('Ctrl Pts',(-36.1263790803309,-62.4166571862875,
70.2471166389011));
#211611=CARTESIAN_POINT('Ctrl Pts',(-36.2240464666209,-64.0397765902539,
66.2263945085208));
#211612=CARTESIAN_POINT('Ctrl Pts',(-36.3217138529109,-66.9052860562882,
62.9722312444263));
#211613=CARTESIAN_POINT('Ctrl Pts',(-36.4193812392009,-70.6883673438916,
60.8535007234066));
#211614=CARTESIAN_POINT('Ctrl Pts',(-36.5170486254909,-74.9601913662926,
60.1103704717333));
#211615=CARTESIAN_POINT('Ctrl Pts',(-36.6147160117809,-79.2365278743448,
60.8270776080123));
#211616=CARTESIAN_POINT('Ctrl Pts',(-36.7123833980709,-83.032635108598,
62.9223801912564));
#211617=CARTESIAN_POINT('Ctrl Pts',(-36.8100507843609,-85.9182074332976,
66.1587663561375));
#211618=CARTESIAN_POINT('Ctrl Pts',(-36.9077181706509,-87.566152393697,
70.1693773391154));
#211619=CARTESIAN_POINT('Ctrl Pts',(-37.0053855569409,-87.7896681003677,
74.4995925506423));
#211620=CARTESIAN_POINT('Ctrl Pts',(-37.1030529432309,-86.5634180540064,
78.6585628406411));
#211621=CARTESIAN_POINT('Ctrl Pts',(-37.2007203295209,-84.0264031503354,
82.1748504323777));
#211622=CARTESIAN_POINT('Ctrl Pts',(-37.2983877158209,-80.4662053104341,
84.6498684909032));
#211623=CARTESIAN_POINT('Ctrl Pts',(-37.3960551021109,-76.2863887911529,
85.8030627132264));
#211624=CARTESIAN_POINT('Ctrl Pts',(-37.4937224884009,-71.9607543820079,
85.5037134061586));
#211625=CARTESIAN_POINT('Ctrl Pts',(-37.5913898746909,-67.9796319787588,
83.7857531448031));
#211626=CARTESIAN_POINT('Ctrl Pts',(-37.6890572609809,-64.7942995092932,
80.8439203643351));
#211627=CARTESIAN_POINT('Ctrl Pts',(-37.7867246472709,-62.7658285737666,
77.0116848923228));
#211628=CARTESIAN_POINT('Ctrl Pts',(-37.8843920335609,-62.1241553730382,
72.723447660932));
#211629=CARTESIAN_POINT('Ctrl Pts',(-37.9820594198509,-62.9420164178251,
68.4652994295259));
#211630=CARTESIAN_POINT('Ctrl Pts',(-38.0797268061409,-65.126703521839,
64.7199202355243));
#211631=CARTESIAN_POINT('Ctrl Pts',(-38.1773941924309,-68.4305726866551,
61.9118654657189));
#211632=CARTESIAN_POINT('Ctrl Pts',(-38.2750615787209,-72.479115651301,
60.359440615331));
#211633=CARTESIAN_POINT('Ctrl Pts',(-38.3727289650109,-76.8134120648424,
60.238619944442));
#211634=CARTESIAN_POINT('Ctrl Pts',(-38.4703963513009,-80.9421501644669,
61.5630990137955));
#211635=CARTESIAN_POINT('Ctrl Pts',(-38.5680637375909,-84.397319090609,
64.1827422295159));
#211636=CARTESIAN_POINT('Ctrl Pts',(-38.6657311238809,-86.7872602154302,
67.8006013898866));
#211637=CARTESIAN_POINT('Ctrl Pts',(-38.7633985101709,-87.8410625823901,
72.0065760486924));
#211638=CARTESIAN_POINT('Ctrl Pts',(-38.8610658964609,-87.4392748817876,
76.3239003581206));
#211639=CARTESIAN_POINT('Ctrl Pts',(-38.9587332827509,-85.6274345396819,
80.2631860989099));
#211640=CARTESIAN_POINT('Ctrl Pts',(-39.0564006690409,-82.6109478271435,
83.3778988728008));
#211641=CARTESIAN_POINT('Ctrl Pts',(-39.1540680553309,-78.7316494782208,
85.3149678148182));
#211642=CARTESIAN_POINT('Ctrl Pts',(-39.2191796461909,-75.8636424227415,
85.6748783876891));
#211643=CARTESIAN_POINT('Ctrl Pts',(-39.2517354416209,-74.4402359800407,
85.6117570961772));
#211644=CARTESIAN_POINT('Ctrl Pts',(-33.2251508293409,-79.9040287823937,
60.8783100640841));
#211645=CARTESIAN_POINT('Ctrl Pts',(-33.2577066247709,-81.2696674810732,
61.4313085050615));
#211646=CARTESIAN_POINT('Ctrl Pts',(-33.3228182156309,-83.811729992399,
63.0035716608669));
#211647=CARTESIAN_POINT('Ctrl Pts',(-33.4204856019209,-86.6262501677223,
66.49395799585));
#211648=CARTESIAN_POINT('Ctrl Pts',(-33.5181529882109,-88.1228094499778,
70.7205438274274));
#211649=CARTESIAN_POINT('Ctrl Pts',(-33.6158203745009,-88.1318596833692,
75.2042647157331));
#211650=CARTESIAN_POINT('Ctrl Pts',(-33.7134877607909,-86.6523499320974,
79.4368608152641));
#211651=CARTESIAN_POINT('Ctrl Pts',(-33.8111551470709,-83.8519959181997,
82.9385512545613));
#211652=CARTESIAN_POINT('Ctrl Pts',(-33.9088225333609,-80.0482284232973,
85.3124031224554));
#211653=CARTESIAN_POINT('Ctrl Pts',(-34.0064899196509,-75.6722218896999,
86.2893299487034));
#211654=CARTESIAN_POINT('Ctrl Pts',(-34.1041573059409,-71.2200159883432,
85.7585926810093));
#211655=CARTESIAN_POINT('Ctrl Pts',(-34.2018246922309,-67.1962880910714,
83.7803527627688));
#211656=CARTESIAN_POINT('Ctrl Pts',(-34.2994920785209,-64.0571456387238,
80.5788524819327));
#211657=CARTESIAN_POINT('Ctrl Pts',(-34.3971594648109,-62.1584243900869,
76.5169961329518));
#211658=CARTESIAN_POINT('Ctrl Pts',(-34.4948268511009,-61.7153528413655,
72.0552131952207));
#211659=CARTESIAN_POINT('Ctrl Pts',(-34.5924942373909,-62.7781551230735,
67.6992666057196));
#211660=CARTESIAN_POINT('Ctrl Pts',(-34.6901616236809,-65.2263578703911,
63.9429222806304));
#211661=CARTESIAN_POINT('Ctrl Pts',(-34.7878290099709,-68.7824464151142,
61.2119785531442));
#211662=CARTESIAN_POINT('Ctrl Pts',(-34.8854963962609,-73.0433223072712,
59.8160000388975));
#211663=CARTESIAN_POINT('Ctrl Pts',(-34.9831637825509,-77.5259963169692,
59.9132271101948));
#211664=CARTESIAN_POINT('Ctrl Pts',(-35.0808311688409,-81.7223374113863,
61.4926386461447));
#211665=CARTESIAN_POINT('Ctrl Pts',(-35.1784985551309,-85.1566716669334,
64.3752013257362));
#211666=CARTESIAN_POINT('Ctrl Pts',(-35.2761659414209,-87.43970202375,68.2341638508803));
#211667=CARTESIAN_POINT('Ctrl Pts',(-35.3738333277109,-88.3126368385637,
72.632095659094));
#211668=CARTESIAN_POINT('Ctrl Pts',(-35.4715007140009,-87.6765250683029,
77.0704716229308));
#211669=CARTESIAN_POINT('Ctrl Pts',(-35.5691681002909,-85.6034728108319,
81.0461820900503));
#211670=CARTESIAN_POINT('Ctrl Pts',(-35.6668354865809,-82.3284697580989,
84.1085625995896));
#211671=CARTESIAN_POINT('Ctrl Pts',(-35.7645028728709,-78.2227520696129,
85.9104787028144));
#211672=CARTESIAN_POINT('Ctrl Pts',(-35.8621702591609,-73.7517211029078,
86.2476751965479));
#211673=CARTESIAN_POINT('Ctrl Pts',(-35.9598376454509,-69.4221881001095,
85.0819293587689));
#211674=CARTESIAN_POINT('Ctrl Pts',(-36.0575050317409,-65.7249248799056,
82.545383664097));
#211675=CARTESIAN_POINT('Ctrl Pts',(-36.1551724180309,-63.0790326695276,
78.9255668466803));
#211676=CARTESIAN_POINT('Ctrl Pts',(-36.2528398043209,-61.7844351169188,
74.6328012395937));
#211677=CARTESIAN_POINT('Ctrl Pts',(-36.3505071906109,-61.9878806115566,
70.1536909137268));
#211678=CARTESIAN_POINT('Ctrl Pts',(-36.4481745769009,-63.666307701945,
65.995962942479));
#211679=CARTESIAN_POINT('Ctrl Pts',(-36.5458419631909,-66.6294592136506,
62.6309142802354));
#211680=CARTESIAN_POINT('Ctrl Pts',(-36.6435093494809,-70.5414487461066,
60.4399881567566));
#211681=CARTESIAN_POINT('Ctrl Pts',(-36.7411767357709,-74.9588348897375,
59.6715357908676));
#211682=CARTESIAN_POINT('Ctrl Pts',(-36.8388441220609,-79.3808872816728,
60.4126646754531));
#211683=CARTESIAN_POINT('Ctrl Pts',(-36.9365115083509,-83.3063466190444,
62.5793645557408));
#211684=CARTESIAN_POINT('Ctrl Pts',(-37.0341788946409,-86.2902446299875,
65.9260303652965));
#211685=CARTESIAN_POINT('Ctrl Pts',(-37.1318462809309,-87.994343206,70.0733026524509));
#211686=CARTESIAN_POINT('Ctrl Pts',(-37.2295136672209,-88.2254751955924,
74.5510696611245));
#211687=CARTESIAN_POINT('Ctrl Pts',(-37.3271810535109,-86.9574407599487,
78.8517565888795));
#211688=CARTESIAN_POINT('Ctrl Pts',(-37.4248484398009,-84.3339772411099,
82.4878614479098));
#211689=CARTESIAN_POINT('Ctrl Pts',(-37.5225158260909,-80.6524658951112,
85.0472155832));
#211690=CARTESIAN_POINT('Ctrl Pts',(-37.6201832123809,-76.3302224041847,
86.2397048224279));
#211691=CARTESIAN_POINT('Ctrl Pts',(-37.7178505986709,-71.857192288432,
85.9301552074926));
#211692=CARTESIAN_POINT('Ctrl Pts',(-37.8155179849609,-67.7404134024109,
84.1536555637811));
#211693=CARTESIAN_POINT('Ctrl Pts',(-37.9131853712509,-64.4465409395824,
81.1115800257429));
#211694=CARTESIAN_POINT('Ctrl Pts',(-38.0108527575409,-62.3489499909946,
77.1487613832986));
#211695=CARTESIAN_POINT('Ctrl Pts',(-38.1085201438309,-61.6854118183574,
72.7144027516668));
#211696=CARTESIAN_POINT('Ctrl Pts',(-38.2061875301209,-62.5311414241959,
68.3111584007035));
#211697=CARTESIAN_POINT('Ctrl Pts',(-38.3038549164109,-64.7902715968898,
64.4381556582015));
#211698=CARTESIAN_POINT('Ctrl Pts',(-38.4015223027009,-68.206719885141,
61.534416607706));
#211699=CARTESIAN_POINT('Ctrl Pts',(-38.4991896889909,-72.3932166837339,
59.9290929831488));
#211700=CARTESIAN_POINT('Ctrl Pts',(-38.5968570752809,-76.875203961106,
59.8041553558837));
#211701=CARTESIAN_POINT('Ctrl Pts',(-38.6945244615809,-81.1446285386002,
61.1737659619934));
#211702=CARTESIAN_POINT('Ctrl Pts',(-38.7921918478709,-84.7175321175373,
63.8826733471557));
#211703=CARTESIAN_POINT('Ctrl Pts',(-38.8898592341609,-87.1889103282383,
67.6238108193033));
#211704=CARTESIAN_POINT('Ctrl Pts',(-38.9875266204509,-88.2786209412064,
71.9731037866268));
#211705=CARTESIAN_POINT('Ctrl Pts',(-39.0851940067409,-87.8631423512599,
76.4375406365594));
#211706=CARTESIAN_POINT('Ctrl Pts',(-39.1828613930309,-85.9895636692369,
80.5110572786137));
#211707=CARTESIAN_POINT('Ctrl Pts',(-39.2805287793209,-82.8702903713335,
83.7319036844191));
#211708=CARTESIAN_POINT('Ctrl Pts',(-39.3781961656109,-78.8588051875596,
85.7349781226078));
#211709=CARTESIAN_POINT('Ctrl Pts',(-39.4433077564709,-75.8930709812184,
86.1071526244662));
#211710=CARTESIAN_POINT('Ctrl Pts',(-39.4758635519009,-74.4211620580609,
86.0418804791265));
#211711=CARTESIAN_POINT('Ctrl Pts',(-37.9553013365568,-62.9850802944281,
77.9529305295057));
#211712=CARTESIAN_POINT('Ctrl Pts',(-37.9474201705531,-63.1216095490577,
78.2833846866343));
#211713=CARTESIAN_POINT('Ctrl Pts',(-37.9395319063314,-63.271795121894,
78.6082626989507));
#211714=CARTESIAN_POINT('Ctrl Pts',(-37.9145482658144,-63.7864029611045,
79.6105293665822));
#211715=CARTESIAN_POINT('Ctrl Pts',(-37.8972687988449,-64.1974606125135,
80.2618535031525));
#211716=CARTESIAN_POINT('Ctrl Pts',(-37.8610792187594,-65.1847264324815,
81.5561899246955));
#211717=CARTESIAN_POINT('Ctrl Pts',(-37.8423433620313,-65.7722569016136,
82.1860084574922));
#211718=CARTESIAN_POINT('Ctrl Pts',(-37.8109478109972,-66.8312005758723,
83.1167677105313));
#211719=CARTESIAN_POINT('Ctrl Pts',(-37.7985886876602,-67.2674656454352,
83.4536451729963));
#211720=CARTESIAN_POINT('Ctrl Pts',(-37.7691084875777,-68.3637012594982,
84.1940605472006));
#211721=CARTESIAN_POINT('Ctrl Pts',(-37.752260997049,-69.0408691600133,
84.5684007187656));
#211722=CARTESIAN_POINT('Ctrl Pts',(-37.7176829609665,-70.4665992089544,
85.1981775476462));
#211723=CARTESIAN_POINT('Ctrl Pts',(-37.6999872682034,-71.2133015775831,
85.4500028177778));
#211724=CARTESIAN_POINT('Ctrl Pts',(-37.6640147271937,-72.78986964161,85.8267949841164));
#211725=CARTESIAN_POINT('Ctrl Pts',(-37.6457906302058,-73.6183716817423,
85.9421750277991));
#211726=CARTESIAN_POINT('Ctrl Pts',(-37.6179084997543,-74.8690218240065,
85.9949223926247));
#211727=CARTESIAN_POINT('Ctrl Pts',(-37.608565090223,-75.2864483781191,
85.9924272170315));
#211728=CARTESIAN_POINT('Ctrl Pts',(-37.5800013565997,-76.5622250903209,
85.9233331417926));
#211729=CARTESIAN_POINT('Ctrl Pts',(-37.561208726608,-77.4146797158845,
85.791611988895));
#211730=CARTESIAN_POINT('Ctrl Pts',(-37.5247928902469,-79.005561520104,
85.3811380147145));
#211731=CARTESIAN_POINT('Ctrl Pts',(-37.5072055842918,-79.7440710258465,
85.1176208937734));
#211732=CARTESIAN_POINT('Ctrl Pts',(-37.4706991061669,-81.2343611254123,
84.4287793423801));
#211733=CARTESIAN_POINT('Ctrl Pts',(-37.4519642982971,-81.9766763907336,
83.9918133103111));
#211734=CARTESIAN_POINT('Ctrl Pts',(-37.4235240123576,-83.0079247368912,
83.2381757820445));
#211735=CARTESIAN_POINT('Ctrl Pts',(-37.4141646745884,-83.3333225848237,
82.9754034813127));
#211736=CARTESIAN_POINT('Ctrl Pts',(-37.3855784673059,-84.2880441829575,
82.1252187149311));
#211737=CARTESIAN_POINT('Ctrl Pts',(-37.3667761154245,-84.8722039841866,
81.4906462028291));
#211738=CARTESIAN_POINT('Ctrl Pts',(-37.3288884631521,-85.900057666322,
80.1240524272387));
#211739=CARTESIAN_POINT('Ctrl Pts',(-37.3097661738678,-86.3429472217326,
79.3966463528337));
#211740=CARTESIAN_POINT('Ctrl Pts',(-37.2723777773446,-87.0746795871862,
77.8778102789801));
#211741=CARTESIAN_POINT('Ctrl Pts',(-37.2541052672179,-87.3641153421296,
77.0910954575695));
#211742=CARTESIAN_POINT('Ctrl Pts',(-37.2261946318884,-87.6814127958953,
75.8793939520376));
#211743=CARTESIAN_POINT('Ctrl Pts',(-37.216870478266,-87.7674530863341,
75.4719092966888));
#211744=CARTESIAN_POINT('Ctrl Pts',(-37.188334955032,-87.9709508310614,
74.2115296624505));
#211745=CARTESIAN_POINT('Ctrl Pts',(-37.1695528444446,-88.0234260694818,
73.3505374940313));
#211746=CARTESIAN_POINT('Ctrl Pts',(-37.1324546555661,-87.9593077821367,
71.6786479533309));
#211747=CARTESIAN_POINT('Ctrl Pts',(-37.1141663205998,-87.8520911218072,
70.8713112465121));
#211748=CARTESIAN_POINT('Ctrl Pts',(-37.0776055093155,-87.4832538348699,
69.265165449192));
#211749=CARTESIAN_POINT('Ctrl Pts',(-37.0593609396572,-87.2182658519536,
68.4709546004865));
#211750=CARTESIAN_POINT('Ctrl Pts',(-37.028756307801,-86.6601778752232,
67.2156601142761));
#211751=CARTESIAN_POINT('Ctrl Pts',(-37.0166706348671,-86.4110793261731,
66.7377142091686));
#211752=CARTESIAN_POINT('Ctrl Pts',(-36.9874851340614,-85.7347609734185,
65.6159671225058));
#211753=CARTESIAN_POINT('Ctrl Pts',(-36.9706554515717,-85.2784462954607,
64.9921013330032));
#211754=CARTESIAN_POINT('Ctrl Pts',(-36.9368299445691,-84.2726486204961,
63.8463944526631));
#211755=CARTESIAN_POINT('Ctrl Pts',(-36.9198965764989,-83.7275327721831,
63.3246569542117));
#211756=CARTESIAN_POINT('Ctrl Pts',(-36.8938644165587,-82.8143090573121,
62.5912253381851));
#211757=CARTESIAN_POINT('Ctrl Pts',(-36.8846757283285,-82.4758480186136,
62.3452743352519));
#211758=CARTESIAN_POINT('Ctrl Pts',(-36.8533476314567,-81.2877080817444,
61.5665594157926));
#211759=CARTESIAN_POINT('Ctrl Pts',(-36.8309230422989,-80.3885391871815,
61.1158732010766));
#211760=CARTESIAN_POINT('Ctrl Pts',(-36.7894494876858,-78.6387021441159,
60.4789344798652));
#211761=CARTESIAN_POINT('Ctrl Pts',(-36.7707178990796,-77.8036529097714,
60.2657349567428));
#211762=CARTESIAN_POINT('Ctrl Pts',(-36.7386712591883,-76.3794260285354,
60.0492377442393));
#211763=CARTESIAN_POINT('Ctrl Pts',(-36.7256353124818,-75.7999574332354,
60.0005305292947));
#211764=CARTESIAN_POINT('Ctrl Pts',(-36.6954200028567,-74.4448263249971,
59.9776797137621));
#211765=CARTESIAN_POINT('Ctrl Pts',(-36.6785226408525,-73.6708544423597,
60.033845272356));
#211766=CARTESIAN_POINT('Ctrl Pts',(-36.6444393144521,-72.1542417281374,
60.2813083751712));
#211767=CARTESIAN_POINT('Ctrl Pts',(-36.6273040887924,-71.4142410833303,
60.4699725635176));
#211768=CARTESIAN_POINT('Ctrl Pts',(-36.5912629985515,-69.8843497244514,
61.0068902560186));
#211769=CARTESIAN_POINT('Ctrl Pts',(-36.5725265787893,-69.1038501365627,
61.3710752108196));
#211770=CARTESIAN_POINT('Ctrl Pts',(-36.5440917128776,-68.0058455111706,
62.0227490315051));
#211771=CARTESIAN_POINT('Ctrl Pts',(-36.5347393239218,-67.6571704750053,
62.2530948298418));
#211772=CARTESIAN_POINT('Ctrl Pts',(-36.5061627867718,-66.6259532144554,
63.0081240836906));
#211773=CARTESIAN_POINT('Ctrl Pts',(-36.487364783741,-65.9838937259926,
63.5840945896985));
#211774=CARTESIAN_POINT('Ctrl Pts',(-36.4508287270761,-64.8716835789756,
64.8011777568565));
#211775=CARTESIAN_POINT('Ctrl Pts',(-36.4331132215708,-64.3939415100505,
65.4302567804368));
#211776=CARTESIAN_POINT('Ctrl Pts',(-36.3984301762417,-63.5673059184115,
66.7528247588843));
#211777=CARTESIAN_POINT('Ctrl Pts',(-36.3815971455736,-63.2175024656728,
67.4420206215753));
#211778=CARTESIAN_POINT('Ctrl Pts',(-36.3484649018998,-62.6632765516673,
68.8267002319811));
#211779=CARTESIAN_POINT('Ctrl Pts',(-36.3322686753649,-62.4516988960482,
69.5163260240136));
#211780=CARTESIAN_POINT('Ctrl Pts',(-36.3002569422527,-62.1447056281685,
70.9245458454321));
#211781=CARTESIAN_POINT('Ctrl Pts',(-36.2845007616004,-62.0499953695942,
71.6407444006773));
#211782=CARTESIAN_POINT('Ctrl Pts',(-36.2513677547303,-61.9779183273901,
73.1315272034695));
#211783=CARTESIAN_POINT('Ctrl Pts',(-36.2340081542753,-62.0093114894252,
73.903746883324));
#211784=CARTESIAN_POINT('Ctrl Pts',(-36.1994040444446,-62.2108802467661,
75.4506851127403));
#211785=CARTESIAN_POINT('Ctrl Pts',(-36.1821713308395,-62.3837445293686,
76.2218644194105));
#211786=CARTESIAN_POINT('Ctrl Pts',(-36.1568663165771,-62.7321991006185,
77.304263693113));
#211787=CARTESIAN_POINT('Ctrl Pts',(-36.1490816133291,-62.8521945973888,
77.6312952057894));
#211788=CARTESIAN_POINT('Ctrl Pts',(-36.1412950695185,-62.9850802944281,
77.9529305295057));
#211789=CARTESIAN_POINT('',(-32.7070373297029,-83.5022665033036,64.749780674319));
#211790=CARTESIAN_POINT('Ctrl Pts',(-26.5424658037409,-63.226796009855,
73.1405558201252));
#211791=CARTESIAN_POINT('Ctrl Pts',(-26.5750215991709,-63.2096934794613,
71.8129609505269));
#211792=CARTESIAN_POINT('Ctrl Pts',(-26.6401331900309,-63.6289072208686,
69.1522693813868));
#211793=CARTESIAN_POINT('Ctrl Pts',(-26.7378005763209,-65.5466883188414,
65.595862444819));
#211794=CARTESIAN_POINT('Ctrl Pts',(-26.8354679626109,-68.5360452568475,
62.8775596699701));
#211795=CARTESIAN_POINT('Ctrl Pts',(-26.9331353489009,-72.2581199618507,
61.3054018749864));
#211796=CARTESIAN_POINT('Ctrl Pts',(-27.0308027351909,-76.2909990282318,
61.0576244908063));
#211797=CARTESIAN_POINT('Ctrl Pts',(-27.1284701214809,-80.1775375961095,
62.1623076602056));
#211798=CARTESIAN_POINT('Ctrl Pts',(-27.2261375077709,-83.4771792584479,
64.4942323820704));
#211799=CARTESIAN_POINT('Ctrl Pts',(-27.3238048940609,-85.8158949537486,
67.789064150928));
#211800=CARTESIAN_POINT('Ctrl Pts',(-27.4214722803509,-86.9285808596196,
71.6733192596676));
#211801=CARTESIAN_POINT('Ctrl Pts',(-27.5191396666409,-86.6891090802536,
75.7067000853347));
#211802=CARTESIAN_POINT('Ctrl Pts',(-27.6168070529309,-85.1246248068445,
79.4320049844843));
#211803=CARTESIAN_POINT('Ctrl Pts',(-27.7144744392209,-82.4124692887962,
82.4269540784775));
#211804=CARTESIAN_POINT('Ctrl Pts',(-27.8121418255109,-78.860077414659,
84.3520565700369));
#211805=CARTESIAN_POINT('Ctrl Pts',(-27.9098092118009,-74.870128600351,
84.9890935309175));
#211806=CARTESIAN_POINT('Ctrl Pts',(-28.0074765980909,-70.8949012867121,
84.2658539888278));
#211807=CARTESIAN_POINT('Ctrl Pts',(-28.1051439843809,-67.3850051670203,
82.2643203620043));
#211808=CARTESIAN_POINT('Ctrl Pts',(-28.2028113706709,-64.7383025744529,
79.2113753875849));
#211809=CARTESIAN_POINT('Ctrl Pts',(-28.3004787569609,-63.254809017389,
75.453083954434));
#211810=CARTESIAN_POINT('Ctrl Pts',(-28.3981461432509,-63.1026850874199,
71.4154651090891));
#211811=CARTESIAN_POINT('Ctrl Pts',(-28.4958135295409,-64.2991747084623,
67.5562009023972));
#211812=CARTESIAN_POINT('Ctrl Pts',(-28.5934809158309,-66.7086504613652,
64.3127560937844));
#211813=CARTESIAN_POINT('Ctrl Pts',(-28.6911483021209,-70.0579875549346,
62.0527895754544));
#211814=CARTESIAN_POINT('Ctrl Pts',(-28.7888156884109,-73.9675237355834,
61.0324786020043));
#211815=CARTESIAN_POINT('Ctrl Pts',(-28.8864830747009,-77.994095692078,
61.367479959455));
#211816=CARTESIAN_POINT('Ctrl Pts',(-28.9841504609909,-81.6812735875568,
63.0198197542421));
#211817=CARTESIAN_POINT('Ctrl Pts',(-29.0818178472809,-84.6110994112092,
65.8021979228998));
#211818=CARTESIAN_POINT('Ctrl Pts',(-29.1794852335709,-86.4514643773875,
69.3992195271719));
#211819=CARTESIAN_POINT('Ctrl Pts',(-29.2771526198609,-86.99375493335,73.4031461727609));
#211820=CARTESIAN_POINT('Ctrl Pts',(-29.3748200061509,-86.176500033081,
77.3601149694952));
#211821=CARTESIAN_POINT('Ctrl Pts',(-29.4724873924409,-84.0923391537426,
80.8215859081834));
#211822=CARTESIAN_POINT('Ctrl Pts',(-29.5701547787309,-80.9775211989782,
83.3951858652538));
#211823=CARTESIAN_POINT('Ctrl Pts',(-29.6678221650209,-77.1851246351153,
84.789185841132));
#211824=CARTESIAN_POINT('Ctrl Pts',(-29.7654895513109,-73.1450344769205,
84.8455697396331));
#211825=CARTESIAN_POINT('Ctrl Pts',(-29.8631569376009,-69.3152129095361,
83.5579461951267));
#211826=CARTESIAN_POINT('Ctrl Pts',(-29.9608243238909,-66.1297872383019,
81.0722730622718));
#211827=CARTESIAN_POINT('Ctrl Pts',(-30.0584917101809,-63.9498396281978,
77.6703124441067));
#211828=CARTESIAN_POINT('Ctrl Pts',(-30.1561590964709,-63.0224768347345,
73.7376917047466));
#211829=CARTESIAN_POINT('Ctrl Pts',(-30.2538264827609,-63.4528195544114,
69.7201908928029));
#211830=CARTESIAN_POINT('Ctrl Pts',(-30.3514938690509,-65.1920865262802,
66.0732115905697));
#211831=CARTESIAN_POINT('Ctrl Pts',(-30.4491612553409,-68.0431241048049,
63.2101551195605));
#211832=CARTESIAN_POINT('Ctrl Pts',(-30.5468286416309,-71.6827545022938,
61.4555616623674));
#211833=CARTESIAN_POINT('Ctrl Pts',(-30.6444960279209,-75.6984094282703,
61.0083221897941));
#211834=CARTESIAN_POINT('Ctrl Pts',(-30.7421634142109,-79.634896539825,
61.9191332848712));
#211835=CARTESIAN_POINT('Ctrl Pts',(-30.8398308005009,-83.0459975178568,
64.0847504597221));
#211836=CARTESIAN_POINT('Ctrl Pts',(-30.9374981867909,-85.5450488978255,
67.2596913773822));
#211837=CARTESIAN_POINT('Ctrl Pts',(-31.0351655730809,-86.8487720928805,
71.0840623663197));
#211838=CARTESIAN_POINT('Ctrl Pts',(-31.1328329593709,-86.8093842813913,
75.1243539684997));
#211839=CARTESIAN_POINT('Ctrl Pts',(-31.2305003456609,-85.4313502469366,
78.9225811642113));
#211840=CARTESIAN_POINT('Ctrl Pts',(-31.3281677319509,-82.8708762752482,
82.0481980106353));
#211841=CARTESIAN_POINT('Ctrl Pts',(-31.4258351182409,-79.4182034770832,
84.1469019390542));
#211842=CARTESIAN_POINT('Ctrl Pts',(-31.5235025045309,-75.4647076676689,
84.980795526557));
#211843=CARTESIAN_POINT('Ctrl Pts',(-31.6211698908209,-71.4585351776186,
84.4553532267351));
#211844=CARTESIAN_POINT('Ctrl Pts',(-31.7188372771109,-67.8538034736301,
82.630136261015));
#211845=CARTESIAN_POINT('Ctrl Pts',(-31.8165046634009,-65.0591249238588,
79.712041088333));
#211846=CARTESIAN_POINT('Ctrl Pts',(-31.9141720496909,-63.3912887702861,
76.0318467751409));
#211847=CARTESIAN_POINT('Ctrl Pts',(-32.0118394359809,-63.0393516544576,
72.0067197036773));
#211848=CARTESIAN_POINT('Ctrl Pts',(-32.1095068222709,-64.0432072250839,
68.0929259582381));
#211849=CARTESIAN_POINT('Ctrl Pts',(-32.2071742085609,-66.2890639457993,
64.7341113461543));
#211850=CARTESIAN_POINT('Ctrl Pts',(-32.3048415948509,-69.5223441324314,
62.3110128795057));
#211851=CARTESIAN_POINT('Ctrl Pts',(-32.4025089811409,-73.3765404928114,
61.0982979039962));
#211852=CARTESIAN_POINT('Ctrl Pts',(-32.5001763674309,-77.4147649885621,
61.233439177867));
#211853=CARTESIAN_POINT('Ctrl Pts',(-32.5978437537209,-81.1792584882072,
62.7010949855073));
#211854=CARTESIAN_POINT('Ctrl Pts',(-32.6955111400109,-84.2433303651157,
65.3349852966984));
#211855=CARTESIAN_POINT('Ctrl Pts',(-32.7606227308709,-85.5874681664406,
67.6691475357372));
#211856=CARTESIAN_POINT('Ctrl Pts',(-32.7931785263009,-86.0468748830494,
68.9148385500206));
#211857=CARTESIAN_POINT('Ctrl Pts',(-26.7665939140209,-62.7962856369908,
73.1461018017394));
#211858=CARTESIAN_POINT('Ctrl Pts',(-26.7991497094509,-62.7785577189135,
71.7699608131093));
#211859=CARTESIAN_POINT('Ctrl Pts',(-26.8642613003109,-63.2131008357698,
69.0119758206586));
#211860=CARTESIAN_POINT('Ctrl Pts',(-26.9619286865909,-65.2010093736661,
65.3255218656522));
#211861=CARTESIAN_POINT('Ctrl Pts',(-27.0595960728809,-68.2996780309902,
62.5078190003945));
#211862=CARTESIAN_POINT('Ctrl Pts',(-27.1572634591709,-72.1578577224007,
60.8781721617226));
#211863=CARTESIAN_POINT('Ctrl Pts',(-27.2549308454609,-76.3382069483097,
60.6213343098834));
#211864=CARTESIAN_POINT('Ctrl Pts',(-27.3525982317509,-80.3668644473949,
61.766412393317));
#211865=CARTESIAN_POINT('Ctrl Pts',(-27.4502656180409,-83.787164000609,
64.1836085317263));
#211866=CARTESIAN_POINT('Ctrl Pts',(-27.5479330043309,-86.2113994377659,
67.5989223082413));
#211867=CARTESIAN_POINT('Ctrl Pts',(-27.6456003906209,-87.3647728934875,
71.6252128490111));
#211868=CARTESIAN_POINT('Ctrl Pts',(-27.7432677769109,-87.1165443572374,
75.8060821820241));
#211869=CARTESIAN_POINT('Ctrl Pts',(-27.8409351632009,-85.4948516375614,
79.6676101859858));
#211870=CARTESIAN_POINT('Ctrl Pts',(-27.9386025494909,-82.6835208156347,
82.7720754874777));
#211871=CARTESIAN_POINT('Ctrl Pts',(-28.0362699357809,-79.0012287417265,
84.7675731401279));
#211872=CARTESIAN_POINT('Ctrl Pts',(-28.1339373220709,-74.8653795970425,
85.4279046111302));
#211873=CARTESIAN_POINT('Ctrl Pts',(-28.2316047083609,-70.7447902736733,
84.6782183919009));
#211874=CARTESIAN_POINT('Ctrl Pts',(-28.3292720946509,-67.1065478950989,
82.6034947491145));
#211875=CARTESIAN_POINT('Ctrl Pts',(-28.4269394809409,-64.3630634136857,
79.4389128336908));
#211876=CARTESIAN_POINT('Ctrl Pts',(-28.5246068672309,-62.8253229952768,
75.543192078198));
#211877=CARTESIAN_POINT('Ctrl Pts',(-28.6222742535209,-62.6676363544306,
71.3579297539833));
#211878=CARTESIAN_POINT('Ctrl Pts',(-28.7199416398109,-63.9078779730934,
67.3575439567693));
#211879=CARTESIAN_POINT('Ctrl Pts',(-28.8176090261009,-66.4054609486044,
63.9954962058266));
#211880=CARTESIAN_POINT('Ctrl Pts',(-28.9152764123909,-69.8772731442938,
61.6528895642723));
#211881=CARTESIAN_POINT('Ctrl Pts',(-29.0129437986809,-73.9297692091192,
60.5952689121647));
#211882=CARTESIAN_POINT('Ctrl Pts',(-29.1106111849709,-78.1035806932568,
60.9425202535141));
#211883=CARTESIAN_POINT('Ctrl Pts',(-29.2082785712609,-81.9255875046266,
62.6552811046037));
#211884=CARTESIAN_POINT('Ctrl Pts',(-29.3059459575509,-84.9625481752439,
65.5394024065493));
#211885=CARTESIAN_POINT('Ctrl Pts',(-29.4036133438509,-86.8702097081482,
69.2679561845011));
#211886=CARTESIAN_POINT('Ctrl Pts',(-29.5012807301409,-87.4323301854809,
73.4182942873751));
#211887=CARTESIAN_POINT('Ctrl Pts',(-29.5989481164309,-86.5851907514749,
77.5199574352398));
#211888=CARTESIAN_POINT('Ctrl Pts',(-29.6966155027209,-84.4248184280816,
81.1080038707725));
#211889=CARTESIAN_POINT('Ctrl Pts',(-29.7942828890109,-81.1961010250256,
83.7757125749618));
#211890=CARTESIAN_POINT('Ctrl Pts',(-29.8919502753009,-77.2650280175932,
85.2206869032595));
#211891=CARTESIAN_POINT('Ctrl Pts',(-29.9896176615909,-73.0772040121119,
85.2791325899756));
#211892=CARTESIAN_POINT('Ctrl Pts',(-30.0872850478809,-69.1073374822569,
83.9444245566035));
#211893=CARTESIAN_POINT('Ctrl Pts',(-30.1849524341709,-65.8054304526251,
81.3678578939925));
#211894=CARTESIAN_POINT('Ctrl Pts',(-30.2826198204609,-63.5457687681484,
77.8414978909712));
#211895=CARTESIAN_POINT('Ctrl Pts',(-30.3802872067509,-62.5844951291497,
73.7650731351128));
#211896=CARTESIAN_POINT('Ctrl Pts',(-30.4779545930409,-63.0305741772578,
69.6006644997806));
#211897=CARTESIAN_POINT('Ctrl Pts',(-30.5756219793309,-64.8334408687264,
65.8203262223269));
#211898=CARTESIAN_POINT('Ctrl Pts',(-30.6732893656209,-67.7887322469773,
62.8525764571267));
#211899=CARTESIAN_POINT('Ctrl Pts',(-30.7709567519109,-71.5614528925225,
61.0338228372305));
#211900=CARTESIAN_POINT('Ctrl Pts',(-30.8686241382009,-75.7239481434376,
60.570229173206));
#211901=CARTESIAN_POINT('Ctrl Pts',(-30.9662915244909,-79.8043806529974,
61.5143458683933));
#211902=CARTESIAN_POINT('Ctrl Pts',(-31.0639589107809,-83.3402152511359,
63.7591530970452));
#211903=CARTESIAN_POINT('Ctrl Pts',(-31.1616262970709,-85.930649362801,
67.0501919774507));
#211904=CARTESIAN_POINT('Ctrl Pts',(-31.2592936833609,-87.2820457621323,
71.0144086177314));
#211905=CARTESIAN_POINT('Ctrl Pts',(-31.3569610696509,-87.2412176577989,
75.2024414334004));
#211906=CARTESIAN_POINT('Ctrl Pts',(-31.4546284559409,-85.8127930969901,
79.1395582812056));
#211907=CARTESIAN_POINT('Ctrl Pts',(-31.5522958422309,-83.1586903556685,
82.3794694586463));
#211908=CARTESIAN_POINT('Ctrl Pts',(-31.6499632285209,-79.5797637819886,
84.5549166263378));
#211909=CARTESIAN_POINT('Ctrl Pts',(-31.7476306148109,-75.4817006180579,
85.4193031739153));
#211910=CARTESIAN_POINT('Ctrl Pts',(-31.8452980011009,-71.329034547002,
84.8746470423661));
#211911=CARTESIAN_POINT('Ctrl Pts',(-31.9429653873909,-67.5924887343543,
82.98268742638));
#211912=CARTESIAN_POINT('Ctrl Pts',(-32.0406327736809,-64.695617263651,
79.9578863610724));
#211913=CARTESIAN_POINT('Ctrl Pts',(-32.1383001599709,-62.9667933989244,
76.1431185004145));
#211914=CARTESIAN_POINT('Ctrl Pts',(-32.2359675462609,-62.6019870098559,
71.970804736377));
#211915=CARTESIAN_POINT('Ctrl Pts',(-32.3336349325509,-63.642550534956,
67.9138954205205));
#211916=CARTESIAN_POINT('Ctrl Pts',(-32.4313023188409,-65.9705314263782,
64.4322591422073));
#211917=CARTESIAN_POINT('Ctrl Pts',(-32.5289697051309,-69.3220428659327,
61.9205553116032));
#211918=CARTESIAN_POINT('Ctrl Pts',(-32.6266370914209,-73.3171755010594,
60.6634950264663));
#211919=CARTESIAN_POINT('Ctrl Pts',(-32.7243044777109,-77.5030656224803,
60.8035780069626));
#211920=CARTESIAN_POINT('Ctrl Pts',(-32.8219718640009,-81.4052152352389,
62.3249015374696));
#211921=CARTESIAN_POINT('Ctrl Pts',(-32.9196392502909,-84.5813309302388,
65.0551052312263));
#211922=CARTESIAN_POINT('Ctrl Pts',(-32.9847508411509,-85.974619775455,
67.4746207060263));
#211923=CARTESIAN_POINT('Ctrl Pts',(-33.0173066365809,-86.4508256027431,
68.7658628636918));
#211924=CARTESIAN_POINT('Ctrl Pts',(-26.9907220242909,-62.3657752641363,
73.1516477833507));
#211925=CARTESIAN_POINT('Ctrl Pts',(-27.0232778197209,-62.3474219583749,
71.7269606756879));
#211926=CARTESIAN_POINT('Ctrl Pts',(-27.0883894105809,-62.7972944506722,
68.8716822599311));
#211927=CARTESIAN_POINT('Ctrl Pts',(-27.1860567968709,-64.8553304284946,
65.0551812864947));
#211928=CARTESIAN_POINT('Ctrl Pts',(-27.2837241831609,-68.0633108051291,
62.1380783308097));
#211929=CARTESIAN_POINT('Ctrl Pts',(-27.3813915694509,-72.0575954829508,
60.4509424484588));
#211930=CARTESIAN_POINT('Ctrl Pts',(-27.4790589557409,-76.3854148683847,
60.1850441289508));
#211931=CARTESIAN_POINT('Ctrl Pts',(-27.5767263420309,-80.5561912986817,
61.3705171264288));
#211932=CARTESIAN_POINT('Ctrl Pts',(-27.6743937283209,-84.0971487427805,
63.8729846813812));
#211933=CARTESIAN_POINT('Ctrl Pts',(-27.7720611146109,-86.6069039217849,
67.4087804655587));
#211934=CARTESIAN_POINT('Ctrl Pts',(-27.8697285009009,-87.8009649273485,
71.577106438364));
#211935=CARTESIAN_POINT('Ctrl Pts',(-27.9673958871909,-87.5439796342222,
75.9054642787186));
#211936=CARTESIAN_POINT('Ctrl Pts',(-28.0650632734809,-85.8650784682753,
79.9032153874961));
#211937=CARTESIAN_POINT('Ctrl Pts',(-28.1627306597709,-82.9545723424687,
83.1171968964905));
#211938=CARTESIAN_POINT('Ctrl Pts',(-28.2603980460609,-79.1423800687866,
85.1830897102328));
#211939=CARTESIAN_POINT('Ctrl Pts',(-28.3580654323509,-74.860630593725,
85.8667156913575));
#211940=CARTESIAN_POINT('Ctrl Pts',(-28.4557328186409,-70.5946792606203,
85.0905827949681));
#211941=CARTESIAN_POINT('Ctrl Pts',(-28.5534002049309,-66.8280906231621,
82.9426691362138));
#211942=CARTESIAN_POINT('Ctrl Pts',(-28.6510675912209,-63.987824252902,
79.666450279783));
#211943=CARTESIAN_POINT('Ctrl Pts',(-28.7487349775109,-62.3958369731654,
75.6333002019378));
#211944=CARTESIAN_POINT('Ctrl Pts',(-28.8464023638009,-62.2325876214517,
71.3003943988505));
#211945=CARTESIAN_POINT('Ctrl Pts',(-28.9440697500909,-63.5165812377356,
67.1588870111186));
#211946=CARTESIAN_POINT('Ctrl Pts',(-29.0417371363809,-66.1022714358647,
63.6782363178492));
#211947=CARTESIAN_POINT('Ctrl Pts',(-29.1394045226709,-69.6965587336775,
61.2529895530693));
#211948=CARTESIAN_POINT('Ctrl Pts',(-29.2370719089609,-73.8920146826892,
60.1580592223219));
#211949=CARTESIAN_POINT('Ctrl Pts',(-29.3347392952509,-78.2130656944676,
60.5175605475773));
#211950=CARTESIAN_POINT('Ctrl Pts',(-29.4324066815409,-82.1699014217328,
62.2907424549826));
#211951=CARTESIAN_POINT('Ctrl Pts',(-29.5300740678309,-85.3139969393028,
65.2766068902311));
#211952=CARTESIAN_POINT('Ctrl Pts',(-29.6277414541209,-87.2889550389062,
69.1366928418757));
#211953=CARTESIAN_POINT('Ctrl Pts',(-29.7254088404109,-87.8709054376088,
73.4334424020349));
#211954=CARTESIAN_POINT('Ctrl Pts',(-29.8230762267009,-86.9938814698514,
77.6797999010284));
#211955=CARTESIAN_POINT('Ctrl Pts',(-29.9207436129909,-84.7572977023885,
81.3944218333964));
#211956=CARTESIAN_POINT('Ctrl Pts',(-30.0184109992809,-81.4146808510287,
84.1562392846881));
#211957=CARTESIAN_POINT('Ctrl Pts',(-30.1160783855709,-77.3449314000249,
85.652187965406));
#211958=CARTESIAN_POINT('Ctrl Pts',(-30.2137457718609,-73.009373547253,
85.7126954403171));
#211959=CARTESIAN_POINT('Ctrl Pts',(-30.3114131581509,-68.8994620549307,
84.3309029180553));
#211960=CARTESIAN_POINT('Ctrl Pts',(-30.4090805444409,-65.4810736669192,
81.6634427256689));
#211961=CARTESIAN_POINT('Ctrl Pts',(-30.5067479307309,-63.1416979080774,
78.0126833377833));
#211962=CARTESIAN_POINT('Ctrl Pts',(-30.6044153170209,-62.1465134235629,
73.7924545654214));
#211963=CARTESIAN_POINT('Ctrl Pts',(-30.7020827033109,-62.6083288001179,
69.4811381067028));
#211964=CARTESIAN_POINT('Ctrl Pts',(-30.7997500896009,-64.4747952112035,
65.5674408540281));
#211965=CARTESIAN_POINT('Ctrl Pts',(-30.8974174758909,-67.5343403891965,
62.4949977946519));
#211966=CARTESIAN_POINT('Ctrl Pts',(-30.9950848621809,-71.4401512828104,
60.6120840120799));
#211967=CARTESIAN_POINT('Ctrl Pts',(-31.0927522484709,-75.7494868586634,
60.1321361566154));
#211968=CARTESIAN_POINT('Ctrl Pts',(-31.1904196347609,-79.973864766225,
61.1095584519391));
#211969=CARTESIAN_POINT('Ctrl Pts',(-31.2880870210509,-83.6344329844545,
63.4335557344114));
#211970=CARTESIAN_POINT('Ctrl Pts',(-31.3857544073409,-86.3162498277991,
66.8406925775738));
#211971=CARTESIAN_POINT('Ctrl Pts',(-31.4834217936309,-87.7153194313877,
70.9447548692043));
#211972=CARTESIAN_POINT('Ctrl Pts',(-31.5810891799209,-87.6730510341971,
75.2805288983569));
#211973=CARTESIAN_POINT('Ctrl Pts',(-31.6787565662109,-86.1942359470167,
79.3565353982501));
#211974=CARTESIAN_POINT('Ctrl Pts',(-31.7764239525009,-83.4465044360485,
82.7107409066955));
#211975=CARTESIAN_POINT('Ctrl Pts',(-31.8740913387909,-79.7413240868408,
84.9629313136325));
#211976=CARTESIAN_POINT('Ctrl Pts',(-31.9717587250809,-75.4986935683949,
85.8578108212734));
#211977=CARTESIAN_POINT('Ctrl Pts',(-32.0694261113709,-71.1995339163389,
85.2939408579817));
#211978=CARTESIAN_POINT('Ctrl Pts',(-32.1670934976609,-67.331173995054,
83.335238591712));
#211979=CARTESIAN_POINT('Ctrl Pts',(-32.2647608839509,-64.3321096034271,
80.203731633773));
#211980=CARTESIAN_POINT('Ctrl Pts',(-32.3624282702409,-62.5422980275575,
76.2543902256492));
#211981=CARTESIAN_POINT('Ctrl Pts',(-32.4600956565309,-62.1646223652701,
71.9348897690366));
#211982=CARTESIAN_POINT('Ctrl Pts',(-32.5577630428209,-63.2418938448422,
67.7348648827743));
#211983=CARTESIAN_POINT('Ctrl Pts',(-32.6554304291109,-65.6519989069735,
64.1304069382318));
#211984=CARTESIAN_POINT('Ctrl Pts',(-32.7530978154009,-69.1217415994551,
61.5300977436921));
#211985=CARTESIAN_POINT('Ctrl Pts',(-32.8507652016909,-73.2578105093222,
60.2286921489302));
#211986=CARTESIAN_POINT('Ctrl Pts',(-32.9484325879809,-77.5913662564109,
60.373716836065));
#211987=CARTESIAN_POINT('Ctrl Pts',(-33.0460999742709,-81.6311719822709,
61.948708089435));
#211988=CARTESIAN_POINT('Ctrl Pts',(-33.1437673605609,-84.9193314953615,
64.7752251657533));
#211989=CARTESIAN_POINT('Ctrl Pts',(-33.2088789514209,-86.3617713844579,
67.2800938763135));
#211990=CARTESIAN_POINT('Ctrl Pts',(-33.2414347468509,-86.8547763224244,
68.616887177359));
#211991=CARTESIAN_POINT('Ctrl Pts',(-27.2148501345709,-61.9352648912724,
73.1571937649659));
#211992=CARTESIAN_POINT('Ctrl Pts',(-27.2474059300009,-61.9162861978364,
71.6839605382664));
#211993=CARTESIAN_POINT('Ctrl Pts',(-27.3125175208609,-62.3814880655743,
68.7313886992026));
#211994=CARTESIAN_POINT('Ctrl Pts',(-27.4101849071509,-64.5096514833231,
64.7848407073371));
#211995=CARTESIAN_POINT('Ctrl Pts',(-27.5078522934409,-67.8269435792709,
61.7683376612345));
#211996=CARTESIAN_POINT('Ctrl Pts',(-27.6055196797309,-71.9573332435009,
60.023712735195));
#211997=CARTESIAN_POINT('Ctrl Pts',(-27.7031870660209,-76.4326227884626,
59.7487539480279));
#211998=CARTESIAN_POINT('Ctrl Pts',(-27.8008544523109,-80.7455181499671,
60.9746218595402));
#211999=CARTESIAN_POINT('Ctrl Pts',(-27.8985218386009,-84.4071334849508,
63.5623608310333));
#212000=CARTESIAN_POINT('Ctrl Pts',(-27.9961892248909,-87.0024084058022,
67.2186386228721));
#212001=CARTESIAN_POINT('Ctrl Pts',(-28.0938566111809,-88.2371569612167,
71.5290000277085));
#212002=CARTESIAN_POINT('Ctrl Pts',(-28.1915239974709,-87.9714149112048,
76.0048463754075));
#212003=CARTESIAN_POINT('Ctrl Pts',(-28.2891913837609,-86.2353052989911,
80.1388205889948));
#212004=CARTESIAN_POINT('Ctrl Pts',(-28.3868587700509,-83.225623869312,
83.4623183054996));
#212005=CARTESIAN_POINT('Ctrl Pts',(-28.4845261563409,-79.2835313958541,
85.5986062803239));
#212006=CARTESIAN_POINT('Ctrl Pts',(-28.5821935426309,-74.8558815904194,
86.3055267715799));
#212007=CARTESIAN_POINT('Ctrl Pts',(-28.6798609289209,-70.4445682475821,
85.5029471980399));
#212008=CARTESIAN_POINT('Ctrl Pts',(-28.7775283152109,-66.5496333512407,
83.281843523324));
#212009=CARTESIAN_POINT('Ctrl Pts',(-28.8751957015009,-63.6125850921352,
79.8939877258898));
#212010=CARTESIAN_POINT('Ctrl Pts',(-28.9728630877909,-61.9663509510528,
75.7234083257008));
#212011=CARTESIAN_POINT('Ctrl Pts',(-29.0705304740809,-61.7975388884712,
71.24285904374));
#212012=CARTESIAN_POINT('Ctrl Pts',(-29.1681978603709,-63.125284502366,
66.9602300654889));
#212013=CARTESIAN_POINT('Ctrl Pts',(-29.2658652466609,-65.799081923101,
63.3609764298818));
#212014=CARTESIAN_POINT('Ctrl Pts',(-29.3635326329509,-69.5158443230372,
60.8530895418871));
#212015=CARTESIAN_POINT('Ctrl Pts',(-29.4612000192409,-73.8542601562259,
59.720849532482));
#212016=CARTESIAN_POINT('Ctrl Pts',(-29.5588674055309,-78.3225506956497,
60.0926008416416));
#212017=CARTESIAN_POINT('Ctrl Pts',(-29.6565347918209,-82.4142153388091,
61.9262038053415));
#212018=CARTESIAN_POINT('Ctrl Pts',(-29.7542021781109,-85.6654457033379,
65.0138113738816));
#212019=CARTESIAN_POINT('Ctrl Pts',(-29.8518695644009,-87.7077003696673,
69.0054294992058));
#212020=CARTESIAN_POINT('Ctrl Pts',(-29.9495369506909,-88.3094806897396,
73.4485905166491));
#212021=CARTESIAN_POINT('Ctrl Pts',(-30.0472043369809,-87.4025721882447,
77.8396423667743));
#212022=CARTESIAN_POINT('Ctrl Pts',(-30.1448717232709,-85.0897769767237,
81.6808397959762));
#212023=CARTESIAN_POINT('Ctrl Pts',(-30.2425391095609,-81.6332606770752,
84.5367659943965));
#212024=CARTESIAN_POINT('Ctrl Pts',(-30.3402064958509,-77.4248347825067,
86.0836890275427));
#212025=CARTESIAN_POINT('Ctrl Pts',(-30.4378738821409,-72.9415430824435,
86.14625829066));
#212026=CARTESIAN_POINT('Ctrl Pts',(-30.5355412684309,-68.6915866276478,
84.7173812795336));
#212027=CARTESIAN_POINT('Ctrl Pts',(-30.6332086547209,-65.1567168812421,
81.9590275573886));
#212028=CARTESIAN_POINT('Ctrl Pts',(-30.7308760410109,-62.7376270480277,
78.183868784647));
#212029=CARTESIAN_POINT('Ctrl Pts',(-30.8285434273009,-61.7085317179689,
73.8198359957914));
#212030=CARTESIAN_POINT('Ctrl Pts',(-30.9262108135909,-62.1860834229676,
69.361611713678));
#212031=CARTESIAN_POINT('Ctrl Pts',(-31.0238781998809,-64.1161495536497,
65.3145554857853));
#212032=CARTESIAN_POINT('Ctrl Pts',(-31.1215455861709,-67.2799485313697,
62.1374191322177));
#212033=CARTESIAN_POINT('Ctrl Pts',(-31.2192129724609,-71.3188496730437,
60.1903451869519));
#212034=CARTESIAN_POINT('Ctrl Pts',(-31.3168803587509,-75.7750255738315,
59.6940431400269));
#212035=CARTESIAN_POINT('Ctrl Pts',(-31.4145477450409,-80.1433488793987,
60.7047710354617));
#212036=CARTESIAN_POINT('Ctrl Pts',(-31.5122151313309,-83.9286507177339,
63.1079583717354));
#212037=CARTESIAN_POINT('Ctrl Pts',(-31.6098825176209,-86.7018502927658,
66.6311931776471));
#212038=CARTESIAN_POINT('Ctrl Pts',(-31.7075499039109,-88.1485931006402,
70.8751011206178));
#212039=CARTESIAN_POINT('Ctrl Pts',(-31.8052172902009,-88.1048844106144,
75.3586163632546));
#212040=CARTESIAN_POINT('Ctrl Pts',(-31.9028846764909,-86.575678797071,
79.5735125152463));
#212041=CARTESIAN_POINT('Ctrl Pts',(-32.0005520627809,-83.7343185164689,
83.0420123547065));
#212042=CARTESIAN_POINT('Ctrl Pts',(-32.0982194490709,-79.9028843917455,
85.3709460009163));
#212043=CARTESIAN_POINT('Ctrl Pts',(-32.1958868353609,-75.5156865187867,
86.2963184686414));
#212044=CARTESIAN_POINT('Ctrl Pts',(-32.2935542216509,-71.0700332857199,
85.7132346736072));
#212045=CARTESIAN_POINT('Ctrl Pts',(-32.3912216079409,-67.0698592557778,
83.6877897570761));
#212046=CARTESIAN_POINT('Ctrl Pts',(-32.4888889942309,-63.9686019432188,
80.4495769065115));
#212047=CARTESIAN_POINT('Ctrl Pts',(-32.5865563805209,-62.1178026561958,
76.3656619509228));
#212048=CARTESIAN_POINT('Ctrl Pts',(-32.6842237668109,-61.7272577206776,
71.8989748017325));
#212049=CARTESIAN_POINT('Ctrl Pts',(-32.7818911531009,-62.8412371547143,
67.5558343450567));
#212050=CARTESIAN_POINT('Ctrl Pts',(-32.8795585393909,-65.3334663875495,
63.8285547342751));
#212051=CARTESIAN_POINT('Ctrl Pts',(-32.9772259256809,-68.9214403329571,
61.1396401757894));
#212052=CARTESIAN_POINT('Ctrl Pts',(-33.0748933119709,-73.1984455175702,
59.7938892714003));
#212053=CARTESIAN_POINT('Ctrl Pts',(-33.1725606982609,-77.6796668903304,
59.9438556651611));
#212054=CARTESIAN_POINT('Ctrl Pts',(-33.2702280845509,-81.8571287293036,
61.5725146413969));
#212055=CARTESIAN_POINT('Ctrl Pts',(-33.3678954708409,-85.2573320604846,
64.4953451002813));
#212056=CARTESIAN_POINT('Ctrl Pts',(-33.4330070617009,-86.7489229934631,
67.0855670466063));
#212057=CARTESIAN_POINT('Ctrl Pts',(-33.4655628571309,-87.2587270421088,
68.4679114910338));
#212058=CARTESIAN_POINT('',(-26.6970235948769,-64.1107820886051,68.3402936518987));
#212059=CARTESIAN_POINT('Ctrl Pts',(-22.3657263431209,-78.9572065659953,
84.0781567697157));
#212060=CARTESIAN_POINT('Ctrl Pts',(-22.4113638359009,-77.2042658920752,
84.7036938863734));
#212061=CARTESIAN_POINT('Ctrl Pts',(-22.5026388214709,-73.3978907787715,
85.1071590883939));
#212062=CARTESIAN_POINT('Ctrl Pts',(-22.6395512998309,-68.0405685475501,
83.0382494769742));
#212063=CARTESIAN_POINT('Ctrl Pts',(-22.7764637781809,-64.2196078175175,
78.7512421293735));
#212064=CARTESIAN_POINT('Ctrl Pts',(-22.9133762565409,-62.7778618409869,
73.1924757376221));
#212065=CARTESIAN_POINT('Ctrl Pts',(-23.0502887348909,-64.0336581279753,
67.5887670194206));
#212066=CARTESIAN_POINT('Ctrl Pts',(-23.1872012132509,-67.7098000647524,
63.1769076868417));
#212067=CARTESIAN_POINT('Ctrl Pts',(-23.3241136916009,-72.9949448440006,
60.930624514091));
#212068=CARTESIAN_POINT('Ctrl Pts',(-23.4610261699609,-78.7226196025488,
61.3456896355516));
#212069=CARTESIAN_POINT('Ctrl Pts',(-23.5979386483109,-83.6286848555507,
64.3304948862028));
#212070=CARTESIAN_POINT('Ctrl Pts',(-23.7348511266709,-86.6303355967727,
69.226271763487));
#212071=CARTESIAN_POINT('Ctrl Pts',(-23.8717636050209,-87.0650853842986,
74.9524861359762));
#212072=CARTESIAN_POINT('Ctrl Pts',(-24.0086760833809,-84.83698171689,80.2453202044371));
#212073=CARTESIAN_POINT('Ctrl Pts',(-24.1455885617309,-80.4377835331297,
83.9366063979646));
#212074=CARTESIAN_POINT('Ctrl Pts',(-24.2825010400909,-74.8384263620678,
85.2116505915669));
#212075=CARTESIAN_POINT('Ctrl Pts',(-24.4194135184409,-69.2747296862646,
83.7890411146377));
#212076=CARTESIAN_POINT('Ctrl Pts',(-24.5563259967909,-64.9746424533178,
79.9827583856073));
#212077=CARTESIAN_POINT('Ctrl Pts',(-24.6932384751509,-62.8872256743196,
74.6328771144893));
#212078=CARTESIAN_POINT('Ctrl Pts',(-24.8301509535009,-63.4731876492382,
68.920155609978));
#212079=CARTESIAN_POINT('Ctrl Pts',(-24.9670634318609,-66.6032022425639,
64.105433700007));
#212080=CARTESIAN_POINT('Ctrl Pts',(-25.1039759102109,-71.5864521163174,
61.251356069971));
#212081=CARTESIAN_POINT('Ctrl Pts',(-25.2408883885709,-77.3230972196102,
60.9878387312059));
#212082=CARTESIAN_POINT('Ctrl Pts',(-25.3778008669209,-82.5470176072806,
63.3730419092899));
#212083=CARTESIAN_POINT('Ctrl Pts',(-25.5147133452809,-86.1052554762516,
67.8805336366521));
#212084=CARTESIAN_POINT('Ctrl Pts',(-25.6516258236309,-87.212481417992,
73.5154772357479));
#212085=CARTESIAN_POINT('Ctrl Pts',(-25.7885383019909,-85.6243226056579,
79.0341988976569));
#212086=CARTESIAN_POINT('Ctrl Pts',(-25.9254507803409,-81.6912969855573,
83.2186765115833));
#212087=CARTESIAN_POINT('Ctrl Pts',(-26.0623632587009,-76.2814539762174,
85.1453630258059));
#212088=CARTESIAN_POINT('Ctrl Pts',(-26.1992757370509,-70.5887798524084,
84.3890317273547));
#212089=CARTESIAN_POINT('Ctrl Pts',(-26.3361882154009,-65.8697123503377,
81.116583535284));
#212090=CARTESIAN_POINT('Ctrl Pts',(-26.4731006937609,-63.1657005004853,
76.05037264205));
#212091=CARTESIAN_POINT('Ctrl Pts',(-26.6100131721109,-63.0738532573673,
70.3081733636108));
#212092=CARTESIAN_POINT('Ctrl Pts',(-26.7012881576809,-64.7667989074192,
66.8752138971438));
#212093=CARTESIAN_POINT('Ctrl Pts',(-26.7469256504709,-65.9591325242604,
65.446074912737));
#212094=CARTESIAN_POINT('Ctrl Pts',(-22.5898544533909,-79.1019096116296,
84.483657654596));
#212095=CARTESIAN_POINT('Ctrl Pts',(-22.6354919461809,-77.2848692122853,
85.1320687669441));
#212096=CARTESIAN_POINT('Ctrl Pts',(-22.7267669317509,-73.339306502245,
85.5502874680714));
#212097=CARTESIAN_POINT('Ctrl Pts',(-22.8636794101009,-67.7860832407449,
83.405724105221));
#212098=CARTESIAN_POINT('Ctrl Pts',(-23.0005918884609,-63.8254015621982,
78.9619538973823));
#212099=CARTESIAN_POINT('Ctrl Pts',(-23.1375043668109,-62.3309353067667,
73.1999202731971));
#212100=CARTESIAN_POINT('Ctrl Pts',(-23.2744168451709,-63.6326522563196,
67.391300917951));
#212101=CARTESIAN_POINT('Ctrl Pts',(-23.4113293235209,-67.4432195574419,
62.8181132666061));
#212102=CARTESIAN_POINT('Ctrl Pts',(-23.5482418018809,-72.921626056387,
60.4896903290827));
#212103=CARTESIAN_POINT('Ctrl Pts',(-23.6851542802309,-78.8587445142041,
60.9199331235345));
#212104=CARTESIAN_POINT('Ctrl Pts',(-23.8220667585909,-83.9442096980268,
64.0138836520905));
#212105=CARTESIAN_POINT('Ctrl Pts',(-23.9589792369409,-87.0556217056703,
69.088684245488));
#212106=CARTESIAN_POINT('Ctrl Pts',(-24.0958917153009,-87.5062689747379,
75.0242889153553));
#212107=CARTESIAN_POINT('Ctrl Pts',(-24.2328041936509,-85.1966903119605,
80.5106658775061));
#212108=CARTESIAN_POINT('Ctrl Pts',(-24.3697166720109,-80.6366267892543,
84.3369312149314));
#212109=CARTESIAN_POINT('Ctrl Pts',(-24.5066291503609,-74.8325181040322,
85.6585999086832));
#212110=CARTESIAN_POINT('Ctrl Pts',(-24.6435416287209,-69.0653739102596,
84.1839699166283));
#212111=CARTESIAN_POINT('Ctrl Pts',(-24.7804541070709,-64.6080455253229,
80.2385029690766));
#212112=CARTESIAN_POINT('Ctrl Pts',(-24.9173665854309,-62.4442982438864,
74.6929927610358));
#212113=CARTESIAN_POINT('Ctrl Pts',(-25.0542790637809,-63.0516870715546,
68.7713743524177));
#212114=CARTESIAN_POINT('Ctrl Pts',(-25.1911915421409,-66.2961568081638,
63.7805926607206));
#212115=CARTESIAN_POINT('Ctrl Pts',(-25.3281040204909,-71.4616290202873,
60.8221500654866));
#212116=CARTESIAN_POINT('Ctrl Pts',(-25.4650164988409,-77.408045841156,
60.5489966966417));
#212117=CARTESIAN_POINT('Ctrl Pts',(-25.6019289772009,-82.822989158162,
63.0214195228689));
#212118=CARTESIAN_POINT('Ctrl Pts',(-25.7388414555509,-86.5113409972175,
67.6937365557131));
#212119=CARTESIAN_POINT('Ctrl Pts',(-25.8757539339109,-87.6590548344714,
73.5347329567422));
#212120=CARTESIAN_POINT('Ctrl Pts',(-26.0126664122609,-86.0128218697664,
79.255257536733));
#212121=CARTESIAN_POINT('Ctrl Pts',(-26.1495788906209,-81.9359774279065,
83.5927488094103));
#212122=CARTESIAN_POINT('Ctrl Pts',(-26.2864913689709,-76.328312862688,
85.5898884076402));
#212123=CARTESIAN_POINT('Ctrl Pts',(-26.4234038473309,-70.4274749066969,
84.8059003668431));
#212124=CARTESIAN_POINT('Ctrl Pts',(-26.5603163256809,-65.5358454145695,
81.413788666648));
#212125=CARTESIAN_POINT('Ctrl Pts',(-26.6972288040409,-62.73295605009,76.1623218021048));
#212126=CARTESIAN_POINT('Ctrl Pts',(-26.8341412823909,-62.6377502317761,
70.2101477067446));
#212127=CARTESIAN_POINT('Ctrl Pts',(-26.9254162679609,-64.3926017711426,
66.6516553215257));
#212128=CARTESIAN_POINT('Ctrl Pts',(-26.9710537607409,-65.6285354131264,
65.170257057697));
#212129=CARTESIAN_POINT('Ctrl Pts',(-22.8139825636709,-79.2466126572418,
84.8891585394854));
#212130=CARTESIAN_POINT('Ctrl Pts',(-22.8596200564509,-77.3654725324694,
85.5604436475147));
#212131=CARTESIAN_POINT('Ctrl Pts',(-22.9508950420209,-73.2807222256896,
85.9934158477393));
#212132=CARTESIAN_POINT('Ctrl Pts',(-23.0878075203809,-67.5315979339206,
83.7731987334475));
#212133=CARTESIAN_POINT('Ctrl Pts',(-23.2247199987309,-63.4311953068659,
79.1726656653596));
#212134=CARTESIAN_POINT('Ctrl Pts',(-23.3616324770909,-61.8840087725427,
73.2073648087369));
#212135=CARTESIAN_POINT('Ctrl Pts',(-23.4985449554409,-63.2316463846813,
67.193834816445));
#212136=CARTESIAN_POINT('Ctrl Pts',(-23.6354574338009,-67.1766390501634,
62.4593188463355));
#212137=CARTESIAN_POINT('Ctrl Pts',(-23.7723699121509,-72.8483072688198,
60.0487561440661));
#212138=CARTESIAN_POINT('Ctrl Pts',(-23.9092823905109,-78.9948694259072,
60.4941766115334));
#212139=CARTESIAN_POINT('Ctrl Pts',(-24.0461948688609,-84.2597345405397,
63.6972724180149));
#212140=CARTESIAN_POINT('Ctrl Pts',(-24.1831073472209,-87.4809078145793,
68.9510967275428));
#212141=CARTESIAN_POINT('Ctrl Pts',(-24.3200198255709,-87.9474525651767,
75.0960916947856));
#212142=CARTESIAN_POINT('Ctrl Pts',(-24.4569323039309,-85.5563989069964,
80.776011550622));
#212143=CARTESIAN_POINT('Ctrl Pts',(-24.5938447822809,-80.835470045328,
84.7372560319301));
#212144=CARTESIAN_POINT('Ctrl Pts',(-24.7307572606409,-74.8266098459419,
86.1055492258111));
#212145=CARTESIAN_POINT('Ctrl Pts',(-24.8676697389909,-68.8560181341975,
84.5788987185906));
#212146=CARTESIAN_POINT('Ctrl Pts',(-25.0045822173509,-64.2414485972866,
80.4942475524981));
#212147=CARTESIAN_POINT('Ctrl Pts',(-25.1414946957009,-62.0013708134489,
74.7531084075192));
#212148=CARTESIAN_POINT('Ctrl Pts',(-25.2784071740609,-62.6301864938922,
68.6225930947988));
#212149=CARTESIAN_POINT('Ctrl Pts',(-25.4153196524109,-65.9891113738079,
63.4557516213943));
#212150=CARTESIAN_POINT('Ctrl Pts',(-25.5522321307709,-71.3368059243146,
60.3929440609893));
#212151=CARTESIAN_POINT('Ctrl Pts',(-25.6891446091209,-77.4929944627566,
60.1101546620874));
#212152=CARTESIAN_POINT('Ctrl Pts',(-25.8260570874809,-83.0989607090898,
62.6697971364817));
#212153=CARTESIAN_POINT('Ctrl Pts',(-25.9629695658309,-86.9174265182033,
67.5069394748223));
#212154=CARTESIAN_POINT('Ctrl Pts',(-26.0998820441809,-88.1056282509491,
73.5539886777848));
#212155=CARTESIAN_POINT('Ctrl Pts',(-26.2367945225409,-86.4013211338496,
79.4763161758422));
#212156=CARTESIAN_POINT('Ctrl Pts',(-26.3737070008909,-82.1806578702273,
83.9668211072705));
#212157=CARTESIAN_POINT('Ctrl Pts',(-26.5106194792509,-76.3751717491205,
86.0344137894687));
#212158=CARTESIAN_POINT('Ctrl Pts',(-26.6475319576009,-70.2661699609606,
85.2227690063212));
#212159=CARTESIAN_POINT('Ctrl Pts',(-26.7844444359609,-65.2019784787844,
81.7109937979974));
#212160=CARTESIAN_POINT('Ctrl Pts',(-26.9213569143109,-62.3002115996993,
76.2742709621448));
#212161=CARTESIAN_POINT('Ctrl Pts',(-27.0582693926709,-62.2016472061933,
70.1121220498728));
#212162=CARTESIAN_POINT('Ctrl Pts',(-27.1495443782409,-64.0184046348646,
66.4280967459093));
#212163=CARTESIAN_POINT('Ctrl Pts',(-27.1951818710209,-65.2979383019839,
64.8944392026497));
#212164=CARTESIAN_POINT('Ctrl Pts',(-23.0381106739509,-79.391315702872,
85.2946594243565));
#212165=CARTESIAN_POINT('Ctrl Pts',(-23.0837481667309,-77.4460758526756,
85.9888185280761));
#212166=CARTESIAN_POINT('Ctrl Pts',(-23.1750231523009,-73.2221379491631,
86.4365442274168));
#212167=CARTESIAN_POINT('Ctrl Pts',(-23.3119356306609,-67.2771126271247,
84.1406733616905));
#212168=CARTESIAN_POINT('Ctrl Pts',(-23.4488481090109,-63.0369890515466,
79.3833774333684));
#212169=CARTESIAN_POINT('Ctrl Pts',(-23.5857605873609,-61.4370822383221,
73.2148093443111));
#212170=CARTESIAN_POINT('Ctrl Pts',(-23.7226730657209,-62.830640513026,
66.9963687149763));
#212171=CARTESIAN_POINT('Ctrl Pts',(-23.8595855440709,-66.9100585428538,
62.1005244260995));
#212172=CARTESIAN_POINT('Ctrl Pts',(-23.9964980224309,-72.774988481211,
59.6078219590666));
#212173=CARTESIAN_POINT('Ctrl Pts',(-24.1334105007809,-79.1309943375632,
60.0684200995181));
#212174=CARTESIAN_POINT('Ctrl Pts',(-24.2703229791409,-84.5752593830162,
63.3806611839035));
#212175=CARTESIAN_POINT('Ctrl Pts',(-24.4072354574909,-87.9061939234772,
68.8135092095445));
#212176=CARTESIAN_POINT('Ctrl Pts',(-24.5441479358509,-88.3886361556165,
75.1678944741656));
#212177=CARTESIAN_POINT('Ctrl Pts',(-24.6810604142009,-85.9161075020708,
81.0413572237003));
#212178=CARTESIAN_POINT('Ctrl Pts',(-24.8179728925609,-81.0343133014518,
85.1375808488973));
#212179=CARTESIAN_POINT('Ctrl Pts',(-24.9548853709109,-74.8207015879063,
86.5524985429274));
#212180=CARTESIAN_POINT('Ctrl Pts',(-25.0917978492709,-68.6466623581968,
84.9738275205784));
#212181=CARTESIAN_POINT('Ctrl Pts',(-25.2287103276209,-63.8748516692914,
80.7499921359665));
#212182=CARTESIAN_POINT('Ctrl Pts',(-25.3656228059809,-61.5584433830157,
74.8132240540657));
#212183=CARTESIAN_POINT('Ctrl Pts',(-25.5025352843309,-62.2086859162091,
68.4738118372371));
#212184=CARTESIAN_POINT('Ctrl Pts',(-25.6394477626909,-65.6820659394125,
63.1309105821168));
#212185=CARTESIAN_POINT('Ctrl Pts',(-25.7763602410409,-71.2119828282853,
59.9637380565046));
#212186=CARTESIAN_POINT('Ctrl Pts',(-25.9132727194009,-77.5779430843033,
59.6713126275229));
#212187=CARTESIAN_POINT('Ctrl Pts',(-26.0501851977509,-83.3749322599808,
62.3181747500578));
#212188=CARTESIAN_POINT('Ctrl Pts',(-26.1870976761109,-87.3235120391694,
67.3201423938839));
#212189=CARTESIAN_POINT('Ctrl Pts',(-26.3240101544609,-88.5522016674284,
73.5732443987791));
#212190=CARTESIAN_POINT('Ctrl Pts',(-26.4609226328209,-86.7898203979605,
79.697374814927));
#212191=CARTESIAN_POINT('Ctrl Pts',(-26.5978351111709,-82.4253383125765,
84.3408934050975));
#212192=CARTESIAN_POINT('Ctrl Pts',(-26.7347475895209,-76.4220306355901,
86.4789391713034));
#212193=CARTESIAN_POINT('Ctrl Pts',(-26.8716600678809,-70.1048650152488,
85.6396376458087));
#212194=CARTESIAN_POINT('Ctrl Pts',(-27.0085725462309,-64.8681115430162,
82.0081989293614));
#212195=CARTESIAN_POINT('Ctrl Pts',(-27.1454850245909,-61.8674671493036,
76.3862201221987));
#212196=CARTESIAN_POINT('Ctrl Pts',(-27.2823975029409,-61.7655441806113,
70.0140963930029));
#212197=CARTESIAN_POINT('Ctrl Pts',(-27.3736724885109,-63.6442074985899,
66.2045381702958));
#212198=CARTESIAN_POINT('Ctrl Pts',(-27.4193099813009,-64.967341190849,
64.6186213476101));
#212199=CARTESIAN_POINT('',(-22.5674166601918,-72.2136650090823,84.4952548267707));
#212200=CARTESIAN_POINT('Ctrl Pts',(-22.5675364832709,-72.213605770789,
84.4954770366417));
#212201=CARTESIAN_POINT('Ctrl Pts',(-22.5675364832709,-72.7621512638099,
84.6563729599098));
#212202=CARTESIAN_POINT('Ctrl Pts',(-22.5675364832727,-73.3221605020505,
84.7774848925876));
#212203=CARTESIAN_POINT('Ctrl Pts',(-22.5675364832727,-74.4604827599086,
84.9369083570789));
#212204=CARTESIAN_POINT('Ctrl Pts',(-22.5675364832709,-75.0358317053909,
84.9749462493133));
#212205=CARTESIAN_POINT('Ctrl Pts',(-22.5675364832709,-75.6109582839319,
84.971915110047));
#212206=CARTESIAN_POINT('Ctrl Pts',(-22.5674166601918,-72.213719011673,
84.4950313516973));
#212207=CARTESIAN_POINT('Ctrl Pts',(-22.5674566012175,-72.2106294569051,
84.4942847630103));
#212208=CARTESIAN_POINT('Ctrl Pts',(-22.5674965422431,-72.2075402027097,
84.4935369402495));
#212209=CARTESIAN_POINT('Ctrl Pts',(-22.5675364832687,-72.2044512501038,
84.4927878836052));
#212210=CARTESIAN_POINT('Origin',(-21.6548258024609,-75.,72.98888938658));
#212211=CARTESIAN_POINT('Ctrl Pts',(-25.6386080251009,-61.9352648912724,
73.1571937649659));
#212212=CARTESIAN_POINT('Ctrl Pts',(-25.6711638205309,-61.9162861978364,
71.6839605382664));
#212213=CARTESIAN_POINT('Ctrl Pts',(-25.7362754113909,-62.3814880655743,
68.7313886992026));
#212214=CARTESIAN_POINT('Ctrl Pts',(-25.8339427976809,-64.5096514833231,
64.7848407073371));
#212215=CARTESIAN_POINT('Ctrl Pts',(-25.9316101839709,-67.8269435792709,
61.7683376612345));
#212216=CARTESIAN_POINT('Ctrl Pts',(-26.0292775702609,-71.9573332435009,
60.023712735195));
#212217=CARTESIAN_POINT('Ctrl Pts',(-26.1269449565509,-76.4326227884626,
59.7487539480279));
#212218=CARTESIAN_POINT('Ctrl Pts',(-26.2246123428409,-80.7455181499671,
60.9746218595402));
#212219=CARTESIAN_POINT('Ctrl Pts',(-26.3222797291309,-84.4071334849508,
63.5623608310333));
#212220=CARTESIAN_POINT('Ctrl Pts',(-26.4199471154209,-87.0024084058022,
67.2186386228721));
#212221=CARTESIAN_POINT('Ctrl Pts',(-26.5176145017109,-88.2371569612167,
71.5290000277085));
#212222=CARTESIAN_POINT('Ctrl Pts',(-26.6152818880009,-87.9714149112048,
76.0048463754075));
#212223=CARTESIAN_POINT('Ctrl Pts',(-26.7129492742909,-86.2353052989911,
80.1388205889948));
#212224=CARTESIAN_POINT('Ctrl Pts',(-26.8106166605809,-83.225623869312,
83.4623183054996));
#212225=CARTESIAN_POINT('Ctrl Pts',(-26.9082840468709,-79.2835313958541,
85.5986062803239));
#212226=CARTESIAN_POINT('Ctrl Pts',(-27.0059514331609,-74.8558815904194,
86.3055267715799));
#212227=CARTESIAN_POINT('Ctrl Pts',(-27.1036188194509,-70.4445682475821,
85.5029471980399));
#212228=CARTESIAN_POINT('Ctrl Pts',(-27.2012862057409,-66.5496333512407,
83.281843523324));
#212229=CARTESIAN_POINT('Ctrl Pts',(-27.2989535920309,-63.6125850921352,
79.8939877258898));
#212230=CARTESIAN_POINT('Ctrl Pts',(-27.3966209783209,-61.9663509510528,
75.7234083257008));
#212231=CARTESIAN_POINT('Ctrl Pts',(-27.4942883646109,-61.7975388884712,
71.24285904374));
#212232=CARTESIAN_POINT('Ctrl Pts',(-27.5919557509009,-63.125284502366,
66.9602300654889));
#212233=CARTESIAN_POINT('Ctrl Pts',(-27.6896231371909,-65.799081923101,
63.3609764298818));
#212234=CARTESIAN_POINT('Ctrl Pts',(-27.7872905234809,-69.5158443230372,
60.8530895418871));
#212235=CARTESIAN_POINT('Ctrl Pts',(-27.8849579097709,-73.8542601562259,
59.720849532482));
#212236=CARTESIAN_POINT('Ctrl Pts',(-27.9826252960609,-78.3225506956497,
60.0926008416416));
#212237=CARTESIAN_POINT('Ctrl Pts',(-28.0802926823509,-82.4142153388091,
61.9262038053415));
#212238=CARTESIAN_POINT('Ctrl Pts',(-28.1779600686409,-85.6654457033379,
65.0138113738816));
#212239=CARTESIAN_POINT('Ctrl Pts',(-28.2756274549309,-87.7077003696673,
69.0054294992058));
#212240=CARTESIAN_POINT('Ctrl Pts',(-28.3732948412209,-88.3094806897396,
73.4485905166491));
#212241=CARTESIAN_POINT('Ctrl Pts',(-28.4709622275109,-87.4025721882447,
77.8396423667743));
#212242=CARTESIAN_POINT('Ctrl Pts',(-28.5686296138009,-85.0897769767237,
81.6808397959762));
#212243=CARTESIAN_POINT('Ctrl Pts',(-28.6662970000909,-81.6332606770752,
84.5367659943965));
#212244=CARTESIAN_POINT('Ctrl Pts',(-28.7639643863809,-77.4248347825067,
86.0836890275427));
#212245=CARTESIAN_POINT('Ctrl Pts',(-28.8616317726709,-72.9415430824435,
86.14625829066));
#212246=CARTESIAN_POINT('Ctrl Pts',(-28.9592991589609,-68.6915866276478,
84.7173812795336));
#212247=CARTESIAN_POINT('Ctrl Pts',(-29.0569665452509,-65.1567168812421,
81.9590275573886));
#212248=CARTESIAN_POINT('Ctrl Pts',(-29.1546339315409,-62.7376270480277,
78.183868784647));
#212249=CARTESIAN_POINT('Ctrl Pts',(-29.2523013178309,-61.7085317179689,
73.8198359957914));
#212250=CARTESIAN_POINT('Ctrl Pts',(-29.3499687041209,-62.1860834229676,
69.361611713678));
#212251=CARTESIAN_POINT('Ctrl Pts',(-29.4476360904109,-64.1161495536497,
65.3145554857853));
#212252=CARTESIAN_POINT('Ctrl Pts',(-29.5453034767009,-67.2799485313697,
62.1374191322177));
#212253=CARTESIAN_POINT('Ctrl Pts',(-29.6429708629909,-71.3188496730437,
60.1903451869519));
#212254=CARTESIAN_POINT('Ctrl Pts',(-29.7406382492809,-75.7750255738315,
59.6940431400269));
#212255=CARTESIAN_POINT('Ctrl Pts',(-29.8383056355709,-80.1433488793987,
60.7047710354617));
#212256=CARTESIAN_POINT('Ctrl Pts',(-29.9359730218609,-83.9286507177339,
63.1079583717354));
#212257=CARTESIAN_POINT('Ctrl Pts',(-30.0336404081509,-86.7018502927658,
66.6311931776471));
#212258=CARTESIAN_POINT('Ctrl Pts',(-30.1313077944409,-88.1485931006402,
70.8751011206178));
#212259=CARTESIAN_POINT('Ctrl Pts',(-30.2289751807309,-88.1048844106144,
75.3586163632546));
#212260=CARTESIAN_POINT('Ctrl Pts',(-30.3266425670209,-86.575678797071,
79.5735125152463));
#212261=CARTESIAN_POINT('Ctrl Pts',(-30.4243099533109,-83.7343185164689,
83.0420123547065));
#212262=CARTESIAN_POINT('Ctrl Pts',(-30.5219773396009,-79.9028843917455,
85.3709460009163));
#212263=CARTESIAN_POINT('Ctrl Pts',(-30.6196447258909,-75.5156865187867,
86.2963184686414));
#212264=CARTESIAN_POINT('Ctrl Pts',(-30.7173121121809,-71.0700332857199,
85.7132346736072));
#212265=CARTESIAN_POINT('Ctrl Pts',(-30.8149794984709,-67.0698592557778,
83.6877897570761));
#212266=CARTESIAN_POINT('Ctrl Pts',(-30.9126468847609,-63.9686019432188,
80.4495769065115));
#212267=CARTESIAN_POINT('Ctrl Pts',(-31.0103142710509,-62.1178026561954,
76.3656619509219));
#212268=CARTESIAN_POINT('Ctrl Pts',(-31.1079816573409,-61.7272577206776,
71.8989748017325));
#212269=CARTESIAN_POINT('Ctrl Pts',(-31.2056490436309,-62.8412371547143,
67.5558343450567));
#212270=CARTESIAN_POINT('Ctrl Pts',(-31.3033164299209,-65.3334663875495,
63.8285547342751));
#212271=CARTESIAN_POINT('Ctrl Pts',(-31.4009838162109,-68.9214403329571,
61.1396401757894));
#212272=CARTESIAN_POINT('Ctrl Pts',(-31.4986512025009,-73.1984455175702,
59.7938892714003));
#212273=CARTESIAN_POINT('Ctrl Pts',(-31.5963185887909,-77.6796668903304,
59.9438556651611));
#212274=CARTESIAN_POINT('Ctrl Pts',(-31.6939859750809,-81.8571287293036,
61.5725146413969));
#212275=CARTESIAN_POINT('Ctrl Pts',(-31.7916533613709,-85.2573320604846,
64.4953451002813));
#212276=CARTESIAN_POINT('Ctrl Pts',(-31.8567649522309,-86.7489229934631,
67.0855670466063));
#212277=CARTESIAN_POINT('Ctrl Pts',(-31.8893207476609,-87.2587270421088,
68.4679114910338));
#212278=CARTESIAN_POINT('Ctrl Pts',(-25.8627361353809,-62.3657752641363,
73.1516477833507));
#212279=CARTESIAN_POINT('Ctrl Pts',(-25.8952919308109,-62.3474219583749,
71.7269606756879));
#212280=CARTESIAN_POINT('Ctrl Pts',(-25.9604035216709,-62.7972944506722,
68.8716822599311));
#212281=CARTESIAN_POINT('Ctrl Pts',(-26.0580709079509,-64.8553304284946,
65.0551812864947));
#212282=CARTESIAN_POINT('Ctrl Pts',(-26.1557382942409,-68.0633108051291,
62.1380783308097));
#212283=CARTESIAN_POINT('Ctrl Pts',(-26.2534056805309,-72.0575954829508,
60.4509424484588));
#212284=CARTESIAN_POINT('Ctrl Pts',(-26.3510730668209,-76.3854148683847,
60.1850441289508));
#212285=CARTESIAN_POINT('Ctrl Pts',(-26.4487404531109,-80.5561912986817,
61.3705171264288));
#212286=CARTESIAN_POINT('Ctrl Pts',(-26.5464078394009,-84.0971487427805,
63.8729846813812));
#212287=CARTESIAN_POINT('Ctrl Pts',(-26.6440752256909,-86.6069039217849,
67.4087804655587));
#212288=CARTESIAN_POINT('Ctrl Pts',(-26.7417426119809,-87.8009649273485,
71.577106438364));
#212289=CARTESIAN_POINT('Ctrl Pts',(-26.8394099982709,-87.5439796342222,
75.9054642787186));
#212290=CARTESIAN_POINT('Ctrl Pts',(-26.9370773845609,-85.8650784682753,
79.9032153874961));
#212291=CARTESIAN_POINT('Ctrl Pts',(-27.0347447708509,-82.9545723424687,
83.1171968964905));
#212292=CARTESIAN_POINT('Ctrl Pts',(-27.1324121571409,-79.1423800687866,
85.1830897102328));
#212293=CARTESIAN_POINT('Ctrl Pts',(-27.2300795434309,-74.860630593725,
85.8667156913575));
#212294=CARTESIAN_POINT('Ctrl Pts',(-27.3277469297209,-70.5946792606203,
85.0905827949681));
#212295=CARTESIAN_POINT('Ctrl Pts',(-27.4254143160109,-66.8280906231621,
82.9426691362138));
#212296=CARTESIAN_POINT('Ctrl Pts',(-27.5230817023009,-63.9878242529024,
79.6664502797839));
#212297=CARTESIAN_POINT('Ctrl Pts',(-27.6207490885909,-62.3958369731654,
75.6333002019378));
#212298=CARTESIAN_POINT('Ctrl Pts',(-27.7184164748809,-62.2325876214517,
71.3003943988505));
#212299=CARTESIAN_POINT('Ctrl Pts',(-27.8160838611709,-63.5165812377356,
67.1588870111186));
#212300=CARTESIAN_POINT('Ctrl Pts',(-27.9137512474609,-66.1022714358647,
63.6782363178492));
#212301=CARTESIAN_POINT('Ctrl Pts',(-28.0114186337509,-69.6965587336775,
61.2529895530693));
#212302=CARTESIAN_POINT('Ctrl Pts',(-28.1090860200409,-73.8920146826892,
60.1580592223219));
#212303=CARTESIAN_POINT('Ctrl Pts',(-28.2067534063309,-78.2130656944676,
60.5175605475773));
#212304=CARTESIAN_POINT('Ctrl Pts',(-28.3044207926209,-82.1699014217328,
62.2907424549826));
#212305=CARTESIAN_POINT('Ctrl Pts',(-28.4020881789109,-85.3139969393028,
65.2766068902311));
#212306=CARTESIAN_POINT('Ctrl Pts',(-28.4997555652109,-87.2889550389062,
69.1366928418757));
#212307=CARTESIAN_POINT('Ctrl Pts',(-28.5974229515009,-87.8709054376088,
73.4334424020349));
#212308=CARTESIAN_POINT('Ctrl Pts',(-28.6950903377909,-86.9938814698514,
77.6797999010284));
#212309=CARTESIAN_POINT('Ctrl Pts',(-28.7927577240809,-84.7572977023885,
81.3944218333964));
#212310=CARTESIAN_POINT('Ctrl Pts',(-28.8904251103709,-81.4146808510287,
84.1562392846881));
#212311=CARTESIAN_POINT('Ctrl Pts',(-28.9880924966609,-77.3449314000249,
85.652187965406));
#212312=CARTESIAN_POINT('Ctrl Pts',(-29.0857598829509,-73.009373547253,
85.7126954403171));
#212313=CARTESIAN_POINT('Ctrl Pts',(-29.1834272692409,-68.8994620549307,
84.3309029180553));
#212314=CARTESIAN_POINT('Ctrl Pts',(-29.2810946555309,-65.4810736669192,
81.6634427256689));
#212315=CARTESIAN_POINT('Ctrl Pts',(-29.3787620418209,-63.1416979080774,
78.0126833377833));
#212316=CARTESIAN_POINT('Ctrl Pts',(-29.4764294281109,-62.1465134235629,
73.7924545654214));
#212317=CARTESIAN_POINT('Ctrl Pts',(-29.5740968144009,-62.6083288001179,
69.4811381067028));
#212318=CARTESIAN_POINT('Ctrl Pts',(-29.6717642006909,-64.4747952112035,
65.5674408540281));
#212319=CARTESIAN_POINT('Ctrl Pts',(-29.7694315869809,-67.5343403891965,
62.4949977946519));
#212320=CARTESIAN_POINT('Ctrl Pts',(-29.8670989732709,-71.4401512828104,
60.6120840120799));
#212321=CARTESIAN_POINT('Ctrl Pts',(-29.9647663595609,-75.7494868586634,
60.1321361566154));
#212322=CARTESIAN_POINT('Ctrl Pts',(-30.0624337458509,-79.973864766225,
61.1095584519391));
#212323=CARTESIAN_POINT('Ctrl Pts',(-30.1601011321409,-83.6344329844545,
63.4335557344114));
#212324=CARTESIAN_POINT('Ctrl Pts',(-30.2577685184309,-86.3162498277991,
66.8406925775738));
#212325=CARTESIAN_POINT('Ctrl Pts',(-30.3554359047209,-87.7153194313877,
70.9447548692043));
#212326=CARTESIAN_POINT('Ctrl Pts',(-30.4531032910109,-87.6730510341971,
75.2805288983569));
#212327=CARTESIAN_POINT('Ctrl Pts',(-30.5507706773009,-86.1942359470167,
79.3565353982501));
#212328=CARTESIAN_POINT('Ctrl Pts',(-30.6484380635909,-83.4465044360485,
82.7107409066955));
#212329=CARTESIAN_POINT('Ctrl Pts',(-30.7461054498809,-79.7413240868409,
84.9629313136324));
#212330=CARTESIAN_POINT('Ctrl Pts',(-30.8437728361709,-75.4986935683949,
85.8578108212734));
#212331=CARTESIAN_POINT('Ctrl Pts',(-30.9414402224609,-71.1995339163389,
85.2939408579817));
#212332=CARTESIAN_POINT('Ctrl Pts',(-31.0391076087509,-67.331173995054,
83.335238591712));
#212333=CARTESIAN_POINT('Ctrl Pts',(-31.1367749950409,-64.3321096034267,
80.2037316337721));
#212334=CARTESIAN_POINT('Ctrl Pts',(-31.2344423813309,-62.5422980275575,
76.2543902256492));
#212335=CARTESIAN_POINT('Ctrl Pts',(-31.3321097676209,-62.1646223652701,
71.9348897690366));
#212336=CARTESIAN_POINT('Ctrl Pts',(-31.4297771539109,-63.2418938448422,
67.7348648827743));
#212337=CARTESIAN_POINT('Ctrl Pts',(-31.5274445402009,-65.6519989069735,
64.1304069382318));
#212338=CARTESIAN_POINT('Ctrl Pts',(-31.6251119264909,-69.1217415994551,
61.5300977436921));
#212339=CARTESIAN_POINT('Ctrl Pts',(-31.7227793127809,-73.2578105093222,
60.2286921489302));
#212340=CARTESIAN_POINT('Ctrl Pts',(-31.8204466990709,-77.5913662564109,
60.373716836065));
#212341=CARTESIAN_POINT('Ctrl Pts',(-31.9181140853609,-81.6311719822709,
61.948708089435));
#212342=CARTESIAN_POINT('Ctrl Pts',(-32.0157814716509,-84.9193314953615,
64.7752251657533));
#212343=CARTESIAN_POINT('Ctrl Pts',(-32.0808930625109,-86.3617713844579,
67.2800938763135));
#212344=CARTESIAN_POINT('Ctrl Pts',(-32.1134488579409,-86.8547763224244,
68.616887177359));
#212345=CARTESIAN_POINT('Ctrl Pts',(-26.0868642456509,-62.7962856369908,
73.1461018017394));
#212346=CARTESIAN_POINT('Ctrl Pts',(-26.1194200410809,-62.7785577189135,
71.7699608131093));
#212347=CARTESIAN_POINT('Ctrl Pts',(-26.1845316319409,-63.2131008357698,
69.0119758206586));
#212348=CARTESIAN_POINT('Ctrl Pts',(-26.2821990182309,-65.2010093736661,
65.3255218656522));
#212349=CARTESIAN_POINT('Ctrl Pts',(-26.3798664045209,-68.2996780309902,
62.5078190003945));
#212350=CARTESIAN_POINT('Ctrl Pts',(-26.4775337908109,-72.1578577224007,
60.8781721617226));
#212351=CARTESIAN_POINT('Ctrl Pts',(-26.5752011771009,-76.3382069483097,
60.6213343098834));
#212352=CARTESIAN_POINT('Ctrl Pts',(-26.6728685633909,-80.3668644473949,
61.766412393317));
#212353=CARTESIAN_POINT('Ctrl Pts',(-26.7705359496809,-83.787164000609,
64.1836085317263));
#212354=CARTESIAN_POINT('Ctrl Pts',(-26.8682033359709,-86.2113994377659,
67.5989223082413));
#212355=CARTESIAN_POINT('Ctrl Pts',(-26.9658707222609,-87.3647728934875,
71.6252128490111));
#212356=CARTESIAN_POINT('Ctrl Pts',(-27.0635381085509,-87.1165443572374,
75.8060821820241));
#212357=CARTESIAN_POINT('Ctrl Pts',(-27.1612054948409,-85.4948516375614,
79.6676101859858));
#212358=CARTESIAN_POINT('Ctrl Pts',(-27.2588728811309,-82.6835208156347,
82.7720754874777));
#212359=CARTESIAN_POINT('Ctrl Pts',(-27.3565402674209,-79.0012287417265,
84.7675731401279));
#212360=CARTESIAN_POINT('Ctrl Pts',(-27.4542076537109,-74.8653795970425,
85.4279046111302));
#212361=CARTESIAN_POINT('Ctrl Pts',(-27.5518750400009,-70.7447902736733,
84.6782183919009));
#212362=CARTESIAN_POINT('Ctrl Pts',(-27.6495424262909,-67.1065478950989,
82.6034947491145));
#212363=CARTESIAN_POINT('Ctrl Pts',(-27.7472098125809,-64.3630634136857,
79.4389128336908));
#212364=CARTESIAN_POINT('Ctrl Pts',(-27.8448771988709,-62.8253229952768,
75.543192078198));
#212365=CARTESIAN_POINT('Ctrl Pts',(-27.9425445851609,-62.6676363544306,
71.3579297539833));
#212366=CARTESIAN_POINT('Ctrl Pts',(-28.0402119714509,-63.9078779730934,
67.3575439567693));
#212367=CARTESIAN_POINT('Ctrl Pts',(-28.1378793577409,-66.4054609486044,
63.9954962058266));
#212368=CARTESIAN_POINT('Ctrl Pts',(-28.2355467440309,-69.8772731442938,
61.6528895642723));
#212369=CARTESIAN_POINT('Ctrl Pts',(-28.3332141303209,-73.9297692091192,
60.5952689121647));
#212370=CARTESIAN_POINT('Ctrl Pts',(-28.4308815166109,-78.1035806932568,
60.9425202535141));
#212371=CARTESIAN_POINT('Ctrl Pts',(-28.5285489029009,-81.9255875046266,
62.6552811046037));
#212372=CARTESIAN_POINT('Ctrl Pts',(-28.6262162891909,-84.9625481752439,
65.5394024065493));
#212373=CARTESIAN_POINT('Ctrl Pts',(-28.7238836754809,-86.8702097081482,
69.2679561845011));
#212374=CARTESIAN_POINT('Ctrl Pts',(-28.8215510617709,-87.4323301854809,
73.4182942873751));
#212375=CARTESIAN_POINT('Ctrl Pts',(-28.9192184480609,-86.5851907514749,
77.5199574352398));
#212376=CARTESIAN_POINT('Ctrl Pts',(-29.0168858343509,-84.4248184280816,
81.1080038707725));
#212377=CARTESIAN_POINT('Ctrl Pts',(-29.1145532206409,-81.1961010250256,
83.7757125749618));
#212378=CARTESIAN_POINT('Ctrl Pts',(-29.2122206069309,-77.2650280175932,
85.2206869032595));
#212379=CARTESIAN_POINT('Ctrl Pts',(-29.3098879932209,-73.0772040121119,
85.2791325899756));
#212380=CARTESIAN_POINT('Ctrl Pts',(-29.4075553795109,-69.1073374822569,
83.9444245566035));
#212381=CARTESIAN_POINT('Ctrl Pts',(-29.5052227658009,-65.8054304526251,
81.3678578939925));
#212382=CARTESIAN_POINT('Ctrl Pts',(-29.6028901520909,-63.5457687681484,
77.8414978909712));
#212383=CARTESIAN_POINT('Ctrl Pts',(-29.7005575383809,-62.5844951291497,
73.7650731351128));
#212384=CARTESIAN_POINT('Ctrl Pts',(-29.7982249246709,-63.0305741772578,
69.6006644997806));
#212385=CARTESIAN_POINT('Ctrl Pts',(-29.8958923109609,-64.8334408687264,
65.8203262223269));
#212386=CARTESIAN_POINT('Ctrl Pts',(-29.9935596972509,-67.7887322469773,
62.8525764571267));
#212387=CARTESIAN_POINT('Ctrl Pts',(-30.0912270835409,-71.5614528925225,
61.0338228372305));
#212388=CARTESIAN_POINT('Ctrl Pts',(-30.1888944698309,-75.7239481434376,
60.570229173206));
#212389=CARTESIAN_POINT('Ctrl Pts',(-30.2865618561209,-79.8043806529974,
61.5143458683933));
#212390=CARTESIAN_POINT('Ctrl Pts',(-30.3842292424109,-83.3402152511359,
63.7591530970452));
#212391=CARTESIAN_POINT('Ctrl Pts',(-30.4818966287009,-85.930649362801,
67.0501919774507));
#212392=CARTESIAN_POINT('Ctrl Pts',(-30.5795640149909,-87.2820457621323,
71.0144086177314));
#212393=CARTESIAN_POINT('Ctrl Pts',(-30.6772314012809,-87.2412176577989,
75.2024414334004));
#212394=CARTESIAN_POINT('Ctrl Pts',(-30.7748987875709,-85.8127930969901,
79.1395582812056));
#212395=CARTESIAN_POINT('Ctrl Pts',(-30.8725661738609,-83.1586903556685,
82.3794694586463));
#212396=CARTESIAN_POINT('Ctrl Pts',(-30.9702335601509,-79.5797637819886,
84.5549166263378));
#212397=CARTESIAN_POINT('Ctrl Pts',(-31.0679009464409,-75.4817006180579,
85.4193031739153));
#212398=CARTESIAN_POINT('Ctrl Pts',(-31.1655683327309,-71.329034547002,
84.8746470423661));
#212399=CARTESIAN_POINT('Ctrl Pts',(-31.2632357190209,-67.5924887343543,
82.98268742638));
#212400=CARTESIAN_POINT('Ctrl Pts',(-31.3609031053109,-64.695617263651,
79.9578863610724));
#212401=CARTESIAN_POINT('Ctrl Pts',(-31.4585704916009,-62.9667933989244,
76.1431185004145));
#212402=CARTESIAN_POINT('Ctrl Pts',(-31.5562378778909,-62.6019870098559,
71.970804736377));
#212403=CARTESIAN_POINT('Ctrl Pts',(-31.6539052641809,-63.642550534956,
67.9138954205205));
#212404=CARTESIAN_POINT('Ctrl Pts',(-31.7515726504709,-65.9705314263782,
64.4322591422073));
#212405=CARTESIAN_POINT('Ctrl Pts',(-31.8492400367609,-69.3220428659327,
61.9205553116032));
#212406=CARTESIAN_POINT('Ctrl Pts',(-31.9469074230509,-73.3171755010594,
60.6634950264663));
#212407=CARTESIAN_POINT('Ctrl Pts',(-32.0445748093409,-77.5030656224803,
60.8035780069626));
#212408=CARTESIAN_POINT('Ctrl Pts',(-32.1422421956309,-81.4052152352389,
62.3249015374696));
#212409=CARTESIAN_POINT('Ctrl Pts',(-32.2399095819209,-84.5813309302388,
65.0551052312263));
#212410=CARTESIAN_POINT('Ctrl Pts',(-32.3050211727809,-85.974619775455,
67.4746207060263));
#212411=CARTESIAN_POINT('Ctrl Pts',(-32.3375769682109,-86.4508256027431,
68.7658628636918));
#212412=CARTESIAN_POINT('Ctrl Pts',(-26.3109923559309,-63.226796009855,
73.1405558201252));
#212413=CARTESIAN_POINT('Ctrl Pts',(-26.3435481513609,-63.2096934794613,
71.8129609505269));
#212414=CARTESIAN_POINT('Ctrl Pts',(-26.4086597422209,-63.6289072208686,
69.1522693813868));
#212415=CARTESIAN_POINT('Ctrl Pts',(-26.5063271285109,-65.5466883188414,
65.595862444819));
#212416=CARTESIAN_POINT('Ctrl Pts',(-26.6039945148009,-68.5360452568475,
62.8775596699701));
#212417=CARTESIAN_POINT('Ctrl Pts',(-26.7016619010909,-72.2581199618507,
61.3054018749864));
#212418=CARTESIAN_POINT('Ctrl Pts',(-26.7993292873809,-76.2909990282318,
61.0576244908063));
#212419=CARTESIAN_POINT('Ctrl Pts',(-26.8969966736709,-80.1775375961095,
62.1623076602056));
#212420=CARTESIAN_POINT('Ctrl Pts',(-26.9946640599609,-83.4771792584479,
64.4942323820704));
#212421=CARTESIAN_POINT('Ctrl Pts',(-27.0923314462509,-85.8158949537486,
67.789064150928));
#212422=CARTESIAN_POINT('Ctrl Pts',(-27.1899988325409,-86.9285808596196,
71.6733192596676));
#212423=CARTESIAN_POINT('Ctrl Pts',(-27.2876662188309,-86.6891090802536,
75.7067000853347));
#212424=CARTESIAN_POINT('Ctrl Pts',(-27.3853336051209,-85.1246248068445,
79.4320049844843));
#212425=CARTESIAN_POINT('Ctrl Pts',(-27.4830009914109,-82.4124692887962,
82.4269540784775));
#212426=CARTESIAN_POINT('Ctrl Pts',(-27.5806683777009,-78.860077414659,
84.3520565700369));
#212427=CARTESIAN_POINT('Ctrl Pts',(-27.6783357639909,-74.870128600351,
84.9890935309175));
#212428=CARTESIAN_POINT('Ctrl Pts',(-27.7760031502809,-70.8949012867121,
84.2658539888278));
#212429=CARTESIAN_POINT('Ctrl Pts',(-27.8736705365709,-67.3850051670203,
82.2643203620043));
#212430=CARTESIAN_POINT('Ctrl Pts',(-27.9713379228609,-64.7383025744529,
79.2113753875849));
#212431=CARTESIAN_POINT('Ctrl Pts',(-28.0690053091509,-63.254809017389,
75.453083954434));
#212432=CARTESIAN_POINT('Ctrl Pts',(-28.1666726954409,-63.1026850874199,
71.4154651090891));
#212433=CARTESIAN_POINT('Ctrl Pts',(-28.2643400817309,-64.2991747084623,
67.5562009023972));
#212434=CARTESIAN_POINT('Ctrl Pts',(-28.3620074680209,-66.7086504613652,
64.3127560937844));
#212435=CARTESIAN_POINT('Ctrl Pts',(-28.4596748543109,-70.0579875549346,
62.0527895754544));
#212436=CARTESIAN_POINT('Ctrl Pts',(-28.5573422406009,-73.9675237355834,
61.0324786020043));
#212437=CARTESIAN_POINT('Ctrl Pts',(-28.6550096268909,-77.994095692078,
61.367479959455));
#212438=CARTESIAN_POINT('Ctrl Pts',(-28.7526770131809,-81.6812735875568,
63.0198197542421));
#212439=CARTESIAN_POINT('Ctrl Pts',(-28.8503443994709,-84.6110994112092,
65.8021979228998));
#212440=CARTESIAN_POINT('Ctrl Pts',(-28.9480117857609,-86.4514643773875,
69.3992195271719));
#212441=CARTESIAN_POINT('Ctrl Pts',(-29.0456791720509,-86.99375493335,73.4031461727609));
#212442=CARTESIAN_POINT('Ctrl Pts',(-29.1433465583409,-86.176500033081,
77.3601149694952));
#212443=CARTESIAN_POINT('Ctrl Pts',(-29.2410139446309,-84.0923391537426,
80.8215859081834));
#212444=CARTESIAN_POINT('Ctrl Pts',(-29.3386813309209,-80.9775211989782,
83.3951858652538));
#212445=CARTESIAN_POINT('Ctrl Pts',(-29.4363487172109,-77.1851246351153,
84.789185841132));
#212446=CARTESIAN_POINT('Ctrl Pts',(-29.5340161035009,-73.1450344769205,
84.8455697396331));
#212447=CARTESIAN_POINT('Ctrl Pts',(-29.6316834897909,-69.3152129095361,
83.5579461951267));
#212448=CARTESIAN_POINT('Ctrl Pts',(-29.7293508760809,-66.1297872383019,
81.0722730622718));
#212449=CARTESIAN_POINT('Ctrl Pts',(-29.8270182623709,-63.9498396281978,
77.6703124441067));
#212450=CARTESIAN_POINT('Ctrl Pts',(-29.9246856486609,-63.0224768347345,
73.7376917047466));
#212451=CARTESIAN_POINT('Ctrl Pts',(-30.0223530349509,-63.4528195544114,
69.7201908928029));
#212452=CARTESIAN_POINT('Ctrl Pts',(-30.1200204212409,-65.1920865262802,
66.0732115905697));
#212453=CARTESIAN_POINT('Ctrl Pts',(-30.2176878075309,-68.0431241048049,
63.2101551195605));
#212454=CARTESIAN_POINT('Ctrl Pts',(-30.3153551938209,-71.6827545022938,
61.4555616623674));
#212455=CARTESIAN_POINT('Ctrl Pts',(-30.4130225801109,-75.6984094282703,
61.0083221897941));
#212456=CARTESIAN_POINT('Ctrl Pts',(-30.5106899664009,-79.634896539825,
61.9191332848712));
#212457=CARTESIAN_POINT('Ctrl Pts',(-30.6083573526909,-83.0459975178568,
64.0847504597221));
#212458=CARTESIAN_POINT('Ctrl Pts',(-30.7060247389809,-85.5450488978255,
67.2596913773822));
#212459=CARTESIAN_POINT('Ctrl Pts',(-30.8036921252709,-86.8487720928805,
71.0840623663197));
#212460=CARTESIAN_POINT('Ctrl Pts',(-30.9013595115609,-86.8093842813913,
75.1243539684997));
#212461=CARTESIAN_POINT('Ctrl Pts',(-30.9990268978509,-85.4313502469366,
78.9225811642113));
#212462=CARTESIAN_POINT('Ctrl Pts',(-31.0966942841409,-82.8708762752482,
82.0481980106353));
#212463=CARTESIAN_POINT('Ctrl Pts',(-31.1943616704309,-79.4182034770832,
84.1469019390542));
#212464=CARTESIAN_POINT('Ctrl Pts',(-31.2920290567209,-75.4647076676689,
84.980795526557));
#212465=CARTESIAN_POINT('Ctrl Pts',(-31.3896964430109,-71.4585351776186,
84.4553532267351));
#212466=CARTESIAN_POINT('Ctrl Pts',(-31.4873638293009,-67.8538034736301,
82.630136261015));
#212467=CARTESIAN_POINT('Ctrl Pts',(-31.5850312155909,-65.0591249238588,
79.712041088333));
#212468=CARTESIAN_POINT('Ctrl Pts',(-31.6826986018809,-63.3912887702861,
76.0318467751409));
#212469=CARTESIAN_POINT('Ctrl Pts',(-31.7803659881709,-63.0393516544576,
72.0067197036773));
#212470=CARTESIAN_POINT('Ctrl Pts',(-31.8780333744609,-64.0432072250835,
68.0929259582372));
#212471=CARTESIAN_POINT('Ctrl Pts',(-31.9757007607509,-66.2890639457993,
64.7341113461543));
#212472=CARTESIAN_POINT('Ctrl Pts',(-32.0733681470409,-69.5223441324314,
62.3110128795057));
#212473=CARTESIAN_POINT('Ctrl Pts',(-32.1710355333309,-73.3765404928114,
61.0982979039962));
#212474=CARTESIAN_POINT('Ctrl Pts',(-32.2687029196209,-77.4147649885621,
61.233439177867));
#212475=CARTESIAN_POINT('Ctrl Pts',(-32.3663703059109,-81.1792584882072,
62.7010949855073));
#212476=CARTESIAN_POINT('Ctrl Pts',(-32.4640376922009,-84.2433303651157,
65.3349852966984));
#212477=CARTESIAN_POINT('Ctrl Pts',(-32.5291492830609,-85.5874681664406,
67.6691475357372));
#212478=CARTESIAN_POINT('Ctrl Pts',(-32.5617050784909,-86.0468748830494,
68.9148385500206));
#212479=CARTESIAN_POINT('',(-25.7929823067402,-63.0439337595017,67.8848523453354));
#212480=CARTESIAN_POINT('Ctrl Pts',(-21.8528274563309,-63.9256801348964,
79.922508163981));
#212481=CARTESIAN_POINT('Ctrl Pts',(-21.8943126079409,-62.9293684428046,
78.331207182819));
#212482=CARTESIAN_POINT('Ctrl Pts',(-21.9772829111709,-61.634085238876,
74.7135063587071));
#212483=CARTESIAN_POINT('Ctrl Pts',(-22.1017383660109,-62.1361793310051,
68.9705612798485));
#212484=CARTESIAN_POINT('Ctrl Pts',(-22.2261938208509,-64.992093640751,
63.9630709697879));
#212485=CARTESIAN_POINT('Ctrl Pts',(-22.3506492756909,-69.6791054908813,
60.6069640495695));
#212486=CARTESIAN_POINT('Ctrl Pts',(-22.4751047305309,-75.339685598698,
59.516380349804));
#212487=CARTESIAN_POINT('Ctrl Pts',(-22.5995601853709,-80.9381110935543,
60.8908421950948));
#212488=CARTESIAN_POINT('Ctrl Pts',(-22.7240156402109,-85.4500477813155,
64.47887134835));
#212489=CARTESIAN_POINT('Ctrl Pts',(-22.8484710950509,-88.049950735903,
69.6239686585276));
#212490=CARTESIAN_POINT('Ctrl Pts',(-22.9729265498909,-88.262118873329,
75.3847418289771));
#212491=CARTESIAN_POINT('Ctrl Pts',(-23.0973820047309,-86.0477319607849,
80.7071485391445));
#212492=CARTESIAN_POINT('Ctrl Pts',(-23.2218374595709,-81.8119539092029,
84.6173540230353));
#212493=CARTESIAN_POINT('Ctrl Pts',(-23.3462929144109,-76.3298002796115,
86.3999123553094));
#212494=CARTESIAN_POINT('Ctrl Pts',(-23.4707483692509,-70.6043345825818,
85.7286708365146));
#212495=CARTESIAN_POINT('Ctrl Pts',(-23.5952038240909,-65.6831388635119,
82.726445774969));
#212496=CARTESIAN_POINT('Ctrl Pts',(-23.7196592789309,-62.4666387912098,
77.9425509276692));
#212497=CARTESIAN_POINT('Ctrl Pts',(-23.8441147337709,-61.5433537812183,
72.2522901765632));
#212498=CARTESIAN_POINT('Ctrl Pts',(-23.9685701886109,-63.0822162576926,
66.6968041578817));
#212499=CARTESIAN_POINT('Ctrl Pts',(-24.0930256434509,-66.8016622769115,
62.2925739260189));
#212500=CARTESIAN_POINT('Ctrl Pts',(-24.2174810982909,-72.0211489667569,
59.8454365534837));
#212501=CARTESIAN_POINT('Ctrl Pts',(-24.3419365531309,-77.785672693591,
59.8031420245331));
#212502=CARTESIAN_POINT('Ctrl Pts',(-24.4663920079709,-83.0405050080979,
62.1734289212542));
#212503=CARTESIAN_POINT('Ctrl Pts',(-24.5908474628109,-86.824175125915,
66.5226085068829));
#212504=CARTESIAN_POINT('Ctrl Pts',(-24.7153029176509,-88.4443891690571,
72.0549162569263));
#212505=CARTESIAN_POINT('Ctrl Pts',(-24.8397583724909,-87.6046983680189,
77.7581120451255));
#212506=CARTESIAN_POINT('Ctrl Pts',(-24.9642138273309,-84.4587400856684,
82.588688427932));
#212507=CARTESIAN_POINT('Ctrl Pts',(-25.0886692821709,-79.582126496041,
85.6628006211223));
#212508=CARTESIAN_POINT('Ctrl Pts',(-25.2131247370109,-73.8671272050187,
86.4179803938817));
#212509=CARTESIAN_POINT('Ctrl Pts',(-25.3375801918409,-68.3594052031391,
84.7160584470277));
#212510=CARTESIAN_POINT('Ctrl Pts',(-25.4620356466809,-64.0667172511486,
80.8684145069103));
#212511=CARTESIAN_POINT('Ctrl Pts',(-25.5864911015209,-61.7744355441518,
75.5791186817847));
#212512=CARTESIAN_POINT('Ctrl Pts',(-25.7109465563609,-61.9021857092216,
69.8156825060804));
#212513=CARTESIAN_POINT('Ctrl Pts',(-25.7939168595909,-63.5846031768828,
66.3609771213051));
#212514=CARTESIAN_POINT('Ctrl Pts',(-25.8354020112009,-64.7486531924386,
64.8879315138231));
#212515=CARTESIAN_POINT('Ctrl Pts',(-22.0769555666009,-64.2906021585369,
79.6940309097319));
#212516=CARTESIAN_POINT('Ctrl Pts',(-22.1184407182209,-63.327121022488,
78.155166627284));
#212517=CARTESIAN_POINT('Ctrl Pts',(-22.2014110214409,-62.0745201118013,
74.6566766189857));
#212518=CARTESIAN_POINT('Ctrl Pts',(-22.3258664762809,-62.5600691524593,
69.1029736033338));
#212519=CARTESIAN_POINT('Ctrl Pts',(-22.4503219311209,-65.3218751068457,
64.2604905821706));
#212520=CARTESIAN_POINT('Ctrl Pts',(-22.5747773859609,-69.8544401042544,
61.0149744109849));
#212521=CARTESIAN_POINT('Ctrl Pts',(-22.6992328408009,-75.3284922470942,
59.9603277272687));
#212522=CARTESIAN_POINT('Ctrl Pts',(-22.8236882956409,-80.7424379015931,
61.2894981773207));
#212523=CARTESIAN_POINT('Ctrl Pts',(-22.9481437504809,-85.1056968297407,
64.7592942584412));
#212524=CARTESIAN_POINT('Ctrl Pts',(-23.0725992053209,-87.6199275390778,
69.7348498409864));
#212525=CARTESIAN_POINT('Ctrl Pts',(-23.1970546601609,-87.8251042921967,
75.3057934752901));
#212526=CARTESIAN_POINT('Ctrl Pts',(-23.3215101150009,-85.6836860642405,
80.452815741888));
#212527=CARTESIAN_POINT('Ctrl Pts',(-23.4459655698409,-81.5874857670595,
84.2341717690691));
#212528=CARTESIAN_POINT('Ctrl Pts',(-23.5704210246809,-76.2859805764563,
85.9579910725117));
#212529=CARTESIAN_POINT('Ctrl Pts',(-23.6948764795209,-70.7491809604065,
85.3088683670014));
#212530=CARTESIAN_POINT('Ctrl Pts',(-23.8193319343609,-65.9901489428121,
82.4055729063876));
#212531=CARTESIAN_POINT('Ctrl Pts',(-23.9437873892009,-62.8796392816311,
77.7793174093933));
#212532=CARTESIAN_POINT('Ctrl Pts',(-24.0682428440409,-61.9867784456194,
72.2765626625984));
#212533=CARTESIAN_POINT('Ctrl Pts',(-24.1926982988809,-63.4749321818895,
66.9041415386483));
#212534=CARTESIAN_POINT('Ctrl Pts',(-24.3171537537209,-67.0718146681149,
62.6450399131801));
#212535=CARTESIAN_POINT('Ctrl Pts',(-24.4416092085609,-72.1193083445342,
60.278540840157));
#212536=CARTESIAN_POINT('Ctrl Pts',(-24.5660646634009,-77.6938789465367,
60.2376400044813));
#212537=CARTESIAN_POINT('Ctrl Pts',(-24.6905201182409,-82.7755535352872,
62.5298209857594));
#212538=CARTESIAN_POINT('Ctrl Pts',(-24.8149755730809,-86.434543801599,
66.7356859990377));
#212539=CARTESIAN_POINT('Ctrl Pts',(-24.9394310279209,-88.0013684001015,
72.0856926268273));
#212540=CARTESIAN_POINT('Ctrl Pts',(-25.0638864827609,-87.1893471688506,
77.6009561741625));
#212541=CARTESIAN_POINT('Ctrl Pts',(-25.1883419376009,-84.1470547979677,
82.2723549523412));
#212542=CARTESIAN_POINT('Ctrl Pts',(-25.3127973924409,-79.4311358353121,
85.2451687131141));
#212543=CARTESIAN_POINT('Ctrl Pts',(-25.4372528472809,-73.9044577352793,
85.9754637313838));
#212544=CARTESIAN_POINT('Ctrl Pts',(-25.5617083021209,-68.5782267037815,
84.3296236756515));
#212545=CARTESIAN_POINT('Ctrl Pts',(-25.6861637569609,-64.4269918065508,
80.6087676584068));
#212546=CARTESIAN_POINT('Ctrl Pts',(-25.8106192118009,-62.2102455806975,
75.4937652038599));
#212547=CARTESIAN_POINT('Ctrl Pts',(-25.9350746666409,-62.3337861103748,
69.9202463159047));
#212548=CARTESIAN_POINT('Ctrl Pts',(-26.0180449698709,-63.9607644003393,
66.5793807059784));
#212549=CARTESIAN_POINT('Ctrl Pts',(-26.0595301214809,-65.0864565309473,
65.1548750350942));
#212550=CARTESIAN_POINT('Ctrl Pts',(-22.3010836768809,-64.6555241821984,
79.4655536555077));
#212551=CARTESIAN_POINT('Ctrl Pts',(-22.3425688284909,-63.7248736021842,
77.9791260717798));
#212552=CARTESIAN_POINT('Ctrl Pts',(-22.4255391317209,-62.5149549847303,
74.5998468792995));
#212553=CARTESIAN_POINT('Ctrl Pts',(-22.5499945865609,-62.9839589739056,
69.2353859268549));
#212554=CARTESIAN_POINT('Ctrl Pts',(-22.6744500414009,-65.6516565729139,
64.557910194586));
#212555=CARTESIAN_POINT('Ctrl Pts',(-22.7989054962409,-70.0297747175908,
61.4229847724263));
#212556=CARTESIAN_POINT('Ctrl Pts',(-22.9233609510809,-75.3172988954431,
60.4042751047314));
#212557=CARTESIAN_POINT('Ctrl Pts',(-23.0478164059209,-80.5467647095836,
61.6881541595265));
#212558=CARTESIAN_POINT('Ctrl Pts',(-23.1722718607609,-84.761345878138,
65.0397171684909));
#212559=CARTESIAN_POINT('Ctrl Pts',(-23.2967273156009,-87.1899043422416,
69.8457310233925));
#212560=CARTESIAN_POINT('Ctrl Pts',(-23.4211827704409,-87.3880897110839,
75.2268451215454));
#212561=CARTESIAN_POINT('Ctrl Pts',(-23.5456382252809,-85.3196401677329,
80.1984829445947));
#212562=CARTESIAN_POINT('Ctrl Pts',(-23.6700936801209,-81.3630176249706,
83.8509895150804));
#212563=CARTESIAN_POINT('Ctrl Pts',(-23.7945491349609,-76.2421608733568,
85.5160697897019));
#212564=CARTESIAN_POINT('Ctrl Pts',(-23.9190045898009,-70.8940273382887,
84.8890658975066));
#212565=CARTESIAN_POINT('Ctrl Pts',(-24.0434600446409,-66.2971590221518,
82.0847000378495));
#212566=CARTESIAN_POINT('Ctrl Pts',(-24.1679154994809,-63.2926397720848,
77.6160838911696));
#212567=CARTESIAN_POINT('Ctrl Pts',(-24.2923709543209,-62.4302031100231,
72.3008351486921));
#212568=CARTESIAN_POINT('Ctrl Pts',(-24.4168264091609,-63.8676481060571,
67.1114789194617));
#212569=CARTESIAN_POINT('Ctrl Pts',(-24.5412818640009,-67.3419670592723,
62.9975059003819));
#212570=CARTESIAN_POINT('Ctrl Pts',(-24.6657373188409,-72.2174677222541,
60.7116451268433));
#212571=CARTESIAN_POINT('Ctrl Pts',(-24.7901927736809,-77.6020851994283,
60.6721379844194));
#212572=CARTESIAN_POINT('Ctrl Pts',(-24.9146482285209,-82.5106020624308,
62.8862130502326));
#212573=CARTESIAN_POINT('Ctrl Pts',(-25.0391036833609,-86.044912477272,
66.9487634911396));
#212574=CARTESIAN_POINT('Ctrl Pts',(-25.1635591382009,-87.5583476311469,
72.1164689966782));
#212575=CARTESIAN_POINT('Ctrl Pts',(-25.2880145930409,-86.7739959696993,
77.4438003031567));
#212576=CARTESIAN_POINT('Ctrl Pts',(-25.4124700478809,-83.8353695102982,
81.9560214767265));
#212577=CARTESIAN_POINT('Ctrl Pts',(-25.5369255027209,-79.2801451746127,
84.8275368050828));
#212578=CARTESIAN_POINT('Ctrl Pts',(-25.6613809575609,-73.9417882655686,
85.5329470688847));
#212579=CARTESIAN_POINT('Ctrl Pts',(-25.7858364124009,-68.7970482044449,
83.9431889042894));
#212580=CARTESIAN_POINT('Ctrl Pts',(-25.9102918672409,-64.7872663619598,
80.3491208099199));
#212581=CARTESIAN_POINT('Ctrl Pts',(-26.0347473220809,-62.6460556172474,
75.4084117259451));
#212582=CARTESIAN_POINT('Ctrl Pts',(-26.1592027769209,-62.7653865115381,
70.024810125727));
#212583=CARTESIAN_POINT('Ctrl Pts',(-26.2421730801409,-64.3369256238002,
66.7977842906575));
#212584=CARTESIAN_POINT('Ctrl Pts',(-26.2836582317609,-65.4242598694568,
65.4218185563542));
#212585=CARTESIAN_POINT('Ctrl Pts',(-22.5252117871509,-65.0204462058481,
79.2370764012548));
#212586=CARTESIAN_POINT('Ctrl Pts',(-22.5666969387709,-64.1226261818582,
77.8030855162482));
#212587=CARTESIAN_POINT('Ctrl Pts',(-22.6496672419909,-62.9553898576556,
74.5430171395781));
#212588=CARTESIAN_POINT('Ctrl Pts',(-22.7741226968309,-63.4078487953635,
69.3677982503388));
#212589=CARTESIAN_POINT('Ctrl Pts',(-22.8985781516709,-65.9814380390095,
64.8553298069684));
#212590=CARTESIAN_POINT('Ctrl Pts',(-23.0230336065109,-70.2051093309645,
61.8309951338414));
#212591=CARTESIAN_POINT('Ctrl Pts',(-23.1474890613509,-75.3061055438402,
60.8482224821958));
#212592=CARTESIAN_POINT('Ctrl Pts',(-23.2719445161909,-80.3510915176178,
62.0868101417542));
#212593=CARTESIAN_POINT('Ctrl Pts',(-23.3963999710309,-84.4169949265728,
65.3201400785791));
#212594=CARTESIAN_POINT('Ctrl Pts',(-23.5208554258709,-86.7598811454164,
69.9566122058513));
#212595=CARTESIAN_POINT('Ctrl Pts',(-23.6453108807209,-86.9510751299516,
75.1478967678584));
#212596=CARTESIAN_POINT('Ctrl Pts',(-23.7697663355609,-84.9555942711914,
79.9441501473478));
#212597=CARTESIAN_POINT('Ctrl Pts',(-23.8942217904009,-81.1385494828272,
83.4678072611142));
#212598=CARTESIAN_POINT('Ctrl Pts',(-24.0186772452409,-76.1983411702007,
85.0741485069047));
#212599=CARTESIAN_POINT('Ctrl Pts',(-24.1431327000809,-71.0388737161131,
84.4692634279924));
#212600=CARTESIAN_POINT('Ctrl Pts',(-24.2675881549209,-66.6041691014425,
81.7638271692711));
#212601=CARTESIAN_POINT('Ctrl Pts',(-24.3920436097609,-63.7056402625057,
77.4528503728929));
#212602=CARTESIAN_POINT('Ctrl Pts',(-24.5164990646009,-62.8736277744238,
72.3251076347263));
#212603=CARTESIAN_POINT('Ctrl Pts',(-24.6409545194409,-64.260364030253,
67.3188163002233));
#212604=CARTESIAN_POINT('Ctrl Pts',(-24.7654099742709,-67.6121194504766,
63.3499718875427));
#212605=CARTESIAN_POINT('Ctrl Pts',(-24.8898654291109,-72.3156271000323,
61.1447494135163));
#212606=CARTESIAN_POINT('Ctrl Pts',(-25.0143208839509,-77.5102914523739,
61.1066359643676));
#212607=CARTESIAN_POINT('Ctrl Pts',(-25.1387763387909,-82.2456505896205,
63.2426051147388));
#212608=CARTESIAN_POINT('Ctrl Pts',(-25.2632317936309,-85.655281152956,
67.1618409832944));
#212609=CARTESIAN_POINT('Ctrl Pts',(-25.3876872484709,-87.1153268621918,
72.1472453665801));
#212610=CARTESIAN_POINT('Ctrl Pts',(-25.5121427033109,-86.3586447705307,
77.2866444321927));
#212611=CARTESIAN_POINT('Ctrl Pts',(-25.6365981581509,-83.5236842225936,
81.6396880011264));
#212612=CARTESIAN_POINT('Ctrl Pts',(-25.7610536129909,-79.1291545138833,
84.4099048970747));
#212613=CARTESIAN_POINT('Ctrl Pts',(-25.8855090678309,-73.9791187958291,
85.0904304063868));
#212614=CARTESIAN_POINT('Ctrl Pts',(-26.0099645226709,-69.0158697050855,
83.556754132914));
#212615=CARTESIAN_POINT('Ctrl Pts',(-26.1344199775109,-65.1475409173708,
80.0894739614117));
#212616=CARTESIAN_POINT('Ctrl Pts',(-26.2588754323509,-63.0818656537839,
75.3230582480241));
#212617=CARTESIAN_POINT('Ctrl Pts',(-26.3833308871909,-63.1969869126954,
70.1293739355506));
#212618=CARTESIAN_POINT('Ctrl Pts',(-26.4663011904209,-64.7130868472582,
67.0161878753345));
#212619=CARTESIAN_POINT('Ctrl Pts',(-26.5077863420309,-65.7620632079617,
65.688762077616));
#212620=CARTESIAN_POINT('',(-22.5675364832709,-63.0005606563318,73.0560055650936));
#212621=CARTESIAN_POINT('Ctrl Pts',(-22.5675364832709,-63.0009379796994,
73.0559939530083));
#212622=CARTESIAN_POINT('Ctrl Pts',(-22.5675364832709,-63.030239404122,
73.6283224514651));
#212623=CARTESIAN_POINT('Ctrl Pts',(-22.5675364832698,-63.1004752890019,
74.1992222599949));
#212624=CARTESIAN_POINT('Ctrl Pts',(-22.5675364832698,-63.3236284085513,
75.3219313585469));
#212625=CARTESIAN_POINT('Ctrl Pts',(-22.5675364832709,-63.4751104430327,
75.8722213989227));
#212626=CARTESIAN_POINT('Ctrl Pts',(-22.5675364832709,-63.6650775896172,
76.4088722773802));
#212627=CARTESIAN_POINT('Ctrl Pts',(-22.5673477912806,-63.0003719673623,
73.0560066204831));
#212628=CARTESIAN_POINT('Ctrl Pts',(-22.5674106883502,-63.000278188672,
73.0504855961934));
#212629=CARTESIAN_POINT('Ctrl Pts',(-22.5674735854198,-63.0001882203141,
73.0449644637677));
#212630=CARTESIAN_POINT('Ctrl Pts',(-22.5675364824894,-63.000102062494,
73.0394432284656));
#212631=CARTESIAN_POINT('Origin',(-21.7675364832709,-75.,72.98888938658));
#212632=CARTESIAN_POINT('',(-23.0675424572509,-65.2956417762688,76.9983072327892));
#212633=CARTESIAN_POINT('',(-23.0675424572509,-84.7043582237312,68.9794715403708));
#212634=CARTESIAN_POINT('Origin',(-23.0675424572509,-75.,72.98888938658));
#212635=CARTESIAN_POINT('',(-38.5675364832709,-65.2956417762688,76.9983072327892));
#212636=CARTESIAN_POINT('',(-21.7675364832709,-65.2956417762688,76.9983072327892));
#212637=CARTESIAN_POINT('Origin',(-38.5675364832709,-75.,72.98888938658));
#212638=CARTESIAN_POINT('Origin',(-23.0675424572509,-75.,72.98888938658));
#212639=CARTESIAN_POINT('Origin',(-22.8175393993109,-75.,72.98888938658));
#212640=CARTESIAN_POINT('',(-22.5675364832709,-85.1664763034716,68.7885444915901));
#212641=CARTESIAN_POINT('',(-22.8175393993109,-84.9354173291752,68.8840079888882));
#212642=CARTESIAN_POINT('Origin',(-22.5675364832709,-75.,72.98888938658));
#212643=CARTESIAN_POINT('Origin',(-22.5675364832709,-75.,72.98888938658));
#212644=CARTESIAN_POINT('Origin',(-38.5675364832709,-75.,72.98888938658));
#212645=CARTESIAN_POINT('Origin',(-48.5675364832709,-83.3180213346267,69.5522455184007));
#212646=CARTESIAN_POINT('',(-48.5675364832709,-76.1552807409203,72.5115777382218));
#212647=CARTESIAN_POINT('Origin',(-48.5675364832709,-83.3180213346267,69.5522455184007));
#212648=CARTESIAN_POINT('Origin',(-47.7675364832709,-83.3180213346267,69.5522455184007));
#212649=CARTESIAN_POINT('',(-64.0675410045048,-76.1552807409203,72.5115777382218));
#212650=CARTESIAN_POINT('',(-47.7675364832709,-76.1552807409204,72.5115777382218));
#212651=CARTESIAN_POINT('Origin',(-64.0675410045048,-83.3180213346267,69.5522455184007));
#212652=CARTESIAN_POINT('Origin',(-64.3175392245649,-83.3180213346267,69.5522455184006));
#212653=CARTESIAN_POINT('',(-64.5675367041794,-75.6931730807022,72.7025004821099));
#212654=CARTESIAN_POINT('',(-64.3175392245649,-75.924226752407,72.6070391756115));
#212655=CARTESIAN_POINT('Origin',(-64.5675367039552,-83.3180213346267,69.5522455184007));
#212656=CARTESIAN_POINT('Origin',(-64.5675364832709,-83.3180213346267,69.5522455184007));
#212657=CARTESIAN_POINT('Ctrl Pts',(-64.5675364832709,-92.3390416319356,
70.6705889999386));
#212658=CARTESIAN_POINT('Ctrl Pts',(-64.5675364832709,-92.3115488079351,
71.1096763190362));
#212659=CARTESIAN_POINT('Ctrl Pts',(-64.5675364832708,-92.2516905128383,
71.5466701563317));
#212660=CARTESIAN_POINT('Ctrl Pts',(-64.5675364832708,-92.0696201922871,
72.4106673105199));
#212661=CARTESIAN_POINT('Ctrl Pts',(-64.5675364832709,-91.9469758966146,
72.8375946044303));
#212662=CARTESIAN_POINT('Ctrl Pts',(-64.5675364832709,-91.7945388584896,
73.25356812809));
#212663=CARTESIAN_POINT('Origin',(-45.8894114130409,-83.3180213346267,69.5522455184007));
#212664=CARTESIAN_POINT('',(-63.5674079539854,-86.5607427128165,59.8285649416409));
#212665=CARTESIAN_POINT('Ctrl Pts',(-63.567539947994,-86.5649230506972,
59.8300991896837));
#212666=CARTESIAN_POINT('Ctrl Pts',(-63.5674959499171,-86.5635297248365,
59.829587474225));
#212667=CARTESIAN_POINT('Ctrl Pts',(-63.5674519518401,-86.5621362788099,
59.8290760582622));
#212668=CARTESIAN_POINT('Ctrl Pts',(-63.5674079537632,-86.5607427127462,
59.8285649418516));
#212669=CARTESIAN_POINT('',(-62.9075072593131,-73.8447139480805,73.4661881802199));
#212670=CARTESIAN_POINT('Ctrl Pts',(-63.5674123768639,-86.5606760704595,
59.8286818576752));
#212671=CARTESIAN_POINT('Ctrl Pts',(-63.5537244696136,-86.1049641428571,
59.6767091353507));
#212672=CARTESIAN_POINT('Ctrl Pts',(-63.5400136073417,-85.6391282969738,
59.5569597714857));
#212673=CARTESIAN_POINT('Ctrl Pts',(-63.5129296748257,-84.6949018026879,
59.3838289856031));
#212674=CARTESIAN_POINT('Ctrl Pts',(-63.4995889539748,-84.2176985104596,
59.330549021255));
#212675=CARTESIAN_POINT('Ctrl Pts',(-63.4597780386861,-82.7876084763752,
59.2718310830067));
#212676=CARTESIAN_POINT('Ctrl Pts',(-63.4325802602361,-81.8358809821594,
59.3654163782555));
#212677=CARTESIAN_POINT('Ctrl Pts',(-63.3869424607677,-80.2668114174402,
59.744516418622));
#212678=CARTESIAN_POINT('Ctrl Pts',(-63.3686283032081,-79.6394241802636,
59.9621800299818));
#212679=CARTESIAN_POINT('Ctrl Pts',(-63.3128692356677,-77.8226955709727,
60.7971770385973));
#212680=CARTESIAN_POINT('Ctrl Pts',(-63.2745815754463,-76.7288390210066,
61.5877935685209));
#212681=CARTESIAN_POINT('Ctrl Pts',(-63.2002097006855,-74.9063461491549,
63.5444294238348));
#212682=CARTESIAN_POINT('Ctrl Pts',(-63.1618824850836,-74.1952322716333,
64.6917037744084));
#212683=CARTESIAN_POINT('Ctrl Pts',(-63.1061663303517,-73.4911387374014,
66.563278327776));
#212684=CARTESIAN_POINT('Ctrl Pts',(-63.0878060649446,-73.3185146829425,
67.2046067609665));
#212685=CARTESIAN_POINT('Ctrl Pts',(-63.0553782680594,-73.1303627086226,
68.3273127282598));
#212686=CARTESIAN_POINT('Ctrl Pts',(-63.0417928519769,-73.0844909277082,
68.8014397964857));
#212687=CARTESIAN_POINT('Ctrl Pts',(-63.0081560309446,-73.0525026114093,
69.9923893239146));
#212688=CARTESIAN_POINT('Ctrl Pts',(-62.9884692522367,-73.1082554644126,
70.7077860596406));
#212689=CARTESIAN_POINT('Ctrl Pts',(-62.9483777816462,-73.3679537925859,
72.1157259528594));
#212690=CARTESIAN_POINT('Ctrl Pts',(-62.9277656193976,-73.5712828969068,
72.8043756242868));
#212691=CARTESIAN_POINT('Ctrl Pts',(-62.9075072593131,-73.8447139480805,
73.46618818022));
#212692=CARTESIAN_POINT('Ctrl Pts',(-62.9075072593131,-73.8447139480805,
73.4661881802199));
#212693=CARTESIAN_POINT('Ctrl Pts',(-62.9075071281503,-73.8447157184106,
73.4661924651272));
#212694=CARTESIAN_POINT('Ctrl Pts',(-62.9075069969875,-73.8447174887436,
73.4661967500333));
#212695=CARTESIAN_POINT('Ctrl Pts',(-62.9075068658247,-73.8447192590795,
73.4662010349381));
#212696=CARTESIAN_POINT('Ctrl Pts',(-64.7235137149846,-91.0358871866423,
74.2288240611484));
#212697=CARTESIAN_POINT('Ctrl Pts',(-64.6818903153503,-91.7101176437746,
73.1161259264027));
#212698=CARTESIAN_POINT('Ctrl Pts',(-64.5986435160818,-92.5693071181569,
70.5953071644979));
#212699=CARTESIAN_POINT('Ctrl Pts',(-64.4737733171789,-92.1546318852882,
66.6213799744605));
#212700=CARTESIAN_POINT('Ctrl Pts',(-64.3489031182761,-90.1124097711939,
63.1873940424806));
#212701=CARTESIAN_POINT('Ctrl Pts',(-64.2240329193733,-86.8188823631399,
60.9255881378498));
#212702=CARTESIAN_POINT('Ctrl Pts',(-64.0991627204705,-82.8805899113611,
60.2525763176751));
#212703=CARTESIAN_POINT('Ctrl Pts',(-63.9742925215677,-79.0228616330947,
61.2922934738363));
#212704=CARTESIAN_POINT('Ctrl Pts',(-63.8494223226649,-75.9561779481362,
63.8532574547353));
#212705=CARTESIAN_POINT('Ctrl Pts',(-63.7245521237622,-74.2453345756984,
67.4638112038692));
#212706=CARTESIAN_POINT('Ctrl Pts',(-63.5996819248594,-74.2054195650181,
71.4589945804266));
#212707=CARTESIAN_POINT('Ctrl Pts',(-63.4748117259569,-75.8437841906902,
75.1030097681569));
#212708=CARTESIAN_POINT('Ctrl Pts',(-63.3499415270539,-78.8586886049028,
77.7247325999806));
#212709=CARTESIAN_POINT('Ctrl Pts',(-63.2250713281509,-82.694874402881,
78.8413215436999));
#212710=CARTESIAN_POINT('Ctrl Pts',(-63.1002011292489,-86.6458247360063,
78.2471160211358));
#212711=CARTESIAN_POINT('Ctrl Pts',(-62.9753309303459,-89.9838938499185,
76.0516149086199));
#212712=CARTESIAN_POINT('Ctrl Pts',(-62.8504607314429,-92.0942834014676,
72.6589303077136));
#212713=CARTESIAN_POINT('Ctrl Pts',(-62.7672139321749,-92.4236956643394,
70.0161625645472));
#212714=CARTESIAN_POINT('Ctrl Pts',(-62.7255905325409,-92.3038054643285,
68.72066644786));
#212715=CARTESIAN_POINT('Ctrl Pts',(-64.4993856047086,-91.4041086405805,
74.4519448802345));
#212716=CARTESIAN_POINT('Ctrl Pts',(-64.4577622050742,-92.1105068140245,
73.2861596184454));
#212717=CARTESIAN_POINT('Ctrl Pts',(-64.3745154058057,-93.0106884491278,
70.6450719159536));
#212718=CARTESIAN_POINT('Ctrl Pts',(-64.2496452069029,-92.5762289494608,
66.4815475917031));
#212719=CARTESIAN_POINT('Ctrl Pts',(-64.1247750080001,-90.4365718694728,
62.8837252680371));
#212720=CARTESIAN_POINT('Ctrl Pts',(-63.9999048090973,-86.9859093836459,
60.5140079958518));
#212721=CARTESIAN_POINT('Ctrl Pts',(-63.8750346101945,-82.8597199405946,
59.8088866008653));
#212722=CARTESIAN_POINT('Ctrl Pts',(-63.7501644112917,-78.8179384094302,
60.8982089419637));
#212723=CARTESIAN_POINT('Ctrl Pts',(-63.6252942123889,-75.604942421705,
63.5813572026399));
#212724=CARTESIAN_POINT('Ctrl Pts',(-63.5004240134859,-73.8124742521855,
67.3641714414642));
#212725=CARTESIAN_POINT('Ctrl Pts',(-63.3755538145829,-73.7706548856186,
71.5499660906055));
#212726=CARTESIAN_POINT('Ctrl Pts',(-63.2506836156809,-75.4871863278845,
75.3678382222557));
#212727=CARTESIAN_POINT('Ctrl Pts',(-63.1258134167779,-78.6459326419415,
78.1146441549624));
#212728=CARTESIAN_POINT('Ctrl Pts',(-63.0009432178749,-82.6651438952985,
79.2845058572658));
#212729=CARTESIAN_POINT('Ctrl Pts',(-62.8760730189729,-86.8045951306179,
78.6619506295288));
#212730=CARTESIAN_POINT('Ctrl Pts',(-62.7512028200699,-90.3019244190495,
76.3617015689027));
#212731=CARTESIAN_POINT('Ctrl Pts',(-62.6263326211669,-92.5130012232632,
72.8071510739181));
#212732=CARTESIAN_POINT('Ctrl Pts',(-62.5430858218989,-92.8581298337256,
70.0382961714913));
#212733=CARTESIAN_POINT('Ctrl Pts',(-62.5014624222649,-92.7325196400449,
68.6809915869217));
#212734=CARTESIAN_POINT('Ctrl Pts',(-64.2752574944325,-91.7723300945254,
74.6750656993104));
#212735=CARTESIAN_POINT('Ctrl Pts',(-64.2336340947982,-92.5108959842799,
73.456193310475));
#212736=CARTESIAN_POINT('Ctrl Pts',(-64.1503872955297,-93.4520697801033,
70.6948366673944));
#212737=CARTESIAN_POINT('Ctrl Pts',(-64.0255170966268,-92.9978260136282,
66.3417152089329));
#212738=CARTESIAN_POINT('Ctrl Pts',(-63.900646897724,-90.7607339677282,
62.5800564935892));
#212739=CARTESIAN_POINT('Ctrl Pts',(-63.7757766988212,-87.1529364041481,
60.1024278538446));
#212740=CARTESIAN_POINT('Ctrl Pts',(-63.6509064999184,-82.838849969827,
59.3651968840528));
#212741=CARTESIAN_POINT('Ctrl Pts',(-63.5260363010159,-78.6130151857575,
60.5041244100999));
#212742=CARTESIAN_POINT('Ctrl Pts',(-63.4011661021129,-75.2537068952662,
63.309456950552));
#212743=CARTESIAN_POINT('Ctrl Pts',(-63.2762959032099,-73.3796139286711,
67.2645316790695));
#212744=CARTESIAN_POINT('Ctrl Pts',(-63.1514257043069,-73.3358902062209,
71.6409376007934));
#212745=CARTESIAN_POINT('Ctrl Pts',(-63.0265555054049,-75.1305884650834,
75.6326666763601));
#212746=CARTESIAN_POINT('Ctrl Pts',(-62.9016853065019,-78.4331766789858,
78.5045557099474));
#212747=CARTESIAN_POINT('Ctrl Pts',(-62.7768151075989,-82.6354133877224,
79.7276901708313));
#212748=CARTESIAN_POINT('Ctrl Pts',(-62.6519449086969,-86.9633655252361,
79.0767852379245));
#212749=CARTESIAN_POINT('Ctrl Pts',(-62.5270747097939,-90.6199549881801,
76.6717882291845));
#212750=CARTESIAN_POINT('Ctrl Pts',(-62.4022045108909,-92.9317190450487,
72.9553718401246));
#212751=CARTESIAN_POINT('Ctrl Pts',(-62.3189577116229,-93.2925640031029,
70.0604297784402));
#212752=CARTESIAN_POINT('Ctrl Pts',(-62.2773343119879,-93.1612338157616,
68.6413167259844));
#212753=CARTESIAN_POINT('Ctrl Pts',(-64.0511293841564,-92.1405515484729,
74.8981865183927));
#212754=CARTESIAN_POINT('Ctrl Pts',(-64.0095059845222,-92.911285154521,
73.6262270025224));
#212755=CARTESIAN_POINT('Ctrl Pts',(-63.9262591852536,-93.8934511110742,
70.7446014188501));
#212756=CARTESIAN_POINT('Ctrl Pts',(-63.8013889863508,-93.4194230778007,
66.2018828261753));
#212757=CARTESIAN_POINT('Ctrl Pts',(-63.676518787448,-91.0848960660067,
62.2763877191447));
#212758=CARTESIAN_POINT('Ctrl Pts',(-63.5516485885449,-87.319963424663,
59.6908477118418));
#212759=CARTESIAN_POINT('Ctrl Pts',(-63.4267783896419,-82.817979999059,
58.9215071672393));
#212760=CARTESIAN_POINT('Ctrl Pts',(-63.3019081907399,-78.4080919620894,
60.1100398782211));
#212761=CARTESIAN_POINT('Ctrl Pts',(-63.1770379918369,-74.9024713688351,
63.0375566984567));
#212762=CARTESIAN_POINT('Ctrl Pts',(-63.0521677929339,-72.9467536051585,
67.1648919166654));
#212763=CARTESIAN_POINT('Ctrl Pts',(-62.9272975940309,-72.9011255268212,
71.7319091109724));
#212764=CARTESIAN_POINT('Ctrl Pts',(-62.8024273951289,-74.7739906022782,
75.8974951304588));
#212765=CARTESIAN_POINT('Ctrl Pts',(-62.6775571962259,-78.2204207160243,
78.8944672649293));
#212766=CARTESIAN_POINT('Ctrl Pts',(-62.5526869973229,-82.6056828801404,
80.1708744843959));
#212767=CARTESIAN_POINT('Ctrl Pts',(-62.4278167984199,-87.1221359198457,
79.4916198463129));
#212768=CARTESIAN_POINT('Ctrl Pts',(-62.3029465995179,-90.9379855573115,
76.9818748894682));
#212769=CARTESIAN_POINT('Ctrl Pts',(-62.1780764006149,-93.3504368668442,
73.1035926063291));
#212770=CARTESIAN_POINT('Ctrl Pts',(-62.0948296013469,-93.7269981724799,
70.0825633853881));
#212771=CARTESIAN_POINT('Ctrl Pts',(-62.0532062017119,-93.589947991478,
68.601641865046));
#212772=CARTESIAN_POINT('Origin',(-113.778845940191,-83.3180213346267,69.5522455184007));
#212773=CARTESIAN_POINT('',(-47.1840596451118,-88.6014372352785,74.6727879441187));
#212774=CARTESIAN_POINT('Ctrl Pts',(-47.1840596451125,-88.6014372352776,
74.6727879441184));
#212775=CARTESIAN_POINT('Ctrl Pts',(-47.1330608433754,-88.9445087024433,
73.6555434581613));
#212776=CARTESIAN_POINT('Ctrl Pts',(-47.0897582262311,-89.1384560838077,
72.5407972914318));
#212777=CARTESIAN_POINT('Ctrl Pts',(-47.0209270037,-89.1523705823679,70.0468757692862));
#212778=CARTESIAN_POINT('Ctrl Pts',(-47.002286125824,-88.8674259744689,
68.6660964641815));
#212779=CARTESIAN_POINT('Ctrl Pts',(-47.002286125824,-87.8745905336971,
66.2630466589398));
#212780=CARTESIAN_POINT('Ctrl Pts',(-47.0209270037,-87.1018460587871,65.0838049977557));
#212781=CARTESIAN_POINT('Ctrl Pts',(-47.0897582262311,-85.3317069868201,
63.3269766516198));
#212782=CARTESIAN_POINT('Ctrl Pts',(-47.1330608433754,-84.4074978736294,
62.6742040127388));
#212783=CARTESIAN_POINT('Ctrl Pts',(-47.1840596451125,-83.4464714330091,
62.1957559421795));
#212784=CARTESIAN_POINT('Origin',(-113.778845940191,-85.8955042357612,75.7907615193707));
#212785=CARTESIAN_POINT('Origin',(-113.778845940191,-83.3180213346267,69.5522455184007));
#212786=CARTESIAN_POINT('Origin',(-51.8559251551109,-81.1469531033262,77.7526558780789));
#212787=CARTESIAN_POINT('',(-47.1840596451109,-88.6014372352783,74.6727879441188));
#212788=CARTESIAN_POINT('Origin',(-51.5615184913109,-79.584953311077,71.0945865171214));
#212789=CARTESIAN_POINT('',(0.,0.,0.));
#212790=CARTESIAN_POINT('Origin',(-45.8894114130409,66.6819786653733,69.5522455184007));
#212791=CARTESIAN_POINT('',(-50.2096235848679,76.1552807409204,73.4662010349383));
#212792=CARTESIAN_POINT('',(-49.8038356726598,76.1552807409204,73.4662010349383));
#212793=CARTESIAN_POINT('',(-45.8894114130409,76.1552807409204,73.4662010349383));
#212794=CARTESIAN_POINT('',(-48.3958698180353,76.1552807409204,73.4662010349383));
#212795=CARTESIAN_POINT('Ctrl Pts',(-48.3958698180353,76.1552807409204,
73.4662010349383));
#212796=CARTESIAN_POINT('Ctrl Pts',(-48.4037687557346,76.2613287309383,
73.20952345143));
#212797=CARTESIAN_POINT('Ctrl Pts',(-48.4116574019032,76.356944970118,72.9485353906266));
#212798=CARTESIAN_POINT('Ctrl Pts',(-48.4339259826903,76.5990765131584,
72.1939192103763));
#212799=CARTESIAN_POINT('Ctrl Pts',(-48.4481644740065,76.7191699956859,
71.6928212361976));
#212800=CARTESIAN_POINT('Ctrl Pts',(-48.4804668304725,76.9027546290379,
70.5549183741424));
#212801=CARTESIAN_POINT('Ctrl Pts',(-48.4985952978972,76.945342113167,69.9168971044106));
#212802=CARTESIAN_POINT('Ctrl Pts',(-48.5346717449819,76.9115063939614,
68.6477299765805));
#212803=CARTESIAN_POINT('Ctrl Pts',(-48.5522008346175,76.8363585270069,
68.0192878554966));
#212804=CARTESIAN_POINT('Ctrl Pts',(-48.5881874645723,76.5661488628059,
66.7600297743452));
#212805=CARTESIAN_POINT('Ctrl Pts',(-48.606734672987,76.3671254737777,66.1330050342624));
#212806=CARTESIAN_POINT('Ctrl Pts',(-48.6573395820654,75.6689354911155,
64.4968214357699));
#212807=CARTESIAN_POINT('Ctrl Pts',(-48.6880625247023,75.0616977825945,
63.5436660846541));
#212808=CARTESIAN_POINT('Ctrl Pts',(-48.739015526114,73.8608521574925,62.204934139578));
#212809=CARTESIAN_POINT('Ctrl Pts',(-48.7583175195139,73.3609449818661,
61.7477188811338));
#212810=CARTESIAN_POINT('Ctrl Pts',(-48.796059042918,72.2791716184435,60.9389186280048));
#212811=CARTESIAN_POINT('Ctrl Pts',(-48.8147908553493,71.7000674552926,
60.5891683794301));
#212812=CARTESIAN_POINT('Ctrl Pts',(-48.8432065931581,70.7940124609989,
60.1574724749579));
#212813=CARTESIAN_POINT('Ctrl Pts',(-48.852566274679,70.4905886251576,60.0304247050254));
#212814=CARTESIAN_POINT('Ctrl Pts',(-48.8912166403082,69.2128383647712,
59.5662775268822));
#212815=CARTESIAN_POINT('Ctrl Pts',(-48.919427938587,68.1965338099358,59.3624988825998));
#212816=CARTESIAN_POINT('Ctrl Pts',(-48.9579250010423,66.8377107869516,
59.2981281139376));
#212817=CARTESIAN_POINT('Ctrl Pts',(-48.9673076041839,66.5078590897387,
59.2984239158938));
#212818=CARTESIAN_POINT('Ctrl Pts',(-49.0066694303419,65.1253287082858,
59.3664024584995));
#212819=CARTESIAN_POINT('Ctrl Pts',(-49.0355301697569,64.0863348943344,
59.5804252703959));
#212820=CARTESIAN_POINT('Ctrl Pts',(-49.0821868423022,62.5422577967489,
60.1566346720196));
#212821=CARTESIAN_POINT('Ctrl Pts',(-49.0991802722636,62.0052469917899,
60.4120606482223));
#212822=CARTESIAN_POINT('Ctrl Pts',(-49.13012233562,61.0548081345769,60.9699354003627));
#212823=CARTESIAN_POINT('Ctrl Pts',(-49.1441985481586,60.6360151426799,
61.2596328958899));
#212824=CARTESIAN_POINT('Ctrl Pts',(-49.1763003526447,59.745219303344,61.9793191873202));
#212825=CARTESIAN_POINT('Ctrl Pts',(-49.1943953082071,59.2883409062802,
62.4246968243526));
#212826=CARTESIAN_POINT('Ctrl Pts',(-49.2304152812813,58.4667243851996,
63.3902298965006));
#212827=CARTESIAN_POINT('Ctrl Pts',(-49.2479248385016,58.1029727075256,
63.9076463723527));
#212828=CARTESIAN_POINT('Ctrl Pts',(-49.2838818017038,57.46313467177,65.0239820842643));
#212829=CARTESIAN_POINT('Ctrl Pts',(-49.3024121891235,57.1924629443741,
65.6226996657565));
#212830=CARTESIAN_POINT('Ctrl Pts',(-49.3595038007633,56.5445272508622,
67.5222242852832));
#212831=CARTESIAN_POINT('Ctrl Pts',(-49.3964227051368,56.3654717641162,
68.8750548908138));
#212832=CARTESIAN_POINT('Ctrl Pts',(-49.4733091228004,56.5424912469824,
71.5719324914748));
#212833=CARTESIAN_POINT('Ctrl Pts',(-49.510221663426,56.896749352501,72.8895546193486));
#212834=CARTESIAN_POINT('Ctrl Pts',(-49.574895475561,57.9055700503805,74.9269751209315));
#212835=CARTESIAN_POINT('Ctrl Pts',(-49.6003951472506,58.4244902634698,
75.6944736322653));
#212836=CARTESIAN_POINT('Ctrl Pts',(-49.6510179775926,59.6256474344797,
77.0386154294206));
#212837=CARTESIAN_POINT('Ctrl Pts',(-49.6762791927835,60.2943989035603,
77.6167589378013));
#212838=CARTESIAN_POINT('Ctrl Pts',(-49.7143859716436,61.4303856241312,
78.3678616716475));
#212839=CARTESIAN_POINT('Ctrl Pts',(-49.7277380828874,61.8502202856744,
78.6047827107537));
#212840=CARTESIAN_POINT('Ctrl Pts',(-49.7606212093148,62.9083788763079,
79.1072676512745));
#212841=CARTESIAN_POINT('Ctrl Pts',(-49.7803096542754,63.5598991735905,
79.3395385951356));
#212842=CARTESIAN_POINT('Ctrl Pts',(-49.809309783962,64.5543396785134,79.5845625527446));
#212843=CARTESIAN_POINT('Ctrl Pts',(-49.81865052876,64.8826126321066,79.6486070098387));
#212844=CARTESIAN_POINT('Ctrl Pts',(-49.8457240773373,65.8432715171764,
79.7876783315077));
#212845=CARTESIAN_POINT('Ctrl Pts',(-49.8634779845266,66.4802337956011,
79.8200011829438));
#212846=CARTESIAN_POINT('Ctrl Pts',(-49.8956682408361,67.6142406695973,
79.7719330244282));
#212847=CARTESIAN_POINT('Ctrl Pts',(-49.9099239632596,68.1102123514475,
79.7144930808446));
#212848=CARTESIAN_POINT('Ctrl Pts',(-49.9387558076608,69.116613980445,79.5227818061357));
#212849=CARTESIAN_POINT('Ctrl Pts',(-49.953298889289,69.6248619038611,79.3847674347013));
#212850=CARTESIAN_POINT('Ctrl Pts',(-49.9859711912086,70.7235642242247,
78.9935480757809));
#212851=CARTESIAN_POINT('Ctrl Pts',(-50.0041557488555,71.3053952383275,
78.7226660460105));
#212852=CARTESIAN_POINT('Ctrl Pts',(-50.0403294878874,72.4039618302109,
78.0799256841089));
#212853=CARTESIAN_POINT('Ctrl Pts',(-50.0578945679698,72.9190700521586,
77.7107451119027));
#212854=CARTESIAN_POINT('Ctrl Pts',(-50.0939331145991,73.8937406757216,
76.8656229923043));
#212855=CARTESIAN_POINT('Ctrl Pts',(-50.112507719548,74.3479961766235,76.3879723902262));
#212856=CARTESIAN_POINT('Ctrl Pts',(-50.1577532611111,75.3283343011174,
75.1355452762459));
#212857=CARTESIAN_POINT('Ctrl Pts',(-50.1834334662563,75.799782406457,74.3266459468684));
#212858=CARTESIAN_POINT('Ctrl Pts',(-50.2096235848679,76.1552807409204,
73.4662010349383));
#212859=CARTESIAN_POINT('',(-47.5675364832709,76.1552807409204,73.4662010349383));
#212860=CARTESIAN_POINT('',(-45.8894114130409,76.1552807409204,73.4662010349383));
#212861=CARTESIAN_POINT('',(-47.5675364832709,70.5959341819109,60.0789434428536));
#212862=CARTESIAN_POINT('Origin',(-47.5675364832709,66.6819786653733,69.5522455184007));
#212863=CARTESIAN_POINT('Origin',(-47.5675364832709,66.6819786653733,69.5522455184007));
#212864=CARTESIAN_POINT('',(-47.8635970591063,60.3603339176624,77.6206672715226));
#212865=CARTESIAN_POINT('Ctrl Pts',(-47.8635486253615,60.3604524711489,
77.6207526030933));
#212866=CARTESIAN_POINT('Ctrl Pts',(-47.8770447229994,60.7414549300527,
77.9192609886897));
#212867=CARTESIAN_POINT('Ctrl Pts',(-47.8905699687029,61.1431211104073,
78.1904064651098));
#212868=CARTESIAN_POINT('Ctrl Pts',(-47.9176346715792,61.9720633411651,
78.6683172933885));
#212869=CARTESIAN_POINT('Ctrl Pts',(-47.9311325378684,62.3975386486738,
78.8758519992523));
#212870=CARTESIAN_POINT('Ctrl Pts',(-47.9711994802859,63.7080824833602,
79.4063805704902));
#212871=CARTESIAN_POINT('Ctrl Pts',(-47.9969646798076,64.6248316482197,
79.6376897355961));
#212872=CARTESIAN_POINT('Ctrl Pts',(-48.0398256239384,66.1291426136006,
79.8033176844058));
#212873=CARTESIAN_POINT('Ctrl Pts',(-48.0562070950184,66.7023248501976,
79.818194081424));
#212874=CARTESIAN_POINT('Ctrl Pts',(-48.0866516956205,67.7844183957181,
79.7556167899161));
#212875=CARTESIAN_POINT('Ctrl Pts',(-48.1008081906234,68.2921655831365,
79.687898482524));
#212876=CARTESIAN_POINT('Ctrl Pts',(-48.1330139191397,69.416612921757,79.4512727059462));
#212877=CARTESIAN_POINT('Ctrl Pts',(-48.1511303476015,70.0268823608628,
79.2620636919761));
#212878=CARTESIAN_POINT('Ctrl Pts',(-48.1871871027352,71.1986750551804,
78.7750785443067));
#212879=CARTESIAN_POINT('Ctrl Pts',(-48.2047095997858,71.7581107735901,
78.4793996937978));
#212880=CARTESIAN_POINT('Ctrl Pts',(-48.2406862556106,72.836087400015,77.7753770145317));
#212881=CARTESIAN_POINT('Ctrl Pts',(-48.2592278354088,73.3496821753642,
77.3647138069101));
#212882=CARTESIAN_POINT('Ctrl Pts',(-48.309762124485,74.6244967766751,76.1275155310904));
#212883=CARTESIAN_POINT('Ctrl Pts',(-48.340424579748,75.295158013161,75.2206601665416));
#212884=CARTESIAN_POINT('Ctrl Pts',(-48.380049771524,75.9325315626513,73.9757254447151));
#212885=CARTESIAN_POINT('Ctrl Pts',(-48.3879633739574,76.0491319732533,
73.7231225397456));
#212886=CARTESIAN_POINT('Ctrl Pts',(-48.3958698180353,76.1552807409204,
73.4662010349383));
#212887=CARTESIAN_POINT('',(-47.8257920924624,57.2086760965966,65.6382911956718));
#212888=CARTESIAN_POINT('Ctrl Pts',(-47.8635940884285,60.3587924756686,
77.6194517516841));
#212889=CARTESIAN_POINT('Ctrl Pts',(-47.8609618681876,59.70088034951,77.1037712608345));
#212890=CARTESIAN_POINT('Ctrl Pts',(-47.8579335141401,59.1085127669503,
76.5095387599098));
#212891=CARTESIAN_POINT('Ctrl Pts',(-47.8536397962645,58.0877004162917,
75.1986881766103));
#212892=CARTESIAN_POINT('Ctrl Pts',(-47.852298616386,57.6610466594423,74.4885092324322));
#212893=CARTESIAN_POINT('Ctrl Pts',(-47.8482467829846,57.0964955300793,
73.2254447666302));
#212894=CARTESIAN_POINT('Ctrl Pts',(-47.8461648680152,56.9107710683298,
72.6982574235018));
#212895=CARTESIAN_POINT('Ctrl Pts',(-47.840752948818,56.4876427420712,71.0889018852209));
#212896=CARTESIAN_POINT('Ctrl Pts',(-47.838841880717,56.3813930332953,69.9807652008249));
#212897=CARTESIAN_POINT('Ctrl Pts',(-47.8332362516958,56.5277260695749,
67.7636920917063));
#212898=CARTESIAN_POINT('Ctrl Pts',(-47.828574338379,56.7825592211427,66.6696609455421));
#212899=CARTESIAN_POINT('Ctrl Pts',(-47.8257920924624,57.2086760965966,
65.6382911956718));
#212900=CARTESIAN_POINT('',(-47.8068141272352,61.9759278335054,60.4464459619263));
#212901=CARTESIAN_POINT('Ctrl Pts',(-47.8257920924624,57.2086760965966,
65.6382911956718));
#212902=CARTESIAN_POINT('Ctrl Pts',(-47.8243052474299,57.4363949174851,
65.0871224509692));
#212903=CARTESIAN_POINT('Ctrl Pts',(-47.8231856641482,57.7117738155594,
64.5568916645672));
#212904=CARTESIAN_POINT('Ctrl Pts',(-47.8203484488529,58.3555242944295,
63.5441620336238));
#212905=CARTESIAN_POINT('Ctrl Pts',(-47.8182709902653,58.7237180922336,
63.0643356310678));
#212906=CARTESIAN_POINT('Ctrl Pts',(-47.8141911238361,59.5401196520457,
62.1752216331245));
#212907=CARTESIAN_POINT('Ctrl Pts',(-47.8123348538898,59.9867042257069,
61.7676494127296));
#212908=CARTESIAN_POINT('Ctrl Pts',(-47.8093723566015,60.9409141176522,
61.0399854921903));
#212909=CARTESIAN_POINT('Ctrl Pts',(-47.8082478401419,61.4459602057308,
60.7203433366149));
#212910=CARTESIAN_POINT('Ctrl Pts',(-47.8068141268167,61.9759278333883,
60.446445961702));
#212911=CARTESIAN_POINT('',(-48.1735608262671,61.9759278335638,60.4464459619211));
#212912=CARTESIAN_POINT('',(-47.8068954859909,61.9759278333895,60.4464459616985));
#212913=CARTESIAN_POINT('',(-48.5599506281375,57.2086985431952,65.6382368665521));
#212914=CARTESIAN_POINT('Ctrl Pts',(-48.1735608267226,61.9759278334593,
60.4464459616654));
#212915=CARTESIAN_POINT('Ctrl Pts',(-48.2057390453445,61.4459676212693,
60.720339504118));
#212916=CARTESIAN_POINT('Ctrl Pts',(-48.2381635012091,60.9409268906735,
61.0399772116217));
#212917=CARTESIAN_POINT('Ctrl Pts',(-48.3027869041061,59.9867342135912,
61.7676250678449));
#212918=CARTESIAN_POINT('Ctrl Pts',(-48.3348415809302,59.5401513749368,
62.1751899810842));
#212919=CARTESIAN_POINT('Ctrl Pts',(-48.3987590450242,58.7236761239669,
63.0643784397394));
#212920=CARTESIAN_POINT('Ctrl Pts',(-48.4306399072594,58.3554424481484,
63.5442696368759));
#212921=CARTESIAN_POINT('Ctrl Pts',(-48.4954405792784,57.7117295276132,
64.5569822372555));
#212922=CARTESIAN_POINT('Ctrl Pts',(-48.5278559888906,57.4363874184328,
65.0871495574296));
#212923=CARTESIAN_POINT('Ctrl Pts',(-48.5599506281375,57.2086985431952,
65.6382368665521));
#212924=CARTESIAN_POINT('',(-49.2715796128967,60.3604384525828,77.6207039925157));
#212925=CARTESIAN_POINT('Ctrl Pts',(-48.5599506281375,57.2086985431952,
65.6382368665521));
#212926=CARTESIAN_POINT('Ctrl Pts',(-48.6200116739718,56.7826076977302,
66.6695268548047));
#212927=CARTESIAN_POINT('Ctrl Pts',(-48.6777501611375,56.5277719080271,
67.7634817707358));
#212928=CARTESIAN_POINT('Ctrl Pts',(-48.7973670931621,56.3813781413118,
69.9805110412448));
#212929=CARTESIAN_POINT('Ctrl Pts',(-48.8573471180376,56.4876125809909,
71.0887662129764));
#212930=CARTESIAN_POINT('Ctrl Pts',(-48.945646231306,56.9107583214791,72.6982195125108));
#212931=CARTESIAN_POINT('Ctrl Pts',(-48.9749440674501,57.0964827935491,
73.225411282841));
#212932=CARTESIAN_POINT('Ctrl Pts',(-49.0488658367832,57.6610336028653,
74.4884874003299));
#212933=CARTESIAN_POINT('Ctrl Pts',(-49.0938910637438,58.0876892930809,
75.1986713149217));
#212934=CARTESIAN_POINT('Ctrl Pts',(-49.1831733484294,59.1084952031266,
76.5095188164509));
#212935=CARTESIAN_POINT('Ctrl Pts',(-49.2270302012072,59.7008638570257,
77.1037580932682));
#212936=CARTESIAN_POINT('Ctrl Pts',(-49.2714848090302,60.3587906487603,
77.6194503197282));
#212937=CARTESIAN_POINT('Ctrl Pts',(-49.8038356726598,76.1552807409204,
73.4662010349383));
#212938=CARTESIAN_POINT('Ctrl Pts',(-49.7955673541574,76.0420944588995,
73.7401560750152));
#212939=CARTESIAN_POINT('Ctrl Pts',(-49.7873093511155,75.9170383668382,
74.0091679731417));
#212940=CARTESIAN_POINT('Ctrl Pts',(-49.760094216857,75.4696311167998,74.8715676798369));
#212941=CARTESIAN_POINT('Ctrl Pts',(-49.7409083974812,75.1004089147373,
75.4385040151837));
#212942=CARTESIAN_POINT('Ctrl Pts',(-49.702549221666,74.255343090125,76.4922298043504));
#212943=CARTESIAN_POINT('Ctrl Pts',(-49.683863456909,73.7814231596948,76.9763360851991));
#212944=CARTESIAN_POINT('Ctrl Pts',(-49.6332831714931,72.3961975764906,
78.1365052775401));
#212945=CARTESIAN_POINT('Ctrl Pts',(-49.6009500500924,71.4148252078506,
78.7142310089962));
#212946=CARTESIAN_POINT('Ctrl Pts',(-49.5510767881416,69.745458940248,79.3558000519022));
#212947=CARTESIAN_POINT('Ctrl Pts',(-49.5327091028253,69.1106161156783,
79.5320402969566));
#212948=CARTESIAN_POINT('Ctrl Pts',(-49.4960964344567,67.8407209724448,
79.756140657928));
#212949=CARTESIAN_POINT('Ctrl Pts',(-49.4781072698155,67.2093150345555,
79.8081751924792));
#212950=CARTESIAN_POINT('Ctrl Pts',(-49.4452938123236,66.034101362473,79.7961551901444));
#212951=CARTESIAN_POINT('Ctrl Pts',(-49.4302001837212,65.4923566763925,
79.7474516421501));
#212952=CARTESIAN_POINT('Ctrl Pts',(-49.3917423264305,64.1486951600251,
79.518058201218));
#212953=CARTESIAN_POINT('Ctrl Pts',(-49.3682725668919,63.3598305636744,
79.2835506009118));
#212954=CARTESIAN_POINT('Ctrl Pts',(-49.333283631228,62.2098911532063,78.7853691760749));
#212955=CARTESIAN_POINT('Ctrl Pts',(-49.3212478541936,61.823730788727,78.5881498016359));
#212956=CARTESIAN_POINT('Ctrl Pts',(-49.2966979351889,61.0719719741154,
78.1420527743269));
#212957=CARTESIAN_POINT('Ctrl Pts',(-49.284203110542,60.7076560545366,77.8927747027456));
#212958=CARTESIAN_POINT('Ctrl Pts',(-49.2716572296685,60.3605315571557,
77.6208145648926));
#212959=CARTESIAN_POINT('Origin',(-45.8894114130409,66.6819786653733,69.5522455184007));
#212960=CARTESIAN_POINT('',(-52.0239203182307,76.1552807426645,73.4662010307169));
#212961=CARTESIAN_POINT('',(-51.6180871401245,76.1552807409204,73.4662010349383));
#212962=CARTESIAN_POINT('',(-45.8894114130409,76.1552807409204,73.4662010349383));
#212963=CARTESIAN_POINT('Ctrl Pts',(-50.2096235848679,76.1552807409204,
73.4662010349383));
#212964=CARTESIAN_POINT('Ctrl Pts',(-50.215258731149,76.2317708533604,73.2810650675328));
#212965=CARTESIAN_POINT('Ctrl Pts',(-50.2209205166869,76.3028933202327,
73.0935429919239));
#212966=CARTESIAN_POINT('Ctrl Pts',(-50.2421792944852,76.5482161061884,
72.3845326047184));
#212967=CARTESIAN_POINT('Ctrl Pts',(-50.2579032979113,76.6858529284356,
71.8515923228482));
#212968=CARTESIAN_POINT('Ctrl Pts',(-50.2878406499036,76.8685535542951,
70.8021108337046));
#212969=CARTESIAN_POINT('Ctrl Pts',(-50.3021105145622,76.9185322949097,
70.288075520397));
#212970=CARTESIAN_POINT('Ctrl Pts',(-50.3344513860224,76.9433267853221,
69.1343003712923));
#212971=CARTESIAN_POINT('Ctrl Pts',(-50.3525860612613,76.8973985777643,
68.4962506051938));
#212972=CARTESIAN_POINT('Ctrl Pts',(-50.3886731043959,76.6885542782653,
67.2435798090027));
#212973=CARTESIAN_POINT('Ctrl Pts',(-50.406205972037,76.5273071317408,66.63145727533));
#212974=CARTESIAN_POINT('Ctrl Pts',(-50.4421982095905,76.0856698302883,
65.4213772383649));
#212975=CARTESIAN_POINT('Ctrl Pts',(-50.4607485014187,75.8018687172566,
64.8277274844651));
#212976=CARTESIAN_POINT('Ctrl Pts',(-50.5113921507919,74.8836043771975,
63.3025446990711));
#212977=CARTESIAN_POINT('Ctrl Pts',(-50.5421483544674,74.1495408268806,
62.4416229161454));
#212978=CARTESIAN_POINT('Ctrl Pts',(-50.5931362890703,72.7739063837983,
61.281355191233));
#212979=CARTESIAN_POINT('Ctrl Pts',(-50.6124378411329,72.2154848808551,
60.8977936531927));
#212980=CARTESIAN_POINT('Ctrl Pts',(-50.6501790766708,71.0321009746581,
60.2466336853865));
#212981=CARTESIAN_POINT('Ctrl Pts',(-50.668911435612,70.4101277642476,59.9804704590969));
#212982=CARTESIAN_POINT('Ctrl Pts',(-50.7026488261878,69.2737759090788,
59.6218847490646));
#212983=CARTESIAN_POINT('Ctrl Pts',(-50.7174214577685,68.7699775366072,
59.5038756888099));
#212984=CARTESIAN_POINT('Ctrl Pts',(-50.7413547345326,67.9318869727926,
59.3733398517201));
#212985=CARTESIAN_POINT('Ctrl Pts',(-50.7505851433635,67.6020559068877,
59.3382428579477));
#212986=CARTESIAN_POINT('Ctrl Pts',(-50.7975213204535,65.9217355564926,
59.2415055227305));
#212987=CARTESIAN_POINT('Ctrl Pts',(-50.8360007821808,64.5702333574334,
59.4314817097669));
#212988=CARTESIAN_POINT('Ctrl Pts',(-50.9113416243312,62.0203364285534,
60.3243343480095));
#212989=CARTESIAN_POINT('Ctrl Pts',(-50.9497759551382,60.8467192401891,
61.0179025958921));
#212990=CARTESIAN_POINT('Ctrl Pts',(-51.0047808895067,59.3779771638567,
62.3341359280543));
#212991=CARTESIAN_POINT('Ctrl Pts',(-51.0221410764556,58.9534349461415,
62.7906518478777));
#212992=CARTESIAN_POINT('Ctrl Pts',(-51.0542450765866,58.2609288019876,
63.6863618893438));
#212993=CARTESIAN_POINT('Ctrl Pts',(-51.0688308864643,57.9795001410016,
64.1126185471515));
#212994=CARTESIAN_POINT('Ctrl Pts',(-51.1022187659112,57.401244650137,65.1490151296938));
#212995=CARTESIAN_POINT('Ctrl Pts',(-51.1208774390134,57.1308498382281,
65.7711860632812));
#212996=CARTESIAN_POINT('Ctrl Pts',(-51.1548729987492,56.7615727896548,
66.9199684144007));
#212997=CARTESIAN_POINT('Ctrl Pts',(-51.1699759240402,56.6387670726264,
67.436298939574));
#212998=CARTESIAN_POINT('Ctrl Pts',(-51.2117835909392,56.409960425321,68.8911604270164));
#212999=CARTESIAN_POINT('Ctrl Pts',(-51.2375992875244,56.3926845550487,
69.8382887136384));
#213000=CARTESIAN_POINT('Ctrl Pts',(-51.2824202947342,56.5816756122398,
71.4120497051338));
#213001=CARTESIAN_POINT('Ctrl Pts',(-51.3008195271194,56.7180181712124,
72.0411193268221));
#213002=CARTESIAN_POINT('Ctrl Pts',(-51.3329146097462,57.0641612981642,
73.1316242487666));
#213003=CARTESIAN_POINT('Ctrl Pts',(-51.3468118683537,57.2509199578285,
73.5981691204401));
#213004=CARTESIAN_POINT('Ctrl Pts',(-51.3702006408015,57.6168709078841,
74.3477352292522));
#213005=CARTESIAN_POINT('Ctrl Pts',(-51.3795720312953,57.777074511288,74.6390500289914));
#213006=CARTESIAN_POINT('Ctrl Pts',(-51.4025097249837,58.2006412733255,
75.3277306857662));
#213007=CARTESIAN_POINT('Ctrl Pts',(-51.4161202137029,58.4781100706131,
75.7155119559278));
#213008=CARTESIAN_POINT('Ctrl Pts',(-51.4429325966715,59.0846579218839,
76.4493165724212));
#213009=CARTESIAN_POINT('Ctrl Pts',(-51.4561078238984,59.4129517352115,
76.7944913294035));
#213010=CARTESIAN_POINT('Ctrl Pts',(-51.4875650093103,60.2430336687177,
77.5537380621337));
#213011=CARTESIAN_POINT('Ctrl Pts',(-51.5059390037119,60.7625703287845,
77.9453668480491));
#213012=CARTESIAN_POINT('Ctrl Pts',(-51.5339183197109,61.6006904643938,
78.4603850333636));
#213013=CARTESIAN_POINT('Ctrl Pts',(-51.5434030417052,61.8941545437064,
78.6214893759789));
#213014=CARTESIAN_POINT('Ctrl Pts',(-51.5729128059712,62.8412318771266,
79.0826086525093));
#213015=CARTESIAN_POINT('Ctrl Pts',(-51.5927914030891,63.5187973148232,
79.3284127139547));
#213016=CARTESIAN_POINT('Ctrl Pts',(-51.627422427949,64.7069477918233,79.6228502184274));
#213017=CARTESIAN_POINT('Ctrl Pts',(-51.64185928514,65.2057244561556,79.7079580209407));
#213018=CARTESIAN_POINT('Ctrl Pts',(-51.6735664554794,66.3219861829472,
79.8144286228162));
#213019=CARTESIAN_POINT('Ctrl Pts',(-51.690559709204,66.9392594697799,79.8175173393829));
#213020=CARTESIAN_POINT('Ctrl Pts',(-51.7267421583254,68.2253519616075,
79.7078230822468));
#213021=CARTESIAN_POINT('Ctrl Pts',(-51.7459449177058,68.8903332106317,
79.5842398505121));
#213022=CARTESIAN_POINT('Ctrl Pts',(-51.7941678792632,70.5221966859855,
79.1107358518104));
#213023=CARTESIAN_POINT('Ctrl Pts',(-51.8221806889857,71.4577310668171,
78.6793590652402));
#213024=CARTESIAN_POINT('Ctrl Pts',(-51.8681523655424,72.8122167852181,
77.7886683920298));
#213025=CARTESIAN_POINT('Ctrl Pts',(-51.8852020977137,73.2811631637889,
77.4179469403853));
#213026=CARTESIAN_POINT('Ctrl Pts',(-51.9241413610066,74.2930967616012,
76.4634319740288));
#213027=CARTESIAN_POINT('Ctrl Pts',(-51.9461415204161,74.8056691700268,
75.8529812943268));
#213028=CARTESIAN_POINT('Ctrl Pts',(-51.9865585443683,75.589107391047,74.6632673224413));
#213029=CARTESIAN_POINT('Ctrl Pts',(-52.0045251847382,75.8863758838689,
74.1062080654862));
#213030=CARTESIAN_POINT('Ctrl Pts',(-52.0227265369482,76.1388961978591,
73.505682972861));
#213031=CARTESIAN_POINT('Ctrl Pts',(-52.0233235272473,76.14711965887,73.4859540432173));
#213032=CARTESIAN_POINT('Ctrl Pts',(-52.0239203182307,76.1552807444086,
73.4662010264956));
#213033=CARTESIAN_POINT('Ctrl Pts',(-51.6180871401244,76.1552807409204,
73.4662010349383));
#213034=CARTESIAN_POINT('Ctrl Pts',(-51.608868021914,76.0304223264424,73.7684071974832));
#213035=CARTESIAN_POINT('Ctrl Pts',(-51.5995742545812,75.8909546857845,
74.0649988866438));
#213036=CARTESIAN_POINT('Ctrl Pts',(-51.5808374233716,75.5823062716353,
74.6469438444561));
#213037=CARTESIAN_POINT('Ctrl Pts',(-51.5714220806443,75.4133747445076,
74.9313259570918));
#213038=CARTESIAN_POINT('Ctrl Pts',(-51.5488061946735,74.9704115815491,
75.60100464812));
#213039=CARTESIAN_POINT('Ctrl Pts',(-51.5357249876376,74.682904723647,75.9764804561156));
#213040=CARTESIAN_POINT('Ctrl Pts',(-51.5132823918292,74.1520734221524,
76.5785749741797));
#213041=CARTESIAN_POINT('Ctrl Pts',(-51.5040042547753,73.921766249813,76.815653470945));
#213042=CARTESIAN_POINT('Ctrl Pts',(-51.4804745361526,73.3140027491484,
77.3836095300202));
#213043=CARTESIAN_POINT('Ctrl Pts',(-51.466148886558,72.9229552981338,77.6986688597706));
#213044=CARTESIAN_POINT('Ctrl Pts',(-51.4337100285468,71.9797236645986,
78.3506898251033));
#213045=CARTESIAN_POINT('Ctrl Pts',(-51.415927136167,71.4155743166433,78.6666187043906));
#213046=CARTESIAN_POINT('Ctrl Pts',(-51.3715379616585,69.9682202306324,
79.3062992100124));
#213047=CARTESIAN_POINT('Ctrl Pts',(-51.344650347868,69.0630318258767,79.5658133489809));
#213048=CARTESIAN_POINT('Ctrl Pts',(-51.3040111510123,67.6239691693562,
79.7719282461753));
#213049=CARTESIAN_POINT('Ctrl Pts',(-51.2896819770196,67.1078944552536,
79.8064084279483));
#213050=CARTESIAN_POINT('Ctrl Pts',(-51.2561246723312,65.915211626826,79.7958712874477));
#213051=CARTESIAN_POINT('Ctrl Pts',(-51.2367833257127,65.2412543980353,
79.7229927781949));
#213052=CARTESIAN_POINT('Ctrl Pts',(-51.2020430143689,64.037273773024,79.4706552983997));
#213053=CARTESIAN_POINT('Ctrl Pts',(-51.1867380171011,63.5052434517304,
79.313273794622));
#213054=CARTESIAN_POINT('Ctrl Pts',(-51.1397423602316,61.9392746274684,
78.7083636173971));
#213055=CARTESIAN_POINT('Ctrl Pts',(-51.1075820319353,60.96385046603,78.1330818339147));
#213056=CARTESIAN_POINT('Ctrl Pts',(-51.0579012620402,59.5980236625747,
76.9893960511723));
#213057=CARTESIAN_POINT('Ctrl Pts',(-51.0395589195514,59.1362774011232,
76.5204597823409));
#213058=CARTESIAN_POINT('Ctrl Pts',(-51.0029847118296,58.3245251594762,
75.5200386220687));
#213059=CARTESIAN_POINT('Ctrl Pts',(-50.9850016462149,57.9726797226433,
74.9937262870521));
#213060=CARTESIAN_POINT('Ctrl Pts',(-50.9495338631929,57.3671496842344,
73.8770771803941));
#213061=CARTESIAN_POINT('Ctrl Pts',(-50.931788174642,57.1158852502217,73.2885620467056));
#213062=CARTESIAN_POINT('Ctrl Pts',(-50.8990900924942,56.7633089730634,
72.1884355348597));
#213063=CARTESIAN_POINT('Ctrl Pts',(-50.884318789014,56.643041943573,71.6851433128602));
#213064=CARTESIAN_POINT('Ctrl Pts',(-50.8543697421257,56.4751158280907,
70.6377859722055));
#213065=CARTESIAN_POINT('Ctrl Pts',(-50.8393342677898,56.4318924015049,
70.094630897655));
#213066=CARTESIAN_POINT('Ctrl Pts',(-50.7920628773332,56.4321606123153,
68.4057208376649));
#213067=CARTESIAN_POINT('Ctrl Pts',(-50.7593468225165,56.6241629378768,
67.2689077627035));
#213068=CARTESIAN_POINT('Ctrl Pts',(-50.6897388705989,57.4435640292053,
64.9111296610566));
#213069=CARTESIAN_POINT('Ctrl Pts',(-50.6512748709611,58.1351583630064,
63.7350182101061));
#213070=CARTESIAN_POINT('Ctrl Pts',(-50.5953317222099,59.4708205207166,
62.2385426218951));
#213071=CARTESIAN_POINT('Ctrl Pts',(-50.5770569961627,59.9525180000706,
61.7930314647408));
#213072=CARTESIAN_POINT('Ctrl Pts',(-50.540579454897,60.9752307744137,61.0144877782618));
#213073=CARTESIAN_POINT('Ctrl Pts',(-50.522607632927,61.5112610278961,60.6795923034354));
#213074=CARTESIAN_POINT('Ctrl Pts',(-50.4872521942371,62.6419766901064,
60.1106238810853));
#213075=CARTESIAN_POINT('Ctrl Pts',(-50.4696151902856,63.2345912966788,
59.8784999691666));
#213076=CARTESIAN_POINT('Ctrl Pts',(-50.437442117871,64.3275149771177,59.5636879839881));
#213077=CARTESIAN_POINT('Ctrl Pts',(-50.4230938276373,64.8197308052738,
59.4603274320877));
#213078=CARTESIAN_POINT('Ctrl Pts',(-50.3908112378872,65.9508156837442,
59.3084092275465));
#213079=CARTESIAN_POINT('Ctrl Pts',(-50.3731959748618,66.5906628475814,
59.2827545477454));
#213080=CARTESIAN_POINT('Ctrl Pts',(-50.3286438051655,68.1768670943357,
59.3674848671068));
#213081=CARTESIAN_POINT('Ctrl Pts',(-50.3014079559287,69.1133879687202,
59.5496309642269));
#213082=CARTESIAN_POINT('Ctrl Pts',(-50.2559043856523,70.6532771957255,
60.0784980654637));
#213083=CARTESIAN_POINT('Ctrl Pts',(-50.2370734900478,71.2716715836135,
60.3621519386172));
#213084=CARTESIAN_POINT('Ctrl Pts',(-50.2030497788706,72.3090274993817,
60.968977524793));
#213085=CARTESIAN_POINT('Ctrl Pts',(-50.1880912515587,72.7396902152464,
61.2673015705171));
#213086=CARTESIAN_POINT('Ctrl Pts',(-50.1589096202985,73.5425331237562,
61.9196349199222));
#213087=CARTESIAN_POINT('Ctrl Pts',(-50.1447648340832,73.9146903458592,
62.2713226589861));
#213088=CARTESIAN_POINT('Ctrl Pts',(-50.1131010384993,74.6769982649702,
63.1080767011721));
#213089=CARTESIAN_POINT('Ctrl Pts',(-50.0955377374664,75.0524179368028,
63.6038521619826));
#213090=CARTESIAN_POINT('Ctrl Pts',(-50.0394765787788,76.0948692088835,
65.2763779318886));
#213091=CARTESIAN_POINT('Ctrl Pts',(-50.0025913316872,76.5756587319114,
66.5521388207159));
#213092=CARTESIAN_POINT('Ctrl Pts',(-49.9257292001042,77.0153057608379,
69.2179582231263));
#213093=CARTESIAN_POINT('Ctrl Pts',(-49.8888061641626,76.9693013427971,
70.5819990789817));
#213094=CARTESIAN_POINT('Ctrl Pts',(-49.8409269575123,76.5841559806981,
72.2204391079391));
#213095=CARTESIAN_POINT('Ctrl Pts',(-49.8314919310145,76.4926971245251,
72.5392471507234));
#213096=CARTESIAN_POINT('Ctrl Pts',(-49.8160235298243,76.3155897230452,
73.0599197033263));
#213097=CARTESIAN_POINT('Ctrl Pts',(-49.8099262462807,76.2386555387497,
73.2644014380888));
#213098=CARTESIAN_POINT('Ctrl Pts',(-49.8038356726598,76.1552807409204,
73.4662010349383));
#213099=CARTESIAN_POINT('Origin',(-45.8894114130409,66.6819786653733,69.5522455184007));
#213100=CARTESIAN_POINT('',(-53.8378263137955,76.1552807455499,73.466201023733));
#213101=CARTESIAN_POINT('',(-53.4317936414903,76.1552807404427,73.4662010360945));
#213102=CARTESIAN_POINT('',(-45.8894114130409,76.1552807409204,73.4662010349383));
#213103=CARTESIAN_POINT('Ctrl Pts',(-52.0239203182307,76.1552807444086,
73.4662010264956));
#213104=CARTESIAN_POINT('Ctrl Pts',(-52.0422770108351,76.4063075573506,
72.858618026633));
#213105=CARTESIAN_POINT('Ctrl Pts',(-52.0605483699871,76.5983190601092,
72.2282486121129));
#213106=CARTESIAN_POINT('Ctrl Pts',(-52.0942628601814,76.8342785922126,
71.0613553893792));
#213107=CARTESIAN_POINT('Ctrl Pts',(-52.109509966037,76.8990097012618,70.5314701813668));
#213108=CARTESIAN_POINT('Ctrl Pts',(-52.1377410506788,76.9426856907785,
69.5302689434039));
#213109=CARTESIAN_POINT('Ctrl Pts',(-52.1507348112528,76.9309299040568,
69.060722143021));
#213110=CARTESIAN_POINT('Ctrl Pts',(-52.1731866449851,76.8558199394255,
68.2611254536285));
#213111=CARTESIAN_POINT('Ctrl Pts',(-52.182565470545,76.8083537049086,67.9303442100052));
#213112=CARTESIAN_POINT('Ctrl Pts',(-52.2061707517896,76.6496055737009,
67.1110392915593));
#213113=CARTESIAN_POINT('Ctrl Pts',(-52.2204691358635,76.5185141995445,
66.6272430319727));
#213114=CARTESIAN_POINT('Ctrl Pts',(-52.2531015304926,76.13624179264,65.5390740212308));
#213115=CARTESIAN_POINT('Ctrl Pts',(-52.2710913175403,75.8615386249818,
64.9452597677298));
#213116=CARTESIAN_POINT('Ctrl Pts',(-52.3083464588001,75.1917083740434,
63.7987522187586));
#213117=CARTESIAN_POINT('Ctrl Pts',(-52.3275849779464,74.7944341841179,
63.2509572402287));
#213118=CARTESIAN_POINT('Ctrl Pts',(-52.3708967128673,73.7800974002242,
62.1087183049267));
#213119=CARTESIAN_POINT('Ctrl Pts',(-52.3942775022462,73.136655343858,61.5443408291167));
#213120=CARTESIAN_POINT('Ctrl Pts',(-52.4439219816563,71.6801798906722,
60.5576647839447));
#213121=CARTESIAN_POINT('Ctrl Pts',(-52.4697742856366,70.8653966181718,
60.1509939030528));
#213122=CARTESIAN_POINT('Ctrl Pts',(-52.5133914193336,69.3859793698436,
59.6435101412514));
#213123=CARTESIAN_POINT('Ctrl Pts',(-52.5317610538993,68.7450850115821,
59.4905240162853));
#213124=CARTESIAN_POINT('Ctrl Pts',(-52.5683761301054,67.4677768854099,
59.312874055583));
#213125=CARTESIAN_POINT('Ctrl Pts',(-52.5863652927878,66.834855705855,59.2839032554923));
#213126=CARTESIAN_POINT('Ctrl Pts',(-52.621881454637,65.5640769392124,59.3433129011005));
#213127=CARTESIAN_POINT('Ctrl Pts',(-52.6396720718213,64.929050677876,59.4329941080809));
#213128=CARTESIAN_POINT('Ctrl Pts',(-52.6726107951199,63.7972573546196,
59.702627298489));
#213129=CARTESIAN_POINT('Ctrl Pts',(-52.6875812703577,63.2980145759789,
59.8627986517121));
#213130=CARTESIAN_POINT('Ctrl Pts',(-52.7167181006459,62.3414922092398,
60.2526675518071));
#213131=CARTESIAN_POINT('Ctrl Pts',(-52.7308100180983,61.8847714051643,
60.4798269051936));
#213132=CARTESIAN_POINT('Ctrl Pts',(-52.7624846259668,60.911250173591,61.0581723455944));
#213133=CARTESIAN_POINT('Ctrl Pts',(-52.7801148938693,60.405791269077,61.4245124404429));
#213134=CARTESIAN_POINT('Ctrl Pts',(-52.8362389070056,58.920195166244,62.72290451597));
#213135=CARTESIAN_POINT('Ctrl Pts',(-52.873120682505,58.0891313782455,63.8034934717983));
#213136=CARTESIAN_POINT('Ctrl Pts',(-52.9499786041311,56.8929508538953,
66.2259399742553));
#213137=CARTESIAN_POINT('Ctrl Pts',(-52.9869012557287,56.5400992482972,
67.5443463850443));
#213138=CARTESIAN_POINT('Ctrl Pts',(-53.0347819082646,56.4318730028817,
69.2240060578812));
#213139=CARTESIAN_POINT('Ctrl Pts',(-53.0442180124622,56.4266191738947,
69.5556842528337));
#213140=CARTESIAN_POINT('Ctrl Pts',(-53.0681022151183,56.454357797048,70.4044855926411));
#213141=CARTESIAN_POINT('Ctrl Pts',(-53.0824246531834,56.5104483288861,
70.9199142260153));
#213142=CARTESIAN_POINT('Ctrl Pts',(-53.1266168860895,56.7992540037837,
72.4706668034623));
#213143=CARTESIAN_POINT('Ctrl Pts',(-53.1569590297803,57.1536527929157,
73.47607560508));
#213144=CARTESIAN_POINT('Ctrl Pts',(-53.1957257818166,57.8120892038211,
74.6997072152807));
#213145=CARTESIAN_POINT('Ctrl Pts',(-53.2049081400309,57.9823192739764,
74.9824597831962));
#213146=CARTESIAN_POINT('Ctrl Pts',(-53.233067126294,58.5413841432443,75.8171068980668));
#213147=CARTESIAN_POINT('Ctrl Pts',(-53.2522686043099,58.9713201288318,
76.3392548366998));
#213148=CARTESIAN_POINT('Ctrl Pts',(-53.3008078933674,60.183185559936,77.5460228505117));
#213149=CARTESIAN_POINT('Ctrl Pts',(-53.3291196223283,61.0234471184008,
78.1612994266001));
#213150=CARTESIAN_POINT('Ctrl Pts',(-53.3759450656259,62.4870612315103,
78.9247423505657));
#213151=CARTESIAN_POINT('Ctrl Pts',(-53.3935081856289,63.0570763679768,
79.1595931372414));
#213152=CARTESIAN_POINT('Ctrl Pts',(-53.4244969909968,64.1155870140249,
79.4879995130162));
#213153=CARTESIAN_POINT('Ctrl Pts',(-53.4381749346214,64.5963962045297,
79.5999278243685));
#213154=CARTESIAN_POINT('Ctrl Pts',(-53.4710148892474,65.7506402816098,
79.7821738248868));
#213155=CARTESIAN_POINT('Ctrl Pts',(-53.490309821711,66.4266669170699,79.8213070598965));
#213156=CARTESIAN_POINT('Ctrl Pts',(-53.527766563879,67.7495178345174,79.7671049500467));
#213157=CARTESIAN_POINT('Ctrl Pts',(-53.545638863395,68.3934461201163,79.6791341956534));
#213158=CARTESIAN_POINT('Ctrl Pts',(-53.5899561994073,69.9313494250157,
79.3180706904847));
#213159=CARTESIAN_POINT('Ctrl Pts',(-53.6166731041434,70.8047365182997,
78.9826552089806));
#213160=CARTESIAN_POINT('Ctrl Pts',(-53.6567756194245,72.0616229129678,
78.291527030328));
#213161=CARTESIAN_POINT('Ctrl Pts',(-53.6707331929619,72.484028000018,78.0169863498192));
#213162=CARTESIAN_POINT('Ctrl Pts',(-53.7038802475189,73.4225833970076,
77.3035970690918));
#213163=CARTESIAN_POINT('Ctrl Pts',(-53.723194591918,73.9188374929165,76.8424486978672));
#213164=CARTESIAN_POINT('Ctrl Pts',(-53.7593927199058,74.766232090873,75.882563003819));
#213165=CARTESIAN_POINT('Ctrl Pts',(-53.7760763651848,75.1254906812906,
75.3947775192488));
#213166=CARTESIAN_POINT('Ctrl Pts',(-53.8078513762937,75.7146324498198,
74.4260243596755));
#213167=CARTESIAN_POINT('Ctrl Pts',(-53.8228144662272,75.9537821606758,
73.9539063542217));
#213168=CARTESIAN_POINT('Ctrl Pts',(-53.8378263134509,76.1552807455537,
73.466201023724));
#213169=CARTESIAN_POINT('Ctrl Pts',(-53.4317936414903,76.155280739965,73.4662010372508));
#213170=CARTESIAN_POINT('Ctrl Pts',(-53.4314659962319,76.1508777158183,
73.476858076551));
#213171=CARTESIAN_POINT('Ctrl Pts',(-53.4311383819964,76.1464565428961,
73.4875080872006));
#213172=CARTESIAN_POINT('Ctrl Pts',(-53.4128952715418,75.8992278722724,
74.0802219161308));
#213173=CARTESIAN_POINT('Ctrl Pts',(-53.3954072233106,75.6032360752142,
74.6386413343921));
#213174=CARTESIAN_POINT('Ctrl Pts',(-53.3594844790862,74.8992699569684,
75.7139926929329));
#213175=CARTESIAN_POINT('Ctrl Pts',(-53.3409746459319,74.4890956478663,
76.2260685416729));
#213176=CARTESIAN_POINT('Ctrl Pts',(-53.2839183526019,73.0912392500936,
77.6645611382443));
#213177=CARTESIAN_POINT('Ctrl Pts',(-53.2470045196131,71.9671807972707,
78.4379034421667));
#213178=CARTESIAN_POINT('Ctrl Pts',(-53.1760057255058,69.6738585008067,
79.4224570090448));
#213179=CARTESIAN_POINT('Ctrl Pts',(-53.1446794675824,68.5539268955872,
79.6946439382857));
#213180=CARTESIAN_POINT('Ctrl Pts',(-53.0968240154157,66.8695047064349,
79.814968195707));
#213181=CARTESIAN_POINT('Ctrl Pts',(-53.0812542410977,66.3244701339641,
79.8104536841581));
#213182=CARTESIAN_POINT('Ctrl Pts',(-53.0514361458559,65.2676801161755,
79.7173440425143));
#213183=CARTESIAN_POINT('Ctrl Pts',(-53.0371402952996,64.7571477762161,
79.6331432604136));
#213184=CARTESIAN_POINT('Ctrl Pts',(-53.0022205705923,63.5464698036927,
79.3381092421604));
#213185=CARTESIAN_POINT('Ctrl Pts',(-52.9814285047767,62.8582526126167,
79.0902559045379));
#213186=CARTESIAN_POINT('Ctrl Pts',(-52.951284040001,61.9011854719671,78.6252011403551));
#213187=CARTESIAN_POINT('Ctrl Pts',(-52.9419242939361,61.607512904031,78.4642770173353));
#213188=CARTESIAN_POINT('Ctrl Pts',(-52.9143597158301,60.7651940655475,
77.9475554461948));
#213189=CARTESIAN_POINT('Ctrl Pts',(-52.8961354568477,60.2421097217891,
77.55334853467));
#213190=CARTESIAN_POINT('Ctrl Pts',(-52.8641346518973,59.410075329003,76.791526311064));
#213191=CARTESIAN_POINT('Ctrl Pts',(-52.8505713097694,59.0827081741547,
76.4470879423885));
#213192=CARTESIAN_POINT('Ctrl Pts',(-52.8238139978596,58.4778270199905,
75.7150387416729));
#213193=CARTESIAN_POINT('Ctrl Pts',(-52.8106602608988,58.2010832150992,
75.3282771917183));
#213194=CARTESIAN_POINT('Ctrl Pts',(-52.7880664001766,57.7775813447986,
74.6399941606678));
#213195=CARTESIAN_POINT('Ctrl Pts',(-52.7787101072543,57.6169406943703,
74.3479271681421));
#213196=CARTESIAN_POINT('Ctrl Pts',(-52.7550857351583,57.2505846291851,
73.5974083152818));
#213197=CARTESIAN_POINT('Ctrl Pts',(-52.7407446071513,57.0638046904065,
73.1306895624294));
#213198=CARTESIAN_POINT('Ctrl Pts',(-52.7084130093088,56.7181436842887,
72.041273235225));
#213199=CARTESIAN_POINT('Ctrl Pts',(-52.6907451184286,56.5820362161555,
71.4135437557124));
#213200=CARTESIAN_POINT('Ctrl Pts',(-52.6462484222969,56.3924438733585,
69.8385019542338));
#213201=CARTESIAN_POINT('Ctrl Pts',(-52.6191261781079,56.409875066736,68.8886457120217));
#213202=CARTESIAN_POINT('Ctrl Pts',(-52.5776949972587,56.6409096623561,
67.4244244104058));
#213203=CARTESIAN_POINT('Ctrl Pts',(-52.5628004968698,56.7661086461411,
66.901545438304));
#213204=CARTESIAN_POINT('Ctrl Pts',(-52.5286159491664,57.1404901287403,
65.7468748791583));
#213205=CARTESIAN_POINT('Ctrl Pts',(-52.5092323715014,57.4125885703912,
65.1251422765157));
#213206=CARTESIAN_POINT('Ctrl Pts',(-52.4763357891551,57.9838006896954,
64.1075959623724));
#213207=CARTESIAN_POINT('Ctrl Pts',(-52.462775196895,58.253933658796,63.6981383530843));
#213208=CARTESIAN_POINT('Ctrl Pts',(-52.4309630398224,58.9467892134872,
62.7958510850989));
#213209=CARTESIAN_POINT('Ctrl Pts',(-52.4126301421501,59.3890721713321,
62.3206812564263));
#213210=CARTESIAN_POINT('Ctrl Pts',(-52.3846926948985,60.1232844105761,
61.6682144426206));
#213211=CARTESIAN_POINT('Ctrl Pts',(-52.3752083042255,60.3840820643844,
61.4583639214501));
#213212=CARTESIAN_POINT('Ctrl Pts',(-52.3457945900397,61.2332793232641,
60.8409940997788));
#213213=CARTESIAN_POINT('Ctrl Pts',(-52.3260119706135,61.8543300575416,
60.4820724925773));
#213214=CARTESIAN_POINT('Ctrl Pts',(-52.2915787960311,62.9660902412387,
59.9863372313077));
#213215=CARTESIAN_POINT('Ctrl Pts',(-52.27724080382,63.4388995537073,59.8158774645287));
#213216=CARTESIAN_POINT('Ctrl Pts',(-52.2448876252375,64.5403538432876,
59.507953324019));
#213217=CARTESIAN_POINT('Ctrl Pts',(-52.2271965762748,65.1732813415432,
59.3935941786054));
#213218=CARTESIAN_POINT('Ctrl Pts',(-52.182722997773,66.7531234704477,59.2591326564387));
#213219=CARTESIAN_POINT('Ctrl Pts',(-52.1556494594568,67.7000717842061,
59.3093587972366));
#213220=CARTESIAN_POINT('Ctrl Pts',(-52.1143881196541,69.1494645880636,
59.5894407375375));
#213221=CARTESIAN_POINT('Ctrl Pts',(-52.0996164392368,69.6635432057282,
59.7310318151772));
#213222=CARTESIAN_POINT('Ctrl Pts',(-52.0655683577469,70.8008720402759,
60.1418613680364));
#213223=CARTESIAN_POINT('Ctrl Pts',(-52.0461939530619,71.4131075471757,
60.4342951777518));
#213224=CARTESIAN_POINT('Ctrl Pts',(-52.0129298404671,72.4219705123723,
61.0453279018358));
#213225=CARTESIAN_POINT('Ctrl Pts',(-51.999021691533,72.8321732375763,61.3369996558632));
#213226=CARTESIAN_POINT('Ctrl Pts',(-51.9673054183399,73.7055664631982,
62.0602315082084));
#213227=CARTESIAN_POINT('Ctrl Pts',(-51.9494382004535,74.1535709799477,
62.5069382812588));
#213228=CARTESIAN_POINT('Ctrl Pts',(-51.8930940034553,75.4213424280378,
64.0289120405076));
#213229=CARTESIAN_POINT('Ctrl Pts',(-51.8562261475554,76.0718418595893,
65.2262598337549));
#213230=CARTESIAN_POINT('Ctrl Pts',(-51.7793862998523,76.8721659737517,
67.8060300810223));
#213231=CARTESIAN_POINT('Ctrl Pts',(-51.7424659076742,77.0133878904221,
69.1634389134832));
#213232=CARTESIAN_POINT('Ctrl Pts',(-51.6749180973905,76.791730248281,71.5275396952808));
#213233=CARTESIAN_POINT('Ctrl Pts',(-51.6468253635685,76.5444946475245,
72.5241512610753));
#213234=CARTESIAN_POINT('Ctrl Pts',(-51.6180871401245,76.1552807409204,
73.4662010349383));
#213235=CARTESIAN_POINT('Origin',(-45.8894114130409,66.6819786653733,69.5522455184007));
#213236=CARTESIAN_POINT('',(-55.6519493945588,76.1552807409204,73.4662010349383));
#213237=CARTESIAN_POINT('',(-55.2458788384028,76.1552807409204,73.4662010349383));
#213238=CARTESIAN_POINT('',(-45.8894114130409,76.1552807409204,73.4662010349383));
#213239=CARTESIAN_POINT('',(-54.9945936623312,57.5592308793253,74.2253572046497));
#213240=CARTESIAN_POINT('Ctrl Pts',(-54.9945936623312,57.5592308793253,
74.2253572046497));
#213241=CARTESIAN_POINT('Ctrl Pts',(-55.0084372590718,57.7855821470804,
74.6672352647992));
#213242=CARTESIAN_POINT('Ctrl Pts',(-55.0223123077768,58.0437377263266,
75.0920812588877));
#213243=CARTESIAN_POINT('Ctrl Pts',(-55.0500493198654,58.6121913701251,
75.8906232303414));
#213244=CARTESIAN_POINT('Ctrl Pts',(-55.0638656775378,58.920268216079,76.2643500438473));
#213245=CARTESIAN_POINT('Ctrl Pts',(-55.1051653283116,59.9255405894118,
77.3216780637746));
#213246=CARTESIAN_POINT('Ctrl Pts',(-55.1318714947715,60.6949359305111,
77.9289311633348));
#213247=CARTESIAN_POINT('Ctrl Pts',(-55.1730512387199,61.9505392495489,
78.6573496489838));
#213248=CARTESIAN_POINT('Ctrl Pts',(-55.1866646088001,62.3787647802416,
78.8673832391282));
#213249=CARTESIAN_POINT('Ctrl Pts',(-55.2150290111367,63.311710122981,79.2468586413377));
#213250=CARTESIAN_POINT('Ctrl Pts',(-55.2297040018442,63.8181737520004,
79.4083533588378));
#213251=CARTESIAN_POINT('Ctrl Pts',(-55.2635851799419,64.9956836599146,
79.6853476283084));
#213252=CARTESIAN_POINT('Ctrl Pts',(-55.2828822587737,65.6703126693746,
79.7747630098718));
#213253=CARTESIAN_POINT('Ctrl Pts',(-55.3200521570506,66.9784724279672,
79.8173075347476));
#213254=CARTESIAN_POINT('Ctrl Pts',(-55.337507810066,67.6086897567368,79.7796897600188));
#213255=CARTESIAN_POINT('Ctrl Pts',(-55.3773061078025,69.0158950847412,
79.5644914169816));
#213256=CARTESIAN_POINT('Ctrl Pts',(-55.3998750351786,69.7837514486007,
79.353837768276));
#213257=CARTESIAN_POINT('Ctrl Pts',(-55.4392788189713,71.0726734457158,
78.8334141112913));
#213258=CARTESIAN_POINT('Ctrl Pts',(-55.4557763960126,71.6052193096335,
78.5622396134129));
#213259=CARTESIAN_POINT('Ctrl Pts',(-55.5011128136525,72.9800616350833,
77.7036912942383));
#213260=CARTESIAN_POINT('Ctrl Pts',(-55.5304852313319,73.7627295822315,
77.0338820012117));
#213261=CARTESIAN_POINT('Ctrl Pts',(-55.577991334307,74.8745375971509,75.7489967300131));
#213262=CARTESIAN_POINT('Ctrl Pts',(-55.5966995204025,75.2645755879978,
75.1964263112878));
#213263=CARTESIAN_POINT('Ctrl Pts',(-55.6251264558726,75.7602715179669,
74.3225663411172));
#213264=CARTESIAN_POINT('Ctrl Pts',(-55.6345161010389,75.9091114434636,
74.027888642471));
#213265=CARTESIAN_POINT('Ctrl Pts',(-55.646586044891,76.0819598875626,73.6402500653772));
#213266=CARTESIAN_POINT('Ctrl Pts',(-55.6492703896237,76.1192295478691,
73.5534590123262));
#213267=CARTESIAN_POINT('Ctrl Pts',(-55.6519493945588,76.1552807409204,
73.4662010349383));
#213268=CARTESIAN_POINT('Ctrl Pts',(-53.8378263134509,76.1552807455537,
73.466201023724));
#213269=CARTESIAN_POINT('Ctrl Pts',(-53.8522474144839,76.3488499584049,
72.9976878727012));
#213270=CARTESIAN_POINT('Ctrl Pts',(-53.8665858984656,76.5076744897429,
72.5147867212634));
#213271=CARTESIAN_POINT('Ctrl Pts',(-53.8899527568025,76.7093946581641,
71.7020543778137));
#213272=CARTESIAN_POINT('Ctrl Pts',(-53.8991093787747,76.7732299909849,
71.3790996265538));
#213273=CARTESIAN_POINT('Ctrl Pts',(-53.9378312622193,76.9756655140685,
70.0119776316187));
#213274=CARTESIAN_POINT('Ctrl Pts',(-53.9679861255333,76.9684723074621,
68.952747027349));
#213275=CARTESIAN_POINT('Ctrl Pts',(-54.0065619492763,76.7473926300935,
67.5879195820092));
#213276=CARTESIAN_POINT('Ctrl Pts',(-54.0157365034357,76.6790277257479,
67.2652946459151));
#213277=CARTESIAN_POINT('Ctrl Pts',(-54.0539158267811,76.3327208626224,
65.9477968743099));
#213278=CARTESIAN_POINT('Ctrl Pts',(-54.083497459971,75.9207775580982,64.9944523687732));
#213279=CARTESIAN_POINT('Ctrl Pts',(-54.1214905131542,75.1990667965299,
63.839992244076));
#213280=CARTESIAN_POINT('Ctrl Pts',(-54.1306414926061,75.0114421441789,
63.5697154926513));
#213281=CARTESIAN_POINT('Ctrl Pts',(-54.1695411982524,74.1656992385936,
62.468507946713));
#213282=CARTESIAN_POINT('Ctrl Pts',(-54.1998831053543,73.3938081254763,
61.7332453362441));
#213283=CARTESIAN_POINT('Ctrl Pts',(-54.2386496142671,72.2519730235472,
60.9414114358815));
#213284=CARTESIAN_POINT('Ctrl Pts',(-54.247831961414,71.9720065996045,60.7666377017056));
#213285=CARTESIAN_POINT('Ctrl Pts',(-54.2759909336803,71.0951687493672,
60.2763886497195));
#213286=CARTESIAN_POINT('Ctrl Pts',(-54.2951924069054,70.4751608137961,
60.0060672344893));
#213287=CARTESIAN_POINT('Ctrl Pts',(-54.3437331660042,68.8477003097819,
59.4802772900666));
#213288=CARTESIAN_POINT('Ctrl Pts',(-54.3720462930882,67.8197122229352,
59.3130826041624));
#213289=CARTESIAN_POINT('Ctrl Pts',(-54.4188763753811,66.168872058537,59.2966184682286));
#213290=CARTESIAN_POINT('Ctrl Pts',(-54.4364425234928,65.5542343895586,
59.3459056636689));
#213291=CARTESIAN_POINT('Ctrl Pts',(-54.4674489004025,64.4613015187775,
59.5335287842442));
#213292=CARTESIAN_POINT('Ctrl Pts',(-54.4811414040499,63.9815337580726,
59.6520591737922));
#213293=CARTESIAN_POINT('Ctrl Pts',(-54.5139972835219,62.8697597235691,
60.0135963485974));
#213294=CARTESIAN_POINT('Ctrl Pts',(-54.5332931809973,62.2495741251418,
60.2854976560029));
#213295=CARTESIAN_POINT('Ctrl Pts',(-54.5706830646895,61.0973819238806,
60.9329499567827));
#213296=CARTESIAN_POINT('Ctrl Pts',(-54.5884923418836,60.5652905220523,
61.3020270385938));
#213297=CARTESIAN_POINT('Ctrl Pts',(-54.6328612068691,59.3565286821881,
62.3220677315632));
#213298=CARTESIAN_POINT('Ctrl Pts',(-54.6596992020544,58.7275211877893,
63.0204538552515));
#213299=CARTESIAN_POINT('Ctrl Pts',(-54.7001769534581,57.9141518712627,
64.2183634506065));
#213300=CARTESIAN_POINT('Ctrl Pts',(-54.7143931148832,57.6584966712826,
64.6632929281237));
#213301=CARTESIAN_POINT('Ctrl Pts',(-54.7478249708634,57.1452019521253,
65.735247376952));
#213302=CARTESIAN_POINT('Ctrl Pts',(-54.7671576445172,56.9142648049202,
66.3724127761249));
#213303=CARTESIAN_POINT('Ctrl Pts',(-54.8023434816488,56.6075074454265,
67.5794990132264));
#213304=CARTESIAN_POINT('Ctrl Pts',(-54.8180706895508,56.5134928585929,
68.14206878208));
#213305=CARTESIAN_POINT('Ctrl Pts',(-54.8604034816512,56.3892128592203,
69.6485737620773));
#213306=CARTESIAN_POINT('Ctrl Pts',(-54.8874311493389,56.4415970092537,
70.5938250436981));
#213307=CARTESIAN_POINT('Ctrl Pts',(-54.9270660553076,56.7131276846823,
71.9829717459558));
#213308=CARTESIAN_POINT('Ctrl Pts',(-54.9401815920977,56.8359557255954,
72.4405415227217));
#213309=CARTESIAN_POINT('Ctrl Pts',(-54.9670530131731,57.1478277224444,
73.3466886280764));
#213310=CARTESIAN_POINT('Ctrl Pts',(-54.9807860052725,57.3380653584498,
73.7936026652801));
#213311=CARTESIAN_POINT('Ctrl Pts',(-54.9945874883696,57.5592309567654,
74.2253573558264));
#213312=CARTESIAN_POINT('Ctrl Pts',(-55.2458788384028,76.1552807409204,
73.4662010349383));
#213313=CARTESIAN_POINT('Ctrl Pts',(-55.2243124915029,75.8599701795553,
74.180968012256));
#213314=CARTESIAN_POINT('Ctrl Pts',(-55.2025647280681,75.4840079051681,
74.8617220383151));
#213315=CARTESIAN_POINT('Ctrl Pts',(-55.1469981393143,74.3515537139317,
76.4532424940862));
#213316=CARTESIAN_POINT('Ctrl Pts',(-55.1147951169291,73.5096645610282,
77.2871576634901));
#213317=CARTESIAN_POINT('Ctrl Pts',(-55.0664437014297,72.1104937279418,
78.2628168623936));
#213318=CARTESIAN_POINT('Ctrl Pts',(-55.051298710415,71.6533815832847,78.5315542634988));
#213319=CARTESIAN_POINT('Ctrl Pts',(-55.0173903034329,70.5696060050378,
79.0604785237848));
#213320=CARTESIAN_POINT('Ctrl Pts',(-54.9987323542363,69.9337692211884,
79.2962698052724));
#213321=CARTESIAN_POINT('Ctrl Pts',(-54.9581124061482,68.5394305632959,
79.6615195359488));
#213322=CARTESIAN_POINT('Ctrl Pts',(-54.9361746118771,67.7801351488511,
79.7719133506492));
#213323=CARTESIAN_POINT('Ctrl Pts',(-54.8958423061881,66.3409028041523,
79.818789892051));
#213324=CARTESIAN_POINT('Ctrl Pts',(-54.877165535705,65.6656342445293,79.7740512914097));
#213325=CARTESIAN_POINT('Ctrl Pts',(-54.8389851930708,64.3325458542862,
79.5522483951396));
#213326=CARTESIAN_POINT('Ctrl Pts',(-54.8196031415924,63.6780289190024,
79.3754927901739));
#213327=CARTESIAN_POINT('Ctrl Pts',(-54.7817047194038,62.4142616155419,
78.8959714791988));
#213328=CARTESIAN_POINT('Ctrl Pts',(-54.7630394630545,61.8080437372174,
78.594556454494));
#213329=CARTESIAN_POINT('Ctrl Pts',(-54.7240902845646,60.6392221738559,
77.8614960599658));
#213330=CARTESIAN_POINT('Ctrl Pts',(-54.7039000764441,60.0827100559538,
77.4267749513204));
#213331=CARTESIAN_POINT('Ctrl Pts',(-54.6702884916899,59.2185387844903,
76.5952922282852));
#213332=CARTESIAN_POINT('Ctrl Pts',(-54.6565774184773,58.8872209795158,
76.2267639897297));
#213333=CARTESIAN_POINT('Ctrl Pts',(-54.625092293712,58.199101303284,75.3399177304646));
#213334=CARTESIAN_POINT('Ctrl Pts',(-54.6072442516165,57.8607302600861,
74.8098040166607));
#213335=CARTESIAN_POINT('Ctrl Pts',(-54.5715079278915,57.2838667216351,
73.6917566269042));
#213336=CARTESIAN_POINT('Ctrl Pts',(-54.554027115688,57.0470780046594,73.1059411198935));
#213337=CARTESIAN_POINT('Ctrl Pts',(-54.5181163178736,56.6773304307878,
71.875511919092));
#213338=CARTESIAN_POINT('Ctrl Pts',(-54.4996139683888,56.549466915596,71.2323477821425));
#213339=CARTESIAN_POINT('Ctrl Pts',(-54.4495571938241,56.3727762684054,
69.4814802870216));
#213340=CARTESIAN_POINT('Ctrl Pts',(-54.4193029272258,56.440451973092,68.3708037207158));
#213341=CARTESIAN_POINT('Ctrl Pts',(-54.372011124297,56.808511139124,66.7424089895317));
#213342=CARTESIAN_POINT('Ctrl Pts',(-54.355871334505,56.9780284385155,66.2035297033478));
#213343=CARTESIAN_POINT('Ctrl Pts',(-54.3256092730652,57.3848256021668,
65.2061158091956));
#213344=CARTESIAN_POINT('Ctrl Pts',(-54.3114066674863,57.6140630165044,
64.7461235116986));
#213345=CARTESIAN_POINT('Ctrl Pts',(-54.2704474398064,58.3621786160401,
63.4906836068886));
#213346=CARTESIAN_POINT('Ctrl Pts',(-54.2432433980074,58.9582583690056,
62.7474123375254));
#213347=CARTESIAN_POINT('Ctrl Pts',(-54.1978537859097,60.1386360227913,
61.6337711224434));
#213348=CARTESIAN_POINT('Ctrl Pts',(-54.1791599386208,60.6738137336899,
61.2204075412817));
#213349=CARTESIAN_POINT('Ctrl Pts',(-54.1507294596653,61.5259552401333,
60.6873033667533));
#213350=CARTESIAN_POINT('Ctrl Pts',(-54.1413243075175,61.8145190729074,
60.5256396912466));
#213351=CARTESIAN_POINT('Ctrl Pts',(-54.106385453136,62.914022822591,59.9777370919764));
#213352=CARTESIAN_POINT('Ctrl Pts',(-54.0816685970493,63.766804995361,59.6845977050456));
#213353=CARTESIAN_POINT('Ctrl Pts',(-54.0333038138775,65.4517072700732,
59.3432611125962));
#213354=CARTESIAN_POINT('Ctrl Pts',(-54.0097423741449,66.2732798037355,
59.2775239016227));
#213355=CARTESIAN_POINT('Ctrl Pts',(-53.9731697700608,67.5786574994477,
59.3300208643908));
#213356=CARTESIAN_POINT('Ctrl Pts',(-53.9597186847645,68.0614602011573,
59.3839151786058));
#213357=CARTESIAN_POINT('Ctrl Pts',(-53.9265874021746,69.2224689976322,
59.5977533672385));
#213358=CARTESIAN_POINT('Ctrl Pts',(-53.9067471765375,69.8917217836102,
59.7929660144528));
#213359=CARTESIAN_POINT('Ctrl Pts',(-53.8775898947858,70.8458210187467,
60.1801224750558));
#213360=CARTESIAN_POINT('Ctrl Pts',(-53.8682463981352,71.1492749555572,
60.3209109392519));
#213361=CARTESIAN_POINT('Ctrl Pts',(-53.8411009308922,72.0110396946509,
60.7731898745245));
#213362=CARTESIAN_POINT('Ctrl Pts',(-53.8232780321355,72.5477690435606,
61.1223460234573));
#213363=CARTESIAN_POINT('Ctrl Pts',(-53.7910712414706,73.4377327987901,
61.8276766968787));
#213364=CARTESIAN_POINT('Ctrl Pts',(-53.7768719520978,73.8040404404524,
62.1640512086842));
#213365=CARTESIAN_POINT('Ctrl Pts',(-53.7438427360603,74.6085507419804,
63.0184749854055));
#213366=CARTESIAN_POINT('Ctrl Pts',(-53.7251832826996,75.0226277241806,
63.5560561509127));
#213367=CARTESIAN_POINT('Ctrl Pts',(-53.6910623951486,75.6633881270673,
64.5841027553956));
#213368=CARTESIAN_POINT('Ctrl Pts',(-53.6758314564432,75.9101849166998,
65.0590995070581));
#213369=CARTESIAN_POINT('Ctrl Pts',(-53.6338431560758,76.4875329605039,
66.4208152873592));
#213370=CARTESIAN_POINT('Ctrl Pts',(-53.6079792362328,76.7342739860762,
67.3372712705771));
#213371=CARTESIAN_POINT('Ctrl Pts',(-53.5631322447755,76.9319766110032,
68.9108520115754));
#213372=CARTESIAN_POINT('Ctrl Pts',(-53.5447588668118,76.9520249426517,
69.5533128542441));
#213373=CARTESIAN_POINT('Ctrl Pts',(-53.5126853153771,76.8805045666242,
70.6944122332943));
#213374=CARTESIAN_POINT('Ctrl Pts',(-53.4987850526581,76.812344483354,71.1924183457376));
#213375=CARTESIAN_POINT('Ctrl Pts',(-53.4672275751477,76.5783393297752,
72.2932815484876));
#213376=CARTESIAN_POINT('Ctrl Pts',(-53.4495081764723,76.3933355363178,
72.8900153894336));
#213377=CARTESIAN_POINT('Ctrl Pts',(-53.4317936414903,76.155280739965,73.4662010372508));
#213378=CARTESIAN_POINT('Origin',(-45.8894114130409,66.6819786653733,69.5522455184007));
#213379=CARTESIAN_POINT('',(-57.4656305641639,76.1552807494535,73.4662010142848));
#213380=CARTESIAN_POINT('',(-57.0597576325586,76.1552807409204,73.4662010349383));
#213381=CARTESIAN_POINT('',(-45.8894114130409,76.1552807409204,73.4662010349383));
#213382=CARTESIAN_POINT('Ctrl Pts',(-55.6519493945588,76.1552807409204,
73.4662010349383));
#213383=CARTESIAN_POINT('Ctrl Pts',(-55.6746958093889,76.4613777478853,
72.7253266435083));
#213384=CARTESIAN_POINT('Ctrl Pts',(-55.6967311479311,76.6796366011113,
71.9507821246546));
#213385=CARTESIAN_POINT('Ctrl Pts',(-55.7421069158573,76.9322895411356,
70.3583648508813));
#213386=CARTESIAN_POINT('Ctrl Pts',(-55.7653466256031,76.9639372508576,
69.5460762671887));
#213387=CARTESIAN_POINT('Ctrl Pts',(-55.806925292861,76.8460434176339,68.0656456112224));
#213388=CARTESIAN_POINT('Ctrl Pts',(-55.82560912636,76.7261109082097,67.3996653582486));
#213389=CARTESIAN_POINT('Ctrl Pts',(-55.8578065452673,76.4146828609178,
66.3037895256571));
#213390=CARTESIAN_POINT('Ctrl Pts',(-55.8710467590946,76.2575969551468,
65.8663903296937));
#213391=CARTESIAN_POINT('Ctrl Pts',(-55.9015061502112,75.8269700354966,
64.8828707740773));
#213392=CARTESIAN_POINT('Ctrl Pts',(-55.9183723033464,75.5332283220548,
64.3475064800913));
#213393=CARTESIAN_POINT('Ctrl Pts',(-55.9642808919294,74.6185712654834,
62.984258552835));
#213394=CARTESIAN_POINT('Ctrl Pts',(-55.9938741312891,73.9172839314932,
62.2188756965993));
#213395=CARTESIAN_POINT('Ctrl Pts',(-56.0415967105518,72.5881977023298,
61.1478221903385));
#213396=CARTESIAN_POINT('Ctrl Pts',(-56.0603060724811,72.0223100023036,
60.7773600349768));
#213397=CARTESIAN_POINT('Ctrl Pts',(-56.088732412173,71.1316852544978,60.3125792487002));
#213398=CARTESIAN_POINT('Ctrl Pts',(-56.0981205329324,70.8320354863306,
60.1741674261336));
#213399=CARTESIAN_POINT('Ctrl Pts',(-56.1376559883003,69.543270156717,59.6527561343609));
#213400=CARTESIAN_POINT('Ctrl Pts',(-56.1666755817687,68.5045214558714,
59.4099960162732));
#213401=CARTESIAN_POINT('Ctrl Pts',(-56.213397765002,66.8588571896004,59.2868087178602));
#213402=CARTESIAN_POINT('Ctrl Pts',(-56.2302860349057,66.2678997718162,
59.2936382150129));
#213403=CARTESIAN_POINT('Ctrl Pts',(-56.2658276588423,65.0081500307784,
59.4172744788482));
#213404=CARTESIAN_POINT('Ctrl Pts',(-56.2844862109658,64.3436587722586,
59.5496654525987));
#213405=CARTESIAN_POINT('Ctrl Pts',(-56.3178429932004,63.2122255775121,
59.8940807117341));
#213406=CARTESIAN_POINT('Ctrl Pts',(-56.3322909912631,62.7390163823665,
60.0774169095307));
#213407=CARTESIAN_POINT('Ctrl Pts',(-56.3642103686336,61.7233069579406,
60.5602593341932));
#213408=CARTESIAN_POINT('Ctrl Pts',(-56.3813164175117,61.1904262552062,
60.8754319085674));
#213409=CARTESIAN_POINT('Ctrl Pts',(-56.4168192794982,60.1603499538491,
61.6177787778474));
#213410=CARTESIAN_POINT('Ctrl Pts',(-56.4352685726779,59.6690857904514,
62.0484650065876));
#213411=CARTESIAN_POINT('Ctrl Pts',(-56.4847043251642,58.4771130954218,
63.3134442904562));
#213412=CARTESIAN_POINT('Ctrl Pts',(-56.5144312187865,57.8625515955255,
64.2174375450141));
#213413=CARTESIAN_POINT('Ctrl Pts',(-56.5614677909185,57.1575056607049,
65.7211836639762));
#213414=CARTESIAN_POINT('Ctrl Pts',(-56.5779136226738,56.9577674094946,
66.2609931461306));
#213415=CARTESIAN_POINT('Ctrl Pts',(-56.6084175060458,56.6677089626359,
67.307583325813));
#213416=CARTESIAN_POINT('Ctrl Pts',(-56.6225730702787,56.5681892132335,
67.810013278484));
#213417=CARTESIAN_POINT('Ctrl Pts',(-56.6547733103649,56.4298267965272,
68.9504896347172));
#213418=CARTESIAN_POINT('Ctrl Pts',(-56.6728850392413,56.4122481955756,
69.5889895371447));
#213419=CARTESIAN_POINT('Ctrl Pts',(-56.7089331308968,56.4955145498018,
70.8549562551205));
#213420=CARTESIAN_POINT('Ctrl Pts',(-56.7264522871935,56.5950685835595,
71.4797711172831));
#213421=CARTESIAN_POINT('Ctrl Pts',(-56.7624239808063,56.9139695724793,
72.7269537020968));
#213422=CARTESIAN_POINT('Ctrl Pts',(-56.7809628328593,57.1370950324909,
73.3453913173354));
#213423=CARTESIAN_POINT('Ctrl Pts',(-56.8380682761259,57.9960908523302,
75.1597803461317));
#213424=CARTESIAN_POINT('Ctrl Pts',(-56.8749886634776,58.8103360011574,
76.2549562375439));
#213425=CARTESIAN_POINT('Ctrl Pts',(-56.9393984543463,60.4909328726403,
77.7721164903898));
#213426=CARTESIAN_POINT('Ctrl Pts',(-56.9645961674213,61.2469785226243,
78.2904440043893));
#213427=CARTESIAN_POINT('Ctrl Pts',(-57.0145366542064,62.8336518914627,
79.0916868218928));
#213428=CARTESIAN_POINT('Ctrl Pts',(-57.0393538750368,63.6519495740406,
79.3822755591976));
#213429=CARTESIAN_POINT('Ctrl Pts',(-57.082448978218,65.1565013419189,79.7105473689902));
#213430=CARTESIAN_POINT('Ctrl Pts',(-57.1011421541805,65.8286271481142,
79.788942745876));
#213431=CARTESIAN_POINT('Ctrl Pts',(-57.1385964345675,67.1532251391229,
79.8120024934277));
#213432=CARTESIAN_POINT('Ctrl Pts',(-57.1572121997389,67.8024927481622,
79.7615130239616));
#213433=CARTESIAN_POINT('Ctrl Pts',(-57.1894880445944,68.9360918926912,
79.5638593128264));
#213434=CARTESIAN_POINT('Ctrl Pts',(-57.2033605279661,69.4226124385091,
79.4417534316169));
#213435=CARTESIAN_POINT('Ctrl Pts',(-57.2374376203684,70.5764964570531,
79.0604255012093));
#213436=CARTESIAN_POINT('Ctrl Pts',(-57.2578086786501,71.2294539039164,
78.7659963548634));
#213437=CARTESIAN_POINT('Ctrl Pts',(-57.294600289576,72.3514686598769,78.1115201994638));
#213438=CARTESIAN_POINT('Ctrl Pts',(-57.3107630531777,72.8303406105761,
77.7742857865217));
#213439=CARTESIAN_POINT('Ctrl Pts',(-57.355556261234,74.0559448204746,76.7439384096182));
#213440=CARTESIAN_POINT('Ctrl Pts',(-57.3847050489666,74.7324172633522,
75.9776842499415));
#213441=CARTESIAN_POINT('Ctrl Pts',(-57.4306208500471,75.6251682462822,
74.5993554303877));
#213442=CARTESIAN_POINT('Ctrl Pts',(-57.4479646045207,75.9164493598438,
74.0442663252789));
#213443=CARTESIAN_POINT('Ctrl Pts',(-57.4656305635332,76.1552807494603,
73.4662010142683));
#213444=CARTESIAN_POINT('',(-56.4026916770479,57.5592259231377,74.2253475292746));
#213445=CARTESIAN_POINT('Ctrl Pts',(-56.4026916770479,57.5592259231377,
74.2253475292746));
#213446=CARTESIAN_POINT('Ctrl Pts',(-56.389088155609,57.3368004938124,73.7911322712726));
#213447=CARTESIAN_POINT('Ctrl Pts',(-56.3754551144229,57.1456610282986,
73.3415934269327));
#213448=CARTESIAN_POINT('Ctrl Pts',(-56.3481953671734,56.8327947824228,
72.4301667046301));
#213449=CARTESIAN_POINT('Ctrl Pts',(-56.3346117192863,56.7098440227171,
71.9699678589818));
#213450=CARTESIAN_POINT('Ctrl Pts',(-56.2942042303519,56.4384143469144,
70.5697661844793));
#213451=CARTESIAN_POINT('Ctrl Pts',(-56.2681802563034,56.3881991142826,
69.6159961022789));
#213452=CARTESIAN_POINT('Ctrl Pts',(-56.2257203683172,56.5173224467139,
68.1230596009114));
#213453=CARTESIAN_POINT('Ctrl Pts',(-56.2100416967376,56.6082508580759,
67.5817580222648));
#213454=CARTESIAN_POINT('Ctrl Pts',(-56.1756348109084,56.907086450217,66.3945036641586));
#213455=CARTESIAN_POINT('Ctrl Pts',(-56.1569777938711,57.1366591444924,
65.7566249072161));
#213456=CARTESIAN_POINT('Ctrl Pts',(-56.1233002220583,57.6502426864429,
64.6779224322218));
#213457=CARTESIAN_POINT('Ctrl Pts',(-56.1085221247771,57.9083002920568,
64.2274129090497));
#213458=CARTESIAN_POINT('Ctrl Pts',(-56.0671772523844,58.7259404725428,
63.0220068134701));
#213459=CARTESIAN_POINT('Ctrl Pts',(-56.0414886867618,59.3566494640493,
62.3216082655819));
#213460=CARTESIAN_POINT('Ctrl Pts',(-55.9967337203048,60.5666241009019,
61.3011483520127));
#213461=CARTESIAN_POINT('Ctrl Pts',(-55.9782634496156,61.097590930154,60.9329191081807));
#213462=CARTESIAN_POINT('Ctrl Pts',(-55.9412289858562,62.2484962784064,
60.2860127608426));
#213463=CARTESIAN_POINT('Ctrl Pts',(-55.9225668534959,62.8686539055051,
60.0140383592924));
#213464=CARTESIAN_POINT('Ctrl Pts',(-55.8833053485378,64.1915962962261,
59.5836618985219));
#213465=CARTESIAN_POINT('Ctrl Pts',(-55.8627876392765,64.8934658696332,
59.4341481077287));
#213466=CARTESIAN_POINT('Ctrl Pts',(-55.8238098344682,66.2766548428917,
59.2880291180159));
#213467=CARTESIAN_POINT('Ctrl Pts',(-55.8051399099569,66.9535088606638,
59.2836184812238));
#213468=CARTESIAN_POINT('Ctrl Pts',(-55.7665497361985,68.3141750195008,
59.40945217659));
#213469=CARTESIAN_POINT('Ctrl Pts',(-55.7467365157939,68.9942841791439,
59.5425714904494));
#213470=CARTESIAN_POINT('Ctrl Pts',(-55.7084286876881,70.3020656894231,
59.9390509222948));
#213471=CARTESIAN_POINT('Ctrl Pts',(-55.6897617569757,70.9273840402981,
60.1983651290787));
#213472=CARTESIAN_POINT('Ctrl Pts',(-55.6509522504458,72.1389852901321,
60.8475054328729));
#213473=CARTESIAN_POINT('Ctrl Pts',(-55.6309086384268,72.719923744177,61.239926358534));
#213474=CARTESIAN_POINT('Ctrl Pts',(-55.5974228927443,73.6364737528791,
62.0061903735278));
#213475=CARTESIAN_POINT('Ctrl Pts',(-55.5836980689193,73.9930298871489,
62.3511009808872));
#213476=CARTESIAN_POINT('Ctrl Pts',(-55.5521817069278,74.7419573403004,
63.1887643642372));
#213477=CARTESIAN_POINT('Ctrl Pts',(-55.5343160631464,75.1167285258278,
63.6945898270689));
#213478=CARTESIAN_POINT('Ctrl Pts',(-55.4985615269735,75.7701296843823,
64.7704486766459));
#213479=CARTESIAN_POINT('Ctrl Pts',(-55.4810803503927,76.0470085755227,
65.3384244954077));
#213480=CARTESIAN_POINT('Ctrl Pts',(-55.4451689454345,76.5012685317673,
66.5402490532224));
#213481=CARTESIAN_POINT('Ctrl Pts',(-55.4266662118752,76.6734640365655,
67.1730058975518));
#213482=CARTESIAN_POINT('Ctrl Pts',(-55.3696226465601,77.0127962394095,
69.149469887891));
#213483=CARTESIAN_POINT('Ctrl Pts',(-55.3327110137903,76.975882711877,70.5132611827388));
#213484=CARTESIAN_POINT('Ctrl Pts',(-55.2779314050506,76.5478670960637,
72.3906925793006));
#213485=CARTESIAN_POINT('Ctrl Pts',(-55.2618238758761,76.3736180415815,
72.9377394326584));
#213486=CARTESIAN_POINT('Ctrl Pts',(-55.2458788384028,76.1552807409204,
73.4662010349383));
#213487=CARTESIAN_POINT('Ctrl Pts',(-57.0597576325586,76.1552807409204,
73.4662010349383));
#213488=CARTESIAN_POINT('Ctrl Pts',(-57.0573264371889,76.1220824344896,
73.5465539116859));
#213489=CARTESIAN_POINT('Ctrl Pts',(-57.0548982484733,76.0878506663623,
73.6265113407856));
#213490=CARTESIAN_POINT('Ctrl Pts',(-57.0432786636594,75.9190847628144,
74.0072319048199));
#213491=CARTESIAN_POINT('Ctrl Pts',(-57.0341088716949,75.7711357874271,
74.3017986694038));
#213492=CARTESIAN_POINT('Ctrl Pts',(-56.9957885762682,75.0992476589838,
75.4927358238407));
#213493=CARTESIAN_POINT('Ctrl Pts',(-56.9660576349432,74.4548694757294,
76.3140514136448));
#213494=CARTESIAN_POINT('Ctrl Pts',(-56.9279130819348,73.4583336590304,
77.2497627599759));
#213495=CARTESIAN_POINT('Ctrl Pts',(-56.9187560496566,73.2077666176067,
77.4633042281827));
#213496=CARTESIAN_POINT('Ctrl Pts',(-56.8800484754342,72.1143958811979,
78.3077617050326));
#213497=CARTESIAN_POINT('Ctrl Pts',(-56.8499085692913,71.1872894119421,
78.8189818871622));
#213498=CARTESIAN_POINT('Ctrl Pts',(-56.811347805582,69.8891147015116,79.293159231546));
#213499=CARTESIAN_POINT('Ctrl Pts',(-56.8021738211618,69.5742688114049,
79.3912382909656));
#213500=CARTESIAN_POINT('Ctrl Pts',(-56.7639701171207,68.2547933773763,
79.7334530962459));
#213501=CARTESIAN_POINT('Ctrl Pts',(-56.7343632675314,67.2208270205417,
79.8401211356915));
#213502=CARTESIAN_POINT('Ctrl Pts',(-56.6963451969654,65.8599854096043,
79.774524049877));
#213503=CARTESIAN_POINT('Ctrl Pts',(-56.6871933048202,65.5324560266127,
79.7428906714159));
#213504=CARTESIAN_POINT('Ctrl Pts',(-56.6483561336814,64.1606193960235,
79.543408852849));
#213505=CARTESIAN_POINT('Ctrl Pts',(-56.618077292278,63.1440448474573,79.230242652439));
#213506=CARTESIAN_POINT('Ctrl Pts',(-56.5735389156253,61.708965591362,78.531221992244));
#213507=CARTESIAN_POINT('Ctrl Pts',(-56.5585384715947,61.2438784419826,
78.2574129661823));
#213508=CARTESIAN_POINT('Ctrl Pts',(-56.5206383555161,60.1447937104879,
77.4877590858182));
#213509=CARTESIAN_POINT('Ctrl Pts',(-56.4976849102169,59.5434899221976,
76.9515131398106));
#213510=CARTESIAN_POINT('Ctrl Pts',(-56.4633784313638,58.7282296931324,
76.031603029883));
#213511=CARTESIAN_POINT('Ctrl Pts',(-56.4515293700947,58.4656868142205,
75.6952695211716));
#213512=CARTESIAN_POINT('Ctrl Pts',(-56.4273567704757,57.9795111395256,
74.9853022222109));
#213513=CARTESIAN_POINT('Ctrl Pts',(-56.4150514704382,57.7571893384102,
74.6118084623104));
#213514=CARTESIAN_POINT('Ctrl Pts',(-56.4026978510105,57.5592258456979,
74.2253473780977));
#213515=CARTESIAN_POINT('Origin',(-45.8894114130409,66.6819786653733,69.5522455184007));
#213516=CARTESIAN_POINT('',(-59.2798347108578,76.1552807432749,73.4662010292395));
#213517=CARTESIAN_POINT('',(-58.8740778711611,76.1552807409204,73.4662010349383));
#213518=CARTESIAN_POINT('',(-45.8894114130409,76.1552807409204,73.4662010349383));
#213519=CARTESIAN_POINT('Ctrl Pts',(-57.4656305635332,76.1552807494603,
73.4662010142683));
#213520=CARTESIAN_POINT('Ctrl Pts',(-57.467015478482,76.1740038293382,73.4208838429784));
#213521=CARTESIAN_POINT('Ctrl Pts',(-57.4684018508168,76.1924045744336,
73.3754254530908));
#213522=CARTESIAN_POINT('Ctrl Pts',(-57.4791268110136,76.3321029248102,
73.0230530886952));
#213523=CARTESIAN_POINT('Ctrl Pts',(-57.4885180256257,76.4388381018525,
72.7105830796696));
#213524=CARTESIAN_POINT('Ctrl Pts',(-57.5234071649755,76.7789118976196,
71.5318265754218));
#213525=CARTESIAN_POINT('Ctrl Pts',(-57.548081462003,76.9133480225109,70.6412313736066));
#213526=CARTESIAN_POINT('Ctrl Pts',(-57.5888899472172,76.9405547933868,
69.1913898745211));
#213527=CARTESIAN_POINT('Ctrl Pts',(-57.6046512409984,76.9061305640136,
68.6382920006278));
#213528=CARTESIAN_POINT('Ctrl Pts',(-57.6381300269269,76.7379961738035,
67.471202685675));
#213529=CARTESIAN_POINT('Ctrl Pts',(-57.6554659860436,76.5921995880529,
66.8611953949494));
#213530=CARTESIAN_POINT('Ctrl Pts',(-57.6912072352798,76.1826351896035,
65.650227797998));
#213531=CARTESIAN_POINT('Ctrl Pts',(-57.7096703604995,75.9150563337205,
65.0535258809456));
#213532=CARTESIAN_POINT('Ctrl Pts',(-57.7592658898742,75.0532745094317,
63.5377100374715));
#213533=CARTESIAN_POINT('Ctrl Pts',(-57.7891281575416,74.365922388328,62.6812739258004));
#213534=CARTESIAN_POINT('Ctrl Pts',(-57.8362286934362,73.1324183228756,
61.5659286972865));
#213535=CARTESIAN_POINT('Ctrl Pts',(-57.8525941770464,72.6769632259057,
61.2186032224233));
#213536=CARTESIAN_POINT('Ctrl Pts',(-57.8830343509336,71.7633527920207,
60.6357324287105));
#213537=CARTESIAN_POINT('Ctrl Pts',(-57.8972020711146,71.3117553325347,
60.3931112262922));
#213538=CARTESIAN_POINT('Ctrl Pts',(-57.9294173302583,70.2613766767877,
59.9264068332462));
#213539=CARTESIAN_POINT('Ctrl Pts',(-57.9475315653734,69.6559529717776,
59.7224783141321));
#213540=CARTESIAN_POINT('Ctrl Pts',(-57.9835838838913,68.4210159102935,
59.4311340719715));
#213541=CARTESIAN_POINT('Ctrl Pts',(-58.0011045049236,67.7944202696037,
59.3432482785523));
#213542=CARTESIAN_POINT('Ctrl Pts',(-58.037078420087,66.508443372804,59.2827403411216));
#213543=CARTESIAN_POINT('Ctrl Pts',(-58.0556185294718,65.8517130605504,
59.314887703157));
#213544=CARTESIAN_POINT('Ctrl Pts',(-58.1127259894106,63.8652087101706,
59.6046365097492));
#213545=CARTESIAN_POINT('Ctrl Pts',(-58.1496465648698,62.5795290112645,
60.0623024095847));
#213546=CARTESIAN_POINT('Ctrl Pts',(-58.2140602109587,60.6364591286289,
61.2247457994848));
#213547=CARTESIAN_POINT('Ctrl Pts',(-58.239261910165,59.9192867258378,61.7958566469786));
#213548=CARTESIAN_POINT('Ctrl Pts',(-58.2892121356522,58.6881528212927,
63.0784745967642));
#213549=CARTESIAN_POINT('Ctrl Pts',(-58.3140360354789,58.1704875432274,
63.7759588221726));
#213550=CARTESIAN_POINT('Ctrl Pts',(-58.3571375745576,57.4158586407829,
65.1186017190906));
#213551=CARTESIAN_POINT('Ctrl Pts',(-58.3758307916097,57.1440556581665,
65.7382969422851));
#213552=CARTESIAN_POINT('Ctrl Pts',(-58.413283526736,56.7340904429182,66.9980073249814));
#213553=CARTESIAN_POINT('Ctrl Pts',(-58.431897657372,56.5922226913977,67.6335361595996));
#213554=CARTESIAN_POINT('Ctrl Pts',(-58.4641721348272,56.4492006941421,
68.7752647657879));
#213555=CARTESIAN_POINT('Ctrl Pts',(-58.4780448026808,56.4234574692962,
69.2762201526426));
#213556=CARTESIAN_POINT('Ctrl Pts',(-58.501263199602,56.4416173325673,70.1040382693353));
#213557=CARTESIAN_POINT('Ctrl Pts',(-58.5104876105461,56.4644375849527,
70.4304981763454));
#213558=CARTESIAN_POINT('Ctrl Pts',(-58.5334900665772,56.5596121598773,
71.2357751792123));
#213559=CARTESIAN_POINT('Ctrl Pts',(-58.5473187248335,56.6503451183651,
71.7116215901185));
#213560=CARTESIAN_POINT('Ctrl Pts',(-58.5745365302001,56.8981014858657,
72.6460147409833));
#213561=CARTESIAN_POINT('Ctrl Pts',(-58.5879052191749,57.0546854938996,
73.10342730167));
#213562=CARTESIAN_POINT('Ctrl Pts',(-58.618885913421,57.4864607270938,74.1233723398853));
#213563=CARTESIAN_POINT('Ctrl Pts',(-58.636565387954,57.7820738379356,74.6751774283459));
#213564=CARTESIAN_POINT('Ctrl Pts',(-58.6927354152295,58.869456319419,76.3234632986077));
#213565=CARTESIAN_POINT('Ctrl Pts',(-58.7296145133947,59.8281828204287,
77.2924245069557));
#213566=CARTESIAN_POINT('Ctrl Pts',(-58.8064690912451,62.0673178743056,
78.803961807114));
#213567=CARTESIAN_POINT('Ctrl Pts',(-58.8433913930995,63.3261654160311,
79.3311957990547));
#213568=CARTESIAN_POINT('Ctrl Pts',(-58.8912730138153,64.9759640755396,
79.6647104567306));
#213569=CARTESIAN_POINT('Ctrl Pts',(-58.9007099114221,65.3039499037962,
79.714601179347));
#213570=CARTESIAN_POINT('Ctrl Pts',(-58.9246479319593,66.1507039200396,
79.8016496087106));
#213571=CARTESIAN_POINT('Ctrl Pts',(-58.9390230634061,66.6709254233852,
79.8154039115158));
#213572=CARTESIAN_POINT('Ctrl Pts',(-58.9830883241446,68.2417342164512,
79.7374628040431));
#213573=CARTESIAN_POINT('Ctrl Pts',(-59.0132451353013,69.2792255166301,
79.5234944200773));
#213574=CARTESIAN_POINT('Ctrl Pts',(-59.0518229434675,70.5746421187004,
79.040043347047));
#213575=CARTESIAN_POINT('Ctrl Pts',(-59.0609975786872,70.8776998603756,
78.9099727849275));
#213576=CARTESIAN_POINT('Ctrl Pts',(-59.0991745161019,72.1020906034945,
78.3130146834841));
#213577=CARTESIAN_POINT('Ctrl Pts',(-59.1287536205988,72.9565327629299,
77.7228433579753));
#213578=CARTESIAN_POINT('Ctrl Pts',(-59.1667441086041,73.9477299291393,
76.7896127231644));
#213579=CARTESIAN_POINT('Ctrl Pts',(-59.1758949855277,74.1761531570951,
76.552815053904));
#213580=CARTESIAN_POINT('Ctrl Pts',(-59.2147979782659,75.0910456081536,
75.5081892252033));
#213581=CARTESIAN_POINT('Ctrl Pts',(-59.2451433370461,75.6614373004834,
74.6074410484701));
#213582=CARTESIAN_POINT('Ctrl Pts',(-59.2764194054209,76.1080083511556,
73.5791817217942));
#213583=CARTESIAN_POINT('Ctrl Pts',(-59.2781271442582,76.1318989104646,
73.5227942033599));
#213584=CARTESIAN_POINT('Ctrl Pts',(-59.2798347108578,76.1552807456294,
73.4662010235407));
#213585=CARTESIAN_POINT('Ctrl Pts',(-58.8740778711611,76.1552807409204,
73.4662010349383));
#213586=CARTESIAN_POINT('Ctrl Pts',(-58.8654806787207,76.0383768587021,
73.7491541204752));
#213587=CARTESIAN_POINT('Ctrl Pts',(-58.8568298367276,75.90878836642,74.0268879792384));
#213588=CARTESIAN_POINT('Ctrl Pts',(-58.8302237446842,75.4747103220283,
74.8577554124336));
#213589=CARTESIAN_POINT('Ctrl Pts',(-58.8122496817308,75.1315460085142,
75.388802228158));
#213590=CARTESIAN_POINT('Ctrl Pts',(-58.7768679551842,74.3488587311254,
76.3849487576114));
#213591=CARTESIAN_POINT('Ctrl Pts',(-58.7592049358076,73.9102993558927,
76.8473302188392));
#213592=CARTESIAN_POINT('Ctrl Pts',(-58.7269131362887,73.0513189722705,
77.5989542394252));
#213593=CARTESIAN_POINT('Ctrl Pts',(-58.7124707373962,72.646803865238,77.9032259682973));
#213594=CARTESIAN_POINT('Ctrl Pts',(-58.6807977859588,71.7043343448384,
78.5085980765727));
#213595=CARTESIAN_POINT('Ctrl Pts',(-58.6638417719715,71.1583389362967,
78.793593297296));
#213596=CARTESIAN_POINT('Ctrl Pts',(-58.6276988074985,69.9663460640599,
79.2852149710834));
#213597=CARTESIAN_POINT('Ctrl Pts',(-58.6084968950721,69.3187055868823,
79.4802573030972));
#213598=CARTESIAN_POINT('Ctrl Pts',(-58.5600660604257,67.6442285837402,
79.8090006783218));
#213599=CARTESIAN_POINT('Ctrl Pts',(-58.5318568413971,66.6076070209451,
79.853770689239));
#213600=CARTESIAN_POINT('Ctrl Pts',(-58.4853315968718,64.9767548724265,
79.6777139821547));
#213601=CARTESIAN_POINT('Ctrl Pts',(-58.4679512565759,64.3786780257699,
79.5586295355342));
#213602=CARTESIAN_POINT('Ctrl Pts',(-58.4380529585056,63.3530690024533,
79.2575385648589));
#213603=CARTESIAN_POINT('Ctrl Pts',(-58.4252826161563,62.9206670011429,
79.0982859507564));
#213604=CARTESIAN_POINT('Ctrl Pts',(-58.3934258607863,61.8841174279368,
78.6351257548048));
#213605=CARTESIAN_POINT('Ctrl Pts',(-58.3741846239427,61.2965120122271,
78.299526150952));
#213606=CARTESIAN_POINT('Ctrl Pts',(-58.331302717783,60.0633423854162,77.4235669864371));
#213607=CARTESIAN_POINT('Ctrl Pts',(-58.3083255357522,59.442522328844,76.8566497643465));
#213608=CARTESIAN_POINT('Ctrl Pts',(-58.2592759945427,58.3112313678633,
75.5360167756007));
#213609=CARTESIAN_POINT('Ctrl Pts',(-58.2335467836475,57.817687165605,74.7771172273428));
#213610=CARTESIAN_POINT('Ctrl Pts',(-58.1901612235394,57.1482227094101,
73.3729767633361));
#213611=CARTESIAN_POINT('Ctrl Pts',(-58.1719011545338,56.923856123056,72.7568556656188));
#213612=CARTESIAN_POINT('Ctrl Pts',(-58.1354437498611,56.6015724733037,
71.5132272243054));
#213613=CARTESIAN_POINT('Ctrl Pts',(-58.1174736775659,56.5000540132254,
70.8895808585808));
#213614=CARTESIAN_POINT('Ctrl Pts',(-58.0823674528289,56.4132050083097,
69.6358101939047));
#213615=CARTESIAN_POINT('Ctrl Pts',(-58.0649788425391,56.4272759715382,
69.0084018077861));
#213616=CARTESIAN_POINT('Ctrl Pts',(-58.0333067844926,56.554698426862,67.8955662288894));
#213617=CARTESIAN_POINT('Ctrl Pts',(-58.0192056868718,56.6462646928936,
67.4096225844261));
#213618=CARTESIAN_POINT('Ctrl Pts',(-57.9849711817108,56.9553018835286,
66.2407983865155));
#213619=CARTESIAN_POINT('Ctrl Pts',(-57.9652950581261,57.2099560940189,
65.5704477543328));
#213620=CARTESIAN_POINT('Ctrl Pts',(-57.9262115605762,57.83679855784,64.3290633884311));
#213621=CARTESIAN_POINT('Ctrl Pts',(-57.906915621022,58.200157196157,63.7576331955304));
#213622=CARTESIAN_POINT('Ctrl Pts',(-57.8695297520541,59.0157679561456,
62.7178464370234));
#213623=CARTESIAN_POINT('Ctrl Pts',(-57.8517243389694,59.4616146862542,
62.2484010846137));
#213624=CARTESIAN_POINT('Ctrl Pts',(-57.8073541786503,60.654170304857,61.2093691844293));
#213625=CARTESIAN_POINT('Ctrl Pts',(-57.7805104802939,61.4405265081503,
60.694184432741));
#213626=CARTESIAN_POINT('Ctrl Pts',(-57.7400124097595,62.749174302271,60.0728650906821));
#213627=CARTESIAN_POINT('Ctrl Pts',(-57.7257819053405,63.2283970108871,
59.8879619274299));
#213628=CARTESIAN_POINT('Ctrl Pts',(-57.6923337372342,64.3667012515537,
59.5442925133128));
#213629=CARTESIAN_POINT('Ctrl Pts',(-57.6729996626182,65.0317028118234,
59.4133990380026));
#213630=CARTESIAN_POINT('Ctrl Pts',(-57.6378936609327,66.2687727896728,
59.2949151779632));
#213631=CARTESIAN_POINT('Ctrl Pts',(-57.6222427104545,66.8363256955812,
59.2877560179656));
#213632=CARTESIAN_POINT('Ctrl Pts',(-57.5755586861321,68.4994021601375,
59.4047971992212));
#213633=CARTESIAN_POINT('Ctrl Pts',(-57.5440731569583,69.5776699381353,
59.6583730909056));
#213634=CARTESIAN_POINT('Ctrl Pts',(-57.4951466382518,71.1990127732355,
60.3280309135308));
#213635=CARTESIAN_POINT('Ctrl Pts',(-57.4769062785586,71.7778865356518,
60.6347656474687));
#213636=CARTESIAN_POINT('Ctrl Pts',(-57.4404755134304,72.8498076454491,
61.3414219801888));
#213637=CARTESIAN_POINT('Ctrl Pts',(-57.4225074259785,73.3429084055756,
61.7361231035919));
#213638=CARTESIAN_POINT('Ctrl Pts',(-57.3879561490331,74.2332210615537,
62.5945827351945));
#213639=CARTESIAN_POINT('Ctrl Pts',(-57.3711201580598,74.6315892901806,
63.0534746806907));
#213640=CARTESIAN_POINT('Ctrl Pts',(-57.340421131451,75.2684352083772,63.9339023404445));
#213641=CARTESIAN_POINT('Ctrl Pts',(-57.3267248928043,75.5221454235618,
64.3422105789097));
#213642=CARTESIAN_POINT('Ctrl Pts',(-57.2874445637386,76.1687356212143,
65.5669425758004));
#213643=CARTESIAN_POINT('Ctrl Pts',(-57.2626574740573,76.4833659815526,
66.4195142259108));
#213644=CARTESIAN_POINT('Ctrl Pts',(-57.2233290994146,76.788802993578,67.7770247493286));
#213645=CARTESIAN_POINT('Ctrl Pts',(-57.2094406741909,76.8616773711026,
68.2587859908722));
#213646=CARTESIAN_POINT('Ctrl Pts',(-57.1729484303027,76.9632227952369,
69.5423857028234));
#213647=CARTESIAN_POINT('Ctrl Pts',(-57.1509568701997,76.932577635555,70.3455300793908));
#213648=CARTESIAN_POINT('Ctrl Pts',(-57.1055800295041,76.6835918978208,
71.9366919129624));
#213649=CARTESIAN_POINT('Ctrl Pts',(-57.0823786178288,76.4641733992887,
72.7185600744632));
#213650=CARTESIAN_POINT('Ctrl Pts',(-57.0597576325586,76.1552807409204,
73.4662010349383));
#213651=CARTESIAN_POINT('Origin',(-45.8894114130409,66.6819786653733,69.5522455184007));
#213652=CARTESIAN_POINT('',(-61.0939133588288,76.1552807409204,73.4662010349383));
#213653=CARTESIAN_POINT('',(-60.6878802914039,76.1552807419561,73.4662010324316));
#213654=CARTESIAN_POINT('',(-45.8894114130409,76.1552807409204,73.4662010349383));
#213655=CARTESIAN_POINT('Ctrl Pts',(-59.2798347108578,76.1552807456294,
73.4662010235407));
#213656=CARTESIAN_POINT('Ctrl Pts',(-59.2873239377944,76.2578312814522,
73.2179886452789));
#213657=CARTESIAN_POINT('Ctrl Pts',(-59.2948125599407,76.3505958902946,
72.9658202019355));
#213658=CARTESIAN_POINT('Ctrl Pts',(-59.3212550248658,76.6412408841389,
72.0683661022729));
#213659=CARTESIAN_POINT('Ctrl Pts',(-59.3404565657508,76.7852352409474,
71.4074966004155));
#213660=CARTESIAN_POINT('Ctrl Pts',(-59.3889800804819,76.9829003351291,
69.7092774286031));
#213661=CARTESIAN_POINT('Ctrl Pts',(-59.4172768981262,76.9461688502664,
68.6690429788179));
#213662=CARTESIAN_POINT('Ctrl Pts',(-59.4640581665987,76.6404227144672,
67.0484062161532));
#213663=CARTESIAN_POINT('Ctrl Pts',(-59.4815942391593,76.4725145859891,
66.4562414461179));
#213664=CARTESIAN_POINT('Ctrl Pts',(-59.5124154203648,76.0779084293696,
65.4270660907031));
#213665=CARTESIAN_POINT('Ctrl Pts',(-59.5259528021725,75.8709055245387,
64.9845081081328));
#213666=CARTESIAN_POINT('Ctrl Pts',(-59.5586389464261,75.3041133707561,
63.9685683013047));
#213667=CARTESIAN_POINT('Ctrl Pts',(-59.5779246567413,74.9175650253119,
63.4127211099847));
#213668=CARTESIAN_POINT('Ctrl Pts',(-59.6160754061338,74.0425641561455,
62.3872807913945));
#213669=CARTESIAN_POINT('Ctrl Pts',(-59.6346024318829,73.5566506811219,
61.9198261856102));
#213670=CARTESIAN_POINT('Ctrl Pts',(-59.6724351197661,72.4983354380824,
61.0853544833108));
#213671=CARTESIAN_POINT('Ctrl Pts',(-59.6916891483082,71.9282138895974,
60.7207535829762));
#213672=CARTESIAN_POINT('Ctrl Pts',(-59.7328542569981,70.6331193165802,
60.0624708439655));
#213673=CARTESIAN_POINT('Ctrl Pts',(-59.7542186705655,69.9019725341391,
59.7901260313104));
#213674=CARTESIAN_POINT('Ctrl Pts',(-59.7951715089607,68.4901351827486,
59.4403144874627));
#213675=CARTESIAN_POINT('Ctrl Pts',(-59.8145446091965,67.8186828647086,
59.3430110164237));
#213676=CARTESIAN_POINT('Ctrl Pts',(-59.8478622232024,66.6385684477296,
59.2899291105759));
#213677=CARTESIAN_POINT('Ctrl Pts',(-59.8618209806189,66.1335879871315,
59.304499705822));
#213678=CARTESIAN_POINT('Ctrl Pts',(-59.8935251446396,65.0060535038607,
59.4206410901775));
#213679=CARTESIAN_POINT('Ctrl Pts',(-59.9113264579511,64.3876333714385,
59.5425452453374));
#213680=CARTESIAN_POINT('Ctrl Pts',(-59.967609771616,62.4896831880558,60.1019125225695));
#213681=CARTESIAN_POINT('Ctrl Pts',(-60.0044817633918,61.2830797298608,
60.7354424055245));
#213682=CARTESIAN_POINT('Ctrl Pts',(-60.0813271442445,59.1832849088952,
62.4347426735237));
#213683=CARTESIAN_POINT('Ctrl Pts',(-60.1182483120269,58.3111222160689,
63.4844601762531));
#213684=CARTESIAN_POINT('Ctrl Pts',(-60.1661319992958,57.5098768998731,
64.9647575329513));
#213685=CARTESIAN_POINT('Ctrl Pts',(-60.175570853064,57.3662509499148,65.2639221863736));
#213686=CARTESIAN_POINT('Ctrl Pts',(-60.1996436772939,57.0335944489885,
66.0527814412899));
#213687=CARTESIAN_POINT('Ctrl Pts',(-60.2141508145759,56.8671983647576,
66.5509691579901));
#213688=CARTESIAN_POINT('Ctrl Pts',(-60.2579230862595,56.4873765134373,
68.0660100749166));
#213689=CARTESIAN_POINT('Ctrl Pts',(-60.2876399944278,56.3893297683789,
69.1048132112122));
#213690=CARTESIAN_POINT('Ctrl Pts',(-60.3257703432487,56.4677601315748,
70.4690258915158));
#213691=CARTESIAN_POINT('Ctrl Pts',(-60.3349268208386,56.5024479063959,
70.7963916758307));
#213692=CARTESIAN_POINT('Ctrl Pts',(-60.3736532148053,56.7140616379533,
72.162289314325));
#213693=CARTESIAN_POINT('Ctrl Pts',(-60.4038128271924,57.0347519115952,
73.1720137110355));
#213694=CARTESIAN_POINT('Ctrl Pts',(-60.4423934893387,57.6503102991411,
74.4102394881232));
#213695=CARTESIAN_POINT('Ctrl Pts',(-60.4515682410964,57.8111861304835,
74.6981349684982));
#213696=CARTESIAN_POINT('Ctrl Pts',(-60.4897417630452,58.5321412935251,
75.8537195879102));
#213697=CARTESIAN_POINT('Ctrl Pts',(-60.5193172463587,59.2078496718595,
76.6420853490512));
#213698=CARTESIAN_POINT('Ctrl Pts',(-60.5573040612076,60.2389420037159,
77.5308356752901));
#213699=CARTESIAN_POINT('Ctrl Pts',(-60.5664547917166,60.4981936958185,
77.7334083585058));
#213700=CARTESIAN_POINT('Ctrl Pts',(-60.6053624474569,61.6323858776986,
78.5348762542881));
#213701=CARTESIAN_POINT('Ctrl Pts',(-60.6357127054609,62.5877081838141,
79.0086189465251));
#213702=CARTESIAN_POINT('Ctrl Pts',(-60.674487735492,63.9131697130843,79.4267077905138));
#213703=CARTESIAN_POINT('Ctrl Pts',(-60.6836704322661,64.2323578677275,
79.5106924671336));
#213704=CARTESIAN_POINT('Ctrl Pts',(-60.7118298660933,65.21508558333,79.7191521568226));
#213705=CARTESIAN_POINT('Ctrl Pts',(-60.7310315029189,65.8873448685828,
79.7936470979331));
#213706=CARTESIAN_POINT('Ctrl Pts',(-60.7795309967203,67.5960717486121,
79.8136461475118));
#213707=CARTESIAN_POINT('Ctrl Pts',(-60.8078051086568,68.6260197611533,
79.6691923839409));
#213708=CARTESIAN_POINT('Ctrl Pts',(-60.85451944694,70.2039656251719,79.1976383421178));
#213709=CARTESIAN_POINT('Ctrl Pts',(-60.8720146380996,70.7741772355134,
78.969884356699));
#213710=CARTESIAN_POINT('Ctrl Pts',(-60.9025867168087,71.7490578343482,
78.4751395451311));
#213711=CARTESIAN_POINT('Ctrl Pts',(-60.9159159079656,72.1616733403399,
78.2278593814121));
#213712=CARTESIAN_POINT('Ctrl Pts',(-60.9483752296809,73.1088119638081,
77.5656261636239));
#213713=CARTESIAN_POINT('Ctrl Pts',(-60.9676476524271,73.6226153704897,
77.1249598270608));
#213714=CARTESIAN_POINT('Ctrl Pts',(-61.0069126057781,74.5810939893403,
76.1228360744059));
#213715=CARTESIAN_POINT('Ctrl Pts',(-61.026489504624,75.0179865180214,75.5588800128241));
#213716=CARTESIAN_POINT('Ctrl Pts',(-61.0621754880272,75.6872603427455,
74.4796447268075));
#213717=CARTESIAN_POINT('Ctrl Pts',(-61.0780551106555,75.9421911667023,
73.9819610882114));
#213718=CARTESIAN_POINT('Ctrl Pts',(-61.0939133588288,76.1552807409204,
73.4662010349383));
#213719=CARTESIAN_POINT('Ctrl Pts',(-60.6878802914039,76.1552807429917,
73.4662010299249));
#213720=CARTESIAN_POINT('Ctrl Pts',(-60.6549485341108,75.7132504877363,
74.5360870118048));
#213721=CARTESIAN_POINT('Ctrl Pts',(-60.6232629579733,75.0931226335129,
75.5234705721753));
#213722=CARTESIAN_POINT('Ctrl Pts',(-60.5753209784772,73.965374356376,76.7840831573706));
#213723=CARTESIAN_POINT('Ctrl Pts',(-60.5600539347455,73.5790171038901,
77.1534423333565));
#213724=CARTESIAN_POINT('Ctrl Pts',(-60.5260316711703,72.6417442432974,
77.9189216694829));
#213725=CARTESIAN_POINT('Ctrl Pts',(-60.5073738169853,72.0767549475306,
78.2938972018152));
#213726=CARTESIAN_POINT('Ctrl Pts',(-60.4735852252674,71.0172501247381,
78.8549804079524));
#213727=CARTESIAN_POINT('Ctrl Pts',(-60.4586939776463,70.537527052056,79.0638277026571));
#213728=CARTESIAN_POINT('Ctrl Pts',(-60.4262453781121,69.4576424072261,
79.43877344229));
#213729=CARTESIAN_POINT('Ctrl Pts',(-60.409058418936,68.8540231352694,79.5886775647626));
#213730=CARTESIAN_POINT('Ctrl Pts',(-60.3734714870408,67.5960713455299,
79.7822078911068));
#213731=CARTESIAN_POINT('Ctrl Pts',(-60.355017215576,66.9435951390965,79.8196325924058));
#213732=CARTESIAN_POINT('Ctrl Pts',(-60.3055240992358,65.2047612307084,
79.7534292233736));
#213733=CARTESIAN_POINT('Ctrl Pts',(-60.2757486247089,64.1310079803187,
79.5391809452647));
#213734=CARTESIAN_POINT('Ctrl Pts',(-60.2286892275576,62.5735019927232,
78.9603211407063));
#213735=CARTESIAN_POINT('Ctrl Pts',(-60.2122723783564,62.0535931967266,
78.7157340010946));
#213736=CARTESIAN_POINT('Ctrl Pts',(-60.181791493639,61.1137897171559,78.1731239029127));
#213737=CARTESIAN_POINT('Ctrl Pts',(-60.1676315602797,60.6904769236396,
77.8844831172379));
#213738=CARTESIAN_POINT('Ctrl Pts',(-60.1329740426831,59.7237980888031,
77.1134404341653));
#213739=CARTESIAN_POINT('Ctrl Pts',(-60.1123084476268,59.2066537291693,
76.6025959714561));
#213740=CARTESIAN_POINT('Ctrl Pts',(-60.082295326596,58.5358905214297,75.7824723433042));
#213741=CARTESIAN_POINT('Ctrl Pts',(-60.0729376397816,58.3368489241872,
75.5132260455352));
#213742=CARTESIAN_POINT('Ctrl Pts',(-60.0454258533623,57.7900555909077,
74.6923694873538));
#213743=CARTESIAN_POINT('Ctrl Pts',(-60.0272520902436,57.4813255399839,
74.1167986352783));
#213744=CARTESIAN_POINT('Ctrl Pts',(-59.9952901842338,57.0456129228912,
73.0776794715103));
#213745=CARTESIAN_POINT('Ctrl Pts',(-59.9817127483809,56.892578447159,72.6272857226267));
#213746=CARTESIAN_POINT('Ctrl Pts',(-59.9549264327128,56.6499902430636,
71.708128035941));
#213747=CARTESIAN_POINT('Ctrl Pts',(-59.9417584347214,56.5607852278596,
71.2404603787749));
#213748=CARTESIAN_POINT('Ctrl Pts',(-59.9191599910854,56.4648900413591,
70.4378726483234));
#213749=CARTESIAN_POINT('Ctrl Pts',(-59.9098138709983,56.441525080417,70.1057288119717));
#213750=CARTESIAN_POINT('Ctrl Pts',(-59.8862018942639,56.4235443216733,
69.2711961468919));
#213751=CARTESIAN_POINT('Ctrl Pts',(-59.8718628566535,56.4496103948148,
68.7692382534012));
#213752=CARTESIAN_POINT('Ctrl Pts',(-59.839516880951,56.5925153240701,67.6347664157159));
#213753=CARTESIAN_POINT('Ctrl Pts',(-59.8218335602107,56.7322556075732,
67.007248505875));
#213754=CARTESIAN_POINT('Ctrl Pts',(-59.7773523524945,57.220434708535,65.4984210150842));
#213755=CARTESIAN_POINT('Ctrl Pts',(-59.7502626452442,57.633921297722,64.6443974106474));
#213756=CARTESIAN_POINT('Ctrl Pts',(-59.7089452485514,58.4549724285869,
63.4151545489328));
#213757=CARTESIAN_POINT('Ctrl Pts',(-59.6941331228875,58.7857298103031,
62.9950532064511));
#213758=CARTESIAN_POINT('Ctrl Pts',(-59.6600401087609,59.6066435074168,
62.1050767582944));
#213759=CARTESIAN_POINT('Ctrl Pts',(-59.6406626778559,60.1137418848491,
61.6542114447438));
#213760=CARTESIAN_POINT('Ctrl Pts',(-59.6075214539254,61.0649230001214,
60.963906100831));
#213761=CARTESIAN_POINT('Ctrl Pts',(-59.5937295363409,61.4890949026599,
60.700982854176));
#213762=CARTESIAN_POINT('Ctrl Pts',(-59.5619836481202,62.4948812706617,
60.1748196345405));
#213763=CARTESIAN_POINT('Ctrl Pts',(-59.5439632172434,63.0853266098694,
59.9328910318027));
#213764=CARTESIAN_POINT('Ctrl Pts',(-59.5163445957165,64.0141391665109,
59.6498785787787));
#213765=CARTESIAN_POINT('Ctrl Pts',(-59.5068630287181,64.3384759567163,
59.5681462490696));
#213766=CARTESIAN_POINT('Ctrl Pts',(-59.4781411725836,65.3433315880202,
59.366596917901));
#213767=CARTESIAN_POINT('Ctrl Pts',(-59.4590485401284,66.0324285189169,
59.299562823386));
#213768=CARTESIAN_POINT('Ctrl Pts',(-59.4259185778911,67.2049256704212,
59.3042570477717));
#213769=CARTESIAN_POINT('Ctrl Pts',(-59.4121692654834,67.6860998487761,
59.3401703957783));
#213770=CARTESIAN_POINT('Ctrl Pts',(-59.3737534033847,69.0266224411124,
59.5359101890221));
#213771=CARTESIAN_POINT('Ctrl Pts',(-59.3498274925003,69.8706508586717,
59.7718212381078));
#213772=CARTESIAN_POINT('Ctrl Pts',(-59.299281691461,71.5193218358627,60.4690792530385));
#213773=CARTESIAN_POINT('Ctrl Pts',(-59.2731736187973,72.3123426922754,
60.9381397042643));
#213774=CARTESIAN_POINT('Ctrl Pts',(-59.2099049123124,74.0932680633157,
62.3437747327888));
#213775=CARTESIAN_POINT('Ctrl Pts',(-59.1714264730219,74.9781754503829,
63.3827736498539));
#213776=CARTESIAN_POINT('Ctrl Pts',(-59.1153877058776,75.9562112306616,
65.1381831109986));
#213777=CARTESIAN_POINT('Ctrl Pts',(-59.0969999679401,76.2203414750931,
65.7423948469949));
#213778=CARTESIAN_POINT('Ctrl Pts',(-59.0603571616319,76.6212706720565,
66.9690058615184));
#213779=CARTESIAN_POINT('Ctrl Pts',(-59.0423634308292,76.7617220829095,
67.5871901044692));
#213780=CARTESIAN_POINT('Ctrl Pts',(-59.0155634669358,76.8870309466762,
68.5390172346081));
#213781=CARTESIAN_POINT('Ctrl Pts',(-59.0064538859771,76.9141896502028,
68.865527374132));
#213782=CARTESIAN_POINT('Ctrl Pts',(-58.966135792939,76.9646919211623,70.304674835983));
#213783=CARTESIAN_POINT('Ctrl Pts',(-58.9343155956169,76.8224161565893,
71.4155415775799));
#213784=CARTESIAN_POINT('Ctrl Pts',(-58.8935634996675,76.4048021503051,
72.8157919687679));
#213785=CARTESIAN_POINT('Ctrl Pts',(-58.8838562479809,76.2882462665789,
73.1443724947634));
#213786=CARTESIAN_POINT('Ctrl Pts',(-58.8740778711611,76.1552807409204,
73.4662010349383));
#213787=CARTESIAN_POINT('Origin',(-45.8894114130409,66.6819786653733,69.5522455184007));
#213788=CARTESIAN_POINT('',(-62.9075068658247,76.1552807409205,73.4662010349382));
#213789=CARTESIAN_POINT('',(-62.5017927896903,76.155280734099,73.4662010514488));
#213790=CARTESIAN_POINT('',(-45.8894114130409,76.1552807409204,73.4662010349383));
#213791=CARTESIAN_POINT('',(-62.1255457361908,56.4404739457998,69.970346603214));
#213792=CARTESIAN_POINT('Ctrl Pts',(-62.9075068658247,76.1552807409205,
73.4662010349381));
#213793=CARTESIAN_POINT('Ctrl Pts',(-62.8890297137549,75.9058901354936,
74.0698237715866));
#213794=CARTESIAN_POINT('Ctrl Pts',(-62.8709501951456,75.5993777230872,
74.6482296293145));
#213795=CARTESIAN_POINT('Ctrl Pts',(-62.8346556323582,74.8824994691326,
75.7357486846771));
#213796=CARTESIAN_POINT('Ctrl Pts',(-62.816127299745,74.4743566483045,76.2427667065411));
#213797=CARTESIAN_POINT('Ctrl Pts',(-62.7595831183316,73.087620491147,77.6650712602951));
#213798=CARTESIAN_POINT('Ctrl Pts',(-62.7232980830353,71.975875999061,78.4305795136537));
#213799=CARTESIAN_POINT('Ctrl Pts',(-62.6471481891127,69.5250490757961,
79.4898561694311));
#213800=CARTESIAN_POINT('Ctrl Pts',(-62.6109576119547,68.2100385426075,
79.7749756124774));
#213801=CARTESIAN_POINT('Ctrl Pts',(-62.5541063933798,66.212220750335,79.8130641293939));
#213802=CARTESIAN_POINT('Ctrl Pts',(-62.535111901963,65.5474139902432,79.760960059608));
#213803=CARTESIAN_POINT('Ctrl Pts',(-62.4978581696945,64.2397658569823,
79.5290869291397));
#213804=CARTESIAN_POINT('Ctrl Pts',(-62.4796746883654,63.5999399229083,
79.3503470402618));
#213805=CARTESIAN_POINT('Ctrl Pts',(-62.4424295539205,62.3682979709726,
78.8735937106281));
#213806=CARTESIAN_POINT('Ctrl Pts',(-62.4235188596298,61.7790196920629,
78.5775642584995));
#213807=CARTESIAN_POINT('Ctrl Pts',(-62.3861515017278,60.6593754335759,
77.8728813615583));
#213808=CARTESIAN_POINT('Ctrl Pts',(-62.367792036736,60.1323725892804,77.4647286706259));
#213809=CARTESIAN_POINT('Ctrl Pts',(-62.3306363167817,59.1642311111784,
76.5514880424947));
#213810=CARTESIAN_POINT('Ctrl Pts',(-62.3115449033513,58.7255184123369,
76.0484475302655));
#213811=CARTESIAN_POINT('Ctrl Pts',(-62.2644735866284,57.763231000053,74.7000482335411));
#213812=CARTESIAN_POINT('Ctrl Pts',(-62.237467135121,57.3076947730774,73.8144878831635));
#213813=CARTESIAN_POINT('Ctrl Pts',(-62.1815044190819,56.6647956602292,
71.9398912558015));
#213814=CARTESIAN_POINT('Ctrl Pts',(-62.1531555603416,56.4809386499188,
70.9606701984124));
#213815=CARTESIAN_POINT('Ctrl Pts',(-62.1255316836823,56.4405094161815,
69.9703455277974));
#213816=CARTESIAN_POINT('Ctrl Pts',(-61.0939133588288,76.1552807409204,
73.4662010349383));
#213817=CARTESIAN_POINT('Ctrl Pts',(-61.0972367439251,76.1999375471068,
73.3581141103563));
#213818=CARTESIAN_POINT('Ctrl Pts',(-61.1005568733328,76.2427567690946,
73.2492332337271));
#213819=CARTESIAN_POINT('Ctrl Pts',(-61.1224307548111,76.5133223357398,
72.5250515977391));
#213820=CARTESIAN_POINT('Ctrl Pts',(-61.1405086451475,76.6833975931833,
71.8898758938489));
#213821=CARTESIAN_POINT('Ctrl Pts',(-61.1778581615379,76.9029391447842,
70.5770148905306));
#213822=CARTESIAN_POINT('Ctrl Pts',(-61.1970990172255,76.9482316221127,
69.9018442930587));
#213823=CARTESIAN_POINT('Ctrl Pts',(-61.2400395265103,76.9001918497218,
68.3879451290524));
#213824=CARTESIAN_POINT('Ctrl Pts',(-61.2630717386202,76.7705483014273,
67.5551875938367));
#213825=CARTESIAN_POINT('Ctrl Pts',(-61.312198681151,76.2940135131976,65.880082552741));
#213826=CARTESIAN_POINT('Ctrl Pts',(-61.3379412428464,75.9337910039552,
65.0489153455686));
#213827=CARTESIAN_POINT('Ctrl Pts',(-61.3813544223569,75.1324778699189,
63.7144282365011));
#213828=CARTESIAN_POINT('Ctrl Pts',(-61.3996290326739,74.742489401471,63.186775714214));
#213829=CARTESIAN_POINT('Ctrl Pts',(-61.4361064185458,73.8832261135128,
62.2308855240864));
#213830=CARTESIAN_POINT('Ctrl Pts',(-61.4540782302245,73.4191962866505,
61.8017492157138));
#213831=CARTESIAN_POINT('Ctrl Pts',(-61.4894335104073,72.4146824655236,
61.0315685733077));
#213832=CARTESIAN_POINT('Ctrl Pts',(-61.5070703523648,71.8758691137458,
60.6928252217055));
#213833=CARTESIAN_POINT('Ctrl Pts',(-61.5392428845874,70.8610138634007,
60.1793893499888));
#213834=CARTESIAN_POINT('Ctrl Pts',(-61.5535907935117,70.39678499443,59.9858993636265));
#213835=CARTESIAN_POINT('Ctrl Pts',(-61.585876373904,69.3138961483048,59.6253154434844));
#213836=CARTESIAN_POINT('Ctrl Pts',(-61.603494777744,68.6899897691559,59.4805612565544));
#213837=CARTESIAN_POINT('Ctrl Pts',(-61.6480441332805,67.1159772358438,
59.2675350741756));
#213838=CARTESIAN_POINT('Ctrl Pts',(-61.6752737373193,66.1621390075234,
59.271516041684));
#213839=CARTESIAN_POINT('Ctrl Pts',(-61.7207714169046,64.5507744930857,
59.5033120523018));
#213840=CARTESIAN_POINT('Ctrl Pts',(-61.7396021229131,63.8902760825381,
59.6664228414106));
#213841=CARTESIAN_POINT('Ctrl Pts',(-61.7736284575458,62.7577122202194,
60.0687646542903));
#213842=CARTESIAN_POINT('Ctrl Pts',(-61.7885898979955,62.2788005150607,
60.2814151338566));
#213843=CARTESIAN_POINT('Ctrl Pts',(-61.8177696215568,61.3682737972457,
60.7722496029264));
#213844=CARTESIAN_POINT('Ctrl Pts',(-61.8319097085121,60.9370959355713,
61.0481221638876));
#213845=CARTESIAN_POINT('Ctrl Pts',(-61.8635657927953,60.0320550465909,
61.7275375424783));
#213846=CARTESIAN_POINT('Ctrl Pts',(-61.8811261608956,59.5706660897355,
62.1443605664694));
#213847=CARTESIAN_POINT('Ctrl Pts',(-61.9371865882037,58.2340501941442,
63.5925388739433));
#213848=CARTESIAN_POINT('Ctrl Pts',(-61.9740772309726,57.5232964863006,
64.7559831093433));
#213849=CARTESIAN_POINT('Ctrl Pts',(-62.0507304415328,56.595657382813,67.2859393327457));
#213850=CARTESIAN_POINT('Ctrl Pts',(-62.0874436008208,56.385669728745,68.6270190094509));
#213851=CARTESIAN_POINT('Ctrl Pts',(-62.1256936736044,56.4405092384687,
69.970341174655));
#213852=CARTESIAN_POINT('Ctrl Pts',(-62.5017927901887,76.1552807340937,
73.4662010514616));
#213853=CARTESIAN_POINT('Ctrl Pts',(-62.4841922972289,75.9145711506133,
74.0488123192402));
#213854=CARTESIAN_POINT('Ctrl Pts',(-62.4666695608352,75.6205925594882,
74.6080634458034));
#213855=CARTESIAN_POINT('Ctrl Pts',(-62.4394943477806,75.0973719085795,
75.4133374247731));
#213856=CARTESIAN_POINT('Ctrl Pts',(-62.4301092507227,74.9044674712425,
75.6810234098114));
#213857=CARTESIAN_POINT('Ctrl Pts',(-62.3906691516004,74.0402843286251,
76.7658050470616));
#213858=CARTESIAN_POINT('Ctrl Pts',(-62.3617368215435,73.2575992204254,
77.4858024457807));
#213859=CARTESIAN_POINT('Ctrl Pts',(-62.3224962160946,72.1053173772563,
78.25615692612));
#213860=CARTESIAN_POINT('Ctrl Pts',(-62.3131328650323,71.823252316642,78.4256879595615));
#213861=CARTESIAN_POINT('Ctrl Pts',(-62.2743688109905,70.6222510105518,
79.0710130229089));
#213862=CARTESIAN_POINT('Ctrl Pts',(-62.2460538557988,69.6420793705324,
79.4198942368236));
#213863=CARTESIAN_POINT('Ctrl Pts',(-62.2074497315998,68.3027992898412,
79.6786487708405));
#213864=CARTESIAN_POINT('Ctrl Pts',(-62.1980699502291,67.9764083234649,
79.7255219348873));
#213865=CARTESIAN_POINT('Ctrl Pts',(-62.1587963366469,66.6014304642697,
79.8557322082481));
#213866=CARTESIAN_POINT('Ctrl Pts',(-62.1300162389156,65.5454851851599,
79.793178877457));
#213867=CARTESIAN_POINT('Ctrl Pts',(-62.0855242684048,64.0092360112201,
79.461304617849));
#213868=CARTESIAN_POINT('Ctrl Pts',(-62.070654090811,63.5099597587049,79.3129472836041));
#213869=CARTESIAN_POINT('Ctrl Pts',(-62.0466204641156,62.7143708676141,
79.0090169142959));
#213870=CARTESIAN_POINT('Ctrl Pts',(-62.0373875858622,62.4105596550341,
78.8757329341445));
#213871=CARTESIAN_POINT('Ctrl Pts',(-61.9904501189389,60.9038137257355,
78.1255817594361));
#213872=CARTESIAN_POINT('Ctrl Pts',(-61.9519710838904,59.8248949818888,
77.2897960181841));
#213873=CARTESIAN_POINT('Ctrl Pts',(-61.8792589333449,58.1163135090342,
75.3201748664833));
#213874=CARTESIAN_POINT('Ctrl Pts',(-61.8434477977863,57.4747010030091,
74.228320341494));
#213875=CARTESIAN_POINT('Ctrl Pts',(-61.7895071829267,56.8162421860416,
72.413248143466));
#213876=CARTESIAN_POINT('Ctrl Pts',(-61.7707657618205,56.6492959879891,
71.7575500086725));
#213877=CARTESIAN_POINT('Ctrl Pts',(-61.7325192602644,56.4466488491963,
70.42227352131));
#213878=CARTESIAN_POINT('Ctrl Pts',(-61.7132062075065,56.411563542068,69.7459346692063));
#213879=CARTESIAN_POINT('Ctrl Pts',(-61.6754559768368,56.4749534317402,
68.3970798056311));
#213880=CARTESIAN_POINT('Ctrl Pts',(-61.6567441080256,56.5731019559975,
67.7278599535121));
#213881=CARTESIAN_POINT('Ctrl Pts',(-61.6283190342541,56.8160501993116,
66.7531936361492));
#213882=CARTESIAN_POINT('Ctrl Pts',(-61.6189341589787,56.9111982087794,
66.4372681446033));
#213883=CARTESIAN_POINT('Ctrl Pts',(-61.5795010328776,57.37465676238,65.1303265128581));
#213884=CARTESIAN_POINT('Ctrl Pts',(-61.5505750818935,57.8798668347393,
64.1947793356987));
#213885=CARTESIAN_POINT('Ctrl Pts',(-61.5113410431149,58.7180248529935,
63.0911217362924));
#213886=CARTESIAN_POINT('Ctrl Pts',(-61.5019775256112,58.9294404974505,
62.8389131309679));
#213887=CARTESIAN_POINT('Ctrl Pts',(-61.4632083193789,59.8546679717751,
61.8372687115672));
#213888=CARTESIAN_POINT('Ctrl Pts',(-61.4348886658117,60.6677702807964,
61.1878960272877));
#213889=CARTESIAN_POINT('Ctrl Pts',(-61.3907375002071,62.0194455357514,
60.4089801986216));
#213890=CARTESIAN_POINT('Ctrl Pts',(-61.3757162824535,62.4941382459002,
60.1820531209446));
#213891=CARTESIAN_POINT('Ctrl Pts',(-61.3515272726771,63.2934640245289,
59.8728614805776));
#213892=CARTESIAN_POINT('Ctrl Pts',(-61.3422905752263,63.6084255106306,
59.7682903446434));
#213893=CARTESIAN_POINT('Ctrl Pts',(-61.2953515245365,65.2297471767491,
59.3160256255313));
#213894=CARTESIAN_POINT('Ctrl Pts',(-61.2568736358841,66.5906529660278,
59.2139267751174));
#213895=CARTESIAN_POINT('Ctrl Pts',(-61.1815476488329,69.2716270960578,
59.5433682057727));
#213896=CARTESIAN_POINT('Ctrl Pts',(-61.1431284236275,70.5655415412455,
59.970917131753));
#213897=CARTESIAN_POINT('Ctrl Pts',(-61.0879192858583,72.2872921442577,
60.9476120127659));
#213898=CARTESIAN_POINT('Ctrl Pts',(-61.0703450852994,72.80534901744,61.3082425228484));
#213899=CARTESIAN_POINT('Ctrl Pts',(-61.0381959693188,73.672257774307,62.0387710039529));
#213900=CARTESIAN_POINT('Ctrl Pts',(-61.0237913443329,74.033043166991,62.3913688874729));
#213901=CARTESIAN_POINT('Ctrl Pts',(-60.9948506921104,74.7136963947578,
63.1624598137185));
#213902=CARTESIAN_POINT('Ctrl Pts',(-60.9803381643744,75.0302345998815,
63.5819457145789));
#213903=CARTESIAN_POINT('Ctrl Pts',(-60.9477026318596,75.6585442783944,
64.5628973954093));
#213904=CARTESIAN_POINT('Ctrl Pts',(-60.929523342466,75.9525650523743,65.133134905363));
#213905=CARTESIAN_POINT('Ctrl Pts',(-60.8933588951831,76.4274396498665,
66.3136799793408));
#213906=CARTESIAN_POINT('Ctrl Pts',(-60.8757973779874,76.6086228929761,
66.9208855829549));
#213907=CARTESIAN_POINT('Ctrl Pts',(-60.8397638334601,76.8617260615403,
68.1856495294659));
#213908=CARTESIAN_POINT('Ctrl Pts',(-60.8211917604325,76.9284120227369,
68.8413094635645));
#213909=CARTESIAN_POINT('Ctrl Pts',(-60.7640366603233,76.9388849077235,
70.8504171533983));
#213910=CARTESIAN_POINT('Ctrl Pts',(-60.7271143861794,76.6785175472096,
72.1901584257861));
#213911=CARTESIAN_POINT('Ctrl Pts',(-60.6884024604886,76.1622782263207,
73.4492321076023));
#213912=CARTESIAN_POINT('Ctrl Pts',(-60.6881413685773,76.1587850810255,
73.4577191622393));
#213913=CARTESIAN_POINT('Ctrl Pts',(-60.6878802914039,76.1552807429917,
73.4662010299249));
#213914=CARTESIAN_POINT('Origin',(-21.6548258024609,75.,72.9888893865801));
#213915=CARTESIAN_POINT('',(-23.7494631149408,87.0149197165679,77.9529305028912));
#213916=CARTESIAN_POINT('',(-23.5675316904177,87.0149197054641,77.9529305294612));
#213917=CARTESIAN_POINT('',(-21.6548258024609,87.0149197055719,77.9529305295058));
#213918=CARTESIAN_POINT('',(-23.5675316903009,81.8060517138039,84.0648841531475));
#213919=CARTESIAN_POINT('Ctrl Pts',(-23.7494631142982,87.0149197165734,
77.9529305028779));
#213920=CARTESIAN_POINT('Ctrl Pts',(-23.7335469728164,86.7427187400688,
78.6117632568488));
#213921=CARTESIAN_POINT('Ctrl Pts',(-23.7173356484354,86.4167322474098,
79.2472274990606));
#213922=CARTESIAN_POINT('Ctrl Pts',(-23.6789660693055,85.5103834448235,
80.7050232771271));
#213923=CARTESIAN_POINT('Ctrl Pts',(-23.6573462260829,84.8836923221021,
81.4929757686694));
#213924=CARTESIAN_POINT('Ctrl Pts',(-23.6129675706424,83.4586738982171,
82.9118922602039));
#213925=CARTESIAN_POINT('Ctrl Pts',(-23.5899173818351,82.6644777038016,
83.5373927807216));
#213926=CARTESIAN_POINT('Ctrl Pts',(-23.5675316903009,81.8060517138039,
84.0648841531474));
#213927=CARTESIAN_POINT('Origin',(-23.5675316903009,75.,72.9888893865801));
#213928=CARTESIAN_POINT('Origin',(-21.6548258024609,75.,72.9888893865801));
#213929=CARTESIAN_POINT('',(-25.5628518781596,87.0149197055719,77.9529305295058));
#213930=CARTESIAN_POINT('',(-25.2581222247367,87.0149197055719,77.9529305295058));
#213931=CARTESIAN_POINT('',(-21.6548258024609,87.0149197055719,77.9529305295058));
#213932=CARTESIAN_POINT('Ctrl Pts',(-25.5628518781596,87.0149197055719,
77.9529305295058));
#213933=CARTESIAN_POINT('Ctrl Pts',(-25.5342348853662,86.524408980039,79.1401581958999));
#213934=CARTESIAN_POINT('Ctrl Pts',(-25.506780222184,85.859722271091,80.250298001449));
#213935=CARTESIAN_POINT('Ctrl Pts',(-25.4598723099545,84.537509974558,81.858175099878));
#213936=CARTESIAN_POINT('Ctrl Pts',(-25.4420110595247,83.9790909030928,
82.4230970114736));
#213937=CARTESIAN_POINT('Ctrl Pts',(-25.4061623457357,82.7368144036211,
83.46899814892));
#213938=CARTESIAN_POINT('Ctrl Pts',(-25.3882919641257,82.0510448433343,
83.9421414655669));
#213939=CARTESIAN_POINT('Ctrl Pts',(-25.3604186304516,80.9574848293449,
84.551118847472));
#213940=CARTESIAN_POINT('Ctrl Pts',(-25.350916041777,80.580447467698,84.7377352997618));
#213941=CARTESIAN_POINT('Ctrl Pts',(-25.3031624035225,78.63948693439,85.5838769037982));
#213942=CARTESIAN_POINT('Ctrl Pts',(-25.2671492367615,76.9661123482892,
85.9509106010206));
#213943=CARTESIAN_POINT('Ctrl Pts',(-25.2110937833321,74.4788017793984,
86.0024934260275));
#213944=CARTESIAN_POINT('Ctrl Pts',(-25.1932702125315,73.6882045327406,
85.9466959719249));
#213945=CARTESIAN_POINT('Ctrl Pts',(-25.1573545097553,72.0826904798649,
85.6848678052996));
#213946=CARTESIAN_POINT('Ctrl Pts',(-25.1393881007222,71.272686857849,85.4711042328599));
#213947=CARTESIAN_POINT('Ctrl Pts',(-25.1114105692349,70.0945458901189,
85.0351860135718));
#213948=CARTESIAN_POINT('Ctrl Pts',(-25.1019084706643,69.7075720149055,
84.8702591362608));
#213949=CARTESIAN_POINT('Ctrl Pts',(-25.0541466985092,67.8019242994457,
83.9464752146266));
#213950=CARTESIAN_POINT('Ctrl Pts',(-25.0181261672443,66.4342651665973,
82.9140686343922));
#213951=CARTESIAN_POINT('Ctrl Pts',(-24.9617637202306,64.7681195006503,
81.0483612746353));
#213952=CARTESIAN_POINT('Ctrl Pts',(-24.9436507628794,64.2893456262384,
80.4002570731414));
#213953=CARTESIAN_POINT('Ctrl Pts',(-24.9079838183038,63.4533687006,79.0167666311959));
#213954=CARTESIAN_POINT('Ctrl Pts',(-24.8905073373037,63.0993246365807,
78.2835953282246));
#213955=CARTESIAN_POINT('Ctrl Pts',(-24.8630645895267,62.6693559715836,
77.1279872899257));
#213956=CARTESIAN_POINT('Ctrl Pts',(-24.8535596220526,62.5419006961698,
76.7268933833944));
#213957=CARTESIAN_POINT('Ctrl Pts',(-24.8058503480044,61.9998300936705,
74.6822528929047));
#213958=CARTESIAN_POINT('Ctrl Pts',(-24.7698813216614,61.8900144000392,
72.9749547962966));
#213959=CARTESIAN_POINT('Ctrl Pts',(-24.7143843430214,62.2110645219798,
70.5324051813204));
#213960=CARTESIAN_POINT('Ctrl Pts',(-24.6970419222636,62.3787014145589,
69.7804588734101));
#213961=CARTESIAN_POINT('Ctrl Pts',(-24.6632901642082,62.8415470111348,
68.3255961552879));
#213962=CARTESIAN_POINT('Ctrl Pts',(-24.6469281069572,63.1339929094341,
67.6249218798871));
#213963=CARTESIAN_POINT('Ctrl Pts',(-24.6085627568924,63.9405482866857,
66.0861333089842));
#213964=CARTESIAN_POINT('Ctrl Pts',(-24.5861603841818,64.4918984265292,
65.2727174091015));
#213965=CARTESIAN_POINT('Ctrl Pts',(-24.5478929218032,65.6118513645777,
63.9660075581907));
#213966=CARTESIAN_POINT('Ctrl Pts',(-24.5317890202232,66.1416283591875,
63.4453584440137));
#213967=CARTESIAN_POINT('Ctrl Pts',(-24.478678041785,68.0084483911288,61.9008022575695));
#213968=CARTESIAN_POINT('Ctrl Pts',(-24.4404197776328,69.4997497811424,
61.0903726254267));
#213969=CARTESIAN_POINT('Ctrl Pts',(-24.3944539989604,71.5059127553458,
60.4601679353283));
#213970=CARTESIAN_POINT('Ctrl Pts',(-24.3852625240197,71.9137615352939,
60.3535169796907));
#213971=CARTESIAN_POINT('Ctrl Pts',(-24.3589735379831,73.0715263622877,
60.1101762674291));
#213972=CARTESIAN_POINT('Ctrl Pts',(-24.3416198348962,73.829319278862,60.0193181026902));
#213973=CARTESIAN_POINT('Ctrl Pts',(-24.3153476699086,75.0034597100019,
59.9823322175879));
#213974=CARTESIAN_POINT('Ctrl Pts',(-24.3062012240956,75.4166079409204,
59.9890054637244));
#213975=CARTESIAN_POINT('Ctrl Pts',(-24.2791962632356,76.6425985097674,
60.0673205172565));
#213976=CARTESIAN_POINT('Ctrl Pts',(-24.2616122208314,77.4497550355971,
60.1957750471302));
#213977=CARTESIAN_POINT('Ctrl Pts',(-24.2174452577425,79.358630216496,60.6869544139071));
#213978=CARTESIAN_POINT('Ctrl Pts',(-24.1913574606352,80.4343690257702,
61.1228465529736));
#213979=CARTESIAN_POINT('Ctrl Pts',(-24.1481030157837,82.1490683603878,
62.1003517955465));
#213980=CARTESIAN_POINT('Ctrl Pts',(-24.1303270077378,82.8200217247972,
62.5717550113872));
#213981=CARTESIAN_POINT('Ctrl Pts',(-24.0934607218744,84.0657367716937,
63.6355618776563));
#213982=CARTESIAN_POINT('Ctrl Pts',(-24.0749439293719,84.6374991871952,
64.2258447186507));
#213983=CARTESIAN_POINT('Ctrl Pts',(-24.0399256256361,85.6278339792556,
65.4633093765027));
#213984=CARTESIAN_POINT('Ctrl Pts',(-24.0234209550587,86.052170387339,66.1016021099573));
#213985=CARTESIAN_POINT('Ctrl Pts',(-23.986480861679,86.8507665052518,67.5686511770748));
#213986=CARTESIAN_POINT('Ctrl Pts',(-23.9657965863791,87.1993699844182,
68.4068572517046));
#213987=CARTESIAN_POINT('Ctrl Pts',(-23.9286751730297,87.6752780539253,
70.0030333534241));
#213988=CARTESIAN_POINT('Ctrl Pts',(-23.9121337744981,87.8281748594039,
70.7492595749639));
#213989=CARTESIAN_POINT('Ctrl Pts',(-23.8584168754291,88.1082626488629,
73.18626923684));
#213990=CARTESIAN_POINT('Ctrl Pts',(-23.8198811582619,87.9712232475782,
74.8896421088131));
#213991=CARTESIAN_POINT('Ctrl Pts',(-23.7736771942424,87.3973357905358,
76.9237439180041));
#213992=CARTESIAN_POINT('Ctrl Pts',(-23.7645045072649,87.2635037493548,
77.3228814710253));
#213993=CARTESIAN_POINT('Ctrl Pts',(-23.7532764802347,87.0794545224418,
77.7945212352546));
#213994=CARTESIAN_POINT('Ctrl Pts',(-23.7513724844872,87.0475741404218,
77.8738940340539));
#213995=CARTESIAN_POINT('Ctrl Pts',(-23.7494631142981,87.0149197165734,
77.952930502878));
#213996=CARTESIAN_POINT('',(-23.5675316904177,87.9904527821819,72.490756361305));
#213997=CARTESIAN_POINT('Origin',(-23.5675316903009,75.,72.9888893865801));
#213998=CARTESIAN_POINT('',(-23.5676924422401,87.9901782351292,72.4836474449556));
#213999=CARTESIAN_POINT('Ctrl Pts',(-23.5675316904177,87.9904527821819,
72.490756361305));
#214000=CARTESIAN_POINT('Ctrl Pts',(-23.5675873235413,87.9904177973111,
72.4883921330275));
#214001=CARTESIAN_POINT('Ctrl Pts',(-23.5676429566649,87.9903821670158,
72.4860278991294));
#214002=CARTESIAN_POINT('Ctrl Pts',(-23.5676985897885,87.9903458912847,
72.483663659963));
#214003=CARTESIAN_POINT('',(-24.3504740810588,62.9850814687467,68.0248454013454));
#214004=CARTESIAN_POINT('Ctrl Pts',(-23.5676924422401,87.9901782351292,
72.4836474449556));
#214005=CARTESIAN_POINT('Ctrl Pts',(-23.579866516381,87.9692398735109,71.9453052627941));
#214006=CARTESIAN_POINT('Ctrl Pts',(-23.5921363130451,87.9148563762113,
71.4087819670215));
#214007=CARTESIAN_POINT('Ctrl Pts',(-23.6163677338714,87.7397953767718,
70.3453912998746));
#214008=CARTESIAN_POINT('Ctrl Pts',(-23.6283050919863,87.6192627227127,
69.8195543991763));
#214009=CARTESIAN_POINT('Ctrl Pts',(-23.6548809171444,87.274925491956,68.6550241764215));
#214010=CARTESIAN_POINT('Ctrl Pts',(-23.6693811451346,87.0332275773113,
68.023246912331));
#214011=CARTESIAN_POINT('Ctrl Pts',(-23.7137157498716,86.1721125160913,
66.2095881368177));
#214012=CARTESIAN_POINT('Ctrl Pts',(-23.7444931511871,85.4190515220121,
65.1010209222251));
#214013=CARTESIAN_POINT('Ctrl Pts',(-23.7829206451029,84.224537357421,63.8191474354379));
#214014=CARTESIAN_POINT('Ctrl Pts',(-23.792027110996,83.9236127931091,63.5260466635811));
#214015=CARTESIAN_POINT('Ctrl Pts',(-23.8386873210016,82.3161449889425,
62.10535751495));
#214016=CARTESIAN_POINT('Ctrl Pts',(-23.8784725722724,80.8086174661391,
61.231457189744));
#214017=CARTESIAN_POINT('Ctrl Pts',(-23.9304375078449,78.5567988600886,
60.467921189179));
#214018=CARTESIAN_POINT('Ctrl Pts',(-23.944451268879,77.9241855151621,60.3052546592794));
#214019=CARTESIAN_POINT('Ctrl Pts',(-23.9734151603134,76.6342131999977,
60.0752384248521));
#214020=CARTESIAN_POINT('Ctrl Pts',(-23.9884516930088,75.9785489184828,
60.0090797283746));
#214021=CARTESIAN_POINT('Ctrl Pts',(-24.0419614354671,73.6141729955495,
59.9507329783205));
#214022=CARTESIAN_POINT('Ctrl Pts',(-24.077636442192,71.9159497188868,60.2451583872028));
#214023=CARTESIAN_POINT('Ctrl Pts',(-24.133518316589,69.6097364794835,61.1343653793949));
#214024=CARTESIAN_POINT('Ctrl Pts',(-24.1509196237138,68.9219381508364,
61.4718643510489));
#214025=CARTESIAN_POINT('Ctrl Pts',(-24.1919754352576,67.3408833122785,
62.4289671184786));
#214026=CARTESIAN_POINT('Ctrl Pts',(-24.2148896691121,66.4877584805762,
63.1037622587486));
#214027=CARTESIAN_POINT('Ctrl Pts',(-24.2533759923444,65.2787446307964,
64.3339212689603));
#214028=CARTESIAN_POINT('Ctrl Pts',(-24.2680418990405,64.8636792060789,
64.8239471120891));
#214029=CARTESIAN_POINT('Ctrl Pts',(-24.2940935767858,64.1847342464081,
65.7574852536576));
#214030=CARTESIAN_POINT('Ctrl Pts',(-24.3055351499497,63.9078155261211,
66.1898725772495));
#214031=CARTESIAN_POINT('Ctrl Pts',(-24.3281398473403,63.4058937918095,
67.0862442270404));
#214032=CARTESIAN_POINT('Ctrl Pts',(-24.3392828333262,63.1814723764496,
67.5495029661559));
#214033=CARTESIAN_POINT('Ctrl Pts',(-24.3504740810588,62.9850814687467,
68.0248454013453));
#214034=CARTESIAN_POINT('Ctrl Pts',(-25.2581222247367,87.0149197055719,
77.9529305295058));
#214035=CARTESIAN_POINT('Ctrl Pts',(-25.2371139398987,86.6552691734239,
78.8234253826726));
#214036=CARTESIAN_POINT('Ctrl Pts',(-25.21540963982,86.2018081844466,79.6529161935503));
#214037=CARTESIAN_POINT('Ctrl Pts',(-25.1819196289472,85.3392991491601,
80.8893513410912));
#214038=CARTESIAN_POINT('Ctrl Pts',(-25.169745613827,84.9866696364086,81.3306425359654));
#214039=CARTESIAN_POINT('Ctrl Pts',(-25.1201329901855,83.4509550568779,
83.0149971163702));
#214040=CARTESIAN_POINT('Ctrl Pts',(-25.0805800079591,82.0559752886199,
84.0412504737423));
#214041=CARTESIAN_POINT('Ctrl Pts',(-25.0292609529725,79.9279759288953,
85.0353238638776));
#214042=CARTESIAN_POINT('Ctrl Pts',(-25.0156013108458,79.3350240530373,
85.2611792863697));
#214043=CARTESIAN_POINT('Ctrl Pts',(-24.9750095399314,77.5673393760012,
85.7903165773942));
#214044=CARTESIAN_POINT('Ctrl Pts',(-24.9470863164354,76.3638564276923,
85.9737863082347));
#214045=CARTESIAN_POINT('Ctrl Pts',(-24.9074472810324,74.5784121188101,
85.9947286348465));
#214046=CARTESIAN_POINT('Ctrl Pts',(-24.8950686465802,74.0045315539647,
85.9634276728041));
#214047=CARTESIAN_POINT('Ctrl Pts',(-24.8452804596057,71.7345459005824,
85.6880829545065));
#214048=CARTESIAN_POINT('Ctrl Pts',(-24.8057674949643,70.0918887737977,
85.1479662710231));
#214049=CARTESIAN_POINT('Ctrl Pts',(-24.7535182297264,68.0089873638452,
83.9701726821653));
#214050=CARTESIAN_POINT('Ctrl Pts',(-24.7388535665513,67.4439846541188,
83.5893363030982));
#214051=CARTESIAN_POINT('Ctrl Pts',(-24.698671883696,66.0184478844832,82.4563454180001));
#214052=CARTESIAN_POINT('Ctrl Pts',(-24.6723892453867,65.2228080106428,
81.6322347885949));
#214053=CARTESIAN_POINT('Ctrl Pts',(-24.6343728549527,64.2061403484082,
80.256461050092));
#214054=CARTESIAN_POINT('Ctrl Pts',(-24.6220757074902,63.8978517413121,
79.7761802700339));
#214055=CARTESIAN_POINT('Ctrl Pts',(-24.5723410170108,62.7926248175406,
77.7764145957868));
#214056=CARTESIAN_POINT('Ctrl Pts',(-24.5327923771568,62.2682504897212,
76.1262380636946));
#214057=CARTESIAN_POINT('Ctrl Pts',(-24.4727154955514,61.9651282535958,
73.3931830852563));
#214058=CARTESIAN_POINT('Ctrl Pts',(-24.450423176884,61.9742992358757,72.3544900136934));
#214059=CARTESIAN_POINT('Ctrl Pts',(-24.4014705356543,62.2527429291364,
70.1930457335824));
#214060=CARTESIAN_POINT('Ctrl Pts',(-24.3753730910726,62.5481383061654,
69.0824179202065));
#214061=CARTESIAN_POINT('Ctrl Pts',(-24.3504740810588,62.9850814687467,
68.0248454013453));
#214062=CARTESIAN_POINT('Origin',(-21.6548258024609,75.,72.9888893865801));
#214063=CARTESIAN_POINT('',(-27.3772428998516,87.0149197057112,77.9529305291688));
#214064=CARTESIAN_POINT('',(-27.071820154481,87.0149197055719,77.9529305295058));
#214065=CARTESIAN_POINT('',(-21.6548258024609,87.0149197055719,77.9529305295058));
#214066=CARTESIAN_POINT('',(-25.7929126252424,86.9560726709681,67.8848479330955));
#214067=CARTESIAN_POINT('Ctrl Pts',(-27.3772428998516,87.0149197058504,
77.9529305288318));
#214068=CARTESIAN_POINT('Ctrl Pts',(-27.3585026366247,86.6920930370044,
78.7342972407386));
#214069=CARTESIAN_POINT('Ctrl Pts',(-27.3400433155629,86.2938005397031,
79.4823430155439));
#214070=CARTESIAN_POINT('Ctrl Pts',(-27.3118499074165,85.5953734961236,
80.5328339483534));
#214071=CARTESIAN_POINT('Ctrl Pts',(-27.3025307943751,85.348569085002,80.8679856481114));
#214072=CARTESIAN_POINT('Ctrl Pts',(-27.274613720519,84.5582100824996,81.839921252302));
#214073=CARTESIAN_POINT('Ctrl Pts',(-27.2563294776812,83.9688536705665,
82.4366299088375));
#214074=CARTESIAN_POINT('Ctrl Pts',(-27.2185818420799,82.66146632564,83.5269761458286));
#214075=CARTESIAN_POINT('Ctrl Pts',(-27.1990975050948,81.9429570105276,
84.01362043297));
#214076=CARTESIAN_POINT('Ctrl Pts',(-27.1608686233789,80.4246186178578,
84.8342939279908));
#214077=CARTESIAN_POINT('Ctrl Pts',(-27.1420577344777,79.629070187145,85.1672227095795));
#214078=CARTESIAN_POINT('Ctrl Pts',(-27.1134541677068,78.4061460599412,
85.5417166702577));
#214079=CARTESIAN_POINT('Ctrl Pts',(-27.1040817102919,78.0001138129745,
85.6449006902839));
#214080=CARTESIAN_POINT('Ctrl Pts',(-27.0756316214871,76.7475906674452,
85.899527575069));
#214081=CARTESIAN_POINT('Ctrl Pts',(-27.0568990797288,75.8904665626252,
85.9868013423841));
#214082=CARTESIAN_POINT('Ctrl Pts',(-27.0176781623146,74.127690109845,85.9910081379894));
#214083=CARTESIAN_POINT('Ctrl Pts',(-26.9974077424435,73.2265835598246,
85.8990029018832));
#214084=CARTESIAN_POINT('Ctrl Pts',(-26.968250549752,71.9348259340739,85.6292215760866));
#214085=CARTESIAN_POINT('Ctrl Pts',(-26.9591046860196,71.5316602483832,
85.5245947390282));
#214086=CARTESIAN_POINT('Ctrl Pts',(-26.9349401815241,70.488075109287,85.199561969259));
#214087=CARTESIAN_POINT('Ctrl Pts',(-26.9197323165762,69.8586419172962,
84.9481711651819));
#214088=CARTESIAN_POINT('Ctrl Pts',(-26.8859122844744,68.498424915887,84.2775901023272));
#214089=CARTESIAN_POINT('Ctrl Pts',(-26.8675404929102,67.7829525778628,
83.834140109348));
#214090=CARTESIAN_POINT('Ctrl Pts',(-26.8299101986688,66.4320387623489,
82.8035971260288));
#214091=CARTESIAN_POINT('Ctrl Pts',(-26.8105585703119,65.8021719605181,
82.2159370712263));
#214092=CARTESIAN_POINT('Ctrl Pts',(-26.7724324749667,64.6668976818974,
80.9240898258221));
#214093=CARTESIAN_POINT('Ctrl Pts',(-26.7536453108212,64.1644601915041,
80.2229397836913));
#214094=CARTESIAN_POINT('Ctrl Pts',(-26.7250956737158,63.5270109069143,
79.1162186341038));
#214095=CARTESIAN_POINT('Ctrl Pts',(-26.715761955723,63.3365114880958,78.7453361357191));
#214096=CARTESIAN_POINT('Ctrl Pts',(-26.6878646566231,62.8185801602425,
77.605278466486));
#214097=CARTESIAN_POINT('Ctrl Pts',(-26.6696154374097,62.5471417669723,
76.8130691020841));
#214098=CARTESIAN_POINT('Ctrl Pts',(-26.6329190489758,62.1639564653197,
75.2038925083435));
#214099=CARTESIAN_POINT('Ctrl Pts',(-26.6144941074024,62.049964964534,74.3913345736975));
#214100=CARTESIAN_POINT('Ctrl Pts',(-26.5772663572282,61.9744567925888,
72.7138662237188));
#214101=CARTESIAN_POINT('Ctrl Pts',(-26.5584809883254,62.0212044236113,
71.852545420024));
#214102=CARTESIAN_POINT('Ctrl Pts',(-26.5299362395003,62.2163619130141,
70.5905354922137));
#214103=CARTESIAN_POINT('Ctrl Pts',(-26.5206058473888,62.2997667635459,
70.1821865398606));
#214104=CARTESIAN_POINT('Ctrl Pts',(-26.4927037374686,62.6090275943298,
68.9686480648817));
#214105=CARTESIAN_POINT('Ctrl Pts',(-26.4744462598849,62.8930467479042,
68.1805412489976));
#214106=CARTESIAN_POINT('Ctrl Pts',(-26.4375071524084,63.6057605027665,
66.6754580572646));
#214107=CARTESIAN_POINT('Ctrl Pts',(-26.4188376326829,64.0317228180229,
65.9614423333998));
#214108=CARTESIAN_POINT('Ctrl Pts',(-26.3813781293124,65.0321953444006,
64.5994160557959));
#214109=CARTESIAN_POINT('Ctrl Pts',(-26.3625868347542,65.6091804053644,
63.9582250617695));
#214110=CARTESIAN_POINT('Ctrl Pts',(-26.3340264446216,66.553586253858,63.0978810349136));
#214111=CARTESIAN_POINT('Ctrl Pts',(-26.3246853485288,66.8752439694295,
62.8320054219483));
#214112=CARTESIAN_POINT('Ctrl Pts',(-26.2967994471399,67.8773984430049,
62.0817619822098));
#214113=CARTESIAN_POINT('Ctrl Pts',(-26.2785692142129,68.5923066241011,
61.6470051727518));
#214114=CARTESIAN_POINT('Ctrl Pts',(-26.2424224009397,70.0590097150615,
60.9382741883589));
#214115=CARTESIAN_POINT('Ctrl Pts',(-26.2245511524584,70.8042374504039,
60.6589950005373));
#214116=CARTESIAN_POINT('Ctrl Pts',(-26.1897733046434,72.3165714552708,
60.2453486461837));
#214117=CARTESIAN_POINT('Ctrl Pts',(-26.1728928390523,73.0795965666424,
60.1082578434061));
#214118=CARTESIAN_POINT('Ctrl Pts',(-26.1429023266542,74.4197179295013,
59.9892701169044));
#214119=CARTESIAN_POINT('Ctrl Pts',(-26.1300716403104,74.9918828037437,
59.9763275579365));
#214120=CARTESIAN_POINT('Ctrl Pts',(-26.0982220008237,76.4218187852646,
60.0383171234002));
#214121=CARTESIAN_POINT('Ctrl Pts',(-26.0794903366003,77.2747899921236,
60.1606308648086));
#214122=CARTESIAN_POINT('Ctrl Pts',(-26.0392642115874,79.0293957409234,
60.5928547252689));
#214123=CARTESIAN_POINT('Ctrl Pts',(-26.0180298275783,79.9218450641421,
60.9193753076888));
#214124=CARTESIAN_POINT('Ctrl Pts',(-25.9887478158431,81.1105915754084,
61.5082789939621));
#214125=CARTESIAN_POINT('Ctrl Pts',(-25.980414557455,81.4427986662038,61.6913635913145));
#214126=CARTESIAN_POINT('Ctrl Pts',(-25.9453511555322,82.7962653180951,
62.5164191486459));
#214127=CARTESIAN_POINT('Ctrl Pts',(-25.9182823831953,83.7336670457999,
63.2843824439299));
#214128=CARTESIAN_POINT('Ctrl Pts',(-25.8835582823454,84.802145820081,64.4417136345005));
#214129=CARTESIAN_POINT('Ctrl Pts',(-25.8754354658025,85.0408914382205,
64.7234931914111));
#214130=CARTESIAN_POINT('Ctrl Pts',(-25.8424562339689,85.9509334591754,
65.8952865936117));
#214131=CARTESIAN_POINT('Ctrl Pts',(-25.8175223603503,86.518524818664,66.859797753857));
#214132=CARTESIAN_POINT('Ctrl Pts',(-25.7929565710457,86.9561115222891,
67.8848324446381));
#214133=CARTESIAN_POINT('Ctrl Pts',(-25.7925315892805,86.9561078343949,
67.8848238058573));
#214134=CARTESIAN_POINT('Ctrl Pts',(-25.7738172320668,87.2899529717186,
68.6668451961985));
#214135=CARTESIAN_POINT('Ctrl Pts',(-25.7554910654485,87.5462664477491,
69.479728285654));
#214136=CARTESIAN_POINT('Ctrl Pts',(-25.7174585685915,87.89551651574,71.1393471814782));
#214137=CARTESIAN_POINT('Ctrl Pts',(-25.6982654760428,87.9885017447245,
71.9819134464591));
#214138=CARTESIAN_POINT('Ctrl Pts',(-25.6580815311063,88.0110086692369,
73.7950592766131));
#214139=CARTESIAN_POINT('Ctrl Pts',(-25.6373707278172,87.9149608356701,
74.760904048186));
#214140=CARTESIAN_POINT('Ctrl Pts',(-25.6073298168375,87.6337185281454,
76.0762223461118));
#214141=CARTESIAN_POINT('Ctrl Pts',(-25.5988027409164,87.5387580880639,
76.4417162546927));
#214142=CARTESIAN_POINT('Ctrl Pts',(-25.5810816491095,87.3082309444352,
77.1929608534129));
#214143=CARTESIAN_POINT('Ctrl Pts',(-25.5719178118877,87.1703147103061,
77.576813883658));
#214144=CARTESIAN_POINT('Ctrl Pts',(-25.5628518781596,87.0149197055719,
77.9529305295058));
#214145=CARTESIAN_POINT('Ctrl Pts',(-27.071820154481,87.0149197055719,77.9529305295058));
#214146=CARTESIAN_POINT('Ctrl Pts',(-27.0605085365974,86.8166613733047,
78.4327931806334));
#214147=CARTESIAN_POINT('Ctrl Pts',(-27.049101654611,86.5896253620448,78.9008516142056));
#214148=CARTESIAN_POINT('Ctrl Pts',(-27.0197225666822,85.9448502140688,
80.0489617246627));
#214149=CARTESIAN_POINT('Ctrl Pts',(-27.0015063043549,85.4918565712577,
80.70609693059));
#214150=CARTESIAN_POINT('Ctrl Pts',(-26.9591716635365,84.2850054963717,
82.1524488952687));
#214151=CARTESIAN_POINT('Ctrl Pts',(-26.9361717726357,83.4864499048139,
82.8965790426729));
#214152=CARTESIAN_POINT('Ctrl Pts',(-26.8941455410223,81.9446283737061,
84.0086132753054));
#214153=CARTESIAN_POINT('Ctrl Pts',(-26.8756807836608,81.2414038974203,
84.421606780749));
#214154=CARTESIAN_POINT('Ctrl Pts',(-26.8189728420717,78.9721657266138,
85.4821578977096));
#214155=CARTESIAN_POINT('Ctrl Pts',(-26.7836305989519,77.3150352142353,
85.8923958059138));
#214156=CARTESIAN_POINT('Ctrl Pts',(-26.7312779156254,74.9997905288434,
86.0039922207733));
#214157=CARTESIAN_POINT('Ctrl Pts',(-26.7169492121584,74.372336987336,85.9888485981267));
#214158=CARTESIAN_POINT('Ctrl Pts',(-26.6742994714576,72.4684258750948,
85.8046950112485));
#214159=CARTESIAN_POINT('Ctrl Pts',(-26.6471833125259,71.2138486459522,
85.4916438799536));
#214160=CARTESIAN_POINT('Ctrl Pts',(-26.6020301406656,69.3559903103541,
84.7222014240607));
#214161=CARTESIAN_POINT('Ctrl Pts',(-26.5854317064412,68.7106481624918,
84.3893060366484));
#214162=CARTESIAN_POINT('Ctrl Pts',(-26.5450219175929,67.181239395849,83.4308014465017));
#214163=CARTESIAN_POINT('Ctrl Pts',(-26.5221896305854,66.3410918902448,
82.7454188415464));
#214164=CARTESIAN_POINT('Ctrl Pts',(-26.4780446581086,64.9659409652747,
81.3044741245955));
#214165=CARTESIAN_POINT('Ctrl Pts',(-26.4572014080688,64.4076145893941,
80.5805045840409));
#214166=CARTESIAN_POINT('Ctrl Pts',(-26.4036318027753,63.1590546347934,
78.5523955573464));
#214167=CARTESIAN_POINT('Ctrl Pts',(-26.3728346457708,62.6063171379071,
77.17902371207));
#214168=CARTESIAN_POINT('Ctrl Pts',(-26.3244976064021,62.1517516696246,
75.0816632598761));
#214169=CARTESIAN_POINT('Ctrl Pts',(-26.3090236792136,62.0603060695958,
74.410685161115));
#214170=CARTESIAN_POINT('Ctrl Pts',(-26.2641235956774,61.9448936273482,
72.4048400651594));
#214171=CARTESIAN_POINT('Ctrl Pts',(-26.2360680888913,62.0734620859508,
71.0701429440428));
#214172=CARTESIAN_POINT('Ctrl Pts',(-26.1966699289764,62.5063482147525,
69.3715812671164));
#214173=CARTESIAN_POINT('Ctrl Pts',(-26.1871415785778,62.629674256928,68.9700224075527));
#214174=CARTESIAN_POINT('Ctrl Pts',(-26.1506331525675,63.1764235758087,
67.4553166575137));
#214175=CARTESIAN_POINT('Ctrl Pts',(-26.1251170344048,63.7325528158873,
66.3963153232645));
#214176=CARTESIAN_POINT('Ctrl Pts',(-26.0806649581723,64.9095364125484,
64.7501647278864));
#214177=CARTESIAN_POINT('Ctrl Pts',(-26.061906909934,65.4580950871485,64.1206280522381));
#214178=CARTESIAN_POINT('Ctrl Pts',(-26.015547404288,66.9426901021429,62.7152958770042));
#214179=CARTESIAN_POINT('Ctrl Pts',(-25.9895183092078,67.9343472290684,
62.0096573409437));
#214180=CARTESIAN_POINT('Ctrl Pts',(-25.9446017362212,69.7502091534502,
61.0667794261834));
#214181=CARTESIAN_POINT('Ctrl Pts',(-25.9258205977896,70.5264831300893,
60.7543225527409));
#214182=CARTESIAN_POINT('Ctrl Pts',(-25.8792531495497,72.4961488897322,
60.1742348887389));
#214183=CARTESIAN_POINT('Ctrl Pts',(-25.8530429820679,73.7075859543001,
59.9960325963783));
#214184=CARTESIAN_POINT('Ctrl Pts',(-25.7978641992108,76.221579111487,59.9817283532551));
#214185=CARTESIAN_POINT('Ctrl Pts',(-25.7679576827334,77.5109436766013,
60.1680641200787));
#214186=CARTESIAN_POINT('Ctrl Pts',(-25.7252345790019,79.3600452531562,
60.7253599424855));
#214187=CARTESIAN_POINT('Ctrl Pts',(-25.7115677709115,79.9544559836962,
60.9532121514447));
#214188=CARTESIAN_POINT('Ctrl Pts',(-25.6608585552852,82.0562660521998,
61.941087947732));
#214189=CARTESIAN_POINT('Ctrl Pts',(-25.6219008261527,83.4285950314223,
62.9487898664131));
#214190=CARTESIAN_POINT('Ctrl Pts',(-25.5674029111453,85.122148925319,64.790880633502));
#214191=CARTESIAN_POINT('Ctrl Pts',(-25.5497603779432,85.6164336888591,
65.4419311246971));
#214192=CARTESIAN_POINT('Ctrl Pts',(-25.5071780938393,86.6226461392791,
67.0636464884068));
#214193=CARTESIAN_POINT('Ctrl Pts',(-25.4819488655756,87.0794462568247,
68.06127024736));
#214194=CARTESIAN_POINT('Ctrl Pts',(-25.4375428607714,87.6846242953266,
69.9939712119277));
#214195=CARTESIAN_POINT('Ctrl Pts',(-25.4175628093938,87.866700763943,70.911088538553));
#214196=CARTESIAN_POINT('Ctrl Pts',(-25.3726675196419,88.0448682000109,
72.9188124382479));
#214197=CARTESIAN_POINT('Ctrl Pts',(-25.3476385525466,88.0053767103916,
74.005599745462));
#214198=CARTESIAN_POINT('Ctrl Pts',(-25.3071797422961,87.710143730812,75.821687234242));
#214199=CARTESIAN_POINT('Ctrl Pts',(-25.2909561985655,87.5237651081034,
76.5564960547168));
#214200=CARTESIAN_POINT('Ctrl Pts',(-25.2689347587987,87.1943353664899,
77.5008148016953));
#214201=CARTESIAN_POINT('Ctrl Pts',(-25.2635448812528,87.1077526672685,
77.7282384794804));
#214202=CARTESIAN_POINT('Ctrl Pts',(-25.2581222247367,87.0149197055719,
77.9529305295058));
#214203=CARTESIAN_POINT('Origin',(-21.6548258024609,75.,72.9888893865801));
#214204=CARTESIAN_POINT('',(-29.191473624437,87.0149197052612,77.9529305302578));
#214205=CARTESIAN_POINT('',(-28.8854250924613,87.0149197055719,77.9529305295058));
#214206=CARTESIAN_POINT('',(-21.6548258024609,87.0149197055719,77.9529305295058));
#214207=CARTESIAN_POINT('Ctrl Pts',(-29.191473624437,87.0149197049505,77.9529305310098));
#214208=CARTESIAN_POINT('Ctrl Pts',(-29.1748720876648,86.7289553381427,
78.6450760643983));
#214209=CARTESIAN_POINT('Ctrl Pts',(-29.1580149809245,86.3837020063489,
79.3112532791676));
#214210=CARTESIAN_POINT('Ctrl Pts',(-29.124299147414,85.571916627344,80.5931613503198));
#214211=CARTESIAN_POINT('Ctrl Pts',(-29.1075265747482,85.1040975117078,
81.2045804644005));
#214212=CARTESIAN_POINT('Ctrl Pts',(-29.0719165439695,84.0216019566031,
82.3860326371831));
#214213=CARTESIAN_POINT('Ctrl Pts',(-29.0531686040573,83.400296735343,82.9453261314133));
#214214=CARTESIAN_POINT('Ctrl Pts',(-29.0254578252239,82.3940610068601,
83.6894563361449));
#214215=CARTESIAN_POINT('Ctrl Pts',(-29.0162756596396,82.0466521866939,
83.9213623179776));
#214216=CARTESIAN_POINT('Ctrl Pts',(-28.9880846702559,80.9508731496388,
84.5788624319063));
#214217=CARTESIAN_POINT('Ctrl Pts',(-28.968753497635,80.1709259228678,84.9472287683825));
#214218=CARTESIAN_POINT('Ctrl Pts',(-28.9321198753148,78.6199709504613,
85.4994218773942));
#214219=CARTESIAN_POINT('Ctrl Pts',(-28.9149486411076,77.8572365707559,
85.6953367527481));
#214220=CARTESIAN_POINT('Ctrl Pts',(-28.8804006429214,76.319908017302,85.9447035848871));
#214221=CARTESIAN_POINT('Ctrl Pts',(-28.8630365366872,75.5488317126422,
86.000194742609));
#214222=CARTESIAN_POINT('Ctrl Pts',(-28.8299316869188,74.0577519012817,
85.974658983903));
#214223=CARTESIAN_POINT('Ctrl Pts',(-28.8142064869176,73.3403740924139,
85.9025905663761));
#214224=CARTESIAN_POINT('Ctrl Pts',(-28.7822406653669,71.9251851481273,
85.640498115977));
#214225=CARTESIAN_POINT('Ctrl Pts',(-28.7660578641987,71.229805419051,85.450965044082));
#214226=CARTESIAN_POINT('Ctrl Pts',(-28.7329339171202,69.8286644159398,
84.9409847514264));
#214227=CARTESIAN_POINT('Ctrl Pts',(-28.7160965468475,69.1285756681097,
84.6130739307271));
#214228=CARTESIAN_POINT('Ctrl Pts',(-28.6814663693343,67.7825461534335,
83.8298215910126));
#214229=CARTESIAN_POINT('Ctrl Pts',(-28.6638066304726,67.1406086921955,
83.3738511520525));
#214230=CARTESIAN_POINT('Ctrl Pts',(-28.6273228458363,65.8902559677678,
82.3030143783936));
#214231=CARTESIAN_POINT('Ctrl Pts',(-28.6085271767135,65.2939104292582,
81.679814776386));
#214232=CARTESIAN_POINT('Ctrl Pts',(-28.5799560800039,64.5061977061064,
80.6735741452155));
#214233=CARTESIAN_POINT('Ctrl Pts',(-28.5706075320066,64.2648558037467,
80.3326586225553));
#214234=CARTESIAN_POINT('Ctrl Pts',(-28.5427341981161,63.5917536584481,
79.2775744658596));
#214235=CARTESIAN_POINT('Ctrl Pts',(-28.5245241146975,63.2118827786116,
78.5328886001411));
#214236=CARTESIAN_POINT('Ctrl Pts',(-28.4889453592806,62.6239769793031,
77.0416904741416));
#214237=CARTESIAN_POINT('Ctrl Pts',(-28.4716462600002,62.4059890416338,
76.3028051357496));
#214238=CARTESIAN_POINT('Ctrl Pts',(-28.4374968922271,62.1029596373628,
74.79418291339));
#214239=CARTESIAN_POINT('Ctrl Pts',(-28.4207003956739,62.0186962073909,
74.0273904754124));
#214240=CARTESIAN_POINT('Ctrl Pts',(-28.3812460335961,61.9820704138856,
72.2562631386752));
#214241=CARTESIAN_POINT('Ctrl Pts',(-28.3588390415407,62.0771648609283,
71.2558023076267));
#214242=CARTESIAN_POINT('Ctrl Pts',(-28.3275291901714,62.3734187427387,
69.8673081502499));
#214243=CARTESIAN_POINT('Ctrl Pts',(-28.3183412063837,62.4803432102327,
69.4628411396055));
#214244=CARTESIAN_POINT('Ctrl Pts',(-28.2923755504632,62.8330635637699,
68.3490075777341));
#214245=CARTESIAN_POINT('Ctrl Pts',(-28.2755070075871,63.1210447020856,
67.6547282024298));
#214246=CARTESIAN_POINT('Ctrl Pts',(-28.2417582543861,63.8229839058438,
66.3054550517388));
#214247=CARTESIAN_POINT('Ctrl Pts',(-28.2249441368782,64.2387725268455,
65.6547251696));
#214248=CARTESIAN_POINT('Ctrl Pts',(-28.1960445766112,65.0315160668254,
64.6278736278802));
#214249=CARTESIAN_POINT('Ctrl Pts',(-28.1842258494247,65.3783142874616,
64.231011675039));
#214250=CARTESIAN_POINT('Ctrl Pts',(-28.1538344070745,66.3362913012858,
63.2605346562643));
#214251=CARTESIAN_POINT('Ctrl Pts',(-28.1355402688503,66.9805262409467,
62.7229862544525));
#214252=CARTESIAN_POINT('Ctrl Pts',(-28.0974818801123,68.3984355273252,
61.7553264165708));
#214253=CARTESIAN_POINT('Ctrl Pts',(-28.077684353741,69.1733633480648,61.3345381023075));
#214254=CARTESIAN_POINT('Ctrl Pts',(-28.0391615851677,70.7783713925089,
60.6634003441353));
#214255=CARTESIAN_POINT('Ctrl Pts',(-28.0203440667548,71.6028949814444,
60.4111510069592));
#214256=CARTESIAN_POINT('Ctrl Pts',(-27.9917283516021,72.8573435161289,
60.1598290194321));
#214257=CARTESIAN_POINT('Ctrl Pts',(-27.9823455955259,73.2721645197844,
60.0974056651172));
#214258=CARTESIAN_POINT('Ctrl Pts',(-27.9538883157487,74.5444829827186,
59.9684671118984));
#214259=CARTESIAN_POINT('Ctrl Pts',(-27.9351567136414,75.4061785530909,
59.9668347644462));
#214260=CARTESIAN_POINT('Ctrl Pts',(-27.8949029168007,77.2059437756855,
60.1423383019933));
#214261=CARTESIAN_POINT('Ctrl Pts',(-27.8736417249549,78.1372751239506,
60.3375024609604));
#214262=CARTESIAN_POINT('Ctrl Pts',(-27.8435000938951,79.4352842125235,
60.761787114919));
#214263=CARTESIAN_POINT('Ctrl Pts',(-27.8343431385889,79.8250579186713,
60.9102888508809));
#214264=CARTESIAN_POINT('Ctrl Pts',(-27.806068651421,80.9944788766643,61.4214866700108));
#214265=CARTESIAN_POINT('Ctrl Pts',(-27.7867170866246,81.7458640588492,
61.8429527291791));
#214266=CARTESIAN_POINT('Ctrl Pts',(-27.7485971918739,83.1552834822207,
62.8285874493229));
#214267=CARTESIAN_POINT('Ctrl Pts',(-27.7298045572284,83.8097219140442,
63.3904946116153));
#214268=CARTESIAN_POINT('Ctrl Pts',(-27.7012408120807,84.691884529798,64.314707962388));
#214269=CARTESIAN_POINT('Ctrl Pts',(-27.6918973945536,84.9652449281237,
64.6301847203721));
#214270=CARTESIAN_POINT('Ctrl Pts',(-27.6640152773653,85.7385092525964,
65.6145471493112));
#214271=CARTESIAN_POINT('Ctrl Pts',(-27.6457912017925,86.1896591627655,
66.3189551409814));
#214272=CARTESIAN_POINT('Ctrl Pts',(-27.6098192685302,86.9287037331747,
67.7616130856516));
#214273=CARTESIAN_POINT('Ctrl Pts',(-27.5921241879336,87.2229985640537,
68.4925905055258));
#214274=CARTESIAN_POINT('Ctrl Pts',(-27.5575468408499,87.6717811724289,
69.9851787610371));
#214275=CARTESIAN_POINT('Ctrl Pts',(-27.5406994570977,87.8277990288113,
70.7430295666117));
#214276=CARTESIAN_POINT('Ctrl Pts',(-27.5112209523472,87.9782559482579,
72.0572259881749));
#214277=CARTESIAN_POINT('Ctrl Pts',(-27.4988633979556,88.0060670538526,
72.6076465536683));
#214278=CARTESIAN_POINT('Ctrl Pts',(-27.4674693610454,87.9877096261058,
74.0173047691573));
#214279=CARTESIAN_POINT('Ctrl Pts',(-27.4487334796038,87.8913750969979,
74.8732140521648));
#214280=CARTESIAN_POINT('Ctrl Pts',(-27.4125506948449,87.5502774816522,
76.4646545510302));
#214281=CARTESIAN_POINT('Ctrl Pts',(-27.3952778289842,87.3229510848624,
77.2002187729921));
#214282=CARTESIAN_POINT('Ctrl Pts',(-27.3779066749826,87.0263291301507,
77.9252475393518));
#214283=CARTESIAN_POINT('Ctrl Pts',(-27.3775747483253,87.020636249744,77.9390942583602));
#214284=CARTESIAN_POINT('Ctrl Pts',(-27.3772428998516,87.0149197058504,
77.9529305288318));
#214285=CARTESIAN_POINT('',(-27.3009674773552,86.9560726238069,67.8848561928421));
#214286=CARTESIAN_POINT('Ctrl Pts',(-27.3016104665866,86.9561198926212,
67.8848520519528));
#214287=CARTESIAN_POINT('Ctrl Pts',(-27.2822043885439,87.2951893562206,
68.6791164534333));
#214288=CARTESIAN_POINT('Ctrl Pts',(-27.2623604058397,87.5542721652542,
69.5051986871067));
#214289=CARTESIAN_POINT('Ctrl Pts',(-27.2247684056633,87.9002962357792,
71.1748980595603));
#214290=CARTESIAN_POINT('Ctrl Pts',(-27.2067907055177,87.9906504840547,
72.0135794964742));
#214291=CARTESIAN_POINT('Ctrl Pts',(-27.1756917368117,88.0051539398962,
73.4227565893461));
#214292=CARTESIAN_POINT('Ctrl Pts',(-27.1629591016859,87.9738071072631,
73.99018325198));
#214293=CARTESIAN_POINT('Ctrl Pts',(-27.1372090798418,87.8369700906062,
75.1186947614233));
#214294=CARTESIAN_POINT('Ctrl Pts',(-27.1242209102934,87.7314420438741,
75.6785468397757));
#214295=CARTESIAN_POINT('Ctrl Pts',(-27.0980726513746,87.4382792427217,
76.8174033129033));
#214296=CARTESIAN_POINT('Ctrl Pts',(-27.0850145273716,87.2461770192046,
77.3931974461928));
#214297=CARTESIAN_POINT('Ctrl Pts',(-27.071820154481,87.0149197055719,77.9529305295058));
#214298=CARTESIAN_POINT('Ctrl Pts',(-28.8854250924613,87.0149197055719,
77.9529305295058));
#214299=CARTESIAN_POINT('Ctrl Pts',(-28.8824657061371,86.9641248974214,
78.07587381781));
#214300=CARTESIAN_POINT('Ctrl Pts',(-28.8795002899751,86.9114288111352,
78.1980719467812));
#214301=CARTESIAN_POINT('Ctrl Pts',(-28.8672396720504,86.6861614970234,
78.6991345686103));
#214302=CARTESIAN_POINT('Ctrl Pts',(-28.85790713716,86.4973408615809,79.0703713766788));
#214303=CARTESIAN_POINT('Ctrl Pts',(-28.8331154639791,85.9467030888406,
80.0353338803234));
#214304=CARTESIAN_POINT('Ctrl Pts',(-28.8179195844283,85.5545514401051,
80.610184072988));
#214305=CARTESIAN_POINT('Ctrl Pts',(-28.7840038631501,84.5919001765483,
81.8035658259997));
#214306=CARTESIAN_POINT('Ctrl Pts',(-28.7651844263082,84.0035487921546,
82.4037267980327));
#214307=CARTESIAN_POINT('Ctrl Pts',(-28.7276150004718,82.7113055402472,
83.4892160188048));
#214308=CARTESIAN_POINT('Ctrl Pts',(-28.7091084160755,82.0091389010379,
83.9703769223539));
#214309=CARTESIAN_POINT('Ctrl Pts',(-28.6710757148091,80.5111363836892,
84.7943023480581));
#214310=CARTESIAN_POINT('Ctrl Pts',(-28.6517365479907,79.7178740929953,
85.1331091609983));
#214311=CARTESIAN_POINT('Ctrl Pts',(-28.6235540749995,78.4993036765176,
85.5160051569611));
#214312=CARTESIAN_POINT('Ctrl Pts',(-28.6143870150687,78.0958534094773,
85.6217610820052));
#214313=CARTESIAN_POINT('Ctrl Pts',(-28.5866706223603,76.8708386070266,
85.8806532998752));
#214314=CARTESIAN_POINT('Ctrl Pts',(-28.567902739722,76.038917234555,85.9741983900568));
#214315=CARTESIAN_POINT('Ctrl Pts',(-28.5313313335661,74.3942339589746,
85.9999846244162));
#214316=CARTESIAN_POINT('Ctrl Pts',(-28.5136689781962,73.5852537378235,
85.9370186488788));
#214317=CARTESIAN_POINT('Ctrl Pts',(-28.4765264015262,71.9394859923286,
85.6527617372223));
#214318=CARTESIAN_POINT('Ctrl Pts',(-28.4571790904682,71.1081997231846,
85.4224853881641));
#214319=CARTESIAN_POINT('Ctrl Pts',(-28.4290075316119,69.9177814281301,
84.9615319511398));
#214320=CARTESIAN_POINT('Ctrl Pts',(-28.4198590143517,69.5372190569592,
84.7927506157629));
#214321=CARTESIAN_POINT('Ctrl Pts',(-28.3921379113707,68.4178096980704,
84.2305375552029));
#214322=CARTESIAN_POINT('Ctrl Pts',(-28.3733480092101,67.7082051386715,
83.7837768461554));
#214323=CARTESIAN_POINT('Ctrl Pts',(-28.3356160482187,66.3665029863644,
82.746023955881));
#214324=CARTESIAN_POINT('Ctrl Pts',(-28.3168778777699,65.7403786425432,
82.1539515382366));
#214325=CARTESIAN_POINT('Ctrl Pts',(-28.2785889933486,64.6137354201889,
80.8543635225977));
#214326=CARTESIAN_POINT('Ctrl Pts',(-28.2592740996115,64.1160992638615,
80.1499571314905));
#214327=CARTESIAN_POINT('Ctrl Pts',(-28.2310705762345,63.485298007818,79.0375859269632));
#214328=CARTESIAN_POINT('Ctrl Pts',(-28.2218640006324,63.2965830577881,
78.6638451860493));
#214329=CARTESIAN_POINT('Ctrl Pts',(-28.1935575655176,62.7763359508144,
77.4967242676392));
#214330=CARTESIAN_POINT('Ctrl Pts',(-28.1742147305241,62.5051462879013,
76.6790331332835));
#214331=CARTESIAN_POINT('Ctrl Pts',(-28.13553707715,62.1225407789516,74.9773354996262));
#214332=CARTESIAN_POINT('Ctrl Pts',(-28.1162057659808,62.0170866958016,
74.0965199011238));
#214333=CARTESIAN_POINT('Ctrl Pts',(-28.078268587886,61.987921446801,72.3962011304826));
#214334=CARTESIAN_POINT('Ctrl Pts',(-28.0600134566556,62.0507353882327,
71.5810452228492));
#214335=CARTESIAN_POINT('Ctrl Pts',(-28.0236265245261,62.3315440089111,
69.9545773365316));
#214336=CARTESIAN_POINT('Ctrl Pts',(-28.0051829628842,62.5524646578503,
69.1475767222341));
#214337=CARTESIAN_POINT('Ctrl Pts',(-27.9771298133304,62.9982787259586,
67.9754591654159));
#214338=CARTESIAN_POINT('Ctrl Pts',(-27.9677390142899,63.1662066934128,
67.5910069257234));
#214339=CARTESIAN_POINT('Ctrl Pts',(-27.9370287574911,63.7818224627086,
66.349060825342));
#214340=CARTESIAN_POINT('Ctrl Pts',(-27.9158767653462,64.3065324424989,
65.533381975057));
#214341=CARTESIAN_POINT('Ctrl Pts',(-27.8849412670348,65.1801585010924,
64.4598336454975));
#214342=CARTESIAN_POINT('Ctrl Pts',(-27.8755848279818,65.4589341724681,
64.1490849776268));
#214343=CARTESIAN_POINT('Ctrl Pts',(-27.8473308132092,66.3516610491003,
63.2454906496998));
#214344=CARTESIAN_POINT('Ctrl Pts',(-27.8287354763865,67.0094212758992,
62.699173963006));
#214345=CARTESIAN_POINT('Ctrl Pts',(-27.790598345434,68.4285698429715,61.7391537518352));
#214346=CARTESIAN_POINT('Ctrl Pts',(-27.7712781789703,69.1873064754114,
61.3290072595462));
#214347=CARTESIAN_POINT('Ctrl Pts',(-27.7430781552989,70.3667123452662,
60.8353920205676));
#214348=CARTESIAN_POINT('Ctrl Pts',(-27.7338787555852,70.7600093741734,
60.6926569597947));
#214349=CARTESIAN_POINT('Ctrl Pts',(-27.7055841569337,71.9804540657243,
60.3152650493847));
#214350=CARTESIAN_POINT('Ctrl Pts',(-27.6862456860974,72.824555129948,60.1434294170083));
#214351=CARTESIAN_POINT('Ctrl Pts',(-27.6496231645155,74.4670898531631,
59.9757072121913));
#214352=CARTESIAN_POINT('Ctrl Pts',(-27.6323226821408,75.2604702770383,
59.9674045950463));
#214353=CARTESIAN_POINT('Ctrl Pts',(-27.5955515295513,76.9072526729874,
60.1008067118721));
#214354=CARTESIAN_POINT('Ctrl Pts',(-27.5762273817978,77.7558348782639,
60.2552460394781));
#214355=CARTESIAN_POINT('Ctrl Pts',(-27.5480309082657,78.9846379265348,
60.6075604536139));
#214356=CARTESIAN_POINT('Ctrl Pts',(-27.5388377802742,79.380570584004,60.7420429913732));
#214357=CARTESIAN_POINT('Ctrl Pts',(-27.5105536384159,80.5686610096575,
61.2105913528594));
#214358=CARTESIAN_POINT('Ctrl Pts',(-27.4912191807338,81.3347621600151,
61.6042915492844));
#214359=CARTESIAN_POINT('Ctrl Pts',(-27.4548946107977,82.7098171497384,
62.4929847277351));
#214360=CARTESIAN_POINT('Ctrl Pts',(-27.437895175373,83.3240090917863,62.9730931068896));
#214361=CARTESIAN_POINT('Ctrl Pts',(-27.4008866114246,84.5376412426188,
64.1109558996629));
#214362=CARTESIAN_POINT('Ctrl Pts',(-27.3809948754877,85.1201218069142,
64.7811217819716));
#214363=CARTESIAN_POINT('Ctrl Pts',(-27.3514639952375,85.8909626243882,
65.8760463333275));
#214364=CARTESIAN_POINT('Ctrl Pts',(-27.3414897687577,86.1324106356795,
66.2602166990751));
#214365=CARTESIAN_POINT('Ctrl Pts',(-27.3213168088313,86.5756651997547,
67.0548885316681));
#214366=CARTESIAN_POINT('Ctrl Pts',(-27.3111305725315,86.7768845333005,
67.4649977218528));
#214367=CARTESIAN_POINT('Ctrl Pts',(-27.3009162452284,86.9561136407892,
67.8848374071686));
#214368=CARTESIAN_POINT('Origin',(-21.6548258024609,75.,72.9888893865801));
#214369=CARTESIAN_POINT('',(-31.0052564152503,87.0149197055719,77.9529305295058));
#214370=CARTESIAN_POINT('',(-30.6991941617974,87.0149197055719,77.9529305295058));
#214371=CARTESIAN_POINT('',(-21.6548258024609,87.0149197055719,77.9529305295058));
#214372=CARTESIAN_POINT('Ctrl Pts',(-31.0052564152503,87.0149197055719,
77.9529305295058));
#214373=CARTESIAN_POINT('Ctrl Pts',(-30.9917690488268,86.7838685708455,
78.5121645792832));
#214374=CARTESIAN_POINT('Ctrl Pts',(-30.978424675615,86.5139457893124,79.0548487104576));
#214375=CARTESIAN_POINT('Ctrl Pts',(-30.947081719252,85.7934089254036,80.2805586134048));
#214376=CARTESIAN_POINT('Ctrl Pts',(-30.9288274919334,85.3144592787945,
80.9436385734192));
#214377=CARTESIAN_POINT('Ctrl Pts',(-30.8907219891804,84.1888208488232,
82.2279694179499));
#214378=CARTESIAN_POINT('Ctrl Pts',(-30.8712396609758,83.5336950227652,
82.8362782998089));
#214379=CARTESIAN_POINT('Ctrl Pts',(-30.8324131676161,82.1350383383838,
83.8897976090933));
#214380=CARTESIAN_POINT('Ctrl Pts',(-30.8130689348788,81.3990007294873,
84.337517908959));
#214381=CARTESIAN_POINT('Ctrl Pts',(-30.7847585542864,80.2468455373728,
84.8903927636798));
#214382=CARTESIAN_POINT('Ctrl Pts',(-30.7755495903525,79.86098288616,85.0531347620494));
#214383=CARTESIAN_POINT('Ctrl Pts',(-30.7473449652769,78.6600270726954,
85.4926632164057));
#214384=CARTESIAN_POINT('Ctrl Pts',(-30.7280319465382,77.8247529729081,
85.7074159361789));
#214385=CARTESIAN_POINT('Ctrl Pts',(-30.6910603912866,76.1833097779639,
85.9596412280131));
#214386=CARTESIAN_POINT('Ctrl Pts',(-30.6735710441109,75.3826698359065,
86.0078825015437));
#214387=CARTESIAN_POINT('Ctrl Pts',(-30.6367612694799,73.723799707552,85.9546048289067));
#214388=CARTESIAN_POINT('Ctrl Pts',(-30.6174206737797,72.8697508673038,
85.8419244905332));
#214389=CARTESIAN_POINT('Ctrl Pts',(-30.5891203967703,71.625834320556,85.5503372772465));
#214390=CARTESIAN_POINT('Ctrl Pts',(-30.5799175548124,71.2234276662779,
85.4352731540193));
#214391=CARTESIAN_POINT('Ctrl Pts',(-30.5517158090505,70.0124310690293,
85.0248514265013));
#214392=CARTESIAN_POINT('Ctrl Pts',(-30.5323980990866,69.2270193158836,
84.6684830853844));
#214393=CARTESIAN_POINT('Ctrl Pts',(-30.4941887309648,67.7418127631924,
83.8079329876412));
#214394=CARTESIAN_POINT('Ctrl Pts',(-30.4755254322597,67.0452443059709,
83.3065849621175));
#214395=CARTESIAN_POINT('Ctrl Pts',(-30.4378741503665,65.7755713791571,
82.1872388125171));
#214396=CARTESIAN_POINT('Ctrl Pts',(-30.4190857000926,65.2029574684524,
81.5747899403001));
#214397=CARTESIAN_POINT('Ctrl Pts',(-30.3913648517823,64.4395602890922,
80.5816671073266));
#214398=CARTESIAN_POINT('Ctrl Pts',(-30.3822150418368,64.2019447331048,
80.2397626378297));
#214399=CARTESIAN_POINT('Ctrl Pts',(-30.3540427097426,63.5245441071243,
79.1577086904222));
#214400=CARTESIAN_POINT('Ctrl Pts',(-30.3346959136119,63.1414925942369,
78.384833382503));
#214401=CARTESIAN_POINT('Ctrl Pts',(-30.2969818153582,62.5426256359343,
76.7982985002516));
#214402=CARTESIAN_POINT('Ctrl Pts',(-30.2787732689618,62.3236428415581,
75.9901789180012));
#214403=CARTESIAN_POINT('Ctrl Pts',(-30.2508987994316,62.1138560264226,
74.7555711816159));
#214404=CARTESIAN_POINT('Ctrl Pts',(-30.241547686786,62.0638225373116,74.3413625467781));
#214405=CARTESIAN_POINT('Ctrl Pts',(-30.2108955544545,61.9649968470735,
72.9731955847784));
#214406=CARTESIAN_POINT('Ctrl Pts',(-30.1900135419002,62.0013269251022,
72.0162419579962));
#214407=CARTESIAN_POINT('Ctrl Pts',(-30.149811678117,62.2688678602672,70.2217270883568));
#214408=CARTESIAN_POINT('Ctrl Pts',(-30.1304569567233,62.4796377824916,
69.3861894619105));
#214409=CARTESIAN_POINT('Ctrl Pts',(-30.0987099752017,62.9657266805747,
68.0386905203795));
#214410=CARTESIAN_POINT('Ctrl Pts',(-30.0861499083022,63.1955356089743,
67.5132321762431));
#214411=CARTESIAN_POINT('Ctrl Pts',(-30.0641712084464,63.6527600071269,
66.6314639443198));
#214412=CARTESIAN_POINT('Ctrl Pts',(-30.0547676958645,63.8642552474804,
66.2678850765865));
#214413=CARTESIAN_POINT('Ctrl Pts',(-30.0178988288399,64.7609078072379,
64.8853263443044));
#214414=CARTESIAN_POINT('Ctrl Pts',(-29.9911962885626,65.5713348830826,
63.9552290855923));
#214415=CARTESIAN_POINT('Ctrl Pts',(-29.9545359336962,66.8151514200182,
62.880396375519));
#214416=CARTESIAN_POINT('Ctrl Pts',(-29.9451992868035,67.1431014367415,
62.6234408896241));
#214417=CARTESIAN_POINT('Ctrl Pts',(-29.9154777248646,68.2292233056485,
61.8536494978173));
#214418=CARTESIAN_POINT('Ctrl Pts',(-29.8954815089603,69.0293898410136,
61.4049008852747));
#214419=CARTESIAN_POINT('Ctrl Pts',(-29.8561491607125,70.6597401524625,
60.7047186172491));
#214420=CARTESIAN_POINT('Ctrl Pts',(-29.836800587082,71.4811624772142,60.4447076416566));
#214421=CARTESIAN_POINT('Ctrl Pts',(-29.8084773743039,72.7320732180116,
60.1813941330134));
#214422=CARTESIAN_POINT('Ctrl Pts',(-29.7992606631811,73.1458609453379,
60.1149779630723));
#214423=CARTESIAN_POINT('Ctrl Pts',(-29.7710526926903,74.4171129081448,
59.9735027293807));
#214424=CARTESIAN_POINT('Ctrl Pts',(-29.7517461979083,75.2794287901344,
59.9634544442968));
#214425=CARTESIAN_POINT('Ctrl Pts',(-29.7132365836367,77.0023514705184,
60.114641695641));
#214426=CARTESIAN_POINT('Ctrl Pts',(-29.6942902410553,77.8585081271593,
60.2772966406358));
#214427=CARTESIAN_POINT('Ctrl Pts',(-29.6656703653338,79.0919904728141,
60.642649394471));
#214428=CARTESIAN_POINT('Ctrl Pts',(-29.6563152116875,79.4860451648727,
60.7803093475951));
#214429=CARTESIAN_POINT('Ctrl Pts',(-29.6254462295597,80.7665405145654,
61.2980229125601));
#214430=CARTESIAN_POINT('Ctrl Pts',(-29.6043576289001,81.6173189050517,
61.7576637055568));
#214431=CARTESIAN_POINT('Ctrl Pts',(-29.565955471714,83.0415172632508,62.7455614485674));
#214432=CARTESIAN_POINT('Ctrl Pts',(-29.5486374992503,83.6334380938079,
63.2392476757865));
#214433=CARTESIAN_POINT('Ctrl Pts',(-29.5146922579461,84.715526424702,64.3180095817668));
#214434=CARTESIAN_POINT('Ctrl Pts',(-29.4981279757756,85.2049024155273,
64.8996638324907));
#214435=CARTESIAN_POINT('Ctrl Pts',(-29.4719894373469,85.880670516805,65.8625001577654));
#214436=CARTESIAN_POINT('Ctrl Pts',(-29.4626248789256,86.1039778442336,
66.2157003332167));
#214437=CARTESIAN_POINT('Ctrl Pts',(-29.4312913619077,86.7950129211955,
67.4350001219214));
#214438=CARTESIAN_POINT('Ctrl Pts',(-29.4097597523413,87.1813903963534,
68.3432747335166));
#214439=CARTESIAN_POINT('Ctrl Pts',(-29.3709189800937,87.6807751072625,
70.0240727435726));
#214440=CARTESIAN_POINT('Ctrl Pts',(-29.3535944272079,87.8340129956633,
70.7797482706167));
#214441=CARTESIAN_POINT('Ctrl Pts',(-29.3199808831717,88.0020982996774,
72.2832335622355));
#214442=CARTESIAN_POINT('Ctrl Pts',(-29.3037410645682,88.0211750548048,
73.0276616018292));
#214443=CARTESIAN_POINT('Ctrl Pts',(-29.2779607616765,87.9514273241659,
74.1869315593425));
#214444=CARTESIAN_POINT('Ctrl Pts',(-29.2685881002784,87.906204755505,74.6027829499671));
#214445=CARTESIAN_POINT('Ctrl Pts',(-29.2368855131641,87.6851712490229,
76.0031381799151));
#214446=CARTESIAN_POINT('Ctrl Pts',(-29.215001493764,87.4159475290683,76.9692793700861));
#214447=CARTESIAN_POINT('Ctrl Pts',(-29.1923989754345,87.0308162878128,
77.9143229035002));
#214448=CARTESIAN_POINT('Ctrl Pts',(-29.1919363963037,87.0228910310784,
77.933636806284));
#214449=CARTESIAN_POINT('Ctrl Pts',(-29.191473624437,87.0149197049505,77.9529305310098));
#214450=CARTESIAN_POINT('Ctrl Pts',(-30.6991941617974,87.0149197055719,
77.9529305295058));
#214451=CARTESIAN_POINT('Ctrl Pts',(-30.683487502314,86.7453849041422,78.6053100936136));
#214452=CARTESIAN_POINT('Ctrl Pts',(-30.6680646534442,86.423064275653,79.2348940782624));
#214453=CARTESIAN_POINT('Ctrl Pts',(-30.6351661800128,85.6414886819256,
80.496450934198));
#214454=CARTESIAN_POINT('Ctrl Pts',(-30.6176869597372,85.173438915591,81.119442347468));
#214455=CARTESIAN_POINT('Ctrl Pts',(-30.5812917504726,84.0769697870016,
82.3348469910265));
#214456=CARTESIAN_POINT('Ctrl Pts',(-30.5625565966655,83.4395720445536,
82.9142072901222));
#214457=CARTESIAN_POINT('Ctrl Pts',(-30.5341175409455,82.4141430219993,
83.675570097848));
#214458=CARTESIAN_POINT('Ctrl Pts',(-30.5247597961772,82.0667775703784,
83.9083818204726));
#214459=CARTESIAN_POINT('Ctrl Pts',(-30.4961757833556,80.9718250985024,
84.5680775450416));
#214460=CARTESIAN_POINT('Ctrl Pts',(-30.4773744419514,80.1925835798765,
84.9378379286018));
#214461=CARTESIAN_POINT('Ctrl Pts',(-30.4407631920138,78.63698675406,85.4948662864242));
#214462=CARTESIAN_POINT('Ctrl Pts',(-30.4229673875434,77.8685963057515,
85.6931514335049));
#214463=CARTESIAN_POINT('Ctrl Pts',(-30.3882077810994,76.3258553895781,
85.9440701974503));
#214464=CARTESIAN_POINT('Ctrl Pts',(-30.3713805720948,75.5552452569285,
85.9998966561579));
#214465=CARTESIAN_POINT('Ctrl Pts',(-30.3381954147479,74.0615379456218,
85.9751027001413));
#214466=CARTESIAN_POINT('Ctrl Pts',(-30.3219380215231,73.3410942776849,
85.9028536120454));
#214467=CARTESIAN_POINT('Ctrl Pts',(-30.2898766920788,71.9216513043095,
85.6397139236053));
#214468=CARTESIAN_POINT('Ctrl Pts',(-30.2741277391862,71.2250530960396,
85.4496026577302));
#214469=CARTESIAN_POINT('Ctrl Pts',(-30.2410058827312,69.8232952005922,
84.938634196457));
#214470=CARTESIAN_POINT('Ctrl Pts',(-30.2236501801234,69.1237157754223,
84.6105912010207));
#214471=CARTESIAN_POINT('Ctrl Pts',(-30.1889939369819,67.7735893450981,
83.8242530979093));
#214472=CARTESIAN_POINT('Ctrl Pts',(-30.1717043987259,67.1276141582225,
83.3644214827376));
#214473=CARTESIAN_POINT('Ctrl Pts',(-30.1349447442983,65.8748944413803,
82.2879618489353));
#214474=CARTESIAN_POINT('Ctrl Pts',(-30.1156198528478,65.2795974654932,
81.6638006618464));
#214475=CARTESIAN_POINT('Ctrl Pts',(-30.087423350035,64.4932999188011,80.6559535239909));
#214476=CARTESIAN_POINT('Ctrl Pts',(-30.0782309027133,64.2522932598192,
80.3142848457365));
#214477=CARTESIAN_POINT('Ctrl Pts',(-30.0499477074029,63.56729832787,79.2364185978482));
#214478=CARTESIAN_POINT('Ctrl Pts',(-30.030613679607,63.1794683809488,78.4673298951771));
#214479=CARTESIAN_POINT('Ctrl Pts',(-29.9943582613655,62.5915949928642,
76.9426142359236));
#214480=CARTESIAN_POINT('Ctrl Pts',(-29.9774277283934,62.3780308024885,
76.1961243240493));
#214481=CARTESIAN_POINT('Ctrl Pts',(-29.9410515613493,62.0703077754327,
74.5899724049097));
#214482=CARTESIAN_POINT('Ctrl Pts',(-29.9217091327139,61.992699412414,73.7308796678632));
#214483=CARTESIAN_POINT('Ctrl Pts',(-29.8935307167979,62.0043350551339,
72.4539048674676));
#214484=CARTESIAN_POINT('Ctrl Pts',(-29.8843706324115,62.0281484803234,
72.0377932588003));
#214485=CARTESIAN_POINT('Ctrl Pts',(-29.856652196523,62.1596741401908,70.7924099809308));
#214486=CARTESIAN_POINT('Ctrl Pts',(-29.8378757242906,62.3273948229381,
69.9716799211151));
#214487=CARTESIAN_POINT('Ctrl Pts',(-29.8008659262445,62.8159392159901,
68.3807326612484));
#214488=CARTESIAN_POINT('Ctrl Pts',(-29.7827974453274,63.1343099047363,
67.6137753764481));
#214489=CARTESIAN_POINT('Ctrl Pts',(-29.7452214016125,63.9276828070571,
66.1227272575466));
#214490=CARTESIAN_POINT('Ctrl Pts',(-29.725884467204,64.4062923013186,65.4051068112389));
#214491=CARTESIAN_POINT('Ctrl Pts',(-29.6976994255059,65.2168928217506,
64.4177329161527));
#214492=CARTESIAN_POINT('Ctrl Pts',(-29.6885278845024,65.4968615400463,
64.1083337423874));
#214493=CARTESIAN_POINT('Ctrl Pts',(-29.6608129838283,66.3805145173726,
63.2215199253372));
#214494=CARTESIAN_POINT('Ctrl Pts',(-29.6420508216541,67.0254128448869,
62.6882592610116));
#214495=CARTESIAN_POINT('Ctrl Pts',(-29.6057630221928,68.3775425608711,
61.773765084264));
#214496=CARTESIAN_POINT('Ctrl Pts',(-29.588363277267,69.0778239474529,61.388725890832));
#214497=CARTESIAN_POINT('Ctrl Pts',(-29.5534121047939,70.5190466965732,
60.7610142168751));
#214498=CARTESIAN_POINT('Ctrl Pts',(-29.5359768301,71.2553544349169,60.5158180731919));
#214499=CARTESIAN_POINT('Ctrl Pts',(-29.5059736898199,72.5750224054888,
60.2038333795925));
#214500=CARTESIAN_POINT('Ctrl Pts',(-29.4932246047683,73.1492892939941,
60.1081656105193));
#214501=CARTESIAN_POINT('Ctrl Pts',(-29.4612737528292,74.5836345257894,
59.967146809208));
#214502=CARTESIAN_POINT('Ctrl Pts',(-29.441913072983,75.4454771584534,59.968110292761));
#214503=CARTESIAN_POINT('Ctrl Pts',(-29.4005791665963,77.3024537657004,
60.1548729888451));
#214504=CARTESIAN_POINT('Ctrl Pts',(-29.3785386794421,78.2889343016288,
60.3715921653986));
#214505=CARTESIAN_POINT('Ctrl Pts',(-29.3466721202713,79.63589476985,60.8363819123887));
#214506=CARTESIAN_POINT('Ctrl Pts',(-29.337295744946,80.0244819828131,60.991825551247));
#214507=CARTESIAN_POINT('Ctrl Pts',(-29.3109609302171,81.1038978180587,
61.4852751765406));
#214508=CARTESIAN_POINT('Ctrl Pts',(-29.2941686238249,81.7731848908891,
61.8661791844435));
#214509=CARTESIAN_POINT('Ctrl Pts',(-29.2579408311842,83.1121287271607,
62.794097809553));
#214510=CARTESIAN_POINT('Ctrl Pts',(-29.2385928061241,83.7689585709696,
63.3532377044086));
#214511=CARTESIAN_POINT('Ctrl Pts',(-29.2104223409726,84.6542137681349,
64.27285767758));
#214512=CARTESIAN_POINT('Ctrl Pts',(-29.2012756477301,84.928162211407,64.5862322291635));
#214513=CARTESIAN_POINT('Ctrl Pts',(-29.1735542035811,85.7064522694633,
65.5678398967372));
#214514=CARTESIAN_POINT('Ctrl Pts',(-29.1547622732909,86.1617767551519,
66.2721327119445));
#214515=CARTESIAN_POINT('Ctrl Pts',(-29.116916366813,86.9435113337627,67.7831280194739));
#214516=CARTESIAN_POINT('Ctrl Pts',(-29.098072423964,87.2631860069253,68.5886973960785));
#214517=CARTESIAN_POINT('Ctrl Pts',(-29.0596713147632,87.7367018161264,
70.2472590047661));
#214518=CARTESIAN_POINT('Ctrl Pts',(-29.0403605782177,87.8901804322048,
71.0959102590723));
#214519=CARTESIAN_POINT('Ctrl Pts',(-29.0121546979943,87.9920446606397,
72.3707958832831));
#214520=CARTESIAN_POINT('Ctrl Pts',(-29.0029429272309,88.0052104471586,
72.7894780506037));
#214521=CARTESIAN_POINT('Ctrl Pts',(-28.9746279035492,87.983662591991,74.0673762813916));
#214522=CARTESIAN_POINT('Ctrl Pts',(-28.9552820635389,87.8839947534392,
74.9231335477672));
#214523=CARTESIAN_POINT('Ctrl Pts',(-28.9192277563573,87.5370075915119,
76.5118633438581));
#214524=CARTESIAN_POINT('Ctrl Pts',(-28.9024715747196,87.3075049584308,
77.2447598639295));
#214525=CARTESIAN_POINT('Ctrl Pts',(-28.8854250924613,87.0149197055719,
77.9529305295058));
#214526=CARTESIAN_POINT('Origin',(-21.6548258024609,75.,72.9888893865801));
#214527=CARTESIAN_POINT('',(-32.819270903196,87.0149197055719,77.9529305295058));
#214528=CARTESIAN_POINT('',(-32.5134098057851,87.0149197055719,77.9529305295058));
#214529=CARTESIAN_POINT('',(-21.6548258024609,87.0149197055719,77.9529305295058));
#214530=CARTESIAN_POINT('',(-31.8032572668915,65.6642719369909,63.9421119750625));
#214531=CARTESIAN_POINT('Ctrl Pts',(-31.8032572668915,65.6642719369909,
63.9421119750625));
#214532=CARTESIAN_POINT('Ctrl Pts',(-31.8135733380367,65.3385656683114,
64.2782211788701));
#214533=CARTESIAN_POINT('Ctrl Pts',(-31.8239028665893,65.0312489587717,
64.6316736406528));
#214534=CARTESIAN_POINT('Ctrl Pts',(-31.8446497618166,64.458312651216,65.3673088614644));
#214535=CARTESIAN_POINT('Ctrl Pts',(-31.8550507549726,64.1927991754078,
65.7487187740987));
#214536=CARTESIAN_POINT('Ctrl Pts',(-31.8857791041659,63.469068259206,66.9171692590297));
#214537=CARTESIAN_POINT('Ctrl Pts',(-31.9056269465411,63.0724313378894,
67.7390056154748));
#214538=CARTESIAN_POINT('Ctrl Pts',(-31.9423166756006,62.513779546848,69.294791851719));
#214539=CARTESIAN_POINT('Ctrl Pts',(-31.9590233980021,62.3230926914423,
70.0143187716436));
#214540=CARTESIAN_POINT('Ctrl Pts',(-31.9836814319382,62.1316498998252,
71.1073896767436));
#214541=CARTESIAN_POINT('Ctrl Pts',(-31.9917495291653,62.0836986306711,
71.4711162185924));
#214542=CARTESIAN_POINT('Ctrl Pts',(-32.0263623363712,61.9444997996125,
73.0350631533012));
#214543=CARTESIAN_POINT('Ctrl Pts',(-32.0533773329147,62.0047705901487,
74.2427715948304));
#214544=CARTESIAN_POINT('Ctrl Pts',(-32.0892096891712,62.3082996330555,
75.8339102814937));
#214545=CARTESIAN_POINT('Ctrl Pts',(-32.0983575985955,62.405937461001,76.2389650225414));
#214546=CARTESIAN_POINT('Ctrl Pts',(-32.1278230373569,62.780470583843,77.5193580315241));
#214547=CARTESIAN_POINT('Ctrl Pts',(-32.1484059703415,63.1306211086671,
78.3703268030057));
#214548=CARTESIAN_POINT('Ctrl Pts',(-32.1879520538945,63.9765823916936,
79.9331668466769));
#214549=CARTESIAN_POINT('Ctrl Pts',(-32.2066841825695,64.4596806333664,
80.6465912662357));
#214550=CARTESIAN_POINT('Ctrl Pts',(-32.2384146572364,65.3718995347885,
81.742186566815));
#214551=CARTESIAN_POINT('Ctrl Pts',(-32.2511214127918,65.7621942789836,
82.1531391066049));
#214552=CARTESIAN_POINT('Ctrl Pts',(-32.2731089279731,66.4867285575212,
82.8225484010837));
#214553=CARTESIAN_POINT('Ctrl Pts',(-32.2823645111182,66.8090751745151,
83.0926209277359));
#214554=CARTESIAN_POINT('Ctrl Pts',(-32.3186284223173,68.1198341268779,
84.0867981090575));
#214555=CARTESIAN_POINT('Ctrl Pts',(-32.3461123736615,69.1954616791803,
84.6853669253804));
#214556=CARTESIAN_POINT('Ctrl Pts',(-32.3824141307471,70.7275723256521,
85.2738289342571));
#214557=CARTESIAN_POINT('Ctrl Pts',(-32.3915615106238,71.1232226654734,
85.4043626424828));
#214558=CARTESIAN_POINT('Ctrl Pts',(-32.4209738567902,72.4063196478546,
85.7603565975389));
#214559=CARTESIAN_POINT('Ctrl Pts',(-32.441503262611,73.3115543342576,85.9112220916367));
#214560=CARTESIAN_POINT('Ctrl Pts',(-32.4789869647881,74.9930306227604,
86.0116302776272));
#214561=CARTESIAN_POINT('Ctrl Pts',(-32.4957723959841,75.7635232247348,
85.9892303391343));
#214562=CARTESIAN_POINT('Ctrl Pts',(-32.529097733169,77.2539602171473,85.8128823263586));
#214563=CARTESIAN_POINT('Ctrl Pts',(-32.5455487687377,77.9718656649989,
85.6657635364555));
#214564=CARTESIAN_POINT('Ctrl Pts',(-32.579135811788,79.4220603514326,85.2385520285343));
#214565=CARTESIAN_POINT('Ctrl Pts',(-32.5961693648489,80.1491790912049,
84.9511139013838));
#214566=CARTESIAN_POINT('Ctrl Pts',(-32.6268443157916,81.3816067348078,
84.3306056441482));
#214567=CARTESIAN_POINT('Ctrl Pts',(-32.6402975044144,81.8977977270893,
84.0242785943624));
#214568=CARTESIAN_POINT('Ctrl Pts',(-32.6630465611979,82.7370776852665,
83.4442518058244));
#214569=CARTESIAN_POINT('Ctrl Pts',(-32.6723157786034,83.0713407117878,
83.1884204480479));
#214570=CARTESIAN_POINT('Ctrl Pts',(-32.7088655896348,84.3376510901744,
82.1179418422261));
#214571=CARTESIAN_POINT('Ctrl Pts',(-32.7366253494161,85.1637971527023,
81.1881909555477));
#214572=CARTESIAN_POINT('Ctrl Pts',(-32.773203608357,86.0755540950393,79.8083810977813));
#214573=CARTESIAN_POINT('Ctrl Pts',(-32.782350752454,86.2882775758034,79.4501706690866));
#214574=CARTESIAN_POINT('Ctrl Pts',(-32.8007507006903,86.6787198769651,
78.7143643607418));
#214575=CARTESIAN_POINT('Ctrl Pts',(-32.8099869769191,86.8560578530742,
78.3374383019199));
#214576=CARTESIAN_POINT('Ctrl Pts',(-32.819270903196,87.0149197055719,77.9529305295058));
#214577=CARTESIAN_POINT('Ctrl Pts',(-31.8032546359729,65.6642718921576,
63.9421120213278));
#214578=CARTESIAN_POINT('Ctrl Pts',(-31.7842284681536,66.2560091425745,
63.3314749007115));
#214579=CARTESIAN_POINT('Ctrl Pts',(-31.7654238551895,66.9062344712278,
62.7803635629509));
#214580=CARTESIAN_POINT('Ctrl Pts',(-31.728504118784,68.2838663363805,61.8276341158955));
#214581=CARTESIAN_POINT('Ctrl Pts',(-31.7100617480658,69.0052280770819,
61.4241685258146));
#214582=CARTESIAN_POINT('Ctrl Pts',(-31.6718429273203,70.5729452195354,
60.7336692325463));
#214583=CARTESIAN_POINT('Ctrl Pts',(-31.6524317557486,71.4205314357544,
60.4598578773549));
#214584=CARTESIAN_POINT('Ctrl Pts',(-31.6136746885707,73.1298798352618,
60.095434315327));
#214585=CARTESIAN_POINT('Ctrl Pts',(-31.5943314241114,73.986071048588,60.000029197985));
#214586=CARTESIAN_POINT('Ctrl Pts',(-31.562881818816,75.4056682551647,59.9831450953161));
#214587=CARTESIAN_POINT('Ctrl Pts',(-31.5505969704306,75.9657858978662,
60.0127109359883));
#214588=CARTESIAN_POINT('Ctrl Pts',(-31.5210871038211,77.2900265256507,
60.1688478647222));
#214589=CARTESIAN_POINT('Ctrl Pts',(-31.5036829091261,78.0482033068846,
60.3276833323172));
#214590=CARTESIAN_POINT('Ctrl Pts',(-31.4673980769323,79.6096046724077,
60.8032570735867));
#214591=CARTESIAN_POINT('Ctrl Pts',(-31.4486815423165,80.404613767649,61.1344286833351));
#214592=CARTESIAN_POINT('Ctrl Pts',(-31.4202443593273,81.527856597147,61.7389763999586));
#214593=CARTESIAN_POINT('Ctrl Pts',(-31.410905144574,81.8848939385131,61.953868331928));
#214594=CARTESIAN_POINT('Ctrl Pts',(-31.3809917514735,82.9981248456975,
62.6989855387059));
#214595=CARTESIAN_POINT('Ctrl Pts',(-31.3608129843137,83.708379801769,63.2926924838235));
#214596=CARTESIAN_POINT('Ctrl Pts',(-31.3310663415844,84.6408211138014,
64.2579053239863));
#214597=CARTESIAN_POINT('Ctrl Pts',(-31.3216800837528,84.9171638610513,
64.573108212071));
#214598=CARTESIAN_POINT('Ctrl Pts',(-31.2936664521116,85.6963073046544,
65.5535948162585));
#214599=CARTESIAN_POINT('Ctrl Pts',(-31.2752613335763,86.1508664949386,
66.2544421967027));
#214600=CARTESIAN_POINT('Ctrl Pts',(-31.2389086390138,86.9112415809572,
67.7175257133276));
#214601=CARTESIAN_POINT('Ctrl Pts',(-31.2206515149041,87.2183687057085,
68.4748661687591));
#214602=CARTESIAN_POINT('Ctrl Pts',(-31.1828793143346,87.7046520773152,
70.0970395384582));
#214603=CARTESIAN_POINT('Ctrl Pts',(-31.1636970411606,87.8709224718629,
70.9614956475302));
#214604=CARTESIAN_POINT('Ctrl Pts',(-31.1349413547196,87.9859043416946,
72.2530214836414));
#214605=CARTESIAN_POINT('Ctrl Pts',(-31.1255602693797,88.0028642364736,
72.6715053387859));
#214606=CARTESIAN_POINT('Ctrl Pts',(-31.0934877823317,87.9917030279652,
74.10542105164));
#214607=CARTESIAN_POINT('Ctrl Pts',(-31.0712508455816,87.8648704341448,
75.1163507153663));
#214608=CARTESIAN_POINT('Ctrl Pts',(-31.03947192201,87.5212073175799,76.5096092073126));
#214609=CARTESIAN_POINT('Ctrl Pts',(-31.0300766281358,87.4010408798071,
76.9119344551807));
#214610=CARTESIAN_POINT('Ctrl Pts',(-31.0155341825007,87.1850859522539,
77.5250511349386));
#214611=CARTESIAN_POINT('Ctrl Pts',(-31.0103872385355,87.1028154818789,
77.7401883977667));
#214612=CARTESIAN_POINT('Ctrl Pts',(-31.0052564152503,87.0149197055719,
77.9529305295058));
#214613=CARTESIAN_POINT('Ctrl Pts',(-32.5134098057851,87.0149197055719,
77.9529305295058));
#214614=CARTESIAN_POINT('Ctrl Pts',(-32.5075997933644,86.9146418918773,
78.1956420311034));
#214615=CARTESIAN_POINT('Ctrl Pts',(-32.5017690584973,86.8069826178028,
78.4353803885588));
#214616=CARTESIAN_POINT('Ctrl Pts',(-32.4838109340488,86.4545420879065,
79.1604936379299));
#214617=CARTESIAN_POINT('Ctrl Pts',(-32.4716151683794,86.1866124201152,
79.6338073004822));
#214618=CARTESIAN_POINT('Ctrl Pts',(-32.4423112173233,85.4683690181421,
80.7354249903596));
#214619=CARTESIAN_POINT('Ctrl Pts',(-32.4254745688282,84.9901551749687,
81.3430718605348));
#214620=CARTESIAN_POINT('Ctrl Pts',(-32.3909691756996,83.9235056915968,
82.4749303419633));
#214621=CARTESIAN_POINT('Ctrl Pts',(-32.3733384476991,83.3356814762439,
82.9954039613138));
#214622=CARTESIAN_POINT('Ctrl Pts',(-32.337430403783,82.0324512357819,83.9543344917921));
#214623=CARTESIAN_POINT('Ctrl Pts',(-32.3192085828059,81.3142562951554,
84.3830340939489));
#214624=CARTESIAN_POINT('Ctrl Pts',(-32.2913278650799,80.1827923149245,
84.9183801317905));
#214625=CARTESIAN_POINT('Ctrl Pts',(-32.2819836082309,79.797270011951,85.0785661809406));
#214626=CARTESIAN_POINT('Ctrl Pts',(-32.2534186544639,78.5951583303169,
85.5114776060869));
#214627=CARTESIAN_POINT('Ctrl Pts',(-32.2346255300043,77.758655028736,85.721925287822));
#214628=CARTESIAN_POINT('Ctrl Pts',(-32.1970950751662,76.0836806853654,
85.9703866976567));
#214629=CARTESIAN_POINT('Ctrl Pts',(-32.1783506117603,75.2500110699179,
86.0131407334634));
#214630=CARTESIAN_POINT('Ctrl Pts',(-32.1413371328631,73.5829692638462,
85.9384339552752));
#214631=CARTESIAN_POINT('Ctrl Pts',(-32.1230771433696,72.7534880564385,
85.8205639948546));
#214632=CARTESIAN_POINT('Ctrl Pts',(-32.0951735876016,71.5362867104418,
85.5258807657098));
#214633=CARTESIAN_POINT('Ctrl Pts',(-32.0858442209667,71.1364359369947,
85.4084841601795));
#214634=CARTESIAN_POINT('Ctrl Pts',(-32.0573009838373,69.9298848928574,
84.9903203794736));
#214635=CARTESIAN_POINT('Ctrl Pts',(-32.0385161603638,69.1468406483531,
84.6285173885043));
#214636=CARTESIAN_POINT('Ctrl Pts',(-32.0003874137635,67.6647780431255,
83.7561040859797));
#214637=CARTESIAN_POINT('Ctrl Pts',(-31.9810358762197,66.9692967255576,
83.2478463122074));
#214638=CARTESIAN_POINT('Ctrl Pts',(-31.9434039408314,65.7031284230795,
82.1143467604991));
#214639=CARTESIAN_POINT('Ctrl Pts',(-31.9250222758533,65.1329804070874,
81.4946358664839));
#214640=CARTESIAN_POINT('Ctrl Pts',(-31.8913006292345,64.2216681034031,
80.288134727132));
#214641=CARTESIAN_POINT('Ctrl Pts',(-31.8762028233835,63.858882935033,79.7214178144745));
#214642=CARTESIAN_POINT('Ctrl Pts',(-31.8521448114598,63.3449044615873,
78.7622803770684));
#214643=CARTESIAN_POINT('Ctrl Pts',(-31.8429988603328,63.1660163439334,
78.3861226572369));
#214644=CARTESIAN_POINT('Ctrl Pts',(-31.8138208557924,62.6567570514172,
77.1676617000098));
#214645=CARTESIAN_POINT('Ctrl Pts',(-31.7935292548616,62.396043768211,76.2991841604238));
#214646=CARTESIAN_POINT('Ctrl Pts',(-31.7542863072485,62.0674673988842,
74.5663088062888));
#214647=CARTESIAN_POINT('Ctrl Pts',(-31.7355537963974,61.9914880216104,
73.7081064929883));
#214648=CARTESIAN_POINT('Ctrl Pts',(-31.7071035349279,62.0052709553146,
72.4300220550393));
#214649=CARTESIAN_POINT('Ctrl Pts',(-31.6977308382133,62.0300109726611,
72.0118023620038));
#214650=CARTESIAN_POINT('Ctrl Pts',(-31.6691269703002,62.1670970869241,
70.7401805414656));
#214651=CARTESIAN_POINT('Ctrl Pts',(-31.6503159240616,62.3439801615891,
69.8961150526805));
#214652=CARTESIAN_POINT('Ctrl Pts',(-31.6120805004828,62.8636003199811,
68.2499355214424));
#214653=CARTESIAN_POINT('Ctrl Pts',(-31.5925892083222,63.2061228202923,
67.4522537560806));
#214654=CARTESIAN_POINT('Ctrl Pts',(-31.5548346716221,64.030534095666,65.9624416214482));
#214655=CARTESIAN_POINT('Ctrl Pts',(-31.5365502063061,64.5054110851407,
65.2711331158504));
#214656=CARTESIAN_POINT('Ctrl Pts',(-31.5086330122316,65.3108801702628,
64.3116782590005));
#214657=CARTESIAN_POINT('Ctrl Pts',(-31.4993139962588,65.5934778173574,
64.006107216035));
#214658=CARTESIAN_POINT('Ctrl Pts',(-31.4707861181307,66.5041026698939,
63.1116356769772));
#214659=CARTESIAN_POINT('Ctrl Pts',(-31.4520065855794,67.1763190514444,
62.5710954819328));
#214660=CARTESIAN_POINT('Ctrl Pts',(-31.4150123669398,68.5735484664381,
61.6595800493482));
#214661=CARTESIAN_POINT('Ctrl Pts',(-31.3968335965468,69.2897667003974,
61.2822349691715));
#214662=CARTESIAN_POINT('Ctrl Pts',(-31.3603815292869,70.8082550101268,
60.6549203508464));
#214663=CARTESIAN_POINT('Ctrl Pts',(-31.3421407074077,71.6090923015082,
60.4111601719133));
#214664=CARTESIAN_POINT('Ctrl Pts',(-31.3142483905366,72.8363906628502,
60.163423457877));
#214665=CARTESIAN_POINT('Ctrl Pts',(-31.3049113628243,73.2487508542692,
60.1006425291059));
#214666=CARTESIAN_POINT('Ctrl Pts',(-31.2763568850329,74.5193177389937,
59.9693138810174));
#214667=CARTESIAN_POINT('Ctrl Pts',(-31.2575678935881,75.3818940328471,
59.966041762369));
#214668=CARTESIAN_POINT('Ctrl Pts',(-31.2212335515245,77.0135281432915,
60.1221898690667));
#214669=CARTESIAN_POINT('Ctrl Pts',(-31.2037330433807,77.7803744388936,
60.2658489075672));
#214670=CARTESIAN_POINT('Ctrl Pts',(-31.1673159196836,79.3567104591316,
60.7105594778463));
#214671=CARTESIAN_POINT('Ctrl Pts',(-31.1485808358536,80.1585174025768,
61.0252771705167));
#214672=CARTESIAN_POINT('Ctrl Pts',(-31.1201415347332,81.2954281594925,
61.6072260922669));
#214673=CARTESIAN_POINT('Ctrl Pts',(-31.1107834729899,81.6580632094587,
61.8154893569849));
#214674=CARTESIAN_POINT('Ctrl Pts',(-31.0821990223593,82.734626612722,62.5048137631266));
#214675=CARTESIAN_POINT('Ctrl Pts',(-31.0633974804975,83.4113707080935,
63.0395609964287));
#214676=CARTESIAN_POINT('Ctrl Pts',(-31.0255413687474,84.6404053738881,
64.2263624082217));
#214677=CARTESIAN_POINT('Ctrl Pts',(-31.0064524825665,85.191385486151,64.8737831658655));
#214678=CARTESIAN_POINT('Ctrl Pts',(-30.9690972308968,86.1526095639457,
66.2569751945058));
#214679=CARTESIAN_POINT('Ctrl Pts',(-30.9508258171705,86.5624697843879,
66.9881669713929));
#214680=CARTESIAN_POINT('Ctrl Pts',(-30.9229157932786,87.0668817808325,
68.13465099886));
#214681=CARTESIAN_POINT('Ctrl Pts',(-30.9135911763968,87.2161150735975,
68.5234893164158));
#214682=CARTESIAN_POINT('Ctrl Pts',(-30.8850549657918,87.6158356070293,
69.7360280810617));
#214683=CARTESIAN_POINT('Ctrl Pts',(-30.8662726181079,87.8034327564835,
70.5779713807514));
#214684=CARTESIAN_POINT('Ctrl Pts',(-30.8291649364347,88.0038269288232,
72.2394920522822));
#214685=CARTESIAN_POINT('Ctrl Pts',(-30.8108665953109,88.0252391035558,
73.0540816277721));
#214686=CARTESIAN_POINT('Ctrl Pts',(-30.7742958530402,87.9141078888471,
74.6987386374438));
#214687=CARTESIAN_POINT('Ctrl Pts',(-30.7560509419293,87.7775952862349,
75.5247984171261));
#214688=CARTESIAN_POINT('Ctrl Pts',(-30.7281561876402,87.4555936971577,
76.7348072049893));
#214689=CARTESIAN_POINT('Ctrl Pts',(-30.7188207626934,87.3291018834203,
77.1321924632432));
#214690=CARTESIAN_POINT('Ctrl Pts',(-30.7060591949955,87.1300003055977,
77.6672262756005));
#214691=CARTESIAN_POINT('Ctrl Pts',(-30.7026204048056,87.073715895164,77.8106207708631));
#214692=CARTESIAN_POINT('Ctrl Pts',(-30.6991941617974,87.0149197055719,
77.9529305295058));
#214693=CARTESIAN_POINT('Origin',(-21.6548258024609,75.,72.9888893865801));
#214694=CARTESIAN_POINT('',(-34.6333744106366,87.0149197055719,77.9529305295058));
#214695=CARTESIAN_POINT('',(-34.3273949797549,87.0149197055719,77.9529305295058));
#214696=CARTESIAN_POINT('',(-21.6548258024609,87.0149197055719,77.9529305295058));
#214697=CARTESIAN_POINT('Ctrl Pts',(-32.819270903196,87.0149197055719,77.9529305295058));
#214698=CARTESIAN_POINT('Ctrl Pts',(-32.8303492893789,87.2044874487043,
77.4941025007035));
#214699=CARTESIAN_POINT('Ctrl Pts',(-32.8415001971829,87.3677464596969,
77.0244787448557));
#214700=CARTESIAN_POINT('Ctrl Pts',(-32.8618829569116,87.6184066977144,
76.1434512817156));
#214701=CARTESIAN_POINT('Ctrl Pts',(-32.8710927370109,87.7134904735021,
75.7352704421921));
#214702=CARTESIAN_POINT('Ctrl Pts',(-32.9028840772483,87.9724059114136,
74.3167894059358));
#214703=CARTESIAN_POINT('Ctrl Pts',(-32.925752002725,88.0366642288654,73.2921902487054));
#214704=CARTESIAN_POINT('Ctrl Pts',(-32.9578897961531,87.9569617157058,
71.8516619677294));
#214705=CARTESIAN_POINT('Ctrl Pts',(-32.9671257230642,87.9134966956485,
71.4339789389983));
#214706=CARTESIAN_POINT('Ctrl Pts',(-32.9948122310079,87.7231975056415,
70.1925447133568));
#214707=CARTESIAN_POINT('Ctrl Pts',(-33.0133770239326,87.5170292474647,
69.3801132161319));
#214708=CARTESIAN_POINT('Ctrl Pts',(-33.050347567485,86.9582785244051,67.8249971947681));
#214709=CARTESIAN_POINT('Ctrl Pts',(-33.0682711390013,86.6105575235084,
67.0845548514814));
#214710=CARTESIAN_POINT('Ctrl Pts',(-33.1060395069239,85.74201255568,65.6128453231014));
#214711=CARTESIAN_POINT('Ctrl Pts',(-33.1260757975856,85.2103360810908,
64.8928485371945));
#214712=CARTESIAN_POINT('Ctrl Pts',(-33.1650533361119,84.0302700332628,
63.5977869024856));
#214713=CARTESIAN_POINT('Ctrl Pts',(-33.1837862547422,83.3898671157429,
63.0215066535477));
#214714=CARTESIAN_POINT('Ctrl Pts',(-33.2122343752409,82.360001722789,62.2648248635988));
#214715=CARTESIAN_POINT('Ctrl Pts',(-33.2216041277003,82.0109346076854,
62.0334350381732));
#214716=CARTESIAN_POINT('Ctrl Pts',(-33.2502042439525,80.9121335321621,
61.3791168043054));
#214717=CARTESIAN_POINT('Ctrl Pts',(-33.2690133538773,80.1310797993482,
61.0134075639596));
#214718=CARTESIAN_POINT('Ctrl Pts',(-33.3071691420166,78.5064325375152,
60.4410479395259));
#214719=CARTESIAN_POINT('Ctrl Pts',(-33.326575808564,77.6667357252942,60.2361678403155));
#214720=CARTESIAN_POINT('Ctrl Pts',(-33.364246377408,75.9844855781902,59.999248268048));
#214721=CARTESIAN_POINT('Ctrl Pts',(-33.38252812792,75.1466759776841,59.9628200488981));
#214722=CARTESIAN_POINT('Ctrl Pts',(-33.4104438502265,73.895743675265,60.0291940811623));
#214723=CARTESIAN_POINT('Ctrl Pts',(-33.4197640468687,73.4815917907657,
60.0711682248313));
#214724=CARTESIAN_POINT('Ctrl Pts',(-33.4482936853185,72.2192296161529,
60.2606636956289));
#214725=CARTESIAN_POINT('Ctrl Pts',(-33.4670738020269,71.3830744700052,
60.4725694786873));
#214726=CARTESIAN_POINT('Ctrl Pts',(-33.5040917059498,69.8134338164243,
61.0409252526616));
#214727=CARTESIAN_POINT('Ctrl Pts',(-33.522295431567,69.0802262856134,61.3867090959163));
#214728=CARTESIAN_POINT('Ctrl Pts',(-33.5587722675796,67.664970945732,62.2234391375012));
#214729=CARTESIAN_POINT('Ctrl Pts',(-33.5770139445228,66.9886507511057,
62.7167979507159));
#214730=CARTESIAN_POINT('Ctrl Pts',(-33.6049067728145,66.0527525540762,
63.548522294637));
#214731=CARTESIAN_POINT('Ctrl Pts',(-33.6142434667843,65.7546604683032,
63.8402575975047));
#214732=CARTESIAN_POINT('Ctrl Pts',(-33.6427974576095,64.8857802564834,
64.7765230099947));
#214733=CARTESIAN_POINT('Ctrl Pts',(-33.6615862629468,64.3645242570598,
65.4637940548586));
#214734=CARTESIAN_POINT('Ctrl Pts',(-33.6989489141149,63.4840134475982,
66.9009771068278));
#214735=CARTESIAN_POINT('Ctrl Pts',(-33.7175161861705,63.1209666569287,
67.6438747452044));
#214736=CARTESIAN_POINT('Ctrl Pts',(-33.7543538258173,62.5368341013194,
69.1983991292577));
#214737=CARTESIAN_POINT('Ctrl Pts',(-33.7726078614505,62.3190020832833,
70.0071749283648));
#214738=CARTESIAN_POINT('Ctrl Pts',(-33.8005079772522,62.1111595771066,
71.2420763958167));
#214739=CARTESIAN_POINT('Ctrl Pts',(-33.8098397642832,62.0618026721878,
71.6559932981437));
#214740=CARTESIAN_POINT('Ctrl Pts',(-33.8383865660572,61.9716873813061,
72.9298889535711));
#214741=CARTESIAN_POINT('Ctrl Pts',(-33.8571726828789,61.9963379837603,
73.7921242859579));
#214742=CARTESIAN_POINT('Ctrl Pts',(-33.8952999633214,62.2155039798007,
75.4978903519339));
#214743=CARTESIAN_POINT('Ctrl Pts',(-33.9146515593895,62.4092514119537,
76.3372431241239));
#214744=CARTESIAN_POINT('Ctrl Pts',(-33.952282593488,62.9533283389689,77.9470330552479));
#214745=CARTESIAN_POINT('Ctrl Pts',(-33.9706588100548,63.2987482786594,
78.7148129343067));
#214746=CARTESIAN_POINT('Ctrl Pts',(-34.0044349703634,64.05076051187,80.0294294318639));
#214747=CARTESIAN_POINT('Ctrl Pts',(-34.0195937255112,64.4307815671972,
80.5880129367791));
#214748=CARTESIAN_POINT('Ctrl Pts',(-34.043710710607,65.1126285388131,81.4395211765081));
#214749=CARTESIAN_POINT('Ctrl Pts',(-34.0528566123954,65.3882857390685,
81.7517794139277));
#214750=CARTESIAN_POINT('Ctrl Pts',(-34.0820230583186,66.3084077888566,
82.6983197802078));
#214751=CARTESIAN_POINT('Ctrl Pts',(-34.1023028968185,67.0042272195077,
83.2789045014865));
#214752=CARTESIAN_POINT('Ctrl Pts',(-34.1415336101932,68.4681981288636,
84.2616092321369));
#214753=CARTESIAN_POINT('Ctrl Pts',(-34.1602661381447,69.2275293085514,
84.6686683300158));
#214754=CARTESIAN_POINT('Ctrl Pts',(-34.1887163038381,70.4082368105509,
85.1581547938577));
#214755=CARTESIAN_POINT('Ctrl Pts',(-34.1980888677721,70.802536777373,85.299722462373));
#214756=CARTESIAN_POINT('Ctrl Pts',(-34.2266925686778,72.0257499581929,
85.6732864135495));
#214757=CARTESIAN_POINT('Ctrl Pts',(-34.2455035276184,72.8714346049849,
85.8422664987384));
#214758=CARTESIAN_POINT('Ctrl Pts',(-34.2837353197547,74.5892192478275,
86.0112103592344));
#214759=CARTESIAN_POINT('Ctrl Pts',(-34.3032227509619,75.4571569903084,
86.0096644762231));
#214760=CARTESIAN_POINT('Ctrl Pts',(-34.3409734567283,77.1509044130273,
85.8369924861105));
#214761=CARTESIAN_POINT('Ctrl Pts',(-34.3592577985572,77.9732010418807,
85.6719578852339));
#214762=CARTESIAN_POINT('Ctrl Pts',(-34.387174925913,79.1719815355225,85.3082890595779));
#214763=CARTESIAN_POINT('Ctrl Pts',(-34.396493995771,79.5640204239145,85.1684934390129));
#214764=CARTESIAN_POINT('Ctrl Pts',(-34.4250219542817,80.7443686519268,
84.6825903029927));
#214765=CARTESIAN_POINT('Ctrl Pts',(-34.4438015133866,81.5055714903305,
84.2768454927081));
#214766=CARTESIAN_POINT('Ctrl Pts',(-34.4799213390596,82.8600103940223,
83.3720786412212));
#214767=CARTESIAN_POINT('Ctrl Pts',(-34.4971936814308,83.4598341179283,
82.8894741619705));
#214768=CARTESIAN_POINT('Ctrl Pts',(-34.533375927297,84.6326601303735,81.7610094245599));
#214769=CARTESIAN_POINT('Ctrl Pts',(-34.5521118107011,85.1912236252756,
81.1053664772444));
#214770=CARTESIAN_POINT('Ctrl Pts',(-34.5805483990319,85.9191496652819,
80.0561870100941));
#214771=CARTESIAN_POINT('Ctrl Pts',(-34.5899029774701,86.1406073486229,
79.7016676415927));
#214772=CARTESIAN_POINT('Ctrl Pts',(-34.6107233525499,86.5953149174206,
78.8890800648757));
#214773=CARTESIAN_POINT('Ctrl Pts',(-34.6220712822385,86.8191104022253,
78.4268655734703));
#214774=CARTESIAN_POINT('Ctrl Pts',(-34.6333744106366,87.0149197055719,
77.9529305295058));
#214775=CARTESIAN_POINT('',(-33.3112169404745,65.6642757110361,63.9421080804774));
#214776=CARTESIAN_POINT('Ctrl Pts',(-33.3112143094266,65.6642756705897,
63.9421081222156));
#214777=CARTESIAN_POINT('Ctrl Pts',(-33.3011530209772,65.9819378957081,
63.6143001563865));
#214778=CARTESIAN_POINT('Ctrl Pts',(-33.2910793698672,66.3166445043513,
63.3034516989295));
#214779=CARTESIAN_POINT('Ctrl Pts',(-33.2708446150653,67.0148633494904,
62.7203455116794));
#214780=CARTESIAN_POINT('Ctrl Pts',(-33.2606986075489,67.3776751568669,
62.4482270281143));
#214781=CARTESIAN_POINT('Ctrl Pts',(-33.2307671604748,68.488845839857,61.7022445712945));
#214782=CARTESIAN_POINT('Ctrl Pts',(-33.2114320471333,69.2722075581934,
61.2852200541596));
#214783=CARTESIAN_POINT('Ctrl Pts',(-33.1787503430636,70.6373979198212,
60.7285952391906));
#214784=CARTESIAN_POINT('Ctrl Pts',(-33.1655723528332,71.197443039727,60.54350207004));
#214785=CARTESIAN_POINT('Ctrl Pts',(-33.133160570118,72.6015034113583,60.1831278966833));
#214786=CARTESIAN_POINT('Ctrl Pts',(-33.114359740488,73.4540839038891,60.0524888559181));
#214787=CARTESIAN_POINT('Ctrl Pts',(-33.0777586365687,75.1036139273006,
59.9652335843315));
#214788=CARTESIAN_POINT('Ctrl Pts',(-33.0599736298245,75.8960926133116,
59.9956853011575));
#214789=CARTESIAN_POINT('Ctrl Pts',(-33.0252192077184,77.4457428445872,
60.197746707406));
#214790=CARTESIAN_POINT('Ctrl Pts',(-33.0083865484756,78.2002310484827,
60.3653591569273));
#214791=CARTESIAN_POINT('Ctrl Pts',(-32.9752391164359,79.6224206619558,
60.8170839334507));
#214792=CARTESIAN_POINT('Ctrl Pts',(-32.9590265762345,80.2901020089395,
61.092064837245));
#214793=CARTESIAN_POINT('Ctrl Pts',(-32.9255873095396,81.6297955898788,
61.7790023735103));
#214794=CARTESIAN_POINT('Ctrl Pts',(-32.9084557450833,82.2942060404131,
62.1995277917367));
#214795=CARTESIAN_POINT('Ctrl Pts',(-32.8778314769896,83.3865938986748,
63.0382061924307));
#214796=CARTESIAN_POINT('Ctrl Pts',(-32.8645353439765,83.8313399736833,
63.4307261721247));
#214797=CARTESIAN_POINT('Ctrl Pts',(-32.8340356118969,84.7927287577772,
64.4038026238821));
#214798=CARTESIAN_POINT('Ctrl Pts',(-32.8171172936067,85.2872556168821,
65.0030504225077));
#214799=CARTESIAN_POINT('Ctrl Pts',(-32.7829672966371,86.1573694942003,
66.2734299318871));
#214800=CARTESIAN_POINT('Ctrl Pts',(-32.7657834393555,86.5328486269691,
66.9409407885883));
#214801=CARTESIAN_POINT('Ctrl Pts',(-32.7296922896985,87.2011752105809,
68.4205721579918));
#214802=CARTESIAN_POINT('Ctrl Pts',(-32.7109560648433,87.4763561162233,
69.236723973125));
#214803=CARTESIAN_POINT('Ctrl Pts',(-32.6795826241964,87.7922379270936,
70.6096609682824));
#214804=CARTESIAN_POINT('Ctrl Pts',(-32.6672464094614,87.8813806697013,
71.1525590898731));
#214805=CARTESIAN_POINT('Ctrl Pts',(-32.6377909529484,88.0124818817826,
72.4678051521302));
#214806=CARTESIAN_POINT('Ctrl Pts',(-32.6209450117024,88.0204620489175,
73.2414421537243));
#214807=CARTESIAN_POINT('Ctrl Pts',(-32.5863770461848,87.8979292100688,
74.7947794161168));
#214808=CARTESIAN_POINT('Ctrl Pts',(-32.5686903127928,87.7651796837949,
75.5711359094499));
#214809=CARTESIAN_POINT('Ctrl Pts',(-32.5385603550143,87.4161659902799,
76.8831980345399));
#214810=CARTESIAN_POINT('Ctrl Pts',(-32.5260450915273,87.2329982117584,
77.4250953110014));
#214811=CARTESIAN_POINT('Ctrl Pts',(-32.5134098057851,87.0149197055719,
77.9529305295058));
#214812=CARTESIAN_POINT('Ctrl Pts',(-34.3273949797549,87.0149197055719,
77.9529305295058));
#214813=CARTESIAN_POINT('Ctrl Pts',(-34.3222659641844,86.9262956441725,
78.1674353958109));
#214814=CARTESIAN_POINT('Ctrl Pts',(-34.3171225529525,86.8319053648498,
78.3796197710729));
#214815=CARTESIAN_POINT('Ctrl Pts',(-34.2948046279984,86.3993570431063,
79.2857375148203));
#214816=CARTESIAN_POINT('Ctrl Pts',(-34.277429777375,86.0055155106241,79.9512358991139));
#214817=CARTESIAN_POINT('Ctrl Pts',(-34.2483014228856,85.2373570206595,
81.0196149185656));
#214818=CARTESIAN_POINT('Ctrl Pts',(-34.2363710132047,84.892316512885,81.4409960525426));
#214819=CARTESIAN_POINT('Ctrl Pts',(-34.2058500439899,83.9537884077597,
82.4507056320329));
#214820=CARTESIAN_POINT('Ctrl Pts',(-34.1870952982888,83.3281615847613,
83.0057752951113));
#214821=CARTESIAN_POINT('Ctrl Pts',(-34.1511658409779,82.0215106026655,
83.9574819248889));
#214822=CARTESIAN_POINT('Ctrl Pts',(-34.1340977716159,81.3490863657803,
84.3599378215143));
#214823=CARTESIAN_POINT('Ctrl Pts',(-34.099566968348,79.9496049205403,85.0344950070419));
#214824=CARTESIAN_POINT('Ctrl Pts',(-34.082198363434,79.2261880694725,85.306946908301));
#214825=CARTESIAN_POINT('Ctrl Pts',(-34.0531702411385,77.9628688572581,
85.6582519546531));
#214826=CARTESIAN_POINT('Ctrl Pts',(-34.0413343931215,77.4343400645138,
85.770334138519));
#214827=CARTESIAN_POINT('Ctrl Pts',(-34.0108988120774,76.0742343351886,
85.971317396461));
#214828=CARTESIAN_POINT('Ctrl Pts',(-33.9921328797055,75.2382530569122,
86.0135059638339));
#214829=CARTESIAN_POINT('Ctrl Pts',(-33.9556588893021,73.5993996063151,
85.9382949619383));
#214830=CARTESIAN_POINT('Ctrl Pts',(-33.9380867492596,72.7999443211295,
85.8266675374436));
#214831=CARTESIAN_POINT('Ctrl Pts',(-33.9010405308774,71.1784818734973,
85.444265901033));
#214832=CARTESIAN_POINT('Ctrl Pts',(-33.8816911855315,70.362662397949,85.1640901963068));
#214833=CARTESIAN_POINT('Ctrl Pts',(-33.8535228001869,69.2025344330137,
84.6320128779897));
#214834=CARTESIAN_POINT('Ctrl Pts',(-33.844379571971,68.8330790123165,84.4406148964829));
#214835=CARTESIAN_POINT('Ctrl Pts',(-33.8166575402668,67.7495989575,83.8116515107386));
#214836=CARTESIAN_POINT('Ctrl Pts',(-33.7978618271786,67.0680368267213,
83.3225450944089));
#214837=CARTESIAN_POINT('Ctrl Pts',(-33.7597997553321,65.7806670303727,
82.1958171576032));
#214838=CARTESIAN_POINT('Ctrl Pts',(-33.7407550949359,65.1827979707771,
81.555462203927));
#214839=CARTESIAN_POINT('Ctrl Pts',(-33.7021414094037,64.1328765984622,
80.175375567761));
#214840=CARTESIAN_POINT('Ctrl Pts',(-33.682839143146,63.6812806004565,79.4407540146172));
#214841=CARTESIAN_POINT('Ctrl Pts',(-33.6546292299432,63.1225457536784,
78.2899893501863));
#214842=CARTESIAN_POINT('Ctrl Pts',(-33.6454078184583,62.9578599763085,
77.9044202230711));
#214843=CARTESIAN_POINT('Ctrl Pts',(-33.6170767572343,62.5130524810403,
76.7057344151352));
#214844=CARTESIAN_POINT('Ctrl Pts',(-33.5977256972488,62.2946797467361,
75.8722255205868));
#214845=CARTESIAN_POINT('Ctrl Pts',(-33.5580794599566,62.0147439387142,
74.1054476306213));
#214846=CARTESIAN_POINT('Ctrl Pts',(-33.5377636242054,61.9681514221822,
73.1746553003406));
#214847=CARTESIAN_POINT('Ctrl Pts',(-33.508484753883,62.0429790849531,71.8658179188578));
#214848=CARTESIAN_POINT('Ctrl Pts',(-33.4999291116805,62.0815359334979,
71.485903537963));
#214849=CARTESIAN_POINT('Ctrl Pts',(-33.4761071074569,62.2359829592044,
70.4295195145831));
#214850=CARTESIAN_POINT('Ctrl Pts',(-33.4611010983193,62.3887756438287,
69.7597214309783));
#214851=CARTESIAN_POINT('Ctrl Pts',(-33.4236530676507,62.8946047984785,
68.1439051395504));
#214852=CARTESIAN_POINT('Ctrl Pts',(-33.4009695995417,63.3061994461789,
67.2209180035347));
#214853=CARTESIAN_POINT('Ctrl Pts',(-33.3675458891444,64.0778580688789,
65.9205273594993));
#214854=CARTESIAN_POINT('Ctrl Pts',(-33.3564646251883,64.3605967533275,
65.5016986277275));
#214855=CARTESIAN_POINT('Ctrl Pts',(-33.3339968452133,64.9764058514039,
64.6950610429881));
#214856=CARTESIAN_POINT('Ctrl Pts',(-33.3226268060556,65.3094146853376,
64.3083029275426));
#214857=CARTESIAN_POINT('Ctrl Pts',(-33.3112169404745,65.6642757110361,
63.9421080804774));
#214858=CARTESIAN_POINT('Origin',(-21.6548258024609,75.,72.9888893865801));
#214859=CARTESIAN_POINT('',(-36.4473639743914,87.0149197055719,77.9529305295058));
#214860=CARTESIAN_POINT('',(-36.1412950695185,87.0149197055719,77.9529305295058));
#214861=CARTESIAN_POINT('',(-21.6548258024609,87.0149197055719,77.9529305295058));
#214862=CARTESIAN_POINT('Ctrl Pts',(-34.6333744106366,87.0149197055719,
77.9529305295058));
#214863=CARTESIAN_POINT('Ctrl Pts',(-34.6410144983003,87.1472724658191,
77.6325851211187));
#214864=CARTESIAN_POINT('Ctrl Pts',(-34.6486583935817,87.2668387887337,
77.3068853606196));
#214865=CARTESIAN_POINT('Ctrl Pts',(-34.6738484033645,87.6155424360587,
76.2249071553366));
#214866=CARTESIAN_POINT('Ctrl Pts',(-34.6915963640561,87.7887956245091,
75.4527109380275));
#214867=CARTESIAN_POINT('Ctrl Pts',(-34.7263102933153,87.990609401202,73.9048043249291));
#214868=CARTESIAN_POINT('Ctrl Pts',(-34.7431409118189,88.0220646059666,
73.1326648094785));
#214869=CARTESIAN_POINT('Ctrl Pts',(-34.7762781355641,87.9501651988379,
71.6426752970501));
#214870=CARTESIAN_POINT('Ctrl Pts',(-34.7924822107326,87.855676750075,70.9271815437092));
#214871=CARTESIAN_POINT('Ctrl Pts',(-34.8245199274,87.5488040528677,69.5177537052255));
#214872=CARTESIAN_POINT('Ctrl Pts',(-34.8402934076479,87.3367026937042,
68.8263132726193));
#214873=CARTESIAN_POINT('Ctrl Pts',(-34.8734422301321,86.7815923625556,
67.4401181718058));
#214874=CARTESIAN_POINT('Ctrl Pts',(-34.8907994054764,86.4317462687593,
66.7511050424085));
#214875=CARTESIAN_POINT('Ctrl Pts',(-34.9254355268943,85.6039486300616,
65.4270899110364));
#214876=CARTESIAN_POINT('Ctrl Pts',(-34.9427031652308,85.1247666244966,
64.7965975177365));
#214877=CARTESIAN_POINT('Ctrl Pts',(-34.9794395177859,84.010501831775,63.5787263235851));
#214878=CARTESIAN_POINT('Ctrl Pts',(-34.9987656114896,83.3681062130668,
63.0031434726594));
#214879=CARTESIAN_POINT('Ctrl Pts',(-35.0269611300624,82.3363247293893,
62.2486428640155));
#214880=CARTESIAN_POINT('Ctrl Pts',(-35.0361517023222,81.9873840917416,
62.0184281753119));
#214881=CARTESIAN_POINT('Ctrl Pts',(-35.0644318262463,80.8888088134717,
61.3673496404138));
#214882=CARTESIAN_POINT('Ctrl Pts',(-35.0837646192032,80.1080443615473,
61.0036431587081));
#214883=CARTESIAN_POINT('Ctrl Pts',(-35.1199264595917,78.5698626863148,
60.4649172597747));
#214884=CARTESIAN_POINT('Ctrl Pts',(-35.1367626891527,77.8213855619841,
60.2753694849194));
#214885=CARTESIAN_POINT('Ctrl Pts',(-35.1730376670567,76.2109465644052,
60.0168418104364));
#214886=CARTESIAN_POINT('Ctrl Pts',(-35.1923839804659,75.3499051511802,
59.9651423693992));
#214887=CARTESIAN_POINT('Ctrl Pts',(-35.2205570259837,74.074235674986,60.0152174964822));
#214888=CARTESIAN_POINT('Ctrl Pts',(-35.2297080310198,73.6594045914688,
60.0515014820007));
#214889=CARTESIAN_POINT('Ctrl Pts',(-35.2574286343145,72.4182548404463,
60.2204054804586));
#214890=CARTESIAN_POINT('Ctrl Pts',(-35.2762157315111,71.6023019547656,
60.4129114049523));
#214891=CARTESIAN_POINT('Ctrl Pts',(-35.313792459455,70.0030946179789,60.9573297756987));
#214892=CARTESIAN_POINT('Ctrl Pts',(-35.3323865847917,69.2246777222068,
61.3109979269255));
#214893=CARTESIAN_POINT('Ctrl Pts',(-35.3705224383085,67.7419341476506,
62.1694287967758));
#214894=CARTESIAN_POINT('Ctrl Pts',(-35.3898426629352,67.0419700700413,
62.6733662263117));
#214895=CARTESIAN_POINT('Ctrl Pts',(-35.4180426922991,66.0834484591887,
63.5194670460732));
#214896=CARTESIAN_POINT('Ctrl Pts',(-35.4272420435321,65.7834928920688,
63.8111528869795));
#214897=CARTESIAN_POINT('Ctrl Pts',(-35.4555365738423,64.9116654239943,
64.7448662934268));
#214898=CARTESIAN_POINT('Ctrl Pts',(-35.4748750176126,64.3889339507664,
65.4295455466578));
#214899=CARTESIAN_POINT('Ctrl Pts',(-35.5114915870395,63.521864149559,66.8343076002342));
#214900=CARTESIAN_POINT('Ctrl Pts',(-35.5287861377058,63.1685136464488,
67.544404319794));
#214901=CARTESIAN_POINT('Ctrl Pts',(-35.5655511234903,62.5704350035212,
69.0842496789816));
#214902=CARTESIAN_POINT('Ctrl Pts',(-35.5848757371742,62.3393145831473,
69.915234724591));
#214903=CARTESIAN_POINT('Ctrl Pts',(-35.6130724628373,62.1204346444043,
71.174659599355));
#214904=CARTESIAN_POINT('Ctrl Pts',(-35.622265337517,62.0687744297023,71.5895901190422));
#214905=CARTESIAN_POINT('Ctrl Pts',(-35.6505492332774,61.9722424867744,
72.8630698276623));
#214906=CARTESIAN_POINT('Ctrl Pts',(-35.6698835404298,61.9924009342307,
73.7241800810811));
#214907=CARTESIAN_POINT('Ctrl Pts',(-35.7061605490294,62.1921485258402,
75.3470532185749));
#214908=CARTESIAN_POINT('Ctrl Pts',(-35.7231128405259,62.3556818101983,
76.1070973531199));
#214909=CARTESIAN_POINT('Ctrl Pts',(-35.7595123308866,62.8414434762071,
77.6696915924371));
#214910=CARTESIAN_POINT('Ctrl Pts',(-35.7788538220983,63.1778294579789,
78.4639875642219));
#214911=CARTESIAN_POINT('Ctrl Pts',(-35.8070334432503,63.7898918328367,
79.5848776875493));
#214912=CARTESIAN_POINT('Ctrl Pts',(-35.8161955881248,64.0070310580069,
79.9407395369645));
#214913=CARTESIAN_POINT('Ctrl Pts',(-35.8439134553117,64.709891921015,80.9771250993757));
#214914=CARTESIAN_POINT('Ctrl Pts',(-35.8626874295874,65.2444848391333,
81.6218577646133));
#214915=CARTESIAN_POINT('Ctrl Pts',(-35.8995680876586,66.4210303757784,
82.7908559751471));
#214916=CARTESIAN_POINT('Ctrl Pts',(-35.9175169075991,67.0585854030976,
83.3141598198811));
#214917=CARTESIAN_POINT('Ctrl Pts',(-35.9549652982439,68.4551599768391,
84.2541222654419));
#214918=CARTESIAN_POINT('Ctrl Pts',(-35.9743055043938,69.2149449454332,
84.6625156941114));
#214919=CARTESIAN_POINT('Ctrl Pts',(-36.0024867255381,70.3943086154943,
85.152823300772));
#214920=CARTESIAN_POINT('Ctrl Pts',(-36.0116516207469,70.7865987406913,
85.2942106379164));
#214921=CARTESIAN_POINT('Ctrl Pts',(-36.0393686835006,71.9836159836327,
85.6616679382997));
#214922=CARTESIAN_POINT('Ctrl Pts',(-36.0581392723562,72.8039998782774,
85.8292732298157));
#214923=CARTESIAN_POINT('Ctrl Pts',(-36.0948471064515,74.4457882050427,
86.0026489020353));
#214924=CARTESIAN_POINT('Ctrl Pts',(-36.1126358225816,75.2630700598925,
86.0117879939816));
#214925=CARTESIAN_POINT('Ctrl Pts',(-36.1499133284127,76.9333250757294,
85.8730915011334));
#214926=CARTESIAN_POINT('Ctrl Pts',(-36.169257629372,77.7816622711618,85.7169204670744));
#214927=CARTESIAN_POINT('Ctrl Pts',(-36.1974335359189,79.0083435510802,
85.3625125683815));
#214928=CARTESIAN_POINT('Ctrl Pts',(-36.2065893584936,79.4025750479469,
85.2277905438018));
#214929=CARTESIAN_POINT('Ctrl Pts',(-36.2343088797544,80.5669144822184,
84.7663455979332));
#214930=CARTESIAN_POINT('Ctrl Pts',(-36.2530904160522,81.3126370513456,
84.384046693144));
#214931=CARTESIAN_POINT('Ctrl Pts',(-36.2903666117951,82.7235994368813,
83.4794370187516));
#214932=CARTESIAN_POINT('Ctrl Pts',(-36.3086820169662,83.3851307160123,
82.9586018770635));
#214933=CARTESIAN_POINT('Ctrl Pts',(-36.3465212556786,84.6131905871474,
81.7824614731507));
#214934=CARTESIAN_POINT('Ctrl Pts',(-36.3658508378358,85.1739860388722,
81.1270932549301));
#214935=CARTESIAN_POINT('Ctrl Pts',(-36.3940433126084,85.9046378054383,
80.0785465049186));
#214936=CARTESIAN_POINT('Ctrl Pts',(-36.4032281993759,86.1267213877352,
79.7246472984632));
#214937=CARTESIAN_POINT('Ctrl Pts',(-36.4240420244147,86.5874331272118,
78.9053318148693));
#214938=CARTESIAN_POINT('Ctrl Pts',(-36.4356882939277,86.8156600708001,
78.4352167240423));
#214939=CARTESIAN_POINT('Ctrl Pts',(-36.4473639743914,87.0149197055719,
77.9529305295058));
#214940=CARTESIAN_POINT('Ctrl Pts',(-36.1412950695185,87.0149197055719,
77.9529305295058));
#214941=CARTESIAN_POINT('Ctrl Pts',(-36.1298525502738,86.8196408780571,
78.4255816146268));
#214942=CARTESIAN_POINT('Ctrl Pts',(-36.1184583697883,86.596525045201,78.8865806401068));
#214943=CARTESIAN_POINT('Ctrl Pts',(-36.0979502789332,86.1427955726876,
79.6980294853537));
#214944=CARTESIAN_POINT('Ctrl Pts',(-36.0887627234461,85.9214998403717,
80.0525495586229));
#214945=CARTESIAN_POINT('Ctrl Pts',(-36.0604875345434,85.1939912928237,
81.1018877762301));
#214946=CARTESIAN_POINT('Ctrl Pts',(-36.0411567591015,84.6356671185127,
81.7577039567634));
#214947=CARTESIAN_POINT('Ctrl Pts',(-36.005141592816,83.4665101443726,82.8834150940506));
#214948=CARTESIAN_POINT('Ctrl Pts',(-35.98845316749,82.8706522301808,83.3636796878424));
#214949=CARTESIAN_POINT('Ctrl Pts',(-35.9542340749897,81.5921201549929,
84.2203098349429));
#214950=CARTESIAN_POINT('Ctrl Pts',(-35.9367849374459,80.910852539125,84.593314433653));
#214951=CARTESIAN_POINT('Ctrl Pts',(-35.9065947946083,79.6601739007216,
85.1392086270328));
#214952=CARTESIAN_POINT('Ctrl Pts',(-35.8936717608624,79.1045078316714,
85.3379984858156));
#214953=CARTESIAN_POINT('Ctrl Pts',(-35.8631504302149,77.7800427230511,
85.7125134755317));
#214954=CARTESIAN_POINT('Ctrl Pts',(-35.845451574069,77.004936163505,85.857435042336));
#214955=CARTESIAN_POINT('Ctrl Pts',(-35.8119077179347,75.5013839149763,
85.9993391579588));
#214956=CARTESIAN_POINT('Ctrl Pts',(-35.7961055627523,74.7768473497895,
86.0070843132759));
#214957=CARTESIAN_POINT('Ctrl Pts',(-35.7629303782296,73.2864365511284,
85.898505926007));
#214958=CARTESIAN_POINT('Ctrl Pts',(-35.7455770786224,72.5239468151579,
85.7741799727015));
#214959=CARTESIAN_POINT('Ctrl Pts',(-35.7108868074003,71.0087798231814,
85.3864273950003));
#214960=CARTESIAN_POINT('Ctrl Pts',(-35.6935603236903,70.2601713027601,
85.1199577033177));
#214961=CARTESIAN_POINT('Ctrl Pts',(-35.6567613902556,68.7596768214792,
84.4256128919062));
#214962=CARTESIAN_POINT('Ctrl Pts',(-35.6374385692242,68.0166264949497,
83.9876521989185));
#214963=CARTESIAN_POINT('Ctrl Pts',(-35.6092404454297,66.9849945013812,
83.2326392530982));
#214964=CARTESIAN_POINT('Ctrl Pts',(-35.6000448638896,66.6597835518844,
82.9696465609767));
#214965=CARTESIAN_POINT('Ctrl Pts',(-35.5717565278372,65.706492535983,82.1195554927621));
#214966=CARTESIAN_POINT('Ctrl Pts',(-35.5524204694709,65.123457971628,81.4854917713839));
#214967=CARTESIAN_POINT('Ctrl Pts',(-35.5160044050387,64.1373087680155,
80.1731712204565));
#214968=CARTESIAN_POINT('Ctrl Pts',(-35.4989119659459,63.7247642495407,
79.506636882953));
#214969=CARTESIAN_POINT('Ctrl Pts',(-35.4623624821328,62.9895514411598,
78.0376027251217));
#214970=CARTESIAN_POINT('Ctrl Pts',(-35.443027406734,62.6817967463728,77.2317964309454));
#214971=CARTESIAN_POINT('Ctrl Pts',(-35.4148403435027,62.3464065441204,
75.9989730879931));
#214972=CARTESIAN_POINT('Ctrl Pts',(-35.4056652342491,62.2563351350567,
75.5913952682117));
#214973=CARTESIAN_POINT('Ctrl Pts',(-35.3779516248455,62.0453332897541,
74.3575303193435));
#214974=CARTESIAN_POINT('Ctrl Pts',(-35.3591941342385,61.9842008020369,
73.5232338078267));
#214975=CARTESIAN_POINT('Ctrl Pts',(-35.3231332769107,62.0216426046779,
71.9013533735228));
#214976=CARTESIAN_POINT('Ctrl Pts',(-35.3059436051296,62.1113612201544,
71.1171275422089));
#214977=CARTESIAN_POINT('Ctrl Pts',(-35.2712619618553,62.4285603751698,
69.5895374388546));
#214978=CARTESIAN_POINT('Ctrl Pts',(-35.2538720381301,62.6527066399022,
68.8487156849491));
#214979=CARTESIAN_POINT('Ctrl Pts',(-35.2245121001951,63.148280938239,67.6182535143398));
#214980=CARTESIAN_POINT('Ctrl Pts',(-35.212363927004,63.3879146739514,67.1180759417574));
#214981=CARTESIAN_POINT('Ctrl Pts',(-35.1810619263656,64.0787253779095,
65.8850795563455));
#214982=CARTESIAN_POINT('Ctrl Pts',(-35.1617255453019,64.5720124689809,
65.1789329448341));
#214983=CARTESIAN_POINT('Ctrl Pts',(-35.1252831314442,65.641357267583,63.9318661176365));
#214984=CARTESIAN_POINT('Ctrl Pts',(-35.1081641341423,66.2040941070758,
63.384415887291));
#214985=CARTESIAN_POINT('Ctrl Pts',(-35.0715862747248,67.4810526523204,
62.3490677629285));
#214986=CARTESIAN_POINT('Ctrl Pts',(-35.0522524904512,68.2015736270285,
61.874853984205));
#214987=CARTESIAN_POINT('Ctrl Pts',(-35.0240640822832,69.3332023665428,
61.2815618711429));
#214988=CARTESIAN_POINT('Ctrl Pts',(-35.0148865760114,69.7118740965361,
61.1057148441394));
#214989=CARTESIAN_POINT('Ctrl Pts',(-34.9871738864033,70.871174050503,60.6337671809289));
#214990=CARTESIAN_POINT('Ctrl Pts',(-34.9684195930582,71.6724955656291,
60.3942894384212));
#214991=CARTESIAN_POINT('Ctrl Pts',(-34.9325116520515,73.2576783180675,
60.0825148469752));
#214992=CARTESIAN_POINT('Ctrl Pts',(-34.9154634923922,74.0361699556754,
60.0011556725565));
#214993=CARTESIAN_POINT('Ctrl Pts',(-34.8809570298485,75.5885194412834,
59.979330204309));
#214994=CARTESIAN_POINT('Ctrl Pts',(-34.8635915756472,76.3592323104988,
60.0371529876881));
#214995=CARTESIAN_POINT('Ctrl Pts',(-34.8346151917973,77.6505818690484,
60.2506263943429));
#214996=CARTESIAN_POINT('Ctrl Pts',(-34.8228282368789,78.1749578050771,
60.3711014270372));
#214997=CARTESIAN_POINT('Ctrl Pts',(-34.7924368846693,79.491455892608,60.760855423949));
#214998=CARTESIAN_POINT('Ctrl Pts',(-34.7736652954155,80.2678135037159,
61.0746912797687));
#214999=CARTESIAN_POINT('Ctrl Pts',(-34.7369066461279,81.7337947492177,
61.8387922762775));
#215000=CARTESIAN_POINT('Ctrl Pts',(-34.7190708588111,82.4216467956235,
62.2843192095421));
#215001=CARTESIAN_POINT('Ctrl Pts',(-34.6817431027039,83.7380427758999,
63.3251935441175));
#215002=CARTESIAN_POINT('Ctrl Pts',(-34.6623999726677,84.35835774346,63.9245880071219));
#215003=CARTESIAN_POINT('Ctrl Pts',(-34.6342224804547,85.1842612527145,
64.8985071785536));
#215004=CARTESIAN_POINT('Ctrl Pts',(-34.6250639691175,85.4382125726879,
65.2289164659393));
#215005=CARTESIAN_POINT('Ctrl Pts',(-34.5973451184325,86.1528232112991,
66.2573800370101));
#215006=CARTESIAN_POINT('Ctrl Pts',(-34.5785667610308,86.5624635873858,
66.9882140541144));
#215007=CARTESIAN_POINT('Ctrl Pts',(-34.541458538371,87.2344805718937,68.5155273723569));
#215008=CARTESIAN_POINT('Ctrl Pts',(-34.5232988409555,87.4958477473876,
69.308226663165));
#215009=CARTESIAN_POINT('Ctrl Pts',(-34.4856255323828,87.869451885214,70.9597061078104));
#215010=CARTESIAN_POINT('Ctrl Pts',(-34.4662912175051,87.9755189309129,
71.8157330745989));
#215011=CARTESIAN_POINT('Ctrl Pts',(-34.4381033563664,88.0062765790443,
73.0930489463427));
#215012=CARTESIAN_POINT('Ctrl Pts',(-34.4289268273952,87.9962343871544,
73.5103979950093));
#215013=CARTESIAN_POINT('Ctrl Pts',(-34.4012137576439,87.9059515380183,
74.7588594088365));
#215014=CARTESIAN_POINT('Ctrl Pts',(-34.3824581549403,87.7657603498323,
75.5834465426814));
#215015=CARTESIAN_POINT('Ctrl Pts',(-34.3516509315271,87.4032629321684,
76.9212247748124));
#215016=CARTESIAN_POINT('Ctrl Pts',(-34.3395731065913,87.2253450875266,
77.4436188627799));
#215017=CARTESIAN_POINT('Ctrl Pts',(-34.3273949797549,87.0149197055719,
77.9529305295058));
#215018=CARTESIAN_POINT('Origin',(-21.6548258024609,75.,72.9888893865801));
#215019=CARTESIAN_POINT('',(-39.5675364832709,87.0149197055719,77.9529305295058));
#215020=CARTESIAN_POINT('',(-39.5675364832709,79.9640411429257,60.9739696810082));
#215021=CARTESIAN_POINT('Origin',(-39.5675364832709,75.,72.9888893865801));
#215022=CARTESIAN_POINT('Origin',(-39.5675364832709,75.,72.9888893865801));
#215023=CARTESIAN_POINT('',(-39.3655152556871,87.0149196672213,77.9529306223295));
#215024=CARTESIAN_POINT('',(-21.6548258024609,87.0149197055719,77.9529305295058));
#215025=CARTESIAN_POINT('',(-39.378281183842,87.9789324623827,72.2490839199061));
#215026=CARTESIAN_POINT('Ctrl Pts',(-39.3655152559408,87.014919667221,77.9529306223301));
#215027=CARTESIAN_POINT('Ctrl Pts',(-39.367974326097,87.3865627273345,77.0534091840337));
#215028=CARTESIAN_POINT('Ctrl Pts',(-39.3710406973607,87.6560163266104,
76.1149984769994));
#215029=CARTESIAN_POINT('Ctrl Pts',(-39.3753005433957,87.9804112067045,
74.1956296276193));
#215030=CARTESIAN_POINT('Ctrl Pts',(-39.376513824047,88.0343195956285,73.2207797100457));
#215031=CARTESIAN_POINT('Ctrl Pts',(-39.3782811843755,87.9789324627048,
72.2490839198887));
#215032=CARTESIAN_POINT('',(-38.9114901702032,87.9789324623618,72.2490839198538));
#215033=CARTESIAN_POINT('',(-38.9115960243709,87.9789324627076,72.2490839198856));
#215034=CARTESIAN_POINT('',(-38.6651607695591,87.0149202732382,77.9529291555314));
#215035=CARTESIAN_POINT('Ctrl Pts',(-38.9114901696398,87.9789324627004,
72.2490839198105));
#215036=CARTESIAN_POINT('Ctrl Pts',(-38.87002296087,88.0343175630345,73.2207440507034));
#215037=CARTESIAN_POINT('Ctrl Pts',(-38.8281416219942,87.9804138359084,
74.1955869480231));
#215038=CARTESIAN_POINT('Ctrl Pts',(-38.7459661857041,87.6560286922808,
76.1149524347907));
#215039=CARTESIAN_POINT('Ctrl Pts',(-38.7059499709518,87.3865732800262,
77.0533833312218));
#215040=CARTESIAN_POINT('Ctrl Pts',(-38.6651607695591,87.0149202732382,
77.9529291555314));
#215041=CARTESIAN_POINT('',(-37.9553013386749,87.0149197239183,77.9529304851004));
#215042=CARTESIAN_POINT('',(-21.6548258024609,87.0149197055719,77.9529305295058));
#215043=CARTESIAN_POINT('',(-39.3215010433097,70.2740072122874,85.0994220373138));
#215044=CARTESIAN_POINT('Ctrl Pts',(-39.321506023786,70.2738583024975,85.099363557938));
#215045=CARTESIAN_POINT('Ctrl Pts',(-39.3114020880209,69.8468174583147,
84.9327098405302));
#215046=CARTESIAN_POINT('Ctrl Pts',(-39.3012855729604,69.4288913059223,
84.7435856333423));
#215047=CARTESIAN_POINT('Ctrl Pts',(-39.280963349317,68.6176528904388,84.3234743085914));
#215048=CARTESIAN_POINT('Ctrl Pts',(-39.2707729228055,68.2247471115269,
84.0930830360041));
#215049=CARTESIAN_POINT('Ctrl Pts',(-39.2407041203334,67.1021730628955,
83.3530282551602));
#215050=CARTESIAN_POINT('Ctrl Pts',(-39.2212815979088,66.4118048498001,
82.7885807671965));
#215051=CARTESIAN_POINT('Ctrl Pts',(-39.1884559885027,65.3675884171679,
81.7390900665183));
#215052=CARTESIAN_POINT('Ctrl Pts',(-39.1752312649901,64.9797544211849,
81.2921440976121));
#215053=CARTESIAN_POINT('Ctrl Pts',(-39.1427805644905,64.1053250437752,
80.1335688480066));
#215054=CARTESIAN_POINT('Ctrl Pts',(-39.1239870143577,63.6564342372199,
79.3970017841523));
#215055=CARTESIAN_POINT('Ctrl Pts',(-39.0864295461419,62.9222219147695,
77.8697693025234));
#215056=CARTESIAN_POINT('Ctrl Pts',(-39.0676566045221,62.63401471161,77.0849988222401));
#215057=CARTESIAN_POINT('Ctrl Pts',(-39.030614924758,62.2114826142195,75.4693290884284));
#215058=CARTESIAN_POINT('Ctrl Pts',(-39.012353616074,62.0784797054115,74.6420922817204));
#215059=CARTESIAN_POINT('Ctrl Pts',(-38.9844493981105,61.9995852932347,
73.3921966966507));
#215060=CARTESIAN_POINT('Ctrl Pts',(-38.9751206225394,61.9933378521099,
72.9755430471695));
#215061=CARTESIAN_POINT('Ctrl Pts',(-38.946578292483,62.0355334386009,71.6993073294617));
#215062=CARTESIAN_POINT('Ctrl Pts',(-38.9277937808025,62.1492825577064,
70.8442501044364));
#215063=CARTESIAN_POINT('Ctrl Pts',(-38.8915606746817,62.5241755004248,
69.2535805458345));
#215064=CARTESIAN_POINT('Ctrl Pts',(-38.8741679040607,62.7685641781066,
68.5177937551494));
#215065=CARTESIAN_POINT('Ctrl Pts',(-38.8378616598784,63.4193471623844,
67.0200742385238));
#215066=CARTESIAN_POINT('Ctrl Pts',(-38.8191262125368,63.8390537658709,
66.2679101802637));
#215067=CARTESIAN_POINT('Ctrl Pts',(-38.790688162261,64.568589507438,65.2197014772622));
#215068=CARTESIAN_POINT('Ctrl Pts',(-38.7813317124692,64.823687144539,64.888441178162));
#215069=CARTESIAN_POINT('Ctrl Pts',(-38.7527494948693,65.6514972276645,
63.9144306783834));
#215070=CARTESIAN_POINT('Ctrl Pts',(-38.7339489678599,66.272414068001,63.3157538675906));
#215071=CARTESIAN_POINT('Ctrl Pts',(-38.6961323116346,67.6122913153949,
62.258655584523));
#215072=CARTESIAN_POINT('Ctrl Pts',(-38.6770852008029,68.32626924716,61.8006157399202));
#215073=CARTESIAN_POINT('Ctrl Pts',(-38.649063492353,69.4511464508941,61.2252027944466));
#215074=CARTESIAN_POINT('Ctrl Pts',(-38.6398975354063,69.8315507630826,
61.0531769281282));
#215075=CARTESIAN_POINT('Ctrl Pts',(-38.609331741426,71.1197986245397,60.5437628631491));
#215076=CARTESIAN_POINT('Ctrl Pts',(-38.5876505567486,72.0569819038552,
60.2894501687834));
#215077=CARTESIAN_POINT('Ctrl Pts',(-38.5489686896933,73.7739355034221,
60.023990570254));
#215078=CARTESIAN_POINT('Ctrl Pts',(-38.5321845447893,74.5431454813509,
59.9741622638402));
#215079=CARTESIAN_POINT('Ctrl Pts',(-38.5008117355056,75.9561224552041,
60.0081089072099));
#215080=CARTESIAN_POINT('Ctrl Pts',(-38.4863650581999,76.5979715007598,
60.0714084547044));
#215081=CARTESIAN_POINT('Ctrl Pts',(-38.4626017641503,77.6473753072034,
60.2543388149753));
#215082=CARTESIAN_POINT('Ctrl Pts',(-38.4533157484133,78.0585156925993,
60.3467828974843));
#215083=CARTESIAN_POINT('Ctrl Pts',(-38.4164245293697,79.6716516533196,
60.7928065998949));
#215084=CARTESIAN_POINT('Ctrl Pts',(-38.3883367518857,80.8243084251877,
61.2993133040721));
#215085=CARTESIAN_POINT('Ctrl Pts',(-38.3514289180863,82.2397648680118,
62.1833742844974));
#215086=CARTESIAN_POINT('Ctrl Pts',(-38.3422820314882,82.5821013107596,
62.4207726013387));
#215087=CARTESIAN_POINT('Ctrl Pts',(-38.3129369998464,83.636119886382,63.2293150724732));
#215088=CARTESIAN_POINT('Ctrl Pts',(-38.2924757734087,84.2993534094154,
63.8590557240803));
#215089=CARTESIAN_POINT('Ctrl Pts',(-38.2530563239258,85.4489216617826,
65.2069402920131));
#215090=CARTESIAN_POINT('Ctrl Pts',(-38.2343240422644,85.9404230632382,
65.9145806437461));
#215091=CARTESIAN_POINT('Ctrl Pts',(-38.2058724294769,86.5621961834555,
67.0314554614813));
#215092=CARTESIAN_POINT('Ctrl Pts',(-38.1964978479394,86.7481070142651,
67.4070097828176));
#215093=CARTESIAN_POINT('Ctrl Pts',(-38.1678916339641,87.2595380844619,
68.5793797065549));
#215094=CARTESIAN_POINT('Ctrl Pts',(-38.1490793502634,87.5243955576249,
69.4000778515985));
#215095=CARTESIAN_POINT('Ctrl Pts',(-38.1107919550294,87.8898085558847,
71.0896871066573));
#215096=CARTESIAN_POINT('Ctrl Pts',(-38.0912453846014,87.987865078529,71.9547294911018));
#215097=CARTESIAN_POINT('Ctrl Pts',(-38.0534359995219,88.0096166010421,
73.6598078459812));
#215098=CARTESIAN_POINT('Ctrl Pts',(-38.03514977022,87.9394741214373,74.4956319081321));
#215099=CARTESIAN_POINT('Ctrl Pts',(-38.0072316254609,87.7149408798079,
75.72810147097));
#215100=CARTESIAN_POINT('Ctrl Pts',(-37.9979133811153,87.6207958687613,
76.1334903360733));
#215101=CARTESIAN_POINT('Ctrl Pts',(-37.9774099080487,87.3706399895231,
77.0161397197716));
#215102=CARTESIAN_POINT('Ctrl Pts',(-37.966341833165,87.2061795722548,77.4900068955137));
#215103=CARTESIAN_POINT('Ctrl Pts',(-37.9553013376164,87.0149197239272,
77.9529304850788));
#215104=CARTESIAN_POINT('Ctrl Pts',(-39.3215011869246,70.2741248823959,
85.0994675880043));
#215105=CARTESIAN_POINT('Ctrl Pts',(-39.3236712637677,71.0632752616707,
85.4074154067983));
#215106=CARTESIAN_POINT('Ctrl Pts',(-39.3262569458996,71.880640057225,85.6374944349641));
#215107=CARTESIAN_POINT('Ctrl Pts',(-39.3301175566085,73.5347367964358,
85.9328892466978));
#215108=CARTESIAN_POINT('Ctrl Pts',(-39.3314200360407,74.3670796427984,
86.0001740554811));
#215109=CARTESIAN_POINT('Ctrl Pts',(-39.3355204404005,76.8868812019081,
85.9613804639162));
#215110=CARTESIAN_POINT('Ctrl Pts',(-39.3415199539802,78.5525524484387,
85.6073365102985));
#215111=CARTESIAN_POINT('Ctrl Pts',(-39.3463525919956,80.8711551225581,
84.617527519692));
#215112=CARTESIAN_POINT('Ctrl Pts',(-39.3473555822715,81.6049539354431,
84.2169902570333));
#215113=CARTESIAN_POINT('Ctrl Pts',(-39.3513429793926,83.3501269679487,
83.0337632759548));
#215114=CARTESIAN_POINT('Ctrl Pts',(-39.3558794304814,84.2940584038291,
82.1673740340381));
#215115=CARTESIAN_POINT('Ctrl Pts',(-39.3612997924158,85.8887379039215,
80.2011041664733));
#215116=CARTESIAN_POINT('Ctrl Pts',(-39.3623386985112,86.5348437171632,
79.1149045610223));
#215117=CARTESIAN_POINT('Ctrl Pts',(-39.3655152812068,87.0149234856985,
77.9529213801122));
#215118=CARTESIAN_POINT('Origin',(-23.4378585958609,75.,72.9888893865801));
#215119=CARTESIAN_POINT('',(-23.3083467243891,86.7753674719618,77.8539778944305));
#215120=CARTESIAN_POINT('',(-23.4378585958609,86.8950725984871,77.9034149284857));
#215121=CARTESIAN_POINT('',(-23.5671968062386,81.7816282713719,84.0797707272729));
#215122=CARTESIAN_POINT('Ctrl Pts',(-23.5672140314447,81.7816648771554,
84.07983260589));
#215123=CARTESIAN_POINT('Ctrl Pts',(-23.5673199177301,81.7897993012429,
84.0748587333312));
#215124=CARTESIAN_POINT('Ctrl Pts',(-23.5674258040155,81.7979282533515,
84.0698759117298));
#215125=CARTESIAN_POINT('Ctrl Pts',(-23.5675316903009,81.8060517138039,
84.0648841531474));
#215126=CARTESIAN_POINT('',(-22.5675364824894,86.9998979375059,73.039443228467));
#215127=CARTESIAN_POINT('Ctrl Pts',(-23.5671139309304,81.7814521506577,
84.0794730118532));
#215128=CARTESIAN_POINT('Ctrl Pts',(-23.5554441969661,81.093704963152,84.4863247226582));
#215129=CARTESIAN_POINT('Ctrl Pts',(-23.5440549453205,80.3694906051007,
84.8293747514794));
#215130=CARTESIAN_POINT('Ctrl Pts',(-23.5205294743054,78.8459785012502,
85.3850651834404));
#215131=CARTESIAN_POINT('Ctrl Pts',(-23.5081796031132,78.0485116703269,
85.5920974487081));
#215132=CARTESIAN_POINT('Ctrl Pts',(-23.4721296505078,75.648480810247,85.9772996965804));
#215133=CARTESIAN_POINT('Ctrl Pts',(-23.4493257715469,74.0212183490508,
85.9346245406178));
#215134=CARTESIAN_POINT('Ctrl Pts',(-23.400751606844,70.8562592203477,85.2427926589502));
#215135=CARTESIAN_POINT('Ctrl Pts',(-23.3776454762802,69.3427417189109,
84.5970625631213));
#215136=CARTESIAN_POINT('Ctrl Pts',(-23.3403526762987,67.289062705934,83.2069683034419));
#215137=CARTESIAN_POINT('Ctrl Pts',(-23.3274897439033,66.633733857187,82.6607486085187));
#215138=CARTESIAN_POINT('Ctrl Pts',(-23.3030014708832,65.4741786697172,
81.4799624604395));
#215139=CARTESIAN_POINT('Ctrl Pts',(-23.2913605641576,64.9652158093804,
80.8531966773066));
#215140=CARTESIAN_POINT('Ctrl Pts',(-23.273148804062,64.2923408780737,79.8406857186491));
#215141=CARTESIAN_POINT('Ctrl Pts',(-23.266907699706,64.0819260352267,79.4879801447772));
#215142=CARTESIAN_POINT('Ctrl Pts',(-23.2363418036894,63.135444316788,77.7111294603452));
#215143=CARTESIAN_POINT('Ctrl Pts',(-23.2132436084909,62.6532773507385,
76.1605022589756));
#215144=CARTESIAN_POINT('Ctrl Pts',(-23.1759412452441,62.3852856750543,
73.7273574819093));
#215145=CARTESIAN_POINT('Ctrl Pts',(-23.1630923328798,62.376935370315,72.8851889496607));
#215146=CARTESIAN_POINT('Ctrl Pts',(-23.1386272326454,62.5232656519847,
71.2588084415987));
#215147=CARTESIAN_POINT('Ctrl Pts',(-23.1269905153999,62.6689014872749,
70.4759290443836));
#215148=CARTESIAN_POINT('Ctrl Pts',(-23.1023462125105,63.1162283208151,
68.9167373502686));
#215149=CARTESIAN_POINT('Ctrl Pts',(-23.0894884991716,63.4231978635774,
68.1451374417189));
#215150=CARTESIAN_POINT('Ctrl Pts',(-23.064779964354,64.1707164063792,66.7003125165312));
#215151=CARTESIAN_POINT('Ctrl Pts',(-23.0529403525713,64.6051802209593,
66.0267421448527));
#215152=CARTESIAN_POINT('Ctrl Pts',(-23.0283692983427,65.6150627386631,
64.7498100788519));
#215153=CARTESIAN_POINT('Ctrl Pts',(-23.0154222549054,66.1928994922378,
64.1532084285951));
#215154=CARTESIAN_POINT('Ctrl Pts',(-22.9905384216501,67.4277670869574,
63.108792457982));
#215155=CARTESIAN_POINT('Ctrl Pts',(-22.9786497998762,68.0785768235615,
62.6567224664561));
#215156=CARTESIAN_POINT('Ctrl Pts',(-22.9417990983282,70.2075954434887,
61.4614169297251));
#215157=CARTESIAN_POINT('Ctrl Pts',(-22.9159564408367,71.7892810380742,
60.9523140322329));
#215158=CARTESIAN_POINT('Ctrl Pts',(-22.8848941253732,73.8228050179139,
60.7213246443219));
#215159=CARTESIAN_POINT('Ctrl Pts',(-22.8788053233582,74.2242359646979,
60.6955106593124));
#215160=CARTESIAN_POINT('Ctrl Pts',(-22.8601629334116,75.4343458629007,
60.6773776226708));
#215161=CARTESIAN_POINT('Ctrl Pts',(-22.8473408710597,76.2422172252888,
60.7453967284844));
#215162=CARTESIAN_POINT('Ctrl Pts',(-22.822646349902,77.8052043610332,61.0335899700925));
#215163=CARTESIAN_POINT('Ctrl Pts',(-22.8107879232795,78.559075510394,61.2483269085615));
#215164=CARTESIAN_POINT('Ctrl Pts',(-22.7739585650263,80.7943332456824,
62.1240879218893));
#215165=CARTESIAN_POINT('Ctrl Pts',(-22.7483049277878,82.1656766468166,
63.0075631318245));
#215166=CARTESIAN_POINT('Ctrl Pts',(-22.6985290046578,84.4883882135417,
65.2585150327436));
#215167=CARTESIAN_POINT('Ctrl Pts',(-22.6726909441824,85.4096795911242,
66.6031378681074));
#215168=CARTESIAN_POINT('Ctrl Pts',(-22.6412225596302,86.2045837909721,
68.4717174240305));
#215169=CARTESIAN_POINT('Ctrl Pts',(-22.6347891537383,86.3477834654584,
68.8633544227412));
#215170=CARTESIAN_POINT('Ctrl Pts',(-22.6081787237398,86.8465827549896,
70.4844388954695));
#215171=CARTESIAN_POINT('Ctrl Pts',(-22.5874829697694,87.0252275441048,
71.7617031373274));
#215172=CARTESIAN_POINT('Ctrl Pts',(-22.5675364824894,86.9998979375059,
73.039443228467));
#215173=CARTESIAN_POINT('',(-22.5675364829333,74.3890640007607,84.9729941181989));
#215174=CARTESIAN_POINT('Origin',(-22.5675364832709,75.,72.98888938658));
#215175=CARTESIAN_POINT('Ctrl Pts',(-22.5675364828275,74.3890709851988,
84.9733322994732));
#215176=CARTESIAN_POINT('Ctrl Pts',(-22.582124664134,74.6718425512144,85.0023542290884));
#215177=CARTESIAN_POINT('Ctrl Pts',(-22.5966303455749,74.9561571119262,
85.0212811334547));
#215178=CARTESIAN_POINT('Ctrl Pts',(-22.6110726647668,75.2412883501049,
85.0300127005125));
#215179=CARTESIAN_POINT('Ctrl Pts',(-22.6255527714039,75.5271656167355,
85.0387671131816));
#215180=CARTESIAN_POINT('Ctrl Pts',(-22.6399691837915,75.813863596684,85.0372727556581));
#215181=CARTESIAN_POINT('Ctrl Pts',(-22.6543411901568,76.1006465657745,
85.0254808020078));
#215182=CARTESIAN_POINT('Ctrl Pts',(-22.6687338767191,76.3878421932063,
85.0136718806553));
#215183=CARTESIAN_POINT('Ctrl Pts',(-22.6830820293737,76.6751228126908,
84.9915357218146));
#215184=CARTESIAN_POINT('Ctrl Pts',(-22.6974050197304,76.9617494722563,
84.9590756102513));
#215185=CARTESIAN_POINT('Ctrl Pts',(-22.711758435899,77.248985002497,84.9265465448437));
#215186=CARTESIAN_POINT('Ctrl Pts',(-22.7260865827534,77.5355635524261,
84.8836496437204));
#215187=CARTESIAN_POINT('Ctrl Pts',(-22.7404089556175,77.8207450199491,
84.8304404268258));
#215188=CARTESIAN_POINT('Ctrl Pts',(-22.744959834007,77.9113603244082,84.8135334046732));
#215189=CARTESIAN_POINT('Ctrl Pts',(-22.7495101294395,78.001834617382,84.7955856168893));
#215190=CARTESIAN_POINT('Ctrl Pts',(-22.7540604673341,78.0921442910401,
84.7765999369994));
#215191=CARTESIAN_POINT('Ctrl Pts',(-22.7682603128447,78.3739658708317,
84.7173529695009));
#215192=CARTESIAN_POINT('Ctrl Pts',(-22.7824601583552,78.6541757753439,
84.6479966081922));
#215193=CARTESIAN_POINT('Ctrl Pts',(-22.7966600038657,78.9320516198127,
84.568636466251));
#215194=CARTESIAN_POINT('Ctrl Pts',(-22.810844131221,79.2096198767334,84.489364169986));
#215195=CARTESIAN_POINT('Ctrl Pts',(-22.8250282585763,79.4848589921676,
84.4001102585485));
#215196=CARTESIAN_POINT('Ctrl Pts',(-22.8392123859315,79.7570558754403,
84.301031531765));
#215197=CARTESIAN_POINT('Ctrl Pts',(-22.8533857637286,80.0290464720533,
84.2020278926142));
#215198=CARTESIAN_POINT('Ctrl Pts',(-22.8675591415256,80.2979992025523,
84.0932143694567));
#215199=CARTESIAN_POINT('Ctrl Pts',(-22.8817325193226,80.5632131543211,
83.9747983265767));
#215200=CARTESIAN_POINT('Ctrl Pts',(-22.8958952491306,80.8282278596376,
83.8564712457451));
#215201=CARTESIAN_POINT('Ctrl Pts',(-22.9100579789387,81.0895091623533,
83.7285561304107));
#215202=CARTESIAN_POINT('Ctrl Pts',(-22.9242207087467,81.3463718930863,
83.5913099327499));
#215203=CARTESIAN_POINT('Ctrl Pts',(-22.9383728914716,81.6030433363624,
83.4541659432843));
#215204=CARTESIAN_POINT('Ctrl Pts',(-22.9525250741965,81.8553025520532,
83.3077048435267));
#215205=CARTESIAN_POINT('Ctrl Pts',(-22.9666772569214,82.1024835994402,
83.1522319476038));
#215206=CARTESIAN_POINT('Ctrl Pts',(-22.9808147545179,82.3494081573861,
82.9969203794065));
#215207=CARTESIAN_POINT('Ctrl Pts',(-22.9949522521143,82.5912648537644,
82.8326158057161));
#215208=CARTESIAN_POINT('Ctrl Pts',(-23.0090897497107,82.8274109397139,
82.6596701102719));
#215209=CARTESIAN_POINT('Ctrl Pts',(-23.0232178305836,83.0633997331586,
82.4868396107309));
#215210=CARTESIAN_POINT('Ctrl Pts',(-23.0373459114565,83.2936853006919,
82.305379608006));
#215211=CARTESIAN_POINT('Ctrl Pts',(-23.0514739923294,83.5176506330175,
82.1156872009436));
#215212=CARTESIAN_POINT('Ctrl Pts',(-23.0655889575854,83.7414080500905,
81.9261708923171));
#215213=CARTESIAN_POINT('Ctrl Pts',(-23.0797039228413,83.9588567506015,
81.7284375853734));
#215214=CARTESIAN_POINT('Ctrl Pts',(-23.0938188880973,84.1694090888517,
81.5229273256865));
#215215=CARTESIAN_POINT('Ctrl Pts',(-23.1038933836672,84.3196899121112,
81.3762452642539));
#215216=CARTESIAN_POINT('Ctrl Pts',(-23.1139678792372,84.4664580709411,
81.2256022909389));
#215217=CARTESIAN_POINT('Ctrl Pts',(-23.1240423748071,84.6095094049711,
81.0711715801781));
#215218=CARTESIAN_POINT('Ctrl Pts',(-23.1381651212178,84.8100432878027,
80.8546857272689));
#215219=CARTESIAN_POINT('Ctrl Pts',(-23.1522876470482,85.0032687820581,
80.630758074656));
#215220=CARTESIAN_POINT('Ctrl Pts',(-23.1663998896936,85.188646319028,80.399892177041));
#215221=CARTESIAN_POINT('Ctrl Pts',(-23.1804719706654,85.3734962947653,
80.1696832948306));
#215222=CARTESIAN_POINT('Ctrl Pts',(-23.1945338268983,85.5505427275545,
79.9325757540413));
#215223=CARTESIAN_POINT('Ctrl Pts',(-23.2085754814538,85.7192839577915,
79.6891085031162));
#215224=CARTESIAN_POINT('Ctrl Pts',(-23.2225931230926,85.8877366202471,
79.4460576104477));
#215225=CARTESIAN_POINT('Ctrl Pts',(-23.2365906320896,86.0479122750287,
79.196668899111));
#215226=CARTESIAN_POINT('Ctrl Pts',(-23.2505580826043,86.1993479138062,
78.9415158489488));
#215227=CARTESIAN_POINT('Ctrl Pts',(-23.2644919766457,86.3504197320023,
78.6869757980239));
#215228=CARTESIAN_POINT('Ctrl Pts',(-23.2783959564609,86.4927933085359,
78.4266992478357));
#215229=CARTESIAN_POINT('Ctrl Pts',(-23.2922601675774,86.6260475700772,
78.1612901952401));
#215230=CARTESIAN_POINT('Ctrl Pts',(-23.2975737953986,86.6771188892796,
78.0595689422945));
#215231=CARTESIAN_POINT('Ctrl Pts',(-23.3028815815996,86.7268510904777,
77.9570941250128));
#215232=CARTESIAN_POINT('Ctrl Pts',(-23.3081829713998,86.7752220564,77.8539010146614));
#215233=CARTESIAN_POINT('Origin',(-54.462516693425,66.6776194928561,69.5544896765311));
#215234=CARTESIAN_POINT('',(-55.3469857987243,58.2763555356819,66.0834535849112));
#215235=CARTESIAN_POINT('',(-55.5509564659454,58.2763798771986,66.0833946695127));
#215236=CARTESIAN_POINT('',(-54.462516693425,58.276355535683,66.0834535849087));
#215237=CARTESIAN_POINT('',(-55.3469876474783,58.2763332605869,66.0835074998374));
#215238=CARTESIAN_POINT('Ctrl Pts',(-55.3469857987243,58.2763555356809,
66.0834535849137));
#215239=CARTESIAN_POINT('Ctrl Pts',(-55.3469865205619,58.2763468384005,
66.0834746357315));
#215240=CARTESIAN_POINT('Ctrl Pts',(-55.34698692564,58.2763419577341,66.0834864489592));
#215241=CARTESIAN_POINT('Ctrl Pts',(-55.3469876474783,58.2763332605869,
66.0835074998374));
#215242=CARTESIAN_POINT('',(-55.5974859706232,58.587245489697,73.6987840815406));
#215243=CARTESIAN_POINT('Ctrl Pts',(-55.5958816852329,58.5872629367333,
73.6988181411009));
#215244=CARTESIAN_POINT('Ctrl Pts',(-55.5642543225698,58.1370349043123,
72.819904863597));
#215245=CARTESIAN_POINT('Ctrl Pts',(-55.5337095641794,57.8330219216737,
71.8734645115865));
#215246=CARTESIAN_POINT('Ctrl Pts',(-55.4920076933008,57.6391257286882,
70.5747597609728));
#215247=CARTESIAN_POINT('Ctrl Pts',(-55.4815921437647,57.6083851839778,
70.2504131744609));
#215248=CARTESIAN_POINT('Ctrl Pts',(-55.4607410660172,57.5817045190807,
69.5965855223251));
#215249=CARTESIAN_POINT('Ctrl Pts',(-55.4503222021789,57.5861334573964,
69.2675652529914));
#215250=CARTESIAN_POINT('Ctrl Pts',(-55.4246589713448,57.6412754033317,
68.4543773063773));
#215251=CARTESIAN_POINT('Ctrl Pts',(-55.409556102247,57.7130444170084,67.9726706635946));
#215252=CARTESIAN_POINT('Ctrl Pts',(-55.3785950880418,57.9352139923274,
67.0155987805645));
#215253=CARTESIAN_POINT('Ctrl Pts',(-55.3627155406804,58.0868340317194,
66.5421780378772));
#215254=CARTESIAN_POINT('Ctrl Pts',(-55.3469876474783,58.2763332605869,
66.0835074998374));
#215255=CARTESIAN_POINT('',(-55.7997963168797,58.5872206257229,73.6987355424395));
#215256=CARTESIAN_POINT('',(-55.7986426798444,58.5872330572012,73.6987598112127));
#215257=CARTESIAN_POINT('Ctrl Pts',(-55.8013975426223,58.587203371073,73.698701857855));
#215258=CARTESIAN_POINT('Ctrl Pts',(-55.7703307595377,58.1370141619865,
72.8198332392404));
#215259=CARTESIAN_POINT('Ctrl Pts',(-55.738609114948,57.8330252662733,71.8734459075331));
#215260=CARTESIAN_POINT('Ctrl Pts',(-55.6969348134739,57.6391324266434,
70.5748181414704));
#215261=CARTESIAN_POINT('Ctrl Pts',(-55.6866939433116,57.608389849271,70.2504736082707));
#215262=CARTESIAN_POINT('Ctrl Pts',(-55.6660029351568,57.5817073282663,
69.5967087730762));
#215263=CARTESIAN_POINT('Ctrl Pts',(-55.6555661301364,57.5861300062074,
69.2677545658034));
#215264=CARTESIAN_POINT('Ctrl Pts',(-55.629490900948,57.6412378757168,68.4547261711262));
#215265=CARTESIAN_POINT('Ctrl Pts',(-55.6137725475604,57.7129722962947,
67.9731075839917));
#215266=CARTESIAN_POINT('Ctrl Pts',(-55.5823353923309,57.9351089370947,
67.0159225655129));
#215267=CARTESIAN_POINT('Ctrl Pts',(-55.5667469045371,58.0867766859385,
66.5423084960526));
#215268=CARTESIAN_POINT('Ctrl Pts',(-55.5509584931268,58.2763555356848,
66.0834535849044));
#215269=CARTESIAN_POINT('Origin',(-54.462516693425,66.6776194928561,69.5544896765311));
#215270=CARTESIAN_POINT('',(-53.7366673713217,58.276355535683,66.0834535849087));
#215271=CARTESIAN_POINT('Ctrl Pts',(-55.5509564659454,58.2763798771986,
66.0833946695127));
#215272=CARTESIAN_POINT('Ctrl Pts',(-55.5293519760116,58.5357993236408,
65.4555106945378));
#215273=CARTESIAN_POINT('Ctrl Pts',(-55.5073947993138,58.8647867368264,
64.8586951524983));
#215274=CARTESIAN_POINT('Ctrl Pts',(-55.4641515221015,59.641820374335,63.7604976646574));
#215275=CARTESIAN_POINT('Ctrl Pts',(-55.4432920030105,60.0850422111019,
63.2607833392951));
#215276=CARTESIAN_POINT('Ctrl Pts',(-55.4034957953534,61.0069687435062,
62.42663124984));
#215277=CARTESIAN_POINT('Ctrl Pts',(-55.3847616723786,61.4710034794686,
62.0809506872743));
#215278=CARTESIAN_POINT('Ctrl Pts',(-55.3493583763049,62.4130313959237,
61.50976809141));
#215279=CARTESIAN_POINT('Ctrl Pts',(-55.3328563273452,62.8840698709349,
61.2772171285064));
#215280=CARTESIAN_POINT('Ctrl Pts',(-55.3066526577161,63.6494857328239,
60.9784691431388));
#215281=CARTESIAN_POINT('Ctrl Pts',(-55.2971246844391,63.9315843450776,
60.884021908299));
#215282=CARTESIAN_POINT('Ctrl Pts',(-55.2686864356095,64.7811364350475,
60.6452191699261));
#215283=CARTESIAN_POINT('Ctrl Pts',(-55.2497306634879,65.3584552015835,
60.5416338472421));
#215284=CARTESIAN_POINT('Ctrl Pts',(-55.2154989596548,66.4315305155951,
60.454474878268));
#215285=CARTESIAN_POINT('Ctrl Pts',(-55.1999659970024,66.9237640368931,
60.454476440718));
#215286=CARTESIAN_POINT('Ctrl Pts',(-55.1694541313247,67.8729393850907,
60.5315775352599));
#215287=CARTESIAN_POINT('Ctrl Pts',(-55.1545490352729,68.3287977518769,
60.6037724386958));
#215288=CARTESIAN_POINT('Ctrl Pts',(-55.12154803696,69.326174810265,60.8405448962535));
#215289=CARTESIAN_POINT('Ctrl Pts',(-55.1038064141092,69.861815684947,61.0216955323755));
#215290=CARTESIAN_POINT('Ctrl Pts',(-55.063999601112,71.0064666283551,61.5317097012693));
#215291=CARTESIAN_POINT('Ctrl Pts',(-55.0417962598498,71.6018231054538,
61.8827158375686));
#215292=CARTESIAN_POINT('Ctrl Pts',(-55.0016951825324,72.600435801391,62.6360073565726));
#215293=CARTESIAN_POINT('Ctrl Pts',(-54.9841070732111,73.0167318888312,
63.0153149028952));
#215294=CARTESIAN_POINT('Ctrl Pts',(-54.956911094595,73.5946968075922,63.6493272193589));
#215295=CARTESIAN_POINT('Ctrl Pts',(-54.947487901833,73.7832613577235,63.877628380177));
#215296=CARTESIAN_POINT('Ctrl Pts',(-54.9190534935064,74.3148611040193,
64.5893308930821));
#215297=CARTESIAN_POINT('Ctrl Pts',(-54.9000080938475,74.6221306839518,
65.0974704511788));
#215298=CARTESIAN_POINT('Ctrl Pts',(-54.8651085839444,75.0997198591477,
66.0958640835209));
#215299=CARTESIAN_POINT('Ctrl Pts',(-54.8489882282909,75.2818881212308,
66.5778429379041));
#215300=CARTESIAN_POINT('Ctrl Pts',(-54.8161206223998,75.5641844346651,
67.572499567804));
#215301=CARTESIAN_POINT('Ctrl Pts',(-54.7994273699867,75.662931038084,68.0836078723164));
#215302=CARTESIAN_POINT('Ctrl Pts',(-54.7659657458026,75.7735740350487,
69.1318698417486));
#215303=CARTESIAN_POINT('Ctrl Pts',(-54.749361305166,75.7826879763227,69.6673118176174));
#215304=CARTESIAN_POINT('Ctrl Pts',(-54.723226180653,75.7237379107367,70.4947770869297));
#215305=CARTESIAN_POINT('Ctrl Pts',(-54.7138851163246,75.6884499719406,
70.7879122301499));
#215306=CARTESIAN_POINT('Ctrl Pts',(-54.6854713453321,75.5386710585311,
71.6684501055308));
#215307=CARTESIAN_POINT('Ctrl Pts',(-54.6664084456847,75.3804204367525,
72.2467631845367));
#215308=CARTESIAN_POINT('Ctrl Pts',(-54.6307736532416,74.9733416854762,
73.3097646919201));
#215309=CARTESIAN_POINT('Ctrl Pts',(-54.6139269174089,74.7355907205756,
73.7959745111832));
#215310=CARTESIAN_POINT('Ctrl Pts',(-54.5842320055116,74.250242856249,74.5985898232458));
#215311=CARTESIAN_POINT('Ctrl Pts',(-54.5715492183761,74.0222783036838,
74.9251093954127));
#215312=CARTESIAN_POINT('Ctrl Pts',(-54.5411564525276,73.4229474861732,
75.6737032519809));
#215313=CARTESIAN_POINT('Ctrl Pts',(-54.5237921110022,73.0324247648255,
76.0783440664095));
#215314=CARTESIAN_POINT('Ctrl Pts',(-54.4849014956126,72.0913866883103,
76.8882046029579));
#215315=CARTESIAN_POINT('Ctrl Pts',(-54.4632576605534,71.5274824055733,
77.2727186656698));
#215316=CARTESIAN_POINT('Ctrl Pts',(-54.424685322754,70.4492787161637,77.8427152235626));
#215317=CARTESIAN_POINT('Ctrl Pts',(-54.4080137844851,69.9510881874095,
78.0518127948251));
#215318=CARTESIAN_POINT('Ctrl Pts',(-54.3697944876016,68.7882585464024,
78.4223285187575));
#215319=CARTESIAN_POINT('Ctrl Pts',(-54.3481195233592,68.1180159738578,
78.5555229109669));
#215320=CARTESIAN_POINT('Ctrl Pts',(-54.3171705141335,67.1431958327321,
78.6374858473127));
#215321=CARTESIAN_POINT('Ctrl Pts',(-54.3078829134622,66.8461257552885,
78.6478491855203));
#215322=CARTESIAN_POINT('Ctrl Pts',(-54.2824028362145,66.0302894258696,
78.6363115634944));
#215323=CARTESIAN_POINT('Ctrl Pts',(-54.2661991957931,65.5130826681465,
78.5845712617889));
#215324=CARTESIAN_POINT('Ctrl Pts',(-54.2405085930586,64.7161012667595,
78.4352019279697));
#215325=CARTESIAN_POINT('Ctrl Pts',(-54.2312097061039,64.4318372928247,
78.3676086043772));
#215326=CARTESIAN_POINT('Ctrl Pts',(-54.1936146716957,63.2963495553903,
78.039093676153));
#215327=CARTESIAN_POINT('Ctrl Pts',(-54.1662304751788,62.4823262415862,
77.6675044830376));
#215328=CARTESIAN_POINT('Ctrl Pts',(-54.118931725783,61.2309279616505,76.8568237565957));
#215329=CARTESIAN_POINT('Ctrl Pts',(-54.099645498139,60.7601649384632,76.4808359800358));
#215330=CARTESIAN_POINT('Ctrl Pts',(-54.0618618311743,59.9011709522606,
75.6428327128146));
#215331=CARTESIAN_POINT('Ctrl Pts',(-54.0431808362138,59.5147800172535,
75.1831579282922));
#215332=CARTESIAN_POINT('Ctrl Pts',(-54.0078044448732,58.8865153419934,
74.2652719391899));
#215333=CARTESIAN_POINT('Ctrl Pts',(-53.9912907602423,58.6330018531612,
73.8179267415289));
#215334=CARTESIAN_POINT('Ctrl Pts',(-53.9656531530641,58.2960950129963,
73.085124826228));
#215335=CARTESIAN_POINT('Ctrl Pts',(-53.9564336345394,58.1865554971259,
72.8128896896097));
#215336=CARTESIAN_POINT('Ctrl Pts',(-53.909615991058,57.6991564449222,71.4090211601971));
#215337=CARTESIAN_POINT('Ctrl Pts',(-53.871311701512,57.5335351163601,70.2161476308588));
#215338=CARTESIAN_POINT('Ctrl Pts',(-53.8015513714535,57.6619983086808,
68.0128916894792));
#215339=CARTESIAN_POINT('Ctrl Pts',(-53.7689112883543,57.8899947788509,
67.018597621202));
#215340=CARTESIAN_POINT('Ctrl Pts',(-53.7366673713217,58.276355535683,66.0834535849087));
#215341=CARTESIAN_POINT('',(-53.5332787937082,58.276355535683,66.0834535849087));
#215342=CARTESIAN_POINT('',(-54.462516693425,58.276355535683,66.0834535849087));
#215343=CARTESIAN_POINT('Ctrl Pts',(-53.5332787937082,58.276355535683,66.0834535849087));
#215344=CARTESIAN_POINT('Ctrl Pts',(-53.5655626775805,57.8867451875228,
67.0264629022823));
#215345=CARTESIAN_POINT('Ctrl Pts',(-53.5970516509312,57.6582247284551,
68.0295019086322));
#215346=CARTESIAN_POINT('Ctrl Pts',(-53.6676791533075,57.5354242743256,
70.2411464584609));
#215347=CARTESIAN_POINT('Ctrl Pts',(-53.7043653688208,57.7042326106747,
71.4332008671241));
#215348=CARTESIAN_POINT('Ctrl Pts',(-53.7518962835288,58.1953384732383,
72.8357123780027));
#215349=CARTESIAN_POINT('Ctrl Pts',(-53.7612947348906,58.3057274807103,
73.1079302723123));
#215350=CARTESIAN_POINT('Ctrl Pts',(-53.7862473225142,58.6365895942013,
73.8223905877668));
#215351=CARTESIAN_POINT('Ctrl Pts',(-53.8016632114925,58.8802475200011,
74.2528015851126));
#215352=CARTESIAN_POINT('Ctrl Pts',(-53.8461401751329,59.6694318506876,
75.4149068128443));
#215353=CARTESIAN_POINT('Ctrl Pts',(-53.875528330836,60.2915996961264,76.0873249387124));
#215354=CARTESIAN_POINT('Ctrl Pts',(-53.9225729919868,61.4550088496706,
77.016929560116));
#215355=CARTESIAN_POINT('Ctrl Pts',(-53.9408334467599,61.9401457211529,
77.3339501839349));
#215356=CARTESIAN_POINT('Ctrl Pts',(-53.977277277685,62.9453814781525,77.8617235755638));
#215357=CARTESIAN_POINT('Ctrl Pts',(-53.995278074046,63.4614421781021,78.07481546934));
#215358=CARTESIAN_POINT('Ctrl Pts',(-54.0296422055439,64.4957981534369,
78.3944612651201));
#215359=CARTESIAN_POINT('Ctrl Pts',(-54.0462059068673,65.0103444407188,
78.5057820273322));
#215360=CARTESIAN_POINT('Ctrl Pts',(-54.0773745812104,65.9757803903488,
78.62847541936));
#215361=CARTESIAN_POINT('Ctrl Pts',(-54.0918530074528,66.4235068791955,
78.6520287760528));
#215362=CARTESIAN_POINT('Ctrl Pts',(-54.1403128133875,67.9273566874276,
78.6200062744246));
#215363=CARTESIAN_POINT('Ctrl Pts',(-54.1732503539562,68.9716109476033,
78.4135544007001));
#215364=CARTESIAN_POINT('Ctrl Pts',(-54.2169174594595,70.2318207791961,
77.9260997599377));
#215365=CARTESIAN_POINT('Ctrl Pts',(-54.2264512621277,70.5013847242329,
77.80646056663));
#215366=CARTESIAN_POINT('Ctrl Pts',(-54.2519427279785,71.2125176461925,
77.4485015693435));
#215367=CARTESIAN_POINT('Ctrl Pts',(-54.2677356448227,71.6409576010732,
77.1863967565669));
#215368=CARTESIAN_POINT('Ctrl Pts',(-54.2998622272673,72.4530656255441,
76.5921373222878));
#215369=CARTESIAN_POINT('Ctrl Pts',(-54.3161473410997,72.8349827406509,
76.2605415590481));
#215370=CARTESIAN_POINT('Ctrl Pts',(-54.3517907845278,73.6051258911224,
75.4703339182632));
#215371=CARTESIAN_POINT('Ctrl Pts',(-54.3707287271076,73.9795165901898,
75.0014946722767));
#215372=CARTESIAN_POINT('Ctrl Pts',(-54.4084654085077,74.6252684857957,
74.0054013195963));
#215373=CARTESIAN_POINT('Ctrl Pts',(-54.4273542154633,74.8967110002721,
73.4816083068042));
#215374=CARTESIAN_POINT('Ctrl Pts',(-54.455941123101,75.2262509370908,72.6591201293671));
#215375=CARTESIAN_POINT('Ctrl Pts',(-54.4655159703041,75.3232727549448,
72.3776994682275));
#215376=CARTESIAN_POINT('Ctrl Pts',(-54.4955040289261,75.5862504835227,
71.4731000360478));
#215377=CARTESIAN_POINT('Ctrl Pts',(-54.5157455546589,75.6998411821233,
70.8367892945741));
#215378=CARTESIAN_POINT('Ctrl Pts',(-54.553591351842,75.7829174207925,69.6585502476179));
#215379=CARTESIAN_POINT('Ctrl Pts',(-54.5709597629142,75.773187030605,69.120975511141));
#215380=CARTESIAN_POINT('Ctrl Pts',(-54.6049064040635,75.6596473684368,
68.0598205514083));
#215381=CARTESIAN_POINT('Ctrl Pts',(-54.6215179372701,75.5571124338195,
67.5381882265612));
#215382=CARTESIAN_POINT('Ctrl Pts',(-54.6544696694349,75.268936383534,66.5420041139739));
#215383=CARTESIAN_POINT('Ctrl Pts',(-54.6707279760388,75.0877995034649,
66.0681362343352));
#215384=CARTESIAN_POINT('Ctrl Pts',(-54.7061676472104,74.6077637515443,
65.0709037461789));
#215385=CARTESIAN_POINT('Ctrl Pts',(-54.7249207921526,74.294433378991,64.5571022944996));
#215386=CARTESIAN_POINT('Ctrl Pts',(-54.7625453618885,73.5760389004118,
63.6053990232175));
#215387=CARTESIAN_POINT('Ctrl Pts',(-54.781435990255,73.1740194179169,63.1688303405712));
#215388=CARTESIAN_POINT('Ctrl Pts',(-54.8191787545644,72.2923760428621,
62.3814911264832));
#215389=CARTESIAN_POINT('Ctrl Pts',(-54.8375876280151,71.8151169441302,
62.0322875949448));
#215390=CARTESIAN_POINT('Ctrl Pts',(-54.8654485062721,71.0519849546158,
61.5806362743694));
#215391=CARTESIAN_POINT('Ctrl Pts',(-54.8748073230891,70.7893271961805,
61.4420751545686));
#215392=CARTESIAN_POINT('Ctrl Pts',(-54.9011635586761,70.0364678518818,
61.0908868353993));
#215393=CARTESIAN_POINT('Ctrl Pts',(-54.9182752578256,69.5336214813441,
60.9082365854418));
#215394=CARTESIAN_POINT('Ctrl Pts',(-54.9521294825018,68.4948704348333,
60.6315063744957));
#215395=CARTESIAN_POINT('Ctrl Pts',(-54.9688975589155,67.9606901776106,
60.5391822805108));
#215396=CARTESIAN_POINT('Ctrl Pts',(-55.0014383011775,66.9307320458366,
60.4546151403975));
#215397=CARTESIAN_POINT('Ctrl Pts',(-55.0171040942008,66.4375248985683,
60.4542627280721));
#215398=CARTESIAN_POINT('Ctrl Pts',(-55.0513165144325,65.3633367342361,
60.5409138398399));
#215399=CARTESIAN_POINT('Ctrl Pts',(-55.069463862521,64.7858546030156,60.6442081211182));
#215400=CARTESIAN_POINT('Ctrl Pts',(-55.0970861308951,63.9360441440502,
60.8826100723));
#215401=CARTESIAN_POINT('Ctrl Pts',(-55.1064307458234,63.6538826901546,
60.9769174549123));
#215402=CARTESIAN_POINT('Ctrl Pts',(-55.1323657620152,62.8897840562762,
61.2747011696298));
#215403=CARTESIAN_POINT('Ctrl Pts',(-55.1490609507609,62.4199951699038,
61.5061833247957));
#215404=CARTESIAN_POINT('Ctrl Pts',(-55.1820030100303,61.522283991715,62.0492269412328));
#215405=CARTESIAN_POINT('Ctrl Pts',(-55.1982907980861,61.0963763792673,
62.3603126797909));
#215406=CARTESIAN_POINT('Ctrl Pts',(-55.2367067708785,60.1755747206076,
63.1641104969289));
#215407=CARTESIAN_POINT('Ctrl Pts',(-55.2589711383476,59.7056367005308,
63.6803953102331));
#215408=CARTESIAN_POINT('Ctrl Pts',(-55.3029292155024,58.8882690149415,
64.8163076429406));
#215409=CARTESIAN_POINT('Ctrl Pts',(-55.3246879318393,58.5450181575742,
65.4331850361657));
#215410=CARTESIAN_POINT('Ctrl Pts',(-55.3469857987243,58.2763555356809,
66.0834535849137));
#215411=CARTESIAN_POINT('Origin',(-54.462516693425,66.6776194928561,69.5544896765311));
#215412=CARTESIAN_POINT('',(-51.7190489450981,58.276355535683,66.0834535849087));
#215413=CARTESIAN_POINT('',(-51.9229031375498,58.2763555332145,66.0834535908833));
#215414=CARTESIAN_POINT('',(-54.462516693425,58.276355535683,66.0834535849087));
#215415=CARTESIAN_POINT('Ctrl Pts',(-51.7190489450981,58.276355535683,66.0834535849086));
#215416=CARTESIAN_POINT('Ctrl Pts',(-51.7297909865996,58.1452767990722,
66.4007153581577));
#215417=CARTESIAN_POINT('Ctrl Pts',(-51.7405829583826,58.0321969222248,
66.7253355117126));
#215418=CARTESIAN_POINT('Ctrl Pts',(-51.7671844604377,57.8013703463813,
67.5327114967342));
#215419=CARTESIAN_POINT('Ctrl Pts',(-51.7830641197152,57.704284738644,68.0200041119831));
#215420=CARTESIAN_POINT('Ctrl Pts',(-51.8080188068358,57.6138010436533,
68.804368958479));
#215421=CARTESIAN_POINT('Ctrl Pts',(-51.817194791681,57.5943064002912,69.0974220773683));
#215422=CARTESIAN_POINT('Ctrl Pts',(-51.8592177464655,57.5701720672488,
70.4382974657879));
#215423=CARTESIAN_POINT('Ctrl Pts',(-51.8927662132002,57.7325169240372,
71.4811043123403));
#215424=CARTESIAN_POINT('Ctrl Pts',(-51.9446543809477,58.2613918916844,
73.0410264061283));
#215425=CARTESIAN_POINT('Ctrl Pts',(-51.9634037738247,58.5096182058567,
73.5884180661377));
#215426=CARTESIAN_POINT('Ctrl Pts',(-52.0016163719075,59.1099745473828,
74.6258755825583));
#215427=CARTESIAN_POINT('Ctrl Pts',(-52.0209296563522,59.4605480935123,
75.113455015466));
#215428=CARTESIAN_POINT('Ctrl Pts',(-52.0588686893564,60.2532267253739,
76.0133347474263));
#215429=CARTESIAN_POINT('Ctrl Pts',(-52.0776830551728,60.6935439328099,
76.4232844203296));
#215430=CARTESIAN_POINT('Ctrl Pts',(-52.1126338797061,61.5634236510416,
77.0855951123235));
#215431=CARTESIAN_POINT('Ctrl Pts',(-52.1285697204729,61.9794687477448,
77.3519202515112));
#215432=CARTESIAN_POINT('Ctrl Pts',(-52.1537182355886,62.6742548444957,
77.7207936911086));
#215433=CARTESIAN_POINT('Ctrl Pts',(-52.1629927917558,62.9399662666728,
77.8457741971178));
#215434=CARTESIAN_POINT('Ctrl Pts',(-52.2098136240202,64.3075493608403,
78.4099093559652));
#215435=CARTESIAN_POINT('Ctrl Pts',(-52.2480628999824,65.4818136675885,
78.643259277779));
#215436=CARTESIAN_POINT('Ctrl Pts',(-52.3040881464568,67.2477783879154,
78.6451840249999));
#215437=CARTESIAN_POINT('Ctrl Pts',(-52.3225131095039,67.8265701659199,
78.5902911792699));
#215438=CARTESIAN_POINT('Ctrl Pts',(-52.3595295668438,68.9539700452295,
78.3732328713076));
#215439=CARTESIAN_POINT('Ctrl Pts',(-52.3778973643229,69.5004860289171,
78.2137877221895));
#215440=CARTESIAN_POINT('Ctrl Pts',(-52.4140545301813,70.5576359137233,
77.7945606084078));
#215441=CARTESIAN_POINT('Ctrl Pts',(-52.4320745666133,71.0658550902994,
77.5355097194339));
#215442=CARTESIAN_POINT('Ctrl Pts',(-52.4674002329574,71.9927932922179,
76.9475651068214));
#215443=CARTESIAN_POINT('Ctrl Pts',(-52.4845761304828,72.4135503083147,
76.6261047834406));
#215444=CARTESIAN_POINT('Ctrl Pts',(-52.5179670940298,73.1857150076729,
75.9216717201334));
#215445=CARTESIAN_POINT('Ctrl Pts',(-52.5342433170281,73.5370541495871,
75.5415152241367));
#215446=CARTESIAN_POINT('Ctrl Pts',(-52.5662763717388,74.1521757655702,
74.7502628796883));
#215447=CARTESIAN_POINT('Ctrl Pts',(-52.581950416172,74.4189726128819,74.3436958487136));
#215448=CARTESIAN_POINT('Ctrl Pts',(-52.6169307455104,74.9394935738121,
73.3923854213503));
#215449=CARTESIAN_POINT('Ctrl Pts',(-52.6358128319037,75.1743424436644,
72.8398680566229));
#215450=CARTESIAN_POINT('Ctrl Pts',(-52.6642021536451,75.4411186332504,
71.9870297038072));
#215451=CARTESIAN_POINT('Ctrl Pts',(-52.6736001389969,75.5153668048818,
71.7016713015829));
#215452=CARTESIAN_POINT('Ctrl Pts',(-52.7005200820087,75.6869461038813,
70.8802940815234));
#215453=CARTESIAN_POINT('Ctrl Pts',(-52.7181571859923,75.7501682284098,
70.3384477093478));
#215454=CARTESIAN_POINT('Ctrl Pts',(-52.7539696199146,75.7798597050836,
69.2129442652462));
#215455=CARTESIAN_POINT('Ctrl Pts',(-52.7721897099371,75.7393861088041,
68.6315478859276));
#215456=CARTESIAN_POINT('Ctrl Pts',(-52.8065558247652,75.5619672989915,
67.5685563511103));
#215457=CARTESIAN_POINT('Ctrl Pts',(-52.8225403875164,75.4403337548272,
67.0866159433306));
#215458=CARTESIAN_POINT('Ctrl Pts',(-52.861854617124,75.0431684405423,65.9235202423042));
#215459=CARTESIAN_POINT('Ctrl Pts',(-52.8846025666856,74.7233642266042,
65.2611991817657));
#215460=CARTESIAN_POINT('Ctrl Pts',(-52.9238158502275,74.0571175243991,
64.2231705879217));
#215461=CARTESIAN_POINT('Ctrl Pts',(-52.9398941888697,73.7523626374077,
63.8249208396988));
#215462=CARTESIAN_POINT('Ctrl Pts',(-52.9766967184228,72.9768367067566,
62.9682840108232));
#215463=CARTESIAN_POINT('Ctrl Pts',(-52.9969933203808,72.4861149505907,
62.5316963366546));
#215464=CARTESIAN_POINT('Ctrl Pts',(-53.0334867491832,71.5460372241218,
61.8618144110017));
#215465=CARTESIAN_POINT('Ctrl Pts',(-53.0494388776599,71.1161258988521,
61.6060056457897));
#215466=CARTESIAN_POINT('Ctrl Pts',(-53.0979197277774,69.747581117297,60.9374950055504));
#215467=CARTESIAN_POINT('Ctrl Pts',(-53.1293484776116,68.7584477903061,
60.6467731515279));
#215468=CARTESIAN_POINT('Ctrl Pts',(-53.1712046497495,67.4513676644178,
60.4926926534559));
#215469=CARTESIAN_POINT('Ctrl Pts',(-53.1805221582027,67.1594503901744,
60.4724914816801));
#215470=CARTESIAN_POINT('Ctrl Pts',(-53.2070124229002,66.3213843424688,
60.4550213283923));
#215471=CARTESIAN_POINT('Ctrl Pts',(-53.2238855276084,65.7757832089102,
60.4928163888376));
#215472=CARTESIAN_POINT('Ctrl Pts',(-53.2576262207124,64.714181512971,60.6632305163589));
#215473=CARTESIAN_POINT('Ctrl Pts',(-53.2744219506812,64.1998171398207,
60.7926368877312));
#215474=CARTESIAN_POINT('Ctrl Pts',(-53.3098179404078,63.1462982245024,
61.1579359757481));
#215475=CARTESIAN_POINT('Ctrl Pts',(-53.3280076005827,62.6127810599663,
61.4028372586244));
#215476=CARTESIAN_POINT('Ctrl Pts',(-53.3556258902385,61.8491815284432,
61.847079914686));
#215477=CARTESIAN_POINT('Ctrl Pts',(-53.3649702061992,61.599336313249,62.0093576969857));
#215478=CARTESIAN_POINT('Ctrl Pts',(-53.3898639392663,60.9604045687096,
62.4704870885438));
#215479=CARTESIAN_POINT('Ctrl Pts',(-53.4055080051247,60.5867619892367,
62.7890561532968));
#215480=CARTESIAN_POINT('Ctrl Pts',(-53.437438933781,59.8718678681658,63.5060318544576));
#215481=CARTESIAN_POINT('Ctrl Pts',(-53.4535879884448,59.5356605431283,
63.9069659835912));
#215482=CARTESIAN_POINT('Ctrl Pts',(-53.4858087684677,58.9459658308018,
64.7476712063653));
#215483=CARTESIAN_POINT('Ctrl Pts',(-53.5018112337239,58.6910935895951,
65.1842073837295));
#215484=CARTESIAN_POINT('Ctrl Pts',(-53.5230144855764,58.4039439418394,
65.7859480088557));
#215485=CARTESIAN_POINT('Ctrl Pts',(-53.5281604188844,58.3381254207757,
65.9339463209189));
#215486=CARTESIAN_POINT('Ctrl Pts',(-53.5332787937082,58.276355535683,66.0834535849087));
#215487=CARTESIAN_POINT('Ctrl Pts',(-53.7366673713217,58.276355535683,66.0834535849087));
#215488=CARTESIAN_POINT('Ctrl Pts',(-53.7311924318832,58.3419586614738,
65.9246683802505));
#215489=CARTESIAN_POINT('Ctrl Pts',(-53.7257379418286,58.4121273391153,
65.7675881140914));
#215490=CARTESIAN_POINT('Ctrl Pts',(-53.7012784846244,58.7467389739019,
65.0723349768854));
#215491=CARTESIAN_POINT('Ctrl Pts',(-53.68226410661,59.0594466298307,64.5592909907682));
#215492=CARTESIAN_POINT('Ctrl Pts',(-53.6440710268083,59.7730809282138,
63.6131281747025));
#215493=CARTESIAN_POINT('Ctrl Pts',(-53.6251642980075,60.1701800452071,
63.1806622316127));
#215494=CARTESIAN_POINT('Ctrl Pts',(-53.5909939976614,60.9706951840624,
62.4622180755958));
#215495=CARTESIAN_POINT('Ctrl Pts',(-53.575474758473,61.3611218065782,62.1650275357795));
#215496=CARTESIAN_POINT('Ctrl Pts',(-53.543512083073,62.1990648694285,61.6281266777756));
#215497=CARTESIAN_POINT('Ctrl Pts',(-53.5271071357313,62.6465335046139,
61.3914618649718));
#215498=CARTESIAN_POINT('Ctrl Pts',(-53.4940927068657,63.5919501222416,
60.9882198705243));
#215499=CARTESIAN_POINT('Ctrl Pts',(-53.4776501716035,64.0893400320841,
60.8250483118051));
#215500=CARTESIAN_POINT('Ctrl Pts',(-53.4515011764791,64.8874480684872,
60.6374817478447));
#215501=CARTESIAN_POINT('Ctrl Pts',(-53.441970765598,65.1800727413696,60.5836984088002));
#215502=CARTESIAN_POINT('Ctrl Pts',(-53.4135047195804,66.0556830139493,
60.4668081126836));
#215503=CARTESIAN_POINT('Ctrl Pts',(-53.3945384953424,66.6427094200249,
60.4456171533872));
#215504=CARTESIAN_POINT('Ctrl Pts',(-53.3570293722958,67.8210826162455,
60.517054256725));
#215505=CARTESIAN_POINT('Ctrl Pts',(-53.33824063788,68.4095227784195,60.6111539031541));
#215506=CARTESIAN_POINT('Ctrl Pts',(-53.3037808204978,69.4466278606999,
60.8832650107809));
#215507=CARTESIAN_POINT('Ctrl Pts',(-53.2882999316967,69.8984319767658,
61.0407412355476));
#215508=CARTESIAN_POINT('Ctrl Pts',(-53.2565712011872,70.8080872919673,
61.4406270428976));
#215509=CARTESIAN_POINT('Ctrl Pts',(-53.2403824324189,71.2618801399946,
61.688099632371));
#215510=CARTESIAN_POINT('Ctrl Pts',(-53.2040930968364,72.2133226175424,
62.3173872972681));
#215511=CARTESIAN_POINT('Ctrl Pts',(-53.183939473219,72.697496313979,62.714845756158));
#215512=CARTESIAN_POINT('Ctrl Pts',(-53.1462258971347,73.5268006904438,
63.552417439899));
#215513=CARTESIAN_POINT('Ctrl Pts',(-53.1289153258879,73.8797380436296,
63.9808333396457));
#215514=CARTESIAN_POINT('Ctrl Pts',(-53.1020034726543,74.357971412337,64.6832433562619));
#215515=CARTESIAN_POINT('Ctrl Pts',(-53.0925914463726,74.5124263739884,
64.9357619592791));
#215516=CARTESIAN_POINT('Ctrl Pts',(-53.0641411353165,74.9390844612585,
65.7164939021594));
#215517=CARTESIAN_POINT('Ctrl Pts',(-53.0450838003077,75.1721256350204,
66.2642924312581));
#215518=CARTESIAN_POINT('Ctrl Pts',(-53.0092068472208,75.5135324920802,
67.3513984616382));
#215519=CARTESIAN_POINT('Ctrl Pts',(-52.9921213947985,75.6298054510112,
67.8855577007919));
#215520=CARTESIAN_POINT('Ctrl Pts',(-52.9591460990218,75.7584613520713,
68.9147142293431));
#215521=CARTESIAN_POINT('Ctrl Pts',(-52.943370378706,75.7797701191653,69.4066621395435));
#215522=CARTESIAN_POINT('Ctrl Pts',(-52.911095693656,75.7412819636644,70.4246802732259));
#215523=CARTESIAN_POINT('Ctrl Pts',(-52.8947343811169,75.6755823410685,
70.9487203678477));
#215524=CARTESIAN_POINT('Ctrl Pts',(-52.8688560994954,75.5028705016795,
71.7525088367728));
#215525=CARTESIAN_POINT('Ctrl Pts',(-52.8595254225974,75.4268994499431,
72.0377218640758));
#215526=CARTESIAN_POINT('Ctrl Pts',(-52.8311270335815,75.1552027324261,
72.8888691141832));
#215527=CARTESIAN_POINT('Ctrl Pts',(-52.8120780996225,74.9173443869597,
73.4396479332205));
#215528=CARTESIAN_POINT('Ctrl Pts',(-52.7773610510153,74.3790085656657,
74.4103703648679));
#215529=CARTESIAN_POINT('Ctrl Pts',(-52.7614170741286,74.0936192220105,
74.8359587895104));
#215530=CARTESIAN_POINT('Ctrl Pts',(-52.7298730908476,73.470066651144,75.6148892266165));
#215531=CARTESIAN_POINT('Ctrl Pts',(-52.7143505704592,73.1362089965511,
75.9695032833215));
#215532=CARTESIAN_POINT('Ctrl Pts',(-52.682531006495,72.3886843419833,76.645699858249));
#215533=CARTESIAN_POINT('Ctrl Pts',(-52.6664022672045,71.9723579023323,
76.9617342519526));
#215534=CARTESIAN_POINT('Ctrl Pts',(-52.6322390103953,71.0507229972334,
77.5437483372261));
#215535=CARTESIAN_POINT('Ctrl Pts',(-52.6142123432411,70.5428224261473,
77.8014577569882));
#215536=CARTESIAN_POINT('Ctrl Pts',(-52.578175097805,69.486223313356,78.2183942640377));
#215537=CARTESIAN_POINT('Ctrl Pts',(-52.5605556197902,68.9398896018736,
78.3768269863344));
#215538=CARTESIAN_POINT('Ctrl Pts',(-52.5246847482757,67.8131002898757,
78.5919603651484));
#215539=CARTESIAN_POINT('Ctrl Pts',(-52.5063744298448,67.2347576412136,
78.6459569374812));
#215540=CARTESIAN_POINT('Ctrl Pts',(-52.4502646779272,65.4693496476904,
78.6416089451388));
#215541=CARTESIAN_POINT('Ctrl Pts',(-52.4139257778699,64.2954222045958,
78.4066522721589));
#215542=CARTESIAN_POINT('Ctrl Pts',(-52.3668074694311,62.9285056104644,
77.8406030075759));
#215543=CARTESIAN_POINT('Ctrl Pts',(-52.3574542691322,62.6628429772777,
77.7151943835185));
#215544=CARTESIAN_POINT('Ctrl Pts',(-52.3314026873732,61.9334863960864,
77.3266448147371));
#215545=CARTESIAN_POINT('Ctrl Pts',(-52.3148571809506,61.4861912750879,
77.0352832186051));
#215546=CARTESIAN_POINT('Ctrl Pts',(-52.2790825333981,60.5946063699471,
76.3358437178863));
#215547=CARTESIAN_POINT('Ctrl Pts',(-52.2598405536161,60.1600952896223,
75.9193679903975));
#215548=CARTESIAN_POINT('Ctrl Pts',(-52.2199383850187,59.3443572919324,
74.9656871986867));
#215549=CARTESIAN_POINT('Ctrl Pts',(-52.1996324508646,58.9738516611268,
74.4237562134378));
#215550=CARTESIAN_POINT('Ctrl Pts',(-52.159830619563,58.3814408224882,73.3178356340863));
#215551=CARTESIAN_POINT('Ctrl Pts',(-52.1405028579493,58.1511829363678,
72.7621712009817));
#215552=CARTESIAN_POINT('Ctrl Pts',(-52.1044482223889,57.8231178466625,
71.6783057699179));
#215553=CARTESIAN_POINT('Ctrl Pts',(-52.087817524682,57.7139444648366,71.1561539683518));
#215554=CARTESIAN_POINT('Ctrl Pts',(-52.0420519854254,57.5436879712687,
69.7238411266884));
#215555=CARTESIAN_POINT('Ctrl Pts',(-52.0126390402298,57.5725696407299,
68.8092010332304));
#215556=CARTESIAN_POINT('Ctrl Pts',(-51.9655607911578,57.8409930992436,
67.3461209787052));
#215557=CARTESIAN_POINT('Ctrl Pts',(-51.9472899306698,57.9991045718153,
66.789307985591));
#215558=CARTESIAN_POINT('Ctrl Pts',(-51.9267839175271,58.2308768134648,
66.1950996618202));
#215559=CARTESIAN_POINT('Ctrl Pts',(-51.9248440301999,58.2533412531563,
66.1391571437214));
#215560=CARTESIAN_POINT('Ctrl Pts',(-51.9229031375498,58.276355530746,66.083453596858));
#215561=CARTESIAN_POINT('Origin',(-54.462516693425,66.6776194928561,69.5544896765311));
#215562=CARTESIAN_POINT('',(-49.9050113929448,58.276355535683,66.0834535849087));
#215563=CARTESIAN_POINT('',(-50.1089321285242,58.276355535683,66.0834535849087));
#215564=CARTESIAN_POINT('',(-54.462516693425,58.276355535683,66.0834535849087));
#215565=CARTESIAN_POINT('Ctrl Pts',(-49.9050113929448,58.276355535683,66.0834535849087));
#215566=CARTESIAN_POINT('Ctrl Pts',(-49.9146376833535,58.1605312070027,
66.363793728952));
#215567=CARTESIAN_POINT('Ctrl Pts',(-49.9243138080825,58.0587404443406,
66.6499272247979));
#215568=CARTESIAN_POINT('Ctrl Pts',(-49.9515580498989,57.8121177239994,
67.471427229109));
#215569=CARTESIAN_POINT('Ctrl Pts',(-49.9687688148612,57.7016626603582,
68.0155058286091));
#215570=CARTESIAN_POINT('Ctrl Pts',(-50.0043152237878,57.5785750352218,
69.1409824503157));
#215571=CARTESIAN_POINT('Ctrl Pts',(-50.0226790664577,57.5706958512298,
69.7203997185111));
#215572=CARTESIAN_POINT('Ctrl Pts',(-50.0700859037347,57.6919873595473,
71.2010948169454));
#215573=CARTESIAN_POINT('Ctrl Pts',(-50.0981155088323,57.901108321059,72.089396074077));
#215574=CARTESIAN_POINT('Ctrl Pts',(-50.1427607988033,58.4223748973441,
73.3918995671297));
#215575=CARTESIAN_POINT('Ctrl Pts',(-50.158698840709,58.6437477551811,73.8360406501164));
#215576=CARTESIAN_POINT('Ctrl Pts',(-50.1838000986255,59.0521723087971,
74.511108620969));
#215577=CARTESIAN_POINT('Ctrl Pts',(-50.193034235206,59.2162213075673,74.7547833431456));
#215578=CARTESIAN_POINT('Ctrl Pts',(-50.2398490858395,60.1046299937437,
75.9456002244812));
#215579=CARTESIAN_POINT('Ctrl Pts',(-50.2781407182629,60.9985364195232,
76.7516063210605));
#215580=CARTESIAN_POINT('Ctrl Pts',(-50.353271030748,63.0396463716975,77.9685817028853));
#215581=CARTESIAN_POINT('Ctrl Pts',(-50.3914240457153,64.165605894035,78.3704740552869));
#215582=CARTESIAN_POINT('Ctrl Pts',(-50.4451731795604,65.842168222641,78.6204871531557));
#215583=CARTESIAN_POINT('Ctrl Pts',(-50.461353595056,66.3528744867564,78.6531063296549));
#215584=CARTESIAN_POINT('Ctrl Pts',(-50.4943139559629,67.378474783785,78.6321176486079));
#215585=CARTESIAN_POINT('Ctrl Pts',(-50.511036904118,67.8915159290587,78.5778473333094));
#215586=CARTESIAN_POINT('Ctrl Pts',(-50.5432465355915,68.8801642663428,
78.3873851183966));
#215587=CARTESIAN_POINT('Ctrl Pts',(-50.5587389673875,69.354788650321,78.2552951422154));
#215588=CARTESIAN_POINT('Ctrl Pts',(-50.583940284417,70.0958202741404,77.9826496449354));
#215589=CARTESIAN_POINT('Ctrl Pts',(-50.5934933843494,70.3700261754071,
77.8661747027161));
#215590=CARTESIAN_POINT('Ctrl Pts',(-50.6219859413768,71.1652013490339,
77.4812779949944));
#215591=CARTESIAN_POINT('Ctrl Pts',(-50.6409237167971,71.6664960982399,
77.1757422003745));
#215592=CARTESIAN_POINT('Ctrl Pts',(-50.6763378807529,72.5574722536808,
76.5068886530519));
#215593=CARTESIAN_POINT('Ctrl Pts',(-50.6930710464352,72.9515749083736,
76.1534290051907));
#215594=CARTESIAN_POINT('Ctrl Pts',(-50.7260223099667,73.6523580210189,
75.4050648915069));
#215595=CARTESIAN_POINT('Ctrl Pts',(-50.7421497152092,73.9616699917789,
75.0151501759862));
#215596=CARTESIAN_POINT('Ctrl Pts',(-50.7748067987056,74.5273539247205,
74.1678795193282));
#215597=CARTESIAN_POINT('Ctrl Pts',(-50.7912098810465,74.779226674521,73.7096867698027));
#215598=CARTESIAN_POINT('Ctrl Pts',(-50.8283330401849,75.2505826166256,
72.6443390962046));
#215599=CARTESIAN_POINT('Ctrl Pts',(-50.8491231513436,75.4476356806003,
72.0303058935975));
#215600=CARTESIAN_POINT('Ctrl Pts',(-50.8874941927951,75.6904825234003,
70.8595051234087));
#215601=CARTESIAN_POINT('Ctrl Pts',(-50.9048197603625,75.7531415644071,
70.3092523220413));
#215602=CARTESIAN_POINT('Ctrl Pts',(-50.9317880127308,75.772030474855,69.4604356269019));
#215603=CARTESIAN_POINT('Ctrl Pts',(-50.9412446810199,75.7641302129071,
69.1640047887181));
#215604=CARTESIAN_POINT('Ctrl Pts',(-50.9696989533205,75.6971824565697,
68.2794181303715));
#215605=CARTESIAN_POINT('Ctrl Pts',(-50.9887247546056,75.5952797477216,
67.6960827496695));
#215606=CARTESIAN_POINT('Ctrl Pts',(-51.0250367061594,75.2883452243661,
66.5885792041862));
#215607=CARTESIAN_POINT('Ctrl Pts',(-51.0425797657269,75.0899108323937,
66.0652813064536));
#215608=CARTESIAN_POINT('Ctrl Pts',(-51.0775110688586,74.6092042509539,
65.0815682163962));
#215609=CARTESIAN_POINT('Ctrl Pts',(-51.0947969734681,74.3314962344145,
64.6214136999578));
#215610=CARTESIAN_POINT('Ctrl Pts',(-51.1279166649473,73.7140401509426,
63.7771410902842));
#215611=CARTESIAN_POINT('Ctrl Pts',(-51.1438020793535,73.3791882248007,
63.3918640769683));
#215612=CARTESIAN_POINT('Ctrl Pts',(-51.1792414538755,72.5752140017154,
62.6102914883718));
#215613=CARTESIAN_POINT('Ctrl Pts',(-51.1988411835993,72.094690709306,62.2292704752158));
#215614=CARTESIAN_POINT('Ctrl Pts',(-51.2357170665386,71.1169936572975,
61.6032010717346));
#215615=CARTESIAN_POINT('Ctrl Pts',(-51.2527597871759,70.6285324823468,
61.3495324946817));
#215616=CARTESIAN_POINT('Ctrl Pts',(-51.287916534422,69.5938927469422,60.9261632208876));
#215617=CARTESIAN_POINT('Ctrl Pts',(-51.3060043217276,69.0485740446644,
60.7606719443466));
#215618=CARTESIAN_POINT('Ctrl Pts',(-51.3421598214664,67.934464811533,60.533808294777));
#215619=CARTESIAN_POINT('Ctrl Pts',(-51.3598341688668,67.3681329371056,
60.4728847533926));
#215620=CARTESIAN_POINT('Ctrl Pts',(-51.4002746967788,66.0763747861971,
60.4555165893947));
#215621=CARTESIAN_POINT('Ctrl Pts',(-51.4232630002298,65.3543436284031,
60.5321993747226));
#215622=CARTESIAN_POINT('Ctrl Pts',(-51.4636153297325,64.1118883107877,
60.8166375859706));
#215623=CARTESIAN_POINT('Ctrl Pts',(-51.4806582044059,63.586988269362,60.9882165208285));
#215624=CARTESIAN_POINT('Ctrl Pts',(-51.5060913559596,62.8411300632569,
61.3095628688017));
#215625=CARTESIAN_POINT('Ctrl Pts',(-51.5142995740101,62.6059561312179,
61.4231290637743));
#215626=CARTESIAN_POINT('Ctrl Pts',(-51.5379184528011,61.9478040952251,
61.7766731081608));
#215627=CARTESIAN_POINT('Ctrl Pts',(-51.5534318886634,61.5387509664118,
62.0406616117935));
#215628=CARTESIAN_POINT('Ctrl Pts',(-51.5780070871286,60.9191133937169,
62.5149219064706));
#215629=CARTESIAN_POINT('Ctrl Pts',(-51.5871702059434,60.6942752001404,
62.705000669812));
#215630=CARTESIAN_POINT('Ctrl Pts',(-51.6290211295816,59.7134012114723,
63.6194479110496));
#215631=CARTESIAN_POINT('Ctrl Pts',(-51.6623823994008,59.0767722619121,
64.4601621641708));
#215632=CARTESIAN_POINT('Ctrl Pts',(-51.7031473001465,58.4805834086687,
65.6171256403115));
#215633=CARTESIAN_POINT('Ctrl Pts',(-51.7110858807856,58.373524068264,65.8482677588338));
#215634=CARTESIAN_POINT('Ctrl Pts',(-51.7190489450981,58.276355535683,66.0834535849086));
#215635=CARTESIAN_POINT('Ctrl Pts',(-51.9229031375498,58.276355530746,66.083453596858));
#215636=CARTESIAN_POINT('Ctrl Pts',(-51.9066584569547,58.4689780276898,
65.6172318680371));
#215637=CARTESIAN_POINT('Ctrl Pts',(-51.8903671818083,58.7001181376414,
65.1677498718171));
#215638=CARTESIAN_POINT('Ctrl Pts',(-51.8567750261386,59.2600464270107,
64.2711065545253));
#215639=CARTESIAN_POINT('Ctrl Pts',(-51.8393335771109,59.5947731060437,
63.8301720239684));
#215640=CARTESIAN_POINT('Ctrl Pts',(-51.8064926448627,60.2848652969986,
63.0750287758916));
#215641=CARTESIAN_POINT('Ctrl Pts',(-51.7912378456738,60.6287658210384,
62.7528659666705));
#215642=CARTESIAN_POINT('Ctrl Pts',(-51.7540899580665,61.5303275168572,
62.0309817897715));
#215643=CARTESIAN_POINT('Ctrl Pts',(-51.7326467220305,62.1112109213727,
61.6648951873634));
#215644=CARTESIAN_POINT('Ctrl Pts',(-51.6958595553788,63.144881879531,61.1661829224993));
#215645=CARTESIAN_POINT('Ctrl Pts',(-51.6808649979164,63.5768836711471,
60.9970743285224));
#215646=CARTESIAN_POINT('Ctrl Pts',(-51.6475424666645,64.5645712707152,
60.6951006710349));
#215647=CARTESIAN_POINT('Ctrl Pts',(-51.6295815813372,65.1237046144991,
60.5801318943607));
#215648=CARTESIAN_POINT('Ctrl Pts',(-51.6020861452689,65.9822427504294,
60.4862893635124));
#215649=CARTESIAN_POINT('Ctrl Pts',(-51.5926856426807,66.2759498740023,
60.4685408819194));
#215650=CARTESIAN_POINT('Ctrl Pts',(-51.5658158243222,67.111431733078,60.4586485236363));
#215651=CARTESIAN_POINT('Ctrl Pts',(-51.548234974849,67.6523594844531,60.5006281173763));
#215652=CARTESIAN_POINT('Ctrl Pts',(-51.5116901283149,68.782621052906,60.690859871711));
#215653=CARTESIAN_POINT('Ctrl Pts',(-51.4926875717132,69.3674141003031,
60.8504690468474));
#215654=CARTESIAN_POINT('Ctrl Pts',(-51.4573922890429,70.3966496544497,
61.2451115053121));
#215655=CARTESIAN_POINT('Ctrl Pts',(-51.4412970110226,70.8458665983852,
61.4611181558444));
#215656=CARTESIAN_POINT('Ctrl Pts',(-51.4053923165603,71.8123189681,62.027741444852));
#215657=CARTESIAN_POINT('Ctrl Pts',(-51.3859380166555,72.3157147916126,
62.3970486157093));
#215658=CARTESIAN_POINT('Ctrl Pts',(-51.3500832598207,73.1511722389079,
63.1531936849593));
#215659=CARTESIAN_POINT('Ctrl Pts',(-51.3338769617531,73.496155691826,63.5219916343335));
#215660=CARTESIAN_POINT('Ctrl Pts',(-51.2984535933001,74.1811404506166,
64.3885382682181));
#215661=CARTESIAN_POINT('Ctrl Pts',(-51.2796655308721,74.5059119262911,
64.8953350221338));
#215662=CARTESIAN_POINT('Ctrl Pts',(-51.2420078521155,75.0465997312735,
65.9573889766624));
#215663=CARTESIAN_POINT('Ctrl Pts',(-51.2231169997875,75.2628083268442,
66.5092501744975));
#215664=CARTESIAN_POINT('Ctrl Pts',(-51.1853034100103,75.5849402611807,
67.6470109015176));
#215665=CARTESIAN_POINT('Ctrl Pts',(-51.1668269068216,75.6901165191788,
68.2302007927246));
#215666=CARTESIAN_POINT('Ctrl Pts',(-51.1388976071206,75.7619025294626,
69.1150714484619));
#215667=CARTESIAN_POINT('Ctrl Pts',(-51.1295337372783,75.7714024648193,
69.4116741122853));
#215668=CARTESIAN_POINT('Ctrl Pts',(-51.1030906296812,75.7573250217166,
70.2440195880202));
#215669=CARTESIAN_POINT('Ctrl Pts',(-51.0858958042147,75.700899034983,70.7779825825479));
#215670=CARTESIAN_POINT('Ctrl Pts',(-51.0520446944832,75.4942747147157,
71.8315741008777));
#215671=CARTESIAN_POINT('Ctrl Pts',(-51.0353585289282,75.3441563616161,
72.3490678790225));
#215672=CARTESIAN_POINT('Ctrl Pts',(-51.0027307823126,74.9687850928878,
73.3139374287333));
#215673=CARTESIAN_POINT('Ctrl Pts',(-50.9868874434386,74.7506283652911,
73.7620299782548));
#215674=CARTESIAN_POINT('Ctrl Pts',(-50.9524775979752,74.1982749419539,
74.6937510060772));
#215675=CARTESIAN_POINT('Ctrl Pts',(-50.9343115959941,73.851662385872,75.1674547776925));
#215676=CARTESIAN_POINT('Ctrl Pts',(-50.9066674140993,73.2640931755435,
75.8263331465221));
#215677=CARTESIAN_POINT('Ctrl Pts',(-50.8973217425598,73.0555284415371,
76.0383104446865));
#215678=CARTESIAN_POINT('Ctrl Pts',(-50.8710903428876,72.4457864247927,
76.6000898098844));
#215679=CARTESIAN_POINT('Ctrl Pts',(-50.854099884282,72.0237359436145,76.9254649701064));
#215680=CARTESIAN_POINT('Ctrl Pts',(-50.8182450177606,71.0611827188948,
77.5411462999966));
#215681=CARTESIAN_POINT('Ctrl Pts',(-50.7993634060826,70.5148462065648,
77.8175403811517));
#215682=CARTESIAN_POINT('Ctrl Pts',(-50.7652851830786,69.5065847435217,
78.2059023661214));
#215683=CARTESIAN_POINT('Ctrl Pts',(-50.7503208419736,69.0558068048182,
78.3405130464432));
#215684=CARTESIAN_POINT('Ctrl Pts',(-50.7112164587197,67.8481684378219,
78.6013405062761));
#215685=CARTESIAN_POINT('Ctrl Pts',(-50.6876878372036,67.0822485392285,
78.6677751324582));
#215686=CARTESIAN_POINT('Ctrl Pts',(-50.6488921054763,65.855090021021,78.6190672115604));
#215687=CARTESIAN_POINT('Ctrl Pts',(-50.6341413594616,65.3951515695407,
78.5655047520926));
#215688=CARTESIAN_POINT('Ctrl Pts',(-50.5963750843635,64.2249825391195,
78.33779364235));
#215689=CARTESIAN_POINT('Ctrl Pts',(-50.5738938554618,63.5280612165873,
78.112651914641));
#215690=CARTESIAN_POINT('Ctrl Pts',(-50.5368219599937,62.4639131746578,
77.6210734798956));
#215691=CARTESIAN_POINT('Ctrl Pts',(-50.5226929158353,62.0763273093222,
77.406444917496));
#215692=CARTESIAN_POINT('Ctrl Pts',(-50.4751077633651,60.8242974683905,
76.5884753004597));
#215693=CARTESIAN_POINT('Ctrl Pts',(-50.4426746836312,60.0494402382401,
75.86365452694));
#215694=CARTESIAN_POINT('Ctrl Pts',(-50.3996305760705,59.2396772045108,
74.7882500359777));
#215695=CARTESIAN_POINT('Ctrl Pts',(-50.3902460389154,59.0747993299534,
74.545717979835));
#215696=CARTESIAN_POINT('Ctrl Pts',(-50.3650565516947,58.6605054081258,
73.8680062214918));
#215697=CARTESIAN_POINT('Ctrl Pts',(-50.3494191532467,58.434900102059,73.4194768297401));
#215698=CARTESIAN_POINT('Ctrl Pts',(-50.304431063181,57.9031719808351,72.1011313949032));
#215699=CARTESIAN_POINT('Ctrl Pts',(-50.2747514895586,57.6905336946499,
71.2002732586477));
#215700=CARTESIAN_POINT('Ctrl Pts',(-50.2274030973064,57.570396953899,69.7058979582394));
#215701=CARTESIAN_POINT('Ctrl Pts',(-50.2091218482721,57.5792338353981,
69.12577343449));
#215702=CARTESIAN_POINT('Ctrl Pts',(-50.1724353252622,57.7054849798947,
67.9897595629765));
#215703=CARTESIAN_POINT('Ctrl Pts',(-50.1542207163723,57.8198572872672,
67.4360846626437));
#215704=CARTESIAN_POINT('Ctrl Pts',(-50.1271781319156,58.0690980510039,
66.6209286899905));
#215705=CARTESIAN_POINT('Ctrl Pts',(-50.1180768395745,58.1664030290617,
66.3495816246336));
#215706=CARTESIAN_POINT('Ctrl Pts',(-50.1089321285242,58.276355535683,66.0834535849087));
#215707=CARTESIAN_POINT('Origin',(-61.5936228798467,66.6770802411476,69.5524554490054));
#215708=CARTESIAN_POINT('',(-62.6023291620188,58.2758162839759,66.0814193573862));
#215709=CARTESIAN_POINT('',(-62.8075051404766,58.2758467353478,66.0813456540807));
#215710=CARTESIAN_POINT('',(-61.5936228798467,58.2758162839768,66.0814193573839));
#215711=CARTESIAN_POINT('',(-62.6023317437084,58.2757853463631,66.0814942394464));
#215712=CARTESIAN_POINT('Ctrl Pts',(-62.6023291620188,58.2758162839749,
66.0814193573885));
#215713=CARTESIAN_POINT('Ctrl Pts',(-62.6023301287421,58.2758046991418,
66.0814473972124));
#215714=CARTESIAN_POINT('Ctrl Pts',(-62.6023310954659,58.2757931144483,
66.0814754370963));
#215715=CARTESIAN_POINT('Ctrl Pts',(-62.6023320621901,58.2757815298943,
66.0815034770401));
#215716=CARTESIAN_POINT('',(-62.7290132089978,57.5946335568169,69.9232336695064));
#215717=CARTESIAN_POINT('Ctrl Pts',(-62.7269877844547,57.5945799011542,
69.9232858703779));
#215718=CARTESIAN_POINT('Ctrl Pts',(-62.7059767167849,57.5678166503396,
69.2677915511051));
#215719=CARTESIAN_POINT('Ctrl Pts',(-62.6852394928937,57.6120930723197,
68.6113136984255));
#215720=CARTESIAN_POINT('Ctrl Pts',(-62.6544240531954,57.7834457997657,
67.6449849877674));
#215721=CARTESIAN_POINT('Ctrl Pts',(-62.6442290356214,57.8574078132741,
67.3279207418244));
#215722=CARTESIAN_POINT('Ctrl Pts',(-62.6234162513844,58.040356981802,66.6984486864255));
#215723=CARTESIAN_POINT('Ctrl Pts',(-62.6128525065426,58.1497114542633,
66.3866500398473));
#215724=CARTESIAN_POINT('Ctrl Pts',(-62.6023317437084,58.2757853463631,
66.0814942394464));
#215725=CARTESIAN_POINT('',(-62.9304638037219,57.5945049974057,69.9232129291766));
#215726=CARTESIAN_POINT('',(-62.9299583493521,57.5945773164048,69.9232225584337));
#215727=CARTESIAN_POINT('Ctrl Pts',(-62.9325038108326,57.5945747891981,
69.9231606454938));
#215728=CARTESIAN_POINT('Ctrl Pts',(-62.9116762545802,57.5675772732949,
69.2617048911573));
#215729=CARTESIAN_POINT('Ctrl Pts',(-62.8907033963375,57.6129186405627,
68.5992795600948));
#215730=CARTESIAN_POINT('Ctrl Pts',(-62.85911645307,57.7866934413854,67.6304133938896));
#215731=CARTESIAN_POINT('Ctrl Pts',(-62.8487672427708,57.8604331702437,
67.3163960962927));
#215732=CARTESIAN_POINT('Ctrl Pts',(-62.8281485912862,58.0423315204011,
66.6928186356272));
#215733=CARTESIAN_POINT('Ctrl Pts',(-62.8178556351171,58.1508626454292,
66.3838559993944));
#215734=CARTESIAN_POINT('Ctrl Pts',(-62.8075076622655,58.2758162839768,
66.0814193573839));
#215735=CARTESIAN_POINT('Origin',(-61.5936228798467,66.6770802411476,69.5524554490054));
#215736=CARTESIAN_POINT('',(-60.993278523103,58.2758162839768,66.0814193573839));
#215737=CARTESIAN_POINT('Ctrl Pts',(-62.8075051404766,58.2758467353478,
66.0813456540807));
#215738=CARTESIAN_POINT('Ctrl Pts',(-62.7827585996791,58.5746718414298,
65.3580900839858));
#215739=CARTESIAN_POINT('Ctrl Pts',(-62.7575867818917,58.9656412879929,
64.6764534053843));
#215740=CARTESIAN_POINT('Ctrl Pts',(-62.7076612405528,59.9079275399909,
63.4361951464086));
#215741=CARTESIAN_POINT('Ctrl Pts',(-62.6834874527537,60.453825861867,62.8815352655141));
#215742=CARTESIAN_POINT('Ctrl Pts',(-62.6418528328706,61.4740133937407,
62.0805138507002));
#215743=CARTESIAN_POINT('Ctrl Pts',(-62.6249116919099,61.9115880273756,
61.7941115554923));
#215744=CARTESIAN_POINT('Ctrl Pts',(-62.5926328302465,62.8008280984047,
61.3158394451234));
#215745=CARTESIAN_POINT('Ctrl Pts',(-62.5772771158596,63.2482362687151,
61.1197685888594));
#215746=CARTESIAN_POINT('Ctrl Pts',(-62.5522217402567,63.9905960020285,
60.8633383483942));
#215747=CARTESIAN_POINT('Ctrl Pts',(-62.5426740764964,64.2765858947229,
60.7800225781601));
#215748=CARTESIAN_POINT('Ctrl Pts',(-62.5141917610593,65.1358303777023,
60.5748768688081));
#215749=CARTESIAN_POINT('Ctrl Pts',(-62.4952519587902,65.7173373284889,
60.494239432827));
#215750=CARTESIAN_POINT('Ctrl Pts',(-62.4586443494421,66.8678934254916,
60.4467937668689));
#215751=CARTESIAN_POINT('Ctrl Pts',(-62.4407218880458,67.4341768201499,
60.4763172308115));
#215752=CARTESIAN_POINT('Ctrl Pts',(-62.4067121422934,68.4796855133982,
60.6294031440396));
#215753=CARTESIAN_POINT('Ctrl Pts',(-62.3907689417157,68.9587860956276,
60.7397335511125));
#215754=CARTESIAN_POINT('Ctrl Pts',(-62.3588267718022,69.9100311455759,
61.0416056107918));
#215755=CARTESIAN_POINT('Ctrl Pts',(-62.342864162994,70.3797482102385,61.2351967274013));
#215756=CARTESIAN_POINT('Ctrl Pts',(-62.3064768420909,71.3942058159256,
61.7563561812658));
#215757=CARTESIAN_POINT('Ctrl Pts',(-62.2859769344181,71.9257607533805,
62.1038465208793));
#215758=CARTESIAN_POINT('Ctrl Pts',(-62.2480189698315,72.8422683937824,
62.8501602504118));
#215759=CARTESIAN_POINT('Ctrl Pts',(-62.2308009241964,73.2354454508964,
63.2343739445442));
#215760=CARTESIAN_POINT('Ctrl Pts',(-62.1951974733025,73.9622073414218,
64.0859907161967));
#215761=CARTESIAN_POINT('Ctrl Pts',(-62.1768342962594,74.2910940309015,
64.5542461698788));
#215762=CARTESIAN_POINT('Ctrl Pts',(-62.1402813141876,74.8541666534339,
65.5418640199265));
#215763=CARTESIAN_POINT('Ctrl Pts',(-62.1224831178287,75.087935532165,66.0585888868009));
#215764=CARTESIAN_POINT('Ctrl Pts',(-62.0817639257673,75.5068656162761,
67.275558289919));
#215765=CARTESIAN_POINT('Ctrl Pts',(-62.0586270483711,75.6596174315433,
67.9829420927733));
#215766=CARTESIAN_POINT('Ctrl Pts',(-62.0175060546965,75.7801278767569,
69.2636845606806));
#215767=CARTESIAN_POINT('Ctrl Pts',(-61.99987197195,75.7804715495623,69.8301848231031));
#215768=CARTESIAN_POINT('Ctrl Pts',(-61.9726963351648,75.7009037857973,
70.6869416792319));
#215769=CARTESIAN_POINT('Ctrl Pts',(-61.9633329853358,75.6593103335437,
70.9793370954806));
#215770=CARTESIAN_POINT('Ctrl Pts',(-61.9349406935905,75.4911724330965,
71.8536028518237));
#215771=CARTESIAN_POINT('Ctrl Pts',(-61.915867253474,75.3216558936171,72.4255773475958));
#215772=CARTESIAN_POINT('Ctrl Pts',(-61.881532200228,74.9100731217729,73.4376279523369));
#215773=CARTESIAN_POINT('Ctrl Pts',(-61.8659985082016,74.6851893526394,
73.8822273586314));
#215774=CARTESIAN_POINT('Ctrl Pts',(-61.833264459617,74.1444827544418,74.7635106413054));
#215775=CARTESIAN_POINT('Ctrl Pts',(-61.8160830782531,73.823960567157,75.1950871383287));
#215776=CARTESIAN_POINT('Ctrl Pts',(-61.7822572443624,73.1135399396358,
75.9932919904183));
#215777=CARTESIAN_POINT('Ctrl Pts',(-61.7657762630245,72.7256138598147,
76.3588960487237));
#215778=CARTESIAN_POINT('Ctrl Pts',(-61.7312540836744,71.8628284640962,
77.0397003278377));
#215779=CARTESIAN_POINT('Ctrl Pts',(-61.7132339311628,71.3858258825639,
77.3485136648221));
#215780=CARTESIAN_POINT('Ctrl Pts',(-61.6772032272859,70.3799360315444,
77.8735394216446));
#215781=CARTESIAN_POINT('Ctrl Pts',(-61.6595801463188,69.853192360704,78.0884905207624));
#215782=CARTESIAN_POINT('Ctrl Pts',(-61.6237352249995,68.7564464131023,
78.4203673109301));
#215783=CARTESIAN_POINT('Ctrl Pts',(-61.6054645307211,68.1883319352046,
78.5346450594559));
#215784=CARTESIAN_POINT('Ctrl Pts',(-61.5494981065453,66.4354979537243,
78.7161279993807));
#215785=CARTESIAN_POINT('Ctrl Pts',(-61.5132749974563,65.2452066928191,
78.6067908307184));
#215786=CARTESIAN_POINT('Ctrl Pts',(-61.4439774707116,63.1528917115972,
77.9906812584831));
#215787=CARTESIAN_POINT('Ctrl Pts',(-61.4133567723254,62.2492109921292,
77.5535520320839));
#215788=CARTESIAN_POINT('Ctrl Pts',(-61.372511416718,61.195681842865,76.8098067289323));
#215789=CARTESIAN_POINT('Ctrl Pts',(-61.3631996323689,60.9650192984978,
76.6296890041399));
#215790=CARTESIAN_POINT('Ctrl Pts',(-61.3251373636124,60.0585343567079,
75.8486100481436));
#215791=CARTESIAN_POINT('Ctrl Pts',(-61.2973225302177,59.465488555232,75.1595635958174));
#215792=CARTESIAN_POINT('Ctrl Pts',(-61.2495715790222,58.6638192095476,
73.8858242979422));
#215793=CARTESIAN_POINT('Ctrl Pts',(-61.2302911091849,58.3949457432561,
73.3467533407717));
#215794=CARTESIAN_POINT('Ctrl Pts',(-61.1925163314495,57.9681958687,72.2251964261833));
#215795=CARTESIAN_POINT('Ctrl Pts',(-61.1738295834256,57.8110238947228,
71.6456003758838));
#215796=CARTESIAN_POINT('Ctrl Pts',(-61.1385558059292,57.6277603155242,
70.5519746426347));
#215797=CARTESIAN_POINT('Ctrl Pts',(-61.1221533967664,57.5859523878683,
70.0429852871717));
#215798=CARTESIAN_POINT('Ctrl Pts',(-61.0966297976346,57.5876547657298,
69.2399596518455));
#215799=CARTESIAN_POINT('Ctrl Pts',(-61.0874121528402,57.602464249246,68.9469350082234));
#215800=CARTESIAN_POINT('Ctrl Pts',(-61.0501113182517,57.7193395302956,
67.7687383620738));
#215801=CARTESIAN_POINT('Ctrl Pts',(-61.0216484906896,57.9369166166898,
66.9016890073447));
#215802=CARTESIAN_POINT('Ctrl Pts',(-60.9932785231031,58.2758162839768,
66.0814193573839));
#215803=CARTESIAN_POINT('',(-60.7885639123434,58.2758162839768,66.0814193573839));
#215804=CARTESIAN_POINT('',(-61.5936228798467,58.2758162839768,66.0814193573839));
#215805=CARTESIAN_POINT('Ctrl Pts',(-60.7885639123434,58.2758162839768,
66.0814193573839));
#215806=CARTESIAN_POINT('Ctrl Pts',(-60.8165473472842,57.9369608312523,
66.9015819908227));
#215807=CARTESIAN_POINT('Ctrl Pts',(-60.8442152543235,57.7193974192671,
67.7685080573625));
#215808=CARTESIAN_POINT('Ctrl Pts',(-60.8820788621428,57.6024881991777,
68.9465773614098));
#215809=CARTESIAN_POINT('Ctrl Pts',(-60.8914689841111,57.5876670022784,
69.2396014868228));
#215810=CARTESIAN_POINT('Ctrl Pts',(-60.9169257724154,57.5859338443228,
70.0423343359673));
#215811=CARTESIAN_POINT('Ctrl Pts',(-60.9328238216174,57.627672833315,70.5510319849962));
#215812=CARTESIAN_POINT('Ctrl Pts',(-60.9775352109377,57.8608162618331,
71.9434798747403));
#215813=CARTESIAN_POINT('Ctrl Pts',(-61.0066469216558,58.1415007775707,
72.8062831413013));
#215814=CARTESIAN_POINT('Ctrl Pts',(-61.0534060471856,58.8027561945617,
74.1304666122758));
#215815=CARTESIAN_POINT('Ctrl Pts',(-61.071649492068,59.1095844962329,74.6215940641858));
#215816=CARTESIAN_POINT('Ctrl Pts',(-61.1078882009044,59.7961967047495,
75.5179145969811));
#215817=CARTESIAN_POINT('Ctrl Pts',(-61.1257064779507,60.1705752195452,
75.9241636522968));
#215818=CARTESIAN_POINT('Ctrl Pts',(-61.1587188475635,60.9416661273783,
76.6216060002487));
#215819=CARTESIAN_POINT('Ctrl Pts',(-61.1741112087812,61.3296977850336,
76.9195013345673));
#215820=CARTESIAN_POINT('Ctrl Pts',(-61.208855899165,62.2422348086538,77.5098160220488));
#215821=CARTESIAN_POINT('Ctrl Pts',(-61.228270860995,62.7755579818415,77.7844390413501));
#215822=CARTESIAN_POINT('Ctrl Pts',(-61.2642438684955,63.8191658535208,
78.1974642400836));
#215823=CARTESIAN_POINT('Ctrl Pts',(-61.2807198566024,64.3221095717221,
78.3477933918406));
#215824=CARTESIAN_POINT('Ctrl Pts',(-61.3283324670262,65.783379249252,78.6501568821174));
#215825=CARTESIAN_POINT('Ctrl Pts',(-61.3597192290084,66.7568480676607,
78.693599470245));
#215826=CARTESIAN_POINT('Ctrl Pts',(-61.4281169265037,68.8961192897166,
78.446827760361));
#215827=CARTESIAN_POINT('Ctrl Pts',(-61.4664202734848,70.0356498357558,
78.0820517269475));
#215828=CARTESIAN_POINT('Ctrl Pts',(-61.5224094342196,71.5794231561345,
77.2291128902152));
#215829=CARTESIAN_POINT('Ctrl Pts',(-61.5407709521873,72.0579438740127,
76.901627865946));
#215830=CARTESIAN_POINT('Ctrl Pts',(-61.5776828394934,72.937946573046,76.1670772939815));
#215831=CARTESIAN_POINT('Ctrl Pts',(-61.5960250555282,73.3387725571802,
75.7632155309537));
#215832=CARTESIAN_POINT('Ctrl Pts',(-61.6320400842896,74.0596370682187,
74.8862341888564));
#215833=CARTESIAN_POINT('Ctrl Pts',(-61.6499384167133,74.3781316996655,
74.4150828476952));
#215834=CARTESIAN_POINT('Ctrl Pts',(-61.6855335246671,74.9114633913786,
73.4408177884735));
#215835=CARTESIAN_POINT('Ctrl Pts',(-61.7031153881128,75.1290740315015,
72.9418853840914));
#215836=CARTESIAN_POINT('Ctrl Pts',(-61.7368933998136,75.4651026724446,
71.9336157900771));
#215837=CARTESIAN_POINT('Ctrl Pts',(-61.7531680691965,75.5868127939801,
71.4275376897543));
#215838=CARTESIAN_POINT('Ctrl Pts',(-61.7857433181699,75.7403393205686,
70.4139912827648));
#215839=CARTESIAN_POINT('Ctrl Pts',(-61.8019744568581,75.77422227908,69.9086982042928));
#215840=CARTESIAN_POINT('Ctrl Pts',(-61.8373848076953,75.7560669168494,
68.8029687331288));
#215841=CARTESIAN_POINT('Ctrl Pts',(-61.8561363593999,75.6867723500449,
68.2051688784902));
#215842=CARTESIAN_POINT('Ctrl Pts',(-61.8937598743357,75.4331074672901,
67.040131079595));
#215843=CARTESIAN_POINT('Ctrl Pts',(-61.9126494440181,75.2509564655508,
66.4753756260395));
#215844=CARTESIAN_POINT('Ctrl Pts',(-61.9503885951798,74.7802486150384,
65.3911999619088));
#215845=CARTESIAN_POINT('Ctrl Pts',(-61.968795420232,74.4931720024805,64.8741972967853));
#215846=CARTESIAN_POINT('Ctrl Pts',(-61.9966562260526,73.9894400224411,
64.1444245840252));
#215847=CARTESIAN_POINT('Ctrl Pts',(-62.0060150486286,73.8089918375229,
63.9085880933557));
#215848=CARTESIAN_POINT('Ctrl Pts',(-62.0324031298607,73.271861586515,63.2735741056103));
#215849=CARTESIAN_POINT('Ctrl Pts',(-62.0495464558552,72.8910095255566,
62.8964371446764));
#215850=CARTESIAN_POINT('Ctrl Pts',(-62.0819374027553,72.0991586949565,
62.2398540898828));
#215851=CARTESIAN_POINT('Ctrl Pts',(-62.0972543547778,71.6940639775007,
61.9562095194195));
#215852=CARTESIAN_POINT('Ctrl Pts',(-62.129099833235,70.8197771606755,61.4446186812144));
#215853=CARTESIAN_POINT('Ctrl Pts',(-62.1456004240847,70.3499645204559,
61.221257008585));
#215854=CARTESIAN_POINT('Ctrl Pts',(-62.1807049022731,69.3148423125416,
60.8338002075288));
#215855=CARTESIAN_POINT('Ctrl Pts',(-62.1989001788807,68.7474384662482,
60.6819222598256));
#215856=CARTESIAN_POINT('Ctrl Pts',(-62.2265394851784,67.8758442776549,
60.53686683111));
#215857=CARTESIAN_POINT('Ctrl Pts',(-62.235884325555,67.5800952234876,60.502459011075));
#215858=CARTESIAN_POINT('Ctrl Pts',(-62.2613184522206,66.7771778698587,
60.4488021160657));
#215859=CARTESIAN_POINT('Ctrl Pts',(-62.2775119444156,66.2692202919945,
60.4573923659707));
#215860=CARTESIAN_POINT('Ctrl Pts',(-62.3087892996319,65.280280849755,60.5571639643559));
#215861=CARTESIAN_POINT('Ctrl Pts',(-62.3238535962417,64.8006291363324,
60.6448601307839));
#215862=CARTESIAN_POINT('Ctrl Pts',(-62.3473142461334,64.0775673291655,
60.8380822025366));
#215863=CARTESIAN_POINT('Ctrl Pts',(-62.3555518205413,63.8278589097013,
60.916501249032));
#215864=CARTESIAN_POINT('Ctrl Pts',(-62.380624321535,63.0830599950247,61.186225556435));
#215865=CARTESIAN_POINT('Ctrl Pts',(-62.3975665990526,62.6010054913371,
61.4101948690422));
#215866=CARTESIAN_POINT('Ctrl Pts',(-62.4359648220922,61.5402401777661,
62.0209777247797));
#215867=CARTESIAN_POINT('Ctrl Pts',(-62.4574452932637,60.9808127241981,
62.4346733468827));
#215868=CARTESIAN_POINT('Ctrl Pts',(-62.4995279255077,60.0106482273865,
63.3404009052831));
#215869=CARTESIAN_POINT('Ctrl Pts',(-62.5197370473476,59.5939033403095,
63.8201297648542));
#215870=CARTESIAN_POINT('Ctrl Pts',(-62.5498902602688,59.0418253317485,
64.6087332374532));
#215871=CARTESIAN_POINT('Ctrl Pts',(-62.5601640094589,58.8679605841081,
64.8882131315763));
#215872=CARTESIAN_POINT('Ctrl Pts',(-62.5810561208043,58.5484688232857,
65.4699227574098));
#215873=CARTESIAN_POINT('Ctrl Pts',(-62.5916621719048,58.4036453073442,
65.7720231602976));
#215874=CARTESIAN_POINT('Ctrl Pts',(-62.6023291620188,58.2758162839749,
66.0814193573885));
#215875=CARTESIAN_POINT('Origin',(-61.5936228798467,66.6770802411476,69.5524554490054));
#215876=CARTESIAN_POINT('',(-58.974273988216,58.2758162753068,66.0814193783688));
#215877=CARTESIAN_POINT('',(-59.1795703763521,58.275816290262,66.0814193421713));
#215878=CARTESIAN_POINT('',(-61.5936228798467,58.2758162839768,66.0814193573839));
#215879=CARTESIAN_POINT('Ctrl Pts',(-58.9742739875024,58.2758162752982,
66.0814193783896));
#215880=CARTESIAN_POINT('Ctrl Pts',(-58.9911038138538,58.0715593177539,
66.5758010506857));
#215881=CARTESIAN_POINT('Ctrl Pts',(-59.0081251209979,57.9113071395147,
67.0873265040614));
#215882=CARTESIAN_POINT('Ctrl Pts',(-59.0633622145753,57.5418582166893,
68.7763376497993));
#215883=CARTESIAN_POINT('Ctrl Pts',(-59.1001880361245,57.5189956372051,
69.9815383517207));
#215884=CARTESIAN_POINT('Ctrl Pts',(-59.1769506047935,57.9415126003576,
72.3381137918141));
#215885=CARTESIAN_POINT('Ctrl Pts',(-59.2141023465274,58.3852626414375,
73.4659946727289));
#215886=CARTESIAN_POINT('Ctrl Pts',(-59.2804378253646,59.5019504018343,
75.1995352173277));
#215887=CARTESIAN_POINT('Ctrl Pts',(-59.3074037942511,60.0693039913178,
75.8539871979905));
#215888=CARTESIAN_POINT('Ctrl Pts',(-59.3567993348846,61.2376021988887,
76.8675410777012));
#215889=CARTESIAN_POINT('Ctrl Pts',(-59.379048121626,61.8040067040322,77.2564515187191));
#215890=CARTESIAN_POINT('Ctrl Pts',(-59.4101600368057,62.665999914094,77.7148996843177));
#215891=CARTESIAN_POINT('Ctrl Pts',(-59.4193782968166,62.929738949022,77.8392941371504));
#215892=CARTESIAN_POINT('Ctrl Pts',(-59.4473201316425,63.7426779625362,
78.1759638046202));
#215893=CARTESIAN_POINT('Ctrl Pts',(-59.4661662278638,64.3069346828376,
78.3477956756026));
#215894=CARTESIAN_POINT('Ctrl Pts',(-59.494716409947,65.1731993978973,78.5221155288877));
#215895=CARTESIAN_POINT('Ctrl Pts',(-59.5042582022465,65.4652465181133,
78.5662183241016));
#215896=CARTESIAN_POINT('Ctrl Pts',(-59.5289780514452,66.2340909413064,
78.6442759770403));
#215897=CARTESIAN_POINT('Ctrl Pts',(-59.5440323453596,66.7123245113538,
78.6549936863834));
#215898=CARTESIAN_POINT('Ctrl Pts',(-59.5674248403096,67.4441681822125,
78.6136986733134));
#215899=CARTESIAN_POINT('Ctrl Pts',(-59.57561052084,67.6984335496873,78.5885712552251));
#215900=CARTESIAN_POINT('Ctrl Pts',(-59.6019313915972,68.5076002506141,
78.4740133444789));
#215901=CARTESIAN_POINT('Ctrl Pts',(-59.6201701450891,69.0554059998211,
78.3438477157663));
#215902=CARTESIAN_POINT('Ctrl Pts',(-59.6512970835278,69.9811404253804,
78.0309581578981));
#215903=CARTESIAN_POINT('Ctrl Pts',(-59.6644189740089,70.3650219160779,
77.8711638200664));
#215904=CARTESIAN_POINT('Ctrl Pts',(-59.6940122776478,71.1947236006463,
77.4570336833513));
#215905=CARTESIAN_POINT('Ctrl Pts',(-59.7105209139073,71.6326795192761,
77.1900915948514));
#215906=CARTESIAN_POINT('Ctrl Pts',(-59.7463544810056,72.5287828863619,
76.534224948955));
#215907=CARTESIAN_POINT('Ctrl Pts',(-59.7652519010259,72.9756540813877,
76.1339068713837));
#215908=CARTESIAN_POINT('Ctrl Pts',(-59.7936257547136,73.5791854720248,
75.4750636182617));
#215909=CARTESIAN_POINT('Ctrl Pts',(-59.8030263097735,73.7677339744296,
75.2479775613684));
#215910=CARTESIAN_POINT('Ctrl Pts',(-59.829384649667,74.2614816435717,74.5907088525881));
#215911=CARTESIAN_POINT('Ctrl Pts',(-59.8464597131991,74.5408036513983,
74.1425531515353));
#215912=CARTESIAN_POINT('Ctrl Pts',(-59.878925249695,75.0023994276505,73.2348115483913));
#215913=CARTESIAN_POINT('Ctrl Pts',(-59.8943318225078,75.1892173679364,
72.7795614929971));
#215914=CARTESIAN_POINT('Ctrl Pts',(-59.9272701617939,75.5040722447159,
71.791144133584));
#215915=CARTESIAN_POINT('Ctrl Pts',(-59.9447982877611,75.6225906238265,
71.2569639124577));
#215916=CARTESIAN_POINT('Ctrl Pts',(-59.9813618271596,75.7684301293272,
70.1263829293776));
#215917=CARTESIAN_POINT('Ctrl Pts',(-59.9999665523777,75.7865036260607,
69.5313429436259));
#215918=CARTESIAN_POINT('Ctrl Pts',(-60.0280581225139,75.7264397887533,
68.6436455588647));
#215919=CARTESIAN_POINT('Ctrl Pts',(-60.0374337131608,75.6920722794492,
68.3496418588188));
#215920=CARTESIAN_POINT('Ctrl Pts',(-60.0645239597047,75.5523465640712,
67.5114130736661));
#215921=CARTESIAN_POINT('Ctrl Pts',(-60.0823494810074,75.4115013628887,
66.9744516372166));
#215922=CARTESIAN_POINT('Ctrl Pts',(-60.1195679273578,75.0095579413445,
65.8660093281956));
#215923=CARTESIAN_POINT('Ctrl Pts',(-60.1390205161559,74.7364157729125,
65.3019042324966));
#215924=CARTESIAN_POINT('Ctrl Pts',(-60.1752363848728,74.1359845803842,
64.3312910834203));
#215925=CARTESIAN_POINT('Ctrl Pts',(-60.1917865248931,73.8275063813815,
63.9162143441071));
#215926=CARTESIAN_POINT('Ctrl Pts',(-60.2231695427559,73.169996016359,63.1729511098809));
#215927=CARTESIAN_POINT('Ctrl Pts',(-60.2379525545349,72.8269866850854,
62.8416666264532));
#215928=CARTESIAN_POINT('Ctrl Pts',(-60.2715699470804,72.000872928672,62.160565141108));
#215929=CARTESIAN_POINT('Ctrl Pts',(-60.2904595269813,71.5061378533602,
61.8282726276767));
#215930=CARTESIAN_POINT('Ctrl Pts',(-60.3279705543224,70.466353576707,61.269085250254));
#215931=CARTESIAN_POINT('Ctrl Pts',(-60.3461616892115,69.9245495720509,
61.0420640976496));
#215932=CARTESIAN_POINT('Ctrl Pts',(-60.3738156326458,69.0806136893065,
60.7808665141748));
#215933=CARTESIAN_POINT('Ctrl Pts',(-60.3831614764318,68.7924150616687,
60.7069423313539));
#215934=CARTESIAN_POINT('Ctrl Pts',(-60.4090671731526,67.9899813686328,
60.542581068052));
#215935=CARTESIAN_POINT('Ctrl Pts',(-60.4257343281076,67.4707817327735,
60.4820867986367));
#215936=CARTESIAN_POINT('Ctrl Pts',(-60.4578635074531,66.4485183276783,
60.451463132225));
#215937=CARTESIAN_POINT('Ctrl Pts',(-60.4733677527643,65.9473848483799,
60.4778837818462));
#215938=CARTESIAN_POINT('Ctrl Pts',(-60.5045987239673,64.9614375358099,
60.6120977543049));
#215939=CARTESIAN_POINT('Ctrl Pts',(-60.5202690540823,64.4781399883781,
60.7185390121146));
#215940=CARTESIAN_POINT('Ctrl Pts',(-60.554551462598,63.4460687161177,61.0358292203882));
#215941=CARTESIAN_POINT('Ctrl Pts',(-60.5727682647228,62.9041818506703,
61.2616412093218));
#215942=CARTESIAN_POINT('Ctrl Pts',(-60.6098300336945,61.8593306985531,
61.8208395923513));
#215943=CARTESIAN_POINT('Ctrl Pts',(-60.6287747734129,61.3601399426014,
62.155244787345));
#215944=CARTESIAN_POINT('Ctrl Pts',(-60.6855784598625,59.9815838596318,
63.2908375436745));
#215945=CARTESIAN_POINT('Ctrl Pts',(-60.7219797380526,59.2222036094218,
64.2174450661231));
#215946=CARTESIAN_POINT('Ctrl Pts',(-60.76945264915,58.5197435485548,65.5302025555244));
#215947=CARTESIAN_POINT('Ctrl Pts',(-60.7790684393769,58.3907983366686,
65.8031178504267));
#215948=CARTESIAN_POINT('Ctrl Pts',(-60.7885639123434,58.2758162839768,
66.0814193573839));
#215949=CARTESIAN_POINT('Ctrl Pts',(-60.9932785231031,58.2758162839768,
66.0814193573839));
#215950=CARTESIAN_POINT('Ctrl Pts',(-60.9836574173467,58.3907473120026,
65.8032413500608));
#215951=CARTESIAN_POINT('Ctrl Pts',(-60.9741335746798,58.5196312768922,
65.5304403346781));
#215952=CARTESIAN_POINT('Ctrl Pts',(-60.9270767181657,59.2219598823845,
64.2177907759692));
#215953=CARTESIAN_POINT('Ctrl Pts',(-60.8888495077651,59.9812789843619,
63.2911689638367));
#215954=CARTESIAN_POINT('Ctrl Pts',(-60.8322317794888,61.3597740556388,
62.1555056628057));
#215955=CARTESIAN_POINT('Ctrl Pts',(-60.8132145108189,61.8589609984774,
61.8210694669032));
#215956=CARTESIAN_POINT('Ctrl Pts',(-60.7750208682129,62.9037877655204,
61.2618208629497));
#215957=CARTESIAN_POINT('Ctrl Pts',(-60.7561185972566,63.4456715069743,
61.0359790233309));
#215958=CARTESIAN_POINT('Ctrl Pts',(-60.721830257427,64.477378335204,60.7187498471518));
#215959=CARTESIAN_POINT('Ctrl Pts',(-60.7061891359679,64.9602845356755,
60.6123406655328));
#215960=CARTESIAN_POINT('Ctrl Pts',(-60.6737997807858,65.9593277127877,
60.4761687121902));
#215961=CARTESIAN_POINT('Ctrl Pts',(-60.6570865355666,66.474199778111,60.4500939653191));
#215962=CARTESIAN_POINT('Ctrl Pts',(-60.6240285138677,67.5037440395565,
60.4853864037791));
#215963=CARTESIAN_POINT('Ctrl Pts',(-60.6078027272971,68.0165517576591,
60.5468497135589));
#215964=CARTESIAN_POINT('Ctrl Pts',(-60.5818657107383,68.8126432717828,
60.7118007384783));
#215965=CARTESIAN_POINT('Ctrl Pts',(-60.5723287908477,69.1007688658806,
60.786410917448));
#215966=CARTESIAN_POINT('Ctrl Pts',(-60.5438441306482,69.9444216977029,
61.0496571008243));
#215967=CARTESIAN_POINT('Ctrl Pts',(-60.5248796499584,70.4859273562666,
61.2780491295712));
#215968=CARTESIAN_POINT('Ctrl Pts',(-60.4896548250228,71.4612757412648,
61.8055946956147));
#215969=CARTESIAN_POINT('Ctrl Pts',(-60.4731368229985,71.8986014309954,
62.0933608398127));
#215970=CARTESIAN_POINT('Ctrl Pts',(-60.4427964367961,72.6411614875954,
62.6794382413306));
#215971=CARTESIAN_POINT('Ctrl Pts',(-60.4291071651479,72.9548101017499,
62.9646837622432));
#215972=CARTESIAN_POINT('Ctrl Pts',(-60.3973406433091,73.6375194682958,
63.6787631400394));
#215973=CARTESIAN_POINT('Ctrl Pts',(-60.3796177587049,73.9887549030509,
64.122226045083));
#215974=CARTESIAN_POINT('Ctrl Pts',(-60.3401194862685,74.6672830748177,
65.1651930946685));
#215975=CARTESIAN_POINT('Ctrl Pts',(-60.3182272479531,74.9728948688753,
65.7747773161216));
#215976=CARTESIAN_POINT('Ctrl Pts',(-60.2784671051933,75.401781746051,66.9400457991524));
#215977=CARTESIAN_POINT('Ctrl Pts',(-60.2609020586654,75.5465592047606,
67.4842568298563));
#215978=CARTESIAN_POINT('Ctrl Pts',(-60.2222460400084,75.7499098948984,
68.6880320557067));
#215979=CARTESIAN_POINT('Ctrl Pts',(-60.2010841832317,75.7886956464272,
69.3477287843693));
#215980=CARTESIAN_POINT('Ctrl Pts',(-60.1621997556977,75.7279122212125,
70.5650223770047));
#215981=CARTESIAN_POINT('Ctrl Pts',(-60.1447616738229,75.6483764654476,
71.1204788855499));
#215982=CARTESIAN_POINT('Ctrl Pts',(-60.1091224528921,75.3858741071912,
72.2190296645011));
#215983=CARTESIAN_POINT('Ctrl Pts',(-60.0909494791804,75.2017370326686,
72.7593112313773));
#215984=CARTESIAN_POINT('Ctrl Pts',(-60.0546575342054,74.7353549782504,
73.7970219676803));
#215985=CARTESIAN_POINT('Ctrl Pts',(-60.0369333867693,74.4543718763219,
74.2922735798259));
#215986=CARTESIAN_POINT('Ctrl Pts',(-60.0008984767205,73.7968468880922,
75.2335348482422));
#215987=CARTESIAN_POINT('Ctrl Pts',(-59.982524972817,73.4199477940229,75.6761361533574));
#215988=CARTESIAN_POINT('Ctrl Pts',(-59.9262689039094,72.1513027115486,
76.9057234160608));
#215989=CARTESIAN_POINT('Ctrl Pts',(-59.8899075616287,71.1455924541413,
77.5568329908592));
#215990=CARTESIAN_POINT('Ctrl Pts',(-59.8225564684792,69.1771385069917,
78.3415598177888));
#215991=CARTESIAN_POINT('Ctrl Pts',(-59.7938698603394,68.2630575438678,
78.551529702784));
#215992=CARTESIAN_POINT('Ctrl Pts',(-59.7478083985132,66.8067769738529,
78.6569038840467));
#215993=CARTESIAN_POINT('Ctrl Pts',(-59.7309666231927,66.2781321343834,
78.6490832631358));
#215994=CARTESIAN_POINT('Ctrl Pts',(-59.7050207793426,65.4596078240484,
78.5654550958333));
#215995=CARTESIAN_POINT('Ctrl Pts',(-59.6958263910263,65.1676876787616,
78.5211865101182));
#215996=CARTESIAN_POINT('Ctrl Pts',(-59.6682566110299,64.3016287448672,
78.3463637163783));
#215997=CARTESIAN_POINT('Ctrl Pts',(-59.6498248026862,63.7374927199421,
78.174195837292));
#215998=CARTESIAN_POINT('Ctrl Pts',(-59.6218885118325,62.9247555053169,
77.8370397192005));
#215999=CARTESIAN_POINT('Ctrl Pts',(-59.6126077341618,62.6610669258908,
77.7124747335175));
#216000=CARTESIAN_POINT('Ctrl Pts',(-59.5819615934409,61.8062678371396,
77.2571863633938));
#216001=CARTESIAN_POINT('Ctrl Pts',(-59.5610950063817,61.2461417411016,
76.873152214441));
#216002=CARTESIAN_POINT('Ctrl Pts',(-59.5125333127205,60.081336540321,75.8666618148354));
#216003=CARTESIAN_POINT('Ctrl Pts',(-59.4850150054097,59.5123514979381,
75.2128184311312));
#216004=CARTESIAN_POINT('Ctrl Pts',(-59.4204115384272,58.3923723042013,
73.4809525463652));
#216005=CARTESIAN_POINT('Ctrl Pts',(-59.3821095492668,57.9466601155748,
72.3541034375975));
#216006=CARTESIAN_POINT('Ctrl Pts',(-59.3068948782278,57.5199243416264,
69.9991888063659));
#216007=CARTESIAN_POINT('Ctrl Pts',(-59.2686839989018,57.5404091526254,
68.7946198347029));
#216008=CARTESIAN_POINT('Ctrl Pts',(-59.2139668682485,57.9075501483386,
67.0993459426679));
#216009=CARTESIAN_POINT('Ctrl Pts',(-59.1969006211707,58.0691564265514,
66.581616980467));
#216010=CARTESIAN_POINT('Ctrl Pts',(-59.1795703768786,58.2758162902684,
66.0814193421557));
#216011=CARTESIAN_POINT('Origin',(-61.5936228798467,66.6770802411476,69.5524554490054));
#216012=CARTESIAN_POINT('',(-57.1603612091034,58.2758162839768,66.0814193573839));
#216013=CARTESIAN_POINT('',(-57.3654750273695,58.2758162995835,66.0814193196097));
#216014=CARTESIAN_POINT('',(-61.5936228798467,58.2758162839768,66.0814193573839));
#216015=CARTESIAN_POINT('Ctrl Pts',(-57.1603612091034,58.2758162839768,
66.0814193573839));
#216016=CARTESIAN_POINT('Ctrl Pts',(-57.1712661222024,58.1452475191716,
66.3974467995468));
#216017=CARTESIAN_POINT('Ctrl Pts',(-57.1822082696841,58.0325603578707,
66.7207210309766));
#216018=CARTESIAN_POINT('Ctrl Pts',(-57.2022902639678,57.8577543618638,
67.3310862654529));
#216019=CARTESIAN_POINT('Ctrl Pts',(-57.2114561398119,57.7908072758794,
67.6161847140629));
#216020=CARTESIAN_POINT('Ctrl Pts',(-57.2488139815612,57.5751044910439,
68.7859228785457));
#216021=CARTESIAN_POINT('Ctrl Pts',(-57.2775002790807,57.5438792129275,
69.6870618058065));
#216022=CARTESIAN_POINT('Ctrl Pts',(-57.3153519316008,57.6781633218177,
70.8696153349638));
#216023=CARTESIAN_POINT('Ctrl Pts',(-57.3245791482665,57.7253640432311,
71.1593761419318));
#216024=CARTESIAN_POINT('Ctrl Pts',(-57.3713979897335,58.0349246889547,
72.6125612709308));
#216025=CARTESIAN_POINT('Ctrl Pts',(-57.4096981557563,58.5104086352701,
73.7185760902699));
#216026=CARTESIAN_POINT('Ctrl Pts',(-57.4848700000108,59.8571791108076,
75.6780789692153));
#216027=CARTESIAN_POINT('Ctrl Pts',(-57.5230595210081,60.7131947610366,
76.5142356270351));
#216028=CARTESIAN_POINT('Ctrl Pts',(-57.5796441116146,62.2072545352926,
77.4902858809949));
#216029=CARTESIAN_POINT('Ctrl Pts',(-57.5986519251277,62.740165289574,77.7676356633207));
#216030=CARTESIAN_POINT('Ctrl Pts',(-57.6368452303225,63.8403216663152,
78.2083996142362));
#216031=CARTESIAN_POINT('Ctrl Pts',(-57.655766277681,64.4039667314164,78.3732002473953));
#216032=CARTESIAN_POINT('Ctrl Pts',(-57.6897387779918,65.4543830364979,
78.5728746111333));
#216033=CARTESIAN_POINT('Ctrl Pts',(-57.7050478799915,65.9356663071116,
78.6251205984618));
#216034=CARTESIAN_POINT('Ctrl Pts',(-57.7370708345046,66.9327473194481,
78.6534610644127));
#216035=CARTESIAN_POINT('Ctrl Pts',(-57.7537613267708,67.4469907610752,
78.6244398746684));
#216036=CARTESIAN_POINT('Ctrl Pts',(-57.7871348189707,68.4754525927143,
78.4782860108434));
#216037=CARTESIAN_POINT('Ctrl Pts',(-57.8036443426759,68.9875269111625,
78.3596362446721));
#216038=CARTESIAN_POINT('Ctrl Pts',(-57.8298588862109,69.7692601472806,
78.1055921361851));
#216039=CARTESIAN_POINT('Ctrl Pts',(-57.8393871631765,70.0473385829312,
77.9998858624186));
#216040=CARTESIAN_POINT('Ctrl Pts',(-57.8678503423865,70.8566869358599,
77.6458904277372));
#216041=CARTESIAN_POINT('Ctrl Pts',(-57.8868175490356,71.3696771208958,
77.3596542156613));
#216042=CARTESIAN_POINT('Ctrl Pts',(-57.9238936972256,72.3291526637955,
76.6953454487992));
#216043=CARTESIAN_POINT('Ctrl Pts',(-57.9422489360509,72.7739700497115,
76.3196359653321));
#216044=CARTESIAN_POINT('Ctrl Pts',(-57.9770719450073,73.5315159120539,
75.5440567629026));
#216045=CARTESIAN_POINT('Ctrl Pts',(-57.9933836481066,73.8526463595235,
75.1554750045786));
#216046=CARTESIAN_POINT('Ctrl Pts',(-58.0187848528206,74.3072610344771,
74.5017513189591));
#216047=CARTESIAN_POINT('Ctrl Pts',(-58.028037645517,74.4628283109775,74.253233815517));
#216048=CARTESIAN_POINT('Ctrl Pts',(-58.0701920469263,75.1141070978494,
73.0915228206117));
#216049=CARTESIAN_POINT('Ctrl Pts',(-58.1037242784327,75.4630308272156,
72.1050031088081));
#216050=CARTESIAN_POINT('Ctrl Pts',(-58.1524676847489,75.7222762122848,
70.5852533494513));
#216051=CARTESIAN_POINT('Ctrl Pts',(-58.1682524561354,75.7655562463051,
70.0833465289902));
#216052=CARTESIAN_POINT('Ctrl Pts',(-58.2047836169146,75.7690907655136,
68.935399037384));
#216053=CARTESIAN_POINT('Ctrl Pts',(-58.2255939759217,75.7024113135775,
68.2919709574742));
#216054=CARTESIAN_POINT('Ctrl Pts',(-58.2552154228212,75.5073742760806,
67.3751486446046));
#216055=CARTESIAN_POINT('Ctrl Pts',(-58.2643773180735,75.4328036095068,
67.092360514292));
#216056=CARTESIAN_POINT('Ctrl Pts',(-58.3045017033824,75.0484451482113,
65.8759556777904));
#216057=CARTESIAN_POINT('Ctrl Pts',(-58.336068754348,74.6019405620201,64.9925218483251));
#216058=CARTESIAN_POINT('Ctrl Pts',(-58.3822526367361,73.7358253968244,
63.8043649141929));
#216059=CARTESIAN_POINT('Ctrl Pts',(-58.3974266595016,73.4178414285652,
63.4345663647324));
#216060=CARTESIAN_POINT('Ctrl Pts',(-58.4279556190062,72.7308328995985,
62.7545488554096));
#216061=CARTESIAN_POINT('Ctrl Pts',(-58.4432567326164,72.3637128552019,
62.4445964553867));
#216062=CARTESIAN_POINT('Ctrl Pts',(-58.4764805164098,71.5137406186533,
61.8351638570873));
#216063=CARTESIAN_POINT('Ctrl Pts',(-58.4940433119074,71.0238101118098,
61.5489677739113));
#216064=CARTESIAN_POINT('Ctrl Pts',(-58.539322767445,69.7133632638821,60.9394952450883));
#216065=CARTESIAN_POINT('Ctrl Pts',(-58.5674459569514,68.8667077798379,
60.686361062059));
#216066=CARTESIAN_POINT('Ctrl Pts',(-58.6096268545979,67.5336098069249,
60.4907231393167));
#216067=CARTESIAN_POINT('Ctrl Pts',(-58.6241568416528,67.0657078671985,
60.4586331073629));
#216068=CARTESIAN_POINT('Ctrl Pts',(-58.6613914551525,65.8811233892635,
60.4690142903216));
#216069=CARTESIAN_POINT('Ctrl Pts',(-58.6843080721214,65.1680742831271,
60.5599388880564));
#216070=CARTESIAN_POINT('Ctrl Pts',(-58.7254861003152,63.8936855332633,
60.878427776453));
#216071=CARTESIAN_POINT('Ctrl Pts',(-58.743973657381,63.3299318828987,61.0799916400413));
#216072=CARTESIAN_POINT('Ctrl Pts',(-58.7812950465515,62.2609946026372,
61.5856475973009));
#216073=CARTESIAN_POINT('Ctrl Pts',(-58.8000170831936,61.7573601925702,
61.8864137427804));
#216074=CARTESIAN_POINT('Ctrl Pts',(-58.8333116900395,60.9048892011469,
62.5143197920547));
#216075=CARTESIAN_POINT('Ctrl Pts',(-58.8479994067537,60.546159044615,62.8245024333472));
#216076=CARTESIAN_POINT('Ctrl Pts',(-58.8806737948661,59.815039009383,63.563928902679));
#216077=CARTESIAN_POINT('Ctrl Pts',(-58.8987004399109,59.4553575779274,
64.0029717438398));
#216078=CARTESIAN_POINT('Ctrl Pts',(-58.934685010945,58.8232541514026,64.9409774547609));
#216079=CARTESIAN_POINT('Ctrl Pts',(-58.9522657383296,58.5519691498512,
65.4377396990574));
#216080=CARTESIAN_POINT('Ctrl Pts',(-58.9714304678815,58.3106519828565,
65.9979863624172));
#216081=CARTESIAN_POINT('Ctrl Pts',(-58.9728517828832,58.2930770112353,
66.0396416509611));
#216082=CARTESIAN_POINT('Ctrl Pts',(-58.9742739875024,58.2758162752982,
66.0814193783896));
#216083=CARTESIAN_POINT('Ctrl Pts',(-59.1795703768786,58.2758162902684,
66.0814193421557));
#216084=CARTESIAN_POINT('Ctrl Pts',(-59.1783554619545,58.2903039194333,
66.0463536174298));
#216085=CARTESIAN_POINT('Ctrl Pts',(-59.1771395900977,58.3050129701034,
66.0113740408932));
#216086=CARTESIAN_POINT('Ctrl Pts',(-59.1580023294326,58.5398278942509,
65.4626057038298));
#216087=CARTESIAN_POINT('Ctrl Pts',(-59.1399707993854,58.8066445512896,
64.9700978274778));
#216088=CARTESIAN_POINT('Ctrl Pts',(-59.1045782801853,59.4265937330867,
64.0414972473066));
#216089=CARTESIAN_POINT('Ctrl Pts',(-59.0870175121321,59.7781931064481,
63.6072414840463));
#216090=CARTESIAN_POINT('Ctrl Pts',(-59.0544426846447,60.4877515876011,
62.8792057532509));
#216091=CARTESIAN_POINT('Ctrl Pts',(-59.0395901828067,60.8325871584719,
62.575210473491));
#216092=CARTESIAN_POINT('Ctrl Pts',(-59.0012790595759,61.7841913576702,
61.856553700059));
#216093=CARTESIAN_POINT('Ctrl Pts',(-58.9783540265279,62.4208275422783,
61.4869994547136));
#216094=CARTESIAN_POINT('Ctrl Pts',(-58.9400811224291,63.5174394878648,
61.016804275142));
#216095=CARTESIAN_POINT('Ctrl Pts',(-58.9251903171076,63.953093187273,60.8679542643804));
#216096=CARTESIAN_POINT('Ctrl Pts',(-58.8909811787837,64.9811578734939,
60.6017069430898));
#216097=CARTESIAN_POINT('Ctrl Pts',(-58.8720516156921,65.577749454958,60.5090310517618));
#216098=CARTESIAN_POINT('Ctrl Pts',(-58.8212592288542,67.166698702915,60.4218549865817));
#216099=CARTESIAN_POINT('Ctrl Pts',(-58.7892241126204,68.1565398106472,
60.529219092223));
#216100=CARTESIAN_POINT('Ctrl Pts',(-58.7201571117459,70.2523067611285,
61.1112638136952));
#216101=CARTESIAN_POINT('Ctrl Pts',(-58.681850112035,71.32198831223,61.6492411305714));
#216102=CARTESIAN_POINT('Ctrl Pts',(-58.6258058726589,72.7171825145136,
62.7344864657189));
#216103=CARTESIAN_POINT('Ctrl Pts',(-58.6073477142965,73.1408941228739,
63.1347737130986));
#216104=CARTESIAN_POINT('Ctrl Pts',(-58.5703125342873,73.8980738912673,
64.0016995709332));
#216105=CARTESIAN_POINT('Ctrl Pts',(-58.5519771880011,74.2315657457138,
64.4648818344744));
#216106=CARTESIAN_POINT('Ctrl Pts',(-58.5158348585072,74.8089160117557,
65.4499994977671));
#216107=CARTESIAN_POINT('Ctrl Pts',(-58.4977904556718,75.0510264461407,
65.9700094761895));
#216108=CARTESIAN_POINT('Ctrl Pts',(-58.4613656205717,75.4318737860649,
67.0419846493673));
#216109=CARTESIAN_POINT('Ctrl Pts',(-58.443127277265,75.5710199766267,67.5911489293482));
#216110=CARTESIAN_POINT('Ctrl Pts',(-58.401200214888,75.775568699142,68.9007522046425));
#216111=CARTESIAN_POINT('Ctrl Pts',(-58.3773978757872,75.7982019020291,
69.6635873513281));
#216112=CARTESIAN_POINT('Ctrl Pts',(-58.3437328865942,75.6977249455514,
70.7112048530297));
#216113=CARTESIAN_POINT('Ctrl Pts',(-58.3343624876357,75.6558120920739,
71.0005941924054));
#216114=CARTESIAN_POINT('Ctrl Pts',(-58.3048335829351,75.4788394292506,
71.9107461828793));
#216115=CARTESIAN_POINT('Ctrl Pts',(-58.2851404281767,75.2926736038043,
72.5196181081777));
#216116=CARTESIAN_POINT('Ctrl Pts',(-58.2491126807415,74.8472787644228,
73.5689448890223));
#216117=CARTESIAN_POINT('Ctrl Pts',(-58.2329863022464,74.6115832198505,
74.01653283224));
#216118=CARTESIAN_POINT('Ctrl Pts',(-58.1978145991745,74.0174894617805,
74.9475511251046));
#216119=CARTESIAN_POINT('Ctrl Pts',(-58.1791932012746,73.6458381627093,
75.419744531366));
#216120=CARTESIAN_POINT('Ctrl Pts',(-58.1416916477773,72.8180576880623,
76.2808866161529));
#216121=CARTESIAN_POINT('Ctrl Pts',(-58.1227926241545,72.364574562876,76.6683380391131));
#216122=CARTESIAN_POINT('Ctrl Pts',(-58.085241683661,71.395467668143,77.3441215888984));
#216123=CARTESIAN_POINT('Ctrl Pts',(-58.0670255559941,70.8831010247478,
77.6322224346307));
#216124=CARTESIAN_POINT('Ctrl Pts',(-58.039360530937,70.07443944786,77.9890273496044));
#216125=CARTESIAN_POINT('Ctrl Pts',(-58.0300144317083,69.7965888814801,
78.0956667373039));
#216126=CARTESIAN_POINT('Ctrl Pts',(-58.0042966191099,69.0239109083977,
78.3494909837965));
#216127=CARTESIAN_POINT('Ctrl Pts',(-57.9878171919291,68.5209926492301,
78.4684767935116));
#216128=CARTESIAN_POINT('Ctrl Pts',(-57.9554716500303,67.5034843834249,
78.6193907481706));
#216129=CARTESIAN_POINT('Ctrl Pts',(-57.9396109832204,66.9908056785546,
78.6515675826335));
#216130=CARTESIAN_POINT('Ctrl Pts',(-57.9079361110378,65.9817938881639,
78.6294811702175));
#216131=CARTESIAN_POINT('Ctrl Pts',(-57.8921897251693,65.4871604701479,
78.5779694030605));
#216132=CARTESIAN_POINT('Ctrl Pts',(-57.8578333563049,64.4236249111287,
78.3782280819368));
#216133=CARTESIAN_POINT('Ctrl Pts',(-57.8396197007314,63.8598222823445,
78.2147522744286));
#216134=CARTESIAN_POINT('Ctrl Pts',(-57.8025602807082,62.7587331594926,
77.7765177574505));
#216135=CARTESIAN_POINT('Ctrl Pts',(-57.783615510512,62.2250870609842,77.5003096720798));
#216136=CARTESIAN_POINT('Ctrl Pts',(-57.7268277078365,60.72787190169,76.5269614998672));
#216137=CARTESIAN_POINT('Ctrl Pts',(-57.6904418637172,59.8693583329943,
75.6918143451122));
#216138=CARTESIAN_POINT('Ctrl Pts',(-57.6146038668323,58.5181702844445,
73.7338174485842));
#216139=CARTESIAN_POINT('Ctrl Pts',(-57.5779208905498,58.0405516256518,
72.6284875540146));
#216140=CARTESIAN_POINT('Ctrl Pts',(-57.5304110418408,57.7283444453723,
71.175855912788));
#216141=CARTESIAN_POINT('Ctrl Pts',(-57.5210235783432,57.6806385854151,
70.8863747100672));
#216142=CARTESIAN_POINT('Ctrl Pts',(-57.495566040701,57.5885386883781,70.088717004058));
#216143=CARTESIAN_POINT('Ctrl Pts',(-57.4796645880626,57.5727680432773,
69.5783168669611));
#216144=CARTESIAN_POINT('Ctrl Pts',(-57.4445551732079,57.6317087077653,
68.4709984834795));
#216145=CARTESIAN_POINT('Ctrl Pts',(-57.4253083431831,57.7226285145801,
67.8773212063199));
#216146=CARTESIAN_POINT('Ctrl Pts',(-57.3924371001932,57.9774322139581,
66.8825423187258));
#216147=CARTESIAN_POINT('Ctrl Pts',(-57.3789776946765,58.1126384309615,
66.476373532874));
#216148=CARTESIAN_POINT('Ctrl Pts',(-57.3654750286597,58.2758162995991,
66.081419319572));
#216149=CARTESIAN_POINT('Origin',(-64.4265543961493,66.6762871555627,69.5530424137804));
#216150=CARTESIAN_POINT('',(-64.4174334691588,58.2772202579669,66.0829140514164));
#216151=CARTESIAN_POINT('',(-64.5675364832717,58.2772202579675,66.082914051415));
#216152=CARTESIAN_POINT('',(-64.4265543961493,58.2772202579675,66.082914051415));
#216153=CARTESIAN_POINT('',(-64.4174351716144,58.277199894009,66.0829633405634));
#216154=CARTESIAN_POINT('Ctrl Pts',(-64.4174351716144,58.277199894009,66.0829633405634));
#216155=CARTESIAN_POINT('Ctrl Pts',(-64.4174346041292,58.2772066819469,
66.0829469108273));
#216156=CARTESIAN_POINT('Ctrl Pts',(-64.417434036644,58.2772134699327,66.0829304811121));
#216157=CARTESIAN_POINT('Ctrl Pts',(-64.4174334691588,58.2772202579663,
66.0829140514177));
#216158=CARTESIAN_POINT('',(-64.5666618780602,57.6592844329271,70.6707464084894));
#216159=CARTESIAN_POINT('Ctrl Pts',(-64.5657843992066,57.6576119963886,
70.6709037535128));
#216160=CARTESIAN_POINT('Ctrl Pts',(-64.5410292719686,57.5614849398986,
69.8953704510566));
#216161=CARTESIAN_POINT('Ctrl Pts',(-64.5157599548511,57.5657910825955,
69.1106652615182));
#216162=CARTESIAN_POINT('Ctrl Pts',(-64.4664991797538,57.7750153078076,
67.5621750354682));
#216163=CARTESIAN_POINT('Ctrl Pts',(-64.4423690638959,57.978954721852,66.8048452266616));
#216164=CARTESIAN_POINT('Ctrl Pts',(-64.4174351716144,58.277199894009,66.0829633405634));
#216165=CARTESIAN_POINT('Origin',(-64.5675364832709,66.6762871555627,69.5530424137804));
#216166=CARTESIAN_POINT('Origin',(-27.5423496375577,75.0034579025039,72.9903965241317));
#216167=CARTESIAN_POINT('',(-30.7042591052867,64.0608503561673,68.4693880411344));
#216168=CARTESIAN_POINT('',(-31.000413750398,64.0608503608518,68.4693880297961));
#216169=CARTESIAN_POINT('',(-27.5423496375574,64.0608503608518,68.4693880297962));
#216170=CARTESIAN_POINT('',(-32.4074704173708,66.4978162345236,64.7498540653719));
#216171=CARTESIAN_POINT('Ctrl Pts',(-30.7042591049894,64.0608503561645,
68.469388041141));
#216172=CARTESIAN_POINT('Ctrl Pts',(-30.7071426846446,64.0154427292201,
68.5792922457301));
#216173=CARTESIAN_POINT('Ctrl Pts',(-30.7100288359184,63.9716878124109,
68.6898879365682));
#216174=CARTESIAN_POINT('Ctrl Pts',(-30.7314888541783,63.6592255927563,
69.515848345412));
#216175=CARTESIAN_POINT('Ctrl Pts',(-30.7502936496543,63.4586766831916,
70.2550526413332));
#216176=CARTESIAN_POINT('Ctrl Pts',(-30.7880156107471,63.1998218385888,
71.7795464886297));
#216177=CARTESIAN_POINT('Ctrl Pts',(-30.8067238829455,63.1456222748352,
72.5617688967935));
#216178=CARTESIAN_POINT('Ctrl Pts',(-30.8440085560865,63.1912631012398,
74.0910038605536));
#216179=CARTESIAN_POINT('Ctrl Pts',(-30.8623806888472,63.2843220029158,
74.8346162191063));
#216180=CARTESIAN_POINT('Ctrl Pts',(-30.8896020570695,63.5293171722439,
75.9345472556964));
#216181=CARTESIAN_POINT('Ctrl Pts',(-30.8987252784131,63.6294757519157,
76.3004507737405));
#216182=CARTESIAN_POINT('Ctrl Pts',(-30.9264298438691,63.9844125068962,
77.3889408620437));
#216183=CARTESIAN_POINT('Ctrl Pts',(-30.9451999321401,64.2918757388179,
78.0922147103967));
#216184=CARTESIAN_POINT('Ctrl Pts',(-30.9827948279128,65.0460302084666,
79.443360642876));
#216185=CARTESIAN_POINT('Ctrl Pts',(-31.0014216297201,65.4936272557938,
80.0864685814755));
#216186=CARTESIAN_POINT('Ctrl Pts',(-31.0385692917722,66.486983830867,81.2492650194911));
#216187=CARTESIAN_POINT('Ctrl Pts',(-31.0568829521047,67.0254098981056,
81.7704875767997));
#216188=CARTESIAN_POINT('Ctrl Pts',(-31.0840384210422,67.9058691419586,
82.4745158470988));
#216189=CARTESIAN_POINT('Ctrl Pts',(-31.093149591856,68.2135849339152,82.6971936583157));
#216190=CARTESIAN_POINT('Ctrl Pts',(-31.1208186669922,69.1732907502562,
83.3236831828682));
#216191=CARTESIAN_POINT('Ctrl Pts',(-31.1395718503685,69.8542827350363,
83.6793461590018));
#216192=CARTESIAN_POINT('Ctrl Pts',(-31.1771126375038,71.2892595856262,
84.2596240411037));
#216193=CARTESIAN_POINT('Ctrl Pts',(-31.1957134738935,72.0408913952483,
84.4801294607387));
#216194=CARTESIAN_POINT('Ctrl Pts',(-31.2328261856976,73.5432717103284,
84.7635335690407));
#216195=CARTESIAN_POINT('Ctrl Pts',(-31.2511267530039,74.2892704947723,
84.8322225911223));
#216196=CARTESIAN_POINT('Ctrl Pts',(-31.27829085742,75.4168647224421,84.8290518722946));
#216197=CARTESIAN_POINT('Ctrl Pts',(-31.2874176137634,75.7967068024047,
84.8096783011218));
#216198=CARTESIAN_POINT('Ctrl Pts',(-31.3151011656557,76.9370322232514,
84.6962911240781));
#216199=CARTESIAN_POINT('Ctrl Pts',(-31.3338592597317,77.6899539265179,
84.5467542393678));
#216200=CARTESIAN_POINT('Ctrl Pts',(-31.3714446839604,79.1716677353104,
84.099739215657));
#216201=CARTESIAN_POINT('Ctrl Pts',(-31.3900924872514,79.8959898635215,
83.8003273456125));
#216202=CARTESIAN_POINT('Ctrl Pts',(-31.4272898551173,81.2442366145827,
83.079540342749));
#216203=CARTESIAN_POINT('Ctrl Pts',(-31.4456237094184,81.8681769529739,
82.6658180832174));
#216204=CARTESIAN_POINT('Ctrl Pts',(-31.4728620679002,82.7447383616365,
81.9568596407687));
#216205=CARTESIAN_POINT('Ctrl Pts',(-31.4820247386137,83.0288090084183,
81.703525893715));
#216206=CARTESIAN_POINT('Ctrl Pts',(-31.5097611848295,83.8451716263661,
80.9016443138406));
#216207=CARTESIAN_POINT('Ctrl Pts',(-31.5285389512676,84.3370626439491,
80.3148454401391));
#216208=CARTESIAN_POINT('Ctrl Pts',(-31.5691345184249,85.2786526219638,
78.9412856508615));
#216209=CARTESIAN_POINT('Ctrl Pts',(-31.5907117268863,85.7017499304334,
78.1420236914736));
#216210=CARTESIAN_POINT('Ctrl Pts',(-31.6221043829196,86.1683425611218,
76.9488947412377));
#216211=CARTESIAN_POINT('Ctrl Pts',(-31.6314474138179,86.2895437986178,
76.588815954066));
#216212=CARTESIAN_POINT('Ctrl Pts',(-31.6560186422131,86.5635709402545,
75.6234676084616));
#216213=CARTESIAN_POINT('Ctrl Pts',(-31.6710282838724,86.6862204675412,
75.0108756967406));
#216214=CARTESIAN_POINT('Ctrl Pts',(-31.7047675321177,86.8502176585972,
73.6347652353876));
#216215=CARTESIAN_POINT('Ctrl Pts',(-31.7235797176853,86.8671287452743,
72.8711147785176));
#216216=CARTESIAN_POINT('Ctrl Pts',(-31.7649925390056,86.7415693506148,
71.1850076867866));
#216217=CARTESIAN_POINT('Ctrl Pts',(-31.7873184587275,86.5638698267206,
70.2701811467465));
#216218=CARTESIAN_POINT('Ctrl Pts',(-31.8195363190033,86.1654160742036,
69.0236293135017));
#216219=CARTESIAN_POINT('Ctrl Pts',(-31.8289255265732,86.0323725551848,
68.6674815589585));
#216220=CARTESIAN_POINT('Ctrl Pts',(-31.864605379975,85.4592745234184,67.3330086651307));
#216221=CARTESIAN_POINT('Ctrl Pts',(-31.8904165834867,84.904201553612,66.4097114912461));
#216222=CARTESIAN_POINT('Ctrl Pts',(-31.9263510455404,83.9925590087104,
65.2752873839397));
#216223=CARTESIAN_POINT('Ctrl Pts',(-31.9358141557968,83.7383140241215,
64.9885755380937));
#216224=CARTESIAN_POINT('Ctrl Pts',(-31.9582133427393,83.0984926032058,
64.333952009465));
#216225=CARTESIAN_POINT('Ctrl Pts',(-31.9711202053359,82.7011068458162,
63.9787473451167));
#216226=CARTESIAN_POINT('Ctrl Pts',(-32.0026750237428,81.6849222116455,
63.1868450686939));
#216227=CARTESIAN_POINT('Ctrl Pts',(-32.0214467219376,81.0455491664941,
62.7803666280733));
#216228=CARTESIAN_POINT('Ctrl Pts',(-32.0580526551226,79.7158129680039,
62.1039103319514));
#216229=CARTESIAN_POINT('Ctrl Pts',(-32.075846193602,79.0301274923185,61.8320897087201));
#216230=CARTESIAN_POINT('Ctrl Pts',(-32.1123249726576,77.6067419305098,
61.4162476024319));
#216231=CARTESIAN_POINT('Ctrl Pts',(-32.1308571115243,76.8716126199349,
61.2751065960188));
#216232=CARTESIAN_POINT('Ctrl Pts',(-32.1583469877466,75.7504384481428,
61.1681240910288));
#216233=CARTESIAN_POINT('Ctrl Pts',(-32.1675726846286,75.371262005641,61.150260309778));
#216234=CARTESIAN_POINT('Ctrl Pts',(-32.1954647981057,74.2308178101296,
61.1513751461698));
#216235=CARTESIAN_POINT('Ctrl Pts',(-32.2143190124741,73.4715995168137,
61.2254997029869));
#216236=CARTESIAN_POINT('Ctrl Pts',(-32.2522664768761,71.9560477104346,
61.5227405919284));
#216237=CARTESIAN_POINT('Ctrl Pts',(-32.2711443340109,71.2041837518262,
61.7494284969278));
#216238=CARTESIAN_POINT('Ctrl Pts',(-32.309981978744,69.7424751132151,62.3536892187749));
#216239=CARTESIAN_POINT('Ctrl Pts',(-32.3297211176139,69.0374464536894,
62.7325117135954));
#216240=CARTESIAN_POINT('Ctrl Pts',(-32.3590866547182,68.036971548557,63.4083530833487));
#216241=CARTESIAN_POINT('Ctrl Pts',(-32.36901237901,67.7101173600655,63.6547298689732));
#216242=CARTESIAN_POINT('Ctrl Pts',(-32.3889871549098,67.0835947800557,
64.1800127839679));
#216243=CARTESIAN_POINT('Ctrl Pts',(-32.3990228511724,66.7843163110995,
64.4585267821791));
#216244=CARTESIAN_POINT('Ctrl Pts',(-32.4090802221679,66.5000364877912,
64.7519499557376));
#216245=CARTESIAN_POINT('',(-32.7070018384414,66.4978162197124,64.7498540510208));
#216246=CARTESIAN_POINT('Origin',(-32.557235790491,62.9783364609362,61.3397527097253));
#216247=CARTESIAN_POINT('Ctrl Pts',(-32.7053886803439,66.4999818003679,
64.7520064024586));
#216248=CARTESIAN_POINT('Ctrl Pts',(-32.69553011162,66.7838357164023,64.4590189430342));
#216249=CARTESIAN_POINT('Ctrl Pts',(-32.6856649273,67.0826424505334,64.1808973524643));
#216250=CARTESIAN_POINT('Ctrl Pts',(-32.6657877293566,67.708153828014,63.6562902858532));
#216251=CARTESIAN_POINT('Ctrl Pts',(-32.6557887964716,68.0344722672034,
63.4101961781974));
#216252=CARTESIAN_POINT('Ctrl Pts',(-32.6262999049639,69.0332045268677,
62.7350772305994));
#216253=CARTESIAN_POINT('Ctrl Pts',(-32.6072197959714,69.7369472826996,
62.3565181907147));
#216254=CARTESIAN_POINT('Ctrl Pts',(-32.5689385580399,71.197168794757,61.7517989533017));
#216255=CARTESIAN_POINT('Ctrl Pts',(-32.5496988886399,71.9489320636044,
61.5246309910955));
#216256=CARTESIAN_POINT('Ctrl Pts',(-32.5123069727106,73.4641355241297,
61.2264875436045));
#216257=CARTESIAN_POINT('Ctrl Pts',(-32.4941342755606,74.223093637015,61.1518955209385));
#216258=CARTESIAN_POINT('Ctrl Pts',(-32.4664075871642,75.3634572583079,
61.1500161322631));
#216259=CARTESIAN_POINT('Ctrl Pts',(-32.4571372927898,75.7427796746091,
61.1676383890037));
#216260=CARTESIAN_POINT('Ctrl Pts',(-32.4296885153319,76.8641116262045,
61.2739156704039));
#216261=CARTESIAN_POINT('Ctrl Pts',(-32.4118711067863,77.5992898795384,
61.4145763117665));
#216262=CARTESIAN_POINT('Ctrl Pts',(-32.3748773209694,79.0689253298945,
61.8428988407649));
#216263=CARTESIAN_POINT('Ctrl Pts',(-32.3556591558999,79.7978996496223,
62.1364547210756));
#216264=CARTESIAN_POINT('Ctrl Pts',(-32.3274982129129,80.8297798259273,
62.676374092178));
#216265=CARTESIAN_POINT('Ctrl Pts',(-32.3183713064889,81.1583600006871,
62.869019777627));
#216266=CARTESIAN_POINT('Ctrl Pts',(-32.2876728591593,82.2258550138294,
63.5661248169695));
#216267=CARTESIAN_POINT('Ctrl Pts',(-32.2658307792389,82.9168109882992,
64.1383494603416));
#216268=CARTESIAN_POINT('Ctrl Pts',(-32.23486475593,83.8015000256364,65.0581515036157));
#216269=CARTESIAN_POINT('Ctrl Pts',(-32.2256966396352,84.0527919668674,
65.3460777205622));
#216270=CARTESIAN_POINT('Ctrl Pts',(-32.1982533126496,84.7599044459102,
66.2401090071176));
#216271=CARTESIAN_POINT('Ctrl Pts',(-32.1798623274365,85.1719124448039,
66.878346835215));
#216272=CARTESIAN_POINT('Ctrl Pts',(-32.1431317556561,85.8630907085791,
68.2148211866102));
#216273=CARTESIAN_POINT('Ctrl Pts',(-32.1252359546489,86.1425911901294,
68.9090417134335));
#216274=CARTESIAN_POINT('Ctrl Pts',(-32.0875611591384,86.5854727520725,
70.4028444675641));
#216275=CARTESIAN_POINT('Ctrl Pts',(-32.0676444524148,86.7355291046516,
71.2023859468808));
#216276=CARTESIAN_POINT('Ctrl Pts',(-32.0294893527047,86.8653955626351,
72.7668782629184));
#216277=CARTESIAN_POINT('Ctrl Pts',(-32.0113448408402,86.8553566833968,
73.5270791544992));
#216278=CARTESIAN_POINT('Ctrl Pts',(-31.979996561774,86.7151982900055,74.8051252905583));
#216279=CARTESIAN_POINT('Ctrl Pts',(-31.9670375712713,86.6227916829676,
75.3247451323471));
#216280=CARTESIAN_POINT('Ctrl Pts',(-31.944840905975,86.4042186066256,76.2073552875076));
#216281=CARTESIAN_POINT('Ctrl Pts',(-31.9356138391446,86.2944722024968,
76.5735745492717));
#216282=CARTESIAN_POINT('Ctrl Pts',(-31.9079019692038,85.9130993046381,
77.6532264364888));
#216283=CARTESIAN_POINT('Ctrl Pts',(-31.8893055272082,85.590048538782,78.3463600610293));
#216284=CARTESIAN_POINT('Ctrl Pts',(-31.8522266233887,84.8233265681204,
79.6468179367242));
#216285=CARTESIAN_POINT('Ctrl Pts',(-31.8341954264111,84.384079288709,80.2527455045997));
#216286=CARTESIAN_POINT('Ctrl Pts',(-31.7954192498862,83.3308394184371,
81.4492901129661));
#216287=CARTESIAN_POINT('Ctrl Pts',(-31.7744777428662,82.7043190559933,
82.0233852119809));
#216288=CARTESIAN_POINT('Ctrl Pts',(-31.7350937174841,81.4068920363101,
82.9783585419448));
#216289=CARTESIAN_POINT('Ctrl Pts',(-31.7166924725776,80.7495141984602,
83.3704831346131));
#216290=CARTESIAN_POINT('Ctrl Pts',(-31.6854021877319,79.5972140386992,
83.9146054460994));
#216291=CARTESIAN_POINT('Ctrl Pts',(-31.6727692925259,79.1218395882889,
84.1025460178052));
#216292=CARTESIAN_POINT('Ctrl Pts',(-31.6508516209878,78.2725307300772,
84.3763103513238));
#216293=CARTESIAN_POINT('Ctrl Pts',(-31.6415771462094,77.903790584014,84.4757759950525));
#216294=CARTESIAN_POINT('Ctrl Pts',(-31.6063238455528,76.4894928033484,
84.7848090554636));
#216295=CARTESIAN_POINT('Ctrl Pts',(-31.5799383618991,75.422119384323,84.8706816344041));
#216296=CARTESIAN_POINT('Ctrl Pts',(-31.5350170505017,73.5891271361704,
84.7705654860981));
#216297=CARTESIAN_POINT('Ctrl Pts',(-31.5163791926102,72.8264335972992,
84.6537271396055));
#216298=CARTESIAN_POINT('Ctrl Pts',(-31.4785596356244,71.3393754622557,
84.274880775917));
#216299=CARTESIAN_POINT('Ctrl Pts',(-31.4596683236531,70.6182861336933,
84.014704384785));
#216300=CARTESIAN_POINT('Ctrl Pts',(-31.4127644084642,68.8806102415118,
83.190068806834));
#216301=CARTESIAN_POINT('Ctrl Pts',(-31.3841098190006,67.9124382865636,
82.5423603132802));
#216302=CARTESIAN_POINT('Ctrl Pts',(-31.346463958581,66.7718729432973,81.5089613897664));
#216303=CARTESIAN_POINT('Ctrl Pts',(-31.3372185118236,66.5023947921537,
81.2400550046652));
#216304=CARTESIAN_POINT('Ctrl Pts',(-31.3097513689028,65.7453175508535,
80.4080248239167));
#216305=CARTESIAN_POINT('Ctrl Pts',(-31.291380037766,65.297350173782,79.8113812998257));
#216306=CARTESIAN_POINT('Ctrl Pts',(-31.2545593074383,64.5168065285002,
78.5376458706384));
#216307=CARTESIAN_POINT('Ctrl Pts',(-31.2364814277601,64.1867836197617,
77.8629103381064));
#216308=CARTESIAN_POINT('Ctrl Pts',(-31.1990043797762,63.6472878523156,
76.4297260793805));
#216309=CARTESIAN_POINT('Ctrl Pts',(-31.1796109502199,63.4449878567384,
75.6724400221149));
#216310=CARTESIAN_POINT('Ctrl Pts',(-31.1512319403437,63.2574028599595,
74.5250858009222));
#216311=CARTESIAN_POINT('Ctrl Pts',(-31.1420080999806,63.2141357960004,
74.1466687520122));
#216312=CARTESIAN_POINT('Ctrl Pts',(-31.1145807159917,63.1402361027004,
73.022198413814));
#216313=CARTESIAN_POINT('Ctrl Pts',(-31.0962361987064,63.1618075858758,
72.2746107871689));
#216314=CARTESIAN_POINT('Ctrl Pts',(-31.0595156189855,63.3456446913962,
70.7914046029045));
#216315=CARTESIAN_POINT('Ctrl Pts',(-31.0415259421293,63.5078929487642,
70.0591575253195));
#216316=CARTESIAN_POINT('Ctrl Pts',(-31.0156884362488,63.8341785308065,
69.0502524767953));
#216317=CARTESIAN_POINT('Ctrl Pts',(-31.0080604239167,63.9418373514177,
68.7574460275236));
#216318=CARTESIAN_POINT('Ctrl Pts',(-31.000413750398,64.0608503608518,68.4693880297961));
#216319=CARTESIAN_POINT('Origin',(-27.5423496375577,75.0034579025039,72.9903965241317));
#216320=CARTESIAN_POINT('',(-28.8902889611216,64.0608503608518,68.4693880297961));
#216321=CARTESIAN_POINT('',(-29.1863798856003,64.0608503608518,68.4693880297961));
#216322=CARTESIAN_POINT('',(-27.5423496375574,64.0608503608518,68.4693880297962));
#216323=CARTESIAN_POINT('Ctrl Pts',(-28.8902889611216,64.0608503608518,
68.4693880297961));
#216324=CARTESIAN_POINT('Ctrl Pts',(-28.8995283196927,63.9171340345322,
68.8172377094005));
#216325=CARTESIAN_POINT('Ctrl Pts',(-28.9087847528996,63.7900030671402,
69.1719427226877));
#216326=CARTESIAN_POINT('Ctrl Pts',(-28.9365166291705,63.4572271982444,
70.2616197964341));
#216327=CARTESIAN_POINT('Ctrl Pts',(-28.9548136304281,63.3054826777762,
71.0107377528076));
#216328=CARTESIAN_POINT('Ctrl Pts',(-28.9826977015882,63.1877012504632,
72.1465920055058));
#216329=CARTESIAN_POINT('Ctrl Pts',(-28.992003005461,63.1667315488403,72.5256171768658));
#216330=CARTESIAN_POINT('Ctrl Pts',(-29.0195714907716,63.1586040887462,
73.6523155198278));
#216331=CARTESIAN_POINT('Ctrl Pts',(-29.0374679866773,63.2239830584802,
74.3984706514494));
#216332=CARTESIAN_POINT('Ctrl Pts',(-29.0745754382403,63.5010448035412,
75.9038613978213));
#216333=CARTESIAN_POINT('Ctrl Pts',(-29.0938293810776,63.7189370449008,
76.6582798779555));
#216334=CARTESIAN_POINT('Ctrl Pts',(-29.1312567613625,64.2921896779695,
78.0921469569484));
#216335=CARTESIAN_POINT('Ctrl Pts',(-29.1494411325762,64.6421002606472,
78.7697908854879));
#216336=CARTESIAN_POINT('Ctrl Pts',(-29.1834627585719,65.4002903058035,
79.9449581265054));
#216337=CARTESIAN_POINT('Ctrl Pts',(-29.1990955258074,65.7886947130422,
80.4519580793481));
#216338=CARTESIAN_POINT('Ctrl Pts',(-29.2236639274506,66.4707109623571,
81.2072584793979));
#216339=CARTESIAN_POINT('Ctrl Pts',(-29.2327815371745,66.7388238095533,
81.4768807592511));
#216340=CARTESIAN_POINT('Ctrl Pts',(-29.2598230607728,67.5669082104724,
82.2331012105019));
#216341=CARTESIAN_POINT('Ctrl Pts',(-29.2778991999651,68.1601308107924,
82.6805319137459));
#216342=CARTESIAN_POINT('Ctrl Pts',(-29.3141450709817,69.4278956972455,
83.4619064130423));
#216343=CARTESIAN_POINT('Ctrl Pts',(-29.3319583200587,70.1002537270503,
83.7930815033909));
#216344=CARTESIAN_POINT('Ctrl Pts',(-29.3672593377321,71.4644647671734,
84.3112586206249));
#216345=CARTESIAN_POINT('Ctrl Pts',(-29.3846907416036,72.1510031810128,
84.5034276001188));
#216346=CARTESIAN_POINT('Ctrl Pts',(-29.4197344481068,73.5737642407376,
84.7665150208697));
#216347=CARTESIAN_POINT('Ctrl Pts',(-29.437267317923,74.3077937902918,84.832569043604));
#216348=CARTESIAN_POINT('Ctrl Pts',(-29.4732775384949,75.7913509524845,
84.8275898529678));
#216349=CARTESIAN_POINT('Ctrl Pts',(-29.491613648245,76.5375895026883,84.7541701288638));
#216350=CARTESIAN_POINT('Ctrl Pts',(-29.5187968222645,77.6440722559224,
84.5381724213967));
#216351=CARTESIAN_POINT('Ctrl Pts',(-29.5279055197581,78.0125445201575,
84.4476811094524));
#216352=CARTESIAN_POINT('Ctrl Pts',(-29.5556043135655,79.1112967674302,
84.1211728795115));
#216353=CARTESIAN_POINT('Ctrl Pts',(-29.5743943826445,79.8235803821709,
83.8317491984357));
#216354=CARTESIAN_POINT('Ctrl Pts',(-29.6166217721661,81.361006721127,83.0253745327922));
#216355=CARTESIAN_POINT('Ctrl Pts',(-29.6397325115422,82.1606716055852,
82.4716152157968));
#216356=CARTESIAN_POINT('Ctrl Pts',(-29.6727251246817,83.1677281029812,
81.5734914110518));
#216357=CARTESIAN_POINT('Ctrl Pts',(-29.6820549745417,83.4392103276158,
81.3068204495254));
#216358=CARTESIAN_POINT('Ctrl Pts',(-29.7135942069433,84.3181727138243,
80.3560312747861));
#216359=CARTESIAN_POINT('Ctrl Pts',(-29.7354604105003,84.8590724017529,
79.6148479509096));
#216360=CARTESIAN_POINT('Ctrl Pts',(-29.7671521272747,85.4962376963539,
78.4882156517042));
#216361=CARTESIAN_POINT('Ctrl Pts',(-29.7764893680399,85.6671975926004,
78.1487972975652));
#216362=CARTESIAN_POINT('Ctrl Pts',(-29.8140375203506,86.2911770042174,
76.7458108067079));
#216363=CARTESIAN_POINT('Ctrl Pts',(-29.8417316022383,86.603683301564,75.6267776870563));
#216364=CARTESIAN_POINT('Ctrl Pts',(-29.889083706918,86.8460191498429,73.7163248453229));
#216365=CARTESIAN_POINT('Ctrl Pts',(-29.9076925494568,86.868159572991,72.944711902705));
#216366=CARTESIAN_POINT('Ctrl Pts',(-29.9450551075506,86.762717067064,71.4145921473615));
#216367=CARTESIAN_POINT('Ctrl Pts',(-29.9639086151304,86.6366337551139,
70.6596153030522));
#216368=CARTESIAN_POINT('Ctrl Pts',(-30.0085206985524,86.1656157605052,
68.9041916152091));
#216369=CARTESIAN_POINT('Ctrl Pts',(-30.0338700129661,85.7578132587307,
67.9273261156758));
#216370=CARTESIAN_POINT('Ctrl Pts',(-30.0693094538078,85.0332503972255,
66.6872515359413));
#216371=CARTESIAN_POINT('Ctrl Pts',(-30.0787573876203,84.8244766729224,
66.3666538540317));
#216372=CARTESIAN_POINT('Ctrl Pts',(-30.1002157099478,84.3110038478021,
65.6559414998619));
#216373=CARTESIAN_POINT('Ctrl Pts',(-30.112200390852,83.9966297791216,65.2736936378709));
#216374=CARTESIAN_POINT('Ctrl Pts',(-30.1428896282947,83.1402829464073,
64.3561117856364));
#216375=CARTESIAN_POINT('Ctrl Pts',(-30.1617389531945,82.5689029361146,
63.8513143523389));
#216376=CARTESIAN_POINT('Ctrl Pts',(-30.1997201187605,81.3183893218145,
62.9446825912728));
#216377=CARTESIAN_POINT('Ctrl Pts',(-30.2186358410031,80.6395783999868,
62.5487071409636));
#216378=CARTESIAN_POINT('Ctrl Pts',(-30.2562907179915,79.2474660775924,
61.9122079365959));
#216379=CARTESIAN_POINT('Ctrl Pts',(-30.2748230233428,78.5404412751904,
61.6666327809114));
#216380=CARTESIAN_POINT('Ctrl Pts',(-30.3023168365406,77.4464782846083,
61.3992032615102));
#216381=CARTESIAN_POINT('Ctrl Pts',(-30.3115448502552,77.0738292245333,
61.3268776539251));
#216382=CARTESIAN_POINT('Ctrl Pts',(-30.3394414902501,75.9452472279289,
61.1636368586258));
#216383=CARTESIAN_POINT('Ctrl Pts',(-30.3582986518662,75.1833974202189,
61.1275629500521));
#216384=CARTESIAN_POINT('Ctrl Pts',(-30.3962644743953,73.6408288637397,
61.2032308449913));
#216385=CARTESIAN_POINT('Ctrl Pts',(-30.4151542734454,72.8640206097579,
61.319199271877));
#216386=CARTESIAN_POINT('Ctrl Pts',(-30.4527642488833,71.379827850808,61.6940280567394));
#216387=CARTESIAN_POINT('Ctrl Pts',(-30.4712801870707,70.6742226457001,
61.9451999629897));
#216388=CARTESIAN_POINT('Ctrl Pts',(-30.4987242331526,69.6534852610907,
62.4214951159395));
#216389=CARTESIAN_POINT('Ctrl Pts',(-30.5079245437531,69.3178539669437,
62.5981979017771));
#216390=CARTESIAN_POINT('Ctrl Pts',(-30.5357803140262,68.3345629208456,
63.1777954724162));
#216391=CARTESIAN_POINT('Ctrl Pts',(-30.5546204634495,67.7167695413567,
63.6274130181923));
#216392=CARTESIAN_POINT('Ctrl Pts',(-30.5924875226138,66.5608460375821,
64.6528080587044));
#216393=CARTESIAN_POINT('Ctrl Pts',(-30.6112979661866,66.0281591470195,
65.2291405841927));
#216394=CARTESIAN_POINT('Ctrl Pts',(-30.6487638962762,65.105627462703,66.4503606319373));
#216395=CARTESIAN_POINT('Ctrl Pts',(-30.6672161329818,64.7125007167355,
67.088250543124));
#216396=CARTESIAN_POINT('Ctrl Pts',(-30.6916656655681,64.2672696883344,
67.9921921862697));
#216397=CARTESIAN_POINT('Ctrl Pts',(-30.6979556134436,64.1601112148153,
68.2291379675095));
#216398=CARTESIAN_POINT('Ctrl Pts',(-30.7042591049894,64.0608503561645,
68.469388041141));
#216399=CARTESIAN_POINT('Ctrl Pts',(-31.000413750398,64.0608503608518,68.4693880297961));
#216400=CARTESIAN_POINT('Ctrl Pts',(-30.9894496917122,64.2314952323248,
68.056360746201));
#216401=CARTESIAN_POINT('Ctrl Pts',(-30.9784421942637,64.4254828637911,
67.6530958066313));
#216402=CARTESIAN_POINT('Ctrl Pts',(-30.9489866486578,65.0109590167339,
66.5941692359763));
#216403=CARTESIAN_POINT('Ctrl Pts',(-30.9306856435903,65.4435799455716,
65.9639821995385));
#216404=CARTESIAN_POINT('Ctrl Pts',(-30.9027964538502,66.1776565319684,
65.0891727800485));
#216405=CARTESIAN_POINT('Ctrl Pts',(-30.8934900614081,66.435349072473,64.8104443940101));
#216406=CARTESIAN_POINT('Ctrl Pts',(-30.8659179066328,67.2390950257741,
64.02081564219));
#216407=CARTESIAN_POINT('Ctrl Pts',(-30.8480189096461,67.8206066990283,
63.5487143437753));
#216408=CARTESIAN_POINT('Ctrl Pts',(-30.8109072024215,69.0947801507967,
62.7005335799142));
#216409=CARTESIAN_POINT('Ctrl Pts',(-30.7916515945159,69.7882978510282,
62.3322610185254));
#216410=CARTESIAN_POINT('Ctrl Pts',(-30.7542197263624,71.2171650947603,
61.7465901632417));
#216411=CARTESIAN_POINT('Ctrl Pts',(-30.7360324769979,71.9474318085476,
61.526544373066));
#216412=CARTESIAN_POINT('Ctrl Pts',(-30.7082843981268,73.0660586956442,
61.304047188608));
#216413=CARTESIAN_POINT('Ctrl Pts',(-30.6990064488469,73.4417148441884,
61.2479421664651));
#216414=CARTESIAN_POINT('Ctrl Pts',(-30.6715352735179,74.5626272885663,
61.1352798461866));
#216415=CARTESIAN_POINT('Ctrl Pts',(-30.6537045524294,75.3112417532731,
61.1310797775953));
#216416=CARTESIAN_POINT('Ctrl Pts',(-30.6166987175427,76.8360320209113,
61.2670725843473));
#216417=CARTESIAN_POINT('Ctrl Pts',(-30.5974786215739,77.6079706799152,
61.4140776267444));
#216418=CARTESIAN_POINT('Ctrl Pts',(-30.5601372717332,79.0885388976018,
61.8517288475339));
#216419=CARTESIAN_POINT('Ctrl Pts',(-30.5420056674958,79.7949462173665,
62.1368509983944));
#216420=CARTESIAN_POINT('Ctrl Pts',(-30.5143121205572,80.8061506797072,
62.663089451141));
#216421=CARTESIAN_POINT('Ctrl Pts',(-30.5050377472477,81.1345263561437,
62.8545929730509));
#216422=CARTESIAN_POINT('Ctrl Pts',(-30.4775977076468,82.0790997762352,
63.4681772621597));
#216423=CARTESIAN_POINT('Ctrl Pts',(-30.4597881954024,82.6652183852194,
63.9330903470363));
#216424=CARTESIAN_POINT('Ctrl Pts',(-30.4227954929986,83.7692646956418,
64.9931677192314));
#216425=CARTESIAN_POINT('Ctrl Pts',(-30.4035642689954,84.2795254235964,
65.5910991644193));
#216426=CARTESIAN_POINT('Ctrl Pts',(-30.3661762013661,85.1607767831556,
66.8595510141587));
#216427=CARTESIAN_POINT('Ctrl Pts',(-30.3480147281005,85.5334673392602,
67.5243832837642));
#216428=CARTESIAN_POINT('Ctrl Pts',(-30.3173044039153,86.041964649879,68.6795630408262));
#216429=CARTESIAN_POINT('Ctrl Pts',(-30.305008169594,86.2147106522098,69.1511613564153));
#216430=CARTESIAN_POINT('Ctrl Pts',(-30.2835062852645,86.4654097595363,
69.9987605462407));
#216431=CARTESIAN_POINT('Ctrl Pts',(-30.2743102972342,86.5559953283855,
70.3702618605894));
#216432=CARTESIAN_POINT('Ctrl Pts',(-30.2467410045947,86.7726957501231,
71.4924223678137));
#216433=CARTESIAN_POINT('Ctrl Pts',(-30.2282552018806,86.8446118847982,
72.251514321688));
#216434=CARTESIAN_POINT('Ctrl Pts',(-30.1913586402202,86.8418313287905,
73.7590405627578));
#216435=CARTESIAN_POINT('Ctrl Pts',(-30.1733966849236,86.7697985538877,
74.5040444843898));
#216436=CARTESIAN_POINT('Ctrl Pts',(-30.1353420039617,86.471887487321,76.0453335157137));
#216437=CARTESIAN_POINT('Ctrl Pts',(-30.1150845933223,86.2318747685675,
76.8348930447516));
#216438=CARTESIAN_POINT('Ctrl Pts',(-30.0857305276675,85.7638798586112,
77.9440350612097));
#216439=CARTESIAN_POINT('Ctrl Pts',(-30.0765347506624,85.5989836952713,
78.287570286964));
#216440=CARTESIAN_POINT('Ctrl Pts',(-30.0428586838187,84.9380281839819,
79.5097345220104));
#216441=CARTESIAN_POINT('Ctrl Pts',(-30.017992731629,84.3468343501822,80.3319735493999));
#216442=CARTESIAN_POINT('Ctrl Pts',(-29.9841355838273,83.399247034245,81.3471537239098));
#216443=CARTESIAN_POINT('Ctrl Pts',(-29.9749379466191,83.1266425298508,
81.6123764884997));
#216444=CARTESIAN_POINT('Ctrl Pts',(-29.9427149566454,82.133242284368,82.4898713784685));
#216445=CARTESIAN_POINT('Ctrl Pts',(-29.9193411863813,81.3523246666702,
83.0286095885796));
#216446=CARTESIAN_POINT('Ctrl Pts',(-29.8774996552059,79.8372895143436,
83.8256098815549));
#216447=CARTESIAN_POINT('Ctrl Pts',(-29.858996784471,79.1258264058366,84.1157666172291));
#216448=CARTESIAN_POINT('Ctrl Pts',(-29.8308165594585,78.0276657130448,
84.4437098691035));
#216449=CARTESIAN_POINT('Ctrl Pts',(-29.821439008496,77.658995259724,84.5347605156796));
#216450=CARTESIAN_POINT('Ctrl Pts',(-29.7936444395498,76.5527280944839,
84.7521691217944));
#216451=CARTESIAN_POINT('Ctrl Pts',(-29.7755815110642,75.8068502324153,
84.8265316423571));
#216452=CARTESIAN_POINT('Ctrl Pts',(-29.7391907940041,74.3205379707526,
84.8334988644688));
#216453=CARTESIAN_POINT('Ctrl Pts',(-29.7208679422368,73.5834173872748,
84.7678719069654));
#216454=CARTESIAN_POINT('Ctrl Pts',(-29.6850838483617,72.1500663534938,
84.5036674362149));
#216455=CARTESIAN_POINT('Ctrl Pts',(-29.6677084140159,71.456244169244,84.3091655361203));
#216456=CARTESIAN_POINT('Ctrl Pts',(-29.6316592996819,70.0858288212269,
83.786508493853));
#216457=CARTESIAN_POINT('Ctrl Pts',(-29.6130886579611,69.414090372518,83.4545299006175));
#216458=CARTESIAN_POINT('Ctrl Pts',(-29.5766865576869,68.1467291337866,
82.6711241672695));
#216459=CARTESIAN_POINT('Ctrl Pts',(-29.5586589112334,67.5534087372805,
82.2222968714626));
#216460=CARTESIAN_POINT('Ctrl Pts',(-29.5309788247731,66.725759117199,81.4641411953882));
#216461=CARTESIAN_POINT('Ctrl Pts',(-29.5215695524604,66.4580119297219,
81.1940541730017));
#216462=CARTESIAN_POINT('Ctrl Pts',(-29.4970774975597,65.792768169438,80.4550248991482));
#216463=CARTESIAN_POINT('Ctrl Pts',(-29.4822163965635,65.4179672352868,
79.9672046448307));
#216464=CARTESIAN_POINT('Ctrl Pts',(-29.4485768052823,64.6666833955792,
78.8138212272529));
#216465=CARTESIAN_POINT('Ctrl Pts',(-29.4297129690732,64.3133079962881,
78.1364498539328));
#216466=CARTESIAN_POINT('Ctrl Pts',(-29.3917545451264,63.733881245762,76.7038891397521));
#216467=CARTESIAN_POINT('Ctrl Pts',(-29.3729028524237,63.5130026749589,
75.9506039498728));
#216468=CARTESIAN_POINT('Ctrl Pts',(-29.335357217513,63.2297676312216,74.4462388096491));
#216469=CARTESIAN_POINT('Ctrl Pts',(-29.3168550496804,63.1613394074936,
73.6999727832052));
#216470=CARTESIAN_POINT('Ctrl Pts',(-29.2805033884888,63.1661536575647,
72.2056509896819));
#216471=CARTESIAN_POINT('Ctrl Pts',(-29.2624303821015,63.2391734706643,
71.4609495912181));
#216472=CARTESIAN_POINT('Ctrl Pts',(-29.2347456172582,63.4545805086691,
70.3543832748118));
#216473=CARTESIAN_POINT('Ctrl Pts',(-29.2253655360921,63.5453134983676,
69.9843922354757));
#216474=CARTESIAN_POINT('Ctrl Pts',(-29.2060769114822,63.7696440352676,
69.2290941472924));
#216475=CARTESIAN_POINT('Ctrl Pts',(-29.1962359460276,63.9055604679698,
68.8452502638799));
#216476=CARTESIAN_POINT('Ctrl Pts',(-29.1863798856003,64.0608503608518,
68.4693880297961));
#216477=CARTESIAN_POINT('Origin',(-27.5423496375577,75.0034579025039,72.9903965241317));
#216478=CARTESIAN_POINT('',(-27.0763524842809,64.0608503697698,68.4693880082113));
#216479=CARTESIAN_POINT('',(-27.372320352868,64.0608503540424,68.4693880462777));
#216480=CARTESIAN_POINT('',(-27.5423496375574,64.0608503608518,68.4693880297962));
#216481=CARTESIAN_POINT('Ctrl Pts',(-27.0763524848464,64.060850369775,68.4693880081986));
#216482=CARTESIAN_POINT('Ctrl Pts',(-27.0859054812614,63.9103020442731,
68.8337737939964));
#216483=CARTESIAN_POINT('Ctrl Pts',(-27.0954454003588,63.7779643153705,
69.2056558759773));
#216484=CARTESIAN_POINT('Ctrl Pts',(-27.1240969798107,63.4392340773519,
70.3330959904916));
#216485=CARTESIAN_POINT('Ctrl Pts',(-27.1433969711315,63.2889256567875,
71.103003032948));
#216486=CARTESIAN_POINT('Ctrl Pts',(-27.1716284560733,63.1800423553295,
72.2610696888224));
#216487=CARTESIAN_POINT('Ctrl Pts',(-27.1807979879519,63.162707149997,72.6415477925153));
#216488=CARTESIAN_POINT('Ctrl Pts',(-27.2080544187198,63.1657330101346,
73.7680523132948));
#216489=CARTESIAN_POINT('Ctrl Pts',(-27.226280950715,63.2382106843945,74.5120488357248));
#216490=CARTESIAN_POINT('Ctrl Pts',(-27.2627659024089,63.5225250141981,
75.9782701625852));
#216491=CARTESIAN_POINT('Ctrl Pts',(-27.280636774545,63.7340658601985,76.6971488914858));
#216492=CARTESIAN_POINT('Ctrl Pts',(-27.3162039900716,64.2797231648403,
78.059966517954));
#216493=CARTESIAN_POINT('Ctrl Pts',(-27.3338728650167,64.6079288137639,
78.7028384096687));
#216494=CARTESIAN_POINT('Ctrl Pts',(-27.3606241720471,65.1964491124216,
79.6348414696851));
#216495=CARTESIAN_POINT('Ctrl Pts',(-27.3697957489021,65.4158936025924,
79.9477438654496));
#216496=CARTESIAN_POINT('Ctrl Pts',(-27.4013118299121,66.2180890267998,
80.9813767335047));
#216497=CARTESIAN_POINT('Ctrl Pts',(-27.4239171150195,66.8700467560069,
81.6440703277155));
#216498=CARTESIAN_POINT('Ctrl Pts',(-27.4556963398358,67.8909836980437,
82.4634808560025));
#216499=CARTESIAN_POINT('Ctrl Pts',(-27.4648823409838,68.2008576031965,
82.688398678786));
#216500=CARTESIAN_POINT('Ctrl Pts',(-27.4994364915695,69.4025724377663,
83.4746672666346));
#216501=CARTESIAN_POINT('Ctrl Pts',(-27.5251904055295,70.3571083794556,
83.9312042596608));
#216502=CARTESIAN_POINT('Ctrl Pts',(-27.5598186225791,71.7211337912766,
84.3724476925238));
#216503=CARTESIAN_POINT('Ctrl Pts',(-27.5689345990207,72.0883185096068,
84.4719775829097));
#216504=CARTESIAN_POINT('Ctrl Pts',(-27.5991497969802,73.3133657456307,
84.7414756611852));
#216505=CARTESIAN_POINT('Ctrl Pts',(-27.6205145015352,74.1852477269069,
84.8341620975593));
#216506=CARTESIAN_POINT('Ctrl Pts',(-27.6600365696807,75.8143749013741,
84.8264712668729));
#216507=CARTESIAN_POINT('Ctrl Pts',(-27.6780294399353,76.5673293365037,
84.7506925613435));
#216508=CARTESIAN_POINT('Ctrl Pts',(-27.7095456087994,77.8403516610893,
84.4980831466947));
#216509=CARTESIAN_POINT('Ctrl Pts',(-27.7228394100444,78.3648806946213,
84.3559432110618));
#216510=CARTESIAN_POINT('Ctrl Pts',(-27.7453559160673,79.2394927715973,
84.0530677832568));
#216511=CARTESIAN_POINT('Ctrl Pts',(-27.7545658539053,79.5948966989033,
83.9103496798472));
#216512=CARTESIAN_POINT('Ctrl Pts',(-27.7821587000339,80.6352530604497,
83.4327931444223));
#216513=CARTESIAN_POINT('Ctrl Pts',(-27.8006470615131,81.2954395316747,
83.0488119057356));
#216514=CARTESIAN_POINT('Ctrl Pts',(-27.8375647517096,82.5210570054952,
82.1677915114698));
#216515=CARTESIAN_POINT('Ctrl Pts',(-27.8555428563217,83.0853060917096,
81.675015618743));
#216516=CARTESIAN_POINT('Ctrl Pts',(-27.8943606925205,84.1877046395505,
80.511158397832));
#216517=CARTESIAN_POINT('Ctrl Pts',(-27.9154137136888,84.7070185604496,
79.8280233776928));
#216518=CARTESIAN_POINT('Ctrl Pts',(-27.954775756408,85.5408208222249,78.4423817770702));
#216519=CARTESIAN_POINT('Ctrl Pts',(-27.9730483021463,85.8696066992172,
77.7534814086961));
#216520=CARTESIAN_POINT('Ctrl Pts',(-28.0009899984105,86.2602211074579,
76.6796629656115));
#216521=CARTESIAN_POINT('Ctrl Pts',(-28.0103578636748,86.3731278812414,
76.3154541562814));
#216522=CARTESIAN_POINT('Ctrl Pts',(-28.0380380813857,86.6546221253415,
75.2236967172088));
#216523=CARTESIAN_POINT('Ctrl Pts',(-28.0560037213047,86.7722114001575,
74.4849533402767));
#216524=CARTESIAN_POINT('Ctrl Pts',(-28.0906095327986,86.8621334167247,
73.0676475276407));
#216525=CARTESIAN_POINT('Ctrl Pts',(-28.1072187570474,86.8473184090742,
72.3928080836079));
#216526=CARTESIAN_POINT('Ctrl Pts',(-28.1430038445859,86.6913356491575,
70.9441242962121));
#216527=CARTESIAN_POINT('Ctrl Pts',(-28.1618406358991,86.5304058870406,
70.175580916619));
#216528=CARTESIAN_POINT('Ctrl Pts',(-28.1951734533827,86.1210812944039,
68.8779824025966));
#216529=CARTESIAN_POINT('Ctrl Pts',(-28.2094523077273,85.9073574683635,
68.340829905481));
#216530=CARTESIAN_POINT('Ctrl Pts',(-28.2330439245425,85.4884236466741,
67.4775219853328));
#216531=CARTESIAN_POINT('Ctrl Pts',(-28.2423408547897,85.3049865023518,
67.1419094369747));
#216532=CARTESIAN_POINT('Ctrl Pts',(-28.2782578417886,84.5357602216077,
65.8833966628341));
#216533=CARTESIAN_POINT('Ctrl Pts',(-28.3052941562291,83.8395419508508,
65.034402610614));
#216534=CARTESIAN_POINT('Ctrl Pts',(-28.3508743773173,82.4710875276948,
63.7704280698183));
#216535=CARTESIAN_POINT('Ctrl Pts',(-28.3695262107152,81.8557014650617,
63.3043203361268));
#216536=CARTESIAN_POINT('Ctrl Pts',(-28.407353268538,80.5479670079492,62.5012090031384));
#216537=CARTESIAN_POINT('Ctrl Pts',(-28.426232145784,79.8592840491543,62.1651667892801));
#216538=CARTESIAN_POINT('Ctrl Pts',(-28.4729976683636,78.062547718402,61.4946506627506));
#216539=CARTESIAN_POINT('Ctrl Pts',(-28.5015232990402,76.9289262117093,
61.2514541469712));
#216540=CARTESIAN_POINT('Ctrl Pts',(-28.5390377437249,75.3984674866269,
61.1511013270156));
#216541=CARTESIAN_POINT('Ctrl Pts',(-28.5482828995768,75.0178221458842,
61.1445222316161));
#216542=CARTESIAN_POINT('Ctrl Pts',(-28.5757505507809,73.893349166789,61.1792933163559));
#216543=CARTESIAN_POINT('Ctrl Pts',(-28.594122353014,73.153004926618,61.2724482235333));
#216544=CARTESIAN_POINT('Ctrl Pts',(-28.6309418007174,71.6949132916563,
61.5976226793957));
#216545=CARTESIAN_POINT('Ctrl Pts',(-28.649017270183,70.9806297221474,61.8298133038949));
#216546=CARTESIAN_POINT('Ctrl Pts',(-28.6864894179898,69.575702599145,62.4390419718151));
#216547=CARTESIAN_POINT('Ctrl Pts',(-28.7058811506698,68.8908880624085,
62.8204357804223));
#216548=CARTESIAN_POINT('Ctrl Pts',(-28.7342580628242,67.9360519571189,
63.4837221209304));
#216549=CARTESIAN_POINT('Ctrl Pts',(-28.7434809492352,67.6340703127547,
63.7158500381008));
#216550=CARTESIAN_POINT('Ctrl Pts',(-28.7709065445809,66.7747124842914,
64.4449361288401));
#216551=CARTESIAN_POINT('Ctrl Pts',(-28.7892499725978,66.2525531429998,
64.9804777332998));
#216552=CARTESIAN_POINT('Ctrl Pts',(-28.825967005064,65.3147788628337,66.1442571638897));
#216553=CARTESIAN_POINT('Ctrl Pts',(-28.8439537114784,64.9015594364278,
66.7701252758376));
#216554=CARTESIAN_POINT('Ctrl Pts',(-28.8715192451016,64.3702675886859,
67.769070856942));
#216555=CARTESIAN_POINT('Ctrl Pts',(-28.8808941421672,64.2069848415272,
68.1156854715423));
#216556=CARTESIAN_POINT('Ctrl Pts',(-28.8902889611216,64.0608503608518,
68.4693880297961));
#216557=CARTESIAN_POINT('Ctrl Pts',(-29.1863798856003,64.0608503608518,
68.4693880297961));
#216558=CARTESIAN_POINT('Ctrl Pts',(-29.1772971019915,64.2039566764104,
68.1230148146493));
#216559=CARTESIAN_POINT('Ctrl Pts',(-29.1681963644073,64.3635156285741,
67.7834200366463));
#216560=CARTESIAN_POINT('Ctrl Pts',(-29.1407582807609,64.8892662932338,
66.7900910426804));
#216561=CARTESIAN_POINT('Ctrl Pts',(-29.1223061210834,65.3014574016432,
66.1631089739329));
#216562=CARTESIAN_POINT('Ctrl Pts',(-29.0861268663779,66.2363096871553,
64.9983969506667));
#216563=CARTESIAN_POINT('Ctrl Pts',(-29.068189876378,66.7563087681588,64.4628250183807));
#216564=CARTESIAN_POINT('Ctrl Pts',(-29.0406822289049,67.6128254558339,
63.7327731944003));
#216565=CARTESIAN_POINT('Ctrl Pts',(-29.0313471682774,67.914223574994,63.4999911454192));
#216566=CARTESIAN_POINT('Ctrl Pts',(-28.9963513665927,69.0909345083389,
62.6785523531985));
#216567=CARTESIAN_POINT('Ctrl Pts',(-28.9712333861722,70.0323304310186,
62.1931766204282));
#216568=CARTESIAN_POINT('Ctrl Pts',(-28.9361534913813,71.3849850634084,
61.7106575668398));
#216569=CARTESIAN_POINT('Ctrl Pts',(-28.9268151025283,71.7504684387958,
61.599877742482));
#216570=CARTESIAN_POINT('Ctrl Pts',(-28.8986232864933,72.8790142670072,
61.3165687146644));
#216571=CARTESIAN_POINT('Ctrl Pts',(-28.8799524364392,73.6543621125435,
61.2017806268093));
#216572=CARTESIAN_POINT('Ctrl Pts',(-28.8427762630881,75.1809434534785,
61.1284459314993));
#216573=CARTESIAN_POINT('Ctrl Pts',(-28.8245393308412,75.9282621777524,
61.1632193224014));
#216574=CARTESIAN_POINT('Ctrl Pts',(-28.7973642074259,77.0461147177396,
61.3218872138268));
#216575=CARTESIAN_POINT('Ctrl Pts',(-28.7881723803851,77.4220834695785,
61.3939830137662));
#216576=CARTESIAN_POINT('Ctrl Pts',(-28.7605398889289,78.532781424215,61.6633444752674));
#216577=CARTESIAN_POINT('Ctrl Pts',(-28.7419026732506,79.2526837640225,
61.9132892238843));
#216578=CARTESIAN_POINT('Ctrl Pts',(-28.7024162990105,80.7361329678467,
62.594384563092));
#216579=CARTESIAN_POINT('Ctrl Pts',(-28.6816183982419,81.4860140308851,
63.0446887401063));
#216580=CARTESIAN_POINT('Ctrl Pts',(-28.6511205511374,82.4821459250204,
63.8037720993769));
#216581=CARTESIAN_POINT('Ctrl Pts',(-28.641824948786,82.7733845772097,64.0487477801449));
#216582=CARTESIAN_POINT('Ctrl Pts',(-28.6070570799447,83.8229911513047,
65.02169091833));
#216583=CARTESIAN_POINT('Ctrl Pts',(-28.5820663187113,84.4951307407757,
65.8354971314365));
#216584=CARTESIAN_POINT('Ctrl Pts',(-28.5471143492697,85.2527771483029,
67.0509431192));
#216585=CARTESIAN_POINT('Ctrl Pts',(-28.5377911122329,85.43878229314,67.3841804411063));
#216586=CARTESIAN_POINT('Ctrl Pts',(-28.5057992242645,86.0263292297969,
68.5677288913263));
#216587=CARTESIAN_POINT('Ctrl Pts',(-28.4833135204415,86.3425386972941,
69.4564276996115));
#216588=CARTESIAN_POINT('Ctrl Pts',(-28.4510316165937,86.6345637039432,
70.7447829463107));
#216589=CARTESIAN_POINT('Ctrl Pts',(-28.4416982118052,86.7008126253116,
71.120290507038));
#216590=CARTESIAN_POINT('Ctrl Pts',(-28.411148415327,86.8594463816134,72.3690443886639));
#216591=CARTESIAN_POINT('Ctrl Pts',(-28.3901404593192,86.872893009606,73.249356325545));
#216592=CARTESIAN_POINT('Ctrl Pts',(-28.359381835819,86.7525769523979,74.5012789418191));
#216593=CARTESIAN_POINT('Ctrl Pts',(-28.3500534201444,86.6980386709,74.8775490469038));
#216594=CARTESIAN_POINT('Ctrl Pts',(-28.3145658480163,86.4204866664645,
76.3047667337937));
#216595=CARTESIAN_POINT('Ctrl Pts',(-28.2888789614875,86.0729804728404,
77.3262086786382));
#216596=CARTESIAN_POINT('Ctrl Pts',(-28.2531279933201,85.4215351983815,
78.6286589200921));
#216597=CARTESIAN_POINT('Ctrl Pts',(-28.2437348693344,85.2340537504691,
78.9621005282212));
#216598=CARTESIAN_POINT('Ctrl Pts',(-28.2210600401188,84.7386072304263,
79.7512362195004));
#216599=CARTESIAN_POINT('Ctrl Pts',(-28.2078112198607,84.4144054699502,
80.1956830082397));
#216600=CARTESIAN_POINT('Ctrl Pts',(-28.1753363154878,83.5566907558226,
81.2144043629737));
#216601=CARTESIAN_POINT('Ctrl Pts',(-28.1559785536078,82.9948032368779,
81.7613995684301));
#216602=CARTESIAN_POINT('Ctrl Pts',(-28.1238812834247,81.9658428687735,
82.5815420877053));
#216603=CARTESIAN_POINT('Ctrl Pts',(-28.1109864229189,81.5265898795775,
82.8855280811803));
#216604=CARTESIAN_POINT('Ctrl Pts',(-28.0794700449832,80.418330375655,83.5465389759851));
#216605=CARTESIAN_POINT('Ctrl Pts',(-28.0607213368762,79.7326514086105,
83.8710079993923));
#216606=CARTESIAN_POINT('Ctrl Pts',(-28.0217400834737,78.2352384276097,
84.4111238918871));
#216607=CARTESIAN_POINT('Ctrl Pts',(-28.0015951829068,77.4219904435121,
84.6105569535184));
#216608=CARTESIAN_POINT('Ctrl Pts',(-27.9625972218464,75.8528788255984,
84.8233527843671));
#216609=CARTESIAN_POINT('Ctrl Pts',(-27.9441287971005,75.1033342352144,
84.8533811491028));
#216610=CARTESIAN_POINT('Ctrl Pts',(-27.9073341281364,73.5959182828425,
84.7708230227862));
#216611=CARTESIAN_POINT('Ctrl Pts',(-27.888726346834,72.8416347153993,84.6559924550591));
#216612=CARTESIAN_POINT('Ctrl Pts',(-27.8604417150418,71.7318949057894,
84.375652234997));
#216613=CARTESIAN_POINT('Ctrl Pts',(-27.8509640987074,71.364952415787,84.2637479714313));
#216614=CARTESIAN_POINT('Ctrl Pts',(-27.8282682830005,70.492268569434,83.9505537038313));
#216615=CARTESIAN_POINT('Ctrl Pts',(-27.8150795458088,69.9937130697508,
83.7318272038345));
#216616=CARTESIAN_POINT('Ctrl Pts',(-27.7832572038282,68.8435533450949,
83.1296754073216));
#216617=CARTESIAN_POINT('Ctrl Pts',(-27.7645118776768,68.2101260901553,
82.7166516247409));
#216618=CARTESIAN_POINT('Ctrl Pts',(-27.7245009698029,66.9341789384272,
81.6988558809098));
#216619=CARTESIAN_POINT('Ctrl Pts',(-27.7032793625638,66.3110197248183,
81.0769319392354));
#216620=CARTESIAN_POINT('Ctrl Pts',(-27.6722362673775,65.5243560504484,
80.0947421788309));
#216621=CARTESIAN_POINT('Ctrl Pts',(-27.6628149603627,65.3008445051999,
79.7863065048586));
#216622=CARTESIAN_POINT('Ctrl Pts',(-27.6342006950588,64.6641157117326,
78.8120432954197));
#216623=CARTESIAN_POINT('Ctrl Pts',(-27.615329973039,64.3017571268858,78.115547465555));
#216624=CARTESIAN_POINT('Ctrl Pts',(-27.5777488947944,63.7331080256035,
76.694229870837));
#216625=CARTESIAN_POINT('Ctrl Pts',(-27.5592275305226,63.5217585243477,
75.9753180463411));
#216626=CARTESIAN_POINT('Ctrl Pts',(-27.5228483102149,63.2377878973354,
74.5088659335672));
#216627=CARTESIAN_POINT('Ctrl Pts',(-27.5047697867643,63.1655005946628,
73.7646740156392));
#216628=CARTESIAN_POINT('Ctrl Pts',(-27.4770681652961,63.1628123262026,
72.6379771073962));
#216629=CARTESIAN_POINT('Ctrl Pts',(-27.4676780097333,63.1802633466293,
72.2574861405776));
#216630=CARTESIAN_POINT('Ctrl Pts',(-27.4391622788875,63.289501810978,71.0994279551725));
#216631=CARTESIAN_POINT('Ctrl Pts',(-27.4203808244055,63.440046697084,70.3295595189917));
#216632=CARTESIAN_POINT('Ctrl Pts',(-27.3916342990449,63.7787757506774,
69.2033762014802));
#216633=CARTESIAN_POINT('Ctrl Pts',(-27.3819721225719,63.9107637104782,
68.832656384932));
#216634=CARTESIAN_POINT('Ctrl Pts',(-27.3723203524304,64.0608503540383,
68.4693880462876));
#216635=CARTESIAN_POINT('Origin',(-33.5526503323277,75.000050506625,72.9851176492631));
#216636=CARTESIAN_POINT('',(-37.9576288901553,64.0574429649795,68.4641091549305));
#216637=CARTESIAN_POINT('',(-38.2588681851947,64.0574481338172,68.4640966443434));
#216638=CARTESIAN_POINT('',(-33.5526503323277,64.0574429649796,68.4641091549303));
#216639=CARTESIAN_POINT('',(-37.9576293742551,64.0574354028926,68.4641274581798));
#216640=CARTESIAN_POINT('Ctrl Pts',(-37.9576288901553,64.0574429649794,
68.4641091549307));
#216641=CARTESIAN_POINT('Ctrl Pts',(-37.9576291329798,64.0574391718279,
68.4641183358399));
#216642=CARTESIAN_POINT('Ctrl Pts',(-37.9576293758043,64.0574353786878,
68.4641275167543));
#216643=CARTESIAN_POINT('Ctrl Pts',(-37.9576296186288,64.0574315855591,
68.4641366976736));
#216644=CARTESIAN_POINT('',(-38.418062421717,70.6974291912148,84.0154429842386));
#216645=CARTESIAN_POINT('Ctrl Pts',(-37.9576293742551,64.0574354028926,
68.4641274581798));
#216646=CARTESIAN_POINT('Ctrl Pts',(-37.9743923970413,63.7955819506003,
69.0979181590909));
#216647=CARTESIAN_POINT('Ctrl Pts',(-37.9910143370797,63.5892858234739,
69.753262138451));
#216648=CARTESIAN_POINT('Ctrl Pts',(-38.0246878629418,63.2931806340481,
71.0890404407701));
#216649=CARTESIAN_POINT('Ctrl Pts',(-38.0416261579981,63.2033680661301,
71.7668394361827));
#216650=CARTESIAN_POINT('Ctrl Pts',(-38.069412644704,63.1518376883327,72.9028136644737));
#216651=CARTESIAN_POINT('Ctrl Pts',(-38.0804609656725,63.1574159035511,
73.3578466686248));
#216652=CARTESIAN_POINT('Ctrl Pts',(-38.1107350192916,63.2436885873193,
74.5909878341748));
#216653=CARTESIAN_POINT('Ctrl Pts',(-38.1301458598497,63.3752737739155,
75.3632308490525));
#216654=CARTESIAN_POINT('Ctrl Pts',(-38.1586472136151,63.6827161611728,
76.484141368582));
#216655=CARTESIAN_POINT('Ctrl Pts',(-38.1679026268872,63.8011177859933,
76.8463520341654));
#216656=CARTESIAN_POINT('Ctrl Pts',(-38.1865718759954,64.0736906924759,
77.5614275400821));
#216657=CARTESIAN_POINT('Ctrl Pts',(-38.1959758912443,64.2280236950087,
77.9137470663033));
#216658=CARTESIAN_POINT('Ctrl Pts',(-38.2228550046262,64.7144503548113,
78.8916927172907));
#216659=CARTESIAN_POINT('Ctrl Pts',(-38.2403936753872,65.085880789799,79.4959123706368));
#216660=CARTESIAN_POINT('Ctrl Pts',(-38.2709383733594,65.8347216109281,
80.5000150089951));
#216661=CARTESIAN_POINT('Ctrl Pts',(-38.2841616948544,66.1901443631909,
80.9137044981226));
#216662=CARTESIAN_POINT('Ctrl Pts',(-38.3176332553364,67.1486407712281,
81.8849868311498));
#216663=CARTESIAN_POINT('Ctrl Pts',(-38.3379297371556,67.7835553047492,
82.4071404556692));
#216664=CARTESIAN_POINT('Ctrl Pts',(-38.3680731510726,68.8168416866319,
83.0907477428116));
#216665=CARTESIAN_POINT('Ctrl Pts',(-38.3782385943951,69.178411869877,83.3032741798193));
#216666=CARTESIAN_POINT('Ctrl Pts',(-38.3987282947051,69.9231681713914,
83.6894003576084));
#216667=CARTESIAN_POINT('Ctrl Pts',(-38.4090386083825,70.3058599943613,
83.8626621801093));
#216668=CARTESIAN_POINT('Ctrl Pts',(-38.4193726539769,70.6969410188162,
84.0152321705287));
#216669=CARTESIAN_POINT('',(-38.717056908316,70.6974160226281,84.0154504430313));
#216670=CARTESIAN_POINT('',(-38.4175364832709,70.69729039136,84.0153684626757));
#216671=CARTESIAN_POINT('Ctrl Pts',(-38.2588685144218,64.0574429649797,
68.4641091549301));
#216672=CARTESIAN_POINT('Ctrl Pts',(-38.2753921140801,63.7980242826514,
69.0920037570411));
#216673=CARTESIAN_POINT('Ctrl Pts',(-38.2919909110401,63.5931278905779,
69.7410687161469));
#216674=CARTESIAN_POINT('Ctrl Pts',(-38.3247086479941,63.2978613845077,
71.0629606633982));
#216675=CARTESIAN_POINT('Ctrl Pts',(-38.3408123281424,63.2073159003245,
71.7331880602663));
#216676=CARTESIAN_POINT('Ctrl Pts',(-38.3681764716619,63.152435191933,72.8567104434083));
#216677=CARTESIAN_POINT('Ctrl Pts',(-38.3791668041158,63.1561079854806,
73.3068378553902));
#216678=CARTESIAN_POINT('Ctrl Pts',(-38.404419780308,63.2237743787431,74.3443579761159));
#216679=CARTESIAN_POINT('Ctrl Pts',(-38.4185812414995,63.3061147155748,
74.9293606886987));
#216680=CARTESIAN_POINT('Ctrl Pts',(-38.4507641769266,63.5907017532673,
76.2354439569314));
#216681=CARTESIAN_POINT('Ctrl Pts',(-38.4690337585594,63.818367341293,76.948425810389));
#216682=CARTESIAN_POINT('Ctrl Pts',(-38.5056409803773,64.4099354287515,
78.3336123336521));
#216683=CARTESIAN_POINT('Ctrl Pts',(-38.5237690303283,64.7747131400765,
79.0017114320047));
#216684=CARTESIAN_POINT('Ctrl Pts',(-38.5602504821622,65.619694371161,80.2477433922699));
#216685=CARTESIAN_POINT('Ctrl Pts',(-38.5785684555972,66.0958665941443,
80.8242712373352));
#216686=CARTESIAN_POINT('Ctrl Pts',(-38.6162190079843,67.1937976489437,
81.9235023376853));
#216687=CARTESIAN_POINT('Ctrl Pts',(-38.6355332715921,67.821437222446,82.4349754727852));
#216688=CARTESIAN_POINT('Ctrl Pts',(-38.6653949765358,68.8416573233498,
83.1056540434989));
#216689=CARTESIAN_POINT('Ctrl Pts',(-38.6755171178592,69.1987422076271,
83.3144877599833));
#216690=CARTESIAN_POINT('Ctrl Pts',(-38.6956648674305,69.9338189535861,
83.6942191651615));
#216691=CARTESIAN_POINT('Ctrl Pts',(-38.7056764744093,70.311333866345,83.8648002743078));
#216692=CARTESIAN_POINT('Ctrl Pts',(-38.7156810426871,70.6970057304839,
84.0152574158675));
#216693=CARTESIAN_POINT('Origin',(-33.5526503323277,75.000050506625,72.9851176492631));
#216694=CARTESIAN_POINT('',(-36.4450710296185,64.0574429649796,68.4641091549303));
#216695=CARTESIAN_POINT('Ctrl Pts',(-38.2588681851947,64.0574481338172,
68.4640966443434));
#216696=CARTESIAN_POINT('Ctrl Pts',(-38.2414434766608,64.3310149227641,
67.8019602396254));
#216697=CARTESIAN_POINT('Ctrl Pts',(-38.2243669723514,64.6641105528954,
67.1660294946634));
#216698=CARTESIAN_POINT('Ctrl Pts',(-38.1901425424151,65.4307058494362,
65.9784220822238));
#216699=CARTESIAN_POINT('Ctrl Pts',(-38.1730504638907,65.8597525886812,
65.4272684079564));
#216700=CARTESIAN_POINT('Ctrl Pts',(-38.1448445435794,66.6516037811045,
64.5768018527136));
#216701=CARTESIAN_POINT('Ctrl Pts',(-38.1336955927266,66.9881920041458,
64.2554863627001));
#216702=CARTESIAN_POINT('Ctrl Pts',(-38.1005010922852,68.0368132134697,
63.3663092421297));
#216703=CARTESIAN_POINT('Ctrl Pts',(-38.0781641925283,68.7963532967956,
62.8597893706182));
#216704=CARTESIAN_POINT('Ctrl Pts',(-38.0375951524959,70.2844060093473,
62.0982906842396));
#216705=CARTESIAN_POINT('Ctrl Pts',(-38.019354404517,70.9943439608194,61.8175473993704));
#216706=CARTESIAN_POINT('Ctrl Pts',(-37.9853984113513,72.3315569437106,
61.4328033878864));
#216707=CARTESIAN_POINT('Ctrl Pts',(-37.9698933723247,72.9497326310281,
61.307231540618));
#216708=CARTESIAN_POINT('Ctrl Pts',(-37.9453930639585,73.9518904771438,
61.1857232957817));
#216709=CARTESIAN_POINT('Ctrl Pts',(-37.9362344946197,74.3308063654,61.158179777539));
#216710=CARTESIAN_POINT('Ctrl Pts',(-37.9052180248771,75.6095443451553,
61.1268859598937));
#216711=CARTESIAN_POINT('Ctrl Pts',(-37.8830430633134,76.5082777725493,
61.2074109640022));
#216712=CARTESIAN_POINT('Ctrl Pts',(-37.8424912106608,78.1373424093565,
61.5430432053088));
#216713=CARTESIAN_POINT('Ctrl Pts',(-37.8241156632569,78.8688244084466,
61.7692243491527));
#216714=CARTESIAN_POINT('Ctrl Pts',(-37.7960651734842,79.9243127389037,
62.2112349365072));
#216715=CARTESIAN_POINT('Ctrl Pts',(-37.7866917729287,80.2679321408877,
62.3750125899686));
#216716=CARTESIAN_POINT('Ctrl Pts',(-37.7589614148258,81.2610901329231,
62.9085355290734));
#216717=CARTESIAN_POINT('Ctrl Pts',(-37.7409544483602,81.8841843457121,
63.3235014855631));
#216718=CARTESIAN_POINT('Ctrl Pts',(-37.7036161430274,83.0709458880184,
64.2872940121883));
#216719=CARTESIAN_POINT('Ctrl Pts',(-37.6842369621448,83.6275561640151,
64.8390986245063));
#216720=CARTESIAN_POINT('Ctrl Pts',(-37.6463538210091,84.6135950831142,
66.0319626834408));
#216721=CARTESIAN_POINT('Ctrl Pts',(-37.6278611249987,85.0430814331657,
66.6681453231041));
#216722=CARTESIAN_POINT('Ctrl Pts',(-37.5996702665547,85.5893278172295,
67.6755133465216));
#216723=CARTESIAN_POINT('Ctrl Pts',(-37.590272072703,85.7543378558918,68.0182278249807));
#216724=CARTESIAN_POINT('Ctrl Pts',(-37.5624481356148,86.1940422193922,
69.0565773840484));
#216725=CARTESIAN_POINT('Ctrl Pts',(-37.5443772977862,86.419676216308,69.7709258240512));
#216726=CARTESIAN_POINT('Ctrl Pts',(-37.5069384910856,86.7403526451989,
71.2657909721727));
#216727=CARTESIAN_POINT('Ctrl Pts',(-37.4875270028055,86.8282110558048,
72.0441663747342));
#216728=CARTESIAN_POINT('Ctrl Pts',(-37.4495750678847,86.8490780878975,
73.5918578648581));
#216729=CARTESIAN_POINT('Ctrl Pts',(-37.4310387646194,86.7849732901166,
74.35741132429));
#216730=CARTESIAN_POINT('Ctrl Pts',(-37.4028147437794,86.579152016589,75.4848619131025));
#216731=CARTESIAN_POINT('Ctrl Pts',(-37.3934213460348,86.4930472056369,
75.8548457269552));
#216732=CARTESIAN_POINT('Ctrl Pts',(-37.3655903757164,86.1850285228373,
76.9392906385991));
#216733=CARTESIAN_POINT('Ctrl Pts',(-37.3475139631943,85.9130691799396,
77.6375624088148));
#216734=CARTESIAN_POINT('Ctrl Pts',(-37.310072347362,85.225841874519,79.0037821457513));
#216735=CARTESIAN_POINT('Ctrl Pts',(-37.2906678380084,84.8063176271644,
79.6655555737842));
#216736=CARTESIAN_POINT('Ctrl Pts',(-37.2527790121884,83.8528030073251,
80.8841842070412));
#216737=CARTESIAN_POINT('Ctrl Pts',(-37.2342874438966,83.3235642099088,
81.4400337256653));
#216738=CARTESIAN_POINT('Ctrl Pts',(-37.2061467389023,82.4575542992148,
82.1888991369763));
#216739=CARTESIAN_POINT('Ctrl Pts',(-37.1967849130386,82.1589870568592,
82.4229978799163));
#216740=CARTESIAN_POINT('Ctrl Pts',(-37.1690316885729,81.2398185526467,
83.0749419796226));
#216741=CARTESIAN_POINT('Ctrl Pts',(-37.151006461953,80.5903269559619,83.4487724206279));
#216742=CARTESIAN_POINT('Ctrl Pts',(-37.1136623142814,79.1981706352352,
84.0832158447184));
#216743=CARTESIAN_POINT('Ctrl Pts',(-37.0943072151199,78.4560178963457,
84.3362533233397));
#216744=CARTESIAN_POINT('Ctrl Pts',(-37.0565881341238,76.9503097399315,
84.6881302251893));
#216745=CARTESIAN_POINT('Ctrl Pts',(-37.0382056349772,76.1911765655033,
84.7895761321428));
#216746=CARTESIAN_POINT('Ctrl Pts',(-37.0102222952616,75.0488340970667,
84.8308524154469));
#216747=CARTESIAN_POINT('Ctrl Pts',(-37.0009036630239,74.6696514374755,
84.8263442654468));
#216748=CARTESIAN_POINT('Ctrl Pts',(-36.9732759310988,73.5450728746751,
84.7589078589771));
#216749=CARTESIAN_POINT('Ctrl Pts',(-36.9553346668574,72.804721093565,84.643574932408));
#216750=CARTESIAN_POINT('Ctrl Pts',(-36.9182469519714,71.3257018042379,
84.2672040914431));
#216751=CARTESIAN_POINT('Ctrl Pts',(-36.8990684764574,70.5919789919822,
84.0012518956182));
#216752=CARTESIAN_POINT('Ctrl Pts',(-36.8616582722482,69.2024366261997,
83.3363644730011));
#216753=CARTESIAN_POINT('Ctrl Pts',(-36.8434135515956,68.5485245096775,
82.9419473064971));
#216754=CARTESIAN_POINT('Ctrl Pts',(-36.8155999070953,67.6325819179565,
82.2611353472256));
#216755=CARTESIAN_POINT('Ctrl Pts',(-36.8063125882316,67.3391630212681,
82.0203210204782));
#216756=CARTESIAN_POINT('Ctrl Pts',(-36.7788002724731,66.5036590832524,
81.2646004878822));
#216757=CARTESIAN_POINT('Ctrl Pts',(-36.7609404523299,65.9981986920098,
80.7120296317288));
#216758=CARTESIAN_POINT('Ctrl Pts',(-36.7240649617963,65.0806505347689,
79.4957542552416));
#216759=CARTESIAN_POINT('Ctrl Pts',(-36.7050131040977,64.6751964958442,
78.8315069658785));
#216760=CARTESIAN_POINT('Ctrl Pts',(-36.6678205147483,64.0073444470835,
77.4480743136396));
#216761=CARTESIAN_POINT('Ctrl Pts',(-36.6496859095303,63.7436413231345,
76.7335610705654));
#216762=CARTESIAN_POINT('Ctrl Pts',(-36.6219871628855,63.4534983234491,
75.6311978500145));
#216763=CARTESIAN_POINT('Ctrl Pts',(-36.6127084198458,63.3745175967954,
75.2592309883459));
#216764=CARTESIAN_POINT('Ctrl Pts',(-36.5852547483898,63.1938055523443,
74.1471221349221));
#216765=CARTESIAN_POINT('Ctrl Pts',(-36.5674386766604,63.1440321801278,
73.4004552593166));
#216766=CARTESIAN_POINT('Ctrl Pts',(-36.5304558753239,63.1868329889988,
71.8702137011023));
#216767=CARTESIAN_POINT('Ctrl Pts',(-36.5112359744591,63.2865808289669,
71.090456946076));
#216768=CARTESIAN_POINT('Ctrl Pts',(-36.4830518847883,63.5481892516628,
69.9552594336278));
#216769=CARTESIAN_POINT('Ctrl Pts',(-36.4739208179995,63.6515484448178,
69.5885503747416));
#216770=CARTESIAN_POINT('Ctrl Pts',(-36.4582052209673,63.8586852775821,
68.9696380730014));
#216771=CARTESIAN_POINT('Ctrl Pts',(-36.451650075586,63.9537685944047,68.7150416516842));
#216772=CARTESIAN_POINT('Ctrl Pts',(-36.4450710296185,64.0574429649796,
68.4641091549303));
#216773=CARTESIAN_POINT('',(-36.143425535889,64.0574429649796,68.4641091549303));
#216774=CARTESIAN_POINT('',(-33.5526503323277,64.0574429649796,68.4641091549303));
#216775=CARTESIAN_POINT('Ctrl Pts',(-36.143425535889,64.0574429649796,68.4641091549303));
#216776=CARTESIAN_POINT('Ctrl Pts',(-36.150344663908,63.949728708768,68.7248197538689));
#216777=CARTESIAN_POINT('Ctrl Pts',(-36.157295342917,63.8512897815639,68.9894811601397));
#216778=CARTESIAN_POINT('Ctrl Pts',(-36.1736752316992,63.6424020128784,
69.6192352301631));
#216779=CARTESIAN_POINT('Ctrl Pts',(-36.1831080458738,63.5399756356306,
69.9864465986742));
#216780=CARTESIAN_POINT('Ctrl Pts',(-36.2108803965733,63.289093886627,71.0889039027289));
#216781=CARTESIAN_POINT('Ctrl Pts',(-36.2289847357361,63.1925500483805,
71.8340004654652));
#216782=CARTESIAN_POINT('Ctrl Pts',(-36.2657906428265,63.1417460476561,
73.3297640466191));
#216783=CARTESIAN_POINT('Ctrl Pts',(-36.2843345525679,63.1870974288601,
74.0770488854905));
#216784=CARTESIAN_POINT('Ctrl Pts',(-36.3118251489354,63.3610984532145,
75.1893089803292));
#216785=CARTESIAN_POINT('Ctrl Pts',(-36.3210376246501,63.4375713261465,
75.5605282235205));
#216786=CARTESIAN_POINT('Ctrl Pts',(-36.3489337273685,63.7210228696664,
76.6653419480273));
#216787=CARTESIAN_POINT('Ctrl Pts',(-36.3678039581695,63.9811134418178,
77.3832454842242));
#216788=CARTESIAN_POINT('Ctrl Pts',(-36.4058033435647,64.6448449919314,
78.7785158191203));
#216789=CARTESIAN_POINT('Ctrl Pts',(-36.4246857004833,65.0506980060946,
79.4507291466379));
#216790=CARTESIAN_POINT('Ctrl Pts',(-36.4622871396387,65.9677741190266,
80.6764745687496));
#216791=CARTESIAN_POINT('Ctrl Pts',(-36.4808155600896,66.4712811169162,
81.2312737195149));
#216792=CARTESIAN_POINT('Ctrl Pts',(-36.5172166971965,67.5751281626403,
82.2375453080713));
#216793=CARTESIAN_POINT('Ctrl Pts',(-36.535310990023,68.1728120791836,82.6869578644967));
#216794=CARTESIAN_POINT('Ctrl Pts',(-36.5630353317565,69.1332668695483,
83.2761782650808));
#216795=CARTESIAN_POINT('Ctrl Pts',(-36.5724321849271,69.4671444690562,
83.4594686865642));
#216796=CARTESIAN_POINT('Ctrl Pts',(-36.6009705412535,70.5126686807691,
83.9694738677818));
#216797=CARTESIAN_POINT('Ctrl Pts',(-36.619769591115,71.2483574496679,84.2420035092752));
#216798=CARTESIAN_POINT('Ctrl Pts',(-36.6572285748738,72.7297284296824,
84.6292624832212));
#216799=CARTESIAN_POINT('Ctrl Pts',(-36.6757180584941,73.4702456101325,
84.7494781144531));
#216800=CARTESIAN_POINT('Ctrl Pts',(-36.7119578321393,74.9596528302929,
84.8481817928625));
#216801=CARTESIAN_POINT('Ctrl Pts',(-36.7299152908744,75.7051514321559,
84.8272777263948));
#216802=CARTESIAN_POINT('Ctrl Pts',(-36.75746172588,76.8214862152428,84.6901335000161));
#216803=CARTESIAN_POINT('Ctrl Pts',(-36.7668154143757,77.1967758641369,
84.6255395369988));
#216804=CARTESIAN_POINT('Ctrl Pts',(-36.7952297270275,78.3317958994633,
84.3733289843863));
#216805=CARTESIAN_POINT('Ctrl Pts',(-36.8139300780076,79.0766036901995,
84.1284385623949));
#216806=CARTESIAN_POINT('Ctrl Pts',(-36.8512270455754,80.4775485634038,
83.5084036045176));
#216807=CARTESIAN_POINT('Ctrl Pts',(-36.869675612657,81.1329102440116,83.1404399745297));
#216808=CARTESIAN_POINT('Ctrl Pts',(-36.9067267671718,82.3918362796064,
82.2670205758651));
#216809=CARTESIAN_POINT('Ctrl Pts',(-36.9255158012893,82.9888378618979,
81.7584577091205));
#216810=CARTESIAN_POINT('Ctrl Pts',(-36.9538947456751,83.7952725063491,
80.9204296069613));
#216811=CARTESIAN_POINT('Ctrl Pts',(-36.963214092309,84.0458597771048,80.6335449786799));
#216812=CARTESIAN_POINT('Ctrl Pts',(-36.9914822902786,84.7674231956479,
79.7222961302464));
#216813=CARTESIAN_POINT('Ctrl Pts',(-37.0101030569021,85.1907823934553,
79.0629569003044));
#216814=CARTESIAN_POINT('Ctrl Pts',(-37.0472576464522,85.8864387837798,
77.6997198682105));
#216815=CARTESIAN_POINT('Ctrl Pts',(-37.065612430509,86.1627648953464,77.0019248131487));
#216816=CARTESIAN_POINT('Ctrl Pts',(-37.1016656105856,86.579429173952,75.5651215855737));
#216817=CARTESIAN_POINT('Ctrl Pts',(-37.1195806184897,86.7191342402651,
74.8294348117883));
#216818=CARTESIAN_POINT('Ctrl Pts',(-37.1470332023142,86.8239323455018,
73.7067268535619));
#216819=CARTESIAN_POINT('Ctrl Pts',(-37.1563288769829,86.8410126474363,
73.3264636012985));
#216820=CARTESIAN_POINT('Ctrl Pts',(-37.1919423809732,86.8361742115752,
71.8605275850765));
#216821=CARTESIAN_POINT('Ctrl Pts',(-37.2177409034923,86.6833223747396,
70.7806478277577));
#216822=CARTESIAN_POINT('Ctrl Pts',(-37.2535315604924,86.2806834306116,
69.3693936270167));
#216823=CARTESIAN_POINT('Ctrl Pts',(-37.2628531615979,86.1581434925881,
69.0072912123014));
#216824=CARTESIAN_POINT('Ctrl Pts',(-37.2852523240675,85.8188085323026,
68.1444799016979));
#216825=CARTESIAN_POINT('Ctrl Pts',(-37.2982983178231,85.5845126000387,
67.6515950853675));
#216826=CARTESIAN_POINT('Ctrl Pts',(-37.3298555333421,84.9447047871049,
66.5151714252758));
#216827=CARTESIAN_POINT('Ctrl Pts',(-37.3484845848829,84.5095695974514,
65.8910783032959));
#216828=CARTESIAN_POINT('Ctrl Pts',(-37.3891037638151,83.422752591122,64.6136645209313));
#216829=CARTESIAN_POINT('Ctrl Pts',(-37.4110587849797,82.7484795689489,
63.9859514052492));
#216830=CARTESIAN_POINT('Ctrl Pts',(-37.4427893467416,81.7016955582058,
63.2171591033633));
#216831=CARTESIAN_POINT('Ctrl Pts',(-37.4521155254852,81.3842235651512,
63.0067713299031));
#216832=CARTESIAN_POINT('Ctrl Pts',(-37.4813623614136,80.3502700995172,
62.3911482571134));
#216833=CARTESIAN_POINT('Ctrl Pts',(-37.5010298289139,79.6014209793702,
62.0450794621067));
#216834=CARTESIAN_POINT('Ctrl Pts',(-37.5393383871761,78.1164497815894,
61.5384950013363));
#216835=CARTESIAN_POINT('Ctrl Pts',(-37.5576437284937,77.3889305276865,
61.3648605223285));
#216836=CARTESIAN_POINT('Ctrl Pts',(-37.5941044591884,75.8967514857712,
61.1548764318305));
#216837=CARTESIAN_POINT('Ctrl Pts',(-37.6125360809817,75.1351187113621,
61.1217105030284));
#216838=CARTESIAN_POINT('Ctrl Pts',(-37.6405703393137,73.994637819479,61.1819464044539));
#216839=CARTESIAN_POINT('Ctrl Pts',(-37.6499529261285,73.6148805630276,
61.2204666865765));
#216840=CARTESIAN_POINT('Ctrl Pts',(-37.6818356456923,72.3210422946476,
61.4152303066326));
#216841=CARTESIAN_POINT('Ctrl Pts',(-37.7041476426852,71.4238047089491,
61.6603725433316));
#216842=CARTESIAN_POINT('Ctrl Pts',(-37.7363127895092,70.211192631959,62.1503529944448));
#216843=CARTESIAN_POINT('Ctrl Pts',(-37.7457068258623,69.8650992012847,
62.3100269910231));
#216844=CARTESIAN_POINT('Ctrl Pts',(-37.7748819757287,68.8071456430532,
62.8614988235704));
#216845=CARTESIAN_POINT('Ctrl Pts',(-37.7944363211069,68.1275159740027,
63.3099945510022));
#216846=CARTESIAN_POINT('Ctrl Pts',(-37.8262409401161,67.1261775375445,
64.1299109310361));
#216847=CARTESIAN_POINT('Ctrl Pts',(-37.8381647281714,66.7721994428131,
64.4578069790688));
#216848=CARTESIAN_POINT('Ctrl Pts',(-37.8678433035642,65.9370428220467,
65.3319809651629));
#216849=CARTESIAN_POINT('Ctrl Pts',(-37.8853680887045,65.4843604535277,
65.9027271549346));
#216850=CARTESIAN_POINT('Ctrl Pts',(-37.921291353889,64.6836765487467,67.1288042814053));
#216851=CARTESIAN_POINT('Ctrl Pts',(-37.9396026305779,64.3390303884866,
67.7825575347635));
#216852=CARTESIAN_POINT('Ctrl Pts',(-37.9576288901553,64.0574429649794,
68.4641091549307));
#216853=CARTESIAN_POINT('Origin',(-33.5526503323277,75.000050506625,72.9851176492631));
#216854=CARTESIAN_POINT('',(-34.329622639475,64.0574429649796,68.4641091549303));
#216855=CARTESIAN_POINT('',(-34.6308727569695,64.0574429676145,68.4641091485529));
#216856=CARTESIAN_POINT('',(-33.5526503323277,64.0574429649796,68.4641091549303));
#216857=CARTESIAN_POINT('Ctrl Pts',(-34.329622639475,64.0574429649796,68.4641091549303));
#216858=CARTESIAN_POINT('Ctrl Pts',(-34.3328410372056,64.007573846542,68.5848119123337));
#216859=CARTESIAN_POINT('Ctrl Pts',(-34.3360540786868,63.959688302845,68.7063725776957));
#216860=CARTESIAN_POINT('Ctrl Pts',(-34.3580359830751,63.6448520668864,
69.5461309260396));
#216861=CARTESIAN_POINT('Ctrl Pts',(-34.376557966046,63.44616071442,70.2879342041745));
#216862=CARTESIAN_POINT('Ctrl Pts',(-34.4047790580826,63.2582236639502,
71.4185685693466));
#216863=CARTESIAN_POINT('Ctrl Pts',(-34.4141806967683,63.2139971953326,
71.7962021308897));
#216864=CARTESIAN_POINT('Ctrl Pts',(-34.4420214994181,63.1368760532764,
72.9211034112473));
#216865=CARTESIAN_POINT('Ctrl Pts',(-34.4601026172894,63.1564931489113,
73.6700676863727));
#216866=CARTESIAN_POINT('Ctrl Pts',(-34.4975535582399,63.3407866732681,
75.1879448697782));
#216867=CARTESIAN_POINT('Ctrl Pts',(-34.5169664948619,63.5115530869257,
75.9524904167847));
#216868=CARTESIAN_POINT('Ctrl Pts',(-34.5549000929086,63.9963963469406,
77.4220724239963));
#216869=CARTESIAN_POINT('Ctrl Pts',(-34.5734177476563,64.3064317654138,
78.1245240046365));
#216870=CARTESIAN_POINT('Ctrl Pts',(-34.6016076709931,64.8682642371642,
79.1227957722569));
#216871=CARTESIAN_POINT('Ctrl Pts',(-34.6109892258484,65.0701790035698,
79.4443619490049));
#216872=CARTESIAN_POINT('Ctrl Pts',(-34.6387895248276,65.7147305456016,
80.3690188391609));
#216873=CARTESIAN_POINT('Ctrl Pts',(-34.6568442825143,66.199410787854,80.9404872681069));
#216874=CARTESIAN_POINT('Ctrl Pts',(-34.6936647548305,67.2776918025048,
81.9918041354446));
#216875=CARTESIAN_POINT('Ctrl Pts',(-34.7124516774763,67.8702515653957,
82.4677956902649));
#216876=CARTESIAN_POINT('Ctrl Pts',(-34.7496662449242,69.1415892072909,
83.302081586579));
#216877=CARTESIAN_POINT('Ctrl Pts',(-34.7680254416173,69.8178417682874,
83.657794692478));
#216878=CARTESIAN_POINT('Ctrl Pts',(-34.7960437038153,70.8758878011957,
84.0899040321921));
#216879=CARTESIAN_POINT('Ctrl Pts',(-34.8054165914355,71.2349247367758,
84.2167170773129));
#216880=CARTESIAN_POINT('Ctrl Pts',(-34.8331421595484,72.3150444718224,
84.5405946628289));
#216881=CARTESIAN_POINT('Ctrl Pts',(-34.8511315453349,73.0493501182373,
84.6869583952719));
#216882=CARTESIAN_POINT('Ctrl Pts',(-34.8854695763134,74.4528595272905,
84.8308497642501));
#216883=CARTESIAN_POINT('Ctrl Pts',(-34.9017898275013,75.1177068099017,
84.8428972389196));
#216884=CARTESIAN_POINT('Ctrl Pts',(-34.936406968855,76.528197800239,84.7497731105241));
#216885=CARTESIAN_POINT('Ctrl Pts',(-34.9543702819887,77.2699683015172,
84.6294221197));
#216886=CARTESIAN_POINT('Ctrl Pts',(-34.9898344684854,78.6803005161217,
84.2606291027832));
#216887=CARTESIAN_POINT('Ctrl Pts',(-35.0072655248959,79.3477930374311,
84.0204485537004));
#216888=CARTESIAN_POINT('Ctrl Pts',(-35.0429456340828,80.678985892876,83.4018063075007));
#216889=CARTESIAN_POINT('Ctrl Pts',(-35.0611283723938,81.3357223847079,
83.0159192206579));
#216890=CARTESIAN_POINT('Ctrl Pts',(-35.0958873047512,82.4910163575538,
82.1780881374089));
#216891=CARTESIAN_POINT('Ctrl Pts',(-35.1122714837876,82.9970305716071,
81.7414635134517));
#216892=CARTESIAN_POINT('Ctrl Pts',(-35.1469067087876,83.9992025561383,
80.7170089785071));
#216893=CARTESIAN_POINT('Ctrl Pts',(-35.1652695219503,84.480438013047,80.1187797735805));
#216894=CARTESIAN_POINT('Ctrl Pts',(-35.193204737113,85.1091767267621,79.1601089106799));
#216895=CARTESIAN_POINT('Ctrl Pts',(-35.2025108666628,85.3023859788698,
78.8320684461682));
#216896=CARTESIAN_POINT('Ctrl Pts',(-35.2263321118681,85.7580152097419,
77.9655398777807));
#216897=CARTESIAN_POINT('Ctrl Pts',(-35.2406388975228,85.9959943942473,
77.4154256306083));
#216898=CARTESIAN_POINT('Ctrl Pts',(-35.2736399963111,86.4423444486803,
76.1228501451394));
#216899=CARTESIAN_POINT('Ctrl Pts',(-35.2924354339417,86.6219276736402,
75.3732997522042));
#216900=CARTESIAN_POINT('Ctrl Pts',(-35.3300841136658,86.834912514404,73.8376535630978));
#216901=CARTESIAN_POINT('Ctrl Pts',(-35.3486765129286,86.8653741790135,
73.0549259568729));
#216902=CARTESIAN_POINT('Ctrl Pts',(-35.3857942940093,86.7735803233313,
71.5273709295168));
#216903=CARTESIAN_POINT('Ctrl Pts',(-35.4041420580473,86.6578322326881,
70.7857625520058));
#216904=CARTESIAN_POINT('Ctrl Pts',(-35.4401939098107,86.2882005631754,
69.3359748366212));
#216905=CARTESIAN_POINT('Ctrl Pts',(-35.4581130644233,86.0354513284752,
68.6309814524176));
#216906=CARTESIAN_POINT('Ctrl Pts',(-35.4855759339169,85.556399636919,67.6103399887257));
#216907=CARTESIAN_POINT('Ctrl Pts',(-35.4948726091547,85.3783642430428,
67.2741329989908));
#216908=CARTESIAN_POINT('Ctrl Pts',(-35.531338005368,84.6135679832816,65.9841451450563));
#216909=CARTESIAN_POINT('Ctrl Pts',(-35.5579864562403,83.908981791799,65.1070292498714));
#216910=CARTESIAN_POINT('Ctrl Pts',(-35.5946951251752,82.8122259131197,
64.0802461994236));
#216911=CARTESIAN_POINT('Ctrl Pts',(-35.6040421534392,82.5201421013164,
63.8322467533819));
#216912=CARTESIAN_POINT('Ctrl Pts',(-35.6295659956507,81.6833788311474,
63.1889136151298));
#216913=CARTESIAN_POINT('Ctrl Pts',(-35.6457034022072,81.1162452310444,
62.8251642144548));
#216914=CARTESIAN_POINT('Ctrl Pts',(-35.680277594224,79.8609652453171,62.1634304279172));
#216915=CARTESIAN_POINT('Ctrl Pts',(-35.6986116870204,79.1691773955946,
61.8785522175689));
#216916=CARTESIAN_POINT('Ctrl Pts',(-35.7258814921413,78.0907288638883,
61.5495118547579));
#216917=CARTESIAN_POINT('Ctrl Pts',(-35.735072873367,77.721115173045,61.4559728680872));
#216918=CARTESIAN_POINT('Ctrl Pts',(-35.7628238764255,76.600692547838,61.2293156692559));
#216919=CARTESIAN_POINT('Ctrl Pts',(-35.7815886916175,75.8409082877967,
61.1506814660122));
#216920=CARTESIAN_POINT('Ctrl Pts',(-35.8211037742345,74.2212846613405,
61.139900525995));
#216921=CARTESIAN_POINT('Ctrl Pts',(-35.8416699054654,73.3656228487008,
61.2273840662669));
#216922=CARTESIAN_POINT('Ctrl Pts',(-35.8810222115305,71.7960163506922,
61.5626411689096));
#216923=CARTESIAN_POINT('Ctrl Pts',(-35.899392301876,71.0815089746368,61.7876248417063));
#216924=CARTESIAN_POINT('Ctrl Pts',(-35.9360511252781,69.6906469837769,
62.3751354523281));
#216925=CARTESIAN_POINT('Ctrl Pts',(-35.9546215154439,69.0185986053835,
62.7389616667079));
#216926=CARTESIAN_POINT('Ctrl Pts',(-35.98283479605,68.0687604892494,63.3786674373421));
#216927=CARTESIAN_POINT('Ctrl Pts',(-35.9922707319748,67.7618576907462,
63.6077387753892));
#216928=CARTESIAN_POINT('Ctrl Pts',(-36.0150469978111,67.0422585983395,
64.2012535376619));
#216929=CARTESIAN_POINT('Ctrl Pts',(-36.0283551584318,66.6428322592933,
64.5803793674515));
#216930=CARTESIAN_POINT('Ctrl Pts',(-36.0602688669262,65.7615479882361,
65.5420463597641));
#216931=CARTESIAN_POINT('Ctrl Pts',(-36.0789854907851,65.3062029861294,
66.1456327275155));
#216932=CARTESIAN_POINT('Ctrl Pts',(-36.1128442950801,64.5825234260087,
67.3238345517627));
#216933=CARTESIAN_POINT('Ctrl Pts',(-36.1280349982047,64.2970367858784,
67.884198465803));
#216934=CARTESIAN_POINT('Ctrl Pts',(-36.143425535889,64.0574429649796,68.4641091549303));
#216935=CARTESIAN_POINT('Ctrl Pts',(-36.4450710296185,64.0574429649796,
68.4641091549303));
#216936=CARTESIAN_POINT('Ctrl Pts',(-36.4298164832544,64.2978281972046,
67.8822829410793));
#216937=CARTESIAN_POINT('Ctrl Pts',(-36.4143869921359,64.5844003708168,
67.320155813866));
#216938=CARTESIAN_POINT('Ctrl Pts',(-36.3898142487375,65.1146479711371,
66.457880202735));
#216939=CARTESIAN_POINT('Ctrl Pts',(-36.3806431374805,65.3303077109132,
66.1424509966232));
#216940=CARTESIAN_POINT('Ctrl Pts',(-36.3531792325554,66.0185791796317,
65.2334495843888));
#216941=CARTESIAN_POINT('Ctrl Pts',(-36.3347698949052,66.5333448401378,
64.6742772282592));
#216942=CARTESIAN_POINT('Ctrl Pts',(-36.2980088765867,67.6540259236155,
63.6698862256385));
#216943=CARTESIAN_POINT('Ctrl Pts',(-36.280101406125,68.2559115284866,63.2252915191186));
#216944=CARTESIAN_POINT('Ctrl Pts',(-36.2423773112362,69.5916712184815,
62.4215255838452));
#216945=CARTESIAN_POINT('Ctrl Pts',(-36.2224209560955,70.3289509845132,
62.0754496513156));
#216946=CARTESIAN_POINT('Ctrl Pts',(-36.1841980023478,71.8123473356619,
61.5573109545676));
#216947=CARTESIAN_POINT('Ctrl Pts',(-36.1660256681261,72.5512763520278,
61.3765117920296));
#216948=CARTESIAN_POINT('Ctrl Pts',(-36.1346419626985,73.82391954092,61.1921293544449));
#216949=CARTESIAN_POINT('Ctrl Pts',(-36.1216763190792,74.3498884554293,
61.151473079505));
#216950=CARTESIAN_POINT('Ctrl Pts',(-36.0994659201618,75.2587981889374,
61.1420117351625));
#216951=CARTESIAN_POINT('Ctrl Pts',(-36.0902316936128,75.6407534126919,
61.1565248247328));
#216952=CARTESIAN_POINT('Ctrl Pts',(-36.0624859131522,76.7817823975121,
61.2553171806789));
#216953=CARTESIAN_POINT('Ctrl Pts',(-36.0438624321168,77.534077001011,61.3945401981191));
#216954=CARTESIAN_POINT('Ctrl Pts',(-36.0067408999156,78.9853669007069,
61.8112676918779));
#216955=CARTESIAN_POINT('Ctrl Pts',(-35.988694344898,79.6819222076254,62.0847621186578));
#216956=CARTESIAN_POINT('Ctrl Pts',(-35.9528381109727,80.9957693853785,
62.749953381127));
#216957=CARTESIAN_POINT('Ctrl Pts',(-35.9349493439011,81.6119380123203,
63.1367591984324));
#216958=CARTESIAN_POINT('Ctrl Pts',(-35.907678042527,82.4933009343184,63.8102467212397));
#216959=CARTESIAN_POINT('Ctrl Pts',(-35.8983499566447,82.7863426510017,
64.0575920235313));
#216960=CARTESIAN_POINT('Ctrl Pts',(-35.8614700593617,83.8961440396948,
65.0906122161347));
#216961=CARTESIAN_POINT('Ctrl Pts',(-35.8334895166668,84.6103459856919,
65.9775571670355));
#216962=CARTESIAN_POINT('Ctrl Pts',(-35.7964986090976,85.3813316779486,
67.2795294806806));
#216963=CARTESIAN_POINT('Ctrl Pts',(-35.7872658099445,85.5591885265115,
67.6158215934341));
#216964=CARTESIAN_POINT('Ctrl Pts',(-35.7597598446311,86.0375647481716,
68.6363994632009));
#216965=CARTESIAN_POINT('Ctrl Pts',(-35.7413319462033,86.2898632650145,
69.341193146973));
#216966=CARTESIAN_POINT('Ctrl Pts',(-35.7044264898673,86.6588103655716,
70.7909149069742));
#216967=CARTESIAN_POINT('Ctrl Pts',(-35.6863309381048,86.7742450080173,
71.5326880315955));
#216968=CARTESIAN_POINT('Ctrl Pts',(-35.648818522624,86.8653410612362,73.0604102750672));
#216969=CARTESIAN_POINT('Ctrl Pts',(-35.6293949578551,86.8345171836741,
73.8431304686555));
#216970=CARTESIAN_POINT('Ctrl Pts',(-35.5914248899701,86.6207960504798,
75.3788553687848));
#216971=CARTESIAN_POINT('Ctrl Pts',(-35.5728030752626,86.4408091712799,
76.1284841366248));
#216972=CARTESIAN_POINT('Ctrl Pts',(-35.5391741685667,85.9946680641214,
77.4183380945881));
#216973=CARTESIAN_POINT('Ctrl Pts',(-35.5243979477909,85.7577235077533,
77.9658340946686));
#216974=CARTESIAN_POINT('Ctrl Pts',(-35.5005313230928,85.3035724210339,
78.8299775913738));
#216975=CARTESIAN_POINT('Ctrl Pts',(-35.4912888580847,85.110428363515,79.1580595645729));
#216976=CARTESIAN_POINT('Ctrl Pts',(-35.4633045591508,84.4818599519238,
80.1168940152686));
#216977=CARTESIAN_POINT('Ctrl Pts',(-35.4443955308527,84.0007161641202,
80.7152502025691));
#216978=CARTESIAN_POINT('Ctrl Pts',(-35.4090375332272,82.9964579657966,
81.7422333759297));
#216979=CARTESIAN_POINT('Ctrl Pts',(-35.3928563160963,82.4878873656021,
82.1808725462551));
#216980=CARTESIAN_POINT('Ctrl Pts',(-35.3579265617688,81.3296222879418,
83.0197530690348));
#216981=CARTESIAN_POINT('Ctrl Pts',(-35.3391279751791,80.6728453803328,
83.405135571618));
#216982=CARTESIAN_POINT('Ctrl Pts',(-35.3033828774365,79.3481763536406,
84.0198277539064));
#216983=CARTESIAN_POINT('Ctrl Pts',(-35.2865212158438,78.6877362201186,
84.2577396147604));
#216984=CARTESIAN_POINT('Ctrl Pts',(-35.2510519203333,77.284704845737,84.626559331621));
#216985=CARTESIAN_POINT('Ctrl Pts',(-35.2325091256342,76.5427786576456,
84.7478897133586));
#216986=CARTESIAN_POINT('Ctrl Pts',(-35.1952623815698,75.0135616251408,
84.8507159279305));
#216987=CARTESIAN_POINT('Ctrl Pts',(-35.1763953294977,74.2294630684508,
84.8256751358169));
#216988=CARTESIAN_POINT('Ctrl Pts',(-35.1478966196537,73.0761780802292,
84.6737362045891));
#216989=CARTESIAN_POINT('Ctrl Pts',(-35.138539351106,72.7013848555789,84.6058415969981));
#216990=CARTESIAN_POINT('Ctrl Pts',(-35.1101296852693,71.5685208016559,
84.3436613971395));
#216991=CARTESIAN_POINT('Ctrl Pts',(-35.0914263267071,70.8258735601296,
84.0922397600767));
#216992=CARTESIAN_POINT('Ctrl Pts',(-35.054130075419,69.4309872081884,83.4601886701129));
#216993=CARTESIAN_POINT('Ctrl Pts',(-35.0356993205511,68.7794052416668,
83.0868580877431));
#216994=CARTESIAN_POINT('Ctrl Pts',(-34.9996002786209,67.560023159752,82.2252169376686));
#216995=CARTESIAN_POINT('Ctrl Pts',(-34.9817302608228,66.9943605823161,
81.7396804913581));
#216996=CARTESIAN_POINT('Ctrl Pts',(-34.9543056214923,66.2138359483376,
80.9303940226674));
#216997=CARTESIAN_POINT('Ctrl Pts',(-34.9449898578565,65.9630283097317,
80.643917330957));
#216998=CARTESIAN_POINT('Ctrl Pts',(-34.907689131715,65.0106648544754,79.4440609710513));
#216999=CARTESIAN_POINT('Ctrl Pts',(-34.8802940945988,64.4302316129435,
78.4426538658593));
#217000=CARTESIAN_POINT('Ctrl Pts',(-34.8428433081152,63.8613744289818,
77.017131525699));
#217001=CARTESIAN_POINT('Ctrl Pts',(-34.8335088458404,63.7366295916944,
76.6542583158344));
#217002=CARTESIAN_POINT('Ctrl Pts',(-34.8068931854123,63.4289538650965,
75.5944183497892));
#217003=CARTESIAN_POINT('Ctrl Pts',(-34.7896486514922,63.2917027200569,
74.8859911727886));
#217004=CARTESIAN_POINT('Ctrl Pts',(-34.7539743461902,63.1449742572066,
73.4265644299001));
#217005=CARTESIAN_POINT('Ctrl Pts',(-34.7357712603519,63.14072784864,72.6782228425266));
#217006=CARTESIAN_POINT('Ctrl Pts',(-34.6994034392337,63.2748858221362,
71.1723406594849));
#217007=CARTESIAN_POINT('Ctrl Pts',(-34.6809565209563,63.4165059879159,
70.418575997231));
#217008=CARTESIAN_POINT('Ctrl Pts',(-34.6529840677361,63.736348649039,69.3170045548025));
#217009=CARTESIAN_POINT('Ctrl Pts',(-34.6436639930778,63.8605228427577,
68.9556065871905));
#217010=CARTESIAN_POINT('Ctrl Pts',(-34.633246674525,64.0201624213107,68.5551452692357));
#217011=CARTESIAN_POINT('Ctrl Pts',(-34.6320592341848,64.0386618588475,
68.5095667720041));
#217012=CARTESIAN_POINT('Ctrl Pts',(-34.6308727569695,64.0574429702493,
68.4641091421755));
#217013=CARTESIAN_POINT('Origin',(-33.5526503323277,75.000050506625,72.9851176492631));
#217014=CARTESIAN_POINT('',(-32.5154663289944,64.0574429734778,68.4641091343612));
#217015=CARTESIAN_POINT('',(-32.8170317113719,64.0574429575879,68.464109172821));
#217016=CARTESIAN_POINT('',(-33.5526503323277,64.0574429649796,68.4641091549303));
#217017=CARTESIAN_POINT('Ctrl Pts',(-32.5154663295374,64.0574429734829,
68.464109134349));
#217018=CARTESIAN_POINT('Ctrl Pts',(-32.5181729121248,64.0151117273703,
68.5665672940872));
#217019=CARTESIAN_POINT('Ctrl Pts',(-32.5208831491634,63.9742087564226,
68.6696459656842));
#217020=CARTESIAN_POINT('Ctrl Pts',(-32.5365378811924,63.7466884692259,
69.2673902923806));
#217021=CARTESIAN_POINT('Ctrl Pts',(-32.549578617579,63.5919310328918,69.773504390183));
#217022=CARTESIAN_POINT('Ctrl Pts',(-32.579679363895,63.3144198391241,70.9598095435459));
#217023=CARTESIAN_POINT('Ctrl Pts',(-32.5964491857621,63.2163023712604,
71.6438046500751));
#217024=CARTESIAN_POINT('Ctrl Pts',(-32.631509007593,63.1371761708274,73.0769936812608));
#217025=CARTESIAN_POINT('Ctrl Pts',(-32.6499211125506,63.1665014507285,
73.8237672795319));
#217026=CARTESIAN_POINT('Ctrl Pts',(-32.6868111493593,63.3657179440685,
75.3054641047265));
#217027=CARTESIAN_POINT('Ctrl Pts',(-32.704912584929,63.5358507142816,76.0369737902692));
#217028=CARTESIAN_POINT('Ctrl Pts',(-32.7424335552352,64.0223432761175,
77.4885615806854));
#217029=CARTESIAN_POINT('Ctrl Pts',(-32.7618527034778,64.3434846941796,
78.2032273020582));
#217030=CARTESIAN_POINT('Ctrl Pts',(-32.7902853281375,64.9222311547592,
79.2110793253665));
#217031=CARTESIAN_POINT('Ctrl Pts',(-32.7995280327456,65.1275708077361,
79.5318104969169));
#217032=CARTESIAN_POINT('Ctrl Pts',(-32.8270447993044,65.7808975055577,
80.4514493787191));
#217033=CARTESIAN_POINT('Ctrl Pts',(-32.8454615668622,66.2705269994198,
81.0184419426092));
#217034=CARTESIAN_POINT('Ctrl Pts',(-32.8823126578241,67.3507853437362,
82.0531381278404));
#217035=CARTESIAN_POINT('Ctrl Pts',(-32.9003564060052,67.9391100175202,
82.5183948234867));
#217036=CARTESIAN_POINT('Ctrl Pts',(-32.937754045335,69.2239768130503,83.3499035028791));
#217037=CARTESIAN_POINT('Ctrl Pts',(-32.9571254053667,69.9210371542342,
83.7087100909432));
#217038=CARTESIAN_POINT('Ctrl Pts',(-32.9854965318043,71.0025491703065,
84.1361355379897));
#217039=CARTESIAN_POINT('Ctrl Pts',(-32.9947127388147,71.3632804886609,
84.2589422831795));
#217040=CARTESIAN_POINT('Ctrl Pts',(-33.0229841396186,72.4814353237562,
84.5803407223701));
#217041=CARTESIAN_POINT('Ctrl Pts',(-33.0421997928277,73.2531524578813,
84.7214268900956));
#217042=CARTESIAN_POINT('Ctrl Pts',(-33.079761918093,74.7797659180713,84.8465205931168));
#217043=CARTESIAN_POINT('Ctrl Pts',(-33.097734005379,75.530535854426,84.8366994644064));
#217044=CARTESIAN_POINT('Ctrl Pts',(-33.1350187928347,77.0532501055069,
84.671725927166));
#217045=CARTESIAN_POINT('Ctrl Pts',(-33.1543180996902,77.8209021711521,
84.5105347740466));
#217046=CARTESIAN_POINT('Ctrl Pts',(-33.1825366520723,78.9298947516434,
84.1601488792891));
#217047=CARTESIAN_POINT('Ctrl Pts',(-33.1917039029207,79.2870294189683,
84.0280706730773));
#217048=CARTESIAN_POINT('Ctrl Pts',(-33.2189310943116,80.3222906557612,
83.5873983550509));
#217049=CARTESIAN_POINT('Ctrl Pts',(-33.2371330852797,80.9783622071833,
83.2317939049514));
#217050=CARTESIAN_POINT('Ctrl Pts',(-33.2735865072273,82.2177414112091,
82.4002377705987));
#217051=CARTESIAN_POINT('Ctrl Pts',(-33.2914584980292,82.7979302921072,
81.9256221588403));
#217052=CARTESIAN_POINT('Ctrl Pts',(-33.3285584788554,83.8859759922063,
80.8485587565301));
#217053=CARTESIAN_POINT('Ctrl Pts',(-33.3477954987094,84.3864667553391,
80.2438067442845));
#217054=CARTESIAN_POINT('Ctrl Pts',(-33.375940413939,85.0360006307987,79.2783442208956));
#217055=CARTESIAN_POINT('Ctrl Pts',(-33.385074286717,85.2330777568063,78.9525417070216));
#217056=CARTESIAN_POINT('Ctrl Pts',(-33.4131447479665,85.7869973736596,
77.9284216256599));
#217057=CARTESIAN_POINT('Ctrl Pts',(-33.4322515290968,86.0904964452474,
77.2037041466068));
#217058=CARTESIAN_POINT('Ctrl Pts',(-33.4695410162937,86.5393933668118,
75.7389505218033));
#217059=CARTESIAN_POINT('Ctrl Pts',(-33.487364085763,86.6903275967785,75.0043876740146));
#217060=CARTESIAN_POINT('Ctrl Pts',(-33.5224532382719,86.8465419363969,
73.5626496562674));
#217061=CARTESIAN_POINT('Ctrl Pts',(-33.5396495134092,86.8599451966265,
72.8594514775075));
#217062=CARTESIAN_POINT('Ctrl Pts',(-33.565887804923,86.7843782309649,71.778784663845));
#217063=CARTESIAN_POINT('Ctrl Pts',(-33.5750332280944,86.73940968495,71.3998521049431));
#217064=CARTESIAN_POINT('Ctrl Pts',(-33.6083582939631,86.5100341266544,
70.0343597228469));
#217065=CARTESIAN_POINT('Ctrl Pts',(-33.6329069538302,86.2187538866895,
69.0700985762561));
#217066=CARTESIAN_POINT('Ctrl Pts',(-33.6663560913667,85.6542549138643,
67.8070208840266));
#217067=CARTESIAN_POINT('Ctrl Pts',(-33.6754781943835,85.4824747305474,
67.4675510614521));
#217068=CARTESIAN_POINT('Ctrl Pts',(-33.7059599048676,84.8577672717057,
66.3678727109917));
#217069=CARTESIAN_POINT('Ctrl Pts',(-33.7275935580915,84.3360734543789,
65.6501900329925));
#217070=CARTESIAN_POINT('Ctrl Pts',(-33.7583452584903,83.4819053646819,
64.7156600258739));
#217071=CARTESIAN_POINT('Ctrl Pts',(-33.7675165202791,83.2109939507754,
64.4466049123596));
#217072=CARTESIAN_POINT('Ctrl Pts',(-33.7949968365743,82.3644640973078,
63.6834863394994));
#217073=CARTESIAN_POINT('Ctrl Pts',(-33.8134263206609,81.753910678644,63.231129058799));
#217074=CARTESIAN_POINT('Ctrl Pts',(-33.8502170881033,80.4648078685701,
62.4554617362716));
#217075=CARTESIAN_POINT('Ctrl Pts',(-33.8681357565689,79.7903400725302,
62.1319911260003));
#217076=CARTESIAN_POINT('Ctrl Pts',(-33.9059310831589,78.3266623695969,
61.5932198606606));
#217077=CARTESIAN_POINT('Ctrl Pts',(-33.9259438579676,77.5364847044871,
61.3916640367638));
#217078=CARTESIAN_POINT('Ctrl Pts',(-33.9642674962904,75.9797414048656,
61.1614753622317));
#217079=CARTESIAN_POINT('Ctrl Pts',(-33.9825032037852,75.2186007557229,
61.1229696714893));
#217080=CARTESIAN_POINT('Ctrl Pts',(-34.0173183225318,73.7958921329189,
61.1880475000727));
#217081=CARTESIAN_POINT('Ctrl Pts',(-34.0337048314021,73.1364687683759,
61.2741002085176));
#217082=CARTESIAN_POINT('Ctrl Pts',(-34.0590875503143,72.1166259704857,
61.4955458017704));
#217083=CARTESIAN_POINT('Ctrl Pts',(-34.0682707776253,71.7496017886559,
61.5939376434187));
#217084=CARTESIAN_POINT('Ctrl Pts',(-34.0991154901616,70.5413725129401,
61.9810002693125));
#217085=CARTESIAN_POINT('Ctrl Pts',(-34.1210858444369,69.7280402850099,
62.3466826066562));
#217086=CARTESIAN_POINT('Ctrl Pts',(-34.1615021363173,68.305357747163,63.1899008655832));
#217087=CARTESIAN_POINT('Ctrl Pts',(-34.1799418633589,67.6867226182865,
63.642718364941));
#217088=CARTESIAN_POINT('Ctrl Pts',(-34.2080746303714,66.8322966292095,
64.4053344248759));
#217089=CARTESIAN_POINT('Ctrl Pts',(-34.2174662619616,66.5608694509396,
64.6721695712479));
#217090=CARTESIAN_POINT('Ctrl Pts',(-34.2452567103186,65.7957700539853,
65.5004862202017));
#217091=CARTESIAN_POINT('Ctrl Pts',(-34.2633034374738,65.3418771370186,
66.0961282641829));
#217092=CARTESIAN_POINT('Ctrl Pts',(-34.2975051576547,64.6033398053979,
67.2831729386068));
#217093=CARTESIAN_POINT('Ctrl Pts',(-34.313594856828,64.3057936841928,67.8630033493468));
#217094=CARTESIAN_POINT('Ctrl Pts',(-34.329622639475,64.0574429649796,68.4641091549303));
#217095=CARTESIAN_POINT('Ctrl Pts',(-34.6308727569695,64.0574429702493,
68.4641091421755));
#217096=CARTESIAN_POINT('Ctrl Pts',(-34.6193506401723,64.2398300876496,
68.0226610355699));
#217097=CARTESIAN_POINT('Ctrl Pts',(-34.6079014722085,64.4487809430319,
67.592612006747));
#217098=CARTESIAN_POINT('Ctrl Pts',(-34.5779305593184,65.0568883265986,
66.5125636986354));
#217099=CARTESIAN_POINT('Ctrl Pts',(-34.5592481834225,65.4937954843009,
65.8864181927348));
#217100=CARTESIAN_POINT('Ctrl Pts',(-34.5206541293554,66.5263201696141,
64.6745489590068));
#217101=CARTESIAN_POINT('Ctrl Pts',(-34.5008291531671,67.1298312075825,
64.1009004570284));
#217102=CARTESIAN_POINT('Ctrl Pts',(-34.4623803983329,68.3806459718267,
63.1402533099441));
#217103=CARTESIAN_POINT('Ctrl Pts',(-34.4441274855894,69.0146291071383,
62.7424319607719));
#217104=CARTESIAN_POINT('Ctrl Pts',(-34.4076471356524,70.3649460481053,
62.0635538342914));
#217105=CARTESIAN_POINT('Ctrl Pts',(-34.3891373124602,71.0797066814955,
61.7870979475709));
#217106=CARTESIAN_POINT('Ctrl Pts',(-34.361049697777,72.1841649839589,61.4787284976003));
#217107=CARTESIAN_POINT('Ctrl Pts',(-34.3516820901783,72.5569814841759,
61.3938442480434));
#217108=CARTESIAN_POINT('Ctrl Pts',(-34.3290750741486,73.4737978033568,
61.2313052386171));
#217109=CARTESIAN_POINT('Ctrl Pts',(-34.3158686666609,74.0203569113405,
61.1731848870587));
#217110=CARTESIAN_POINT('Ctrl Pts',(-34.2834734697624,75.3509926791057,
61.1247050893187));
#217111=CARTESIAN_POINT('Ctrl Pts',(-34.2641519258276,76.1339124276137,
61.1738137005168));
#217112=CARTESIAN_POINT('Ctrl Pts',(-34.2320953030451,77.4337737282657,
61.3858563006051));
#217113=CARTESIAN_POINT('Ctrl Pts',(-34.2192063958203,77.9548729189376,
61.5075352063339));
#217114=CARTESIAN_POINT('Ctrl Pts',(-34.1877149343325,79.1903685337703,
61.8857772318997));
#217115=CARTESIAN_POINT('Ctrl Pts',(-34.1689842424272,79.8918123264443,
62.1765664425843));
#217116=CARTESIAN_POINT('Ctrl Pts',(-34.1298563763896,81.3052055716951,
62.9284557091413));
#217117=CARTESIAN_POINT('Ctrl Pts',(-34.1095450191903,82.0053176642944,
63.4029638858185));
#217118=CARTESIAN_POINT('Ctrl Pts',(-34.0794691806072,82.9387301685167,
64.1929868762098));
#217119=CARTESIAN_POINT('Ctrl Pts',(-34.0700949349339,83.2164475033996,
64.4519460101014));
#217120=CARTESIAN_POINT('Ctrl Pts',(-34.0432571153324,83.9776754969654,
65.2334338957908));
#217121=CARTESIAN_POINT('Ctrl Pts',(-34.0260979218382,84.4271560318671,
65.7867821930574));
#217122=CARTESIAN_POINT('Ctrl Pts',(-33.9902141916365,85.2453578099986,
67.0032125914499));
#217123=CARTESIAN_POINT('Ctrl Pts',(-33.971485421099,85.6056659337077,67.6681236254943));
#217124=CARTESIAN_POINT('Ctrl Pts',(-33.9310885358196,86.2493577911117,
69.1860501125651));
#217125=CARTESIAN_POINT('Ctrl Pts',(-33.9094673704172,86.504082512686,70.0462259006034));
#217126=CARTESIAN_POINT('Ctrl Pts',(-33.8779950886871,86.7257156345537,
71.3017110821659));
#217127=CARTESIAN_POINT('Ctrl Pts',(-33.868568337302,86.7737742760017,71.6795491385107));
#217128=CARTESIAN_POINT('Ctrl Pts',(-33.8399302810624,86.8648663597095,
72.840585655259));
#217129=CARTESIAN_POINT('Ctrl Pts',(-33.8210113908767,86.8484111579152,
73.6262878470836));
#217130=CARTESIAN_POINT('Ctrl Pts',(-33.7833517897833,86.6648866794568,
75.1460293063073));
#217131=CARTESIAN_POINT('Ctrl Pts',(-33.7648218705852,86.505394820169,75.877349237697));
#217132=CARTESIAN_POINT('Ctrl Pts',(-33.7373298193746,86.1625685956945,
76.9502656360633));
#217133=CARTESIAN_POINT('Ctrl Pts',(-33.7281000292353,86.029741952418,77.3060105257016));
#217134=CARTESIAN_POINT('Ctrl Pts',(-33.7002071108271,85.5799844689137,
78.3539206464976));
#217135=CARTESIAN_POINT('Ctrl Pts',(-33.6813557955547,85.2132155957022,
79.0225255863));
#217136=CARTESIAN_POINT('Ctrl Pts',(-33.6434139597103,84.3437376786615,
80.298767790114));
#217137=CARTESIAN_POINT('Ctrl Pts',(-33.6245326779248,83.839452988894,80.9008574845915));
#217138=CARTESIAN_POINT('Ctrl Pts',(-33.5869398969987,82.7451952932646,
81.9712951127391));
#217139=CARTESIAN_POINT('Ctrl Pts',(-33.5684366827239,82.1627019208074,
82.4421302754121));
#217140=CARTESIAN_POINT('Ctrl Pts',(-33.5410082140205,81.2235877113892,
83.0643827435643));
#217141=CARTESIAN_POINT('Ctrl Pts',(-33.5318099532505,80.8975668381295,
83.2585446022429));
#217142=CARTESIAN_POINT('Ctrl Pts',(-33.5039667727631,79.8898322658712,
83.7948991041462));
#217143=CARTESIAN_POINT('Ctrl Pts',(-33.4851369145628,79.1838554156084,
84.0872392962354));
#217144=CARTESIAN_POINT('Ctrl Pts',(-33.4473067828707,77.7059728835576,
84.5380790248095));
#217145=CARTESIAN_POINT('Ctrl Pts',(-33.428512547838,76.9364408575445,84.6916683920248));
#217146=CARTESIAN_POINT('Ctrl Pts',(-33.3910778521779,75.413418711161,84.8412617073136));
#217147=CARTESIAN_POINT('Ctrl Pts',(-33.3726448406043,74.6641832111248,
84.8437106768532));
#217148=CARTESIAN_POINT('Ctrl Pts',(-33.3453309286786,73.5421528483799,
84.7409024508214));
#217149=CARTESIAN_POINT('Ctrl Pts',(-33.3361748620735,73.1664518874494,
84.6881881036387));
#217150=CARTESIAN_POINT('Ctrl Pts',(-33.3084116471317,72.0431375258176,
84.4751484011607));
#217151=CARTESIAN_POINT('Ctrl Pts',(-33.2896188289009,71.3078971471474,
84.260406225023));
#217152=CARTESIAN_POINT('Ctrl Pts',(-33.2519364919601,69.8724979234016,
83.6855842913801));
#217153=CARTESIAN_POINT('Ctrl Pts',(-33.2332449359375,69.1770860225593,
83.3236316694871));
#217154=CARTESIAN_POINT('Ctrl Pts',(-33.1959911246191,67.8966503931203,
82.4867395801037));
#217155=CARTESIAN_POINT('Ctrl Pts',(-33.1776373622461,67.3109885926469,
82.0193552701121));
#217156=CARTESIAN_POINT('Ctrl Pts',(-33.1504329688181,66.5004660851745,
81.236250341451));
#217157=CARTESIAN_POINT('Ctrl Pts',(-33.1413090959226,66.2404403303855,
80.9596618765858));
#217158=CARTESIAN_POINT('Ctrl Pts',(-33.1136152048845,65.4970972074817,
80.088659777109));
#217159=CARTESIAN_POINT('Ctrl Pts',(-33.0948548834083,65.0577201636671,
79.4594119749617));
#217160=CARTESIAN_POINT('Ctrl Pts',(-33.05728867943,64.2988546805018,78.1110729050898));
#217161=CARTESIAN_POINT('Ctrl Pts',(-33.0386700448582,63.9839043482313,
77.3936932620491));
#217162=CARTESIAN_POINT('Ctrl Pts',(-33.0015376640987,63.5105141099323,
75.939701665667));
#217163=CARTESIAN_POINT('Ctrl Pts',(-32.9832353344142,63.3469230480352,
75.2085481391496));
#217164=CARTESIAN_POINT('Ctrl Pts',(-32.9560847934007,63.2058233670797,
74.0899686808031));
#217165=CARTESIAN_POINT('Ctrl Pts',(-32.9469683983006,63.1764477566845,
73.7110016473863));
#217166=CARTESIAN_POINT('Ctrl Pts',(-32.9193010016226,63.1429395431197,
72.5654118244789));
#217167=CARTESIAN_POINT('Ctrl Pts',(-32.9005529512463,63.19493406089,71.7991808816112));
#217168=CARTESIAN_POINT('Ctrl Pts',(-32.8630215230713,63.4487474520803,
70.2725148116573));
#217169=CARTESIAN_POINT('Ctrl Pts',(-32.8444150532531,63.65290510332,69.5162398468281));
#217170=CARTESIAN_POINT('Ctrl Pts',(-32.8226405863238,63.9709778019663,
68.6777948318023));
#217171=CARTESIAN_POINT('Ctrl Pts',(-32.8198374151532,64.0134385958395,
68.5706169273563));
#217172=CARTESIAN_POINT('Ctrl Pts',(-32.8170317109009,64.0574429575835,
68.4641091728316));
#217173=CARTESIAN_POINT('Origin',(-64.067537349647,66.6819786653733,69.5522455184007));
#217174=CARTESIAN_POINT('',(-63.567539947994,57.2086765902407,65.6382900020344));
#217175=CARTESIAN_POINT('',(-64.083662457183,57.6856885892254,65.8353741883268));
#217176=CARTESIAN_POINT('',(-64.067537349647,57.6707866405467,65.8292137334027));
#217177=CARTESIAN_POINT('',(-63.5675399484425,56.5589377686512,71.1605188170944));
#217178=CARTESIAN_POINT('Origin',(-63.5675399484425,66.6819786653733,69.5522455184007));
#217179=CARTESIAN_POINT('',(-63.5676514812564,56.5602242475556,71.1683725272604));
#217180=CARTESIAN_POINT('Ctrl Pts',(-63.5675399484425,56.5589377686512,
71.1605188170944));
#217181=CARTESIAN_POINT('Ctrl Pts',(-63.5675771260471,56.5593540010166,
71.1631387308002));
#217182=CARTESIAN_POINT('Ctrl Pts',(-63.5676143036518,56.5597712504601,
71.1657584829202));
#217183=CARTESIAN_POINT('Ctrl Pts',(-63.5676514812564,56.5601895168558,
71.1683780726648));
#217184=CARTESIAN_POINT('',(-64.0597104235077,75.7004037793539,73.2782678282931));
#217185=CARTESIAN_POINT('Ctrl Pts',(-64.0597104235077,75.7004037793539,
73.2782678282931));
#217186=CARTESIAN_POINT('Ctrl Pts',(-64.0451218652925,75.4260421514271,
73.9805348271195));
#217187=CARTESIAN_POINT('Ctrl Pts',(-64.0303356772116,75.0709760863526,
74.649533020937));
#217188=CARTESIAN_POINT('Ctrl Pts',(-64.0010809330892,74.2154841558898,
75.8907572272977));
#217189=CARTESIAN_POINT('Ctrl Pts',(-63.986792125037,73.7171648123145,76.4599526620535));
#217190=CARTESIAN_POINT('Ctrl Pts',(-63.9624118992683,72.784481500054,77.3072526411669));
#217191=CARTESIAN_POINT('Ctrl Pts',(-63.9525239575833,72.383059953084,77.6190644691922));
#217192=CARTESIAN_POINT('Ctrl Pts',(-63.9304794831545,71.4249343683092,
78.2509947667965));
#217193=CARTESIAN_POINT('Ctrl Pts',(-63.9183841578928,70.8568051209136,
78.5508027796505));
#217194=CARTESIAN_POINT('Ctrl Pts',(-63.8936864137596,69.6653511567733,
79.0391399714275));
#217195=CARTESIAN_POINT('Ctrl Pts',(-63.88113511846,69.0430516921984,79.225797709248));
#217196=CARTESIAN_POINT('Ctrl Pts',(-63.856575596689,67.7745311760812,79.4740442805028));
#217197=CARTESIAN_POINT('Ctrl Pts',(-63.8444614159778,67.1311833028043,
79.5360061975211));
#217198=CARTESIAN_POINT('Ctrl Pts',(-63.8259893536362,66.1629495894997,
79.5355609346259));
#217199=CARTESIAN_POINT('Ctrl Pts',(-63.8197844751296,65.8391438196649,
79.5196743975064));
#217200=CARTESIAN_POINT('Ctrl Pts',(-63.8012616880293,64.8742259690284,
79.4251632815208));
#217201=CARTESIAN_POINT('Ctrl Pts',(-63.7892155220506,64.2400125908015,
79.3000344343668));
#217202=CARTESIAN_POINT('Ctrl Pts',(-63.7646866488347,62.9915820917864,
78.9263816821826));
#217203=CARTESIAN_POINT('Ctrl Pts',(-63.7521500622743,62.3801658963736,
78.6758456951229));
#217204=CARTESIAN_POINT('Ctrl Pts',(-63.7273750610242,61.2237694438128,
78.0635093820407));
#217205=CARTESIAN_POINT('Ctrl Pts',(-63.7153700975349,60.680608334847,77.7044378425474));
#217206=CARTESIAN_POINT('Ctrl Pts',(-63.6918930293161,59.7055417620587,
76.9159481552167));
#217207=CARTESIAN_POINT('Ctrl Pts',(-63.6804420652402,59.2696957205743,
76.4937784653886));
#217208=CARTESIAN_POINT('Ctrl Pts',(-63.6520134359374,58.2816372967606,
75.3484072926961));
#217209=CARTESIAN_POINT('Ctrl Pts',(-63.6354546893578,57.784018645059,74.5842894596792));
#217210=CARTESIAN_POINT('Ctrl Pts',(-63.6099369967653,57.1974075459963,
73.353242818012));
#217211=CARTESIAN_POINT('Ctrl Pts',(-63.6013230942664,57.0283706254766,
72.9269478107908));
#217212=CARTESIAN_POINT('Ctrl Pts',(-63.5843894744831,56.7499095059732,
72.0578394046303));
#217213=CARTESIAN_POINT('Ctrl Pts',(-63.5760671502839,56.6402828854334,
71.6159185090166));
#217214=CARTESIAN_POINT('Ctrl Pts',(-63.5676866568907,56.560334274244,71.1683542085754));
#217215=CARTESIAN_POINT('',(-64.5675364832709,60.6333031659922,62.5539864962095));
#217216=CARTESIAN_POINT('Ctrl Pts',(-64.56753648372,60.6339090599576,62.5534304824221));
#217217=CARTESIAN_POINT('Ctrl Pts',(-64.5559053154294,61.0571436471093,
62.1723173071139));
#217218=CARTESIAN_POINT('Ctrl Pts',(-64.5443683788522,61.5150569575824,
61.8309194745767));
#217219=CARTESIAN_POINT('Ctrl Pts',(-64.5208921017017,62.4915898340133,
61.2336544858132));
#217220=CARTESIAN_POINT('Ctrl Pts',(-64.5090141235672,63.0095718878263,
60.9793895503546));
#217221=CARTESIAN_POINT('Ctrl Pts',(-64.4895980530763,63.9049898999737,
60.6390797274406));
#217222=CARTESIAN_POINT('Ctrl Pts',(-64.4819115658727,64.2699923360781,
60.5255089913027));
#217223=CARTESIAN_POINT('Ctrl Pts',(-64.4637503035837,65.1405602157676,
60.3120024769304));
#217224=CARTESIAN_POINT('Ctrl Pts',(-64.4532397072825,65.6498952088197,
60.2307861428219));
#217225=CARTESIAN_POINT('Ctrl Pts',(-64.430296409186,66.7729171495099,60.1455432302508));
#217226=CARTESIAN_POINT('Ctrl Pts',(-64.4181229662858,67.3853348297619,
60.1593209414688));
#217227=CARTESIAN_POINT('Ctrl Pts',(-64.393582019433,68.597723769527,60.3048983612714));
#217228=CARTESIAN_POINT('Ctrl Pts',(-64.3811840907539,69.1958603364025,
60.4364493233302));
#217229=CARTESIAN_POINT('Ctrl Pts',(-64.3626497400445,70.0696915604235,
60.7197347739203));
#217230=CARTESIAN_POINT('Ctrl Pts',(-64.3565059984246,70.3577414698788,
60.8290195178738));
#217231=CARTESIAN_POINT('Ctrl Pts',(-64.3381789619652,71.2014014411427,
61.1971140003167));
#217232=CARTESIAN_POINT('Ctrl Pts',(-64.3259769456409,71.7382300434053,
61.496240439733));
#217233=CARTESIAN_POINT('Ctrl Pts',(-64.3074536245922,72.4961532874526,
62.0201534087073));
#217234=CARTESIAN_POINT('Ctrl Pts',(-64.3012371111907,72.7414996271467,
62.2080285592825));
#217235=CARTESIAN_POINT('Ctrl Pts',(-64.2828087450528,73.4462001197079,
62.8043768560141));
#217236=CARTESIAN_POINT('Ctrl Pts',(-64.2707866092118,73.8757217919052,
63.246099592049));
#217237=CARTESIAN_POINT('Ctrl Pts',(-64.2461815857642,74.6502677961469,
64.2130030553011));
#217238=CARTESIAN_POINT('Ctrl Pts',(-64.2336243377818,74.9927420587892,
64.7383397323999));
#217239=CARTESIAN_POINT('Ctrl Pts',(-64.2090209000687,75.5679416527631,
65.8442881461347));
#217240=CARTESIAN_POINT('Ctrl Pts',(-64.1969313758394,75.8004090675362,
66.4223889606875));
#217241=CARTESIAN_POINT('Ctrl Pts',(-64.1741708575269,76.1254665991152,
67.5280676131162));
#217242=CARTESIAN_POINT('Ctrl Pts',(-64.1635849873021,76.2330829292957,
68.0497086663742));
#217243=CARTESIAN_POINT('Ctrl Pts',(-64.1375350595926,76.3928321250279,
69.3669952652942));
#217244=CARTESIAN_POINT('Ctrl Pts',(-64.1221954863727,76.3904768158639,
70.1665095515024));
#217245=CARTESIAN_POINT('Ctrl Pts',(-64.0986553233582,76.24076456436,71.3543811017856));
#217246=CARTESIAN_POINT('Ctrl Pts',(-64.0907263636134,76.1658342115345,
71.7497160050923));
#217247=CARTESIAN_POINT('Ctrl Pts',(-64.0751169343179,75.9680327516169,
72.5260089561059));
#217248=CARTESIAN_POINT('Ctrl Pts',(-64.0674339216932,75.8456567580364,
72.9064724931336));
#217249=CARTESIAN_POINT('Ctrl Pts',(-64.0597104235077,75.7004037793539,
73.2782678282931));
#217250=CARTESIAN_POINT('',(-64.5675364836265,58.2049936507084,73.253721483482));
#217251=CARTESIAN_POINT('Origin',(-64.5675364832709,66.6819786653733,69.5522455184007));
#217252=CARTESIAN_POINT('Ctrl Pts',(-64.567536483719,58.2048719639793,73.2537614015209));
#217253=CARTESIAN_POINT('Ctrl Pts',(-64.5522519075793,58.0976217008117,
73.0463357077704));
#217254=CARTESIAN_POINT('Ctrl Pts',(-64.5369913991239,57.9980049358009,
72.8343190083415));
#217255=CARTESIAN_POINT('Ctrl Pts',(-64.521750391934,57.9063835252547,72.6182897831504));
#217256=CARTESIAN_POINT('Ctrl Pts',(-64.5065149014817,57.8147952786109,
72.4023387533513));
#217257=CARTESIAN_POINT('Ctrl Pts',(-64.4912988981798,57.731196741534,72.1823783236064));
#217258=CARTESIAN_POINT('Ctrl Pts',(-64.4760978205663,57.6559053051787,
71.9590140988971));
#217259=CARTESIAN_POINT('Ctrl Pts',(-64.4609038574466,57.5806491071448,
71.7357544143683));
#217260=CARTESIAN_POINT('Ctrl Pts',(-64.4457248060474,57.5136923598297,
71.5090943516252));
#217261=CARTESIAN_POINT('Ctrl Pts',(-64.4305561113083,57.4553059750096,
71.279663000753));
#217262=CARTESIAN_POINT('Ctrl Pts',(-64.4153929780724,57.3969409971777,
71.0503157693929));
#217263=CARTESIAN_POINT('Ctrl Pts',(-64.4002401939036,57.3471402054655,
70.8181995207373));
#217264=CARTESIAN_POINT('Ctrl Pts',(-64.38509320875,57.306126469134,70.5839634489254));
#217265=CARTESIAN_POINT('Ctrl Pts',(-64.369953184099,57.265131579868,70.3498350157477));
#217266=CARTESIAN_POINT('Ctrl Pts',(-64.3548189531347,57.23291575996,70.113588953228));
#217267=CARTESIAN_POINT('Ctrl Pts',(-64.3396859720749,57.2096524013204,
69.8758907034779));
#217268=CARTESIAN_POINT('Ctrl Pts',(-64.334832339477,57.2021910957531,69.799653247758));
#217269=CARTESIAN_POINT('Ctrl Pts',(-64.3299788354556,57.1956503379729,
69.7232665234063));
#217270=CARTESIAN_POINT('Ctrl Pts',(-64.3251253100958,57.190034755535,69.6467527948062));
#217271=CARTESIAN_POINT('Ctrl Pts',(-64.3100488689152,57.1725911466023,
69.4090792187472));
#217272=CARTESIAN_POINT('Ctrl Pts',(-64.2949725167308,57.1640786946212,
69.17018381911));
#217273=CARTESIAN_POINT('Ctrl Pts',(-64.2798981906767,57.1646082439414,
68.9307425222474));
#217274=CARTESIAN_POINT('Ctrl Pts',(-64.2648429722312,57.1651371220262,
68.6916047315291));
#217275=CARTESIAN_POINT('Ctrl Pts',(-64.2497897747828,57.1746851526237,
68.4519226836776));
#217276=CARTESIAN_POINT('Ctrl Pts',(-64.2347405281089,57.1933117377907,
68.2123797226737));
#217277=CARTESIAN_POINT('Ctrl Pts',(-64.2197180065408,57.211905245059,67.973262152462));
#217278=CARTESIAN_POINT('Ctrl Pts',(-64.2046994217278,57.2395451263782,
67.7342834363986));
#217279=CARTESIAN_POINT('Ctrl Pts',(-64.1896866931843,57.2762388962374,
67.4961293606103));
#217280=CARTESIAN_POINT('Ctrl Pts',(-64.1746906332512,57.3128919250582,
67.2582397069403));
#217281=CARTESIAN_POINT('Ctrl Pts',(-64.1597004165905,57.3585787693851,
67.0211731258154));
#217282=CARTESIAN_POINT('Ctrl Pts',(-64.1447179563303,57.4132549887369,
66.7856152711256));
#217283=CARTESIAN_POINT('Ctrl Pts',(-64.1297582205198,57.4678482786516,
66.5504146957163));
#217284=CARTESIAN_POINT('Ctrl Pts',(-64.1148062175988,57.5314036925399,
66.3167185364823));
#217285=CARTESIAN_POINT('Ctrl Pts',(-64.0998638520033,57.6038250600662,
66.0852075409195));
#217286=CARTESIAN_POINT('Ctrl Pts',(-64.0944699454783,57.629967780531,66.0016365252333));
#217287=CARTESIAN_POINT('Ctrl Pts',(-64.0890772947654,57.6572653071481,
65.9183502156667));
#217288=CARTESIAN_POINT('Ctrl Pts',(-64.0836859894461,57.6857114539578,
65.8353804738359));
#217289=CARTESIAN_POINT('Origin',(-64.067537349647,66.6819786653733,69.5522455184007));
#217290=CARTESIAN_POINT('',(-63.567539947994,63.4350769493012,59.8300991896842));
#217291=CARTESIAN_POINT('Ctrl Pts',(-64.0833825702184,57.6854166417086,
65.8352994300243));
#217292=CARTESIAN_POINT('Ctrl Pts',(-64.0619309619701,57.7965027550469,
65.510245884164));
#217293=CARTESIAN_POINT('Ctrl Pts',(-64.0405438036779,57.9246131816582,
65.1915387606867));
#217294=CARTESIAN_POINT('Ctrl Pts',(-63.9975780848989,58.2183872019184,
64.5599055048844));
#217295=CARTESIAN_POINT('Ctrl Pts',(-63.9760783705587,58.3845348618842,
64.2483770552226));
#217296=CARTESIAN_POINT('Ctrl Pts',(-63.911488627533,58.938083348327,63.3334815420054));
#217297=CARTESIAN_POINT('Ctrl Pts',(-63.8686493908154,59.3774255368191,
62.7604124769525));
#217298=CARTESIAN_POINT('Ctrl Pts',(-63.8038866668339,60.1101692074064,
61.9886376949769));
#217299=CARTESIAN_POINT('Ctrl Pts',(-63.782504051702,60.3658044398433,61.7463822267538));
#217300=CARTESIAN_POINT('Ctrl Pts',(-63.6782847466954,61.6850726855922,
60.6228146595963));
#217301=CARTESIAN_POINT('Ctrl Pts',(-63.6137547901267,62.7121484755578,
60.1202593968798));
#217302=CARTESIAN_POINT('Ctrl Pts',(-63.567539947994,63.4350769493012,59.8300991896842));
#217303=CARTESIAN_POINT('Origin',(-63.5675399484425,66.6819786653733,69.5522455184007));
#217304=CARTESIAN_POINT('Origin',(-33.9082782203809,71.5694543312839,71.5715374392096));
#217305=CARTESIAN_POINT('',(-48.5675364832709,63.3942272950246,68.1938899513175));
#217306=CARTESIAN_POINT('Origin',(-48.5675364832709,67.9391588995182,70.071657595992));
#217307=CARTESIAN_POINT('',(-38.5675364832709,65.8706796275105,69.2170521170417));
#217308=CARTESIAN_POINT('',(-32.6788877561441,67.3289754150603,69.8195563755258));
#217309=CARTESIAN_POINT('Origin',(-38.5675364832709,70.4156112320045,71.094819761716));
#217310=CARTESIAN_POINT('Origin',(-33.5526503323277,75.000050506625,72.9851176492631));
#217311=CARTESIAN_POINT('Ctrl Pts',(-32.8170317109009,64.0574429575835,
68.4641091728316));
#217312=CARTESIAN_POINT('Ctrl Pts',(-32.8004854807068,64.3169522406309,
67.8359952786588));
#217313=CARTESIAN_POINT('Ctrl Pts',(-32.7839014352646,64.6301458058209,
67.2311874179812));
#217314=CARTESIAN_POINT('Ctrl Pts',(-32.7577872560977,65.2098387558858,
66.3146217715989));
#217315=CARTESIAN_POINT('Ctrl Pts',(-32.7480640102422,65.4434037099935,
65.9840989579143));
#217316=CARTESIAN_POINT('Ctrl Pts',(-32.7284199955665,65.9448748761847,
65.3464375126087));
#217317=CARTESIAN_POINT('Ctrl Pts',(-32.7185111528489,66.2126356336371,
65.0398690125399));
#217318=CARTESIAN_POINT('Ctrl Pts',(-32.7085755548516,66.4956396733205,
64.7476924450699));
#217319=CARTESIAN_POINT('Ctrl Pts',(-32.405898694983,66.4955863073276,64.7477475410809));
#217320=CARTESIAN_POINT('Ctrl Pts',(-32.4157698035306,66.213348129375,65.0391372016825));
#217321=CARTESIAN_POINT('Ctrl Pts',(-32.4256531061311,65.9462722690278,
65.3448398996728));
#217322=CARTESIAN_POINT('Ctrl Pts',(-32.4455076405886,65.4459673773228,
65.9806621814781));
#217323=CARTESIAN_POINT('Ctrl Pts',(-32.4554650299131,65.2128843628617,
66.3102185355673));
#217324=CARTESIAN_POINT('Ctrl Pts',(-32.4822602035662,64.6321241580052,
67.2273710034534));
#217325=CARTESIAN_POINT('Ctrl Pts',(-32.4988212117524,64.3177744264465,
67.8340052739125));
#217326=CARTESIAN_POINT('Ctrl Pts',(-32.5154663295374,64.0574429734829,
68.464109134349));
#217327=CARTESIAN_POINT('Origin',(-27.5423496375577,75.0034579025039,72.9903965241317));
#217328=CARTESIAN_POINT('',(-26.6969350937309,85.8892594304089,68.3402735649357));
#217329=CARTESIAN_POINT('Ctrl Pts',(-27.3723203524304,64.0608503540383,
68.4693880462876));
#217330=CARTESIAN_POINT('Ctrl Pts',(-27.3636083508722,64.1963234386015,
68.1414902321119));
#217331=CARTESIAN_POINT('Ctrl Pts',(-27.3549286023609,64.3465425592909,
67.8196629334019));
#217332=CARTESIAN_POINT('Ctrl Pts',(-27.3282627997169,64.8558294458032,
66.8455262589266));
#217333=CARTESIAN_POINT('Ctrl Pts',(-27.3103235216662,65.2619469917959,
66.2201115322032));
#217334=CARTESIAN_POINT('Ctrl Pts',(-27.2828026355142,65.9604358332311,
65.3386795099181));
#217335=CARTESIAN_POINT('Ctrl Pts',(-27.2734567296289,66.2110529133169,
65.0519687314779));
#217336=CARTESIAN_POINT('Ctrl Pts',(-27.245066551039,67.0174939103502,64.2145128591131));
#217337=CARTESIAN_POINT('Ctrl Pts',(-27.2263832459524,67.6144245613412,
63.7063271980707));
#217338=CARTESIAN_POINT('Ctrl Pts',(-27.1891136084416,68.8734807525916,
62.8333216632523));
#217339=CARTESIAN_POINT('Ctrl Pts',(-27.1706736189322,69.5290999489451,
62.4654641131916));
#217340=CARTESIAN_POINT('Ctrl Pts',(-27.1336442139279,70.930533160993,61.8457387365238));
#217341=CARTESIAN_POINT('Ctrl Pts',(-27.114869717408,71.6755617429044,61.6010497180737));
#217342=CARTESIAN_POINT('Ctrl Pts',(-27.0865099410825,72.8108792767892,
61.3491906253156));
#217343=CARTESIAN_POINT('Ctrl Pts',(-27.0771965350934,73.1862592610267,
61.2847199112335));
#217344=CARTESIAN_POINT('Ctrl Pts',(-27.0489438087402,74.3398690787609,
61.1434269784995));
#217345=CARTESIAN_POINT('Ctrl Pts',(-27.0303330568264,75.1231517273981,
61.1254601993129));
#217346=CARTESIAN_POINT('Ctrl Pts',(-26.9931925794068,76.6492291764433,
61.2416734538101));
#217347=CARTESIAN_POINT('Ctrl Pts',(-26.9748402774108,77.3889104563919,
61.3692657145651));
#217348=CARTESIAN_POINT('Ctrl Pts',(-26.938795595598,78.8323833935359,61.7619711097928));
#217349=CARTESIAN_POINT('Ctrl Pts',(-26.9208878747678,79.5330222579624,
62.0258512466808));
#217350=CARTESIAN_POINT('Ctrl Pts',(-26.8941989674047,80.517902234919,62.507406217329));
#217351=CARTESIAN_POINT('Ctrl Pts',(-26.8856673209247,80.8247494306158,
62.6746441595046));
#217352=CARTESIAN_POINT('Ctrl Pts',(-26.8623096935396,81.6468353161753,
63.1710735303491));
#217353=CARTESIAN_POINT('Ctrl Pts',(-26.8477100682122,82.1446780906913,
63.5269646820952));
#217354=CARTESIAN_POINT('Ctrl Pts',(-26.8106405787466,83.3217913773637,
64.5144381125695));
#217355=CARTESIAN_POINT('Ctrl Pts',(-26.7879383785396,83.9585912266568,
65.1902600866419));
#217356=CARTESIAN_POINT('Ctrl Pts',(-26.7544742250297,84.7850437718349,
66.3035874355147));
#217357=CARTESIAN_POINT('Ctrl Pts',(-26.7434170636367,85.0380446815753,
66.6896103302929));
#217358=CARTESIAN_POINT('Ctrl Pts',(-26.7210007035527,85.5001575689806,
67.4934282204171));
#217359=CARTESIAN_POINT('Ctrl Pts',(-26.7096581122749,85.7083720127467,
67.9108125373918));
#217360=CARTESIAN_POINT('Ctrl Pts',(-26.6982749890421,85.8914418320366,
68.3393768975646));
#217361=CARTESIAN_POINT('',(-26.3969350937309,85.8892594304089,68.3402735649357));
#217362=CARTESIAN_POINT('Origin',(-26.5469350937305,96.4455563604996,63.8278257377735));
#217363=CARTESIAN_POINT('Ctrl Pts',(-26.3955978506944,85.8914161878377,
68.3393168652454));
#217364=CARTESIAN_POINT('Ctrl Pts',(-26.4069424532441,85.7082672857083,
67.9105739168034));
#217365=CARTESIAN_POINT('Ctrl Pts',(-26.4183060567836,85.4999541203497,
67.4930236579193));
#217366=CARTESIAN_POINT('Ctrl Pts',(-26.4411055617826,85.0376098948105,
66.6889042588434));
#217367=CARTESIAN_POINT('Ctrl Pts',(-26.4525195276528,84.784476428515,66.3027447677285));
#217368=CARTESIAN_POINT('Ctrl Pts',(-26.4866843036473,83.9575372610834,
65.1889978992038));
#217369=CARTESIAN_POINT('Ctrl Pts',(-26.5089624396364,83.3203257906962,
64.5129519255814));
#217370=CARTESIAN_POINT('Ctrl Pts',(-26.5468362097196,82.1423355604167,
63.5251696793379));
#217371=CARTESIAN_POINT('Ctrl Pts',(-26.5620028980466,81.6440422855065,
63.1691573508409));
#217372=CARTESIAN_POINT('Ctrl Pts',(-26.5854952714911,80.8212819763206,
62.672682604541));
#217373=CARTESIAN_POINT('Ctrl Pts',(-26.593993736307,80.5142317372497,62.5054706945374));
#217374=CARTESIAN_POINT('Ctrl Pts',(-26.6207668794961,79.5292371216922,
62.0243042286113));
#217375=CARTESIAN_POINT('Ctrl Pts',(-26.6392010159838,78.8287305938289,
61.7607422846029));
#217376=CARTESIAN_POINT('Ctrl Pts',(-26.6761140325086,77.3852967816935,
61.3685194934542));
#217377=CARTESIAN_POINT('Ctrl Pts',(-26.6942100883925,76.645497311909,61.2411459204877));
#217378=CARTESIAN_POINT('Ctrl Pts',(-26.7317170578095,75.1192896074915,
61.125421304211));
#217379=CARTESIAN_POINT('Ctrl Pts',(-26.7511351157852,74.3360036358257,
61.1436434746849));
#217380=CARTESIAN_POINT('Ctrl Pts',(-26.7795748988597,73.1824395779273,
61.2853138249492));
#217381=CARTESIAN_POINT('Ctrl Pts',(-26.7888184636904,72.8070891584055,
61.3499053790692));
#217382=CARTESIAN_POINT('Ctrl Pts',(-26.8171824107733,71.6718535410123,
61.6021333424868));
#217383=CARTESIAN_POINT('Ctrl Pts',(-26.8364701637274,70.9268972234152,
61.8470682365406));
#217384=CARTESIAN_POINT('Ctrl Pts',(-26.874194477388,69.5255826413186,62.4672877684926));
#217385=CARTESIAN_POINT('Ctrl Pts',(-26.8922652752125,68.8700062214772,
62.8354121921109));
#217386=CARTESIAN_POINT('Ctrl Pts',(-26.9297343577378,67.6111740793825,
63.7089150024354));
#217387=CARTESIAN_POINT('Ctrl Pts',(-26.9491080822801,67.0144189406217,
64.2173116018839));
#217388=CARTESIAN_POINT('Ctrl Pts',(-26.977436758888,66.2082763058487,65.0550456594374));
#217389=CARTESIAN_POINT('Ctrl Pts',(-26.986646521672,65.957766563227,65.3418357651074));
#217390=CARTESIAN_POINT('Ctrl Pts',(-27.0139829799489,65.259725731252,66.223332594727));
#217391=CARTESIAN_POINT('Ctrl Pts',(-27.032253517993,64.8539281411214,66.8486943828843));
#217392=CARTESIAN_POINT('Ctrl Pts',(-27.059181657337,64.3455656836393,67.8217560871422));
#217393=CARTESIAN_POINT('Ctrl Pts',(-27.0677840356311,64.1958829423296,
68.1425564084808));
#217394=CARTESIAN_POINT('Ctrl Pts',(-27.0763524848464,64.060850369775,68.4693880081986));
#217395=CARTESIAN_POINT('Origin',(-49.8209604129909,64.4114212759519,68.6141501690631));
#217396=CARTESIAN_POINT('',(-47.4206117411878,75.1063969238644,65.7294283639652));
#217397=CARTESIAN_POINT('',(-47.4206117411893,69.9514311215947,78.2064603659042));
#217398=CARTESIAN_POINT('Ctrl Pts',(-47.4206117411876,75.1063969238639,
65.7294283639681));
#217399=CARTESIAN_POINT('Ctrl Pts',(-47.4072073505217,75.4654570754911,
66.753376001073));
#217400=CARTESIAN_POINT('Ctrl Pts',(-47.3965597695574,75.6742150489095,
67.8789541701247));
#217401=CARTESIAN_POINT('Ctrl Pts',(-47.3802442358666,75.7060386894703,
70.3818352645528));
#217402=CARTESIAN_POINT('Ctrl Pts',(-47.3761425330335,75.4276871521554,
71.7610264219768));
#217403=CARTESIAN_POINT('Ctrl Pts',(-47.3761425330335,74.9319958756762,
72.9607930464209));
#217404=CARTESIAN_POINT('Ctrl Pts',(-47.3761425330335,74.436304599197,74.1605596708651));
#217405=CARTESIAN_POINT('Ctrl Pts',(-47.3802442358666,73.6600106712586,
75.3340227356814));
#217406=CARTESIAN_POINT('Ctrl Pts',(-47.3965597695574,71.8708611554573,
77.0845570904024));
#217407=CARTESIAN_POINT('Ctrl Pts',(-47.4072073505217,70.9285149405077,
77.7345491805734));
#217408=CARTESIAN_POINT('Ctrl Pts',(-47.4206117411876,69.9514311215941,
78.2064603659031));
#217409=CARTESIAN_POINT('',(-40.481003278332,71.6699920780342,78.9164948483173));
#217410=CARTESIAN_POINT('',(-47.4206117411909,69.9514311215961,78.2064603659048));
#217411=CARTESIAN_POINT('',(-40.5852420615047,77.1637469693094,67.7517760446659));
#217412=CARTESIAN_POINT('Ctrl Pts',(-40.4810032783342,71.6699920780332,
78.9164948483157));
#217413=CARTESIAN_POINT('Ctrl Pts',(-40.5698846854173,72.6193246413771,
78.4352946931042));
#217414=CARTESIAN_POINT('Ctrl Pts',(-40.6457193000517,73.5311457149865,
77.7824385307885));
#217415=CARTESIAN_POINT('Ctrl Pts',(-40.7675094263889,75.2904244826386,
76.022759538046));
#217416=CARTESIAN_POINT('Ctrl Pts',(-40.8007888323695,76.0625615407368,
74.838403107781));
#217417=CARTESIAN_POINT('Ctrl Pts',(-40.8007888323695,76.5603508765695,
73.6335583596984));
#217418=CARTESIAN_POINT('Ctrl Pts',(-40.8007888323695,77.056970474425,72.4315448346997));
#217419=CARTESIAN_POINT('Ctrl Pts',(-40.7676642501064,77.3459151424127,
71.0508555808169));
#217420=CARTESIAN_POINT('Ctrl Pts',(-40.668740252843,77.3442754006263,69.0254326994105));
#217421=CARTESIAN_POINT('Ctrl Pts',(-40.6299225890052,77.2825638962586,
68.3789914813538));
#217422=CARTESIAN_POINT('Ctrl Pts',(-40.5852420615047,77.1637469693094,
67.7517760446659));
#217423=CARTESIAN_POINT('',(-40.481003278332,76.8249578803026,66.4394628463787));
#217424=CARTESIAN_POINT('Ctrl Pts',(-40.5852420615047,77.1637469693094,
67.7517760446659));
#217425=CARTESIAN_POINT('Ctrl Pts',(-40.5532232597647,77.0786008029555,
67.3023031346758));
#217426=CARTESIAN_POINT('Ctrl Pts',(-40.5182082030455,76.9642837773573,
66.8626329204887));
#217427=CARTESIAN_POINT('Ctrl Pts',(-40.4810032783489,76.824957880356,66.4394628465471));
#217428=CARTESIAN_POINT('',(-47.4206117411909,75.1063969238651,65.7294283639647));
#217429=CARTESIAN_POINT('Origin',(-64.4265543961493,66.6762871555627,69.5530424137804));
#217430=CARTESIAN_POINT('',(-64.5675364832712,59.0462179431737,64.6166308207574));
#217431=CARTESIAN_POINT('Origin',(-64.5675364832709,66.6762871555627,69.5530424137804));
#217432=CARTESIAN_POINT('',(-63.7081759237673,75.0753993185238,73.0230612142441));
#217433=CARTESIAN_POINT('Ctrl Pts',(-64.5675364832717,59.046217943174,64.6166308207575));
#217434=CARTESIAN_POINT('Ctrl Pts',(-64.5460054318702,59.4140720830844,
64.0480492722603));
#217435=CARTESIAN_POINT('Ctrl Pts',(-64.5242151510805,59.844353182852,63.5223301109439));
#217436=CARTESIAN_POINT('Ctrl Pts',(-64.4802433842163,60.8230886227947,
62.5671481746462));
#217437=CARTESIAN_POINT('Ctrl Pts',(-64.4585326795741,61.3704534354962,
62.1428615462339));
#217438=CARTESIAN_POINT('Ctrl Pts',(-64.4216367999338,62.3527328725573,
61.5465778287498));
#217439=CARTESIAN_POINT('Ctrl Pts',(-64.4067804331069,62.7623749275686,
61.3385500692314));
#217440=CARTESIAN_POINT('Ctrl Pts',(-64.3730365308062,63.7305523780891,
60.9358123869345));
#217441=CARTESIAN_POINT('Ctrl Pts',(-64.3544190590795,64.2958995002949,
60.7628340472615));
#217442=CARTESIAN_POINT('Ctrl Pts',(-64.3166439831112,65.4503787733972,
60.529236790111));
#217443=CARTESIAN_POINT('Ctrl Pts',(-64.2975574490637,66.0367054215919,
60.4688337160353));
#217444=CARTESIAN_POINT('Ctrl Pts',(-64.2597495591603,67.2149662863187,
60.4621504002003));
#217445=CARTESIAN_POINT('Ctrl Pts',(-64.241099252248,67.8041172201248,60.5163118771831));
#217446=CARTESIAN_POINT('Ctrl Pts',(-64.2031978910308,68.9629880021758,
60.7380099725469));
#217447=CARTESIAN_POINT('Ctrl Pts',(-64.184061183931,69.5299767860601,60.9049062666254));
#217448=CARTESIAN_POINT('Ctrl Pts',(-64.1557944571638,70.3503120297366,
61.2359124218975));
#217449=CARTESIAN_POINT('Ctrl Pts',(-64.1464291167281,70.6182984868461,
61.3595292794476));
#217450=CARTESIAN_POINT('Ctrl Pts',(-64.1276217352215,71.1414282045385,
61.6324545404921));
#217451=CARTESIAN_POINT('Ctrl Pts',(-64.1181904779768,71.3962528025367,
61.781612700772));
#217452=CARTESIAN_POINT('Ctrl Pts',(-64.0897741094686,72.136961432337,62.2650675446127));
#217453=CARTESIAN_POINT('Ctrl Pts',(-64.0707214808187,72.5980472818162,
62.6344941894086));
#217454=CARTESIAN_POINT('Ctrl Pts',(-64.0332160558767,73.4422542529727,
63.4575197792183));
#217455=CARTESIAN_POINT('Ctrl Pts',(-64.014559870328,73.8233529525379,63.909182428562));
#217456=CARTESIAN_POINT('Ctrl Pts',(-63.9767300455895,74.4926660386445,
64.8799364829341));
#217457=CARTESIAN_POINT('Ctrl Pts',(-63.9578042896901,74.7792988665418,
65.3967325233348));
#217458=CARTESIAN_POINT('Ctrl Pts',(-63.9297910614553,75.1312269161829,
66.2083219024603));
#217459=CARTESIAN_POINT('Ctrl Pts',(-63.9204656552382,75.2353509543835,
66.4845593731602));
#217460=CARTESIAN_POINT('Ctrl Pts',(-63.8941532883585,75.4893852620833,
67.2727750529987));
#217461=CARTESIAN_POINT('Ctrl Pts',(-63.877060576949,75.6079511899779,67.7935855420381));
#217462=CARTESIAN_POINT('Ctrl Pts',(-63.8344751232092,75.7886203399767,
69.1147594772785));
#217463=CARTESIAN_POINT('Ctrl Pts',(-63.8095863687707,75.7918272774603,
69.918609411374));
#217464=CARTESIAN_POINT('Ctrl Pts',(-63.7713711901292,75.6386878668021,
71.1091500668137));
#217465=CARTESIAN_POINT('Ctrl Pts',(-63.7585739829325,75.5615242742643,
71.5020572684633));
#217466=CARTESIAN_POINT('Ctrl Pts',(-63.7332377069494,75.3560332950464,
72.2747690093564));
#217467=CARTESIAN_POINT('Ctrl Pts',(-63.7207474086351,75.2279788898429,
72.6537453669887));
#217468=CARTESIAN_POINT('Ctrl Pts',(-63.7081759237673,75.0753993185238,
73.0230612142441));
#217469=CARTESIAN_POINT('Ctrl Pts',(-63.7081759237673,75.0753993185238,
73.0230612142441));
#217470=CARTESIAN_POINT('Ctrl Pts',(-63.6875161657482,74.8246527237304,
73.6299884083759));
#217471=CARTESIAN_POINT('Ctrl Pts',(-63.6666330962714,74.5088568775848,
74.2079528890887));
#217472=CARTESIAN_POINT('Ctrl Pts',(-63.625033817803,73.7584474523042,75.285397747626));
#217473=CARTESIAN_POINT('Ctrl Pts',(-63.604712906491,73.3260967966463,75.7817602801978));
#217474=CARTESIAN_POINT('Ctrl Pts',(-63.5702347770151,72.5230362672801,
76.5238902708135));
#217475=CARTESIAN_POINT('Ctrl Pts',(-63.5563499250237,72.1810151983127,
76.7970165522756));
#217476=CARTESIAN_POINT('Ctrl Pts',(-63.5238782363532,71.3348165170477,
77.3781042268528));
#217477=CARTESIAN_POINT('Ctrl Pts',(-63.5056266428151,70.8176553251907,
77.6636872419475));
#217478=CARTESIAN_POINT('Ctrl Pts',(-63.4686546174704,69.7360997838413,
78.1303410844429));
#217479=CARTESIAN_POINT('Ctrl Pts',(-63.4499671432274,69.1743365019085,
78.3104533209256));
#217480=CARTESIAN_POINT('Ctrl Pts',(-63.412843637122,68.02296300716,78.5597118792829));
#217481=CARTESIAN_POINT('Ctrl Pts',(-63.3946215167477,67.4360343720838,
78.6280860916995));
#217482=CARTESIAN_POINT('Ctrl Pts',(-63.3575823140898,66.2577744649439,
78.6501758674783));
#217483=CARTESIAN_POINT('Ctrl Pts',(-63.3388446223193,65.6692399052088,
78.6039452830318));
#217484=CARTESIAN_POINT('Ctrl Pts',(-63.3018702281337,64.5101588768287,
78.3983799325527));
#217485=CARTESIAN_POINT('Ctrl Pts',(-63.283646501263,63.9423247648397,78.2396736254702));
#217486=CARTESIAN_POINT('Ctrl Pts',(-63.2465196644465,62.844006377131,77.814240414913));
#217487=CARTESIAN_POINT('Ctrl Pts',(-63.2277373367691,62.3162201136205,
77.5482653071633));
#217488=CARTESIAN_POINT('Ctrl Pts',(-63.1907483518579,61.3200174392572,
76.9180689523048));
#217489=CARTESIAN_POINT('Ctrl Pts',(-63.1724068011774,60.8539177174493,
76.5554173534265));
#217490=CARTESIAN_POINT('Ctrl Pts',(-63.1350988645248,59.9983322733126,
75.7448462794558));
#217491=CARTESIAN_POINT('Ctrl Pts',(-63.1163171878295,59.6109016499769,
75.2988106682674));
#217492=CARTESIAN_POINT('Ctrl Pts',(-63.0840698114675,59.0161042143516,
74.462098201395));
#217493=CARTESIAN_POINT('Ctrl Pts',(-63.070383528129,58.7888527537334,74.0879744284649));
#217494=CARTESIAN_POINT('Ctrl Pts',(-63.03575802426,58.2899042873179,73.1147421819726));
#217495=CARTESIAN_POINT('Ctrl Pts',(-63.0147220449659,58.0545822896112,
72.499792039988));
#217496=CARTESIAN_POINT('Ctrl Pts',(-62.9836482387311,57.8040493638457,
71.5473602390957));
#217497=CARTESIAN_POINT('Ctrl Pts',(-62.973330254332,57.7377964778962,71.2255528877246));
#217498=CARTESIAN_POINT('Ctrl Pts',(-62.9525789218377,57.640511421009,70.5768646016961));
#217499=CARTESIAN_POINT('Ctrl Pts',(-62.9421606938526,57.6094772131815,
70.2504729419999));
#217500=CARTESIAN_POINT('Ctrl Pts',(-62.931689741507,57.5961353792733,69.9231225687745));
#217501=CARTESIAN_POINT('',(-63.5151079737584,75.0753363416539,73.023213644598));
#217502=CARTESIAN_POINT('Ctrl Pts',(-63.5151079737584,75.0753363416539,
73.023213644598));
#217503=CARTESIAN_POINT('Ctrl Pts',(-63.4920115368903,74.8003777464773,
73.6887112847482));
#217504=CARTESIAN_POINT('Ctrl Pts',(-63.4695346041823,74.4472985330117,
74.3191708931087));
#217505=CARTESIAN_POINT('Ctrl Pts',(-63.423566941987,73.6004910487312,75.4824790007821));
#217506=CARTESIAN_POINT('Ctrl Pts',(-63.4000847322133,73.1099911278997,
76.0113920820928));
#217507=CARTESIAN_POINT('Ctrl Pts',(-63.361777030342,72.1979722538408,76.7866989681039));
#217508=CARTESIAN_POINT('Ctrl Pts',(-63.3466926852378,71.8097504735447,
77.0671855931678));
#217509=CARTESIAN_POINT('Ctrl Pts',(-63.2938297827708,70.3901047296146,
77.9312832124918));
#217510=CARTESIAN_POINT('Ctrl Pts',(-63.2553240369309,69.2683698962628,
78.3432902940439));
#217511=CARTESIAN_POINT('Ctrl Pts',(-63.1802061532443,66.9313631514609,
78.7137875751332));
#217512=CARTESIAN_POINT('Ctrl Pts',(-63.1416991694266,65.7385098139196,
78.669231390451));
#217513=CARTESIAN_POINT('Ctrl Pts',(-63.0854654839921,64.0155033228014,
78.2623486117566));
#217514=CARTESIAN_POINT('Ctrl Pts',(-63.0668904991214,63.4577723005613,
78.0720177871324));
#217515=CARTESIAN_POINT('Ctrl Pts',(-63.0288042469598,62.3857775646909,
77.5857743798567));
#217516=CARTESIAN_POINT('Ctrl Pts',(-63.0097643437471,61.8741393887536,
77.2907842916304));
#217517=CARTESIAN_POINT('Ctrl Pts',(-62.9722947176107,60.9161297538726,
76.6065876086381));
#217518=CARTESIAN_POINT('Ctrl Pts',(-62.9539264956367,60.4718989600415,
76.2191865236179));
#217519=CARTESIAN_POINT('Ctrl Pts',(-62.91777620211,59.6982676713801,75.3997319054868));
#217520=CARTESIAN_POINT('Ctrl Pts',(-62.9002893758449,59.3639057394616,
74.9757373538693));
#217521=CARTESIAN_POINT('Ctrl Pts',(-62.8569675334043,58.6228572569014,
73.8418303929263));
#217522=CARTESIAN_POINT('Ctrl Pts',(-62.8317663795232,58.2705836499956,
73.1020680896929));
#217523=CARTESIAN_POINT('Ctrl Pts',(-62.7795181749645,57.772579724387,71.5473692252264));
#217524=CARTESIAN_POINT('Ctrl Pts',(-62.7533222274278,57.629410894498,70.7393858054451));
#217525=CARTESIAN_POINT('Ctrl Pts',(-62.7276560748581,57.5961385652529,
69.9232007305414));
#217526=CARTESIAN_POINT('Ctrl Pts',(-64.4174334691588,58.2772202579663,
66.0829140514177));
#217527=CARTESIAN_POINT('Ctrl Pts',(-64.4028363489011,58.4518252279933,
65.6603017815621));
#217528=CARTESIAN_POINT('Ctrl Pts',(-64.388254068226,58.6580800871412,65.2514650584679));
#217529=CARTESIAN_POINT('Ctrl Pts',(-64.3594594276788,59.1299016586449,
64.4691031862401));
#217530=CARTESIAN_POINT('Ctrl Pts',(-64.3452859445577,59.3946760999142,
64.0966228430422));
#217531=CARTESIAN_POINT('Ctrl Pts',(-64.3026020263834,60.268874083405,63.0444148664755));
#217532=CARTESIAN_POINT('Ctrl Pts',(-64.2733419665553,60.9536431133377,
62.4348608785046));
#217533=CARTESIAN_POINT('Ctrl Pts',(-64.2264359972265,62.2072784339748,
61.6185901131439));
#217534=CARTESIAN_POINT('Ctrl Pts',(-64.2084843858883,62.72657227493,61.347720171344));
#217535=CARTESIAN_POINT('Ctrl Pts',(-64.1715858497388,63.8140295268703,
60.9078005015644));
#217536=CARTESIAN_POINT('Ctrl Pts',(-64.152733349663,64.3799657775133,60.7405714862318));
#217537=CARTESIAN_POINT('Ctrl Pts',(-64.1156388352873,65.5353959314313,
60.5181036515844));
#217538=CARTESIAN_POINT('Ctrl Pts',(-64.0974824103457,66.122123731388,60.4632319430865));
#217539=CARTESIAN_POINT('Ctrl Pts',(-64.060817865302,67.2978133386995,60.467597049163));
#217540=CARTESIAN_POINT('Ctrl Pts',(-64.0420536590333,67.8839943754661,
60.5268009521494));
#217541=CARTESIAN_POINT('Ctrl Pts',(-64.0046823532411,69.0393038763928,
60.7581054577239));
#217542=CARTESIAN_POINT('Ctrl Pts',(-63.9862706923076,69.605607286876,60.930174162333));
#217543=CARTESIAN_POINT('Ctrl Pts',(-63.9309385666082,71.2472767084625,
61.6095373623021));
#217544=CARTESIAN_POINT('Ctrl Pts',(-63.8929715723796,72.2440018990052,
62.2733606589597));
#217545=CARTESIAN_POINT('Ctrl Pts',(-63.8466555645126,73.2940183642383,
63.3177684313763));
#217546=CARTESIAN_POINT('Ctrl Pts',(-63.8374744635571,73.4927744769004,
63.5356918745553));
#217547=CARTESIAN_POINT('Ctrl Pts',(-63.8096802469964,74.0566727572609,
64.2178346791088));
#217548=CARTESIAN_POINT('Ctrl Pts',(-63.7906820867554,74.3875346091592,
64.7083363402621));
#217549=CARTESIAN_POINT('Ctrl Pts',(-63.7624534805635,74.8089437801989,
65.4869523152072));
#217550=CARTESIAN_POINT('Ctrl Pts',(-63.7531027711834,74.9366784331414,
65.7531568340785));
#217551=CARTESIAN_POINT('Ctrl Pts',(-63.7252693288848,75.2794825367097,
66.5669372241555));
#217552=CARTESIAN_POINT('Ctrl Pts',(-63.7070369345556,75.4546067534806,
67.1296363690236));
#217553=CARTESIAN_POINT('Ctrl Pts',(-63.6595558906483,75.7569768036545,
68.585706998936));
#217554=CARTESIAN_POINT('Ctrl Pts',(-63.6306895773755,75.8081294161607,
69.4884288883275));
#217555=CARTESIAN_POINT('Ctrl Pts',(-63.5879995871343,75.6843268963693,
70.8368980257031));
#217556=CARTESIAN_POINT('Ctrl Pts',(-63.5736937694455,75.6087802633196,
71.2861407676666));
#217557=CARTESIAN_POINT('Ctrl Pts',(-63.5444428965403,75.3910183266301,
72.1696495296368));
#217558=CARTESIAN_POINT('Ctrl Pts',(-63.5297035283193,75.2490935839844,
72.602659289293));
#217559=CARTESIAN_POINT('Ctrl Pts',(-63.5151079737584,75.0753363416539,
73.023213644598));
#217560=CARTESIAN_POINT('Origin',(-61.5936228798467,66.6770802411476,69.5524554490054));
#217561=CARTESIAN_POINT('',(-56.4535514884218,75.0783661981676,73.0234382919152));
#217562=CARTESIAN_POINT('Ctrl Pts',(-57.3654750286596,58.2758162995991,
66.081419319572));
#217563=CARTESIAN_POINT('Ctrl Pts',(-57.3600114213503,58.3418432452923,
65.9216083071428));
#217564=CARTESIAN_POINT('Ctrl Pts',(-57.354538030702,58.4124498587974,65.7636334960766));
#217565=CARTESIAN_POINT('Ctrl Pts',(-57.320335958553,58.8799319911198,64.7931181034278));
#217566=CARTESIAN_POINT('Ctrl Pts',(-57.2910632069123,59.3916444208721,
64.0416260517858));
#217567=CARTESIAN_POINT('Ctrl Pts',(-57.2531441869721,60.2044635996514,
63.163393185142));
#217568=CARTESIAN_POINT('Ctrl Pts',(-57.2438960971557,60.4133869689274,
62.9584408187008));
#217569=CARTESIAN_POINT('Ctrl Pts',(-57.2029172707919,61.3752732899755,
62.1018723117282));
#217570=CARTESIAN_POINT('Ctrl Pts',(-57.1706881268413,62.2224486874346,
61.5664300509027));
#217571=CARTESIAN_POINT('Ctrl Pts',(-57.1015161888563,64.2301218056132,
60.7182282354967));
#217572=CARTESIAN_POINT('Ctrl Pts',(-57.0632515782325,65.4003685532868,
60.4749454867403));
#217573=CARTESIAN_POINT('Ctrl Pts',(-57.0072783845977,67.1622342804553,
60.4569626146788));
#217574=CARTESIAN_POINT('Ctrl Pts',(-56.9889189922805,67.7394058978863,
60.5061953742382));
#217575=CARTESIAN_POINT('Ctrl Pts',(-56.9519861589916,68.8662837545505,
60.7117096933882));
#217576=CARTESIAN_POINT('Ctrl Pts',(-56.9336163160537,69.4138340516044,
60.8655922982073));
#217577=CARTESIAN_POINT('Ctrl Pts',(-56.8975593860576,70.4722303191574,
61.273130373858));
#217578=CARTESIAN_POINT('Ctrl Pts',(-56.8796493552864,70.9808100854609,
61.5257316508818));
#217579=CARTESIAN_POINT('Ctrl Pts',(-56.8444604524034,71.9121132112754,
62.1023983358425));
#217580=CARTESIAN_POINT('Ctrl Pts',(-56.8273003940205,72.3365280341286,
62.4194634437235));
#217581=CARTESIAN_POINT('Ctrl Pts',(-56.7937435649933,73.120819616518,63.1196740244442));
#217582=CARTESIAN_POINT('Ctrl Pts',(-56.7773285095329,73.4799297330221,
63.5007037465333));
#217583=CARTESIAN_POINT('Ctrl Pts',(-56.7445659828364,74.1180595577877,
64.3068205305523));
#217584=CARTESIAN_POINT('Ctrl Pts',(-56.7282914253951,74.3982024995525,
64.7286475597634));
#217585=CARTESIAN_POINT('Ctrl Pts',(-56.6928818440938,74.9290291194141,
65.693724022836));
#217586=CARTESIAN_POINT('Ctrl Pts',(-56.6741711027392,75.1641923499117,
66.2428631704159));
#217587=CARTESIAN_POINT('Ctrl Pts',(-56.6222397366015,75.6589306397739,
67.8069613270961));
#217588=CARTESIAN_POINT('Ctrl Pts',(-56.5886376242235,75.7999415281365,
68.8497498836176));
#217589=CARTESIAN_POINT('Ctrl Pts',(-56.5218871145513,75.720361681532,70.9690038904761));
#217590=CARTESIAN_POINT('Ctrl Pts',(-56.4874035662131,75.4893105070773,
72.028774587768));
#217591=CARTESIAN_POINT('Ctrl Pts',(-56.4535514884218,75.0783661981675,
73.0234382919155));
#217592=CARTESIAN_POINT('Ctrl Pts',(-56.4535514884218,75.0783661981676,
73.0234382919152));
#217593=CARTESIAN_POINT('Ctrl Pts',(-56.4350025485805,74.8531929810001,
73.5684552720914));
#217594=CARTESIAN_POINT('Ctrl Pts',(-56.4166167441613,74.5755185238252,
74.0902687254798));
#217595=CARTESIAN_POINT('Ctrl Pts',(-56.379165442425,73.9223966155769,75.0736683009857));
#217596=CARTESIAN_POINT('Ctrl Pts',(-56.3602283265256,73.5483169666455,
75.532799775141));
#217597=CARTESIAN_POINT('Ctrl Pts',(-56.329596782838,72.861721139502,76.2253320190393));
#217598=CARTESIAN_POINT('Ctrl Pts',(-56.317634398701,72.574065311345,76.4808487169403));
#217599=CARTESIAN_POINT('Ctrl Pts',(-56.2894402152713,71.8658413552301,
77.0337944793754));
#217600=CARTESIAN_POINT('Ctrl Pts',(-56.2731540034383,71.4344701947586,
77.3152453931667));
#217601=CARTESIAN_POINT('Ctrl Pts',(-56.219130437151,69.9379628269114,78.119840148702));
#217602=CARTESIAN_POINT('Ctrl Pts',(-56.1828647639803,68.794575824452,78.4715164095075));
#217603=CARTESIAN_POINT('Ctrl Pts',(-56.1075989870263,66.4376023995509,
78.7162692581898));
#217604=CARTESIAN_POINT('Ctrl Pts',(-56.0713507169347,65.2466035010035,
78.6070995097047));
#217605=CARTESIAN_POINT('Ctrl Pts',(-56.0244312016594,63.8295822101941,
78.1899669390205));
#217606=CARTESIAN_POINT('Ctrl Pts',(-56.0151271426989,63.5531910934736,
78.0938936901133));
#217607=CARTESIAN_POINT('Ctrl Pts',(-55.9899598033859,62.8127982775836,
77.79577991316));
#217608=CARTESIAN_POINT('Ctrl Pts',(-55.9743076255857,62.3602629387578,
77.5680756017296));
#217609=CARTESIAN_POINT('Ctrl Pts',(-55.9325391958517,61.2253033703755,
76.8728703666199));
#217610=CARTESIAN_POINT('Ctrl Pts',(-55.9060931859003,60.5835592141638,
76.3479941800254));
#217611=CARTESIAN_POINT('Ctrl Pts',(-55.8672462318577,59.7404020141169,
75.4416090443032));
#217612=CARTESIAN_POINT('Ctrl Pts',(-55.8543960477821,59.4802236078311,
75.1206589282082));
#217613=CARTESIAN_POINT('Ctrl Pts',(-55.8280947723416,58.9994034129875,
74.437273983811));
#217614=CARTESIAN_POINT('Ctrl Pts',(-55.8146661895923,58.7804893176157,
74.0748461126787));
#217615=CARTESIAN_POINT('Ctrl Pts',(-55.8011708396429,58.5876049474126,
73.6985038205814));
#217616=CARTESIAN_POINT('',(-56.2580209956237,75.0782830932473,73.0236394350927));
#217617=CARTESIAN_POINT('Ctrl Pts',(-56.2580209956237,75.0782830932473,
73.0236394350927));
#217618=CARTESIAN_POINT('Ctrl Pts',(-56.2443250754476,74.9153795836255,
73.4179099304444));
#217619=CARTESIAN_POINT('Ctrl Pts',(-56.2305642181659,74.7249216441682,
73.8002275282812));
#217620=CARTESIAN_POINT('Ctrl Pts',(-56.2033211069302,74.2926394472272,
74.5337242263198));
#217621=CARTESIAN_POINT('Ctrl Pts',(-56.1898709563397,74.0515679752653,
74.8841262966464));
#217622=CARTESIAN_POINT('Ctrl Pts',(-56.1512855608215,73.2926281453491,
75.8368058676945));
#217623=CARTESIAN_POINT('Ctrl Pts',(-56.1256639711522,72.7192902604295,
76.3898681292527));
#217624=CARTESIAN_POINT('Ctrl Pts',(-56.0833810803595,71.6592287485016,
77.1736969095174));
#217625=CARTESIAN_POINT('Ctrl Pts',(-56.0667865829977,71.2106984557556,
77.4487477683132));
#217626=CARTESIAN_POINT('Ctrl Pts',(-56.0320548232101,70.2335982860813,
77.9370958618639));
#217627=CARTESIAN_POINT('Ctrl Pts',(-56.0136903834561,69.7036449059816,
78.1426188139804));
#217628=CARTESIAN_POINT('Ctrl Pts',(-55.9724037787782,68.4715783064651,
78.4921548134416));
#217629=CARTESIAN_POINT('Ctrl Pts',(-55.949910350296,67.7645969923614,78.6053971315291));
#217630=CARTESIAN_POINT('Ctrl Pts',(-55.9038224877719,66.32063622386,78.6649527140372));
#217631=CARTESIAN_POINT('Ctrl Pts',(-55.8800043454388,65.5886261276757,
78.6067319429835));
#217632=CARTESIAN_POINT('Ctrl Pts',(-55.8418580524031,64.4193801977491,
78.369766115404));
#217633=CARTESIAN_POINT('Ctrl Pts',(-55.8272928052753,63.9748501154927,
78.2438378961159));
#217634=CARTESIAN_POINT('Ctrl Pts',(-55.7936110388137,62.9815107330797,
77.8788240150706));
#217635=CARTESIAN_POINT('Ctrl Pts',(-55.7742461928927,62.4428615051065,
77.618249109084));
#217636=CARTESIAN_POINT('Ctrl Pts',(-55.7285410136336,61.2288299480985,
76.8756090000899));
#217637=CARTESIAN_POINT('Ctrl Pts',(-55.702797084058,60.5860673776397,76.3503647630496));
#217638=CARTESIAN_POINT('Ctrl Pts',(-55.6629912962454,59.7417569897272,
75.4432276991319));
#217639=CARTESIAN_POINT('Ctrl Pts',(-55.6496589375082,59.4813000808383,
75.1220745554703));
#217640=CARTESIAN_POINT('Ctrl Pts',(-55.6228882380845,58.9999281637497,
74.4381366140573));
#217641=CARTESIAN_POINT('Ctrl Pts',(-55.6094895732801,58.7807521867564,
74.0753471720821));
#217642=CARTESIAN_POINT('Ctrl Pts',(-55.5961206596756,58.5876577945761,
73.6986069305967));
#217643=CARTESIAN_POINT('Ctrl Pts',(-56.2580209956237,75.0782830932472,
73.0236394350929));
#217644=CARTESIAN_POINT('Ctrl Pts',(-56.2925645228312,75.4891544873887,
72.0292196802937));
#217645=CARTESIAN_POINT('Ctrl Pts',(-56.3259262120769,75.720220574439,70.9697133303432));
#217646=CARTESIAN_POINT('Ctrl Pts',(-56.3939371624248,75.7999941374542,
68.8513038344539));
#217647=CARTESIAN_POINT('Ctrl Pts',(-56.4262220314782,75.6592736023998,
67.8090700677666));
#217648=CARTESIAN_POINT('Ctrl Pts',(-56.4785201578563,75.1651878195993,
66.2454276235155));
#217649=CARTESIAN_POINT('Ctrl Pts',(-56.4975993377663,74.9302102895212,
65.6962571767317));
#217650=CARTESIAN_POINT('Ctrl Pts',(-56.5321607618762,74.4002121154711,
64.7319763436369));
#217651=CARTESIAN_POINT('Ctrl Pts',(-56.5479173463761,74.1208645287935,
64.3109042611982));
#217652=CARTESIAN_POINT('Ctrl Pts',(-56.5798968217344,73.494700938003,63.5188286320515));
#217653=CARTESIAN_POINT('Ctrl Pts',(-56.5960655252397,73.1488683908934,
63.1492876181003));
#217654=CARTESIAN_POINT('Ctrl Pts',(-56.6291348647592,72.3745662518574,
62.4490620080192));
#217655=CARTESIAN_POINT('Ctrl Pts',(-56.6458198189785,71.9436713366265,
62.1239585426187));
#217656=CARTESIAN_POINT('Ctrl Pts',(-56.68057172786,71.0045022454338,61.5383786275759));
#217657=CARTESIAN_POINT('Ctrl Pts',(-56.698616759336,70.4953636692314,61.2836762939568));
#217658=CARTESIAN_POINT('Ctrl Pts',(-56.7346963800063,69.4361721782398,
60.8726227487683));
#217659=CARTESIAN_POINT('Ctrl Pts',(-56.7523394831835,68.8884388797823,
60.7171863104021));
#217660=CARTESIAN_POINT('Ctrl Pts',(-56.788210763293,67.7606126669312,60.5086553183781));
#217661=CARTESIAN_POINT('Ctrl Pts',(-56.8064949562029,67.1826894315703,
60.4580225336636));
#217662=CARTESIAN_POINT('Ctrl Pts',(-56.8624826951612,65.4198876776316,
60.4722152519561));
#217663=CARTESIAN_POINT('Ctrl Pts',(-56.8987059340921,64.2490704839672,
60.7129950715433));
#217664=CARTESIAN_POINT('Ctrl Pts',(-56.9683110302751,62.2292604910183,
61.5612370468008));
#217665=CARTESIAN_POINT('Ctrl Pts',(-56.9992267960155,61.372290861921,62.1024960302811));
#217666=CARTESIAN_POINT('Ctrl Pts',(-57.0403799912866,60.4035474054354,
62.967811165195));
#217667=CARTESIAN_POINT('Ctrl Pts',(-57.0496874866844,60.1950846130766,
63.172918921827));
#217668=CARTESIAN_POINT('Ctrl Pts',(-57.0874168908922,59.3907537315826,
64.0445044560468));
#217669=CARTESIAN_POINT('Ctrl Pts',(-57.1149213725863,58.8848057559073,
64.7871075949958));
#217670=CARTESIAN_POINT('Ctrl Pts',(-57.1489580148019,58.417345561021,65.7526958298713));
#217671=CARTESIAN_POINT('Ctrl Pts',(-57.1546554757547,58.34413324798,65.9160656035786));
#217672=CARTESIAN_POINT('Ctrl Pts',(-57.1603612091034,58.2758162839768,
66.0814193573839));
#217673=CARTESIAN_POINT('Origin',(-54.462516693425,66.6776194928561,69.5544896765311));
#217674=CARTESIAN_POINT('',(-49.1982221066882,75.0787836866508,73.0257672246888));
#217675=CARTESIAN_POINT('Ctrl Pts',(-50.1089321285242,58.276355535683,66.0834535849087));
#217676=CARTESIAN_POINT('Ctrl Pts',(-50.1001648443086,58.3817700064601,
65.8283093655669));
#217677=CARTESIAN_POINT('Ctrl Pts',(-50.091357844461,58.4988095027559,65.5779622274588));
#217678=CARTESIAN_POINT('Ctrl Pts',(-50.0673733290039,58.845963509162,64.9158995804182));
#217679=CARTESIAN_POINT('Ctrl Pts',(-50.0521062390893,59.0968945962679,
64.5162399824942));
#217680=CARTESIAN_POINT('Ctrl Pts',(-50.0169043107424,59.7502004724591,
63.6357882095687));
#217681=CARTESIAN_POINT('Ctrl Pts',(-49.9973020698474,60.1735288431777,
63.1735046916622));
#217682=CARTESIAN_POINT('Ctrl Pts',(-49.9487203819678,61.309018185135,62.1649067208048));
#217683=CARTESIAN_POINT('Ctrl Pts',(-49.9197679943601,62.0609702146647,
61.6732222160602));
#217684=CARTESIAN_POINT('Ctrl Pts',(-49.8537474866652,63.9486953595311,
60.8031147818176));
#217685=CARTESIAN_POINT('Ctrl Pts',(-49.8154492956854,65.1115774613567,
60.5222633777277));
#217686=CARTESIAN_POINT('Ctrl Pts',(-49.7594774935417,66.8729653580385,
60.4481640659964));
#217687=CARTESIAN_POINT('Ctrl Pts',(-49.7411381157849,67.4513788983311,
60.4789943263066));
#217688=CARTESIAN_POINT('Ctrl Pts',(-49.7042566752863,68.5840971818238,
60.6485014929856));
#217689=CARTESIAN_POINT('Ctrl Pts',(-49.6859159986314,69.1361734434929,
60.7848368355366));
#217690=CARTESIAN_POINT('Ctrl Pts',(-49.6499316417008,70.2067879832496,
61.1583482922952));
#217691=CARTESIAN_POINT('Ctrl Pts',(-49.6320659057619,70.7230320092189,
61.3945352583048));
#217692=CARTESIAN_POINT('Ctrl Pts',(-49.5967204675263,71.6787861381583,
61.9449286177151));
#217693=CARTESIAN_POINT('Ctrl Pts',(-49.5793543595703,72.1190398580046,
62.2532544285809));
#217694=CARTESIAN_POINT('Ctrl Pts',(-49.5453889300942,72.9359702314459,
62.9405283869928));
#217695=CARTESIAN_POINT('Ctrl Pts',(-49.5287567027039,73.3116600494043,
63.3174270927594));
#217696=CARTESIAN_POINT('Ctrl Pts',(-49.4957981899007,73.9766818142036,
64.1130850896679));
#217697=CARTESIAN_POINT('Ctrl Pts',(-49.4795549896811,74.268112948659,64.5276022967562));
#217698=CARTESIAN_POINT('Ctrl Pts',(-49.4441253151381,74.8267113564275,
65.4823825902168));
#217699=CARTESIAN_POINT('Ctrl Pts',(-49.425367023484,75.0777970242852,66.0293264987477));
#217700=CARTESIAN_POINT('Ctrl Pts',(-49.3977762232747,75.362219709797,66.8559648315499));
#217701=CARTESIAN_POINT('Ctrl Pts',(-49.3891007077892,75.4395676361253,
67.1188007279758));
#217702=CARTESIAN_POINT('Ctrl Pts',(-49.3654086650421,75.6171323513174,
67.8411921227889));
#217703=CARTESIAN_POINT('Ctrl Pts',(-49.3503126636981,75.6937569548679,
68.3056733009986));
#217704=CARTESIAN_POINT('Ctrl Pts',(-49.3198465655125,75.7762413958645,
69.262778266938));
#217705=CARTESIAN_POINT('Ctrl Pts',(-49.3045871399129,75.7787263345094,
69.7541768791264));
#217706=CARTESIAN_POINT('Ctrl Pts',(-49.2589558776886,75.6688407380179,
71.1999922741479));
#217707=CARTESIAN_POINT('Ctrl Pts',(-49.2282365965666,75.4451500591753,
72.1390896231537));
#217708=CARTESIAN_POINT('Ctrl Pts',(-49.1982221066882,75.0787836866507,
73.025767224689));
#217709=CARTESIAN_POINT('',(-48.6677134573784,61.073680689161,76.7064654074421));
#217710=CARTESIAN_POINT('Ctrl Pts',(-49.1982221066882,75.0787836866508,
73.0257672246888));
#217711=CARTESIAN_POINT('Ctrl Pts',(-49.1846980472593,74.913704732624,73.4252902759224));
#217712=CARTESIAN_POINT('Ctrl Pts',(-49.1712011184087,74.7203369872293,
73.8125282475041));
#217713=CARTESIAN_POINT('Ctrl Pts',(-49.1439889436598,74.2813616534623,
74.5541839958143));
#217714=CARTESIAN_POINT('Ctrl Pts',(-49.1303097641346,74.0366450956581,
74.9078602743798));
#217715=CARTESIAN_POINT('Ctrl Pts',(-49.0903095212971,73.2480510597892,
75.8907898671893));
#217716=CARTESIAN_POINT('Ctrl Pts',(-49.0648068913569,72.6419027431399,
76.4643810840044));
#217717=CARTESIAN_POINT('Ctrl Pts',(-49.0230777014757,71.5671431419043,
77.2332124069004));
#217718=CARTESIAN_POINT('Ctrl Pts',(-49.007421009719,71.1454839454682,77.4859717459455));
#217719=CARTESIAN_POINT('Ctrl Pts',(-48.9742148605163,70.2023028886257,
77.9521673598388));
#217720=CARTESIAN_POINT('Ctrl Pts',(-48.9568877851838,69.6771598053905,
78.1537422593015));
#217721=CARTESIAN_POINT('Ctrl Pts',(-48.9237288294822,68.659861073702,78.4396159088877));
#217722=CARTESIAN_POINT('Ctrl Pts',(-48.9080191469994,68.1727776032606,
78.5344253154042));
#217723=CARTESIAN_POINT('Ctrl Pts',(-48.873683136384,67.0983379452549,78.6536821387682));
#217724=CARTESIAN_POINT('Ctrl Pts',(-48.8554489933668,66.5113839390646,
78.6618866060698));
#217725=CARTESIAN_POINT('Ctrl Pts',(-48.8094548318523,65.0461525300166,
78.5405983068835));
#217726=CARTESIAN_POINT('Ctrl Pts',(-48.7811658054655,64.1799336903606,
78.3393276644481));
#217727=CARTESIAN_POINT('Ctrl Pts',(-48.7396885135181,62.9521885669229,
77.8574497716699));
#217728=CARTESIAN_POINT('Ctrl Pts',(-48.7261817253743,62.5597652232474,
77.6699847473452));
#217729=CARTESIAN_POINT('Ctrl Pts',(-48.6985186227286,61.7952368833308,
77.2349803636798));
#217730=CARTESIAN_POINT('Ctrl Pts',(-48.6843884535666,61.4249317932819,
76.9866399323976));
#217731=CARTESIAN_POINT('Ctrl Pts',(-48.6701794005809,61.0743248382493,
76.7121720277602));
#217732=CARTESIAN_POINT('',(-48.4675099033474,61.0743873391425,76.7079526484011));
#217733=CARTESIAN_POINT('Ctrl Pts',(-48.6675364832709,61.0743296293729,
76.7064311666085));
#217734=CARTESIAN_POINT('Ctrl Pts',(-48.6008609566297,61.0742541501395,
76.7121166899682));
#217735=CARTESIAN_POINT('Ctrl Pts',(-48.5341854299886,61.0742541501395,
76.7121166899682));
#217736=CARTESIAN_POINT('Ctrl Pts',(-48.4675099033474,61.0743873391425,
76.7079526484011));
#217737=CARTESIAN_POINT('',(-49.0012377727522,75.0788851372981,73.0255216843006));
#217738=CARTESIAN_POINT('Ctrl Pts',(-49.0012377727522,75.0788851372981,
73.0255216843007));
#217739=CARTESIAN_POINT('Ctrl Pts',(-48.9869942993643,74.9103006428599,
73.433562612226));
#217740=CARTESIAN_POINT('Ctrl Pts',(-48.9727665448605,74.712211176133,73.828783606424));
#217741=CARTESIAN_POINT('Ctrl Pts',(-48.9446794933677,74.262118103884,74.5840306233706));
#217742=CARTESIAN_POINT('Ctrl Pts',(-48.9308529409508,74.0111842107319,
74.9433420219173));
#217743=CARTESIAN_POINT('Ctrl Pts',(-48.8896864537942,73.1958164999378,
75.9478730054749));
#217744=CARTESIAN_POINT('Ctrl Pts',(-48.8618295254075,72.5650857674712,
76.5330266537419));
#217745=CARTESIAN_POINT('Ctrl Pts',(-48.8153368443041,71.3676828645975,
77.3643920920264));
#217746=CARTESIAN_POINT('Ctrl Pts',(-48.7964053555865,70.8406624110098,
77.6575966007387));
#217747=CARTESIAN_POINT('Ctrl Pts',(-48.7622406354934,69.8684013814934,
78.0784464648355));
#217748=CARTESIAN_POINT('Ctrl Pts',(-48.7474157728122,69.435108204469,78.2283117361156));
#217749=CARTESIAN_POINT('Ctrl Pts',(-48.7035598202974,68.1125708753328,
78.5765719982624));
#217750=CARTESIAN_POINT('Ctrl Pts',(-48.6750545183228,67.2029530271456,
78.6748551441207));
#217751=CARTESIAN_POINT('Ctrl Pts',(-48.6306159838825,65.8273428269903,
78.6167461339114));
#217752=CARTESIAN_POINT('Ctrl Pts',(-48.6156168883705,65.3629184399787,
78.5611000819068));
#217753=CARTESIAN_POINT('Ctrl Pts',(-48.5787691667423,64.2272104950673,
78.3352724470749));
#217754=CARTESIAN_POINT('Ctrl Pts',(-48.5570481635002,63.5671604509319,
78.1237188431728));
#217755=CARTESIAN_POINT('Ctrl Pts',(-48.5231754596626,62.6083701607617,
77.6908842886743));
#217756=CARTESIAN_POINT('Ctrl Pts',(-48.5115549194916,62.2884122013294,
77.5228376567529));
#217757=CARTESIAN_POINT('Ctrl Pts',(-48.4883063582053,61.6652772061066,
77.1466111270594));
#217758=CARTESIAN_POINT('Ctrl Pts',(-48.476702779211,61.3630201280924,76.9381823347568));
#217759=CARTESIAN_POINT('Ctrl Pts',(-48.4651187514169,61.0741848222002,
76.7120624158843));
#217760=CARTESIAN_POINT('Ctrl Pts',(-49.0012377727522,75.078885137298,73.0255216843008));
#217761=CARTESIAN_POINT('Ctrl Pts',(-49.0326707628863,75.450923235459,72.1250428395345));
#217762=CARTESIAN_POINT('Ctrl Pts',(-49.0629964763727,75.6757768809446,
71.1705888299228));
#217763=CARTESIAN_POINT('Ctrl Pts',(-49.1091535004338,75.7777234988366,
69.7357565069057));
#217764=CARTESIAN_POINT('Ctrl Pts',(-49.1241612222689,75.7751111726431,
69.2709474013524));
#217765=CARTESIAN_POINT('Ctrl Pts',(-49.1538032208726,75.6987817530598,
68.3441468554977));
#217766=CARTESIAN_POINT('Ctrl Pts',(-49.1684042707119,75.6249225116427,
67.8835400210816));
#217767=CARTESIAN_POINT('Ctrl Pts',(-49.1917625292445,75.4526744651001,
67.1667291178721));
#217768=CARTESIAN_POINT('Ctrl Pts',(-49.2003960293311,75.3774738893031,
66.9058065330857));
#217769=CARTESIAN_POINT('Ctrl Pts',(-49.2183905535684,75.1975516952871,
66.3725072663987));
#217770=CARTESIAN_POINT('Ctrl Pts',(-49.2277486140921,75.0911654414188,
66.1010130726577));
#217771=CARTESIAN_POINT('Ctrl Pts',(-49.255312390402,74.7393198726834,65.3163913233952));
#217772=CARTESIAN_POINT('Ctrl Pts',(-49.2731546401533,74.4585712256168,
64.8206448802581));
#217773=CARTESIAN_POINT('Ctrl Pts',(-49.3142586916319,73.7122552278678,
63.7506031450283));
#217774=CARTESIAN_POINT('Ctrl Pts',(-49.3377727083167,73.2193616288411,
63.2002168272672));
#217775=CARTESIAN_POINT('Ctrl Pts',(-49.3792277925132,72.2401419089374,
62.3428777396342));
#217776=CARTESIAN_POINT('Ctrl Pts',(-49.3968018831211,71.780930515834,62.0109347506041));
#217777=CARTESIAN_POINT('Ctrl Pts',(-49.4325669000478,70.8017678731028,
61.4337113078101));
#217778=CARTESIAN_POINT('Ctrl Pts',(-49.4507406214612,70.2834231666468,
61.1906502766293));
#217779=CARTESIAN_POINT('Ctrl Pts',(-49.4870584488999,69.2096738967599,
60.8056433766568));
#217780=CARTESIAN_POINT('Ctrl Pts',(-49.5048017336833,68.6567565845836,
60.6642347640358));
#217781=CARTESIAN_POINT('Ctrl Pts',(-49.5408220038162,67.5206384453855,
60.4849875690622));
#217782=CARTESIAN_POINT('Ctrl Pts',(-49.5591749832851,66.9396760153232,
60.4496632851458));
#217783=CARTESIAN_POINT('Ctrl Pts',(-49.6153043366467,65.1754023148062,
60.5114764952306));
#217784=CARTESIAN_POINT('Ctrl Pts',(-49.651559564527,64.0109182429452,60.7840022126295));
#217785=CARTESIAN_POINT('Ctrl Pts',(-49.7211504689484,62.0145825941254,
61.6869474545517));
#217786=CARTESIAN_POINT('Ctrl Pts',(-49.7520481397383,61.1728349495882,
62.2511002479665));
#217787=CARTESIAN_POINT('Ctrl Pts',(-49.7994150585316,60.0831561780242,
63.2788274913772));
#217788=CARTESIAN_POINT('Ctrl Pts',(-49.8151103594854,59.75354956367,63.6444866168048));
#217789=CARTESIAN_POINT('Ctrl Pts',(-49.8460313342345,59.1574259710313,
64.424539596982));
#217790=CARTESIAN_POINT('Ctrl Pts',(-49.8612146371712,58.8917316289723,
64.837535753946));
#217791=CARTESIAN_POINT('Ctrl Pts',(-49.8860248707078,58.5191076372099,
65.5347662480388));
#217792=CARTESIAN_POINT('Ctrl Pts',(-49.8954937757046,58.3908722997412,
65.8062782582976));
#217793=CARTESIAN_POINT('Ctrl Pts',(-49.9050113929448,58.276355535683,66.0834535849087));
#217794=CARTESIAN_POINT('Ctrl Pts',(-48.6992141518181,61.3765724540995,
76.9087096781305));
#217795=CARTESIAN_POINT('Ctrl Pts',(-48.6491771284881,60.0508982292929,
76.0595009463134));
#217796=CARTESIAN_POINT('Ctrl Pts',(-48.5491030818342,57.8143153964347,
73.6287810246093));
#217797=CARTESIAN_POINT('Ctrl Pts',(-48.3989920118381,56.6896833063533,
68.6586256876713));
#217798=CARTESIAN_POINT('Ctrl Pts',(-48.2488809418481,58.2322800110496,
63.6554187246849));
#217799=CARTESIAN_POINT('Ctrl Pts',(-48.1488068951881,60.8521889393111,
61.2125219408773));
#217800=CARTESIAN_POINT('Ctrl Pts',(-48.0987698718642,62.4030393117053,
60.392399558577));
#217801=CARTESIAN_POINT('Ctrl Pts',(-48.6180189895515,61.3765724540995,
76.9087096781305));
#217802=CARTESIAN_POINT('Ctrl Pts',(-48.5679819662217,60.0508982292929,
76.0595009463134));
#217803=CARTESIAN_POINT('Ctrl Pts',(-48.4679079195627,57.8143153964347,
73.6287810246093));
#217804=CARTESIAN_POINT('Ctrl Pts',(-48.3177968495717,56.6896833063533,
68.6586256876713));
#217805=CARTESIAN_POINT('Ctrl Pts',(-48.1676857795814,58.2322800110496,
63.6554187246849));
#217806=CARTESIAN_POINT('Ctrl Pts',(-48.0676117329217,60.8521889393111,
61.2125219408773));
#217807=CARTESIAN_POINT('Ctrl Pts',(-48.0175747095927,62.4030393117053,
60.392399558577));
#217808=CARTESIAN_POINT('Ctrl Pts',(-48.536823827284,61.3765724540995,76.9087096781305));
#217809=CARTESIAN_POINT('Ctrl Pts',(-48.4867868039552,60.0508982292929,
76.0595009463134));
#217810=CARTESIAN_POINT('Ctrl Pts',(-48.3867127572953,57.8143153964347,
73.6287810246093));
#217811=CARTESIAN_POINT('Ctrl Pts',(-48.2366016873052,56.6896833063533,
68.6586256876713));
#217812=CARTESIAN_POINT('Ctrl Pts',(-48.086490617314,58.2322800110496,63.6554187246849));
#217813=CARTESIAN_POINT('Ctrl Pts',(-47.9864165706552,60.8521889393111,
61.2125219408773));
#217814=CARTESIAN_POINT('Ctrl Pts',(-47.9363795473253,62.4030393117053,
60.392399558577));
#217815=CARTESIAN_POINT('Ctrl Pts',(-48.4556286650124,61.3765724540995,
76.9087096781305));
#217816=CARTESIAN_POINT('Ctrl Pts',(-48.4055916416887,60.0508982292929,
76.0595009463134));
#217817=CARTESIAN_POINT('Ctrl Pts',(-48.3055175950287,57.8143153964347,
73.6287810246093));
#217818=CARTESIAN_POINT('Ctrl Pts',(-48.1554065250387,56.6896833063533,
68.6586256876713));
#217819=CARTESIAN_POINT('Ctrl Pts',(-48.0052954550424,58.2322800110496,
63.6554187246849));
#217820=CARTESIAN_POINT('Ctrl Pts',(-47.9052214083887,60.8521889393111,
61.2125219408773));
#217821=CARTESIAN_POINT('Ctrl Pts',(-47.8551843850587,62.4030393117053,
60.392399558577));
#217822=CARTESIAN_POINT('',(-48.0901869004046,62.0494599115474,60.5887241650105));
#217823=CARTESIAN_POINT('Ctrl Pts',(-48.6675364832709,61.0744133081472,
76.7063115883213));
#217824=CARTESIAN_POINT('Ctrl Pts',(-48.6312818814118,60.1377246878961,
76.0508334285312));
#217825=CARTESIAN_POINT('Ctrl Pts',(-48.5950272795537,59.3165180062426,
75.2089926210815));
#217826=CARTESIAN_POINT('Ctrl Pts',(-48.558772677695,58.6733314433729,74.2361378419511));
#217827=CARTESIAN_POINT('Ctrl Pts',(-48.5488391350847,58.4971021979518,
73.9695814902986));
#217828=CARTESIAN_POINT('Ctrl Pts',(-48.5389055924745,58.3342372318397,
73.6931898163599));
#217829=CARTESIAN_POINT('Ctrl Pts',(-48.5289720498641,58.186022422969,73.4081017822123));
#217830=CARTESIAN_POINT('Ctrl Pts',(-48.4789350265345,57.4394380330742,
71.9720625789633));
#217831=CARTESIAN_POINT('Ctrl Pts',(-48.4288980032028,57.0645606697138,
70.3153441333173));
#217832=CARTESIAN_POINT('Ctrl Pts',(-48.378860979872,57.1342214388163,68.6531170833299));
#217833=CARTESIAN_POINT('Ctrl Pts',(-48.3288239565412,57.2038822079187,
66.9908900333425));
#217834=CARTESIAN_POINT('Ctrl Pts',(-48.2787869332112,57.7180811094842,
65.3231543790137));
#217835=CARTESIAN_POINT('Ctrl Pts',(-48.2287499098812,58.6301577923322,
63.8785623558974));
#217836=CARTESIAN_POINT('Ctrl Pts',(-48.1929768542908,59.2822303519465,
62.8457776834833));
#217837=CARTESIAN_POINT('Ctrl Pts',(-48.1572037987003,60.1376805095661,
61.9270378606398));
#217838=CARTESIAN_POINT('Ctrl Pts',(-48.1214304257129,61.1391178756878,
61.1874783353119));
#217839=CARTESIAN_POINT('Ctrl Pts',(-48.111015793019,61.430664393758,60.9721718051091));
#217840=CARTESIAN_POINT('Ctrl Pts',(-48.1006011334239,61.7345839021518,
60.7720515626229));
#217841=CARTESIAN_POINT('Ctrl Pts',(-48.090186439096,62.0494598503368,60.5887240860842));
#217842=CARTESIAN_POINT('',(-47.8901874902887,62.0494598737417,60.588724072085));
#217843=CARTESIAN_POINT('',(-48.0901862140809,62.0494598738326,60.5887240724044));
#217844=CARTESIAN_POINT('Ctrl Pts',(-48.4675451203219,61.0746269353901,
76.7064610762623));
#217845=CARTESIAN_POINT('Ctrl Pts',(-48.4374727537661,60.2976378300801,
76.1627715126034));
#217846=CARTESIAN_POINT('Ctrl Pts',(-48.4076478871442,59.6067484297961,
75.4956452737586));
#217847=CARTESIAN_POINT('Ctrl Pts',(-48.3478038746688,58.4441481286654,
73.9693330989566));
#217848=CARTESIAN_POINT('Ctrl Pts',(-48.3182577310618,57.9861362652872,
73.118218239834));
#217849=CARTESIAN_POINT('Ctrl Pts',(-48.2515859642631,57.2658215968254,
71.0669096930218));
#217850=CARTESIAN_POINT('Ctrl Pts',(-48.2150542464285,57.0838374275983,
69.855443032875));
#217851=CARTESIAN_POINT('Ctrl Pts',(-48.1419859937645,57.1855554964561,
67.4281199427107));
#217852=CARTESIAN_POINT('Ctrl Pts',(-48.1054696631336,57.4774766013662,
66.2128718196243));
#217853=CARTESIAN_POINT('Ctrl Pts',(-48.0390051710523,58.3991305558005,
64.1561131800471));
#217854=CARTESIAN_POINT('Ctrl Pts',(-48.0094233078613,58.959999203317,63.3004156653558));
#217855=CARTESIAN_POINT('Ctrl Pts',(-47.9496630882316,60.3396764638368,
61.7718652461384));
#217856=CARTESIAN_POINT('Ctrl Pts',(-47.9198152757014,61.1536715706108,
61.1102710786235));
#217857=CARTESIAN_POINT('Ctrl Pts',(-47.8901874908167,62.0494598739167,
60.5887240723555));
#217858=CARTESIAN_POINT('Ctrl Pts',(-63.7104920345709,57.8065696683908,
74.8099293892527));
#217859=CARTESIAN_POINT('Ctrl Pts',(-63.6718652093945,57.1031312732521,
73.6224666938169));
#217860=CARTESIAN_POINT('Ctrl Pts',(-63.5946115590417,56.1796658359588,
70.9619911069131));
#217861=CARTESIAN_POINT('Ctrl Pts',(-63.4787310835129,56.4635561166055,
66.7467220222677));
#217862=CARTESIAN_POINT('Ctrl Pts',(-63.3628506079829,58.3717651523206,
62.9775246456951));
#217863=CARTESIAN_POINT('Ctrl Pts',(-63.2469701324539,61.6008831507443,
60.2533615179501));
#217864=CARTESIAN_POINT('Ctrl Pts',(-63.1310896569249,65.6376592981465,
59.007288209015));
#217865=CARTESIAN_POINT('Ctrl Pts',(-63.0152091813959,69.8404311589655,
59.4373596262818));
#217866=CARTESIAN_POINT('Ctrl Pts',(-62.8993287058659,73.5411595353312,
61.4752179418165));
#217867=CARTESIAN_POINT('Ctrl Pts',(-62.7834482303369,76.1516039658375,
64.7969396843518));
#217868=CARTESIAN_POINT('Ctrl Pts',(-62.6675677548079,77.2568279536785,
68.8745291515198));
#217869=CARTESIAN_POINT('Ctrl Pts',(-62.5516872792779,76.6811533646194,
73.0598433065362));
#217870=CARTESIAN_POINT('Ctrl Pts',(-62.4358068037489,74.5160851144003,
76.6876160812524));
#217871=CARTESIAN_POINT('Ctrl Pts',(-62.3199263282199,71.1057661783553,
79.1812039750165));
#217872=CARTESIAN_POINT('Ctrl Pts',(-62.2040458526899,66.9922752255877,
80.1442449974989));
#217873=CARTESIAN_POINT('Ctrl Pts',(-62.0881653771609,62.8294618635471,
79.4236613850277));
#217874=CARTESIAN_POINT('Ctrl Pts',(-61.9722849016309,59.2790156194285,
77.1339916933007));
#217875=CARTESIAN_POINT('Ctrl Pts',(-61.8564044261019,56.9052887454224,
73.6391846088869));
#217876=CARTESIAN_POINT('Ctrl Pts',(-61.7405239505729,56.0855910260969,
69.4947484013197));
#217877=CARTESIAN_POINT('Ctrl Pts',(-61.6246434750429,56.9502154506322,
65.3594515033776));
#217878=CARTESIAN_POINT('Ctrl Pts',(-61.5087629995139,59.361727818425,61.8906096318565));
#217879=CARTESIAN_POINT('Ctrl Pts',(-61.3928825239839,62.9368122467912,
59.6396038211846));
#217880=CARTESIAN_POINT('Ctrl Pts',(-61.2770020484549,67.1072001829157,
58.9642370379884));
#217881=CARTESIAN_POINT('Ctrl Pts',(-61.1611215729249,71.209998102294,59.9718605105236));
#217882=CARTESIAN_POINT('Ctrl Pts',(-61.0452410973959,74.5930560815078,
62.5023099842148));
#217883=CARTESIAN_POINT('Ctrl Pts',(-60.9293606218659,76.7186286489653,
66.1533642278691));
#217884=CARTESIAN_POINT('Ctrl Pts',(-60.8134801463369,77.2488507637066,
70.3446790977719));
#217885=CARTESIAN_POINT('Ctrl Pts',(-60.6975996708069,76.0994423031657,
74.4100346812925));
#217886=CARTESIAN_POINT('Ctrl Pts',(-60.5817191952779,73.4531045980525,
77.7032326073399));
#217887=CARTESIAN_POINT('Ctrl Pts',(-60.4658387197479,69.7304796018871,
79.7008108830386));
#217888=CARTESIAN_POINT('Ctrl Pts',(-60.3499582442189,65.5232878073241,
80.0852494781353));
#217889=CARTESIAN_POINT('Ctrl Pts',(-60.2340777686899,61.5002728036194,
78.7954409227264));
#217890=CARTESIAN_POINT('Ctrl Pts',(-60.1181972931599,58.3009028215076,
76.0364034914597));
#217891=CARTESIAN_POINT('Ctrl Pts',(-60.0023168176309,56.433725669026,72.2466930393406));
#217892=CARTESIAN_POINT('Ctrl Pts',(-59.8864363421009,56.1955337939067,
68.0286934589439));
#217893=CARTESIAN_POINT('Ctrl Pts',(-59.7705558665719,57.624188386514,64.0528662639259));
#217894=CARTESIAN_POINT('Ctrl Pts',(-59.6546753910419,60.4926012496316,
60.9511790655875));
#217895=CARTESIAN_POINT('Ctrl Pts',(-59.5387949155129,64.3448310315735,
59.2166527507834));
#217896=CARTESIAN_POINT('Ctrl Pts',(-59.4229144399829,68.5685562369575,
59.1249945869912));
#217897=CARTESIAN_POINT('Ctrl Pts',(-59.3070339644539,72.4924052498076,
60.690773867081));
#217898=CARTESIAN_POINT('Ctrl Pts',(-59.1911534889249,75.4926725200354,
63.6651060840354));
#217899=CARTESIAN_POINT('Ctrl Pts',(-59.0752730133949,77.0924581103469,
67.575213741715));
#217900=CARTESIAN_POINT('Ctrl Pts',(-58.9593925378659,77.0374721262134,
71.7995755125809));
#217901=CARTESIAN_POINT('Ctrl Pts',(-58.8435120623359,75.3364547264357,
75.6667185969866));
#217902=CARTESIAN_POINT('Ctrl Pts',(-58.7276315868069,72.2597868531839,
78.5619509930676));
#217903=CARTESIAN_POINT('Ctrl Pts',(-58.6117511112779,68.2965125094352,
80.0250683177526));
#217904=CARTESIAN_POINT('Ctrl Pts',(-58.4958706357479,64.076603999578,79.8235044369148));
#217905=CARTESIAN_POINT('Ctrl Pts',(-58.3799901602189,60.2708262663669,
77.9892984302229));
#217906=CARTESIAN_POINT('Ctrl Pts',(-58.2641096846899,57.4841171366094,
74.8140018998644));
#217907=CARTESIAN_POINT('Ctrl Pts',(-58.1482292091609,56.1594309505501,
70.8023361189094));
#217908=CARTESIAN_POINT('Ctrl Pts',(-58.0323487336309,56.5073298688805,
66.5919653309315));
#217909=CARTESIAN_POINT('Ctrl Pts',(-57.9164682581019,58.4725144941193,
62.8521384340947));
#217910=CARTESIAN_POINT('Ctrl Pts',(-57.8005877825729,61.7426138472405,
60.1773102058845));
#217911=CARTESIAN_POINT('Ctrl Pts',(-57.6847073070439,65.7978375109195,
58.992651239347));
#217912=CARTESIAN_POINT('Ctrl Pts',(-57.5688268315149,69.9935976079059,
59.4864660203555));
#217913=CARTESIAN_POINT('Ctrl Pts',(-57.4529463559859,73.6629676456614,
61.5802614638165));
#217914=CARTESIAN_POINT('Ctrl Pts',(-57.3370658804569,76.2226921395821,
64.941223576645));
#217915=CARTESIAN_POINT('Ctrl Pts',(-57.2211854049279,77.2658965208973,
69.0351190986164));
#217916=CARTESIAN_POINT('Ctrl Pts',(-57.1053049293989,76.6267608625964,
73.2112130953809));
#217917=CARTESIAN_POINT('Ctrl Pts',(-56.9894244538699,74.4068773602934,
76.8057053079185));
#217918=CARTESIAN_POINT('Ctrl Pts',(-56.8735439783409,70.9591020322142,
79.2472413050085));
#217919=CARTESIAN_POINT('Ctrl Pts',(-56.7576635028119,66.8314672593026,
80.1477364670454));
#217920=CARTESIAN_POINT('Ctrl Pts',(-56.6417830272829,62.6800711209345,
79.3640414392399));
#217921=CARTESIAN_POINT('Ctrl Pts',(-56.5259025517539,59.1647873166941,
77.0207765453072));
#217922=CARTESIAN_POINT('Ctrl Pts',(-56.4100220762249,56.844382791141,73.4902227664913));
#217923=CARTESIAN_POINT('Ctrl Pts',(-56.3327684258729,56.3399124253312,
70.7195859421522));
#217924=CARTESIAN_POINT('Ctrl Pts',(-56.2941416006959,56.3683493792519,
69.3397002336784));
#217925=CARTESIAN_POINT('Ctrl Pts',(-63.4863639242949,58.1769980971959,
74.5904921130554));
#217926=CARTESIAN_POINT('Ctrl Pts',(-63.4477370991189,57.5029187523924,
73.4525899438659));
#217927=CARTESIAN_POINT('Ctrl Pts',(-63.3704834487659,56.6179955221206,
70.9031532726741));
#217928=CARTESIAN_POINT('Ctrl Pts',(-63.2546029732369,56.8900372185927,
66.863814728757));
#217929=CARTESIAN_POINT('Ctrl Pts',(-63.1387224977069,58.7186043048254,
63.2519304250262));
#217930=CARTESIAN_POINT('Ctrl Pts',(-63.0228420221779,61.8129502485881,
60.6414643074804));
#217931=CARTESIAN_POINT('Ctrl Pts',(-62.9069615466489,65.6812455241418,
59.4473977261369));
#217932=CARTESIAN_POINT('Ctrl Pts',(-62.7910810711199,69.7086084345096,
59.8595194715137));
#217933=CARTESIAN_POINT('Ctrl Pts',(-62.6752005955899,73.2548813938479,
61.8123247315615));
#217934=CARTESIAN_POINT('Ctrl Pts',(-62.5593201200609,75.7563750335582,
64.9954094640758));
#217935=CARTESIAN_POINT('Ctrl Pts',(-62.4434396445319,76.8154708502427,
68.9028146546496));
#217936=CARTESIAN_POINT('Ctrl Pts',(-62.3275591690019,76.2638228985589,
72.9134484825934));
#217937=CARTESIAN_POINT('Ctrl Pts',(-62.2116786934729,74.1891170001427,
76.3898107511058));
#217938=CARTESIAN_POINT('Ctrl Pts',(-62.0957982179439,70.9211328100948,
78.7793250358796));
#217939=CARTESIAN_POINT('Ctrl Pts',(-61.9799177424139,66.9793245359562,
79.7021721052773));
#217940=CARTESIAN_POINT('Ctrl Pts',(-61.8640372668849,62.9902523968414,
79.0116631243529));
#217941=CARTESIAN_POINT('Ctrl Pts',(-61.7481567913549,59.5879893208676,
76.8175562113823));
#217942=CARTESIAN_POINT('Ctrl Pts',(-61.6322763158259,57.3133334774654,
73.4686101118191));
#217943=CARTESIAN_POINT('Ctrl Pts',(-61.5163958402969,56.5278470647294,
69.4971481292357));
#217944=CARTESIAN_POINT('Ctrl Pts',(-61.4005153647669,57.3563850996458,
65.5344440135604));
#217945=CARTESIAN_POINT('Ctrl Pts',(-61.2846348892379,59.667249402905,62.210379430011));
#217946=CARTESIAN_POINT('Ctrl Pts',(-61.1687544137079,63.0931223517737,
60.0533227033746));
#217947=CARTESIAN_POINT('Ctrl Pts',(-61.0528739381789,67.0894529288327,
59.4061433599309));
#217948=CARTESIAN_POINT('Ctrl Pts',(-60.9369934626489,71.0210144592654,
60.3717121643543));
#217949=CARTESIAN_POINT('Ctrl Pts',(-60.8211129871199,74.2628754691667,
62.7965495560487));
#217950=CARTESIAN_POINT('Ctrl Pts',(-60.7052325115899,76.2997340960325,
66.2952216066778));
#217951=CARTESIAN_POINT('Ctrl Pts',(-60.5893520360609,76.8078266001889,
70.3116057007245));
#217952=CARTESIAN_POINT('Ctrl Pts',(-60.4734715605309,75.7063904156562,
74.2072876070264));
#217953=CARTESIAN_POINT('Ctrl Pts',(-60.3575910850019,73.1705015606764,
77.3630390070701));
#217954=CARTESIAN_POINT('Ctrl Pts',(-60.2417106094719,69.6032458696127,
79.277245374799));
#217955=CARTESIAN_POINT('Ctrl Pts',(-60.1258301339429,65.5716474980321,
79.6456388518812));
#217956=CARTESIAN_POINT('Ctrl Pts',(-60.0099496584129,61.7165390243107,
78.4096623797983));
#217957=CARTESIAN_POINT('Ctrl Pts',(-59.8940691828839,58.6506995190535,
75.765777489781));
#217958=CARTESIAN_POINT('Ctrl Pts',(-59.7781887073549,56.86145178922,72.1342362543012));
#217959=CARTESIAN_POINT('Ctrl Pts',(-59.6623082318249,56.6332012071813,
68.0922811759416));
#217960=CARTESIAN_POINT('Ctrl Pts',(-59.5464277562959,58.002228770078,64.2823910573551));
#217961=CARTESIAN_POINT('Ctrl Pts',(-59.4305472807659,60.7509241451938,
61.3101573992297));
#217962=CARTESIAN_POINT('Ctrl Pts',(-59.3146668052369,64.4423753730412,
59.6480241265653));
#217963=CARTESIAN_POINT('Ctrl Pts',(-59.1987863297069,68.4898171088944,
59.5601914529124));
#217964=CARTESIAN_POINT('Ctrl Pts',(-59.0829058541779,72.2498984322556,
61.0606205999848));
#217965=CARTESIAN_POINT('Ctrl Pts',(-58.9670253786489,75.1249450741959,
63.9108146267734));
#217966=CARTESIAN_POINT('Ctrl Pts',(-58.8511449031189,76.6579612274189,
67.6577281109137));
#217967=CARTESIAN_POINT('Ctrl Pts',(-58.7352644275899,76.6052701653223,
71.7057798442352));
#217968=CARTESIAN_POINT('Ctrl Pts',(-58.6193839520599,74.9752472631463,
75.4115219456312));
#217969=CARTESIAN_POINT('Ctrl Pts',(-58.5035034765309,72.0269887112709,
78.1859175005157));
#217970=CARTESIAN_POINT('Ctrl Pts',(-58.3876230010019,68.2291275319825,
79.5879694419675));
#217971=CARTESIAN_POINT('Ctrl Pts',(-58.2717425254719,64.1853431961836,
79.394818130247));
#217972=CARTESIAN_POINT('Ctrl Pts',(-58.1558620499429,60.5384052715379,
77.6371654462714));
#217973=CARTESIAN_POINT('Ctrl Pts',(-58.0399815744139,57.8680036026363,
74.5943946513582));
#217974=CARTESIAN_POINT('Ctrl Pts',(-57.9241010988849,56.5986051698264,
70.7501617236546));
#217975=CARTESIAN_POINT('Ctrl Pts',(-57.8082206233549,56.9319840080419,
66.7155170386891));
#217976=CARTESIAN_POINT('Ctrl Pts',(-57.6923401478259,58.8151487226244,
63.1317773939326));
#217977=CARTESIAN_POINT('Ctrl Pts',(-57.5764596722969,61.9487656031238,
60.5685871103211));
#217978=CARTESIAN_POINT('Ctrl Pts',(-57.4605791967679,65.8347384603639,
59.4333716522234));
#217979=CARTESIAN_POINT('Ctrl Pts',(-57.3446987212389,69.8553822533185,
59.906576337004));
#217980=CARTESIAN_POINT('Ctrl Pts',(-57.2288182457099,73.3716056610648,
61.9129841055396));
#217981=CARTESIAN_POINT('Ctrl Pts',(-57.1129377701809,75.8244962363713,
65.1336714529827));
#217982=CARTESIAN_POINT('Ctrl Pts',(-56.9970572946509,76.8241609272865,
69.0567021408465));
#217983=CARTESIAN_POINT('Ctrl Pts',(-56.8811768191219,76.2117005487124,
73.058500627591));
#217984=CARTESIAN_POINT('Ctrl Pts',(-56.7652963435929,74.0844671944947,
76.502971347812));
#217985=CARTESIAN_POINT('Ctrl Pts',(-56.6494158680649,70.7805899107851,
78.8426061994355));
#217986=CARTESIAN_POINT('Ctrl Pts',(-56.5335353925359,66.8252281299281,
79.705517853136));
#217987=CARTESIAN_POINT('Ctrl Pts',(-56.4176549170069,62.8470966996323,
78.9545315059017));
#217988=CARTESIAN_POINT('Ctrl Pts',(-56.3017744414779,59.4785285066753,
76.7090662664087));
#217989=CARTESIAN_POINT('Ctrl Pts',(-56.1858939659489,57.2549695240061,
73.3258654140387));
#217990=CARTESIAN_POINT('Ctrl Pts',(-56.1086403155959,56.7715539811408,
70.6708652489211));
#217991=CARTESIAN_POINT('Ctrl Pts',(-56.0700134904199,56.7988040763871,
69.3485711280681));
#217992=CARTESIAN_POINT('Ctrl Pts',(-63.2622358140189,58.547426526001,74.3710548368581));
#217993=CARTESIAN_POINT('Ctrl Pts',(-63.2236089888419,57.9027062315234,
73.282713193911));
#217994=CARTESIAN_POINT('Ctrl Pts',(-63.1463553384899,57.0563252082828,
70.8443154384342));
#217995=CARTESIAN_POINT('Ctrl Pts',(-63.0304748629609,57.3165183205799,
66.9809074352464));
#217996=CARTESIAN_POINT('Ctrl Pts',(-62.9145943874309,59.0654434573398,
63.5263362043602));
#217997=CARTESIAN_POINT('Ctrl Pts',(-62.7987139119019,62.0250173464219,
61.0295670970088));
#217998=CARTESIAN_POINT('Ctrl Pts',(-62.6828334363729,65.7248317501465,
59.8875072432628));
#217999=CARTESIAN_POINT('Ctrl Pts',(-62.5669529608439,69.5767857100507,
60.2816793167476));
#218000=CARTESIAN_POINT('Ctrl Pts',(-62.4510724853139,72.9686032523646,
62.1494315213011));
#218001=CARTESIAN_POINT('Ctrl Pts',(-62.3351920097849,75.3611461012774,
65.1938792437982));
#218002=CARTESIAN_POINT('Ctrl Pts',(-62.2193115342559,76.3741137468067,
68.9311001577751));
#218003=CARTESIAN_POINT('Ctrl Pts',(-62.1034310587259,75.8464924324996,
72.7670536586459));
#218004=CARTESIAN_POINT('Ctrl Pts',(-61.9875505831969,73.862148885889,76.0920054209542));
#218005=CARTESIAN_POINT('Ctrl Pts',(-61.8716701076679,70.73649944184,78.3774460967396));
#218006=CARTESIAN_POINT('Ctrl Pts',(-61.7557896321379,66.9663738463322,
79.2600992130555));
#218007=CARTESIAN_POINT('Ctrl Pts',(-61.6399091566089,63.1510429301467,
78.5996648636749));
#218008=CARTESIAN_POINT('Ctrl Pts',(-61.5240286810789,59.8969630223145,
76.5011207294713));
#218009=CARTESIAN_POINT('Ctrl Pts',(-61.4081482055499,57.7213782095142,
73.2980356147634));
#218010=CARTESIAN_POINT('Ctrl Pts',(-61.2922677300209,56.9701031033569,
69.4995478571637));
#218011=CARTESIAN_POINT('Ctrl Pts',(-61.1763872544909,57.7625547486447,
65.7094365237527));
#218012=CARTESIAN_POINT('Ctrl Pts',(-61.0605067789619,59.9727709873796,
62.5301492281785));
#218013=CARTESIAN_POINT('Ctrl Pts',(-60.9446263034319,63.2494324567334,
60.4670415855671));
#218014=CARTESIAN_POINT('Ctrl Pts',(-60.8287458279029,67.0717056747189,
59.8480496818693));
#218015=CARTESIAN_POINT('Ctrl Pts',(-60.7128653523729,70.8320308162221,
60.7715638181682));
#218016=CARTESIAN_POINT('Ctrl Pts',(-60.5969848768439,73.9326948568119,
63.090789127866));
#218017=CARTESIAN_POINT('Ctrl Pts',(-60.4811044013139,75.8808395430932,
66.4370789854654));
#218018=CARTESIAN_POINT('Ctrl Pts',(-60.3652239257849,76.3668024366729,
70.2785323036529));
#218019=CARTESIAN_POINT('Ctrl Pts',(-60.2493434502549,75.3133385281575,
74.004540532737));
#218020=CARTESIAN_POINT('Ctrl Pts',(-60.1334629747259,72.887898523321,77.0228454067829));
#218021=CARTESIAN_POINT('Ctrl Pts',(-60.0175824991959,69.4760121373647,
78.8536798665508));
#218022=CARTESIAN_POINT('Ctrl Pts',(-59.9017020236669,65.6200071887684,
79.2060282256323));
#218023=CARTESIAN_POINT('Ctrl Pts',(-59.7858215481369,61.9328052450312,
78.023883836878));
#218024=CARTESIAN_POINT('Ctrl Pts',(-59.6699410726079,59.0004962166207,
75.4951514881296));
#218025=CARTESIAN_POINT('Ctrl Pts',(-59.5540605970789,57.2891779094226,
72.0217794692935));
#218026=CARTESIAN_POINT('Ctrl Pts',(-59.4381801215489,57.0708686204521,
68.1558688929745));
#218027=CARTESIAN_POINT('Ctrl Pts',(-59.3222996460199,58.3802691536199,
64.5119158508119));
#218028=CARTESIAN_POINT('Ctrl Pts',(-59.2064191704899,61.0092470407258,
61.6691357328929));
#218029=CARTESIAN_POINT('Ctrl Pts',(-59.0905386949609,64.5399197144825,
60.0793955023591));
#218030=CARTESIAN_POINT('Ctrl Pts',(-58.9746582194309,68.4110779807901,
59.9953883188285));
#218031=CARTESIAN_POINT('Ctrl Pts',(-58.8587777439019,72.0073916146724,
61.4304673328671));
#218032=CARTESIAN_POINT('Ctrl Pts',(-58.7428972683729,74.7572176283345,
64.1565231694807));
#218033=CARTESIAN_POINT('Ctrl Pts',(-58.6270167928429,76.2234643444835,
67.7402424800746));
#218034=CARTESIAN_POINT('Ctrl Pts',(-58.5111363173139,76.1730682044392,
71.6119841758516));
#218035=CARTESIAN_POINT('Ctrl Pts',(-58.3952558417839,74.6140397998802,
75.1563252942433));
#218036=CARTESIAN_POINT('Ctrl Pts',(-58.2793753662549,71.7941905693904,
77.8098840079436));
#218037=CARTESIAN_POINT('Ctrl Pts',(-58.1634948907259,68.1617425545688,
79.1508705661768));
#218038=CARTESIAN_POINT('Ctrl Pts',(-58.0476144151959,64.2940823928253,
78.9661318235942));
#218039=CARTESIAN_POINT('Ctrl Pts',(-57.9317339396669,60.8059842767521,
77.2850324623464));
#218040=CARTESIAN_POINT('Ctrl Pts',(-57.8158534641379,58.2518900686915,
74.3747874028885));
#218041=CARTESIAN_POINT('Ctrl Pts',(-57.6999729886089,57.0377793891086,
70.6979873284379));
#218042=CARTESIAN_POINT('Ctrl Pts',(-57.5840925130789,57.3566381471987,
66.8390687464839));
#218043=CARTESIAN_POINT('Ctrl Pts',(-57.4682120375499,59.157782951098,63.4114163537943));
#218044=CARTESIAN_POINT('Ctrl Pts',(-57.3523315620209,62.1549173589786,
60.9598640147741));
#218045=CARTESIAN_POINT('Ctrl Pts',(-57.2364510864919,65.8716394097845,
59.8740920651051));
#218046=CARTESIAN_POINT('Ctrl Pts',(-57.1205706109629,69.7171668986981,
60.326686653654));
#218047=CARTESIAN_POINT('Ctrl Pts',(-57.0046901354339,73.0802436764493,
62.2457067472407));
#218048=CARTESIAN_POINT('Ctrl Pts',(-56.8888096599039,75.4263003331489,
65.3261193292961));
#218049=CARTESIAN_POINT('Ctrl Pts',(-56.7729291843749,76.3824253336746,
69.0782851830545));
#218050=CARTESIAN_POINT('Ctrl Pts',(-56.6570487088459,75.7966402348365,
72.9057881597825));
#218051=CARTESIAN_POINT('Ctrl Pts',(-56.5411682333169,73.7620570287082,
76.2002373876932));
#218052=CARTESIAN_POINT('Ctrl Pts',(-56.4252877577879,70.6020777893704,
78.4379710938565));
#218053=CARTESIAN_POINT('Ctrl Pts',(-56.3094072822599,66.8189890005654,
79.2632992392271));
#218054=CARTESIAN_POINT('Ctrl Pts',(-56.1935268067309,63.0141222783363,
78.5450215725671));
#218055=CARTESIAN_POINT('Ctrl Pts',(-56.0776463312019,59.7922696966654,
76.3973559875148));
#218056=CARTESIAN_POINT('Ctrl Pts',(-55.9617658556729,57.6655562568715,
73.1615080615852));
#218057=CARTESIAN_POINT('Ctrl Pts',(-55.8845122053199,57.2031955369423,
70.6221445556835));
#218058=CARTESIAN_POINT('Ctrl Pts',(-55.8458853801439,57.2292587735241,
69.3574420224531));
#218059=CARTESIAN_POINT('Ctrl Pts',(-63.0381077037429,58.9178549548062,
74.1516175606608));
#218060=CARTESIAN_POINT('Ctrl Pts',(-62.9994808785659,58.3024937106637,
73.11283644396));
#218061=CARTESIAN_POINT('Ctrl Pts',(-62.9222272282139,57.4946548944447,
70.7854776041952));
#218062=CARTESIAN_POINT('Ctrl Pts',(-62.8063467526839,57.7429994225583,
67.098000141731));
#218063=CARTESIAN_POINT('Ctrl Pts',(-62.6904662771549,59.4122826098446,
63.8007419836913));
#218064=CARTESIAN_POINT('Ctrl Pts',(-62.5745858016259,62.2370844442565,
61.4176698865354));
#218065=CARTESIAN_POINT('Ctrl Pts',(-62.4587053260969,65.7684179761418,
60.3276167603848));
#218066=CARTESIAN_POINT('Ctrl Pts',(-62.3428248505679,69.4449629855937,
60.7038391619823));
#218067=CARTESIAN_POINT('Ctrl Pts',(-62.2269443750379,72.6823251108832,
62.4865383110415));
#218068=CARTESIAN_POINT('Ctrl Pts',(-62.1110638995089,74.9659171689976,
65.3923490235231));
#218069=CARTESIAN_POINT('Ctrl Pts',(-61.9951834239799,75.9327566433709,
68.959385660905));
#218070=CARTESIAN_POINT('Ctrl Pts',(-61.8793029484499,75.429161966439,72.6206588347031));
#218071=CARTESIAN_POINT('Ctrl Pts',(-61.7634224729209,73.5351807716313,
75.7942000908075));
#218072=CARTESIAN_POINT('Ctrl Pts',(-61.6475419973919,70.5518660735791,
77.9755671576036));
#218073=CARTESIAN_POINT('Ctrl Pts',(-61.5316615218619,66.9534231567007,
78.8180263208339));
#218074=CARTESIAN_POINT('Ctrl Pts',(-61.4157810463329,63.3118334634422,
78.1876666029973));
#218075=CARTESIAN_POINT('Ctrl Pts',(-61.2999005708029,60.2059367237536,
76.1846852475529));
#218076=CARTESIAN_POINT('Ctrl Pts',(-61.1840200952739,58.1294229415569,
73.1274611176965));
#218077=CARTESIAN_POINT('Ctrl Pts',(-61.0681396197439,57.4123591419893,
69.5019475850797));
#218078=CARTESIAN_POINT('Ctrl Pts',(-60.9522591442149,58.1687243976584,
65.8844290339353));
#218079=CARTESIAN_POINT('Ctrl Pts',(-60.8363786686859,60.2782925718688,
62.8499190263368));
#218080=CARTESIAN_POINT('Ctrl Pts',(-60.7204981931559,63.4057425617159,
60.8807604677571));
#218081=CARTESIAN_POINT('Ctrl Pts',(-60.6046177176269,67.0539584206267,
60.2899560038079));
#218082=CARTESIAN_POINT('Ctrl Pts',(-60.4887372420969,70.6430471731958,
61.1714154719933));
#218083=CARTESIAN_POINT('Ctrl Pts',(-60.3728567665679,73.6025142444707,
63.3850286996998));
#218084=CARTESIAN_POINT('Ctrl Pts',(-60.2569762910379,75.4619449901604,
66.5789363642741));
#218085=CARTESIAN_POINT('Ctrl Pts',(-60.1410958155089,75.9257782731553,
70.2454589066056));
#218086=CARTESIAN_POINT('Ctrl Pts',(-60.0252153399789,74.9202866406472,
73.8017934584711));
#218087=CARTESIAN_POINT('Ctrl Pts',(-59.9093348644499,72.6052954859446,
76.6826518065131));
#218088=CARTESIAN_POINT('Ctrl Pts',(-59.7934543889199,69.34877840509,78.4301143583121));
#218089=CARTESIAN_POINT('Ctrl Pts',(-59.6775739133909,65.6683668794744,
78.7664175993805));
#218090=CARTESIAN_POINT('Ctrl Pts',(-59.5616934378609,62.149071465724,77.6381052939462));
#218091=CARTESIAN_POINT('Ctrl Pts',(-59.4458129623319,59.3502929141666,
75.224525486451));
#218092=CARTESIAN_POINT('Ctrl Pts',(-59.3299324868019,57.7169040296169,
71.9093226842531));
#218093=CARTESIAN_POINT('Ctrl Pts',(-59.2140520112729,57.5085360337358,
68.219456609976));
#218094=CARTESIAN_POINT('Ctrl Pts',(-59.0981715357439,58.7583095371751,
64.7414406442363));
#218095=CARTESIAN_POINT('Ctrl Pts',(-58.9822910602139,61.2675699362972,
62.0281140665389));
#218096=CARTESIAN_POINT('Ctrl Pts',(-58.8664105846849,64.6374640559506,
60.5107668781401));
#218097=CARTESIAN_POINT('Ctrl Pts',(-58.7505301091549,68.3323388527351,
60.4305851847563));
#218098=CARTESIAN_POINT('Ctrl Pts',(-58.6346496336259,71.7648847971204,
61.800314065771));
#218099=CARTESIAN_POINT('Ctrl Pts',(-58.5187691580959,74.3894901824946,
64.4022317122195));
#218100=CARTESIAN_POINT('Ctrl Pts',(-58.4028886825669,75.7889674615547,
67.8227568492751));
#218101=CARTESIAN_POINT('Ctrl Pts',(-58.2870082070379,75.740866243548,71.5181885075058));
#218102=CARTESIAN_POINT('Ctrl Pts',(-58.1711277315079,74.2528323365911,
74.9011286428881));
#218103=CARTESIAN_POINT('Ctrl Pts',(-58.0552472559789,71.5613924274766,
77.4338505153925));
#218104=CARTESIAN_POINT('Ctrl Pts',(-57.9393667804499,68.0943575771148,
78.7137716903922));
#218105=CARTESIAN_POINT('Ctrl Pts',(-57.8234863049199,64.4028215894282,
78.5374455169307));
#218106=CARTESIAN_POINT('Ctrl Pts',(-57.7076058293909,61.0735632819335,
76.9328994783959));
#218107=CARTESIAN_POINT('Ctrl Pts',(-57.5917253538619,58.6357765347184,
74.1551801543823));
#218108=CARTESIAN_POINT('Ctrl Pts',(-57.4758448783329,57.4769536083849,
70.6458129331832));
#218109=CARTESIAN_POINT('Ctrl Pts',(-57.3599644028029,57.7812922863604,
66.9626204542406));
#218110=CARTESIAN_POINT('Ctrl Pts',(-57.2440839272739,59.5004171796032,
63.6910553136322));
#218111=CARTESIAN_POINT('Ctrl Pts',(-57.1282034517449,62.3610691148619,
61.3511409192107));
#218112=CARTESIAN_POINT('Ctrl Pts',(-57.0123229762159,65.908540359229,60.3148124779815));
#218113=CARTESIAN_POINT('Ctrl Pts',(-56.8964425006869,69.5789515441067,
60.7467969703095));
#218114=CARTESIAN_POINT('Ctrl Pts',(-56.7805620251579,72.7888816918543,
62.5784293889601));
#218115=CARTESIAN_POINT('Ctrl Pts',(-56.6646815496279,75.0281044299382,
65.5185672056338));
#218116=CARTESIAN_POINT('Ctrl Pts',(-56.5488010740989,75.9406897400636,
69.0998682252856));
#218117=CARTESIAN_POINT('Ctrl Pts',(-56.4329205985699,75.3815799209528,
72.7530756919932));
#218118=CARTESIAN_POINT('Ctrl Pts',(-56.3170401230409,73.439646862909,75.8975034275876));
#218119=CARTESIAN_POINT('Ctrl Pts',(-56.2011596475119,70.4235656679413,
78.0333359882836));
#218120=CARTESIAN_POINT('Ctrl Pts',(-56.0852791719829,66.81274987119,78.8210806253173));
#218121=CARTESIAN_POINT('Ctrl Pts',(-55.9693986964549,63.1811478570336,
78.1355116392275));
#218122=CARTESIAN_POINT('Ctrl Pts',(-55.8535182209259,60.1060108866471,
76.0856457086154));
#218123=CARTESIAN_POINT('Ctrl Pts',(-55.7376377453969,58.0761429897366,
72.9971507091326));
#218124=CARTESIAN_POINT('Ctrl Pts',(-55.6603840950439,57.6348370927523,
70.5734238624516));
#218125=CARTESIAN_POINT('Ctrl Pts',(-55.6217572698679,57.6597134706593,
69.3663129168428));
#218126=CARTESIAN_POINT('',(-63.5337774910882,56.4405479536543,69.9703292528641));
#218127=CARTESIAN_POINT('',(-63.5337571161032,56.4405871136771,69.9703282277341));
#218128=CARTESIAN_POINT('Ctrl Pts',(-63.5337978660731,56.4405087936315,
69.970330277994));
#218129=CARTESIAN_POINT('Ctrl Pts',(-63.5202231218634,56.4206513278838,
69.4838986812489));
#218130=CARTESIAN_POINT('Ctrl Pts',(-63.5066190833876,56.4354746233135,
68.9966731918193));
#218131=CARTESIAN_POINT('Ctrl Pts',(-63.4794168880834,56.5330349183312,
68.0400039530818));
#218132=CARTESIAN_POINT('Ctrl Pts',(-63.465861497201,56.6139662085722,67.5715749189794));
#218133=CARTESIAN_POINT('Ctrl Pts',(-63.425565687372,56.9527669983538,66.1903259139352));
#218134=CARTESIAN_POINT('Ctrl Pts',(-63.3996267041034,57.3049409708213,
65.3059259002616));
#218135=CARTESIAN_POINT('Ctrl Pts',(-63.3570313944311,58.048595780408,63.9991853257494));
#218136=CARTESIAN_POINT('Ctrl Pts',(-63.3411184424965,58.3625411606416,
63.539031567641));
#218137=CARTESIAN_POINT('Ctrl Pts',(-63.3110423001554,59.0356488652194,
62.7067648440937));
#218138=CARTESIAN_POINT('Ctrl Pts',(-63.2968122207668,59.3886727116809,
62.3318121573921));
#218139=CARTESIAN_POINT('Ctrl Pts',(-63.2645159255659,60.2394786389348,
61.5544994963403));
#218140=CARTESIAN_POINT('Ctrl Pts',(-63.2463846911154,60.7497831421837,
61.1690009106554));
#218141=CARTESIAN_POINT('Ctrl Pts',(-63.2103027884577,61.8298654770057,
60.5013647330321));
#218142=CARTESIAN_POINT('Ctrl Pts',(-63.1927714244286,62.3966764148673,
60.2196342170887));
#218143=CARTESIAN_POINT('Ctrl Pts',(-63.1567815091212,63.5980703290134,
59.7551586861337));
#218144=CARTESIAN_POINT('Ctrl Pts',(-63.1382325648421,64.2316566098064,
59.577812813029));
#218145=CARTESIAN_POINT('Ctrl Pts',(-63.0876061050843,65.9835571276424,
59.2645618345226));
#218146=CARTESIAN_POINT('Ctrl Pts',(-63.0568645631276,67.1143060400938,
59.2499479601664));
#218147=CARTESIAN_POINT('Ctrl Pts',(-63.005891965054,68.8928844070064,59.5207399612207));
#218148=CARTESIAN_POINT('Ctrl Pts',(-62.9865902405449,69.5492990432607,
59.6882858783912));
#218149=CARTESIAN_POINT('Ctrl Pts',(-62.9488489080176,70.8186997677901,
60.1498250157125));
#218150=CARTESIAN_POINT('Ctrl Pts',(-62.9301167844335,71.4286371594735,
60.4425142523593));
#218151=CARTESIAN_POINT('Ctrl Pts',(-62.8963763793845,72.4470147332593,
61.0614295219787));
#218152=CARTESIAN_POINT('Ctrl Pts',(-62.8816004439642,72.8677289241764,
61.3628567478541));
#218153=CARTESIAN_POINT('Ctrl Pts',(-62.8576637723445,73.5180351319628,
61.9075921696466));
#218154=CARTESIAN_POINT('Ctrl Pts',(-62.8484332830644,73.7616829155249,
62.132664553432));
#218155=CARTESIAN_POINT('Ctrl Pts',(-62.8014970604723,74.9411857777908,
63.3333367980829));
#218156=CARTESIAN_POINT('Ctrl Pts',(-62.7630176062056,75.6883752126844,
64.4754208690331));
#218157=CARTESIAN_POINT('Ctrl Pts',(-62.6903484747373,76.6602419101073,
66.8932985386122));
#218158=CARTESIAN_POINT('Ctrl Pts',(-62.6545794831604,76.9104611156789,
68.1331288680544));
#218159=CARTESIAN_POINT('Ctrl Pts',(-62.6006820311669,76.9415153841524,
70.0621434233975));
#218160=CARTESIAN_POINT('Ctrl Pts',(-62.5819408139266,76.8856908376953,
70.7364519076855));
#218161=CARTESIAN_POINT('Ctrl Pts',(-62.5436946277216,76.642179247713,72.0648786987987));
#218162=CARTESIAN_POINT('Ctrl Pts',(-62.5243815110003,76.4549659444319,
72.7157337662098));
#218163=CARTESIAN_POINT('Ctrl Pts',(-62.5042594192214,76.1887426466089,
73.3844628512366));
#218164=CARTESIAN_POINT('Ctrl Pts',(-62.5030257008656,76.1721423876946,
73.4253892597614));
#218165=CARTESIAN_POINT('Ctrl Pts',(-62.5017927901887,76.1552807340937,
73.4662010514616));
#218166=CARTESIAN_POINT('',(-56.402655786563,57.5592983598715,74.2253115652726));
#218167=CARTESIAN_POINT('Ctrl Pts',(-56.5793858481529,60.8283504752015,
78.0464295027996));
#218168=CARTESIAN_POINT('Ctrl Pts',(-56.5407590229759,59.6918928073868,
77.2632582583922));
#218169=CARTESIAN_POINT('Ctrl Pts',(-56.4635053726229,57.7381457991904,
75.2350099031933));
#218170=CARTESIAN_POINT('Ctrl Pts',(-56.3476248970939,56.2287169260511,
71.289035799845));
#218171=CARTESIAN_POINT('Ctrl Pts',(-56.2317444215639,56.3809813114179,
67.0670781799153));
#218172=CARTESIAN_POINT('Ctrl Pts',(-56.1158639460339,58.1705823100065,
63.2401216789652));
#218173=CARTESIAN_POINT('Ctrl Pts',(-55.9999834705049,61.313099618598,60.4164989490926));
#218174=CARTESIAN_POINT('Ctrl Pts',(-55.8841029949749,65.30901125743,59.0450242272283));
#218175=CARTESIAN_POINT('Ctrl Pts',(-55.7682225194459,69.5231601025766,
59.3436988676508));
#218176=CARTESIAN_POINT('Ctrl Pts',(-55.6523420439159,73.2856959312731,
61.2650472476525));
#218177=CARTESIAN_POINT('Ctrl Pts',(-55.5364615683869,75.9985545373602,
64.5036664147486));
#218178=CARTESIAN_POINT('Ctrl Pts',(-55.4205810928579,77.2305202478881,
68.5447697661598));
#218179=CARTESIAN_POINT('Ctrl Pts',(-55.3047006173279,76.7857690673864,
72.746013893864));
#218180=CARTESIAN_POINT('Ctrl Pts',(-55.1888201417989,74.7349952969698,
76.4396006022122));
#218181=CARTESIAN_POINT('Ctrl Pts',(-55.0729396662689,71.4041745240506,
79.0384251072975));
#218182=CARTESIAN_POINT('Ctrl Pts',(-54.9570591907399,67.3227489862028,
80.1293977965976));
#218183=CARTESIAN_POINT('Ctrl Pts',(-54.8411787152099,63.1394714137716,
79.5391058504835));
#218184=CARTESIAN_POINT('Ctrl Pts',(-54.7252982396809,59.5192841709575,
77.3613776404707));
#218185=CARTESIAN_POINT('Ctrl Pts',(-54.6094177641509,57.0376250150175,
73.9423684764854));
#218186=CARTESIAN_POINT('Ctrl Pts',(-54.4935372886209,56.0889598348911,
69.8255383602719));
#218187=CARTESIAN_POINT('Ctrl Pts',(-54.3776568130909,56.8240813181107,
65.6652676678047));
#218188=CARTESIAN_POINT('Ctrl Pts',(-54.2617763375609,59.1261400783554,
62.1228417625685));
#218189=CARTESIAN_POINT('Ctrl Pts',(-54.1458958620309,62.6292181558182,
59.7613380439862));
#218190=CARTESIAN_POINT('Ctrl Pts',(-54.0300153865009,66.776492586088,58.9561233957071));
#218191=CARTESIAN_POINT('Ctrl Pts',(-53.9141349109709,70.9087437938121,
59.8351886867614));
#218192=CARTESIAN_POINT('Ctrl Pts',(-53.7982544354409,74.3691401822294,
62.258804304951));
#218193=CARTESIAN_POINT('Ctrl Pts',(-53.6823739599209,76.6076431474328,
65.8417305258611));
#218194=CARTESIAN_POINT('Ctrl Pts',(-53.5664934843909,77.2684370811464,
70.014452324264));
#218195=CARTESIAN_POINT('Ctrl Pts',(-53.4506130088609,76.2464871457476,
74.1137052024411));
#218196=CARTESIAN_POINT('Ctrl Pts',(-53.3347325333309,73.7042348226836,
77.487902730087));
#218197=CARTESIAN_POINT('Ctrl Pts',(-53.2188520578009,70.0457774353802,
79.6007078263948));
#218198=CARTESIAN_POINT('Ctrl Pts',(-53.1029715822709,65.8526358756345,
80.1162848716646));
#218199=CARTESIAN_POINT('Ctrl Pts',(-52.9870911067409,61.7913204129621,
78.9526816135228));
#218200=CARTESIAN_POINT('Ctrl Pts',(-52.8712106312109,58.5073872312147,
76.2948556810079));
#218201=CARTESIAN_POINT('Ctrl Pts',(-52.7553301556809,56.522825669145,72.5652751099482));
#218202=CARTESIAN_POINT('Ctrl Pts',(-52.6394496801509,56.15308671803,68.356765998908));
#218203=CARTESIAN_POINT('Ctrl Pts',(-52.5235692046209,57.4569413028341,
64.3382813278711));
#218204=CARTESIAN_POINT('Ctrl Pts',(-52.4076887290909,60.2271384976534,
61.1485692199367));
#218205=CARTESIAN_POINT('Ctrl Pts',(-52.2918082535609,64.0233485753049,
59.2946423400516));
#218206=CARTESIAN_POINT('Ctrl Pts',(-52.1759277780309,68.2421545116176,
59.0711869721972));
#218207=CARTESIAN_POINT('Ctrl Pts',(-52.0600473025109,72.2129666206316,
60.5137219022862));
#218208=CARTESIAN_POINT('Ctrl Pts',(-51.9441668269809,75.3046144514435,
63.3929526189662));
#218209=CARTESIAN_POINT('Ctrl Pts',(-51.8282863514509,77.0256728996043,
67.2512182458574));
#218210=CARTESIAN_POINT('Ctrl Pts',(-51.7124058759209,77.1025754485052,
71.4752378750256));
#218211=CARTESIAN_POINT('Ctrl Pts',(-51.5965254003909,75.5230982469212,
75.3935930910952));
#218212=CARTESIAN_POINT('Ctrl Pts',(-51.4806449248609,72.5383031205348,
78.3834515966281));
#218213=CARTESIAN_POINT('Ctrl Pts',(-51.3647644493309,68.6226306709332,
79.9695679533436));
#218214=CARTESIAN_POINT('Ctrl Pts',(-51.2488839738009,64.3984867631581,
79.8998250253566));
#218215=CARTESIAN_POINT('Ctrl Pts',(-51.1330034982709,60.537309566982,78.1853086243629));
#218216=CARTESIAN_POINT('Ctrl Pts',(-51.0171230227409,57.6528427914971,
75.0985453923105));
#218217=CARTESIAN_POINT('Ctrl Pts',(-50.9012425472109,56.2035795976409,
71.1301840145486));
#218218=CARTESIAN_POINT('Ctrl Pts',(-50.7853620716809,56.4198839710304,
66.9110053921681));
#218219=CARTESIAN_POINT('Ctrl Pts',(-50.6694815961509,58.2673737940418,
63.111658450455));
#218220=CARTESIAN_POINT('Ctrl Pts',(-50.5536011206309,61.4523859689387,
60.336058826028));
#218221=CARTESIAN_POINT('Ctrl Pts',(-50.4377206451009,65.4686548966643,
59.0253949753286));
#218222=CARTESIAN_POINT('Ctrl Pts',(-50.3218401695709,69.6777846525631,
59.3880001752186));
#218223=CARTESIAN_POINT('Ctrl Pts',(-50.2059596940409,73.4107236016189,
61.366237423659));
#218224=CARTESIAN_POINT('Ctrl Pts',(-50.0900792185109,76.0741118301684,
64.6456610117157));
#218225=CARTESIAN_POINT('Ctrl Pts',(-49.9741987429809,77.2445971339387,
68.7049983484055));
#218226=CARTESIAN_POINT('Ctrl Pts',(-49.8583182674509,76.7361280689603,
72.8990079143938));
#218227=CARTESIAN_POINT('Ctrl Pts',(-49.7424377919209,74.6295266708348,
76.5610405859094));
#218228=CARTESIAN_POINT('Ctrl Pts',(-49.6265573163909,71.2596439053081,
79.1090104644245));
#218229=CARTESIAN_POINT('Ctrl Pts',(-49.5106768408609,67.1621256395096,
80.1378991151167));
#218230=CARTESIAN_POINT('Ctrl Pts',(-49.3947963653309,62.9883026295467,
79.4842080039734));
#218231=CARTESIAN_POINT('Ctrl Pts',(-49.2789158898109,59.4015395979127,
77.2516717552151));
#218232=CARTESIAN_POINT('Ctrl Pts',(-49.2016622394509,57.7820069698283,
74.9477549101844));
#218233=CARTESIAN_POINT('Ctrl Pts',(-49.1630354142809,57.2293348468531,
73.6830625549967));
#218234=CARTESIAN_POINT('Ctrl Pts',(-56.3552577378769,61.0726603761865,
77.6919120683442));
#218235=CARTESIAN_POINT('Ctrl Pts',(-56.3166309126999,59.9836344637329,
76.9414276436267));
#218236=CARTESIAN_POINT('Ctrl Pts',(-56.2393772623469,58.1114300002093,
74.9978312579017));
#218237=CARTESIAN_POINT('Ctrl Pts',(-56.1234967868169,56.6649993918269,
71.2165482676822));
#218238=CARTESIAN_POINT('Ctrl Pts',(-56.0076163112879,56.8109087960282,
67.1708003444752));
#218239=CARTESIAN_POINT('Ctrl Pts',(-55.8917358357579,58.5258181284236,
63.5035675795475));
#218240=CARTESIAN_POINT('Ctrl Pts',(-55.7758553602289,61.5371777912702,
60.7977929546753));
#218241=CARTESIAN_POINT('Ctrl Pts',(-55.6599748846989,65.3663140994574,
59.4835587753602));
#218242=CARTESIAN_POINT('Ctrl Pts',(-55.5440944091699,69.4045791587436,
59.7697677843113));
#218243=CARTESIAN_POINT('Ctrl Pts',(-55.4282139336399,73.0100799442327,
61.6109258247082));
#218244=CARTESIAN_POINT('Ctrl Pts',(-55.3123334581109,75.6097133511933,
64.7143763916865));
#218245=CARTESIAN_POINT('Ctrl Pts',(-55.1964529825809,76.7902611357812,
68.58681826895));
#218246=CARTESIAN_POINT('Ctrl Pts',(-55.0805725070519,76.3640723089752,
72.612717208417));
#218247=CARTESIAN_POINT('Ctrl Pts',(-54.9646920315229,74.3988906398205,
76.152146567904));
#218248=CARTESIAN_POINT('Ctrl Pts',(-54.8488115559929,71.2070866385185,
78.6425052571067));
#218249=CARTESIAN_POINT('Ctrl Pts',(-54.7329310804639,67.2960054813953,
79.6879445744451));
#218250=CARTESIAN_POINT('Ctrl Pts',(-54.6170506049339,63.2873232362219,
79.1222893429069));
#218251=CARTESIAN_POINT('Ctrl Pts',(-54.5011701294009,59.8182299061273,
77.035451866986));
#218252=CARTESIAN_POINT('Ctrl Pts',(-54.3852896538709,57.4401464955149,
73.7591401486176));
#218253=CARTESIAN_POINT('Ctrl Pts',(-54.2694091783509,56.5310752712668,
69.8141320760029));
#218254=CARTESIAN_POINT('Ctrl Pts',(-54.1535287028209,57.235515363221,65.8274964843525));
#218255=CARTESIAN_POINT('Ctrl Pts',(-54.0376482272909,59.4414942684621,
62.4329190064619));
#218256=CARTESIAN_POINT('Ctrl Pts',(-53.9217677517609,62.7983661588541,
60.1699761668686));
#218257=CARTESIAN_POINT('Ctrl Pts',(-53.8058872762309,66.7725479066749,
59.398368352605));
#218258=CARTESIAN_POINT('Ctrl Pts',(-53.6900068007009,70.7323334485579,
60.2407445429475));
#218259=CARTESIAN_POINT('Ctrl Pts',(-53.5741263251709,74.0483050338323,
62.5632069494067));
#218260=CARTESIAN_POINT('Ctrl Pts',(-53.4582458496409,76.1933807399002,
65.9965944019083));
#218261=CARTESIAN_POINT('Ctrl Pts',(-53.3423653741109,76.8265954534646,
69.9951614340195));
#218262=CARTESIAN_POINT('Ctrl Pts',(-53.2264848985809,75.84729812247,73.9233258808397));
#218263=CARTESIAN_POINT('Ctrl Pts',(-53.1106044230509,73.4111504909153,
77.1566962433291));
#218264=CARTESIAN_POINT('Ctrl Pts',(-52.9947239475209,69.9053842778755,
79.1813202684909));
#218265=CARTESIAN_POINT('Ctrl Pts',(-52.8788434719909,65.8872497336091,
79.6753789369893));
#218266=CARTESIAN_POINT('Ctrl Pts',(-52.7629629964609,61.9954393276913,
78.5603403958908));
#218267=CARTESIAN_POINT('Ctrl Pts',(-52.6470825209309,58.8485659940342,
76.0134427918172));
#218268=CARTESIAN_POINT('Ctrl Pts',(-52.5312020454009,56.946833067975,72.4395218271453));
#218269=CARTESIAN_POINT('Ctrl Pts',(-52.4153215698809,56.5925257233132,
68.4066611192533));
#218270=CARTESIAN_POINT('Ctrl Pts',(-52.2994410943509,57.8419619928253,
64.5558938980169));
#218271=CARTESIAN_POINT('Ctrl Pts',(-52.1835606188209,60.4965408770102,
61.4993091811534));
#218272=CARTESIAN_POINT('Ctrl Pts',(-52.0676801432909,64.1343104664627,
59.7227587040345));
#218273=CARTESIAN_POINT('Ctrl Pts',(-51.9517996677609,68.1770382462698,
59.5086295791555));
#218274=CARTESIAN_POINT('Ctrl Pts',(-51.8359191922309,71.9821225909486,
60.8909581629449));
#218275=CARTESIAN_POINT('Ctrl Pts',(-51.7200387167009,74.9447358895156,
63.6500198923846));
#218276=CARTESIAN_POINT('Ctrl Pts',(-51.6041582411709,76.5939633970318,
67.3472550501956));
#218277=CARTESIAN_POINT('Ctrl Pts',(-51.4882777656409,76.6676563033805,
71.3949789216125));
#218278=CARTESIAN_POINT('Ctrl Pts',(-51.3723972901109,75.1541009379953,
75.1497957399931));
#218279=CARTESIAN_POINT('Ctrl Pts',(-51.2565168145809,72.2938806868999,
78.0148680425532));
#218280=CARTESIAN_POINT('Ctrl Pts',(-51.1406363390509,68.5416346657267,
79.534785468025));
#218281=CARTESIAN_POINT('Ctrl Pts',(-51.0247558635209,64.4937917026564,
79.4679533651302));
#218282=CARTESIAN_POINT('Ctrl Pts',(-50.9088753880009,60.7937664942429,
77.8249948626797));
#218283=CARTESIAN_POINT('Ctrl Pts',(-50.7929949124709,58.0296872407287,
74.8670622968579));
#218284=CARTESIAN_POINT('Ctrl Pts',(-50.6771144369409,56.6409112073073,
71.0643263985101));
#218285=CARTESIAN_POINT('Ctrl Pts',(-50.5612339614109,56.8481877951267,
67.0212414872383));
#218286=CARTESIAN_POINT('Ctrl Pts',(-50.4453534858809,58.6185698755448,
63.3804659554293));
#218287=CARTESIAN_POINT('Ctrl Pts',(-50.3294730103509,61.6706508180947,
60.7207101200916));
#218288=CARTESIAN_POINT('Ctrl Pts',(-50.2135925348209,65.5192947733674,
59.4647487795595));
#218289=CARTESIAN_POINT('Ctrl Pts',(-50.0977120592909,69.552750222577,59.8122201107395));
#218290=CARTESIAN_POINT('Ctrl Pts',(-49.9818315837609,73.1298893983293,
61.7078926778295));
#218291=CARTESIAN_POINT('Ctrl Pts',(-49.8659511082309,75.6821171477224,
64.8504446324208));
#218292=CARTESIAN_POINT('Ctrl Pts',(-49.7500706327009,76.8037505020027,
68.7403594723971));
#218293=CARTESIAN_POINT('Ctrl Pts',(-49.6341901571709,76.3165031516394,
72.7593257953695));
#218294=CARTESIAN_POINT('Ctrl Pts',(-49.5183096816509,74.2978239040633,
76.2685180728018));
#218295=CARTESIAN_POINT('Ctrl Pts',(-49.4024292061209,71.0685882206619,
78.7101446291031));
#218296=CARTESIAN_POINT('Ctrl Pts',(-49.2865487305909,67.1420859895845,
79.6960910777589));
#218297=CARTESIAN_POINT('Ctrl Pts',(-49.1706682550609,63.1424637066209,
79.0696827398739));
#218298=CARTESIAN_POINT('Ctrl Pts',(-49.0547877795309,59.7053995784171,
76.9303247204408));
#218299=CARTESIAN_POINT('Ctrl Pts',(-48.9775341291809,58.1534605594795,
74.7225652803545));
#218300=CARTESIAN_POINT('Ctrl Pts',(-48.9389073040009,57.6238550316623,
73.5106567464228));
#218301=CARTESIAN_POINT('Ctrl Pts',(-56.1311296275999,61.3169702771804,
77.3373946338935));
#218302=CARTESIAN_POINT('Ctrl Pts',(-56.0925028024239,60.2753761200882,
76.619597028865));
#218303=CARTESIAN_POINT('Ctrl Pts',(-56.0152491520709,58.4847142012186,
74.7606526126071));
#218304=CARTESIAN_POINT('Ctrl Pts',(-55.8993686765409,57.1012818576024,
71.1440607355204));
#218305=CARTESIAN_POINT('Ctrl Pts',(-55.7834882010119,57.2408362806385,
67.2745225090351));
#218306=CARTESIAN_POINT('Ctrl Pts',(-55.6676077254819,58.8810539468492,
63.7670134801353));
#218307=CARTESIAN_POINT('Ctrl Pts',(-55.5517272499529,61.7612559639331,
61.1790869602541));
#218308=CARTESIAN_POINT('Ctrl Pts',(-55.4358467744229,65.4236169414932,
59.9220933234976));
#218309=CARTESIAN_POINT('Ctrl Pts',(-55.3199662988939,69.2859982149144,
60.1958367009625));
#218310=CARTESIAN_POINT('Ctrl Pts',(-55.2040858233639,72.7344639571905,
61.9568044017577));
#218311=CARTESIAN_POINT('Ctrl Pts',(-55.0882053478349,75.2208721650242,
64.9250863686192));
#218312=CARTESIAN_POINT('Ctrl Pts',(-54.9723248723049,76.3500020236737,
68.6288667717324));
#218313=CARTESIAN_POINT('Ctrl Pts',(-54.8564443967759,75.9423755505674,
72.4794205229619));
#218314=CARTESIAN_POINT('Ctrl Pts',(-54.7405639212469,74.0627859826778,
75.8646925335889));
#218315=CARTESIAN_POINT('Ctrl Pts',(-54.6246834457169,71.0099987529967,
78.2465854069094));
#218316=CARTESIAN_POINT('Ctrl Pts',(-54.5088029701909,67.2692619766016,
79.2464913522907));
#218317=CARTESIAN_POINT('Ctrl Pts',(-54.3929224946609,63.4351750586927,
78.7054728353225));
#218318=CARTESIAN_POINT('Ctrl Pts',(-54.2770420191309,60.1171756413221,
76.7095260935192));
#218319=CARTESIAN_POINT('Ctrl Pts',(-54.1611615436009,57.8426679760259,
73.5759118207695));
#218320=CARTESIAN_POINT('Ctrl Pts',(-54.0452810680709,56.973190707635,69.8027257917525));
#218321=CARTESIAN_POINT('Ctrl Pts',(-53.9294005925409,57.6469494083309,
65.9897253009273));
#218322=CARTESIAN_POINT('Ctrl Pts',(-53.8135201170109,59.7568484585497,
62.7429962503755));
#218323=CARTESIAN_POINT('Ctrl Pts',(-53.6976396414809,62.9675141618542,
60.5786142897589));
#218324=CARTESIAN_POINT('Ctrl Pts',(-53.5817591659509,66.7686032272295,
59.8406133095026));
#218325=CARTESIAN_POINT('Ctrl Pts',(-53.4658786904209,70.5559231032727,
60.6463003991197));
#218326=CARTESIAN_POINT('Ctrl Pts',(-53.3499982148909,73.7274698854091,
62.8676095938364));
#218327=CARTESIAN_POINT('Ctrl Pts',(-53.2341177393609,75.7791183323543,
66.1514582779196));
#218328=CARTESIAN_POINT('Ctrl Pts',(-53.1182372638309,76.3847538257845,
69.9758705437336));
#218329=CARTESIAN_POINT('Ctrl Pts',(-53.0023567883009,75.4481090992107,
73.7329465591993));
#218330=CARTESIAN_POINT('Ctrl Pts',(-52.8864763127809,73.1180661591807,
76.8254897565408));
#218331=CARTESIAN_POINT('Ctrl Pts',(-52.7705958372509,69.7649911204159,
78.7619327105721));
#218332=CARTESIAN_POINT('Ctrl Pts',(-52.6547153617209,65.9218635916335,
79.2344730023141));
#218333=CARTESIAN_POINT('Ctrl Pts',(-52.5388348861909,62.1995582424626,
78.1679991782881));
#218334=CARTESIAN_POINT('Ctrl Pts',(-52.4229544106609,59.1897447568815,
75.7320299026639));
#218335=CARTESIAN_POINT('Ctrl Pts',(-52.3070739351309,57.3708404668259,
72.3137685443966));
#218336=CARTESIAN_POINT('Ctrl Pts',(-52.1911934596009,57.0319647285943,
68.4565562396562));
#218337=CARTESIAN_POINT('Ctrl Pts',(-52.0753129840709,58.2269826827762,
64.7735064682079));
#218338=CARTESIAN_POINT('Ctrl Pts',(-51.9594325085409,60.7659432563194,
61.8500491424068));
#218339=CARTESIAN_POINT('Ctrl Pts',(-51.8435520330109,64.2452723575601,
60.1508750680324));
#218340=CARTESIAN_POINT('Ctrl Pts',(-51.7276715574809,68.1119219808598,
59.9460721861075));
#218341=CARTESIAN_POINT('Ctrl Pts',(-51.6117910819509,71.7512785612103,
61.2681944235776));
#218342=CARTESIAN_POINT('Ctrl Pts',(-51.4959106064209,74.5848573275517,
63.9070871657535));
#218343=CARTESIAN_POINT('Ctrl Pts',(-51.3800301308909,76.162253894446,67.4432918544721));
#218344=CARTESIAN_POINT('Ctrl Pts',(-51.2641496553709,76.2327371582677,
71.3147199681373));
#218345=CARTESIAN_POINT('Ctrl Pts',(-51.1482691798409,74.7851036291041,
74.9059983888393));
#218346=CARTESIAN_POINT('Ctrl Pts',(-51.0323887043109,72.0494582533171,
77.6462844884435));
#218347=CARTESIAN_POINT('Ctrl Pts',(-50.9165082287809,68.4606386605805,
79.1000029826967));
#218348=CARTESIAN_POINT('Ctrl Pts',(-50.8006277532509,64.5890966422126,
79.0360817049179));
#218349=CARTESIAN_POINT('Ctrl Pts',(-50.6847472777209,61.0502234215632,
77.4646811010362));
#218350=CARTESIAN_POINT('Ctrl Pts',(-50.5688668021909,58.4065316900025,
74.6355792014605));
#218351=CARTESIAN_POINT('Ctrl Pts',(-50.4529863266609,57.0782428169735,
70.9984687825245));
#218352=CARTESIAN_POINT('Ctrl Pts',(-50.3371058511309,57.2764916192201,
67.1314775823678));
#218353=CARTESIAN_POINT('Ctrl Pts',(-50.2212253756009,58.9697659570288,
63.6492734604498));
#218354=CARTESIAN_POINT('Ctrl Pts',(-50.1053449000709,61.8889156671989,
61.105361414176));
#218355=CARTESIAN_POINT('Ctrl Pts',(-49.9894644245409,65.5699346500343,
59.9041025837992));
#218356=CARTESIAN_POINT('Ctrl Pts',(-49.8735839490209,69.4277157925497,
60.2364400462553));
#218357=CARTESIAN_POINT('Ctrl Pts',(-49.7577034734909,72.8490551950089,
62.0495479319754));
#218358=CARTESIAN_POINT('Ctrl Pts',(-49.6418229979609,75.2901224652598,
65.055228253093));
#218359=CARTESIAN_POINT('Ctrl Pts',(-49.5259425224309,76.3629038700644,
68.7757205963566));
#218360=CARTESIAN_POINT('Ctrl Pts',(-49.4100620469009,75.8968782343272,
72.6196436763185));
#218361=CARTESIAN_POINT('Ctrl Pts',(-49.2941815713709,73.9661211373074,
75.9759955596767));
#218362=CARTESIAN_POINT('Ctrl Pts',(-49.1783010958409,70.8775325360307,
78.3112787937738));
#218363=CARTESIAN_POINT('Ctrl Pts',(-49.0624206203109,67.1220463396723,
79.254283040401));
#218364=CARTESIAN_POINT('Ctrl Pts',(-48.9465401447809,63.2966247837026,
78.6551574757722));
#218365=CARTESIAN_POINT('Ctrl Pts',(-48.8306596692509,60.0092595589126,
76.6089776856617));
#218366=CARTESIAN_POINT('Ctrl Pts',(-48.7534060189009,58.5249141491315,
74.4973756505227));
#218367=CARTESIAN_POINT('Ctrl Pts',(-48.7147791937209,58.0183752164734,
73.3382509378444));
#218368=CARTESIAN_POINT('Ctrl Pts',(-55.9070015173239,61.5612801781646,
76.9828771994399));
#218369=CARTESIAN_POINT('Ctrl Pts',(-55.8683746921479,60.5671177764436,
76.2977664141033));
#218370=CARTESIAN_POINT('Ctrl Pts',(-55.7911210417949,58.8579984022376,
74.5234739673154));
#218371=CARTESIAN_POINT('Ctrl Pts',(-55.6752405662649,57.5375643233782,
71.0715732033576));
#218372=CARTESIAN_POINT('Ctrl Pts',(-55.5593600907359,57.67076376524,67.3782446735902));
#218373=CARTESIAN_POINT('Ctrl Pts',(-55.4434796152059,59.2362897652659,
64.0304593807185));
#218374=CARTESIAN_POINT('Ctrl Pts',(-55.3275991396769,61.9853341366056,
61.5603809658357));
#218375=CARTESIAN_POINT('Ctrl Pts',(-55.2117186641469,65.4809197835205,
60.3606278716295));
#218376=CARTESIAN_POINT('Ctrl Pts',(-55.0958381886179,69.1674172710837,
60.6219056176175));
#218377=CARTESIAN_POINT('Ctrl Pts',(-54.9799577130879,72.4588479701517,
62.3026829788097));
#218378=CARTESIAN_POINT('Ctrl Pts',(-54.8640772375589,74.8320309788573,
65.135796345557));
#218379=CARTESIAN_POINT('Ctrl Pts',(-54.7481967620289,75.9097429115672,
68.6709152745216));
#218380=CARTESIAN_POINT('Ctrl Pts',(-54.6323162864999,75.5206787921568,
72.3461238375152));
#218381=CARTESIAN_POINT('Ctrl Pts',(-54.5164358109709,73.7266813255289,
75.5772384992809));
#218382=CARTESIAN_POINT('Ctrl Pts',(-54.4005553354409,70.8129108674647,
77.8506655567186));
#218383=CARTESIAN_POINT('Ctrl Pts',(-54.2846748599109,67.2425184717931,
78.8050381301378));
#218384=CARTESIAN_POINT('Ctrl Pts',(-54.1687943843809,63.5830268811459,
78.2886563277363));
#218385=CARTESIAN_POINT('Ctrl Pts',(-54.0529139088509,60.4161213764918,
76.3836003200345));
#218386=CARTESIAN_POINT('Ctrl Pts',(-53.9370334333209,58.2451894565326,
73.3926834929056));
#218387=CARTESIAN_POINT('Ctrl Pts',(-53.8211529577909,57.4153061440108,
69.7913195074836));
#218388=CARTESIAN_POINT('Ctrl Pts',(-53.7052724822609,58.0583834534414,
66.1519541174747));
#218389=CARTESIAN_POINT('Ctrl Pts',(-53.5893920067309,60.0722026486568,
63.0530734942681));
#218390=CARTESIAN_POINT('Ctrl Pts',(-53.4735115312009,63.1366621648809,
60.9872524126374));
#218391=CARTESIAN_POINT('Ctrl Pts',(-53.3576310556809,66.7646585478257,
60.2828582664043));
#218392=CARTESIAN_POINT('Ctrl Pts',(-53.2417505801509,70.3795127580189,
61.0518562553049));
#218393=CARTESIAN_POINT('Ctrl Pts',(-53.1258701046209,73.4066347370121,
63.172012238292));
#218394=CARTESIAN_POINT('Ctrl Pts',(-53.0099896290909,75.3648559248227,
66.3063221539671));
#218395=CARTESIAN_POINT('Ctrl Pts',(-52.8941091535609,75.9429121981029,
69.9565796534893));
#218396=CARTESIAN_POINT('Ctrl Pts',(-52.7782286780309,75.0489200759327,
73.5425672375986));
#218397=CARTESIAN_POINT('Ctrl Pts',(-52.6623482025009,72.8249818274116,
76.4942832697837));
#218398=CARTESIAN_POINT('Ctrl Pts',(-52.5464677269709,69.6245979629103,
78.3425451526678));
#218399=CARTESIAN_POINT('Ctrl Pts',(-52.4305872514409,65.9564774496083,
78.7935670676356));
#218400=CARTESIAN_POINT('Ctrl Pts',(-52.3147067759109,62.4036771571881,
77.77565796066));
#218401=CARTESIAN_POINT('Ctrl Pts',(-52.1988263003809,59.5309235196917,
75.4506170134694));
#218402=CARTESIAN_POINT('Ctrl Pts',(-52.0829458248509,57.7948478656563,
72.1880152615929));
#218403=CARTESIAN_POINT('Ctrl Pts',(-51.9670653493209,57.4714037338775,
68.5064513600016));
#218404=CARTESIAN_POINT('Ctrl Pts',(-51.8511848737909,58.6120033727586,
64.991119038349));
#218405=CARTESIAN_POINT('Ctrl Pts',(-51.7353043982609,61.0353456356765,
62.2007891036227));
#218406=CARTESIAN_POINT('Ctrl Pts',(-51.6194239227409,64.356234248718,60.5789914320152));
#218407=CARTESIAN_POINT('Ctrl Pts',(-51.5035434472109,68.0468057155105,
60.3835147930695));
#218408=CARTESIAN_POINT('Ctrl Pts',(-51.3876629716809,71.520434531528,61.6454306842399));
#218409=CARTESIAN_POINT('Ctrl Pts',(-51.2717824961509,74.2249787656239,
64.164154439174));
#218410=CARTESIAN_POINT('Ctrl Pts',(-51.1559020206209,75.7305443918741,
67.5393286588116));
#218411=CARTESIAN_POINT('Ctrl Pts',(-51.0400215450909,75.7978180131431,
71.2344610147253));
#218412=CARTESIAN_POINT('Ctrl Pts',(-50.9241410695609,74.4161063201778,
74.6622010377381));
#218413=CARTESIAN_POINT('Ctrl Pts',(-50.8082605940309,71.8050358196814,
77.2777009343682));
#218414=CARTESIAN_POINT('Ctrl Pts',(-50.6923801185009,68.3796426553727,
78.6652204973787));
#218415=CARTESIAN_POINT('Ctrl Pts',(-50.5764996429709,64.6844015817095,
78.604210044692));
#218416=CARTESIAN_POINT('Ctrl Pts',(-50.4606191674409,61.3066803488238,
77.1043673393539));
#218417=CARTESIAN_POINT('Ctrl Pts',(-50.3447386919109,58.7833761392345,
74.4040961060069));
#218418=CARTESIAN_POINT('Ctrl Pts',(-50.2288582163809,57.515574426631,70.9326111664812));
#218419=CARTESIAN_POINT('Ctrl Pts',(-50.1129777408609,57.7047954433261,
67.2417136774408));
#218420=CARTESIAN_POINT('Ctrl Pts',(-49.9970972653309,59.3209620385326,
63.9180809654223));
#218421=CARTESIAN_POINT('Ctrl Pts',(-49.8812167898009,62.107180516346,61.4900127082349));
#218422=CARTESIAN_POINT('Ctrl Pts',(-49.7653363142709,65.6205745267381,
60.3434563880283));
#218423=CARTESIAN_POINT('Ctrl Pts',(-49.6494558387409,69.3026813625722,
60.6606599817841));
#218424=CARTESIAN_POINT('Ctrl Pts',(-49.5335753632109,72.5682209917208,
62.3912031861476));
#218425=CARTESIAN_POINT('Ctrl Pts',(-49.4176948876809,74.8981277828147,
65.2600118737985));
#218426=CARTESIAN_POINT('Ctrl Pts',(-49.3018144121509,75.9220572381282,
68.8110817203493));
#218427=CARTESIAN_POINT('Ctrl Pts',(-49.1859339366209,75.4772533170059,
72.4799615572945));
#218428=CARTESIAN_POINT('Ctrl Pts',(-49.0700534610909,73.634418370535,75.6834730465697));
#218429=CARTESIAN_POINT('Ctrl Pts',(-48.9541729855609,70.6864768513839,
77.9124129584511));
#218430=CARTESIAN_POINT('Ctrl Pts',(-48.8382925100409,67.1020066897472,
78.8124750030432));
#218431=CARTESIAN_POINT('Ctrl Pts',(-48.7224120345109,63.4507858607777,
78.2406322116709));
#218432=CARTESIAN_POINT('Ctrl Pts',(-48.6065315589809,60.313119539417,76.2876306508875));
#218433=CARTESIAN_POINT('Ctrl Pts',(-48.5292779086209,58.896367738792,74.2721860206966));
#218434=CARTESIAN_POINT('Ctrl Pts',(-48.4906510834509,58.4128954012822,
73.1658451292715));
#218435=CARTESIAN_POINT('Ctrl Pts',(-49.2716875596105,60.362314694705,77.6221314644388));
#218436=CARTESIAN_POINT('Ctrl Pts',(-49.1710276021328,60.4814587922915,
77.4698472472393));
#218437=CARTESIAN_POINT('Ctrl Pts',(-49.0703675292835,60.6006070147117,
77.3175659697655));
#218438=CARTESIAN_POINT('Ctrl Pts',(-48.8698648784283,60.8379437239874,
77.01424632034));
#218439=CARTESIAN_POINT('Ctrl Pts',(-48.7700220760568,60.9561324122244,
76.8632075588121));
#218440=CARTESIAN_POINT('Ctrl Pts',(-48.6701794005812,61.0743248382571,
76.7121720277662));
#218441=CARTESIAN_POINT('Ctrl Pts',(-49.3172045433909,60.6595417501922,
77.9029428178256));
#218442=CARTESIAN_POINT('Ctrl Pts',(-49.2671675200609,59.1615528419803,
76.9294625104546));
#218443=CARTESIAN_POINT('Ctrl Pts',(-49.1670934734009,56.6466762806369,
74.1587488145408));
#218444=CARTESIAN_POINT('Ctrl Pts',(-49.0169824034109,55.4130069209437,
68.5383989146951));
#218445=CARTESIAN_POINT('Ctrl Pts',(-48.8668713334209,57.1841073201011,
62.9167841918779));
#218446=CARTESIAN_POINT('Ctrl Pts',(-48.7667972867609,60.1408900588271,
60.1918250007294));
#218447=CARTESIAN_POINT('Ctrl Pts',(-48.7167602634309,61.8842256853186,
59.2817848695541));
#218448=CARTESIAN_POINT('Ctrl Pts',(-49.0930764331109,60.9113854019325,
77.5537369843529));
#218449=CARTESIAN_POINT('Ctrl Pts',(-49.0430394097809,59.4739188100978,
76.6239047484312));
#218450=CARTESIAN_POINT('Ctrl Pts',(-48.9429653631309,57.0567877266815,
73.9726075199027));
#218451=CARTESIAN_POINT('Ctrl Pts',(-48.7928542931309,55.8614156728147,
68.5806263247324));
#218452=CARTESIAN_POINT('Ctrl Pts',(-48.6427432231409,57.5522584141988,
63.176215785295));
#218453=CARTESIAN_POINT('Ctrl Pts',(-48.5426691764809,60.390720514573,60.5503257501769));
#218454=CARTESIAN_POINT('Ctrl Pts',(-48.4926321531609,62.0664492882006,
59.6718675500255));
#218455=CARTESIAN_POINT('Ctrl Pts',(-48.8689483228409,61.1632290536717,
77.204531150883));
#218456=CARTESIAN_POINT('Ctrl Pts',(-48.8189112995109,59.7862847782248,
76.3183469864108));
#218457=CARTESIAN_POINT('Ctrl Pts',(-48.7188372528509,57.4668991727264,
73.7864662252636));
#218458=CARTESIAN_POINT('Ctrl Pts',(-48.5687261828609,56.3098244246853,
68.6228537347707));
#218459=CARTESIAN_POINT('Ctrl Pts',(-48.4186151128609,57.9204095082861,
63.4356473787112));
#218460=CARTESIAN_POINT('Ctrl Pts',(-48.3185410662109,60.6405509703189,
60.9088264996243));
#218461=CARTESIAN_POINT('Ctrl Pts',(-48.2685040428809,62.2486728910826,
60.0619502304968));
#218462=CARTESIAN_POINT('Ctrl Pts',(-48.6448202125609,61.4150727054204,
76.8553253174161));
#218463=CARTESIAN_POINT('Ctrl Pts',(-48.5947831892309,60.0986507463515,
76.0127892243912));
#218464=CARTESIAN_POINT('Ctrl Pts',(-48.4947091425709,57.8770106187709,
73.6003249306255));
#218465=CARTESIAN_POINT('Ctrl Pts',(-48.3445980725809,56.7582331765563,
68.665081144808));
#218466=CARTESIAN_POINT('Ctrl Pts',(-48.1944870025909,58.2885606023838,
63.6950789721284));
#218467=CARTESIAN_POINT('Ctrl Pts',(-48.0944129559309,60.8903814260647,
61.2673272490718));
#218468=CARTESIAN_POINT('Ctrl Pts',(-48.0443759326009,62.4308964939646,
60.4520329109682));
#218469=CARTESIAN_POINT('Ctrl Pts',(-48.173560826516,61.9759278335774,60.4464459620599));
#218470=CARTESIAN_POINT('Ctrl Pts',(-48.1596729098122,61.9881764360414,
60.4701459438214));
#218471=CARTESIAN_POINT('Ctrl Pts',(-48.1457849931352,62.0004250385118,
60.4938459255953));
#218472=CARTESIAN_POINT('Ctrl Pts',(-48.1179938256783,62.0249357675969,
60.5412720571877));
#218473=CARTESIAN_POINT('Ctrl Pts',(-48.1040905748985,62.0371978942117,
60.5649982070061));
#218474=CARTESIAN_POINT('Ctrl Pts',(-48.0901873241468,62.0494600208332,
60.5887243568377));
#218475=CARTESIAN_POINT('Origin',(-47.9901862140809,61.5168009229541,59.5580752732411));
#218476=CARTESIAN_POINT('Ctrl Pts',(-47.890187490573,62.0494598736152,60.5887240719837));
#218477=CARTESIAN_POINT('Ctrl Pts',(-47.8762912240803,62.0372039110344,
60.5650098490355));
#218478=CARTESIAN_POINT('Ctrl Pts',(-47.8623949575891,62.0249479484533,
60.5412956260867));
#218479=CARTESIAN_POINT('Ctrl Pts',(-47.8346038364013,62.0004372684354,
60.4938695894352));
#218480=CARTESIAN_POINT('Ctrl Pts',(-47.8207089817047,61.9881825509987,
60.4701577757327));
#218481=CARTESIAN_POINT('Ctrl Pts',(-47.8068141270095,61.9759278335617,
60.4464459620295));
#218482=CARTESIAN_POINT('Ctrl Pts',(-48.5133467647509,61.4150727054112,
76.8553253174122));
#218483=CARTESIAN_POINT('Ctrl Pts',(-48.4633097414209,60.0986507463519,
76.0127892243903));
#218484=CARTESIAN_POINT('Ctrl Pts',(-48.3632356947609,57.8770106187713,
73.6003249306246));
#218485=CARTESIAN_POINT('Ctrl Pts',(-48.2131246247709,56.7582331765567,
68.6650811448071));
#218486=CARTESIAN_POINT('Ctrl Pts',(-48.0630135547809,58.2885606023838,
63.6950789721284));
#218487=CARTESIAN_POINT('Ctrl Pts',(-47.9629395081209,60.8903814260647,
61.2673272490718));
#218488=CARTESIAN_POINT('Ctrl Pts',(-47.9129024847909,62.4308964939646,
60.4520329109682));
#218489=CARTESIAN_POINT('Ctrl Pts',(-48.2892186544709,61.163229053672,77.2045311508821));
#218490=CARTESIAN_POINT('Ctrl Pts',(-48.2391816311409,59.7862847782252,
76.3183469864098));
#218491=CARTESIAN_POINT('Ctrl Pts',(-48.1391075844909,57.4668991727267,
73.7864662252627));
#218492=CARTESIAN_POINT('Ctrl Pts',(-47.9889965144909,56.3098244246853,
68.6228537347707));
#218493=CARTESIAN_POINT('Ctrl Pts',(-47.8388854445009,57.9204095082865,
63.4356473787103));
#218494=CARTESIAN_POINT('Ctrl Pts',(-47.7388113978409,60.6405509703189,
60.9088264996243));
#218495=CARTESIAN_POINT('Ctrl Pts',(-47.6887743745209,62.2486728910826,
60.0619502304968));
#218496=CARTESIAN_POINT('Ctrl Pts',(-48.0650905442009,60.9113854019325,
77.5537369843529));
#218497=CARTESIAN_POINT('Ctrl Pts',(-48.0150535208709,59.4739188100982,
76.6239047484303));
#218498=CARTESIAN_POINT('Ctrl Pts',(-47.9149794742109,57.0567877266818,
73.9726075199017));
#218499=CARTESIAN_POINT('Ctrl Pts',(-47.7648684042209,55.8614156728147,
68.5806263247324));
#218500=CARTESIAN_POINT('Ctrl Pts',(-47.6147573342209,57.5522584141988,
63.176215785295));
#218501=CARTESIAN_POINT('Ctrl Pts',(-47.5146832875709,60.390720514573,60.5503257501769));
#218502=CARTESIAN_POINT('Ctrl Pts',(-47.4646462642409,62.0664492882006,
59.6718675500255));
#218503=CARTESIAN_POINT('Ctrl Pts',(-47.8409624339209,60.6595417501829,
77.9029428178218));
#218504=CARTESIAN_POINT('Ctrl Pts',(-47.7909254105909,59.1615528419807,
76.9294625104537));
#218505=CARTESIAN_POINT('Ctrl Pts',(-47.6908513639309,56.6466762806373,
74.1587488145399));
#218506=CARTESIAN_POINT('Ctrl Pts',(-47.5407402939409,55.4130069209437,
68.5383989146951));
#218507=CARTESIAN_POINT('Ctrl Pts',(-47.3906292239509,57.1841073201011,
62.9167841918779));
#218508=CARTESIAN_POINT('Ctrl Pts',(-47.2905551772909,60.1408900588271,
60.1918250007294));
#218509=CARTESIAN_POINT('Ctrl Pts',(-47.2405181539609,61.8842256853186,
59.2817848695541));
#218510=CARTESIAN_POINT('Ctrl Pts',(-48.4651187514177,61.0741848222236,
76.7120624159032));
#218511=CARTESIAN_POINT('Ctrl Pts',(-48.3651833447158,60.9558726340169,
76.8632423199665));
#218512=CARTESIAN_POINT('Ctrl Pts',(-48.2652478157504,60.837564185308,77.0144254557038));
#218513=CARTESIAN_POINT('Ctrl Pts',(-48.0647417952908,60.6002034168244,
77.3177584421339));
#218514=CARTESIAN_POINT('Ctrl Pts',(-47.9641710718521,60.4811508722256,
77.4699086827435));
#218515=CARTESIAN_POINT('Ctrl Pts',(-47.8636004674102,60.3621024374858,
77.6220618559046));
#218516=CARTESIAN_POINT('Ctrl Pts',(-55.7755280695129,61.5612801781646,
76.9828771994399));
#218517=CARTESIAN_POINT('Ctrl Pts',(-55.7369012443359,60.5671177764436,
76.2977664141033));
#218518=CARTESIAN_POINT('Ctrl Pts',(-55.6596475939829,58.8579984022376,
74.5234739673154));
#218519=CARTESIAN_POINT('Ctrl Pts',(-55.5437671184529,57.5375643233782,
71.0715732033576));
#218520=CARTESIAN_POINT('Ctrl Pts',(-55.4278866429239,57.67076376524,67.3782446735902));
#218521=CARTESIAN_POINT('Ctrl Pts',(-55.3120061673939,59.2362897652659,
64.0304593807185));
#218522=CARTESIAN_POINT('Ctrl Pts',(-55.1961256918649,61.9853341366056,
61.5603809658357));
#218523=CARTESIAN_POINT('Ctrl Pts',(-55.0802452163349,65.4809197835205,
60.3606278716295));
#218524=CARTESIAN_POINT('Ctrl Pts',(-54.9643647408059,69.1674172710837,
60.6219056176175));
#218525=CARTESIAN_POINT('Ctrl Pts',(-54.8484842652759,72.4588479701517,
62.3026829788097));
#218526=CARTESIAN_POINT('Ctrl Pts',(-54.7326037897459,74.8320309788573,
65.135796345557));
#218527=CARTESIAN_POINT('Ctrl Pts',(-54.6167233142169,75.9097429115672,
68.6709152745216));
#218528=CARTESIAN_POINT('Ctrl Pts',(-54.5008428386909,75.5206787921569,
72.3461238375153));
#218529=CARTESIAN_POINT('Ctrl Pts',(-54.3849623631609,73.7266813255289,
75.5772384992809));
#218530=CARTESIAN_POINT('Ctrl Pts',(-54.2690818876309,70.8129108674647,
77.8506655567186));
#218531=CARTESIAN_POINT('Ctrl Pts',(-54.1532014121009,67.2425184717931,
78.8050381301378));
#218532=CARTESIAN_POINT('Ctrl Pts',(-54.0373209365709,63.5830268811459,
78.2886563277363));
#218533=CARTESIAN_POINT('Ctrl Pts',(-53.9214404610409,60.4161213764918,
76.3836003200345));
#218534=CARTESIAN_POINT('Ctrl Pts',(-53.8055599855109,58.2451894565326,
73.3926834929056));
#218535=CARTESIAN_POINT('Ctrl Pts',(-53.6896795099809,57.4153061440108,
69.7913195074836));
#218536=CARTESIAN_POINT('Ctrl Pts',(-53.5737990344509,58.0583834534414,
66.1519541174747));
#218537=CARTESIAN_POINT('Ctrl Pts',(-53.4579185589209,60.0722026486568,
63.0530734942681));
#218538=CARTESIAN_POINT('Ctrl Pts',(-53.3420380833909,63.1366621648809,
60.9872524126374));
#218539=CARTESIAN_POINT('Ctrl Pts',(-53.2261576078609,66.7646585478257,
60.2828582664043));
#218540=CARTESIAN_POINT('Ctrl Pts',(-53.1102771323309,70.3795127580189,
61.0518562553049));
#218541=CARTESIAN_POINT('Ctrl Pts',(-52.9943966568009,73.4066347370121,
63.172012238292));
#218542=CARTESIAN_POINT('Ctrl Pts',(-52.8785161812709,75.3648559248227,
66.3063221539671));
#218543=CARTESIAN_POINT('Ctrl Pts',(-52.7626357057409,75.9429121981029,
69.9565796534893));
#218544=CARTESIAN_POINT('Ctrl Pts',(-52.6467552302109,75.0489200759327,
73.5425672375986));
#218545=CARTESIAN_POINT('Ctrl Pts',(-52.5308747546809,72.8249818274117,
76.4942832697837));
#218546=CARTESIAN_POINT('Ctrl Pts',(-52.4149942791509,69.6245979629103,
78.3425451526678));
#218547=CARTESIAN_POINT('Ctrl Pts',(-52.2991138036209,65.9564774496083,
78.7935670676356));
#218548=CARTESIAN_POINT('Ctrl Pts',(-52.1832333281009,62.4036771571881,
77.77565796066));
#218549=CARTESIAN_POINT('Ctrl Pts',(-52.0673528525709,59.5309235196917,
75.4506170134694));
#218550=CARTESIAN_POINT('Ctrl Pts',(-51.9514723770409,57.7948478656563,
72.1880152615929));
#218551=CARTESIAN_POINT('Ctrl Pts',(-51.8355919015109,57.4714037338775,
68.5064513600016));
#218552=CARTESIAN_POINT('Ctrl Pts',(-51.7197114259809,58.6120033727586,
64.991119038349));
#218553=CARTESIAN_POINT('Ctrl Pts',(-51.6038309504509,61.0353456356765,
62.2007891036227));
#218554=CARTESIAN_POINT('Ctrl Pts',(-51.4879504749209,64.356234248718,60.5789914320152));
#218555=CARTESIAN_POINT('Ctrl Pts',(-51.3720699993909,68.0468057155105,
60.3835147930695));
#218556=CARTESIAN_POINT('Ctrl Pts',(-51.2561895238609,71.520434531528,61.6454306842399));
#218557=CARTESIAN_POINT('Ctrl Pts',(-51.1403090483309,74.2249787656239,
64.164154439174));
#218558=CARTESIAN_POINT('Ctrl Pts',(-51.0244285728009,75.7305443918741,
67.5393286588116));
#218559=CARTESIAN_POINT('Ctrl Pts',(-50.9085480972709,75.7978180131431,
71.2344610147254));
#218560=CARTESIAN_POINT('Ctrl Pts',(-50.7926676217409,74.4161063201778,
74.6622010377381));
#218561=CARTESIAN_POINT('Ctrl Pts',(-50.6767871462109,71.8050358196814,
77.2777009343682));
#218562=CARTESIAN_POINT('Ctrl Pts',(-50.5609066706809,68.3796426553727,
78.6652204973787));
#218563=CARTESIAN_POINT('Ctrl Pts',(-50.4450261951609,64.6844015817095,
78.604210044692));
#218564=CARTESIAN_POINT('Ctrl Pts',(-50.3291457196309,61.3066803488238,
77.1043673393539));
#218565=CARTESIAN_POINT('Ctrl Pts',(-50.2132652441009,58.7833761392345,
74.4040961060069));
#218566=CARTESIAN_POINT('Ctrl Pts',(-50.0973847685709,57.515574426631,70.9326111664812));
#218567=CARTESIAN_POINT('Ctrl Pts',(-49.9815042930409,57.7047954433261,
67.2417136774408));
#218568=CARTESIAN_POINT('Ctrl Pts',(-49.8656238175109,59.3209620385326,
63.9180809654223));
#218569=CARTESIAN_POINT('Ctrl Pts',(-49.7497433419809,62.107180516346,61.4900127082349));
#218570=CARTESIAN_POINT('Ctrl Pts',(-49.6338628664509,65.6205745267381,
60.3434563880283));
#218571=CARTESIAN_POINT('Ctrl Pts',(-49.5179823909209,69.3026813625722,
60.6606599817841));
#218572=CARTESIAN_POINT('Ctrl Pts',(-49.4021019153909,72.5682209917208,
62.3912031861476));
#218573=CARTESIAN_POINT('Ctrl Pts',(-49.2862214398709,74.8981277828147,
65.2600118737985));
#218574=CARTESIAN_POINT('Ctrl Pts',(-49.1703409643409,75.9220572381282,
68.8110817203493));
#218575=CARTESIAN_POINT('Ctrl Pts',(-49.0544604888109,75.4772533170059,
72.4799615572945));
#218576=CARTESIAN_POINT('Ctrl Pts',(-48.9385800132809,73.634418370535,75.6834730465697));
#218577=CARTESIAN_POINT('Ctrl Pts',(-48.8226995377509,70.6864768513839,
77.9124129584511));
#218578=CARTESIAN_POINT('Ctrl Pts',(-48.7068190622209,67.1020066897472,
78.8124750030432));
#218579=CARTESIAN_POINT('Ctrl Pts',(-48.5909385866909,63.4507858607777,
78.2406322116709));
#218580=CARTESIAN_POINT('Ctrl Pts',(-48.4750581111709,60.313119539417,76.2876306508875));
#218581=CARTESIAN_POINT('Ctrl Pts',(-48.3978044608109,58.896367738792,74.2721860206966));
#218582=CARTESIAN_POINT('Ctrl Pts',(-48.3591776356409,58.4128954012822,
73.1658451292715));
#218583=CARTESIAN_POINT('Ctrl Pts',(-55.5513999592359,61.3169702771804,
77.3373946338935));
#218584=CARTESIAN_POINT('Ctrl Pts',(-55.5127731340599,60.2753761200882,
76.619597028865));
#218585=CARTESIAN_POINT('Ctrl Pts',(-55.4355194837069,58.4847142012186,
74.7606526126071));
#218586=CARTESIAN_POINT('Ctrl Pts',(-55.3196390081769,57.1012818576024,
71.1440607355204));
#218587=CARTESIAN_POINT('Ctrl Pts',(-55.2037585326479,57.2408362806385,
67.2745225090351));
#218588=CARTESIAN_POINT('Ctrl Pts',(-55.0878780571179,58.8810539468492,
63.7670134801353));
#218589=CARTESIAN_POINT('Ctrl Pts',(-54.9719975815889,61.7612559639331,
61.1790869602541));
#218590=CARTESIAN_POINT('Ctrl Pts',(-54.8561171060589,65.4236169414932,
59.9220933234976));
#218591=CARTESIAN_POINT('Ctrl Pts',(-54.7402366305299,69.2859982149144,
60.1958367009625));
#218592=CARTESIAN_POINT('Ctrl Pts',(-54.6243561549999,72.7344639571905,
61.9568044017577));
#218593=CARTESIAN_POINT('Ctrl Pts',(-54.5084756794709,75.2208721650242,
64.9250863686192));
#218594=CARTESIAN_POINT('Ctrl Pts',(-54.3925952039409,76.3500020236737,
68.6288667717324));
#218595=CARTESIAN_POINT('Ctrl Pts',(-54.2767147284109,75.9423755505674,
72.4794205229619));
#218596=CARTESIAN_POINT('Ctrl Pts',(-54.1608342528809,74.0627859826778,
75.8646925335889));
#218597=CARTESIAN_POINT('Ctrl Pts',(-54.0449537773509,71.0099987529967,
78.2465854069094));
#218598=CARTESIAN_POINT('Ctrl Pts',(-53.9290733018209,67.2692619766016,
79.2464913522907));
#218599=CARTESIAN_POINT('Ctrl Pts',(-53.8131928262909,63.4351750586927,
78.7054728353225));
#218600=CARTESIAN_POINT('Ctrl Pts',(-53.6973123507609,60.1171756413221,
76.7095260935192));
#218601=CARTESIAN_POINT('Ctrl Pts',(-53.5814318752309,57.8426679760259,
73.5759118207695));
#218602=CARTESIAN_POINT('Ctrl Pts',(-53.4655513997009,56.973190707635,69.8027257917525));
#218603=CARTESIAN_POINT('Ctrl Pts',(-53.3496709241709,57.6469494083309,
65.9897253009273));
#218604=CARTESIAN_POINT('Ctrl Pts',(-53.2337904486409,59.7568484585497,
62.7429962503755));
#218605=CARTESIAN_POINT('Ctrl Pts',(-53.1179099731109,62.9675141618542,
60.5786142897589));
#218606=CARTESIAN_POINT('Ctrl Pts',(-53.0020294975809,66.7686032272295,
59.8406133095026));
#218607=CARTESIAN_POINT('Ctrl Pts',(-52.8861490220609,70.5559231032727,
60.6463003991197));
#218608=CARTESIAN_POINT('Ctrl Pts',(-52.7702685465309,73.7274698854095,
62.8676095938355));
#218609=CARTESIAN_POINT('Ctrl Pts',(-52.6543880710009,75.7791183323543,
66.1514582779196));
#218610=CARTESIAN_POINT('Ctrl Pts',(-52.5385075954709,76.3847538257845,
69.9758705437336));
#218611=CARTESIAN_POINT('Ctrl Pts',(-52.4226271199409,75.4481090992107,
73.7329465591993));
#218612=CARTESIAN_POINT('Ctrl Pts',(-52.3067466444109,73.1180661591808,
76.8254897565408));
#218613=CARTESIAN_POINT('Ctrl Pts',(-52.1908661688809,69.7649911204159,
78.7619327105721));
#218614=CARTESIAN_POINT('Ctrl Pts',(-52.0749856933509,65.9218635916335,
79.2344730023141));
#218615=CARTESIAN_POINT('Ctrl Pts',(-51.9591052178209,62.1995582424626,
78.1679991782881));
#218616=CARTESIAN_POINT('Ctrl Pts',(-51.8432247422909,59.1897447568815,
75.7320299026639));
#218617=CARTESIAN_POINT('Ctrl Pts',(-51.7273442667609,57.3708404668259,
72.3137685443966));
#218618=CARTESIAN_POINT('Ctrl Pts',(-51.6114637912309,57.0319647285943,
68.4565562396562));
#218619=CARTESIAN_POINT('Ctrl Pts',(-51.4955833157009,58.2269826827762,
64.7735064682079));
#218620=CARTESIAN_POINT('Ctrl Pts',(-51.3797028401709,60.7659432563194,
61.8500491424068));
#218621=CARTESIAN_POINT('Ctrl Pts',(-51.2638223646409,64.2452723575601,
60.1508750680324));
#218622=CARTESIAN_POINT('Ctrl Pts',(-51.1479418891109,68.1119219808598,
59.9460721861075));
#218623=CARTESIAN_POINT('Ctrl Pts',(-51.0320614135809,71.7512785612103,
61.2681944235776));
#218624=CARTESIAN_POINT('Ctrl Pts',(-50.9161809380509,74.5848573275517,
63.9070871657535));
#218625=CARTESIAN_POINT('Ctrl Pts',(-50.8003004625309,76.162253894446,67.4432918544721));
#218626=CARTESIAN_POINT('Ctrl Pts',(-50.6844199870009,76.2327371582677,
71.3147199681373));
#218627=CARTESIAN_POINT('Ctrl Pts',(-50.5685395114709,74.7851036291041,
74.9059983888393));
#218628=CARTESIAN_POINT('Ctrl Pts',(-50.4526590359409,72.0494582533172,
77.6462844884435));
#218629=CARTESIAN_POINT('Ctrl Pts',(-50.3367785604109,68.4606386605805,
79.1000029826967));
#218630=CARTESIAN_POINT('Ctrl Pts',(-50.2208980848809,64.5890966422126,
79.0360817049179));
#218631=CARTESIAN_POINT('Ctrl Pts',(-50.1050176093509,61.0502234215632,
77.4646811010362));
#218632=CARTESIAN_POINT('Ctrl Pts',(-49.9891371338209,58.4065316900025,
74.6355792014605));
#218633=CARTESIAN_POINT('Ctrl Pts',(-49.8732566582909,57.0782428169735,
70.9984687825245));
#218634=CARTESIAN_POINT('Ctrl Pts',(-49.7573761827609,57.2764916192201,
67.1314775823678));
#218635=CARTESIAN_POINT('Ctrl Pts',(-49.6414957072309,58.9697659570288,
63.6492734604498));
#218636=CARTESIAN_POINT('Ctrl Pts',(-49.5256152317109,61.8889156671989,
61.105361414176));
#218637=CARTESIAN_POINT('Ctrl Pts',(-49.4097347561809,65.5699346500343,
59.9041025837992));
#218638=CARTESIAN_POINT('Ctrl Pts',(-49.2938542806509,69.4277157925497,
60.2364400462553));
#218639=CARTESIAN_POINT('Ctrl Pts',(-49.1779738051209,72.8490551950089,
62.0495479319754));
#218640=CARTESIAN_POINT('Ctrl Pts',(-49.0620933295909,75.2901224652598,
65.055228253093));
#218641=CARTESIAN_POINT('Ctrl Pts',(-48.9462128540609,76.3629038700644,
68.7757205963566));
#218642=CARTESIAN_POINT('Ctrl Pts',(-48.8303323785309,75.8968782343273,
72.6196436763184));
#218643=CARTESIAN_POINT('Ctrl Pts',(-48.7144519030009,73.966121137307,75.9759955596776));
#218644=CARTESIAN_POINT('Ctrl Pts',(-48.5985714274709,70.8775325360307,
78.3112787937738));
#218645=CARTESIAN_POINT('Ctrl Pts',(-48.4826909519509,67.1220463396723,
79.254283040401));
#218646=CARTESIAN_POINT('Ctrl Pts',(-48.3668104764209,63.2966247837026,
78.6551574757722));
#218647=CARTESIAN_POINT('Ctrl Pts',(-48.2509300008909,60.0092595589126,
76.6089776856617));
#218648=CARTESIAN_POINT('Ctrl Pts',(-48.1736763505409,58.5249141491315,
74.4973756505227));
#218649=CARTESIAN_POINT('Ctrl Pts',(-48.1350495253609,58.0183752164734,
73.3382509378444));
#218650=CARTESIAN_POINT('Ctrl Pts',(-55.3272718489599,61.0726603761865,
77.6919120683442));
#218651=CARTESIAN_POINT('Ctrl Pts',(-55.2886450237839,59.9836344637329,
76.9414276436267));
#218652=CARTESIAN_POINT('Ctrl Pts',(-55.2113913734309,58.1114300002093,
74.9978312579017));
#218653=CARTESIAN_POINT('Ctrl Pts',(-55.0955108979009,56.6649993918269,
71.2165482676822));
#218654=CARTESIAN_POINT('Ctrl Pts',(-54.9796304223719,56.8109087960282,
67.1708003444752));
#218655=CARTESIAN_POINT('Ctrl Pts',(-54.8637499468419,58.5258181284236,
63.5035675795475));
#218656=CARTESIAN_POINT('Ctrl Pts',(-54.7478694713129,61.5371777912702,
60.7977929546753));
#218657=CARTESIAN_POINT('Ctrl Pts',(-54.6319889957829,65.3663140994574,
59.4835587753602));
#218658=CARTESIAN_POINT('Ctrl Pts',(-54.5161085202509,69.4045791587436,
59.7697677843113));
#218659=CARTESIAN_POINT('Ctrl Pts',(-54.4002280447209,73.0100799442327,
61.6109258247082));
#218660=CARTESIAN_POINT('Ctrl Pts',(-54.2843475691909,75.6097133511933,
64.7143763916865));
#218661=CARTESIAN_POINT('Ctrl Pts',(-54.1684670936609,76.7902611357812,
68.58681826895));
#218662=CARTESIAN_POINT('Ctrl Pts',(-54.0525866181309,76.3640723089752,
72.612717208417));
#218663=CARTESIAN_POINT('Ctrl Pts',(-53.9367061426009,74.3988906398205,
76.152146567904));
#218664=CARTESIAN_POINT('Ctrl Pts',(-53.8208256670709,71.2070866385185,
78.6425052571067));
#218665=CARTESIAN_POINT('Ctrl Pts',(-53.7049451915509,67.2960054813953,
79.6879445744451));
#218666=CARTESIAN_POINT('Ctrl Pts',(-53.5890647160209,63.2873232362219,
79.1222893429069));
#218667=CARTESIAN_POINT('Ctrl Pts',(-53.4731842404909,59.8182299061273,
77.035451866986));
#218668=CARTESIAN_POINT('Ctrl Pts',(-53.3573037649609,57.4401464955149,
73.7591401486176));
#218669=CARTESIAN_POINT('Ctrl Pts',(-53.2414232894309,56.5310752712668,
69.8141320760029));
#218670=CARTESIAN_POINT('Ctrl Pts',(-53.1255428139009,57.235515363221,65.8274964843525));
#218671=CARTESIAN_POINT('Ctrl Pts',(-53.0096623383709,59.4414942684621,
62.4329190064619));
#218672=CARTESIAN_POINT('Ctrl Pts',(-52.8937818628409,62.7983661588541,
60.1699761668686));
#218673=CARTESIAN_POINT('Ctrl Pts',(-52.7779013873109,66.7725479066749,
59.398368352605));
#218674=CARTESIAN_POINT('Ctrl Pts',(-52.6620209117809,70.7323334485579,
60.2407445429475));
#218675=CARTESIAN_POINT('Ctrl Pts',(-52.5461404362509,74.0483050338323,
62.5632069494067));
#218676=CARTESIAN_POINT('Ctrl Pts',(-52.4302599607209,76.1933807399002,
65.9965944019083));
#218677=CARTESIAN_POINT('Ctrl Pts',(-52.3143794851909,76.8265954534646,
69.9951614340195));
#218678=CARTESIAN_POINT('Ctrl Pts',(-52.1984990096609,75.84729812247,73.9233258808397));
#218679=CARTESIAN_POINT('Ctrl Pts',(-52.0826185341309,73.4111504909153,
77.1566962433291));
#218680=CARTESIAN_POINT('Ctrl Pts',(-51.9667380586009,69.9053842778755,
79.1813202684909));
#218681=CARTESIAN_POINT('Ctrl Pts',(-51.8508575830709,65.8872497336091,
79.6753789369893));
#218682=CARTESIAN_POINT('Ctrl Pts',(-51.7349771075409,61.9954393276913,
78.5603403958908));
#218683=CARTESIAN_POINT('Ctrl Pts',(-51.6190966320109,58.8485659940342,
76.0134427918172));
#218684=CARTESIAN_POINT('Ctrl Pts',(-51.5032161564809,56.946833067975,72.4395218271453));
#218685=CARTESIAN_POINT('Ctrl Pts',(-51.3873356809509,56.5925257233132,
68.4066611192533));
#218686=CARTESIAN_POINT('Ctrl Pts',(-51.2714552054309,57.8419619928253,
64.5558938980169));
#218687=CARTESIAN_POINT('Ctrl Pts',(-51.1555747299009,60.4965408770102,
61.4993091811534));
#218688=CARTESIAN_POINT('Ctrl Pts',(-51.0396942543709,64.1343104664627,
59.7227587040345));
#218689=CARTESIAN_POINT('Ctrl Pts',(-50.9238137788409,68.1770382462698,
59.5086295791555));
#218690=CARTESIAN_POINT('Ctrl Pts',(-50.8079333033109,71.9821225909486,
60.8909581629449));
#218691=CARTESIAN_POINT('Ctrl Pts',(-50.6920528277809,74.9447358895156,
63.6500198923846));
#218692=CARTESIAN_POINT('Ctrl Pts',(-50.5761723522509,76.5939633970318,
67.3472550501956));
#218693=CARTESIAN_POINT('Ctrl Pts',(-50.4602918767209,76.6676563033805,
71.3949789216125));
#218694=CARTESIAN_POINT('Ctrl Pts',(-50.3444114011909,75.1541009379953,
75.1497957399931));
#218695=CARTESIAN_POINT('Ctrl Pts',(-50.2285309256609,72.2938806868999,
78.0148680425532));
#218696=CARTESIAN_POINT('Ctrl Pts',(-50.1126504501309,68.5416346657267,
79.534785468025));
#218697=CARTESIAN_POINT('Ctrl Pts',(-49.9967699746009,64.4937917026564,
79.4679533651302));
#218698=CARTESIAN_POINT('Ctrl Pts',(-49.8808894990709,60.7937664942429,
77.8249948626797));
#218699=CARTESIAN_POINT('Ctrl Pts',(-49.7650090235509,58.0296872407287,
74.8670622968579));
#218700=CARTESIAN_POINT('Ctrl Pts',(-49.6491285480209,56.6409112073073,
71.0643263985101));
#218701=CARTESIAN_POINT('Ctrl Pts',(-49.5332480724909,56.8481877951267,
67.0212414872383));
#218702=CARTESIAN_POINT('Ctrl Pts',(-49.4173675969609,58.6185698755448,
63.3804659554293));
#218703=CARTESIAN_POINT('Ctrl Pts',(-49.3014871214309,61.6706508180947,
60.7207101200916));
#218704=CARTESIAN_POINT('Ctrl Pts',(-49.1856066459009,65.5192947733674,
59.4647487795595));
#218705=CARTESIAN_POINT('Ctrl Pts',(-49.0697261703709,69.552750222577,59.8122201107395));
#218706=CARTESIAN_POINT('Ctrl Pts',(-48.9538456948409,73.1298893983293,
61.7078926778295));
#218707=CARTESIAN_POINT('Ctrl Pts',(-48.8379652193109,75.6821171477224,
64.8504446324208));
#218708=CARTESIAN_POINT('Ctrl Pts',(-48.7220847437809,76.8037505020027,
68.7403594723971));
#218709=CARTESIAN_POINT('Ctrl Pts',(-48.6062042682609,76.3165031516395,
72.7593257953694));
#218710=CARTESIAN_POINT('Ctrl Pts',(-48.4903237927309,74.2978239040633,
76.2685180728018));
#218711=CARTESIAN_POINT('Ctrl Pts',(-48.3744433172009,71.0685882206619,
78.7101446291031));
#218712=CARTESIAN_POINT('Ctrl Pts',(-48.2585628416709,67.1420859895845,
79.6960910777589));
#218713=CARTESIAN_POINT('Ctrl Pts',(-48.1426823661409,63.1424637066209,
79.0696827398739));
#218714=CARTESIAN_POINT('Ctrl Pts',(-48.0268018906109,59.7053995784171,
76.9303247204408));
#218715=CARTESIAN_POINT('Ctrl Pts',(-47.9495482402609,58.1534605594795,
74.7225652803545));
#218716=CARTESIAN_POINT('Ctrl Pts',(-47.9109214150809,57.6238550316623,
73.5106567464228));
#218717=CARTESIAN_POINT('Ctrl Pts',(-55.1031437386839,60.8283504752015,
78.0464295027996));
#218718=CARTESIAN_POINT('Ctrl Pts',(-55.0645169135079,59.6918928073868,
77.2632582583922));
#218719=CARTESIAN_POINT('Ctrl Pts',(-54.9872632631549,57.7381457991904,
75.2350099031933));
#218720=CARTESIAN_POINT('Ctrl Pts',(-54.8713827876249,56.2287169260511,
71.289035799845));
#218721=CARTESIAN_POINT('Ctrl Pts',(-54.7555023120959,56.3809813114179,
67.0670781799153));
#218722=CARTESIAN_POINT('Ctrl Pts',(-54.6396218365659,58.1705823100065,
63.2401216789652));
#218723=CARTESIAN_POINT('Ctrl Pts',(-54.5237413610409,61.313099618598,60.4164989490926));
#218724=CARTESIAN_POINT('Ctrl Pts',(-54.4078608855109,65.30901125743,59.0450242272283));
#218725=CARTESIAN_POINT('Ctrl Pts',(-54.2919804099809,69.5231601025766,
59.3436988676508));
#218726=CARTESIAN_POINT('Ctrl Pts',(-54.1760999344509,73.2856959312731,
61.2650472476525));
#218727=CARTESIAN_POINT('Ctrl Pts',(-54.0602194589209,75.9985545373602,
64.5036664147486));
#218728=CARTESIAN_POINT('Ctrl Pts',(-53.9443389833909,77.2305202478881,
68.5447697661598));
#218729=CARTESIAN_POINT('Ctrl Pts',(-53.8284585078609,76.7857690673864,
72.746013893864));
#218730=CARTESIAN_POINT('Ctrl Pts',(-53.7125780323309,74.7349952969698,
76.4396006022122));
#218731=CARTESIAN_POINT('Ctrl Pts',(-53.5966975568009,71.4041745240506,
79.0384251072975));
#218732=CARTESIAN_POINT('Ctrl Pts',(-53.4808170812709,67.3227489862028,
80.1293977965976));
#218733=CARTESIAN_POINT('Ctrl Pts',(-53.3649366057409,63.1394714137716,
79.5391058504835));
#218734=CARTESIAN_POINT('Ctrl Pts',(-53.2490561302109,59.5192841709575,
77.3613776404707));
#218735=CARTESIAN_POINT('Ctrl Pts',(-53.1331756546809,57.0376250150175,
73.9423684764854));
#218736=CARTESIAN_POINT('Ctrl Pts',(-53.0172951791509,56.0889598348911,
69.8255383602719));
#218737=CARTESIAN_POINT('Ctrl Pts',(-52.9014147036209,56.8240813181107,
65.6652676678047));
#218738=CARTESIAN_POINT('Ctrl Pts',(-52.7855342280909,59.1261400783554,
62.1228417625685));
#218739=CARTESIAN_POINT('Ctrl Pts',(-52.6696537525609,62.6292181558182,
59.7613380439862));
#218740=CARTESIAN_POINT('Ctrl Pts',(-52.5537732770309,66.776492586088,58.9561233957071));
#218741=CARTESIAN_POINT('Ctrl Pts',(-52.4378928015009,70.9087437938121,
59.8351886867614));
#218742=CARTESIAN_POINT('Ctrl Pts',(-52.3220123259709,74.3691401822294,
62.258804304951));
#218743=CARTESIAN_POINT('Ctrl Pts',(-52.2061318504409,76.6076431474328,
65.8417305258611));
#218744=CARTESIAN_POINT('Ctrl Pts',(-52.0902513749109,77.2684370811464,
70.014452324264));
#218745=CARTESIAN_POINT('Ctrl Pts',(-51.9743708993809,76.2464871457476,
74.1137052024411));
#218746=CARTESIAN_POINT('Ctrl Pts',(-51.8584904238609,73.7042348226836,
77.487902730087));
#218747=CARTESIAN_POINT('Ctrl Pts',(-51.7426099483309,70.0457774353802,
79.6007078263948));
#218748=CARTESIAN_POINT('Ctrl Pts',(-51.6267294728009,65.8526358756345,
80.1162848716646));
#218749=CARTESIAN_POINT('Ctrl Pts',(-51.5108489972709,61.7913204129621,
78.9526816135228));
#218750=CARTESIAN_POINT('Ctrl Pts',(-51.3949685217409,58.5073872312147,
76.2948556810079));
#218751=CARTESIAN_POINT('Ctrl Pts',(-51.2790880462109,56.522825669145,72.5652751099482));
#218752=CARTESIAN_POINT('Ctrl Pts',(-51.1632075706809,56.15308671803,68.356765998908));
#218753=CARTESIAN_POINT('Ctrl Pts',(-51.0473270951509,57.4569413028341,
64.3382813278711));
#218754=CARTESIAN_POINT('Ctrl Pts',(-50.9314466196209,60.2271384976534,
61.1485692199367));
#218755=CARTESIAN_POINT('Ctrl Pts',(-50.8155661440909,64.0233485753049,
59.2946423400516));
#218756=CARTESIAN_POINT('Ctrl Pts',(-50.6996856685609,68.2421545116176,
59.0711869721972));
#218757=CARTESIAN_POINT('Ctrl Pts',(-50.5838051930309,72.2129666206316,
60.5137219022862));
#218758=CARTESIAN_POINT('Ctrl Pts',(-50.4679247175009,75.3046144514435,
63.3929526189662));
#218759=CARTESIAN_POINT('Ctrl Pts',(-50.3520442419709,77.0256728996043,
67.2512182458574));
#218760=CARTESIAN_POINT('Ctrl Pts',(-50.2361637664409,77.1025754485052,
71.4752378750256));
#218761=CARTESIAN_POINT('Ctrl Pts',(-50.1202832909109,75.5230982469212,
75.3935930910952));
#218762=CARTESIAN_POINT('Ctrl Pts',(-50.0044028153909,72.5383031205348,
78.3834515966281));
#218763=CARTESIAN_POINT('Ctrl Pts',(-49.8885223398609,68.6226306709332,
79.9695679533436));
#218764=CARTESIAN_POINT('Ctrl Pts',(-49.7726418643309,64.3984867631581,
79.8998250253566));
#218765=CARTESIAN_POINT('Ctrl Pts',(-49.6567613888009,60.537309566982,78.1853086243629));
#218766=CARTESIAN_POINT('Ctrl Pts',(-49.5408809132709,57.6528427914971,
75.0985453923105));
#218767=CARTESIAN_POINT('Ctrl Pts',(-49.4250004377409,56.2035795976409,
71.1301840145486));
#218768=CARTESIAN_POINT('Ctrl Pts',(-49.3091199622109,56.4198839710304,
66.9110053921681));
#218769=CARTESIAN_POINT('Ctrl Pts',(-49.1932394866809,58.2673737940418,
63.111658450455));
#218770=CARTESIAN_POINT('Ctrl Pts',(-49.0773590111509,61.4523859689387,
60.336058826028));
#218771=CARTESIAN_POINT('Ctrl Pts',(-48.9614785356209,65.4686548966643,
59.0253949753286));
#218772=CARTESIAN_POINT('Ctrl Pts',(-48.8455980601009,69.6777846525631,
59.3880001752186));
#218773=CARTESIAN_POINT('Ctrl Pts',(-48.7297175845709,73.4107236016189,
61.366237423659));
#218774=CARTESIAN_POINT('Ctrl Pts',(-48.6138371090409,76.0741118301684,
64.6456610117157));
#218775=CARTESIAN_POINT('Ctrl Pts',(-48.4979566335109,77.2445971339387,
68.7049983484055));
#218776=CARTESIAN_POINT('Ctrl Pts',(-48.3820761579809,76.7361280689603,
72.8990079143937));
#218777=CARTESIAN_POINT('Ctrl Pts',(-48.2661956824509,74.6295266708348,
76.5610405859094));
#218778=CARTESIAN_POINT('Ctrl Pts',(-48.1503152069209,71.2596439053081,
79.1090104644245));
#218779=CARTESIAN_POINT('Ctrl Pts',(-48.0344347313909,67.1621256395096,
80.1378991151167));
#218780=CARTESIAN_POINT('Ctrl Pts',(-47.9185542558709,62.9883026295467,
79.4842080039734));
#218781=CARTESIAN_POINT('Ctrl Pts',(-47.8026737803409,59.4015395979127,
77.2516717552151));
#218782=CARTESIAN_POINT('Ctrl Pts',(-47.7254201299809,57.7820069698283,
74.9477549101844));
#218783=CARTESIAN_POINT('Ctrl Pts',(-47.6867933048109,57.2293348468531,
73.6830625549967));
#218784=CARTESIAN_POINT('',(-55.5975553638665,58.5901119100723,73.6973239050991));
#218785=CARTESIAN_POINT('Ctrl Pts',(-62.9066342559309,58.9178549548062,
74.1516175606608));
#218786=CARTESIAN_POINT('Ctrl Pts',(-62.8680074307549,58.3024937106637,
73.11283644396));
#218787=CARTESIAN_POINT('Ctrl Pts',(-62.7907537804019,57.4946548944447,
70.7854776041952));
#218788=CARTESIAN_POINT('Ctrl Pts',(-62.6748733048729,57.7429994225583,
67.098000141731));
#218789=CARTESIAN_POINT('Ctrl Pts',(-62.5589928293429,59.4122826098446,
63.8007419836913));
#218790=CARTESIAN_POINT('Ctrl Pts',(-62.4431123538139,62.2370844442565,
61.4176698865354));
#218791=CARTESIAN_POINT('Ctrl Pts',(-62.3272318782849,65.7684179761418,
60.3276167603848));
#218792=CARTESIAN_POINT('Ctrl Pts',(-62.2113514027559,69.4449629855937,
60.7038391619823));
#218793=CARTESIAN_POINT('Ctrl Pts',(-62.0954709272259,72.6823251108832,
62.4865383110415));
#218794=CARTESIAN_POINT('Ctrl Pts',(-61.9795904516969,74.9659171689976,
65.3923490235231));
#218795=CARTESIAN_POINT('Ctrl Pts',(-61.8637099761679,75.9327566433709,
68.959385660905));
#218796=CARTESIAN_POINT('Ctrl Pts',(-61.7478295006379,75.429161966439,72.6206588347031));
#218797=CARTESIAN_POINT('Ctrl Pts',(-61.6319490251089,73.5351807716313,
75.7942000908075));
#218798=CARTESIAN_POINT('Ctrl Pts',(-61.5160685495799,70.5518660735791,
77.9755671576036));
#218799=CARTESIAN_POINT('Ctrl Pts',(-61.4001880740499,66.9534231567007,
78.8180263208339));
#218800=CARTESIAN_POINT('Ctrl Pts',(-61.2843075985209,63.3118334634422,
78.1876666029973));
#218801=CARTESIAN_POINT('Ctrl Pts',(-61.1684271229909,60.2059367237536,
76.1846852475529));
#218802=CARTESIAN_POINT('Ctrl Pts',(-61.0525466474619,58.1294229415569,
73.1274611176965));
#218803=CARTESIAN_POINT('Ctrl Pts',(-60.9366661719329,57.4123591419893,
69.5019475850797));
#218804=CARTESIAN_POINT('Ctrl Pts',(-60.8207856964029,58.1687243976584,
65.8844290339352));
#218805=CARTESIAN_POINT('Ctrl Pts',(-60.7049052208739,60.2782925718688,
62.8499190263368));
#218806=CARTESIAN_POINT('Ctrl Pts',(-60.5890247453439,63.4057425617159,
60.8807604677571));
#218807=CARTESIAN_POINT('Ctrl Pts',(-60.4731442698149,67.0539584206267,
60.2899560038079));
#218808=CARTESIAN_POINT('Ctrl Pts',(-60.3572637942849,70.6430471731958,
61.1714154719933));
#218809=CARTESIAN_POINT('Ctrl Pts',(-60.2413833187559,73.6025142444707,
63.3850286996998));
#218810=CARTESIAN_POINT('Ctrl Pts',(-60.1255028432259,75.4619449901604,
66.5789363642741));
#218811=CARTESIAN_POINT('Ctrl Pts',(-60.0096223676969,75.9257782731553,
70.2454589066056));
#218812=CARTESIAN_POINT('Ctrl Pts',(-59.8937418921669,74.9202866406472,
73.8017934584711));
#218813=CARTESIAN_POINT('Ctrl Pts',(-59.7778614166379,72.6052954859447,
76.6826518065131));
#218814=CARTESIAN_POINT('Ctrl Pts',(-59.6619809411079,69.34877840509,78.4301143583121));
#218815=CARTESIAN_POINT('Ctrl Pts',(-59.5461004655789,65.6683668794744,
78.7664175993805));
#218816=CARTESIAN_POINT('Ctrl Pts',(-59.4302199900499,62.149071465724,77.6381052939462));
#218817=CARTESIAN_POINT('Ctrl Pts',(-59.3143395145199,59.3502929141666,
75.224525486451));
#218818=CARTESIAN_POINT('Ctrl Pts',(-59.1984590389909,57.7169040296169,
71.9093226842531));
#218819=CARTESIAN_POINT('Ctrl Pts',(-59.0825785634609,57.5085360337358,
68.219456609976));
#218820=CARTESIAN_POINT('Ctrl Pts',(-58.9666980879319,58.7583095371751,
64.7414406442363));
#218821=CARTESIAN_POINT('Ctrl Pts',(-58.8508176124019,61.2675699362972,
62.0281140665389));
#218822=CARTESIAN_POINT('Ctrl Pts',(-58.7349371368729,64.6374640559506,
60.5107668781401));
#218823=CARTESIAN_POINT('Ctrl Pts',(-58.6190566613429,68.3323388527351,
60.4305851847563));
#218824=CARTESIAN_POINT('Ctrl Pts',(-58.5031761858139,71.7648847971213,
61.8003140657714));
#218825=CARTESIAN_POINT('Ctrl Pts',(-58.3872957102849,74.3894901824946,
64.4022317122195));
#218826=CARTESIAN_POINT('Ctrl Pts',(-58.2714152347549,75.7889674615547,
67.8227568492751));
#218827=CARTESIAN_POINT('Ctrl Pts',(-58.1555347592259,75.740866243548,71.5181885075058));
#218828=CARTESIAN_POINT('Ctrl Pts',(-58.0396542836959,74.2528323365911,
74.9011286428881));
#218829=CARTESIAN_POINT('Ctrl Pts',(-57.9237738081669,71.5613924274766,
77.4338505153925));
#218830=CARTESIAN_POINT('Ctrl Pts',(-57.8078933326379,68.0943575771148,
78.7137716903922));
#218831=CARTESIAN_POINT('Ctrl Pts',(-57.6920128571079,64.4028215894282,
78.5374455169307));
#218832=CARTESIAN_POINT('Ctrl Pts',(-57.5761323815789,61.0735632819335,
76.9328994783959));
#218833=CARTESIAN_POINT('Ctrl Pts',(-57.4602519060499,58.6357765347184,
74.1551801543823));
#218834=CARTESIAN_POINT('Ctrl Pts',(-57.3443714305209,57.4769536083849,
70.6458129331832));
#218835=CARTESIAN_POINT('Ctrl Pts',(-57.2284909549909,57.7812922863604,
66.9626204542406));
#218836=CARTESIAN_POINT('Ctrl Pts',(-57.1126104794619,59.5004171796032,
63.6910553136322));
#218837=CARTESIAN_POINT('Ctrl Pts',(-56.9967300039329,62.3610691148619,
61.3511409192107));
#218838=CARTESIAN_POINT('Ctrl Pts',(-56.8808495284039,65.908540359229,60.3148124779815));
#218839=CARTESIAN_POINT('Ctrl Pts',(-56.7649690528749,69.5789515441067,
60.7467969703095));
#218840=CARTESIAN_POINT('Ctrl Pts',(-56.6490885773459,72.7888816918543,
62.5784293889601));
#218841=CARTESIAN_POINT('Ctrl Pts',(-56.5332081018169,75.0281044299382,
65.5185672056338));
#218842=CARTESIAN_POINT('Ctrl Pts',(-56.4173276262869,75.9406897400636,
69.0998682252856));
#218843=CARTESIAN_POINT('Ctrl Pts',(-56.3014471507579,75.3815799209528,
72.7530756919933));
#218844=CARTESIAN_POINT('Ctrl Pts',(-56.1855666752289,73.439646862909,75.8975034275876));
#218845=CARTESIAN_POINT('Ctrl Pts',(-56.0696861997009,70.4235656679413,
78.0333359882836));
#218846=CARTESIAN_POINT('Ctrl Pts',(-55.9538057241719,66.81274987119,78.8210806253173));
#218847=CARTESIAN_POINT('Ctrl Pts',(-55.8379252486429,63.1811478570346,
78.1355116392279));
#218848=CARTESIAN_POINT('Ctrl Pts',(-55.7220447731139,60.1060108866471,
76.0856457086154));
#218849=CARTESIAN_POINT('Ctrl Pts',(-55.6061642975849,58.0761429897366,
72.9971507091326));
#218850=CARTESIAN_POINT('Ctrl Pts',(-55.5289106472319,57.6348370927523,
70.5734238624516));
#218851=CARTESIAN_POINT('Ctrl Pts',(-55.4902838220559,57.6597134706593,
69.3663129168428));
#218852=CARTESIAN_POINT('Ctrl Pts',(-62.6825061456549,58.547426526001,74.3710548368581));
#218853=CARTESIAN_POINT('Ctrl Pts',(-62.6438793204789,57.9027062315234,
73.282713193911));
#218854=CARTESIAN_POINT('Ctrl Pts',(-62.5666256701259,57.0563252082828,
70.8443154384342));
#218855=CARTESIAN_POINT('Ctrl Pts',(-62.4507451945969,57.3165183205799,
66.9809074352464));
#218856=CARTESIAN_POINT('Ctrl Pts',(-62.3348647190669,59.0654434573398,
63.5263362043602));
#218857=CARTESIAN_POINT('Ctrl Pts',(-62.2189842435379,62.0250173464219,
61.0295670970088));
#218858=CARTESIAN_POINT('Ctrl Pts',(-62.1031037680089,65.7248317501465,
59.8875072432628));
#218859=CARTESIAN_POINT('Ctrl Pts',(-61.9872232924799,69.5767857100507,
60.2816793167476));
#218860=CARTESIAN_POINT('Ctrl Pts',(-61.8713428169499,72.9686032523646,
62.1494315213011));
#218861=CARTESIAN_POINT('Ctrl Pts',(-61.7554623414209,75.3611461012774,
65.1938792437982));
#218862=CARTESIAN_POINT('Ctrl Pts',(-61.6395818658919,76.3741137468067,
68.9311001577751));
#218863=CARTESIAN_POINT('Ctrl Pts',(-61.5237013903619,75.8464924324996,
72.7670536586459));
#218864=CARTESIAN_POINT('Ctrl Pts',(-61.4078209148329,73.862148885889,76.0920054209542));
#218865=CARTESIAN_POINT('Ctrl Pts',(-61.2919404393039,70.73649944184,78.3774460967396));
#218866=CARTESIAN_POINT('Ctrl Pts',(-61.1760599637739,66.9663738463322,
79.2600992130555));
#218867=CARTESIAN_POINT('Ctrl Pts',(-61.0601794882449,63.1510429301467,
78.5996648636749));
#218868=CARTESIAN_POINT('Ctrl Pts',(-60.9442990127149,59.8969630223145,
76.5011207294713));
#218869=CARTESIAN_POINT('Ctrl Pts',(-60.8284185371859,57.7213782095142,
73.2980356147634));
#218870=CARTESIAN_POINT('Ctrl Pts',(-60.7125380616569,56.9701031033569,
69.4995478571637));
#218871=CARTESIAN_POINT('Ctrl Pts',(-60.5966575861269,57.7625547486447,
65.7094365237527));
#218872=CARTESIAN_POINT('Ctrl Pts',(-60.4807771105979,59.9727709873792,
62.5301492281794));
#218873=CARTESIAN_POINT('Ctrl Pts',(-60.3648966350679,63.2494324567334,
60.4670415855671));
#218874=CARTESIAN_POINT('Ctrl Pts',(-60.2490161595389,67.0717056747189,
59.8480496818693));
#218875=CARTESIAN_POINT('Ctrl Pts',(-60.1331356840089,70.8320308162221,
60.7715638181682));
#218876=CARTESIAN_POINT('Ctrl Pts',(-60.0172552084799,73.9326948568119,
63.090789127866));
#218877=CARTESIAN_POINT('Ctrl Pts',(-59.9013747329499,75.8808395430932,
66.4370789854654));
#218878=CARTESIAN_POINT('Ctrl Pts',(-59.7854942574209,76.3668024366729,
70.2785323036529));
#218879=CARTESIAN_POINT('Ctrl Pts',(-59.6696137818909,75.3133385281575,
74.004540532737));
#218880=CARTESIAN_POINT('Ctrl Pts',(-59.5537333063619,72.887898523321,77.0228454067829));
#218881=CARTESIAN_POINT('Ctrl Pts',(-59.4378528308319,69.4760121373647,
78.8536798665508));
#218882=CARTESIAN_POINT('Ctrl Pts',(-59.3219723553029,65.6200071887684,
79.2060282256323));
#218883=CARTESIAN_POINT('Ctrl Pts',(-59.2060918797729,61.9328052450312,
78.023883836878));
#218884=CARTESIAN_POINT('Ctrl Pts',(-59.0902114042439,59.0004962166207,
75.4951514881296));
#218885=CARTESIAN_POINT('Ctrl Pts',(-58.9743309287149,57.2891779094226,
72.0217794692935));
#218886=CARTESIAN_POINT('Ctrl Pts',(-58.8584504531849,57.0708686204521,
68.1558688929745));
#218887=CARTESIAN_POINT('Ctrl Pts',(-58.7425699776559,58.3802691536199,
64.5119158508119));
#218888=CARTESIAN_POINT('Ctrl Pts',(-58.6266895021259,61.0092470407258,
61.6691357328929));
#218889=CARTESIAN_POINT('Ctrl Pts',(-58.5108090265969,64.5399197144825,
60.0793955023591));
#218890=CARTESIAN_POINT('Ctrl Pts',(-58.3949285510669,68.4110779807901,
59.9953883188285));
#218891=CARTESIAN_POINT('Ctrl Pts',(-58.2790480755379,72.0073916146724,
61.4304673328671));
#218892=CARTESIAN_POINT('Ctrl Pts',(-58.1631676000089,74.7572176283345,
64.1565231694807));
#218893=CARTESIAN_POINT('Ctrl Pts',(-58.0472871244789,76.2234643444835,
67.7402424800746));
#218894=CARTESIAN_POINT('Ctrl Pts',(-57.9314066489499,76.1730682044392,
71.6119841758516));
#218895=CARTESIAN_POINT('Ctrl Pts',(-57.8155261734199,74.6140397998802,
75.1563252942433));
#218896=CARTESIAN_POINT('Ctrl Pts',(-57.6996456978909,71.7941905693904,
77.8098840079436));
#218897=CARTESIAN_POINT('Ctrl Pts',(-57.5837652223619,68.1617425545688,
79.1508705661768));
#218898=CARTESIAN_POINT('Ctrl Pts',(-57.4678847468319,64.2940823928253,
78.9661318235942));
#218899=CARTESIAN_POINT('Ctrl Pts',(-57.3520042713029,60.8059842767521,
77.2850324623464));
#218900=CARTESIAN_POINT('Ctrl Pts',(-57.2361237957739,58.2518900686915,
74.3747874028885));
#218901=CARTESIAN_POINT('Ctrl Pts',(-57.1202433202449,57.0377793891086,
70.6979873284379));
#218902=CARTESIAN_POINT('Ctrl Pts',(-57.0043628447149,57.3566381471987,
66.8390687464839));
#218903=CARTESIAN_POINT('Ctrl Pts',(-56.8884823691859,59.157782951098,63.4114163537943));
#218904=CARTESIAN_POINT('Ctrl Pts',(-56.7726018936569,62.1549173589786,
60.9598640147741));
#218905=CARTESIAN_POINT('Ctrl Pts',(-56.6567214181279,65.8716394097845,
59.8740920651051));
#218906=CARTESIAN_POINT('Ctrl Pts',(-56.5408409425989,69.7171668986981,
60.326686653654));
#218907=CARTESIAN_POINT('Ctrl Pts',(-56.4249604670699,73.0802436764493,
62.2457067472407));
#218908=CARTESIAN_POINT('Ctrl Pts',(-56.3090799915409,75.4263003331489,
65.3261193292961));
#218909=CARTESIAN_POINT('Ctrl Pts',(-56.1931995160109,76.3824253336746,
69.0782851830545));
#218910=CARTESIAN_POINT('Ctrl Pts',(-56.0773190404819,75.7966402348364,
72.9057881597826));
#218911=CARTESIAN_POINT('Ctrl Pts',(-55.9614385649529,73.7620570287082,
76.2002373876932));
#218912=CARTESIAN_POINT('Ctrl Pts',(-55.8455580894239,70.6020777893704,
78.4379710938565));
#218913=CARTESIAN_POINT('Ctrl Pts',(-55.7296776138959,66.8189890005644,
79.2632992392267));
#218914=CARTESIAN_POINT('Ctrl Pts',(-55.6137971383669,63.0141222783363,
78.5450215725671));
#218915=CARTESIAN_POINT('Ctrl Pts',(-55.4979166628379,59.7922696966654,
76.3973559875148));
#218916=CARTESIAN_POINT('Ctrl Pts',(-55.3820361873089,57.6655562568715,
73.1615080615852));
#218917=CARTESIAN_POINT('Ctrl Pts',(-55.3047825369559,57.2031955369423,
70.6221445556835));
#218918=CARTESIAN_POINT('Ctrl Pts',(-55.2661557117799,57.2292587735241,
69.3574420224531));
#218919=CARTESIAN_POINT('Ctrl Pts',(-62.4583780353789,58.1769980971959,
74.5904921130554));
#218920=CARTESIAN_POINT('Ctrl Pts',(-62.4197512102019,57.5029187523924,
73.4525899438659));
#218921=CARTESIAN_POINT('Ctrl Pts',(-62.3424975598499,56.6179955221206,
70.9031532726741));
#218922=CARTESIAN_POINT('Ctrl Pts',(-62.2266170843209,56.8900372185927,
66.863814728757));
#218923=CARTESIAN_POINT('Ctrl Pts',(-62.1107366087909,58.7186043048254,
63.2519304250262));
#218924=CARTESIAN_POINT('Ctrl Pts',(-61.9948561332619,61.8129502485881,
60.6414643074804));
#218925=CARTESIAN_POINT('Ctrl Pts',(-61.8789756577329,65.6812455241418,
59.4473977261369));
#218926=CARTESIAN_POINT('Ctrl Pts',(-61.7630951822039,69.7086084345096,
59.8595194715137));
#218927=CARTESIAN_POINT('Ctrl Pts',(-61.6472147066739,73.2548813938479,
61.8123247315615));
#218928=CARTESIAN_POINT('Ctrl Pts',(-61.5313342311449,75.7563750335582,
64.9954094640758));
#218929=CARTESIAN_POINT('Ctrl Pts',(-61.4154537556159,76.8154708502427,
68.9028146546496));
#218930=CARTESIAN_POINT('Ctrl Pts',(-61.2995732800859,76.2638228985589,
72.9134484825934));
#218931=CARTESIAN_POINT('Ctrl Pts',(-61.1836928045569,74.1891170001427,
76.3898107511058));
#218932=CARTESIAN_POINT('Ctrl Pts',(-61.0678123290279,70.9211328100948,
78.7793250358796));
#218933=CARTESIAN_POINT('Ctrl Pts',(-60.9519318534979,66.9793245359562,
79.7021721052773));
#218934=CARTESIAN_POINT('Ctrl Pts',(-60.8360513779689,62.9902523968414,
79.0116631243529));
#218935=CARTESIAN_POINT('Ctrl Pts',(-60.7201709024389,59.5879893208676,
76.8175562113823));
#218936=CARTESIAN_POINT('Ctrl Pts',(-60.6042904269099,57.3133334774654,
73.4686101118191));
#218937=CARTESIAN_POINT('Ctrl Pts',(-60.4884099513809,56.5278470647294,
69.4971481292357));
#218938=CARTESIAN_POINT('Ctrl Pts',(-60.3725294758509,57.3563850996458,
65.5344440135604));
#218939=CARTESIAN_POINT('Ctrl Pts',(-60.2566490003219,59.667249402905,62.210379430011));
#218940=CARTESIAN_POINT('Ctrl Pts',(-60.1407685247919,63.0931223517737,
60.0533227033746));
#218941=CARTESIAN_POINT('Ctrl Pts',(-60.0248880492629,67.0894529288327,
59.4061433599309));
#218942=CARTESIAN_POINT('Ctrl Pts',(-59.9090075737329,71.0210144592654,
60.3717121643543));
#218943=CARTESIAN_POINT('Ctrl Pts',(-59.7931270982039,74.2628754691676,
62.796549556049));
#218944=CARTESIAN_POINT('Ctrl Pts',(-59.6772466226739,76.2997340960325,
66.2952216066778));
#218945=CARTESIAN_POINT('Ctrl Pts',(-59.5613661471449,76.8078266001889,
70.3116057007245));
#218946=CARTESIAN_POINT('Ctrl Pts',(-59.4454856716149,75.7063904156562,
74.2072876070264));
#218947=CARTESIAN_POINT('Ctrl Pts',(-59.3296051960859,73.1705015606764,
77.3630390070701));
#218948=CARTESIAN_POINT('Ctrl Pts',(-59.2137247205559,69.6032458696127,
79.277245374799));
#218949=CARTESIAN_POINT('Ctrl Pts',(-59.0978442450269,65.5716474980321,
79.6456388518812));
#218950=CARTESIAN_POINT('Ctrl Pts',(-58.9819637694969,61.7165390243107,
78.4096623797983));
#218951=CARTESIAN_POINT('Ctrl Pts',(-58.8660832939679,58.6506995190535,
75.765777489781));
#218952=CARTESIAN_POINT('Ctrl Pts',(-58.7502028184379,56.86145178922,72.1342362543012));
#218953=CARTESIAN_POINT('Ctrl Pts',(-58.6343223429089,56.6332012071813,
68.0922811759416));
#218954=CARTESIAN_POINT('Ctrl Pts',(-58.5184418673799,58.002228770078,64.2823910573551));
#218955=CARTESIAN_POINT('Ctrl Pts',(-58.4025613918499,60.7509241451938,
61.3101573992297));
#218956=CARTESIAN_POINT('Ctrl Pts',(-58.2866809163209,64.4423753730412,
59.6480241265653));
#218957=CARTESIAN_POINT('Ctrl Pts',(-58.1708004407909,68.4898171088944,
59.5601914529124));
#218958=CARTESIAN_POINT('Ctrl Pts',(-58.0549199652619,72.2498984322556,
61.0606205999848));
#218959=CARTESIAN_POINT('Ctrl Pts',(-57.9390394897319,75.1249450741959,
63.9108146267734));
#218960=CARTESIAN_POINT('Ctrl Pts',(-57.8231590142029,76.6579612274189,
67.6577281109137));
#218961=CARTESIAN_POINT('Ctrl Pts',(-57.7072785386739,76.6052701653223,
71.7057798442352));
#218962=CARTESIAN_POINT('Ctrl Pts',(-57.5913980631439,74.9752472631463,
75.4115219456312));
#218963=CARTESIAN_POINT('Ctrl Pts',(-57.4755175876149,72.0269887112709,
78.1859175005157));
#218964=CARTESIAN_POINT('Ctrl Pts',(-57.3596371120859,68.2291275319825,
79.5879694419675));
#218965=CARTESIAN_POINT('Ctrl Pts',(-57.2437566365559,64.1853431961846,
79.3948181302474));
#218966=CARTESIAN_POINT('Ctrl Pts',(-57.1278761610269,60.5384052715379,
77.6371654462714));
#218967=CARTESIAN_POINT('Ctrl Pts',(-57.0119956854979,57.8680036026363,
74.5943946513582));
#218968=CARTESIAN_POINT('Ctrl Pts',(-56.8961152099689,56.5986051698264,
70.7501617236546));
#218969=CARTESIAN_POINT('Ctrl Pts',(-56.7802347344389,56.9319840080419,
66.7155170386891));
#218970=CARTESIAN_POINT('Ctrl Pts',(-56.6643542589099,58.8151487226244,
63.1317773939326));
#218971=CARTESIAN_POINT('Ctrl Pts',(-56.5484737833809,61.9487656031238,
60.5685871103211));
#218972=CARTESIAN_POINT('Ctrl Pts',(-56.4325933078519,65.8347384603639,
59.4333716522234));
#218973=CARTESIAN_POINT('Ctrl Pts',(-56.3167128323229,69.8553822533185,
59.906576337004));
#218974=CARTESIAN_POINT('Ctrl Pts',(-56.2008323567939,73.3716056610648,
61.9129841055396));
#218975=CARTESIAN_POINT('Ctrl Pts',(-56.0849518812639,75.8244962363713,
65.1336714529827));
#218976=CARTESIAN_POINT('Ctrl Pts',(-55.9690714057349,76.8241609272865,
69.0567021408465));
#218977=CARTESIAN_POINT('Ctrl Pts',(-55.8531909302059,76.2117005487124,
73.058500627591));
#218978=CARTESIAN_POINT('Ctrl Pts',(-55.7373104546769,74.0844671944947,
76.502971347812));
#218979=CARTESIAN_POINT('Ctrl Pts',(-55.6214299791479,70.7805899107851,
78.8426061994355));
#218980=CARTESIAN_POINT('Ctrl Pts',(-55.5055495036199,66.8252281299281,
79.705517853136));
#218981=CARTESIAN_POINT('Ctrl Pts',(-55.3896690280909,62.8470966996323,
78.9545315059017));
#218982=CARTESIAN_POINT('Ctrl Pts',(-55.2737885525619,59.4785285066753,
76.7090662664087));
#218983=CARTESIAN_POINT('Ctrl Pts',(-55.1579080770329,57.2549695240061,
73.3258654140387));
#218984=CARTESIAN_POINT('Ctrl Pts',(-55.0806544266799,56.7715539811408,
70.6708652489211));
#218985=CARTESIAN_POINT('Ctrl Pts',(-55.0420276015039,56.7988040763871,
69.3485711280681));
#218986=CARTESIAN_POINT('Ctrl Pts',(-62.2342499251029,57.8065696683908,
74.8099293892527));
#218987=CARTESIAN_POINT('Ctrl Pts',(-62.1956230999259,57.1031312732521,
73.6224666938169));
#218988=CARTESIAN_POINT('Ctrl Pts',(-62.1183694495739,56.1796658359588,
70.9619911069131));
#218989=CARTESIAN_POINT('Ctrl Pts',(-62.0024889740439,56.4635561166055,
66.7467220222677));
#218990=CARTESIAN_POINT('Ctrl Pts',(-61.8866084985149,58.3717651523206,
62.9775246456951));
#218991=CARTESIAN_POINT('Ctrl Pts',(-61.7707280229859,61.6008831507443,
60.2533615179501));
#218992=CARTESIAN_POINT('Ctrl Pts',(-61.6548475474569,65.6376592981465,
59.007288209015));
#218993=CARTESIAN_POINT('Ctrl Pts',(-61.5389670719279,69.8404311589655,
59.4373596262818));
#218994=CARTESIAN_POINT('Ctrl Pts',(-61.4230865963979,73.5411595353312,
61.4752179418165));
#218995=CARTESIAN_POINT('Ctrl Pts',(-61.3072061208689,76.1516039658375,
64.7969396843518));
#218996=CARTESIAN_POINT('Ctrl Pts',(-61.1913256453399,77.2568279536785,
68.8745291515198));
#218997=CARTESIAN_POINT('Ctrl Pts',(-61.0754451698099,76.6811533646194,
73.0598433065362));
#218998=CARTESIAN_POINT('Ctrl Pts',(-60.9595646942809,74.5160851144003,
76.6876160812524));
#218999=CARTESIAN_POINT('Ctrl Pts',(-60.8436842187519,71.1057661783553,
79.1812039750165));
#219000=CARTESIAN_POINT('Ctrl Pts',(-60.7278037432219,66.9922752255877,
80.1442449974989));
#219001=CARTESIAN_POINT('Ctrl Pts',(-60.6119232676929,62.8294618635471,
79.4236613850277));
#219002=CARTESIAN_POINT('Ctrl Pts',(-60.4960427921629,59.2790156194285,
77.1339916933007));
#219003=CARTESIAN_POINT('Ctrl Pts',(-60.3801623166339,56.9052887454224,
73.6391846088869));
#219004=CARTESIAN_POINT('Ctrl Pts',(-60.2642818411039,56.0855910260969,
69.4947484013197));
#219005=CARTESIAN_POINT('Ctrl Pts',(-60.1484013655749,56.9502154506322,
65.3594515033776));
#219006=CARTESIAN_POINT('Ctrl Pts',(-60.0325208900459,59.361727818425,61.8906096318565));
#219007=CARTESIAN_POINT('Ctrl Pts',(-59.9166404145159,62.9368122467912,
59.6396038211846));
#219008=CARTESIAN_POINT('Ctrl Pts',(-59.8007599389869,67.1072001829157,
58.9642370379884));
#219009=CARTESIAN_POINT('Ctrl Pts',(-59.6848794634569,71.209998102294,59.9718605105236));
#219010=CARTESIAN_POINT('Ctrl Pts',(-59.5689989879279,74.5930560815087,
62.5023099842152));
#219011=CARTESIAN_POINT('Ctrl Pts',(-59.4531185123979,76.7186286489653,
66.1533642278691));
#219012=CARTESIAN_POINT('Ctrl Pts',(-59.3372380368689,77.2488507637066,
70.3446790977719));
#219013=CARTESIAN_POINT('Ctrl Pts',(-59.2213575613389,76.0994423031657,
74.4100346812925));
#219014=CARTESIAN_POINT('Ctrl Pts',(-59.1054770858099,73.4531045980525,
77.7032326073399));
#219015=CARTESIAN_POINT('Ctrl Pts',(-58.9895966102799,69.7304796018871,
79.7008108830386));
#219016=CARTESIAN_POINT('Ctrl Pts',(-58.8737161347509,65.5232878073241,
80.0852494781353));
#219017=CARTESIAN_POINT('Ctrl Pts',(-58.7578356592209,61.5002728036194,
78.7954409227264));
#219018=CARTESIAN_POINT('Ctrl Pts',(-58.6419551836919,58.3009028215076,
76.0364034914597));
#219019=CARTESIAN_POINT('Ctrl Pts',(-58.5260747081619,56.433725669026,72.2466930393406));
#219020=CARTESIAN_POINT('Ctrl Pts',(-58.4101942326329,56.1955337939067,
68.0286934589439));
#219021=CARTESIAN_POINT('Ctrl Pts',(-58.2943137571039,57.624188386514,64.0528662639259));
#219022=CARTESIAN_POINT('Ctrl Pts',(-58.1784332815739,60.4926012496316,
60.9511790655875));
#219023=CARTESIAN_POINT('Ctrl Pts',(-58.0625528060449,64.3448310315735,
59.2166527507834));
#219024=CARTESIAN_POINT('Ctrl Pts',(-57.9466723305149,68.5685562369575,
59.1249945869912));
#219025=CARTESIAN_POINT('Ctrl Pts',(-57.8307918549859,72.4924052498076,
60.690773867081));
#219026=CARTESIAN_POINT('Ctrl Pts',(-57.7149113794559,75.4926725200354,
63.6651060840354));
#219027=CARTESIAN_POINT('Ctrl Pts',(-57.5990309039269,77.0924581103469,
67.575213741715));
#219028=CARTESIAN_POINT('Ctrl Pts',(-57.4831504283979,77.0374721262134,
71.7995755125809));
#219029=CARTESIAN_POINT('Ctrl Pts',(-57.3672699528679,75.3364547264357,
75.6667185969866));
#219030=CARTESIAN_POINT('Ctrl Pts',(-57.2513894773389,72.2597868531839,
78.5619509930676));
#219031=CARTESIAN_POINT('Ctrl Pts',(-57.1355090018099,68.2965125094352,
80.0250683177526));
#219032=CARTESIAN_POINT('Ctrl Pts',(-57.0196285262799,64.076603999578,79.8235044369148));
#219033=CARTESIAN_POINT('Ctrl Pts',(-56.9037480507509,60.2708262663669,
77.9892984302229));
#219034=CARTESIAN_POINT('Ctrl Pts',(-56.7878675752219,57.4841171366094,
74.8140018998644));
#219035=CARTESIAN_POINT('Ctrl Pts',(-56.6719870996929,56.1594309505505,
70.8023361189085));
#219036=CARTESIAN_POINT('Ctrl Pts',(-56.5561066241629,56.5073298688805,
66.5919653309315));
#219037=CARTESIAN_POINT('Ctrl Pts',(-56.4402261486339,58.4725144941193,
62.8521384340947));
#219038=CARTESIAN_POINT('Ctrl Pts',(-56.3243456731049,61.7426138472405,
60.1773102058845));
#219039=CARTESIAN_POINT('Ctrl Pts',(-56.2084651975759,65.7978375109195,
58.992651239347));
#219040=CARTESIAN_POINT('Ctrl Pts',(-56.0925847220469,69.9935976079059,
59.4864660203555));
#219041=CARTESIAN_POINT('Ctrl Pts',(-55.9767042465179,73.6629676456614,
61.5802614638165));
#219042=CARTESIAN_POINT('Ctrl Pts',(-55.8608237709879,76.2226921395821,
64.941223576645));
#219043=CARTESIAN_POINT('Ctrl Pts',(-55.7449432954589,77.2658965208973,
69.0351190986164));
#219044=CARTESIAN_POINT('Ctrl Pts',(-55.6290628199299,76.6267608625964,
73.2112130953809));
#219045=CARTESIAN_POINT('Ctrl Pts',(-55.5131823444009,74.4068773602934,
76.8057053079185));
#219046=CARTESIAN_POINT('Ctrl Pts',(-55.3973018688719,70.9591020322142,
79.2472413050085));
#219047=CARTESIAN_POINT('Ctrl Pts',(-55.2814213933429,66.8314672593026,
80.1477364670454));
#219048=CARTESIAN_POINT('Ctrl Pts',(-55.1655409178149,62.6800711209345,
79.3640414392399));
#219049=CARTESIAN_POINT('Ctrl Pts',(-55.0496604422859,59.1647873166941,
77.0207765453072));
#219050=CARTESIAN_POINT('Ctrl Pts',(-54.9337799667569,56.844382791141,73.4902227664913));
#219051=CARTESIAN_POINT('Ctrl Pts',(-54.8565263164039,56.3399124253312,
70.7195859421522));
#219052=CARTESIAN_POINT('Ctrl Pts',(-54.8178994912279,56.3683493792519,
69.3397002336784));
#219053=CARTESIAN_POINT('',(-62.7285891236391,57.5976540486463,69.9231276410268));
#219054=CARTESIAN_POINT('Ctrl Pts',(-65.2384132905482,57.4206397706274,
65.0087087433499));
#219055=CARTESIAN_POINT('Ctrl Pts',(-65.2029278919597,57.979092375435,63.8703843309197));
#219056=CARTESIAN_POINT('Ctrl Pts',(-65.1319570947826,59.5203119770194,
61.8024113142919));
#219057=CARTESIAN_POINT('Ctrl Pts',(-65.0255008990171,62.7950529612741,
59.7419494328987));
#219058=CARTESIAN_POINT('Ctrl Pts',(-64.9190447032515,66.5922763045987,
59.0003860876846));
#219059=CARTESIAN_POINT('Ctrl Pts',(-64.8125885074859,70.4015698547972,
59.6773007910861));
#219060=CARTESIAN_POINT('Ctrl Pts',(-64.7061323117203,73.7108304890285,
61.6817243939746));
#219061=CARTESIAN_POINT('Ctrl Pts',(-64.5996761159548,76.0751935268562,
64.7441915297997));
#219062=CARTESIAN_POINT('Ctrl Pts',(-64.4932199201892,77.1768132902845,
68.4530125546886));
#219063=CARTESIAN_POINT('Ctrl Pts',(-64.3867637244237,76.8675977656186,
72.3096048992952));
#219064=CARTESIAN_POINT('Ctrl Pts',(-64.2803075286581,75.1891151585901,
75.7955215493427));
#219065=CARTESIAN_POINT('Ctrl Pts',(-64.1738513328926,72.367006249171,78.4421459656916));
#219066=CARTESIAN_POINT('Ctrl Pts',(-64.0673951371271,68.7806511388025,
79.8936880956339));
#219067=CARTESIAN_POINT('Ctrl Pts',(-63.9609389413616,64.9121684082349,
79.9550174392734));
#219068=CARTESIAN_POINT('Ctrl Pts',(-63.8544827455961,61.2816042571687,
78.6178806428873));
#219069=CARTESIAN_POINT('Ctrl Pts',(-63.7480265498306,58.3770181385261,
76.0620635928089));
#219070=CARTESIAN_POINT('Ctrl Pts',(-63.6415703540651,56.58888652557,72.6310262841577));
#219071=CARTESIAN_POINT('Ctrl Pts',(-63.5705995568881,56.3013337084174,
70.0679844126329));
#219072=CARTESIAN_POINT('Ctrl Pts',(-63.5351141582999,56.3933756893344,
68.8033975024123));
#219073=CARTESIAN_POINT('Ctrl Pts',(-65.0142851802722,57.8071755591803,
65.1983400256205));
#219074=CARTESIAN_POINT('Ctrl Pts',(-64.9787997816837,58.3423203118127,
64.1075252799264));
#219075=CARTESIAN_POINT('Ctrl Pts',(-64.9078289845066,59.8192148151818,
62.1258622007476));
#219076=CARTESIAN_POINT('Ctrl Pts',(-64.801372788741,62.9572796014205,60.1513967683752));
#219077=CARTESIAN_POINT('Ctrl Pts',(-64.6949165929754,66.5960201663911,
59.4407836751364));
#219078=CARTESIAN_POINT('Ctrl Pts',(-64.5884603972099,70.2463271701436,
60.0894463340285));
#219079=CARTESIAN_POINT('Ctrl Pts',(-64.4820042014443,73.4174708772949,
62.0102123290094));
#219080=CARTESIAN_POINT('Ctrl Pts',(-64.3755480056787,75.6831536981848,
64.9448628324088));
#219081=CARTESIAN_POINT('Ctrl Pts',(-64.2690918099132,76.738795718137,68.4988906815205));
#219082=CARTESIAN_POINT('Ctrl Pts',(-64.1626356141476,76.4424857644709,
72.1945223939759));
#219083=CARTESIAN_POINT('Ctrl Pts',(-64.0561794183821,74.8340571318683,
75.5349491147065));
#219084=CARTESIAN_POINT('Ctrl Pts',(-63.9497232226166,72.1297331458918,
78.0711127145999));
#219085=CARTESIAN_POINT('Ctrl Pts',(-63.843267026851,68.693059913747,79.4620725693219));
#219086=CARTESIAN_POINT('Ctrl Pts',(-63.7368108310855,64.986034078319,79.5208422413553));
#219087=CARTESIAN_POINT('Ctrl Pts',(-63.63035463532,61.5069969357081,78.2395128430028));
#219088=CARTESIAN_POINT('Ctrl Pts',(-63.5238984395549,58.7236380498246,
75.7903666285429));
#219089=CARTESIAN_POINT('Ctrl Pts',(-63.4174422437889,57.010136776047,72.5025287780578));
#219090=CARTESIAN_POINT('Ctrl Pts',(-63.3464714466119,56.7345854045009,
70.0464592808521));
#219091=CARTESIAN_POINT('Ctrl Pts',(-63.3109860480239,56.8227858761024,
68.8346517909851));
#219092=CARTESIAN_POINT('Ctrl Pts',(-64.7901570699962,58.1937113477375,
65.3879713079069));
#219093=CARTESIAN_POINT('Ctrl Pts',(-64.7546716714076,58.7055482481762,
64.3446662289412));
#219094=CARTESIAN_POINT('Ctrl Pts',(-64.6837008742306,60.1181176533299,
62.4493130872116));
#219095=CARTESIAN_POINT('Ctrl Pts',(-64.577244678465,63.1195062415454,60.5608441038514));
#219096=CARTESIAN_POINT('Ctrl Pts',(-64.4707884826994,66.5997640281635,
59.8811812625842));
#219097=CARTESIAN_POINT('Ctrl Pts',(-64.3643322869338,70.0910844854805,
60.5015918769625));
#219098=CARTESIAN_POINT('Ctrl Pts',(-64.2578760911682,73.1241112655526,
62.3387002640363));
#219099=CARTESIAN_POINT('Ctrl Pts',(-64.1514198954027,75.2911138695092,
65.1455341350098));
#219100=CARTESIAN_POINT('Ctrl Pts',(-64.0449636996371,76.3007781459888,
68.5447688083423));
#219101=CARTESIAN_POINT('Ctrl Pts',(-63.9385075038716,76.0173737633253,
72.0794398886478));
#219102=CARTESIAN_POINT('Ctrl Pts',(-63.832051308106,74.4789991051512,75.2743766800647));
#219103=CARTESIAN_POINT('Ctrl Pts',(-63.7255951123405,71.8924600426187,
77.7000794635043));
#219104=CARTESIAN_POINT('Ctrl Pts',(-63.619138916575,68.6054686886978,79.0304570430104));
#219105=CARTESIAN_POINT('Ctrl Pts',(-63.5126827208099,65.0598997484077,
79.0866670434391));
#219106=CARTESIAN_POINT('Ctrl Pts',(-63.4062265250439,61.7323896142594,
77.8611450431157));
#219107=CARTESIAN_POINT('Ctrl Pts',(-63.2997703292789,59.0702579611228,
75.5186696642778));
#219108=CARTESIAN_POINT('Ctrl Pts',(-63.1933141335129,57.4313870265325,
72.3740312719636));
#219109=CARTESIAN_POINT('Ctrl Pts',(-63.1223433363359,57.1678371005937,
70.0249341490751));
#219110=CARTESIAN_POINT('Ctrl Pts',(-63.0868579377479,57.2521960628615,
68.8659060795531));
#219111=CARTESIAN_POINT('Ctrl Pts',(-64.5660289597201,58.5802471362906,
65.5776025901772));
#219112=CARTESIAN_POINT('Ctrl Pts',(-64.5305435611316,59.0687761845539,
64.5818071779478));
#219113=CARTESIAN_POINT('Ctrl Pts',(-64.4595727639545,60.4170204914826,
62.7727639736645));
#219114=CARTESIAN_POINT('Ctrl Pts',(-64.3531165681889,63.2817328816918,
60.9702914393279));
#219115=CARTESIAN_POINT('Ctrl Pts',(-64.2466603724233,66.6035078899466,
60.3215788500322));
#219116=CARTESIAN_POINT('Ctrl Pts',(-64.1402041766578,69.9358418008276,
60.913737419903));
#219117=CARTESIAN_POINT('Ctrl Pts',(-64.0337479808922,72.8307516538193,
62.6671881990702));
#219118=CARTESIAN_POINT('Ctrl Pts',(-63.9272917851266,74.8990740408378,
65.3462054376189));
#219119=CARTESIAN_POINT('Ctrl Pts',(-63.8208355893611,75.8627605738414,
68.5906469351743));
#219120=CARTESIAN_POINT('Ctrl Pts',(-63.7143793935955,75.5922617621774,
71.9643573833286));
#219121=CARTESIAN_POINT('Ctrl Pts',(-63.60792319783,74.1239410784296,75.0138042454287));
#219122=CARTESIAN_POINT('Ctrl Pts',(-63.5014670020649,71.6551869393394,
77.3290462124126));
#219123=CARTESIAN_POINT('Ctrl Pts',(-63.3950108062989,68.5178774636422,
78.5988415166984));
#219124=CARTESIAN_POINT('Ctrl Pts',(-63.2885546105339,65.1337654184909,
78.6524918455206));
#219125=CARTESIAN_POINT('Ctrl Pts',(-63.1820984147679,61.9577822928,77.4827772432284));
#219126=CARTESIAN_POINT('Ctrl Pts',(-63.0756422190029,59.4168778724121,
75.246972700008));
#219127=CARTESIAN_POINT('Ctrl Pts',(-62.9691860232369,57.8526372770187,
72.2455337658675));
#219128=CARTESIAN_POINT('Ctrl Pts',(-62.8982152260599,57.6010887966773,
70.0034090172943));
#219129=CARTESIAN_POINT('Ctrl Pts',(-62.8627298274719,57.6816062496299,
68.897160368125));
#219130=CARTESIAN_POINT('Ctrl Pts',(-64.5675364832709,60.6333197960278,
62.5540045030464));
#219131=CARTESIAN_POINT('Ctrl Pts',(-64.5675364832709,60.316276790239,62.8628731621224));
#219132=CARTESIAN_POINT('Ctrl Pts',(-64.5675364832687,60.0228219393915,
63.1936835736482));
#219133=CARTESIAN_POINT('Ctrl Pts',(-64.5675364832687,59.4938075108645,
63.8842115791695));
#219134=CARTESIAN_POINT('Ctrl Pts',(-64.5675364832709,59.2568109510257,
64.2429885299645));
#219135=CARTESIAN_POINT('Ctrl Pts',(-64.5675364832709,59.0462179431753,
64.6166308207582));
#219136=CARTESIAN_POINT('Ctrl Pts',(-63.5337949169409,56.4405087963681,
69.9703303450313));
#219137=CARTESIAN_POINT('Ctrl Pts',(-63.5394868426676,56.4486993034411,
70.1709662592209));
#219138=CARTESIAN_POINT('Ctrl Pts',(-63.5451666556007,56.462783905414,70.3713185694427));
#219139=CARTESIAN_POINT('Ctrl Pts',(-63.5564167240732,56.5024402153682,
70.7682868434315));
#219140=CARTESIAN_POINT('Ctrl Pts',(-63.5619850785309,56.527848667695,70.9648330212303));
#219141=CARTESIAN_POINT('Ctrl Pts',(-63.5675399484425,56.5589377686512,
71.1605188170944));
#219142=CARTESIAN_POINT('Origin',(-49.5265537491909,65.9734210682048,61.9560808081071));
#219143=CARTESIAN_POINT('',(-47.1840596451126,66.5535285669906,62.195755942179));
#219144=CARTESIAN_POINT('',(-39.7523422906826,68.3939579446667,62.9561411445198));
#219145=CARTESIAN_POINT('',(-47.1840596451109,66.5535285669907,62.1957559421787));
#219146=CARTESIAN_POINT('',(-47.119731784661,69.2594615665078,63.3137295174307));
#219147=CARTESIAN_POINT('Origin',(-113.778845940191,69.2594615665078,63.3137295174307));
#219148=CARTESIAN_POINT('Origin',(-113.778845940191,69.2594615665078,63.3137295174307));
#219149=CARTESIAN_POINT('Origin',(27.1782499005891,77.5774829011345,66.75037338561));
#219150=CARTESIAN_POINT('Origin',(27.1782499005891,75.,72.9888893865801));
#219151=CARTESIAN_POINT('Origin',(27.1782499005891,75.,72.9888893865801));
#219152=CARTESIAN_POINT('',(-39.7523422906826,63.2389921423977,75.4331731464599));
#219153=CARTESIAN_POINT('Origin',(27.1782499005891,72.4225170988655,79.2274053875501));
#219154=CARTESIAN_POINT('Ctrl Pts',(-39.7523422906847,68.3939579446667,
62.9561411445199));
#219155=CARTESIAN_POINT('Ctrl Pts',(-39.7281387736131,67.4261905019625,
63.4318987914185));
#219156=CARTESIAN_POINT('Ctrl Pts',(-39.7067753132048,66.4946705665665,
64.0835294670284));
#219157=CARTESIAN_POINT('Ctrl Pts',(-39.6724659131911,64.7167905326718,
65.8377960430231));
#219158=CARTESIAN_POINT('Ctrl Pts',(-39.6628533608352,63.9426641268814,
67.0147663024293));
#219159=CARTESIAN_POINT('Ctrl Pts',(-39.6628533608352,62.9504704429495,
69.4162628052949));
#219160=CARTESIAN_POINT('Ctrl Pts',(-39.6724659131911,62.6681079916684,
70.7964084967982));
#219161=CARTESIAN_POINT('Ctrl Pts',(-39.7067753132048,62.6893142216513,
73.2939791024836));
#219162=CARTESIAN_POINT('Ctrl Pts',(-39.7281387736131,62.8892464901659,
74.4130765135442));
#219163=CARTESIAN_POINT('Ctrl Pts',(-39.7523422906848,63.2389921423979,
75.4331731464598));
#219164=CARTESIAN_POINT('Origin',(-23.4378585958609,75.,72.9888893865801));
#219165=CARTESIAN_POINT('Ctrl Pts',(-23.3090332587941,86.7759771267022,
77.8543002128612));
#219166=CARTESIAN_POINT('Ctrl Pts',(-23.3534781005806,87.1687858104401,
77.0199591890651));
#219167=CARTESIAN_POINT('Ctrl Pts',(-23.3969857639789,87.4684685784188,
76.1481661238117));
#219168=CARTESIAN_POINT('Ctrl Pts',(-23.4821035727886,87.8768797291089,
74.3427299956353));
#219169=CARTESIAN_POINT('Ctrl Pts',(-23.5241358609362,87.9823712605097,
73.4125249276302));
#219170=CARTESIAN_POINT('Ctrl Pts',(-23.5675316904177,87.9904527821819,
72.490756361305));
#219171=CARTESIAN_POINT('Ctrl Pts',(-38.3758095864366,70.2663422358007,
83.8196273194875));
#219172=CARTESIAN_POINT('Ctrl Pts',(-38.4258466097666,72.1087543535617,
84.7194504420196));
#219173=CARTESIAN_POINT('Ctrl Pts',(-38.525920656419,76.3137202385278,85.5568522331398));
#219174=CARTESIAN_POINT('Ctrl Pts',(-38.6760317264166,82.5445125465804,
83.4636401838068));
#219175=CARTESIAN_POINT('Ctrl Pts',(-38.826142796409,86.9995287031468,78.4421077647583));
#219176=CARTESIAN_POINT('Ctrl Pts',(-38.9262168430666,87.9290806197203,
73.9710084799022));
#219177=CARTESIAN_POINT('Ctrl Pts',(-38.9762538663893,87.7996291647998,
71.7442636422223));
#219178=CARTESIAN_POINT('Ctrl Pts',(-38.4975359461084,70.2663422358007,
83.8196273194875));
#219179=CARTESIAN_POINT('Ctrl Pts',(-38.5475729694384,72.1087543535617,
84.7194504420196));
#219180=CARTESIAN_POINT('Ctrl Pts',(-38.647647016096,76.3137202385278,85.5568522331398));
#219181=CARTESIAN_POINT('Ctrl Pts',(-38.7977580860884,82.5445125465804,
83.4636401838068));
#219182=CARTESIAN_POINT('Ctrl Pts',(-38.947869156086,86.9995287031468,78.4421077647583));
#219183=CARTESIAN_POINT('Ctrl Pts',(-39.0479432027384,87.9290806197203,
73.9710084799022));
#219184=CARTESIAN_POINT('Ctrl Pts',(-39.0979802260676,87.7996291647998,
71.7442636422223));
#219185=CARTESIAN_POINT('Ctrl Pts',(-38.6192623057863,70.2663422358007,
83.8196273194875));
#219186=CARTESIAN_POINT('Ctrl Pts',(-38.6692993291154,72.1087543535617,
84.7194504420196));
#219187=CARTESIAN_POINT('Ctrl Pts',(-38.7693733757677,76.3137202385278,
85.5568522331398));
#219188=CARTESIAN_POINT('Ctrl Pts',(-38.9194844457654,82.5445125465804,
83.4636401838068));
#219189=CARTESIAN_POINT('Ctrl Pts',(-39.0695955157577,86.9995287031468,
78.4421077647583));
#219190=CARTESIAN_POINT('Ctrl Pts',(-39.1696695624154,87.9290806197203,
73.9710084799022));
#219191=CARTESIAN_POINT('Ctrl Pts',(-39.2197065857454,87.7996291647998,
71.7442636422223));
#219192=CARTESIAN_POINT('Ctrl Pts',(-38.7409886654647,70.2663422358007,
83.8196273194875));
#219193=CARTESIAN_POINT('Ctrl Pts',(-38.7910256887871,72.1087543535617,
84.7194504420196));
#219194=CARTESIAN_POINT('Ctrl Pts',(-38.8910997354449,76.3137202385278,
85.5568522331398));
#219195=CARTESIAN_POINT('Ctrl Pts',(-39.0412108054371,82.5445125465804,
83.4636401838068));
#219196=CARTESIAN_POINT('Ctrl Pts',(-39.1913218754349,86.9995287031468,
78.4421077647583));
#219197=CARTESIAN_POINT('Ctrl Pts',(-39.2913959220871,87.9290806197203,
73.9710084799022));
#219198=CARTESIAN_POINT('Ctrl Pts',(-39.341432945417,87.7996291647998,71.7442636422223));
#219199=CARTESIAN_POINT('',(-38.9948861699879,87.8189932010941,72.2582005417311));
#219200=CARTESIAN_POINT('Ctrl Pts',(-38.4175364832709,70.6959992820295,
84.0186998247411));
#219201=CARTESIAN_POINT('Ctrl Pts',(-38.4515840088496,71.9757680822536,
84.5802970070803));
#219202=CARTESIAN_POINT('Ctrl Pts',(-38.485631534427,73.3662634949739,84.9164019237388));
#219203=CARTESIAN_POINT('Ctrl Pts',(-38.5196790600051,74.7814936945516,
85.0027014194011));
#219204=CARTESIAN_POINT('Ctrl Pts',(-38.5318196218692,75.2861321226979,
85.0334738279137));
#219205=CARTESIAN_POINT('Ctrl Pts',(-38.5439601837334,75.7939152826462,
85.0324846378943));
#219206=CARTESIAN_POINT('Ctrl Pts',(-38.5561007455978,76.3009441519617,
84.9986331104709));
#219207=CARTESIAN_POINT('Ctrl Pts',(-38.6061377689272,78.3906510078787,
84.8591148833621));
#219208=CARTESIAN_POINT('Ctrl Pts',(-38.6561747922594,80.4675817772296,
84.1613775335845));
#219209=CARTESIAN_POINT('Ctrl Pts',(-38.7062118155911,82.2485498546661,
82.9755867888542));
#219210=CARTESIAN_POINT('Ctrl Pts',(-38.7562488389227,84.0295179321026,
81.7897960441239));
#219211=CARTESIAN_POINT('Ctrl Pts',(-38.8062858622539,85.5145233176247,
80.1159519044411));
#219212=CARTESIAN_POINT('Ctrl Pts',(-38.8563228855836,86.4894139895291,
78.1612550133857));
#219213=CARTESIAN_POINT('Ctrl Pts',(-38.8900113257555,87.1457788947348,
76.845215711156));
#219214=CARTESIAN_POINT('Ctrl Pts',(-38.9236997659267,87.570915960302,75.4018511422798));
#219215=CARTESIAN_POINT('Ctrl Pts',(-38.9573884812308,87.7391459645685,
73.9195978901167));
#219216=CARTESIAN_POINT('Ctrl Pts',(-38.9698878032681,87.8015633343225,
73.3696463537504));
#219217=CARTESIAN_POINT('Ctrl Pts',(-38.9823871631799,87.8286156719632,
72.8143415954056));
#219218=CARTESIAN_POINT('Ctrl Pts',(-38.9948865750186,87.8189932821606,
72.2582005494317));
#219219=CARTESIAN_POINT('',(-39.2948856689521,87.8189932822379,72.2582005309434));
#219220=CARTESIAN_POINT('',(-38.9948867524609,87.8189932818422,72.2582005310306));
#219221=CARTESIAN_POINT('Ctrl Pts',(-38.7175257490599,70.6956032368047,
84.0185260206293));
#219222=CARTESIAN_POINT('Ctrl Pts',(-38.7475365958835,71.8236405759,84.5135891741795));
#219223=CARTESIAN_POINT('Ctrl Pts',(-38.7773577336901,73.0301799739484,
84.8302771319025));
#219224=CARTESIAN_POINT('Ctrl Pts',(-38.8371612694423,75.5028698793187,
85.0901078006421));
#219225=CARTESIAN_POINT('Ctrl Pts',(-38.8666805284219,76.7508376105969,
85.0253215589555));
#219226=CARTESIAN_POINT('Ctrl Pts',(-38.9333423802022,79.4983315491103,
84.4457335806272));
#219227=CARTESIAN_POINT('Ctrl Pts',(-38.9699089016275,80.9564254020816,
83.8358955289175));
#219228=CARTESIAN_POINT('Ctrl Pts',(-39.0430464798089,83.5596149995887,
82.1026671558932));
#219229=CARTESIAN_POINT('Ctrl Pts',(-39.0796009224147,84.699796910122,80.9726262266061));
#219230=CARTESIAN_POINT('Ctrl Pts',(-39.1461000544408,86.3398863956807,
78.5958132558447));
#219231=CARTESIAN_POINT('Ctrl Pts',(-39.1756663161435,86.9033056696874,
77.4163792493373));
#219232=CARTESIAN_POINT('Ctrl Pts',(-39.2353970967561,87.6582007704773,
74.9007486757214));
#219233=CARTESIAN_POINT('Ctrl Pts',(-39.2652280895187,87.8418252096164,
73.5778073419934));
#219234=CARTESIAN_POINT('Ctrl Pts',(-39.2948856682995,87.8189932818405,
72.2582005309356));
#219235=CARTESIAN_POINT('Ctrl Pts',(-22.1107451997509,74.4260959710669,
84.8149721769878));
#219236=CARTESIAN_POINT('Ctrl Pts',(-22.1554803513709,76.2585471560719,
84.9038985896115));
#219237=CARTESIAN_POINT('Ctrl Pts',(-22.2449506545909,79.9638470256126,
84.2144079552725));
#219238=CARTESIAN_POINT('Ctrl Pts',(-22.3791561094309,84.4696679742973,
80.7979303917429));
#219239=CARTESIAN_POINT('Ctrl Pts',(-22.5133615642709,86.965463317583,75.7241832750654));
#219240=CARTESIAN_POINT('Ctrl Pts',(-22.6475670191109,86.9220147677009,
70.0699504067063));
#219241=CARTESIAN_POINT('Ctrl Pts',(-22.7817724739509,84.3484238108847,
65.0351802123128));
#219242=CARTESIAN_POINT('Ctrl Pts',(-22.9159779287909,79.7908957547364,
61.6883646725776));
#219243=CARTESIAN_POINT('Ctrl Pts',(-23.0501833836309,74.2166310497644,
60.7397722098012));
#219244=CARTESIAN_POINT('Ctrl Pts',(-23.1843888384709,68.8086151774565,
62.3907153943344));
#219245=CARTESIAN_POINT('Ctrl Pts',(-23.3185942933109,64.7145490031636,
66.2908272630259));
#219246=CARTESIAN_POINT('Ctrl Pts',(-23.4527997481509,62.8032847658051,
71.6124171753859));
#219247=CARTESIAN_POINT('Ctrl Pts',(-23.5870052029909,63.4804352829581,
77.226125163765));
#219248=CARTESIAN_POINT('Ctrl Pts',(-23.7212106578309,66.6022941371127,
81.9405972979455));
#219249=CARTESIAN_POINT('Ctrl Pts',(-23.8554161126709,71.5063333088617,
84.7553175337843));
#219250=CARTESIAN_POINT('Ctrl Pts',(-23.9896215675109,77.1518064053908,
85.0729395141451));
#219251=CARTESIAN_POINT('Ctrl Pts',(-24.1238270223509,82.3406182318677,
82.8260567769257));
#219252=CARTESIAN_POINT('Ctrl Pts',(-24.2580324771909,85.9715872915008,
78.4915079084072));
#219253=CARTESIAN_POINT('Ctrl Pts',(-24.3922379320309,87.2741410374378,
72.9891807694126));
#219254=CARTESIAN_POINT('Ctrl Pts',(-24.5264433868709,85.9718485387383,
67.4867917924943));
#219255=CARTESIAN_POINT('Ctrl Pts',(-24.6606488417109,82.3410852838296,
63.1520705335424));
#219256=CARTESIAN_POINT('Ctrl Pts',(-24.7948542965509,77.1523801433417,
60.9049414386413));
#219257=CARTESIAN_POINT('Ctrl Pts',(-24.9290597513909,71.5068919724511,
61.2222953760158));
#219258=CARTESIAN_POINT('Ctrl Pts',(-25.0632652062309,66.6027191668866,
64.0367827707004));
#219259=CARTESIAN_POINT('Ctrl Pts',(-25.1974706610709,63.4806364728584,
68.7511066704762));
#219260=CARTESIAN_POINT('Ctrl Pts',(-25.3316761159109,62.8032194385157,
74.3647825240852));
#219261=CARTESIAN_POINT('Ctrl Pts',(-25.4658815707509,64.7142309491779,
79.6864630932149));
#219262=CARTESIAN_POINT('Ctrl Pts',(-25.6000870255909,68.8081121689346,
83.586769647843));
#219263=CARTESIAN_POINT('Ctrl Pts',(-25.7342924804309,74.2160488136893,
85.2379684505082));
#219264=CARTESIAN_POINT('Ctrl Pts',(-25.8684979352709,79.7903616710785,
84.2896449343191));
#219265=CARTESIAN_POINT('Ctrl Pts',(-26.0027033901109,84.3480369807344,
80.9430297969229));
#219266=CARTESIAN_POINT('Ctrl Pts',(-26.1369088449509,86.9219104419729,
75.9084414716367));
#219267=CARTESIAN_POINT('Ctrl Pts',(-26.2711142997909,86.9654652521441,
70.2539879752974));
#219268=CARTESIAN_POINT('Ctrl Pts',(-26.3605846030209,85.3021658434783,
66.8719649808209));
#219269=CARTESIAN_POINT('Ctrl Pts',(-26.4053197546309,84.1350213486955,
65.456493688071));
#219270=CARTESIAN_POINT('Ctrl Pts',(-22.2602140739609,74.4260959710669,
84.8149721769878));
#219271=CARTESIAN_POINT('Ctrl Pts',(-22.3049492255709,76.2585471560719,
84.9038985896115));
#219272=CARTESIAN_POINT('Ctrl Pts',(-22.3944195288009,79.9638470256126,
84.2144079552725));
#219273=CARTESIAN_POINT('Ctrl Pts',(-22.5286249836409,84.4696679742973,
80.7979303917429));
#219274=CARTESIAN_POINT('Ctrl Pts',(-22.6628304384809,86.965463317583,75.7241832750654));
#219275=CARTESIAN_POINT('Ctrl Pts',(-22.7970358933209,86.9220147677009,
70.0699504067063));
#219276=CARTESIAN_POINT('Ctrl Pts',(-22.9312413481609,84.3484238108847,
65.0351802123128));
#219277=CARTESIAN_POINT('Ctrl Pts',(-23.0654468030009,79.7908957547364,
61.6883646725776));
#219278=CARTESIAN_POINT('Ctrl Pts',(-23.1996522578409,74.2166310497644,
60.7397722098012));
#219279=CARTESIAN_POINT('Ctrl Pts',(-23.3338577126809,68.8086151774565,
62.3907153943344));
#219280=CARTESIAN_POINT('Ctrl Pts',(-23.4680631675209,64.7145490031636,
66.2908272630259));
#219281=CARTESIAN_POINT('Ctrl Pts',(-23.6022686223609,62.8032847658051,
71.6124171753859));
#219282=CARTESIAN_POINT('Ctrl Pts',(-23.7364740772009,63.4804352829581,
77.226125163765));
#219283=CARTESIAN_POINT('Ctrl Pts',(-23.8706795320409,66.6022941371127,
81.9405972979455));
#219284=CARTESIAN_POINT('Ctrl Pts',(-24.0048849868809,71.5063333088617,
84.7553175337843));
#219285=CARTESIAN_POINT('Ctrl Pts',(-24.1390904417209,77.1518064053908,
85.0729395141451));
#219286=CARTESIAN_POINT('Ctrl Pts',(-24.2732958965609,82.3406182318677,
82.8260567769257));
#219287=CARTESIAN_POINT('Ctrl Pts',(-24.4075013514009,85.9715872915008,
78.4915079084072));
#219288=CARTESIAN_POINT('Ctrl Pts',(-24.5417068062409,87.2741410374378,
72.9891807694126));
#219289=CARTESIAN_POINT('Ctrl Pts',(-24.6759122610809,85.9718485387383,
67.4867917924943));
#219290=CARTESIAN_POINT('Ctrl Pts',(-24.8101177159209,82.3410852838296,
63.1520705335424));
#219291=CARTESIAN_POINT('Ctrl Pts',(-24.9443231707609,77.1523801433417,
60.9049414386413));
#219292=CARTESIAN_POINT('Ctrl Pts',(-25.0785286256009,71.5068919724511,
61.2222953760158));
#219293=CARTESIAN_POINT('Ctrl Pts',(-25.2127340804409,66.6027191668866,
64.0367827707004));
#219294=CARTESIAN_POINT('Ctrl Pts',(-25.3469395352809,63.4806364728584,
68.7511066704762));
#219295=CARTESIAN_POINT('Ctrl Pts',(-25.4811449901209,62.8032194385157,
74.3647825240852));
#219296=CARTESIAN_POINT('Ctrl Pts',(-25.6153504449609,64.7142309491779,
79.6864630932149));
#219297=CARTESIAN_POINT('Ctrl Pts',(-25.7495558998009,68.8081121689346,
83.586769647843));
#219298=CARTESIAN_POINT('Ctrl Pts',(-25.8837613546409,74.2160488136893,
85.2379684505082));
#219299=CARTESIAN_POINT('Ctrl Pts',(-26.0179668094809,79.7903616710785,
84.2896449343191));
#219300=CARTESIAN_POINT('Ctrl Pts',(-26.1521722643209,84.3480369807344,
80.9430297969229));
#219301=CARTESIAN_POINT('Ctrl Pts',(-26.2863777191609,86.9219104419729,
75.9084414716367));
#219302=CARTESIAN_POINT('Ctrl Pts',(-26.4205831740009,86.9654652521441,
70.2539879752974));
#219303=CARTESIAN_POINT('Ctrl Pts',(-26.5100534772209,85.3021658434783,
66.8719649808209));
#219304=CARTESIAN_POINT('Ctrl Pts',(-26.5547886288309,84.1350213486955,
65.456493688071));
#219305=CARTESIAN_POINT('Ctrl Pts',(-22.4096829481609,74.4260959710669,
84.8149721769878));
#219306=CARTESIAN_POINT('Ctrl Pts',(-22.4544180997809,76.2585471560719,
84.9038985896115));
#219307=CARTESIAN_POINT('Ctrl Pts',(-22.5438884030009,79.9638470256126,
84.2144079552725));
#219308=CARTESIAN_POINT('Ctrl Pts',(-22.6780938578409,84.4696679742973,
80.7979303917429));
#219309=CARTESIAN_POINT('Ctrl Pts',(-22.8122993126809,86.965463317583,75.7241832750654));
#219310=CARTESIAN_POINT('Ctrl Pts',(-22.9465047675209,86.9220147677009,
70.0699504067063));
#219311=CARTESIAN_POINT('Ctrl Pts',(-23.0807102223609,84.3484238108847,
65.0351802123128));
#219312=CARTESIAN_POINT('Ctrl Pts',(-23.2149156772009,79.7908957547364,
61.6883646725776));
#219313=CARTESIAN_POINT('Ctrl Pts',(-23.3491211320409,74.2166310497644,
60.7397722098012));
#219314=CARTESIAN_POINT('Ctrl Pts',(-23.4833265868809,68.8086151774565,
62.3907153943344));
#219315=CARTESIAN_POINT('Ctrl Pts',(-23.6175320417209,64.7145490031636,
66.2908272630259));
#219316=CARTESIAN_POINT('Ctrl Pts',(-23.7517374965609,62.8032847658051,
71.6124171753859));
#219317=CARTESIAN_POINT('Ctrl Pts',(-23.8859429514009,63.4804352829581,
77.226125163765));
#219318=CARTESIAN_POINT('Ctrl Pts',(-24.0201484062409,66.6022941371127,
81.9405972979455));
#219319=CARTESIAN_POINT('Ctrl Pts',(-24.1543538610809,71.5063333088617,
84.7553175337843));
#219320=CARTESIAN_POINT('Ctrl Pts',(-24.2885593159209,77.1518064053908,
85.0729395141451));
#219321=CARTESIAN_POINT('Ctrl Pts',(-24.4227647707609,82.3406182318677,
82.8260567769257));
#219322=CARTESIAN_POINT('Ctrl Pts',(-24.5569702256009,85.9715872915008,
78.4915079084072));
#219323=CARTESIAN_POINT('Ctrl Pts',(-24.6911756804409,87.2741410374378,
72.9891807694126));
#219324=CARTESIAN_POINT('Ctrl Pts',(-24.8253811352809,85.9718485387383,
67.4867917924943));
#219325=CARTESIAN_POINT('Ctrl Pts',(-24.9595865901209,82.3410852838296,
63.1520705335424));
#219326=CARTESIAN_POINT('Ctrl Pts',(-25.0937920449609,77.1523801433417,
60.9049414386413));
#219327=CARTESIAN_POINT('Ctrl Pts',(-25.2279974998009,71.5068919724511,
61.2222953760158));
#219328=CARTESIAN_POINT('Ctrl Pts',(-25.3622029546409,66.6027191668866,
64.0367827707004));
#219329=CARTESIAN_POINT('Ctrl Pts',(-25.4964084094809,63.4806364728584,
68.7511066704762));
#219330=CARTESIAN_POINT('Ctrl Pts',(-25.6306138643209,62.8032194385157,
74.3647825240852));
#219331=CARTESIAN_POINT('Ctrl Pts',(-25.7648193191609,64.7142309491779,
79.6864630932149));
#219332=CARTESIAN_POINT('Ctrl Pts',(-25.8990247740009,68.8081121689346,
83.586769647843));
#219333=CARTESIAN_POINT('Ctrl Pts',(-26.0332302288409,74.2160488136893,
85.2379684505082));
#219334=CARTESIAN_POINT('Ctrl Pts',(-26.1674356836809,79.7903616710785,
84.2896449343191));
#219335=CARTESIAN_POINT('Ctrl Pts',(-26.3016411385209,84.3480369807344,
80.9430297969229));
#219336=CARTESIAN_POINT('Ctrl Pts',(-26.4358465933609,86.9219104419729,
75.9084414716367));
#219337=CARTESIAN_POINT('Ctrl Pts',(-26.5700520482009,86.9654652521441,
70.2539879752974));
#219338=CARTESIAN_POINT('Ctrl Pts',(-26.6595223514309,85.3021658434783,
66.8719649808209));
#219339=CARTESIAN_POINT('Ctrl Pts',(-26.7042575030409,84.1350213486955,
65.456493688071));
#219340=CARTESIAN_POINT('Ctrl Pts',(-22.5591518223709,74.4260959710669,
84.8149721769878));
#219341=CARTESIAN_POINT('Ctrl Pts',(-22.6038869739809,76.2585471560719,
84.9038985896115));
#219342=CARTESIAN_POINT('Ctrl Pts',(-22.6933572772109,79.9638470256126,
84.2144079552725));
#219343=CARTESIAN_POINT('Ctrl Pts',(-22.8275627320509,84.4696679742973,
80.7979303917429));
#219344=CARTESIAN_POINT('Ctrl Pts',(-22.9617681868909,86.965463317583,75.7241832750654));
#219345=CARTESIAN_POINT('Ctrl Pts',(-23.0959736417309,86.9220147677009,
70.0699504067063));
#219346=CARTESIAN_POINT('Ctrl Pts',(-23.2301790965709,84.3484238108847,
65.0351802123128));
#219347=CARTESIAN_POINT('Ctrl Pts',(-23.3643845514109,79.7908957547364,
61.6883646725776));
#219348=CARTESIAN_POINT('Ctrl Pts',(-23.4985900062509,74.2166310497644,
60.7397722098012));
#219349=CARTESIAN_POINT('Ctrl Pts',(-23.6327954610909,68.8086151774565,
62.3907153943344));
#219350=CARTESIAN_POINT('Ctrl Pts',(-23.7670009159309,64.7145490031636,
66.2908272630259));
#219351=CARTESIAN_POINT('Ctrl Pts',(-23.9012063707709,62.8032847658051,
71.6124171753859));
#219352=CARTESIAN_POINT('Ctrl Pts',(-24.0354118256109,63.4804352829581,
77.226125163765));
#219353=CARTESIAN_POINT('Ctrl Pts',(-24.1696172804509,66.6022941371127,
81.9405972979455));
#219354=CARTESIAN_POINT('Ctrl Pts',(-24.3038227352909,71.5063333088617,
84.7553175337843));
#219355=CARTESIAN_POINT('Ctrl Pts',(-24.4380281901309,77.1518064053908,
85.0729395141451));
#219356=CARTESIAN_POINT('Ctrl Pts',(-24.5722336449709,82.3406182318677,
82.8260567769257));
#219357=CARTESIAN_POINT('Ctrl Pts',(-24.7064390998109,85.9715872915008,
78.4915079084072));
#219358=CARTESIAN_POINT('Ctrl Pts',(-24.8406445546509,87.2741410374378,
72.9891807694126));
#219359=CARTESIAN_POINT('Ctrl Pts',(-24.9748500094909,85.9718485387383,
67.4867917924943));
#219360=CARTESIAN_POINT('Ctrl Pts',(-25.1090554643309,82.3410852838296,
63.1520705335424));
#219361=CARTESIAN_POINT('Ctrl Pts',(-25.2432609191709,77.1523801433417,
60.9049414386413));
#219362=CARTESIAN_POINT('Ctrl Pts',(-25.3774663740109,71.5068919724511,
61.2222953760158));
#219363=CARTESIAN_POINT('Ctrl Pts',(-25.5116718288509,66.6027191668866,
64.0367827707004));
#219364=CARTESIAN_POINT('Ctrl Pts',(-25.6458772836909,63.4806364728584,
68.7511066704762));
#219365=CARTESIAN_POINT('Ctrl Pts',(-25.7800827385309,62.8032194385157,
74.3647825240852));
#219366=CARTESIAN_POINT('Ctrl Pts',(-25.9142881933709,64.7142309491779,
79.6864630932149));
#219367=CARTESIAN_POINT('Ctrl Pts',(-26.0484936482109,68.8081121689346,
83.586769647843));
#219368=CARTESIAN_POINT('Ctrl Pts',(-26.1826991030509,74.2160488136893,
85.2379684505082));
#219369=CARTESIAN_POINT('Ctrl Pts',(-26.3169045578909,79.7903616710785,
84.2896449343191));
#219370=CARTESIAN_POINT('Ctrl Pts',(-26.4511100127309,84.3480369807344,
80.9430297969229));
#219371=CARTESIAN_POINT('Ctrl Pts',(-26.5853154675709,86.9219104419729,
75.9084414716367));
#219372=CARTESIAN_POINT('Ctrl Pts',(-26.7195209224109,86.9654652521441,
70.2539879752974));
#219373=CARTESIAN_POINT('Ctrl Pts',(-26.8089912256309,85.3021658434783,
66.8719649808209));
#219374=CARTESIAN_POINT('Ctrl Pts',(-26.8537263772509,84.1350213486955,
65.456493688071));
#219375=CARTESIAN_POINT('',(-22.5675364832709,77.7955487498991,84.4927878836045));
#219376=CARTESIAN_POINT('Ctrl Pts',(-22.5675364832709,77.7955487498991,
84.4927878836045));
#219377=CARTESIAN_POINT('Ctrl Pts',(-22.57020057496,77.8986189539504,84.4677938383652));
#219378=CARTESIAN_POINT('Ctrl Pts',(-22.5728694661945,78.0013560923501,
84.441425351644));
#219379=CARTESIAN_POINT('Ctrl Pts',(-22.5892107892951,78.6279360739735,
84.2716538955972));
#219380=CARTESIAN_POINT('Ctrl Pts',(-22.6029000963901,79.1424289701199,
84.0937531125356));
#219381=CARTESIAN_POINT('Ctrl Pts',(-22.6289955619504,80.1303737648569,
83.6729279455323));
#219382=CARTESIAN_POINT('Ctrl Pts',(-22.6413046610228,80.6032904996756,
83.4319232181733));
#219383=CARTESIAN_POINT('Ctrl Pts',(-22.6599801162175,81.2852444850775,
83.0250434517598));
#219384=CARTESIAN_POINT('Ctrl Pts',(-22.6662554006117,81.5084025291211,
82.8815572195231));
#219385=CARTESIAN_POINT('Ctrl Pts',(-22.6893343517265,82.2943804377871,
82.338381580107));
#219386=CARTESIAN_POINT('Ctrl Pts',(-22.7069178418768,82.8283053646328,
81.8966499994326));
#219387=CARTESIAN_POINT('Ctrl Pts',(-22.7321799272807,83.5438776000662,
81.1910813674927));
#219388=CARTESIAN_POINT('Ctrl Pts',(-22.7400417607241,83.7591512188104,
80.9612051460361));
#219389=CARTESIAN_POINT('Ctrl Pts',(-22.7616713766157,84.336272923027,80.2927579212079));
#219390=CARTESIAN_POINT('Ctrl Pts',(-22.7748837672195,84.6748683013689,
79.836706571722));
#219391=CARTESIAN_POINT('Ctrl Pts',(-22.7947609375764,85.1290093994207,
79.1240614113783));
#219392=CARTESIAN_POINT('Ctrl Pts',(-22.8013628413749,85.2707399299882,
78.8833333996349));
#219393=CARTESIAN_POINT('Ctrl Pts',(-22.8237826878272,85.7136353626051,
78.066924838789));
#219394=CARTESIAN_POINT('Ctrl Pts',(-22.8402920915841,85.9768545589435,
77.4705540393854));
#219395=CARTESIAN_POINT('Ctrl Pts',(-22.8648029152498,86.2956042084076,
76.5509224532606));
#219396=CARTESIAN_POINT('Ctrl Pts',(-22.8729157189773,86.3890849049698,
76.240732294204));
#219397=CARTESIAN_POINT('Ctrl Pts',(-22.8959687353953,86.6222757459949,
75.332007597257));
#219398=CARTESIAN_POINT('Ctrl Pts',(-22.9102264149159,86.7271676172055,
74.7270547941961));
#219399=CARTESIAN_POINT('Ctrl Pts',(-22.9311662489936,86.8113873864402,
73.8409316989402));
#219400=CARTESIAN_POINT('Ctrl Pts',(-22.9377614229536,86.8279978971228,
73.5625527580444));
#219401=CARTESIAN_POINT('Ctrl Pts',(-22.9606740565043,86.8513498131262,
72.6142548120919));
#219402=CARTESIAN_POINT('Ctrl Pts',(-22.9777573547803,86.8115150475681,
71.9430921213094));
#219403=CARTESIAN_POINT('Ctrl Pts',(-23.0022394040704,86.671992720847,70.9807639012866));
#219404=CARTESIAN_POINT('Ctrl Pts',(-23.0098099922342,86.6171029656124,
70.6830316311699));
#219405=CARTESIAN_POINT('Ctrl Pts',(-23.0313765416616,86.4242586048633,
69.8254003995603));
#219406=CARTESIAN_POINT('Ctrl Pts',(-23.0447944938455,86.2562544730439,
69.2740313351693));
#219407=CARTESIAN_POINT('Ctrl Pts',(-23.065253732438,85.9431262238287,68.4619538974111));
#219408=CARTESIAN_POINT('Ctrl Pts',(-23.0722491575317,85.8262076718994,
68.1895288569865));
#219409=CARTESIAN_POINT('Ctrl Pts',(-23.0965474361065,85.3945048828662,
67.2786381453861));
#219410=CARTESIAN_POINT('Ctrl Pts',(-23.1147579084652,85.0321561695621,
66.6626023543593));
#219411=CARTESIAN_POINT('Ctrl Pts',(-23.1397715132328,84.4528393429395,
65.8542689058154));
#219412=CARTESIAN_POINT('Ctrl Pts',(-23.1468311929836,84.2798722126102,
65.6303568074651));
#219413=CARTESIAN_POINT('Ctrl Pts',(-23.1676747514248,83.7351091915271,
64.9758232126111));
#219414=CARTESIAN_POINT('Ctrl Pts',(-23.1809179103934,83.3397699452139,
64.5661869646594));
#219415=CARTESIAN_POINT('Ctrl Pts',(-23.2013065948245,82.6947535281514,
63.9868464431381));
#219416=CARTESIAN_POINT('Ctrl Pts',(-23.2083909984642,82.4641120566788,
63.7949330534105));
#219417=CARTESIAN_POINT('Ctrl Pts',(-23.2324629811765,81.6734775488004,
63.1858849928466));
#219418=CARTESIAN_POINT('Ctrl Pts',(-23.2503290955504,81.0829579412128,
62.8082314172617));
#219419=CARTESIAN_POINT('Ctrl Pts',(-23.274884231175,80.2177978658097,62.3572729967872));
#219420=CARTESIAN_POINT('Ctrl Pts',(-23.2818169730839,79.967217664736,62.2376943942904));
#219421=CARTESIAN_POINT('Ctrl Pts',(-23.3035186130702,79.1544845790314,
61.8849216123229));
#219422=CARTESIAN_POINT('Ctrl Pts',(-23.3176588018278,78.5780955922533,
61.6868980638989));
#219423=CARTESIAN_POINT('Ctrl Pts',(-23.3388664824491,77.7066199935249,
61.4600378228033));
#219424=CARTESIAN_POINT('Ctrl Pts',(-23.3458199835038,77.4198619529216,
61.396604555484));
#219425=CARTESIAN_POINT('Ctrl Pts',(-23.3682626536289,76.5069885405669,
61.2296514049591));
#219426=CARTESIAN_POINT('Ctrl Pts',(-23.3844526926338,75.8736638451558,
61.1651917383188));
#219427=CARTESIAN_POINT('Ctrl Pts',(-23.4076843716132,74.9528259617888,
61.1458073048551));
#219428=CARTESIAN_POINT('Ctrl Pts',(-23.4148695247683,74.6661283998542,
61.1502002309265));
#219429=CARTESIAN_POINT('Ctrl Pts',(-23.4372061343355,73.7588131708991,
61.197598239086));
#219430=CARTESIAN_POINT('Ctrl Pts',(-23.4516854993141,73.1415158302191,
61.2799207344635));
#219431=CARTESIAN_POINT('Ctrl Pts',(-23.473533726284,72.2341061026627,61.4737526344134));
#219432=CARTESIAN_POINT('Ctrl Pts',(-23.4808192690093,71.9355685750294,
61.5497313157579));
#219433=CARTESIAN_POINT('Ctrl Pts',(-23.5040385331771,71.014023313647,61.8225462972615));
#219434=CARTESIAN_POINT('Ctrl Pts',(-23.5207281916319,70.4027817691001,
62.0593503041463));
#219435=CARTESIAN_POINT('Ctrl Pts',(-23.5441129061023,69.5685973983824,
62.4648501692936));
#219436=CARTESIAN_POINT('Ctrl Pts',(-23.5509830628036,69.3260891034714,
62.59337145393));
#219437=CARTESIAN_POINT('Ctrl Pts',(-23.5725188546093,68.5661799106487,
63.0311669320326));
#219438=CARTESIAN_POINT('Ctrl Pts',(-23.586588727842,68.0679695342834,63.3723514817946));
#219439=CARTESIAN_POINT('Ctrl Pts',(-23.6083405871129,67.3474767903162,
63.95030372947));
#219440=CARTESIAN_POINT('Ctrl Pts',(-23.6159578353336,67.1044412778182,
64.1620087200796));
#219441=CARTESIAN_POINT('Ctrl Pts',(-23.6398805770154,66.3842235118891,
64.8424376056803));
#219442=CARTESIAN_POINT('Ctrl Pts',(-23.6569839558425,65.9366017169724,
65.3425405823433));
#219443=CARTESIAN_POINT('Ctrl Pts',(-23.6804648193498,65.3762271197312,
66.0871527080676));
#219444=CARTESIAN_POINT('Ctrl Pts',(-23.6870485851372,65.2250152201063,
66.3027475337575));
#219445=CARTESIAN_POINT('Ctrl Pts',(-23.7082031998031,64.753963308414,67.0253571545259));
#219446=CARTESIAN_POINT('Ctrl Pts',(-23.7222219941295,64.4655565082912,
67.5526944759199));
#219447=CARTESIAN_POINT('Ctrl Pts',(-23.7441210530631,64.0823007145137,
68.3991972044232));
#219448=CARTESIAN_POINT('Ctrl Pts',(-23.7519297485862,63.958711695808,68.7054045196297));
#219449=CARTESIAN_POINT('Ctrl Pts',(-23.7755298190367,63.6308976035494,
69.6255567349071));
#219450=CARTESIAN_POINT('Ctrl Pts',(-23.792048790264,63.4632551739869,70.2525895074537));
#219451=CARTESIAN_POINT('Ctrl Pts',(-23.8151391213084,63.3001472115414,
71.153731134077));
#219452=CARTESIAN_POINT('Ctrl Pts',(-23.8218753913198,63.2612963769365,
71.4200932362866));
#219453=CARTESIAN_POINT('Ctrl Pts',(-23.843355585872,63.1650974492894,72.2904016805072));
#219454=CARTESIAN_POINT('Ctrl Pts',(-23.8575579717944,63.145631815119,72.898341634899));
#219455=CARTESIAN_POINT('Ctrl Pts',(-23.8798554463621,63.1873990800895,
73.8427727913731));
#219456=CARTESIAN_POINT('Ctrl Pts',(-23.887881609621,63.216813015148,74.1806799322862));
#219457=CARTESIAN_POINT('Ctrl Pts',(-23.9110847210234,63.3405837357239,
75.1323771410192));
#219458=CARTESIAN_POINT('Ctrl Pts',(-23.9269053581018,63.468623089633,75.7418298181613));
#219459=CARTESIAN_POINT('Ctrl Pts',(-23.9495459158704,63.7217406618819,
76.6026846920868));
#219460=CARTESIAN_POINT('Ctrl Pts',(-23.9564812052755,63.8091170388149,
76.8653374683132));
#219461=CARTESIAN_POINT('Ctrl Pts',(-23.9783573497345,64.1204864991392,
77.7003660271091));
#219462=CARTESIAN_POINT('Ctrl Pts',(-23.9927641337887,64.3807005120457,
78.2589304827354));
#219463=CARTESIAN_POINT('Ctrl Pts',(-24.0155119050265,64.8537349412677,
79.0984245577657));
#219464=CARTESIAN_POINT('Ctrl Pts',(-24.0237891876257,65.0385506994134,
79.3951516670683));
#219465=CARTESIAN_POINT('Ctrl Pts',(-24.0466112890865,65.5718426865505,
80.1732424407906));
#219466=CARTESIAN_POINT('Ctrl Pts',(-24.061713459637,65.9442499022712,80.638247657376));
#219467=CARTESIAN_POINT('Ctrl Pts',(-24.0839137958729,66.5441568990323,
81.2812040167609));
#219468=CARTESIAN_POINT('Ctrl Pts',(-24.0910796733781,66.7465124049511,
81.4828824607709));
#219469=CARTESIAN_POINT('Ctrl Pts',(-24.1140575951936,67.4331012610335,
82.1183964911304));
#219470=CARTESIAN_POINT('Ctrl Pts',(-24.1292856506185,67.9468370336629,
82.5197843027144));
#219471=CARTESIAN_POINT('Ctrl Pts',(-24.1528881185346,68.7808017523536,
83.0682211280822));
#219472=CARTESIAN_POINT('Ctrl Pts',(-24.1611669801198,69.0802693316402,
83.2468935918944));
#219473=CARTESIAN_POINT('Ctrl Pts',(-24.1827559596315,69.8637794574601,
83.6690821495143));
#219474=CARTESIAN_POINT('Ctrl Pts',(-24.1964874148006,70.3580881161013,
83.8935996769948));
#219475=CARTESIAN_POINT('Ctrl Pts',(-24.2174768257465,71.1364599998422,
84.1843685432711));
#219476=CARTESIAN_POINT('Ctrl Pts',(-24.2247571552002,71.4113489338992,
84.2756825250916));
#219477=CARTESIAN_POINT('Ctrl Pts',(-24.2483756982722,72.3324484517258,
84.5438270605486));
#219478=CARTESIAN_POINT('Ctrl Pts',(-24.2640946299929,72.9914513912487,
84.6754742522766));
#219479=CARTESIAN_POINT('Ctrl Pts',(-24.2884926428813,74.0156156886253,
84.7918940226994));
#219480=CARTESIAN_POINT('Ctrl Pts',(-24.2970807599793,74.3762971206503,
84.8163932788444));
#219481=CARTESIAN_POINT('Ctrl Pts',(-24.3182126869123,75.2466209141566,
84.8359863747899));
#219482=CARTESIAN_POINT('Ctrl Pts',(-24.3310868478748,75.7566507505651,
84.8148743652156));
#219483=CARTESIAN_POINT('Ctrl Pts',(-24.3515180034847,76.5608378528089,
84.7292196212533));
#219484=CARTESIAN_POINT('Ctrl Pts',(-24.3590613604394,76.8574867488332,
84.6861535064085));
#219485=CARTESIAN_POINT('Ctrl Pts',(-24.3815384824962,77.7544613305933,
84.5202236828188));
#219486=CARTESIAN_POINT('Ctrl Pts',(-24.3960069964872,78.3477178880852,
84.361341433531));
#219487=CARTESIAN_POINT('Ctrl Pts',(-24.4200877479237,79.3072200064098,
84.0234693101181));
#219488=CARTESIAN_POINT('Ctrl Pts',(-24.4296875364305,79.6823105056442,
83.8695157327653));
#219489=CARTESIAN_POINT('Ctrl Pts',(-24.4517726454238,80.5078291005356,
83.4806056486065));
#219490=CARTESIAN_POINT('Ctrl Pts',(-24.4645281627022,80.9532717977727,
83.2349870119567));
#219491=CARTESIAN_POINT('Ctrl Pts',(-24.4851445577003,81.6411742965046,
82.7956074273199));
#219492=CARTESIAN_POINT('Ctrl Pts',(-24.4929344656444,81.8949348538698,
82.6191436156419));
#219493=CARTESIAN_POINT('Ctrl Pts',(-24.5153697889198,82.619984577831,82.070718348575));
#219494=CARTESIAN_POINT('Ctrl Pts',(-24.5295968633422,83.0704217941672,
81.6718532422128));
#219495=CARTESIAN_POINT('Ctrl Pts',(-24.554091465893,83.7903371793909,80.9304241509068));
#219496=CARTESIAN_POINT('Ctrl Pts',(-24.5643657502694,84.0753692732483,
80.6029215596418));
#219497=CARTESIAN_POINT('Ctrl Pts',(-24.5860905187513,84.6271653904445,
79.8945679247614));
#219498=CARTESIAN_POINT('Ctrl Pts',(-24.5976840511342,84.8912036495773,
79.5115417221267));
#219499=CARTESIAN_POINT('Ctrl Pts',(-24.617262056823,85.293140859179,78.8479458411522));
#219500=CARTESIAN_POINT('Ctrl Pts',(-24.6251367322929,85.4439388309394,
78.5751882904976));
#219501=CARTESIAN_POINT('Ctrl Pts',(-24.6472317420049,85.8435223149737,
77.7784500695001));
#219502=CARTESIAN_POINT('Ctrl Pts',(-24.6610648696817,86.064663119611,77.2407094456923));
#219503=CARTESIAN_POINT('Ctrl Pts',(-24.6908945637501,86.456482279828,76.0472767679595));
#219504=CARTESIAN_POINT('Ctrl Pts',(-24.7068825789411,86.6127117295968,
75.3867366115711));
#219505=CARTESIAN_POINT('Ctrl Pts',(-24.7317749488679,86.7608860128367,
74.3879117013379));
#219506=CARTESIAN_POINT('Ctrl Pts',(-24.7401923448889,86.7959664499832,
74.0559075222126));
#219507=CARTESIAN_POINT('Ctrl Pts',(-24.7610996526957,86.8479953481639,
73.2283760432133));
#219508=CARTESIAN_POINT('Ctrl Pts',(-24.7733789330877,86.8476760342599,
72.7345232328296));
#219509=CARTESIAN_POINT('Ctrl Pts',(-24.7975533204227,86.7836960464734,
71.7369892425435));
#219510=CARTESIAN_POINT('Ctrl Pts',(-24.8094922231537,86.7191369403297,
71.2360827207114));
#219511=CARTESIAN_POINT('Ctrl Pts',(-24.8351973708289,86.5135805647042,
70.1752564221972));
#219512=CARTESIAN_POINT('Ctrl Pts',(-24.8489873208505,86.3628986201724,
69.6171097101358));
#219513=CARTESIAN_POINT('Ctrl Pts',(-24.8715693593638,86.0622123163689,
68.7570415397356));
#219514=CARTESIAN_POINT('Ctrl Pts',(-24.8800360304052,85.9384552655299,
68.4458729535653));
#219515=CARTESIAN_POINT('Ctrl Pts',(-24.9001649362168,85.6112311385889,
67.7156793928889));
#219516=CARTESIAN_POINT('Ctrl Pts',(-24.9116058676399,85.396369265071,67.3042388229351));
#219517=CARTESIAN_POINT('Ctrl Pts',(-24.9367735041841,84.8601517743417,
66.4104777396542));
#219518=CARTESIAN_POINT('Ctrl Pts',(-24.9504401609291,84.5264363613093,
65.9367826121221));
#219519=CARTESIAN_POINT('Ctrl Pts',(-24.9762719223674,83.8412346330971,
65.0999867800875));
#219520=CARTESIAN_POINT('Ctrl Pts',(-24.988409640136,83.4974722462777,64.7304245665329));
#219521=CARTESIAN_POINT('Ctrl Pts',(-25.0096077839032,82.8773660160728,
64.1434312757467));
#219522=CARTESIAN_POINT('Ctrl Pts',(-25.0184772157898,82.6123823701233,
63.913945254008));
#219523=CARTESIAN_POINT('Ctrl Pts',(-25.0395422051444,81.9532506677364,
63.3929967902393));
#219524=CARTESIAN_POINT('Ctrl Pts',(-25.0514814805335,81.5511328915323,
63.1146464292182));
#219525=CARTESIAN_POINT('Ctrl Pts',(-25.0840133009892,80.3941703566912,
62.4152363686961));
#219526=CARTESIAN_POINT('Ctrl Pts',(-25.1043194792746,79.6056888110137,
62.0491341885759));
#219527=CARTESIAN_POINT('Ctrl Pts',(-25.1367303308557,78.3488610258597,
61.6238004627972));
#219528=CARTESIAN_POINT('Ctrl Pts',(-25.1483805833474,77.9017929008133,
61.5009928872115));
#219529=CARTESIAN_POINT('Ctrl Pts',(-25.1736387791005,76.9166702380028,
61.2922240109876));
#219530=CARTESIAN_POINT('Ctrl Pts',(-25.1869032847806,76.3787629153572,
61.2172565919378));
#219531=CARTESIAN_POINT('Ctrl Pts',(-25.2253210748964,74.7863988798278,
61.1055687752883));
#219532=CARTESIAN_POINT('Ctrl Pts',(-25.250090444864,73.7242219547311,61.1721868803465));
#219533=CARTESIAN_POINT('Ctrl Pts',(-25.2866111132704,72.2845467613406,
61.4573505048091));
#219534=CARTESIAN_POINT('Ctrl Pts',(-25.2970871456356,71.8831317764291,
61.5589234989088));
#219535=CARTESIAN_POINT('Ctrl Pts',(-25.3184977186717,71.0566922455767,
61.8158529900833));
#219536=CARTESIAN_POINT('Ctrl Pts',(-25.3294252814237,70.6336872745983,
61.9747898835024));
#219537=CARTESIAN_POINT('Ctrl Pts',(-25.3664389521094,69.224983734498,62.5976549392384));
#219538=CARTESIAN_POINT('Ctrl Pts',(-25.3922393395229,68.2890682628324,
63.1752085088464));
#219539=CARTESIAN_POINT('Ctrl Pts',(-25.4259722928531,67.2491754939645,
64.0348422237022));
#219540=CARTESIAN_POINT('Ctrl Pts',(-25.4325115690716,67.0540968903417,
64.2072922574925));
#219541=CARTESIAN_POINT('Ctrl Pts',(-25.4584055637037,66.2959902400183,
64.9243007064588));
#219542=CARTESIAN_POINT('Ctrl Pts',(-25.4771545578628,65.7814875746081,
65.5197326738897));
#219543=CARTESIAN_POINT('Ctrl Pts',(-25.5148345335165,64.8751005493501,
66.8039004480212));
#219544=CARTESIAN_POINT('Ctrl Pts',(-25.5338126922381,64.4839903217007,
67.493477634905));
#219545=CARTESIAN_POINT('Ctrl Pts',(-25.5649471766414,63.9795411951626,
68.6360369703729));
#219546=CARTESIAN_POINT('Ctrl Pts',(-25.5764187225231,63.8191580945081,
69.0661282181788));
#219547=CARTESIAN_POINT('Ctrl Pts',(-25.603688483182,63.4919624499032,70.1319500539696));
#219548=CARTESIAN_POINT('Ctrl Pts',(-25.6193638008781,63.3521684057306,
70.7735126728818));
#219549=CARTESIAN_POINT('Ctrl Pts',(-25.6676404655836,63.0864418801701,
72.7654883718108));
#219550=CARTESIAN_POINT('Ctrl Pts',(-25.706840999802,63.1059826913564,74.3538296879236));
#219551=CARTESIAN_POINT('Ctrl Pts',(-25.7677255171453,63.7638553875792,
76.7915398688821));
#219552=CARTESIAN_POINT('Ctrl Pts',(-25.7857162873499,64.0285142642929,
77.4989934914382));
#219553=CARTESIAN_POINT('Ctrl Pts',(-25.8216296569917,64.6722868814089,
78.8228079190137));
#219554=CARTESIAN_POINT('Ctrl Pts',(-25.8397202960589,65.0455123990101,
79.4404836250716));
#219555=CARTESIAN_POINT('Ctrl Pts',(-25.8779933757973,65.9757398435127,
80.6982002111685));
#219556=CARTESIAN_POINT('Ctrl Pts',(-25.8981363569753,66.5480633616065,
81.3205005295193));
#219557=CARTESIAN_POINT('Ctrl Pts',(-25.9560699763327,68.3473269415652,
82.9051067066646));
#219558=CARTESIAN_POINT('Ctrl Pts',(-25.9943208487966,69.6965948309391,
83.6873917917103));
#219559=CARTESIAN_POINT('Ctrl Pts',(-26.0504698449138,71.8964316437276,
84.4389540762596));
#219560=CARTESIAN_POINT('Ctrl Pts',(-26.0690068428248,72.6478528993156,
84.6172928635994));
#219561=CARTESIAN_POINT('Ctrl Pts',(-26.0987433017722,73.8478147827651,
84.7809478793954));
#219562=CARTESIAN_POINT('Ctrl Pts',(-26.1097342408935,74.2886635798881,
84.8159239396859));
#219563=CARTESIAN_POINT('Ctrl Pts',(-26.1470592789864,75.8092294267076,
84.8494497159255));
#219564=CARTESIAN_POINT('Ctrl Pts',(-26.1729518813649,76.8897272377984,
84.72474497924));
#219565=CARTESIAN_POINT('Ctrl Pts',(-26.2178106992323,78.6797282706776,
84.2682050190598));
#219566=CARTESIAN_POINT('Ctrl Pts',(-26.2368585546459,79.4076525968821,
84.0054976991742));
#219567=CARTESIAN_POINT('Ctrl Pts',(-26.2902157122182,81.3708528596096,
83.0654858951152));
#219568=CARTESIAN_POINT('Ctrl Pts',(-26.3238790172103,82.5270414745748,
82.2333806609559));
#219569=CARTESIAN_POINT('Ctrl Pts',(-26.3765014687122,84.0251050977193,
80.6895409789442));
#219570=CARTESIAN_POINT('Ctrl Pts',(-26.3948351634072,84.4913388247058,
80.1056895027049));
#219571=CARTESIAN_POINT('Ctrl Pts',(-26.4317390531022,85.3210198323614,
78.8383967304916));
#219572=CARTESIAN_POINT('Ctrl Pts',(-26.4503794465544,85.6797463911431,
78.1542057638403));
#219573=CARTESIAN_POINT('Ctrl Pts',(-26.5123917579555,86.6405138063311,
75.7924075027471));
#219574=CARTESIAN_POINT('Ctrl Pts',(-26.5502886691223,86.8455265760331,
74.2307446510401));
#219575=CARTESIAN_POINT('Ctrl Pts',(-26.6012489913111,86.8339025086032,
72.1366724849289));
#219576=CARTESIAN_POINT('Ctrl Pts',(-26.6203470832269,86.7522129909423,
71.3519615397537));
#219577=CARTESIAN_POINT('Ctrl Pts',(-26.6587218863114,86.4333670988627,
69.8126333019412));
#219578=CARTESIAN_POINT('Ctrl Pts',(-26.6778923634462,86.1958740644985,
69.0608841198639));
#219579=CARTESIAN_POINT('Ctrl Pts',(-26.6970005540986,85.8880596524678,
68.34079083356));
#219580=CARTESIAN_POINT('',(-22.5673849603904,86.330959246387,76.420933693241));
#219581=CARTESIAN_POINT('Ctrl Pts',(-22.5675364832709,86.3312297555765,
76.4210531081684));
#219582=CARTESIAN_POINT('Ctrl Pts',(-22.5675364832709,86.2741961678896,
76.6088225515153));
#219583=CARTESIAN_POINT('Ctrl Pts',(-22.5675364832709,86.2126796921151,
76.7945020356719));
#219584=CARTESIAN_POINT('Ctrl Pts',(-22.5675364832709,86.1467811019396,
76.9781622505484));
#219585=CARTESIAN_POINT('Ctrl Pts',(-22.5675364832709,86.0815911235665,
77.1598475552553));
#219586=CARTESIAN_POINT('Ctrl Pts',(-22.5675364832709,86.0121124400483,
77.3395571455578));
#219587=CARTESIAN_POINT('Ctrl Pts',(-22.5675364832709,85.9383902127073,
77.517347311963));
#219588=CARTESIAN_POINT('Ctrl Pts',(-22.5675364832709,85.8644998030371,
77.6955430706213));
#219589=CARTESIAN_POINT('Ctrl Pts',(-22.5675364832709,85.7863462811828,
77.8718110268535));
#219590=CARTESIAN_POINT('Ctrl Pts',(-22.5675364832709,85.7039258441626,
78.0461899470055));
#219591=CARTESIAN_POINT('Ctrl Pts',(-22.5675364832709,85.6216695539327,
78.220221577807));
#219592=CARTESIAN_POINT('Ctrl Pts',(-22.5675364832709,85.5351631316391,
78.3923720716048));
#219593=CARTESIAN_POINT('Ctrl Pts',(-22.5675364832709,85.444356675763,78.5626563901228));
#219594=CARTESIAN_POINT('Ctrl Pts',(-22.5675364832709,85.3519074893335,
78.7360212302853));
#219595=CARTESIAN_POINT('Ctrl Pts',(-22.5675364832709,85.2550012483283,
78.9074522897057));
#219596=CARTESIAN_POINT('Ctrl Pts',(-22.5675364832709,85.1535389696411,
79.0769339040888));
#219597=CARTESIAN_POINT('Ctrl Pts',(-22.5675364832709,85.1330135891876,
79.1112193021707));
#219598=CARTESIAN_POINT('Ctrl Pts',(-22.5675364832709,85.112301611534,79.1454248056277));
#219599=CARTESIAN_POINT('Ctrl Pts',(-22.5675364832709,85.0914019942509,
79.1795501013667));
#219600=CARTESIAN_POINT('Ctrl Pts',(-22.5675364832709,85.0825999660734,
79.1939222217069));
#219601=CARTESIAN_POINT('Ctrl Pts',(-22.5675364832709,85.0737635427412,
79.2082819117213));
#219602=CARTESIAN_POINT('Ctrl Pts',(-22.5675364832709,85.0648962129969,
79.222623373383));
#219603=CARTESIAN_POINT('Ctrl Pts',(-22.5675364832709,84.9624524331881,
79.3883095024615));
#219604=CARTESIAN_POINT('Ctrl Pts',(-22.5675364832709,84.8563336126465,
79.5508453778107));
#219605=CARTESIAN_POINT('Ctrl Pts',(-22.5675364832709,84.7465736948364,
79.7102890244569));
#219606=CARTESIAN_POINT('Ctrl Pts',(-22.5675364832709,84.6366989413994,
79.8698994880202));
#219607=CARTESIAN_POINT('Ctrl Pts',(-22.5675364832709,84.5231752483645,
80.0264116209949));
#219608=CARTESIAN_POINT('Ctrl Pts',(-22.5675364832709,84.4059903046976,
80.1798598391719));
#219609=CARTESIAN_POINT('Ctrl Pts',(-22.5675364832709,84.317637523426,80.2955536854363));
#219610=CARTESIAN_POINT('Ctrl Pts',(-22.5675364832709,84.2272025167764,
80.4095053825114));
#219611=CARTESIAN_POINT('Ctrl Pts',(-22.5675364832709,84.1346637067308,
80.5217187995516));
#219612=CARTESIAN_POINT('Ctrl Pts',(-22.5675364832709,84.012033104306,80.6704218023783));
#219613=CARTESIAN_POINT('Ctrl Pts',(-22.5675364832709,83.8857092626351,
80.8160736234435));
#219614=CARTESIAN_POINT('Ctrl Pts',(-22.5675364832709,83.7556896189918,
80.9587217968264));
#219615=CARTESIAN_POINT('Ctrl Pts',(-22.5675364832709,83.6254862248831,
81.1015715679642));
#219616=CARTESIAN_POINT('Ctrl Pts',(-22.5675364832709,83.4915762569568,
81.2414094809198));
#219617=CARTESIAN_POINT('Ctrl Pts',(-22.5675364832709,83.3539211456636,
81.3782455399667));
#219618=CARTESIAN_POINT('Ctrl Pts',(-22.5675364832709,83.2896251453197,
81.4421589770841));
#219619=CARTESIAN_POINT('Ctrl Pts',(-22.5675364832709,83.2245116076313,
81.5054169551686));
#219620=CARTESIAN_POINT('Ctrl Pts',(-22.5675364832709,83.1585742143027,
81.5680174025649));
#219621=CARTESIAN_POINT('Ctrl Pts',(-22.5675364832709,83.1405216939231,
81.5851563247355));
#219622=CARTESIAN_POINT('Ctrl Pts',(-22.5675364832709,83.1224029438513,
81.6022500915066));
#219623=CARTESIAN_POINT('Ctrl Pts',(-22.5675364832709,83.1042427730916,
81.6192753723487));
#219624=CARTESIAN_POINT('Ctrl Pts',(-22.5675364832709,82.9650663051577,
81.7497542364821));
#219625=CARTESIAN_POINT('Ctrl Pts',(-22.5675364832709,82.8232381806961,
81.8764274622056));
#219626=CARTESIAN_POINT('Ctrl Pts',(-22.5675364832709,82.6787893153765,
81.999396709168));
#219627=CARTESIAN_POINT('Ctrl Pts',(-22.5675364832709,82.5335582360053,
82.1230318545621));
#219628=CARTESIAN_POINT('Ctrl Pts',(-22.5675364832709,82.3856776242889,
82.2429230596935));
#219629=CARTESIAN_POINT('Ctrl Pts',(-22.5675364832709,82.2351403062011,
82.3591374574759));
#219630=CARTESIAN_POINT('Ctrl Pts',(-22.5675364832709,82.0844127264509,
82.4754987367413));
#219631=CARTESIAN_POINT('Ctrl Pts',(-22.5675364832709,81.931021378805,82.5881741645978));
#219632=CARTESIAN_POINT('Ctrl Pts',(-22.5675364832709,81.7749255723342,
82.6971910900871));
#219633=CARTESIAN_POINT('Ctrl Pts',(-22.5675364832709,81.6196215858302,
82.8056550104683));
#219634=CARTESIAN_POINT('Ctrl Pts',(-22.5675364832709,81.4616401560816,
82.9104976774395));
#219635=CARTESIAN_POINT('Ctrl Pts',(-22.5675364832709,81.3009133123836,
83.0117028803056));
#219636=CARTESIAN_POINT('Ctrl Pts',(-22.5675364832709,81.1803681796102,
83.0876067824552));
#219637=CARTESIAN_POINT('Ctrl Pts',(-22.5675364832709,81.058278152601,83.16146375779));
#219638=CARTESIAN_POINT('Ctrl Pts',(-22.5675364832709,80.9346059377799,
83.2332496877048));
#219639=CARTESIAN_POINT('Ctrl Pts',(-22.5675364832709,80.8809466249279,
83.2643964062887));
#219640=CARTESIAN_POINT('Ctrl Pts',(-22.5675364832709,80.8269893718125,
83.2951530448035));
#219641=CARTESIAN_POINT('Ctrl Pts',(-22.5675364832709,80.7727307612443,
83.325516709298));
#219642=CARTESIAN_POINT('Ctrl Pts',(-22.5675364832709,80.7409297866078,
83.3433128547273));
#219643=CARTESIAN_POINT('Ctrl Pts',(-22.5675364832709,80.7090252876808,
83.3609739976518));
#219644=CARTESIAN_POINT('Ctrl Pts',(-22.5675364832709,80.6770165441255,
83.3784994627323));
#219645=CARTESIAN_POINT('Ctrl Pts',(-22.5675364832709,80.6572219751036,
83.3893374085446));
#219646=CARTESIAN_POINT('Ctrl Pts',(-22.5675364832709,80.6373836646383,
83.400125523986));
#219647=CARTESIAN_POINT('Ctrl Pts',(-22.5675364832709,80.6175267978189,
83.4108500412261));
#219648=CARTESIAN_POINT('Ctrl Pts',(-22.5675364832709,80.4393377980143,
83.507088335906));
#219649=CARTESIAN_POINT('Ctrl Pts',(-22.5675364832709,80.2592938419621,
83.5984099220634));
#219650=CARTESIAN_POINT('Ctrl Pts',(-22.5675364832709,80.0774194424533,
83.6848466134901));
#219651=CARTESIAN_POINT('Ctrl Pts',(-22.5675364832709,79.9816186497369,
83.7303764053729));
#219652=CARTESIAN_POINT('Ctrl Pts',(-22.5675364832709,79.8853094574927,
83.7745501568457));
#219653=CARTESIAN_POINT('Ctrl Pts',(-22.5675364832709,79.7884922163416,
83.8173676866023));
#219654=CARTESIAN_POINT('Ctrl Pts',(-22.5675364832709,79.6051464451119,
83.8984525525005));
#219655=CARTESIAN_POINT('Ctrl Pts',(-22.5675364832709,79.4199800239593,
83.9746766474747));
#219656=CARTESIAN_POINT('Ctrl Pts',(-22.5675364832709,79.2330235033904,
84.0461131619167));
#219657=CARTESIAN_POINT('Ctrl Pts',(-22.5675364832709,79.0453490386799,
84.1178240044586));
#219658=CARTESIAN_POINT('Ctrl Pts',(-22.5675364832709,78.8558702756082,
84.1847105346891));
#219659=CARTESIAN_POINT('Ctrl Pts',(-22.5675364832709,78.6645986034204,
84.2467978873678));
#219660=CARTESIAN_POINT('Ctrl Pts',(-22.5675364832709,78.4733713416908,
84.30887082428));
#219661=CARTESIAN_POINT('Ctrl Pts',(-22.5675364832709,78.2803515695058,
84.3661469096114));
#219662=CARTESIAN_POINT('Ctrl Pts',(-22.5675364832709,78.0855376558692,
84.4186009739626));
#219663=CARTESIAN_POINT('Ctrl Pts',(-22.5675364832709,77.9893128513891,
84.4445097090841));
#219664=CARTESIAN_POINT('Ctrl Pts',(-22.5675364832709,77.892650173136,84.4692412399597));
#219665=CARTESIAN_POINT('Ctrl Pts',(-22.5675364832709,77.7955487498991,
84.4927878836045));
#219666=CARTESIAN_POINT('',(-22.5675364837383,86.3349224095373,76.4088722770814));
#219667=CARTESIAN_POINT('Ctrl Pts',(-22.5673829558621,86.3309582618541,
76.4209333437238));
#219668=CARTESIAN_POINT('Ctrl Pts',(-22.5674341318949,86.3322817703421,
76.4169137400224));
#219669=CARTESIAN_POINT('Ctrl Pts',(-22.5674853079278,86.3336031532802,
76.4128933831607));
#219670=CARTESIAN_POINT('Ctrl Pts',(-22.5675364839606,86.3349224096848,
76.4088722753861));
#219671=CARTESIAN_POINT('Ctrl Pts',(-22.5675364837383,86.3349224095373,
76.4088722770814));
#219672=CARTESIAN_POINT('Ctrl Pts',(-22.5862680853234,86.5592443815844,
75.6674670848345));
#219673=CARTESIAN_POINT('Ctrl Pts',(-22.6057724255725,86.7082163959447,
74.9097552024436));
#219674=CARTESIAN_POINT('Ctrl Pts',(-22.6429310858987,86.8542170642046,
73.4058157535164));
#219675=CARTESIAN_POINT('Ctrl Pts',(-22.6606405257108,86.8569370758779,
72.6625676819964));
#219676=CARTESIAN_POINT('Ctrl Pts',(-22.6917079591717,86.7417407420671,
71.3752055763466));
#219677=CARTESIAN_POINT('Ctrl Pts',(-22.7050393165119,86.6541791296153,
70.828225798091));
#219678=CARTESIAN_POINT('Ctrl Pts',(-22.7250377762276,86.4692968267006,
70.0378179720206));
#219679=CARTESIAN_POINT('Ctrl Pts',(-22.7314888115047,86.4019218698674,
69.7878453758678));
#219680=CARTESIAN_POINT('Ctrl Pts',(-22.7709634204644,85.9375775027767,
68.2665105161627));
#219681=CARTESIAN_POINT('Ctrl Pts',(-22.8027640999299,85.3320805150328,
67.058188819128));
#219682=CARTESIAN_POINT('Ctrl Pts',(-22.8537481998869,84.0928908798262,
65.3669320568875));
#219683=CARTESIAN_POINT('Ctrl Pts',(-22.8725290298923,83.5843297564767,
64.7993630234584));
#219684=CARTESIAN_POINT('Ctrl Pts',(-22.9239292449124,82.0380819403647,
63.3764671688534));
#219685=CARTESIAN_POINT('Ctrl Pts',(-22.9604267297466,80.7640570361906,
62.5103550986123));
#219686=CARTESIAN_POINT('Ctrl Pts',(-23.0202928869871,78.4706153454157,
61.6432305647928));
#219687=CARTESIAN_POINT('Ctrl Pts',(-23.0392730866337,77.7207900189858,
61.4414365269494));
#219688=CARTESIAN_POINT('Ctrl Pts',(-23.0930290504125,75.5544958242202,
61.0779603516221));
#219689=CARTESIAN_POINT('Ctrl Pts',(-23.1299594944175,73.9801568529781,
61.0706562319372));
#219690=CARTESIAN_POINT('Ctrl Pts',(-23.1905021030076,71.5870961726182,
61.6282648933797));
#219691=CARTESIAN_POINT('Ctrl Pts',(-23.209090806836,70.8699378838349,61.8685784075968));
#219692=CARTESIAN_POINT('Ctrl Pts',(-23.2410740979785,69.6615834129092,
62.4056935084534));
#219693=CARTESIAN_POINT('Ctrl Pts',(-23.2545074008348,69.157778146997,62.6745433313228));
#219694=CARTESIAN_POINT('Ctrl Pts',(-23.2863973120801,68.049292023537,63.3759610656699));
#219695=CARTESIAN_POINT('Ctrl Pts',(-23.304848079247,67.4618353137888,63.8305898999364));
#219696=CARTESIAN_POINT('Ctrl Pts',(-23.3350930669858,66.5677869315017,
64.6654052882002));
#219697=CARTESIAN_POINT('Ctrl Pts',(-23.3469809107229,66.2342709156701,
65.0169928637897));
#219698=CARTESIAN_POINT('Ctrl Pts',(-23.3689390275803,65.6479137832039,
65.7159828751924));
#219699=CARTESIAN_POINT('Ctrl Pts',(-23.3790075514597,65.3902080122086,
66.05931915499));
#219700=CARTESIAN_POINT('Ctrl Pts',(-23.3969914175802,64.9729130265417,
66.6842488965277));
#219701=CARTESIAN_POINT('Ctrl Pts',(-23.4048424767607,64.8051745741039,
66.9596772122863));
#219702=CARTESIAN_POINT('Ctrl Pts',(-23.4296186292682,64.3175556008988,
67.8394688951344));
#219703=CARTESIAN_POINT('Ctrl Pts',(-23.4468326360178,64.0380624442595,
68.4665319016422));
#219704=CARTESIAN_POINT('Ctrl Pts',(-23.4767056660225,63.641609652087,69.6102254268264));
#219705=CARTESIAN_POINT('Ctrl Pts',(-23.4894017651609,63.5020116401143,
70.119178511537));
#219706=CARTESIAN_POINT('Ctrl Pts',(-23.509717800407,63.3305870527547,70.960607381492));
#219707=CARTESIAN_POINT('Ctrl Pts',(-23.5175437050303,63.2780012942616,
71.2888547719588));
#219708=CARTESIAN_POINT('Ctrl Pts',(-23.537280129187,63.1830131244648,72.1037210969697));
#219709=CARTESIAN_POINT('Ctrl Pts',(-23.549400167054,63.1571013464539,72.5918834219285));
#219710=CARTESIAN_POINT('Ctrl Pts',(-23.5734791553166,63.1652689824181,
73.5553851328984));
#219711=CARTESIAN_POINT('Ctrl Pts',(-23.5854383058723,63.1979133534347,
74.0310234500722));
#219712=CARTESIAN_POINT('Ctrl Pts',(-23.6099759330427,63.3252210027845,
75.01885650904));
#219713=CARTESIAN_POINT('Ctrl Pts',(-23.6223585606802,63.4253801393107,
75.5304187723416));
#219714=CARTESIAN_POINT('Ctrl Pts',(-23.6423017686356,63.6419834592016,
76.3472594597781));
#219715=CARTESIAN_POINT('Ctrl Pts',(-23.64996574602,63.7382098911753,76.6579018594108));
#219716=CARTESIAN_POINT('Ctrl Pts',(-23.6713796367493,64.0366083519891,
77.4955707899602));
#219717=CARTESIAN_POINT('Ctrl Pts',(-23.6855188631018,64.2643953263507,
78.0123852988475));
#219718=CARTESIAN_POINT('Ctrl Pts',(-23.7091552450763,64.7041018085207,
78.8448886272887));
#219719=CARTESIAN_POINT('Ctrl Pts',(-23.7186618439811,64.897017806972,79.1713809851635));
#219720=CARTESIAN_POINT('Ctrl Pts',(-23.7427639934684,65.434825799796,79.9901439374208));
#219721=CARTESIAN_POINT('Ctrl Pts',(-23.7568771368583,65.8025691386141,
80.4674901565216));
#219722=CARTESIAN_POINT('Ctrl Pts',(-23.778152865229,66.4046745762888,81.1368390030206));
#219723=CARTESIAN_POINT('Ctrl Pts',(-23.7852645329274,66.613437030011,81.3518844373747));
#219724=CARTESIAN_POINT('Ctrl Pts',(-23.8051161905732,67.2061691993328,
81.917120638316));
#219725=CARTESIAN_POINT('Ctrl Pts',(-23.8181956316294,67.6056788130504,
82.2499055715368));
#219726=CARTESIAN_POINT('Ctrl Pts',(-23.8397098155045,68.2971284007469,
82.7532298693984));
#219727=CARTESIAN_POINT('Ctrl Pts',(-23.8481703871645,68.5779558868143,
82.9399204995111));
#219728=CARTESIAN_POINT('Ctrl Pts',(-23.871197050066,69.3780515501284,83.4243581701984));
#219729=CARTESIAN_POINT('Ctrl Pts',(-23.885277863819,69.9132899593637,83.6958827846302));
#219730=CARTESIAN_POINT('Ctrl Pts',(-23.9073163037073,70.7736847555396,
84.053440516099));
#219731=CARTESIAN_POINT('Ctrl Pts',(-23.9152294424713,71.0868725140369,
84.168361390285));
#219732=CARTESIAN_POINT('Ctrl Pts',(-23.9341886438321,71.8321747515983,
84.4061841008895));
#219733=CARTESIAN_POINT('Ctrl Pts',(-23.9454211520969,72.2665804198338,
84.517476771334));
#219734=CARTESIAN_POINT('Ctrl Pts',(-23.9652782132134,73.0404647072046,
84.66967294));
#219735=CARTESIAN_POINT('Ctrl Pts',(-23.9738842404024,73.3782672473474,
84.7210490326943));
#219736=CARTESIAN_POINT('Ctrl Pts',(-23.9968051979931,74.3002900610801,
84.8210702035737));
#219737=CARTESIAN_POINT('Ctrl Pts',(-24.0107033113074,74.8876684986167,
84.8413692782648));
#219738=CARTESIAN_POINT('Ctrl Pts',(-24.0340122827481,75.8702392977051,
84.8028056628792));
#219739=CARTESIAN_POINT('Ctrl Pts',(-24.043432404758,76.2664083199661,84.7673381145656));
#219740=CARTESIAN_POINT('Ctrl Pts',(-24.0646309551325,77.1334984705464,
84.6450363719972));
#219741=CARTESIAN_POINT('Ctrl Pts',(-24.0765713079441,77.6009858284274,
84.5493528448032));
#219742=CARTESIAN_POINT('Ctrl Pts',(-24.0997554081107,78.4910206834455,
84.3103135667122));
#219743=CARTESIAN_POINT('Ctrl Pts',(-24.1108807937146,78.9141664301559,
84.1706526422075));
#219744=CARTESIAN_POINT('Ctrl Pts',(-24.1385332276154,79.9731164787605,
83.7543074460724));
#219745=CARTESIAN_POINT('Ctrl Pts',(-24.1548409783277,80.5960774404369,
83.4445873668435));
#219746=CARTESIAN_POINT('Ctrl Pts',(-24.1798141076855,81.4855472211131,
82.9004178078973));
#219747=CARTESIAN_POINT('Ctrl Pts',(-24.1882658800546,81.7757939264851,
82.7046570188048));
#219748=CARTESIAN_POINT('Ctrl Pts',(-24.2064651621941,82.3680756726774,
82.2650889548938));
#219749=CARTESIAN_POINT('Ctrl Pts',(-24.2162594926789,82.6677628545046,
82.0184893106646));
#219750=CARTESIAN_POINT('Ctrl Pts',(-24.2503354667517,83.6759547075801,
81.1023758653179));
#219751=CARTESIAN_POINT('Ctrl Pts',(-24.2734890978271,84.3165658354487,
80.3575421127005));
#219752=CARTESIAN_POINT('Ctrl Pts',(-24.3359484975005,85.7610812345458,
78.1900043195256));
#219753=CARTESIAN_POINT('Ctrl Pts',(-24.3698713517959,86.2160492920742,
76.9116039690565));
#219754=CARTESIAN_POINT('Ctrl Pts',(-24.4133074766063,86.6618899759425,
75.1700668662206));
#219755=CARTESIAN_POINT('Ctrl Pts',(-24.4319587440237,86.7814690924183,
74.3940693434564));
#219756=CARTESIAN_POINT('Ctrl Pts',(-24.4613547807652,86.8459689720956,
73.1896082034861));
#219757=CARTESIAN_POINT('Ctrl Pts',(-24.4718526033559,86.8455610485519,
72.7660588280728));
#219758=CARTESIAN_POINT('Ctrl Pts',(-24.5046971488066,86.7721213111656,
71.4411529564219));
#219759=CARTESIAN_POINT('Ctrl Pts',(-24.5265462495201,86.6185082957646,
70.5461094578341));
#219760=CARTESIAN_POINT('Ctrl Pts',(-24.5670051429742,86.1518862619208,
68.9404605247924));
#219761=CARTESIAN_POINT('Ctrl Pts',(-24.5856817309166,85.8651065517316,
68.2206283273154));
#219762=CARTESIAN_POINT('Ctrl Pts',(-24.6232006790467,85.1612979160907,
66.8653478737751));
#219763=CARTESIAN_POINT('Ctrl Pts',(-24.6416611232624,84.7487848589079,
66.2297978498545));
#219764=CARTESIAN_POINT('Ctrl Pts',(-24.6882468904586,83.5623680174767,
64.7326308652746));
#219765=CARTESIAN_POINT('Ctrl Pts',(-24.7260382386136,82.4438732841827,
63.5847792685476));
#219766=CARTESIAN_POINT('Ctrl Pts',(-24.7917113773775,80.1048899714854,
62.2801640674017));
#219767=CARTESIAN_POINT('Ctrl Pts',(-24.8105835909982,79.3983530500854,
61.9711661347939));
#219768=CARTESIAN_POINT('Ctrl Pts',(-24.8476505405666,77.9512541423471,
61.4982879163466));
#219769=CARTESIAN_POINT('Ctrl Pts',(-24.8656179042796,77.2118140491652,
61.332268975595));
#219770=CARTESIAN_POINT('Ctrl Pts',(-24.9052918234955,75.5975429275466,
61.1330685277027));
#219771=CARTESIAN_POINT('Ctrl Pts',(-24.9268693700258,74.7252280093247,
61.1221140290984));
#219772=CARTESIAN_POINT('Ctrl Pts',(-24.9577085382453,73.4737815980774,
61.242481028318));
#219773=CARTESIAN_POINT('Ctrl Pts',(-24.967217719536,73.0871932428302,61.2988750337921));
#219774=CARTESIAN_POINT('Ctrl Pts',(-24.9905520650349,72.1351244908571,
61.4862146028957));
#219775=CARTESIAN_POINT('Ctrl Pts',(-25.0042103174994,71.5757510543634,
61.6397751316705));
#219776=CARTESIAN_POINT('Ctrl Pts',(-25.0335288217218,70.4461743726575,
62.0429563473559));
#219777=CARTESIAN_POINT('Ctrl Pts',(-25.0489253600611,69.8810709729959,
62.2963153262076));
#219778=CARTESIAN_POINT('Ctrl Pts',(-25.0800666050386,68.7772565000667,
62.8976245619141));
#219779=CARTESIAN_POINT('Ctrl Pts',(-25.0957726872494,68.2400647626968,
63.2487373898093));
#219780=CARTESIAN_POINT('Ctrl Pts',(-25.1193718523531,67.4564988289902,
63.8566578125516));
#219781=CARTESIAN_POINT('Ctrl Pts',(-25.1276624343069,67.1879359315394,
64.0849197521976));
#219782=CARTESIAN_POINT('Ctrl Pts',(-25.1454609563539,66.6454867103185,
64.5900982371163));
#219783=CARTESIAN_POINT('Ctrl Pts',(-25.1550148296095,66.3742407038714,
64.8694283428638));
#219784=CARTESIAN_POINT('Ctrl Pts',(-25.1821367707909,65.651765776175,65.6906711367853));
#219785=CARTESIAN_POINT('Ctrl Pts',(-25.1999107406031,65.233294526125,66.261769242973));
#219786=CARTESIAN_POINT('Ctrl Pts',(-25.2283952223487,64.630334717106,67.2584876519789));
#219787=CARTESIAN_POINT('Ctrl Pts',(-25.2393089263833,64.4150568461714,
67.6656532103755));
#219788=CARTESIAN_POINT('Ctrl Pts',(-25.261057263207,64.0330799276992,68.5030414663998));
#219789=CARTESIAN_POINT('Ctrl Pts',(-25.2719955468723,63.8668808019813,
68.9323993214274));
#219790=CARTESIAN_POINT('Ctrl Pts',(-25.2937880673866,63.5965624296136,
69.7767493402305));
#219791=CARTESIAN_POINT('Ctrl Pts',(-25.3044379286782,63.4890325077483,
70.1883156831887));
#219792=CARTESIAN_POINT('Ctrl Pts',(-25.3293736091068,63.2891448861663,
71.1638320986694));
#219793=CARTESIAN_POINT('Ctrl Pts',(-25.3436387852029,63.2147405508323,
71.7315450266966));
#219794=CARTESIAN_POINT('Ctrl Pts',(-25.3658368888776,63.1605775869907,
72.6541834421041));
#219795=CARTESIAN_POINT('Ctrl Pts',(-25.3741450297437,63.1555385000925,
73.007689085589));
#219796=CARTESIAN_POINT('Ctrl Pts',(-25.3932547504681,63.1802915989499,
73.8167754615166));
#219797=CARTESIAN_POINT('Ctrl Pts',(-25.4041146979201,63.2206674555497,
74.2716084565794));
#219798=CARTESIAN_POINT('Ctrl Pts',(-25.424894620039,63.3446571966042,75.1053687246365));
#219799=CARTESIAN_POINT('Ctrl Pts',(-25.4345780693059,63.4200964155568,
75.4834915305247));
#219800=CARTESIAN_POINT('Ctrl Pts',(-25.4567619973944,63.6347127373887,
76.3401422706014));
#219801=CARTESIAN_POINT('Ctrl Pts',(-25.4692500578771,63.7861020015207,
76.8156577037989));
#219802=CARTESIAN_POINT('Ctrl Pts',(-25.4890094659493,64.0819679904328,
77.5769828960174));
#219803=CARTESIAN_POINT('Ctrl Pts',(-25.4965644957773,64.2093291045492,
77.8694937917293));
#219804=CARTESIAN_POINT('Ctrl Pts',(-25.5177272011169,64.5997762794745,
78.6759683205503));
#219805=CARTESIAN_POINT('Ctrl Pts',(-25.5313223378866,64.8895155036546,
79.1778737046292));
#219806=CARTESIAN_POINT('Ctrl Pts',(-25.553961967557,65.4070878364213,79.93673654872));
#219807=CARTESIAN_POINT('Ctrl Pts',(-25.562477621451,65.6101301943096,80.2082748200485));
#219808=CARTESIAN_POINT('Ctrl Pts',(-25.5838503196473,66.1473713131949,
80.8660090615544));
#219809=CARTESIAN_POINT('Ctrl Pts',(-25.596696390321,66.4958853551464,81.2405495881967));
#219810=CARTESIAN_POINT('Ctrl Pts',(-25.6174987374245,67.1198671630634,
81.8305356652852));
#219811=CARTESIAN_POINT('Ctrl Pts',(-25.6257626286478,67.3833471538268,
82.0587208875555));
#219812=CARTESIAN_POINT('Ctrl Pts',(-25.6481489502373,68.1250610693869,
82.6461857161893));
#219813=CARTESIAN_POINT('Ctrl Pts',(-25.6622524342847,68.6223957292458,
82.9825882016476));
#219814=CARTESIAN_POINT('Ctrl Pts',(-25.6849535707228,69.4223463877076,
83.4376350608614));
#219815=CARTESIAN_POINT('Ctrl Pts',(-25.6930171765534,69.7074615873909,
83.5846073202147));
#219816=CARTESIAN_POINT('Ctrl Pts',(-25.7146507220582,70.4865706602702,
83.946966015049));
#219817=CARTESIAN_POINT('Ctrl Pts',(-25.7281391359254,70.9906139565075,
84.1408019798077));
#219818=CARTESIAN_POINT('Ctrl Pts',(-25.7520876074811,71.938816783935,84.4337245706673));
#219819=CARTESIAN_POINT('Ctrl Pts',(-25.762810865982,72.3799073071065,84.5429585790459));
#219820=CARTESIAN_POINT('Ctrl Pts',(-25.7851622316922,73.3050912650405,
84.7165901495142));
#219821=CARTESIAN_POINT('Ctrl Pts',(-25.7968063426039,73.7901466473484,
84.7770486933696));
#219822=CARTESIAN_POINT('Ctrl Pts',(-25.8166416512065,74.5925067179341,
84.8260692378714));
#219823=CARTESIAN_POINT('Ctrl Pts',(-25.8245878850798,74.9084143096501,
84.8324891107669));
#219824=CARTESIAN_POINT('Ctrl Pts',(-25.846126398411,75.7648310579256,84.8155658720624));
#219825=CARTESIAN_POINT('Ctrl Pts',(-25.8595502609576,76.3048734411851,
84.7677371052777));
#219826=CARTESIAN_POINT('Ctrl Pts',(-25.8870929365118,77.4331091242953,
84.5901671073612));
#219827=CARTESIAN_POINT('Ctrl Pts',(-25.9012958491276,78.0200692131477,
84.4518600552283));
#219828=CARTESIAN_POINT('Ctrl Pts',(-25.9262597884438,79.0123812129266,
84.1367233640231));
#219829=CARTESIAN_POINT('Ctrl Pts',(-25.9369484716107,79.4245662099935,
83.9800739201575));
#219830=CARTESIAN_POINT('Ctrl Pts',(-25.9593084055024,80.2444445516244,
83.6136503722892));
#219831=CARTESIAN_POINT('Ctrl Pts',(-25.970864562363,80.6503056040749,83.4029204272697));
#219832=CARTESIAN_POINT('Ctrl Pts',(-25.9938343662642,81.4514752177107,
82.9265531223943));
#219833=CARTESIAN_POINT('Ctrl Pts',(-26.005310034174,81.8456631486792,82.6589885236724));
#219834=CARTESIAN_POINT('Ctrl Pts',(-26.0343820127005,82.8058647548344,
81.9199778941042));
#219835=CARTESIAN_POINT('Ctrl Pts',(-26.0518964723227,83.3478025042898,
81.4170463577296));
#219836=CARTESIAN_POINT('Ctrl Pts',(-26.0820442935122,84.165826779719,80.5001478590155));
#219837=CARTESIAN_POINT('Ctrl Pts',(-26.0944271911139,84.469305924103,80.112925251043));
#219838=CARTESIAN_POINT('Ctrl Pts',(-26.1225191227799,85.1145478269457,
79.1752815467396));
#219839=CARTESIAN_POINT('Ctrl Pts',(-26.1381663634797,85.4379364210402,
78.6116580075921));
#219840=CARTESIAN_POINT('Ctrl Pts',(-26.1721088657875,86.0376628276095,
77.3370325344322));
#219841=CARTESIAN_POINT('Ctrl Pts',(-26.1904008122117,86.2958999687812,
76.6173315306904));
#219842=CARTESIAN_POINT('Ctrl Pts',(-26.2163069038108,86.5528168983806,
75.5971963120996));
#219843=CARTESIAN_POINT('Ctrl Pts',(-26.2235318340171,86.613186429361,75.3127304874102));
#219844=CARTESIAN_POINT('Ctrl Pts',(-26.2587554148366,86.8580316646618,
73.9047778024851));
#219845=CARTESIAN_POINT('Ctrl Pts',(-26.286223815663,86.890533153244,72.75432961077));
#219846=CARTESIAN_POINT('Ctrl Pts',(-26.3415801754294,86.6292934641588,
70.4878602924608));
#219847=CARTESIAN_POINT('Ctrl Pts',(-26.3693494802877,86.3347180294922,
69.3856928759218));
#219848=CARTESIAN_POINT('Ctrl Pts',(-26.3971183084764,85.8880607550622,
68.3407934129425));
#219849=CARTESIAN_POINT('Ctrl Pts',(-31.6489087198709,70.0959712176063,
60.8783100640841));
#219850=CARTESIAN_POINT('Ctrl Pts',(-31.6814645153009,68.7303325189268,
61.4313085050616));
#219851=CARTESIAN_POINT('Ctrl Pts',(-31.7465761061609,66.1882700076009,
63.0035716608669));
#219852=CARTESIAN_POINT('Ctrl Pts',(-31.8442434924509,63.3737498322777,
66.4939579958501));
#219853=CARTESIAN_POINT('Ctrl Pts',(-31.9419108787409,61.8771905500222,
70.7205438274275));
#219854=CARTESIAN_POINT('Ctrl Pts',(-32.0395782650309,61.8681403166308,
75.2042647157331));
#219855=CARTESIAN_POINT('Ctrl Pts',(-32.1372456513209,63.3476500679026,
79.4368608152641));
#219856=CARTESIAN_POINT('Ctrl Pts',(-32.2349130376109,66.1480040818002,
82.9385512545613));
#219857=CARTESIAN_POINT('Ctrl Pts',(-32.3325804239009,69.9517715767027,
85.3124031224554));
#219858=CARTESIAN_POINT('Ctrl Pts',(-32.4302478101809,74.3277781103001,
86.2893299487034));
#219859=CARTESIAN_POINT('Ctrl Pts',(-32.5279151964709,78.7799840116568,
85.7585926810094));
#219860=CARTESIAN_POINT('Ctrl Pts',(-32.6255825827609,82.8037119089286,
83.7803527627689));
#219861=CARTESIAN_POINT('Ctrl Pts',(-32.7232499690509,85.9428543612762,
80.5788524819328));
#219862=CARTESIAN_POINT('Ctrl Pts',(-32.8209173553409,87.8415756099131,
76.5169961329518));
#219863=CARTESIAN_POINT('Ctrl Pts',(-32.9185847416309,88.2846471586345,
72.0552131952207));
#219864=CARTESIAN_POINT('Ctrl Pts',(-33.0162521279209,87.2218448769265,
67.6992666057196));
#219865=CARTESIAN_POINT('Ctrl Pts',(-33.1139195142109,84.7736421296089,
63.9429222806305));
#219866=CARTESIAN_POINT('Ctrl Pts',(-33.2115869005009,81.2175535848858,
61.2119785531442));
#219867=CARTESIAN_POINT('Ctrl Pts',(-33.3092542867909,76.9566776927288,
59.8160000388975));
#219868=CARTESIAN_POINT('Ctrl Pts',(-33.4069216730809,72.4740036830308,
59.9132271101949));
#219869=CARTESIAN_POINT('Ctrl Pts',(-33.5045890593709,68.2776625886137,
61.4926386461447));
#219870=CARTESIAN_POINT('Ctrl Pts',(-33.6022564456609,64.8433283330666,
64.3752013257362));
#219871=CARTESIAN_POINT('Ctrl Pts',(-33.6999238319509,62.56029797625,68.2341638508804));
#219872=CARTESIAN_POINT('Ctrl Pts',(-33.7975912182409,61.6873631614363,
72.6320956590941));
#219873=CARTESIAN_POINT('Ctrl Pts',(-33.8952586045309,62.3234749316971,
77.0704716229308));
#219874=CARTESIAN_POINT('Ctrl Pts',(-33.9929259908209,64.3965271891681,
81.0461820900504));
#219875=CARTESIAN_POINT('Ctrl Pts',(-34.0905933771109,67.6715302419011,
84.1085625995897));
#219876=CARTESIAN_POINT('Ctrl Pts',(-34.1882607634009,71.7772479303871,
85.9104787028145));
#219877=CARTESIAN_POINT('Ctrl Pts',(-34.2859281496909,76.2482788970921,
86.247675196548));
#219878=CARTESIAN_POINT('Ctrl Pts',(-34.3835955359809,80.5778118998904,
85.081929358769));
#219879=CARTESIAN_POINT('Ctrl Pts',(-34.4812629222709,84.2750751200944,
82.5453836640971));
#219880=CARTESIAN_POINT('Ctrl Pts',(-34.5789303085609,86.9209673304724,
78.9255668466804));
#219881=CARTESIAN_POINT('Ctrl Pts',(-34.6765976948509,88.2155648830812,
74.6328012395938));
#219882=CARTESIAN_POINT('Ctrl Pts',(-34.7742650811409,88.0121193884434,
70.1536909137269));
#219883=CARTESIAN_POINT('Ctrl Pts',(-34.8719324674309,86.333692298055,65.995962942479));
#219884=CARTESIAN_POINT('Ctrl Pts',(-34.9695998537209,83.3705407863494,
62.6309142802354));
#219885=CARTESIAN_POINT('Ctrl Pts',(-35.0672672400109,79.4585512538933,
60.4399881567567));
#219886=CARTESIAN_POINT('Ctrl Pts',(-35.1649346263009,75.0411651102624,
59.6715357908677));
#219887=CARTESIAN_POINT('Ctrl Pts',(-35.2626020125909,70.6191127183272,
60.4126646754531));
#219888=CARTESIAN_POINT('Ctrl Pts',(-35.3602693988809,66.6936533809556,
62.5793645557409));
#219889=CARTESIAN_POINT('Ctrl Pts',(-35.4579367851709,63.7097553700125,
65.9260303652965));
#219890=CARTESIAN_POINT('Ctrl Pts',(-35.5556041714609,62.005656794,70.0733026524509));
#219891=CARTESIAN_POINT('Ctrl Pts',(-35.6532715577509,61.7745248044076,
74.5510696611246));
#219892=CARTESIAN_POINT('Ctrl Pts',(-35.7509389440409,63.0425592400513,
78.8517565888796));
#219893=CARTESIAN_POINT('Ctrl Pts',(-35.8486063303309,65.6660227588901,
82.4878614479098));
#219894=CARTESIAN_POINT('Ctrl Pts',(-35.9462737166209,69.3475341048888,
85.0472155832));
#219895=CARTESIAN_POINT('Ctrl Pts',(-36.0439411029109,73.6697775958153,
86.239704822428));
#219896=CARTESIAN_POINT('Ctrl Pts',(-36.1416084892009,78.142807711568,85.9301552074927));
#219897=CARTESIAN_POINT('Ctrl Pts',(-36.2392758754909,82.2595865975891,
84.1536555637811));
#219898=CARTESIAN_POINT('Ctrl Pts',(-36.3369432617809,85.5534590604176,
81.111580025743));
#219899=CARTESIAN_POINT('Ctrl Pts',(-36.4346106480709,87.6510500090054,
77.1487613832987));
#219900=CARTESIAN_POINT('Ctrl Pts',(-36.5322780343609,88.3145881816426,
72.7144027516668));
#219901=CARTESIAN_POINT('Ctrl Pts',(-36.6299454206509,87.4688585758041,
68.3111584007035));
#219902=CARTESIAN_POINT('Ctrl Pts',(-36.7276128069509,85.2097284031102,
64.4381556582015));
#219903=CARTESIAN_POINT('Ctrl Pts',(-36.8252801932409,81.793280114859,61.534416607706));
#219904=CARTESIAN_POINT('Ctrl Pts',(-36.9229475795309,77.6067833162661,
59.9290929831489));
#219905=CARTESIAN_POINT('Ctrl Pts',(-37.0206149658209,73.124796038894,59.8041553558838));
#219906=CARTESIAN_POINT('Ctrl Pts',(-37.1182823521109,68.8553714613998,
61.1737659619935));
#219907=CARTESIAN_POINT('Ctrl Pts',(-37.2159497384009,65.2824678824627,
63.8826733471558));
#219908=CARTESIAN_POINT('Ctrl Pts',(-37.3136171246909,62.8110896717617,
67.6238108193035));
#219909=CARTESIAN_POINT('Ctrl Pts',(-37.4112845109809,61.7213790587936,
71.9731037866268));
#219910=CARTESIAN_POINT('Ctrl Pts',(-37.5089518972709,62.1368576487401,
76.4375406365595));
#219911=CARTESIAN_POINT('Ctrl Pts',(-37.6066192835609,64.010436330763,80.5110572786137));
#219912=CARTESIAN_POINT('Ctrl Pts',(-37.7042866698509,67.1297096286665,
83.7319036844192));
#219913=CARTESIAN_POINT('Ctrl Pts',(-37.8019540561409,71.1411948124404,
85.7349781226078));
#219914=CARTESIAN_POINT('Ctrl Pts',(-37.8670656470009,74.1069290187816,
86.1071526244663));
#219915=CARTESIAN_POINT('Ctrl Pts',(-37.8996214424309,75.5788379419391,
86.0418804791266));
#219916=CARTESIAN_POINT('Ctrl Pts',(-31.8730368301509,70.2575692325718,
61.2773790062616));
#219917=CARTESIAN_POINT('Ctrl Pts',(-31.9055926255809,68.9369311879788,
61.8121549909076));
#219918=CARTESIAN_POINT('Ctrl Pts',(-31.9707042164409,66.4786349582126,
63.3326087841967));
#219919=CARTESIAN_POINT('Ctrl Pts',(-32.0683716027309,63.7568591148654,
66.7079795823175));
#219920=CARTESIAN_POINT('Ctrl Pts',(-32.1660389890109,62.3096145940082,
70.7952905623853));
#219921=CARTESIAN_POINT('Ctrl Pts',(-32.2637063753009,62.3008625847488,
75.1312634607482));
#219922=CARTESIAN_POINT('Ctrl Pts',(-32.3613737615909,63.7316193923605,
79.224386657865));
#219923=CARTESIAN_POINT('Ctrl Pts',(-32.4590411478809,66.4396958789624,
82.610689066389));
#219924=CARTESIAN_POINT('Ctrl Pts',(-32.5567085341709,70.1181212717175,
84.9063175455788));
#219925=CARTESIAN_POINT('Ctrl Pts',(-32.6543759204609,74.3499292288595,
85.8510525877097));
#219926=CARTESIAN_POINT('Ctrl Pts',(-32.7520433067509,78.6554256250739,
85.3378042240803));
#219927=CARTESIAN_POINT('Ctrl Pts',(-32.8497106930409,82.5465632644516,
83.4247514525909));
#219928=CARTESIAN_POINT('Ctrl Pts',(-32.9473780793309,85.5822644011988,
80.32874730835));
#219929=CARTESIAN_POINT('Ctrl Pts',(-33.0450454656209,87.4184188097211,
76.4007376295671));
#219930=CARTESIAN_POINT('Ctrl Pts',(-33.1427128519109,87.8468902233397,
72.0859797803774));
#219931=CARTESIAN_POINT('Ctrl Pts',(-33.2403802382009,86.8191095017967,
67.8735707501784));
#219932=CARTESIAN_POINT('Ctrl Pts',(-33.3380476244909,84.4515801603142,
64.2410058345146));
#219933=CARTESIAN_POINT('Ctrl Pts',(-33.4357150107809,81.0126721778146,
61.6000524200778));
#219934=CARTESIAN_POINT('Ctrl Pts',(-33.5333823970709,76.8922010664508,
60.250074320352));
#219935=CARTESIAN_POINT('Ctrl Pts',(-33.6310497833609,72.5572405498546,
60.3440975560973));
#219936=CARTESIAN_POINT('Ctrl Pts',(-33.7287171696509,68.4991776795392,
61.8714641754451));
#219937=CARTESIAN_POINT('Ctrl Pts',(-33.8263845559409,65.1780119274846,
64.6590403800947));
#219938=CARTESIAN_POINT('Ctrl Pts',(-33.9240519422309,62.9702122004541,
68.390842011297));
#219939=CARTESIAN_POINT('Ctrl Pts',(-34.0217193285209,62.1260424152783,
72.6438527593594));
#219940=CARTESIAN_POINT('Ctrl Pts',(-34.1193867148109,62.7411929710006,
76.9359749434432));
#219941=CARTESIAN_POINT('Ctrl Pts',(-34.2170541010909,64.7459338166531,
80.780677427527));
#219942=CARTESIAN_POINT('Ctrl Pts',(-34.3147214873809,67.9130186625803,
83.7421460881763));
#219943=CARTESIAN_POINT('Ctrl Pts',(-34.4123888736709,71.8834443579084,
85.484685283491));
#219944=CARTESIAN_POINT('Ctrl Pts',(-34.5100562599609,76.2071454941548,
85.8107704468362));
#219945=CARTESIAN_POINT('Ctrl Pts',(-34.6077236462509,80.3940113206321,
84.6834383749048));
#219946=CARTESIAN_POINT('Ctrl Pts',(-34.7053910325409,83.9694419775097,
82.2304771711338));
#219947=CARTESIAN_POINT('Ctrl Pts',(-34.8030584188309,86.5281465003784,
78.729940895939));
#219948=CARTESIAN_POINT('Ctrl Pts',(-34.9007258051209,87.7800843533953,
74.5786309025152));
#219949=CARTESIAN_POINT('Ctrl Pts',(-34.9983931914109,87.5833428137125,
70.2471166389011));
#219950=CARTESIAN_POINT('Ctrl Pts',(-35.0960605777009,85.9602234097461,
66.2263945085208));
#219951=CARTESIAN_POINT('Ctrl Pts',(-35.1937279639909,83.0947139437118,
62.9722312444263));
#219952=CARTESIAN_POINT('Ctrl Pts',(-35.2913953502809,79.3116326561084,
60.8535007234067));
#219953=CARTESIAN_POINT('Ctrl Pts',(-35.3890627365809,75.0398086337074,
60.1103704717333));
#219954=CARTESIAN_POINT('Ctrl Pts',(-35.4867301228709,70.7634721256552,
60.8270776080123));
#219955=CARTESIAN_POINT('Ctrl Pts',(-35.5843975091609,66.967364891402,62.9223801912565));
#219956=CARTESIAN_POINT('Ctrl Pts',(-35.6820648954509,64.0817925667024,
66.1587663561376));
#219957=CARTESIAN_POINT('Ctrl Pts',(-35.7797322817409,62.433847606303,70.1693773391154));
#219958=CARTESIAN_POINT('Ctrl Pts',(-35.8773996680309,62.2103318996323,
74.4995925506424));
#219959=CARTESIAN_POINT('Ctrl Pts',(-35.9750670543209,63.4365819459936,
78.6585628406411));
#219960=CARTESIAN_POINT('Ctrl Pts',(-36.0727344406109,65.9735968496646,
82.1748504323778));
#219961=CARTESIAN_POINT('Ctrl Pts',(-36.1704018269009,69.5337946895659,
84.6498684909033));
#219962=CARTESIAN_POINT('Ctrl Pts',(-36.2680692131909,73.7136112088471,
85.8030627132265));
#219963=CARTESIAN_POINT('Ctrl Pts',(-36.3657365994809,78.0392456179921,
85.5037134061586));
#219964=CARTESIAN_POINT('Ctrl Pts',(-36.4634039857709,82.0203680212412,
83.7857531448031));
#219965=CARTESIAN_POINT('Ctrl Pts',(-36.5610713720609,85.2057004907068,
80.8439203643352));
#219966=CARTESIAN_POINT('Ctrl Pts',(-36.6587387583509,87.2341714262334,
77.0116848923229));
#219967=CARTESIAN_POINT('Ctrl Pts',(-36.7564061446409,87.8758446269618,
72.7234476609321));
#219968=CARTESIAN_POINT('Ctrl Pts',(-36.8540735309309,87.0579835821749,
68.4652994295259));
#219969=CARTESIAN_POINT('Ctrl Pts',(-36.9517409172209,84.873296478161,64.7199202355244));
#219970=CARTESIAN_POINT('Ctrl Pts',(-37.0494083035109,81.5694273133449,
61.9118654657189));
#219971=CARTESIAN_POINT('Ctrl Pts',(-37.1470756898009,77.520884348699,60.3594406153311));
#219972=CARTESIAN_POINT('Ctrl Pts',(-37.2447430760909,73.1865879351576,
60.238619944442));
#219973=CARTESIAN_POINT('Ctrl Pts',(-37.3424104623809,69.0578498355331,
61.5630990137956));
#219974=CARTESIAN_POINT('Ctrl Pts',(-37.4400778486709,65.602680909391,64.1827422295159));
#219975=CARTESIAN_POINT('Ctrl Pts',(-37.5377452349609,63.2127397845698,
67.8006013898867));
#219976=CARTESIAN_POINT('Ctrl Pts',(-37.6354126212509,62.1589374176099,
72.0065760486925));
#219977=CARTESIAN_POINT('Ctrl Pts',(-37.7330800075509,62.5607251182124,
76.3239003581206));
#219978=CARTESIAN_POINT('Ctrl Pts',(-37.8307473938409,64.3725654603181,
80.2631860989099));
#219979=CARTESIAN_POINT('Ctrl Pts',(-37.9284147801309,67.3890521728565,
83.3778988728009));
#219980=CARTESIAN_POINT('Ctrl Pts',(-38.0260821664209,71.2683505217792,
85.3149678148183));
#219981=CARTESIAN_POINT('Ctrl Pts',(-38.0911937572809,74.1363575772585,
85.6748783876892));
#219982=CARTESIAN_POINT('Ctrl Pts',(-38.1237495527109,75.5597640199593,
85.6117570961773));
#219983=CARTESIAN_POINT('Ctrl Pts',(-32.0971649404209,70.4191672475379,
61.6764479484404));
#219984=CARTESIAN_POINT('Ctrl Pts',(-32.1297207358509,69.1435298570313,
62.1930014767527));
#219985=CARTESIAN_POINT('Ctrl Pts',(-32.1948323267109,66.7689999088247,
63.6616459075254));
#219986=CARTESIAN_POINT('Ctrl Pts',(-32.2924997130009,64.1399683974443,
66.9220011687802));
#219987=CARTESIAN_POINT('Ctrl Pts',(-32.3901670992909,62.7420386379846,
70.8700372973402));
#219988=CARTESIAN_POINT('Ctrl Pts',(-32.4878344855809,62.7335848528663,
75.0582622057643));
#219989=CARTESIAN_POINT('Ctrl Pts',(-32.5855018718709,64.1155887168238,
79.0119125004583));
#219990=CARTESIAN_POINT('Ctrl Pts',(-32.6831692581609,66.7313876761263,
82.2828268782175));
#219991=CARTESIAN_POINT('Ctrl Pts',(-32.7808366444509,70.2844709667367,
84.500231968704));
#219992=CARTESIAN_POINT('Ctrl Pts',(-32.8785040307409,74.3720803474283,
85.4127752267091));
#219993=CARTESIAN_POINT('Ctrl Pts',(-32.9761714170309,78.5308672385013,
84.9170157671447));
#219994=CARTESIAN_POINT('Ctrl Pts',(-33.0738388033209,82.2894146199872,
83.0691501424084));
#219995=CARTESIAN_POINT('Ctrl Pts',(-33.1715061896109,85.2216744411351,
80.0786421347599));
#219996=CARTESIAN_POINT('Ctrl Pts',(-33.2691735759009,86.9952620095349,
76.2844791261685));
#219997=CARTESIAN_POINT('Ctrl Pts',(-33.3668409621909,87.4091332880509,
72.1167463655193));
#219998=CARTESIAN_POINT('Ctrl Pts',(-33.4645083484809,86.4163741266587,
68.0478748946176));
#219999=CARTESIAN_POINT('Ctrl Pts',(-33.5621757347709,84.1295181910076,
64.5390893883722));
#220000=CARTESIAN_POINT('Ctrl Pts',(-33.6598431210609,80.8077907707222,
61.9881262869919));
#220001=CARTESIAN_POINT('Ctrl Pts',(-33.7575105073509,76.8277244401432,
60.684148601805));
#220002=CARTESIAN_POINT('Ctrl Pts',(-33.8551778936409,72.6404774166431,
60.7749680020176));
#220003=CARTESIAN_POINT('Ctrl Pts',(-33.9528452799309,68.7206927704309,
62.2502897047617));
#220004=CARTESIAN_POINT('Ctrl Pts',(-34.0505126662209,65.5126955218893,
64.9428794344855));
#220005=CARTESIAN_POINT('Ctrl Pts',(-34.1481800525109,63.3801264246425,
68.5475201717517));
#220006=CARTESIAN_POINT('Ctrl Pts',(-34.2458474388009,62.5647216691142,
72.6556098596656));
#220007=CARTESIAN_POINT('Ctrl Pts',(-34.3435148250909,63.1589110103241,
76.8014782640017));
#220008=CARTESIAN_POINT('Ctrl Pts',(-34.4411822113809,65.0953404441711,
80.5151727650388));
#220009=CARTESIAN_POINT('Ctrl Pts',(-34.5388495976709,68.1545070833008,
83.3757295768015));
#220010=CARTESIAN_POINT('Ctrl Pts',(-34.6365169839609,71.9896407854853,
85.0588918641796));
#220011=CARTESIAN_POINT('Ctrl Pts',(-34.7341843702509,76.1660120912788,
85.3738656971174));
#220012=CARTESIAN_POINT('Ctrl Pts',(-34.8318517565409,80.2102107414312,
84.2849473910145));
#220013=CARTESIAN_POINT('Ctrl Pts',(-34.9295191428309,83.6638088349665,
81.9155706781228));
#220014=CARTESIAN_POINT('Ctrl Pts',(-35.0271865291209,86.1353256703195,
78.5343149451388));
#220015=CARTESIAN_POINT('Ctrl Pts',(-35.1248539154109,87.3446038237169,
74.5244605653662));
#220016=CARTESIAN_POINT('Ctrl Pts',(-35.2225213017009,87.1545662389771,
70.3405423640075));
#220017=CARTESIAN_POINT('Ctrl Pts',(-35.3201886879909,85.5867545214038,
66.4568260744839));
#220018=CARTESIAN_POINT('Ctrl Pts',(-35.4178560742809,82.818887101022,63.3135482085524));
#220019=CARTESIAN_POINT('Ctrl Pts',(-35.5155234605709,79.1647140582467,
61.2670132900358));
#220020=CARTESIAN_POINT('Ctrl Pts',(-35.6131908468609,75.0384521570716,
60.5492051525981));
#220021=CARTESIAN_POINT('Ctrl Pts',(-35.7108582331509,70.9078315329049,
61.2414905405987));
#220022=CARTESIAN_POINT('Ctrl Pts',(-35.8085256194409,67.2410764017834,
63.2653958268243));
#220023=CARTESIAN_POINT('Ctrl Pts',(-35.9061930057309,64.4538297633518,
66.3915023470505));
#220024=CARTESIAN_POINT('Ctrl Pts',(-36.0038603920209,62.8620384185835,
70.2654520258604));
#220025=CARTESIAN_POINT('Ctrl Pts',(-36.1015277783109,62.6461389948745,
74.4481154402485));
#220026=CARTESIAN_POINT('Ctrl Pts',(-36.1991951646009,63.8306046519742,
78.4653690924802));
#220027=CARTESIAN_POINT('Ctrl Pts',(-36.2968625508909,66.2811709404978,
81.8618394169132));
#220028=CARTESIAN_POINT('Ctrl Pts',(-36.3945299371809,69.7200552743181,
84.2525213986484));
#220029=CARTESIAN_POINT('Ctrl Pts',(-36.4921973234709,73.7574448219614,
85.3664206040375));
#220030=CARTESIAN_POINT('Ctrl Pts',(-36.5898647097609,77.935683524501,85.0772716047947));
#220031=CARTESIAN_POINT('Ctrl Pts',(-36.6875320960509,81.7811494449743,
83.4178507257861));
#220032=CARTESIAN_POINT('Ctrl Pts',(-36.7851994823409,84.8579419210346,
80.5762607028601));
#220033=CARTESIAN_POINT('Ctrl Pts',(-36.8828668686309,86.8172928434819,
76.8746084012713));
#220034=CARTESIAN_POINT('Ctrl Pts',(-36.9805342549209,87.4371010722797,
72.7324925701221));
#220035=CARTESIAN_POINT('Ctrl Pts',(-37.0782016412109,86.6471085885194,
68.6194404582812));
#220036=CARTESIAN_POINT('Ctrl Pts',(-37.1758690275009,84.5368645531706,
65.0016848127869));
#220037=CARTESIAN_POINT('Ctrl Pts',(-37.2735364137909,81.3455745117745,
62.2893143236978));
#220038=CARTESIAN_POINT('Ctrl Pts',(-37.3712038000809,77.4349853810736,
60.7897882475));
#220039=CARTESIAN_POINT('Ctrl Pts',(-37.4688711863709,73.2483798313682,
60.6730845330001));
#220040=CARTESIAN_POINT('Ctrl Pts',(-37.5665385726609,69.2603282096219,
61.9524320656215));
#220041=CARTESIAN_POINT('Ctrl Pts',(-37.6642059589509,65.9228939362941,
64.4828111119111));
#220042=CARTESIAN_POINT('Ctrl Pts',(-37.7618733452409,63.6143898973541,
67.9773919605015));
#220043=CARTESIAN_POINT('Ctrl Pts',(-37.8595407315309,62.5964957764151,
72.040048310785));
#220044=CARTESIAN_POINT('Ctrl Pts',(-37.9572081178209,62.9845925876825,
76.2102600797003));
#220045=CARTESIAN_POINT('Ctrl Pts',(-38.0548755041109,64.734694589886,80.0153149192114));
#220046=CARTESIAN_POINT('Ctrl Pts',(-38.1525428904009,67.648394717053,83.0238940611853));
#220047=CARTESIAN_POINT('Ctrl Pts',(-38.2502102766909,71.39550623112,84.8949575070187));
#220048=CARTESIAN_POINT('Ctrl Pts',(-38.3153218675509,74.1657861357241,
85.2426041509183));
#220049=CARTESIAN_POINT('Ctrl Pts',(-38.3478776629809,75.5406900979627,
85.1816337132427));
#220050=CARTESIAN_POINT('Ctrl Pts',(-32.3212930507009,70.5807652625035,
62.0755168906179));
#220051=CARTESIAN_POINT('Ctrl Pts',(-32.3538488461309,69.3501285260828,
62.5738479625974));
#220052=CARTESIAN_POINT('Ctrl Pts',(-32.4189604369909,67.0593648594363,
63.9906830308551));
#220053=CARTESIAN_POINT('Ctrl Pts',(-32.5166278232809,64.5230776800325,
67.1360227552467));
#220054=CARTESIAN_POINT('Ctrl Pts',(-32.6142952095709,63.1744626819709,
70.9447840322971));
#220055=CARTESIAN_POINT('Ctrl Pts',(-32.7119625958609,63.1663071209847,
74.9852609507785));
#220056=CARTESIAN_POINT('Ctrl Pts',(-32.8096299821509,64.4995580412843,
78.7994383430527));
#220057=CARTESIAN_POINT('Ctrl Pts',(-32.9072973684309,67.0230794732875,
81.9549646900448));
#220058=CARTESIAN_POINT('Ctrl Pts',(-33.0049647547209,70.4508206617514,
84.0941463918273));
#220059=CARTESIAN_POINT('Ctrl Pts',(-33.1026321410109,74.3942314659886,
84.9744978657157));
#220060=CARTESIAN_POINT('Ctrl Pts',(-33.2002995273009,78.4063088519184,
84.4962273102157));
#220061=CARTESIAN_POINT('Ctrl Pts',(-33.2979669135909,82.0322659755195,
82.7135488322343));
#220062=CARTESIAN_POINT('Ctrl Pts',(-33.3956342998809,84.8610844810572,
79.828536961178));
#220063=CARTESIAN_POINT('Ctrl Pts',(-33.4933016861709,86.5721052093522,
76.1682206227876));
#220064=CARTESIAN_POINT('Ctrl Pts',(-33.5909690724609,86.9713763527652,
72.1475129506798));
#220065=CARTESIAN_POINT('Ctrl Pts',(-33.6886364587509,86.0136387515289,
68.2221790390765));
#220066=CARTESIAN_POINT('Ctrl Pts',(-33.7863038450409,83.8074562217176,
64.8371729422474));
#220067=CARTESIAN_POINT('Ctrl Pts',(-33.8839712313309,80.602909363651,62.3762001539254));
#220068=CARTESIAN_POINT('Ctrl Pts',(-33.9816386176209,76.7632478138661,
61.1182228832598));
#220069=CARTESIAN_POINT('Ctrl Pts',(-34.0793060039109,72.723714283464,61.2058384479297));
#220070=CARTESIAN_POINT('Ctrl Pts',(-34.1769733902009,68.9422078613542,
62.6291152340622));
#220071=CARTESIAN_POINT('Ctrl Pts',(-34.2746407764909,65.8473791163074,
65.226718488844));
#220072=CARTESIAN_POINT('Ctrl Pts',(-34.3723081627809,63.7900406488467,
68.7041983321679));
#220073=CARTESIAN_POINT('Ctrl Pts',(-34.4699755490709,63.0034009229566,
72.66736695993));
#220074=CARTESIAN_POINT('Ctrl Pts',(-34.5676429353609,63.5766290496323,
76.666981584516));
#220075=CARTESIAN_POINT('Ctrl Pts',(-34.6653103216509,65.4447470716599,
80.2496681025062));
#220076=CARTESIAN_POINT('Ctrl Pts',(-34.7629777079409,68.3959955039791,
83.0093130653877));
#220077=CARTESIAN_POINT('Ctrl Pts',(-34.8606450942309,72.0958372130047,
84.6330984448554));
#220078=CARTESIAN_POINT('Ctrl Pts',(-34.9583124805209,76.1248786883367,
84.9369609474145));
#220079=CARTESIAN_POINT('Ctrl Pts',(-35.0559798668109,80.0264101621715,
83.8864564071508));
#220080=CARTESIAN_POINT('Ctrl Pts',(-35.1536472531009,83.3581756923815,
81.6006641851604));
#220081=CARTESIAN_POINT('Ctrl Pts',(-35.2513146393909,85.7425048402344,
78.338688994402));
#220082=CARTESIAN_POINT('Ctrl Pts',(-35.3489820256809,86.909123294031,74.4702902282876));
#220083=CARTESIAN_POINT('Ctrl Pts',(-35.4466494119709,86.7257896642541,
70.4339680891861));
#220084=CARTESIAN_POINT('Ctrl Pts',(-35.5443167982609,85.2132856330985,
66.6872576405197));
#220085=CARTESIAN_POINT('Ctrl Pts',(-35.6419841845509,82.5430602583853,
63.6548651727437));
#220086=CARTESIAN_POINT('Ctrl Pts',(-35.7396515708509,79.0177954604591,
61.6805258566955));
#220087=CARTESIAN_POINT('Ctrl Pts',(-35.8373189571409,75.0370956805214,
60.9880398334549));
#220088=CARTESIAN_POINT('Ctrl Pts',(-35.9349863434309,71.0521909402342,
61.6559034731574));
#220089=CARTESIAN_POINT('Ctrl Pts',(-36.0326537297209,67.5147879122209,
63.6084114623352));
#220090=CARTESIAN_POINT('Ctrl Pts',(-36.1303211160109,64.8258669600518,
66.6242383378935));
#220091=CARTESIAN_POINT('Ctrl Pts',(-36.2279885023009,63.2902292308876,
70.3615267125221));
#220092=CARTESIAN_POINT('Ctrl Pts',(-36.3256558885909,63.0819460901088,
74.3966383297692));
#220093=CARTESIAN_POINT('Ctrl Pts',(-36.4233232748809,64.2246273579156,
78.2721753442413));
#220094=CARTESIAN_POINT('Ctrl Pts',(-36.5209906611709,66.5887450312666,
81.5488284013896));
#220095=CARTESIAN_POINT('Ctrl Pts',(-36.6186580474609,69.9063158589901,
83.8551743063605));
#220096=CARTESIAN_POINT('Ctrl Pts',(-36.7163254337509,73.8012784349875,
84.9297784948445));
#220097=CARTESIAN_POINT('Ctrl Pts',(-36.8139928200409,77.8321214309277,
84.6508298034519));
#220098=CARTESIAN_POINT('Ctrl Pts',(-36.9116602063309,81.5419308686238,
83.0499483068092));
#220099=CARTESIAN_POINT('Ctrl Pts',(-37.0093275926209,84.510183351323,80.3086010414542));
#220100=CARTESIAN_POINT('Ctrl Pts',(-37.1069949789109,86.4004142607001,
76.7375319102928));
#220101=CARTESIAN_POINT('Ctrl Pts',(-37.2046623652009,86.9983575175985,
72.7415374793883));
#220102=CARTESIAN_POINT('Ctrl Pts',(-37.3023297514909,86.2362335948903,
68.7735814871058));
#220103=CARTESIAN_POINT('Ctrl Pts',(-37.3999971377809,84.2004326282222,
65.2834493901101));
#220104=CARTESIAN_POINT('Ctrl Pts',(-37.4976645240709,81.1217217102652,
62.6667631817018));
#220105=CARTESIAN_POINT('Ctrl Pts',(-37.5953319103609,77.3490864135083,
61.220135879683));
#220106=CARTESIAN_POINT('Ctrl Pts',(-37.6929992966509,73.3101717276327,
61.1075491215587));
#220107=CARTESIAN_POINT('Ctrl Pts',(-37.7906666829409,69.4628065837551,
62.3417651174235));
#220108=CARTESIAN_POINT('Ctrl Pts',(-37.8883340692309,66.2431069632321,
64.7828799942742));
#220109=CARTESIAN_POINT('Ctrl Pts',(-37.9860014555209,64.0160400101624,
68.1541825310843));
#220110=CARTESIAN_POINT('Ctrl Pts',(-38.0836688418109,63.0340541352225,
72.0735205728459));
#220111=CARTESIAN_POINT('Ctrl Pts',(-38.1813362281009,63.4084600571474,
76.0966198012584));
#220112=CARTESIAN_POINT('Ctrl Pts',(-38.2790036143909,65.0968237194401,
79.7674437395072));
#220113=CARTESIAN_POINT('Ctrl Pts',(-38.3766710006809,67.907737261243,82.669889249567));
#220114=CARTESIAN_POINT('Ctrl Pts',(-38.4743383869709,71.5226619404589,
84.4749471992292));
#220115=CARTESIAN_POINT('Ctrl Pts',(-38.5394499778309,74.195214694201,84.8103299141412));
#220116=CARTESIAN_POINT('Ctrl Pts',(-38.5720057732609,75.5216161759791,
84.7515103303026));
#220117=CARTESIAN_POINT('',(-37.8135594354587,70.2739654383489,85.0994033094111));
#220118=CARTESIAN_POINT('Ctrl Pts',(-37.8135412566021,70.2734991756117,
85.0992154535004));
#220119=CARTESIAN_POINT('Ctrl Pts',(-37.914194608833,70.3438095733745,84.9191033777816));
#220120=CARTESIAN_POINT('Ctrl Pts',(-38.0148481000433,70.4141195120353,
84.738990837336));
#220121=CARTESIAN_POINT('Ctrl Pts',(-38.2164814619069,70.5549662664303,
84.3781812921325));
#220122=CARTESIAN_POINT('Ctrl Pts',(-38.3174616206795,70.625503279821,84.1974837704057));
#220123=CARTESIAN_POINT('Ctrl Pts',(-38.4184416307608,70.6960396334767,
84.0167862995286));
#220124=CARTESIAN_POINT('',(-31.8032830015106,65.6643078538855,63.942145982536));
#220125=CARTESIAN_POINT('Ctrl Pts',(-36.4473639743914,87.0149197055719,
77.9529305295058));
#220126=CARTESIAN_POINT('Ctrl Pts',(-36.4543242139158,87.1337046269196,
77.665424594093));
#220127=CARTESIAN_POINT('Ctrl Pts',(-36.4612901076495,87.2421954633006,
77.3735933081721));
#220128=CARTESIAN_POINT('Ctrl Pts',(-36.4851178847728,87.5794817571952,
76.3557248300557));
#220129=CARTESIAN_POINT('Ctrl Pts',(-36.5017295071393,87.7549428334773,
75.6138431779786));
#220130=CARTESIAN_POINT('Ctrl Pts',(-36.5357271191037,87.9752973710121,
74.099549431073));
#220131=CARTESIAN_POINT('Ctrl Pts',(-36.5530472978884,88.0182807436117,
73.3298801212865));
#220132=CARTESIAN_POINT('Ctrl Pts',(-36.5916188607997,87.9609665594104,
71.58976080149));
#220133=CARTESIAN_POINT('Ctrl Pts',(-36.6128788214405,87.8201909513787,
70.6252211721631));
#220134=CARTESIAN_POINT('Ctrl Pts',(-36.6439275780304,87.4672144669563,
69.2817701998118));
#220135=CARTESIAN_POINT('Ctrl Pts',(-36.6532862550123,87.3417882891993,
68.8834745078011));
#220136=CARTESIAN_POINT('Ctrl Pts',(-36.6809277077594,86.9117980094235,
67.7171882447898));
#220137=CARTESIAN_POINT('Ctrl Pts',(-36.6989352535155,86.5530137947842,
66.9714444563634));
#220138=CARTESIAN_POINT('Ctrl Pts',(-36.7364462999144,85.680867030899,65.5283614602584));
#220139=CARTESIAN_POINT('Ctrl Pts',(-36.7557849234076,85.1637830132544,
64.8379432567854));
#220140=CARTESIAN_POINT('Ctrl Pts',(-36.7839680363835,84.300566023742,63.8964053745483));
#220141=CARTESIAN_POINT('Ctrl Pts',(-36.79313620763,84.0042231131444,63.6028486954881));
#220142=CARTESIAN_POINT('Ctrl Pts',(-36.8208522435962,83.0733987976403,
62.7654993629996));
#220143=CARTESIAN_POINT('Ctrl Pts',(-36.8396187225315,82.4001330837469,
62.2680924422089));
#220144=CARTESIAN_POINT('Ctrl Pts',(-36.8761199441608,80.991966806184,61.4239852534392));
#220145=CARTESIAN_POINT('Ctrl Pts',(-36.8937173024056,80.2630028772171,
61.0745500786368));
#220146=CARTESIAN_POINT('Ctrl Pts',(-36.9307904571172,78.6992531278834,
60.4966544983454));
#220147=CARTESIAN_POINT('Ctrl Pts',(-36.9501392419649,77.8645104056248,
60.2792475243341));
#220148=CARTESIAN_POINT('Ctrl Pts',(-36.9783085147289,76.6035404801462,
60.0814635701045));
#220149=CARTESIAN_POINT('Ctrl Pts',(-36.9874532249925,76.1897955949716,
60.0367710386153));
#220150=CARTESIAN_POINT('Ctrl Pts',(-37.0151750161543,74.9392545890132,
59.9621232756562));
#220151=CARTESIAN_POINT('Ctrl Pts',(-37.0339691243248,74.1010274283916,
59.9930378008006));
#220152=CARTESIAN_POINT('Ctrl Pts',(-37.0719391167667,72.4094517773143,
60.2199522860539));
#220153=CARTESIAN_POINT('Ctrl Pts',(-37.0908982866283,71.561074100533,60.4218495763451));
#220154=CARTESIAN_POINT('Ctrl Pts',(-37.1294214814689,69.9265064525839,
60.9889023507669));
#220155=CARTESIAN_POINT('Ctrl Pts',(-37.1487274281533,69.1437612082903,
61.3508266538269));
#220156=CARTESIAN_POINT('Ctrl Pts',(-37.1769356443394,68.0416056556518,
61.9999770084488));
#220157=CARTESIAN_POINT('Ctrl Pts',(-37.1861529674104,67.6911753126028,
62.2298685958544));
#220158=CARTESIAN_POINT('Ctrl Pts',(-37.214477195763,66.6574182380909,62.9818891792332));
#220159=CARTESIAN_POINT('Ctrl Pts',(-37.2338260991683,66.0142366260856,
63.5551852269181));
#220160=CARTESIAN_POINT('Ctrl Pts',(-37.2732001920621,64.8116847703535,
64.8624684866943));
#220161=CARTESIAN_POINT('Ctrl Pts',(-37.2932388578807,64.264126164404,65.6009596366178));
#220162=CARTESIAN_POINT('Ctrl Pts',(-37.3230050221112,63.5874803930889,
66.7496754353562));
#220163=CARTESIAN_POINT('Ctrl Pts',(-37.3323422503652,63.3934987902411,
67.1184103729201));
#220164=CARTESIAN_POINT('Ctrl Pts',(-37.3686321206999,62.7058503688647,
68.5933925755802));
#220165=CARTESIAN_POINT('Ctrl Pts',(-37.3949739782692,62.3500174026053,
69.7571023938164));
#220166=CARTESIAN_POINT('Ctrl Pts',(-37.4314600837915,62.0946346744905,
71.3678326654396));
#220167=CARTESIAN_POINT('Ctrl Pts',(-37.4408579427422,62.0490146141995,
71.7854526511129));
#220168=CARTESIAN_POINT('Ctrl Pts',(-37.4619584631861,61.9915130619058,
72.736770787313));
#220169=CARTESIAN_POINT('Ctrl Pts',(-37.4736509812777,61.9921173651715,
73.270469430752));
#220170=CARTESIAN_POINT('Ctrl Pts',(-37.5039566961825,62.077828664538,74.6370913696173));
#220171=CARTESIAN_POINT('Ctrl Pts',(-37.5227388742895,62.2105472640685,
75.464564129881));
#220172=CARTESIAN_POINT('Ctrl Pts',(-37.5600406728055,62.6343126277398,
77.0873268194587));
#220173=CARTESIAN_POINT('Ctrl Pts',(-37.5783792083311,62.9252991418412,
77.8785743582914));
#220174=CARTESIAN_POINT('Ctrl Pts',(-37.6162434269404,63.6644474380039,
79.4111631043095));
#220175=CARTESIAN_POINT('Ctrl Pts',(-37.6355728942984,64.1142489189937,
80.147156340735));
#220176=CARTESIAN_POINT('Ctrl Pts',(-37.6675712385135,64.9895008496932,
81.3038198263665));
#220177=CARTESIAN_POINT('Ctrl Pts',(-37.6805474167461,65.3771686591776,
81.7495558744315));
#220178=CARTESIAN_POINT('Ctrl Pts',(-37.7134056908055,66.420115336078,82.7956509277219));
#220179=CARTESIAN_POINT('Ctrl Pts',(-37.7333333337727,67.109129135656,83.3581304716378));
#220180=CARTESIAN_POINT('Ctrl Pts',(-37.7629134085071,68.229296810036,84.0958152528438));
#220181=CARTESIAN_POINT('Ctrl Pts',(-37.7729023062673,68.6213877917966,
84.3255348210361));
#220182=CARTESIAN_POINT('Ctrl Pts',(-37.7931080409524,69.4308381406786,
84.7444656957888));
#220183=CARTESIAN_POINT('Ctrl Pts',(-37.8033123696457,69.8477910971911,
84.933087944667));
#220184=CARTESIAN_POINT('Ctrl Pts',(-37.8135449901797,70.2738124000625,
85.099345644302));
#220185=CARTESIAN_POINT('Ctrl Pts',(-37.7678684231509,69.7754278285013,
84.9428528583425));
#220186=CARTESIAN_POINT('Ctrl Pts',(-37.8179054464809,71.812510839228,85.9277583999696));
#220187=CARTESIAN_POINT('Ctrl Pts',(-37.9179794931409,76.4517787269631,
86.8316803850283));
#220188=CARTESIAN_POINT('Ctrl Pts',(-38.0680905631309,83.2977536927465,
84.5014189876434));
#220189=CARTESIAN_POINT('Ctrl Pts',(-38.2182016331209,88.1688027886436,
78.9684584806007));
#220190=CARTESIAN_POINT('Ctrl Pts',(-38.3182756797809,89.1697068583504,
74.0638248418015));
#220191=CARTESIAN_POINT('Ctrl Pts',(-38.3683127031109,89.0196937392787,
71.6256255348517));
#220192=CARTESIAN_POINT('Ctrl Pts',(-37.9919965334309,69.9478523514013,
84.5483408522442));
#220193=CARTESIAN_POINT('Ctrl Pts',(-38.0420335567609,71.9165608444039,
85.5033627821869));
#220194=CARTESIAN_POINT('Ctrl Pts',(-38.1421076034109,76.4032882596886,
86.3839207906894));
#220195=CARTESIAN_POINT('Ctrl Pts',(-38.2922186734109,83.0331917990117,
84.1369185523978));
#220196=CARTESIAN_POINT('Ctrl Pts',(-38.4423297434009,87.7581170900009,
78.7835876157209));
#220197=CARTESIAN_POINT('Ctrl Pts',(-38.5424037900609,88.7339600476783,
74.0312248270542));
#220198=CARTESIAN_POINT('Ctrl Pts',(-38.5924408133809,88.5911688293687,
71.6672949557471));
#220199=CARTESIAN_POINT('Ctrl Pts',(-38.2161246437009,70.1202768743014,
84.1538288461459));
#220200=CARTESIAN_POINT('Ctrl Pts',(-38.2661616670309,72.0206108495836,
85.078967164395));
#220201=CARTESIAN_POINT('Ctrl Pts',(-38.3662357136909,76.354797792418,85.9361611963414));
#220202=CARTESIAN_POINT('Ctrl Pts',(-38.5163467836809,82.7686299052744,
83.7724181171587));
#220203=CARTESIAN_POINT('Ctrl Pts',(-38.6664578536809,87.347431391376,78.5987167508506));
#220204=CARTESIAN_POINT('Ctrl Pts',(-38.7665319003309,88.2982132370069,
73.9986248123051));
#220205=CARTESIAN_POINT('Ctrl Pts',(-38.8165689236609,88.1626439194586,
71.7089643766425));
#220206=CARTESIAN_POINT('Ctrl Pts',(-38.4402527539809,70.2927013972014,
83.7593168400476));
#220207=CARTESIAN_POINT('Ctrl Pts',(-38.4902897773109,72.1246608547595,
84.6545715466124));
#220208=CARTESIAN_POINT('Ctrl Pts',(-38.5903638239709,76.3063073251473,
85.4884016019933));
#220209=CARTESIAN_POINT('Ctrl Pts',(-38.7404748939609,82.50406801154,83.4079176819123));
#220210=CARTESIAN_POINT('Ctrl Pts',(-38.8905859639509,86.9367456927425,
78.4138458859747));
#220211=CARTESIAN_POINT('Ctrl Pts',(-38.9906600106109,87.8624664263344,
73.9660247975587));
#220212=CARTESIAN_POINT('Ctrl Pts',(-39.0406970339409,87.7341190095482,
71.7506337975389));
#220213=CARTESIAN_POINT('Ctrl Pts',(-38.9114901698969,87.9789324622055,
72.2490839199139));
#220214=CARTESIAN_POINT('Ctrl Pts',(-38.9253796493603,87.9522946700216,
72.2506022870319));
#220215=CARTESIAN_POINT('Ctrl Pts',(-38.9392691288105,87.9256568778308,
72.2521206541503));
#220216=CARTESIAN_POINT('Ctrl Pts',(-38.9670676750248,87.8723437280596,
72.2551595296326));
#220217=CARTESIAN_POINT('Ctrl Pts',(-38.9809767417889,87.8456683704791,
72.2566800379965));
#220218=CARTESIAN_POINT('Ctrl Pts',(-38.9948858085393,87.8189930128915,
72.2582005463608));
#220219=CARTESIAN_POINT('Ctrl Pts',(-38.6651607695591,87.0149202732382,
77.9529291555314));
#220220=CARTESIAN_POINT('Ctrl Pts',(-38.61247162501,86.5348402930432,79.1149107179875));
#220221=CARTESIAN_POINT('Ctrl Pts',(-38.5579303068348,85.888739014892,80.2010992341742));
#220222=CARTESIAN_POINT('Ctrl Pts',(-38.4509479952484,84.2940740611299,
82.1673583393616));
#220223=CARTESIAN_POINT('Ctrl Pts',(-38.3992043907891,83.350151501424,83.0337413163218));
#220224=CARTESIAN_POINT('Ctrl Pts',(-38.3094997884851,81.6049979618063,
84.2169638927091));
#220225=CARTESIAN_POINT('Ctrl Pts',(-38.2735339351583,80.8712054740595,
84.617501870553));
#220226=CARTESIAN_POINT('Ctrl Pts',(-38.166422504845,78.5525910761281,85.6073284218056));
#220227=CARTESIAN_POINT('Ctrl Pts',(-38.0982006061265,76.8869101288329,
85.9613759922045));
#220228=CARTESIAN_POINT('Ctrl Pts',(-37.9903150495058,74.367121750432,86.0001753956269));
#220229=CARTESIAN_POINT('Ctrl Pts',(-37.9546993734579,73.5347687972715,
85.9328938291296));
#220230=CARTESIAN_POINT('Ctrl Pts',(-37.8839532152002,71.8806570845743,
85.6374986271245));
#220231=CARTESIAN_POINT('Ctrl Pts',(-37.8490190852945,71.0632872725336,
85.4074198623627));
#220232=CARTESIAN_POINT('Ctrl Pts',(-37.8135657720877,70.2741279641925,
85.0994687906042));
#220233=CARTESIAN_POINT('Origin',(-39.1448867524609,88.9773118829169,72.1921758070624));
#220234=CARTESIAN_POINT('Ctrl Pts',(-39.2948856686008,87.8189932824241,
72.2582005309974));
#220235=CARTESIAN_POINT('Ctrl Pts',(-39.3087857943346,87.8456514869417,
72.2566810003664));
#220236=CARTESIAN_POINT('Ctrl Pts',(-39.3226859200676,87.8723096914597,
72.2551614697354));
#220237=CARTESIAN_POINT('Ctrl Pts',(-39.3504844252439,87.925622751396,72.2521225993737));
#220238=CARTESIAN_POINT('Ctrl Pts',(-39.3643828046871,87.9522776068144,
72.250603259643));
#220239=CARTESIAN_POINT('Ctrl Pts',(-39.3782811841296,87.9789324622331,
72.2490839199123));
#220240=CARTESIAN_POINT('Ctrl Pts',(-38.6717262017909,70.2927013972015,
83.7593168400477));
#220241=CARTESIAN_POINT('Ctrl Pts',(-38.7217632251209,72.1246608547595,
84.6545715466124));
#220242=CARTESIAN_POINT('Ctrl Pts',(-38.8218372717809,76.3063073251473,
85.4884016019933));
#220243=CARTESIAN_POINT('Ctrl Pts',(-38.9719483417709,82.50406801154,83.4079176819123));
#220244=CARTESIAN_POINT('Ctrl Pts',(-39.1220594117609,86.9367456927426,
78.4138458859746));
#220245=CARTESIAN_POINT('Ctrl Pts',(-39.2221334584209,87.8624664263348,
73.9660247975578));
#220246=CARTESIAN_POINT('Ctrl Pts',(-39.2721704817509,87.7341190095482,
71.7506337975389));
#220247=CARTESIAN_POINT('Ctrl Pts',(-38.8958543120709,70.1202768743015,
84.153828846146));
#220248=CARTESIAN_POINT('Ctrl Pts',(-38.9458913354009,72.0206108495836,
85.078967164395));
#220249=CARTESIAN_POINT('Ctrl Pts',(-39.0459653820509,76.354797792418,85.9361611963414));
#220250=CARTESIAN_POINT('Ctrl Pts',(-39.1960764520509,82.7686299052747,
83.7724181171578));
#220251=CARTESIAN_POINT('Ctrl Pts',(-39.3461875220409,87.347431391376,78.5987167508506));
#220252=CARTESIAN_POINT('Ctrl Pts',(-39.4462615687009,88.2982132370069,
73.9986248123051));
#220253=CARTESIAN_POINT('Ctrl Pts',(-39.4962985920209,88.1626439194586,
71.7089643766425));
#220254=CARTESIAN_POINT('Ctrl Pts',(-39.1199824223409,69.9478523514015,
84.5483408522443));
#220255=CARTESIAN_POINT('Ctrl Pts',(-39.1700194456709,71.9165608444039,
85.5033627821869));
#220256=CARTESIAN_POINT('Ctrl Pts',(-39.2700934923309,76.4032882596886,
86.3839207906894));
#220257=CARTESIAN_POINT('Ctrl Pts',(-39.4202045623209,83.0331917990117,
84.1369185523978));
#220258=CARTESIAN_POINT('Ctrl Pts',(-39.5703156323209,87.758117090001,78.7835876157208));
#220259=CARTESIAN_POINT('Ctrl Pts',(-39.6703896789709,88.7339600476783,
74.0312248270542));
#220260=CARTESIAN_POINT('Ctrl Pts',(-39.7204267023009,88.5911688293687,
71.6672949557471));
#220261=CARTESIAN_POINT('Ctrl Pts',(-39.3441105326209,69.7754278285015,
84.9428528583426));
#220262=CARTESIAN_POINT('Ctrl Pts',(-39.3941475559509,71.812510839228,85.9277583999696));
#220263=CARTESIAN_POINT('Ctrl Pts',(-39.4942216026109,76.4517787269631,
86.8316803850283));
#220264=CARTESIAN_POINT('Ctrl Pts',(-39.6443326726009,83.2977536927465,
84.5014189876434));
#220265=CARTESIAN_POINT('Ctrl Pts',(-39.7944437425909,88.1688027886436,
78.9684584806006));
#220266=CARTESIAN_POINT('Ctrl Pts',(-39.8945177892509,89.1697068583508,
74.0638248418006));
#220267=CARTESIAN_POINT('Ctrl Pts',(-39.9445548125809,89.0196937392787,
71.6256255348517));
#220268=CARTESIAN_POINT('Ctrl Pts',(-38.7166027955229,70.6961178052446,
84.016824453434));
#220269=CARTESIAN_POINT('Ctrl Pts',(-38.8175043475842,70.6256382812911,
84.1973835573518));
#220270=CARTESIAN_POINT('Ctrl Pts',(-38.9184059185855,70.5551581924261,
84.3779424805074));
#220271=CARTESIAN_POINT('Ctrl Pts',(-39.120038274912,70.4143162025418,84.7387542827717));
#220272=CARTESIAN_POINT('Ctrl Pts',(-39.2207694758059,70.3439540131132,
84.9190079062487));
#220273=CARTESIAN_POINT('Ctrl Pts',(-39.3215005357773,70.2735913682008,
85.0992610619776));
#220274=CARTESIAN_POINT('Ctrl Pts',(-32.5527664985109,70.5807652625035,
62.0755168906179));
#220275=CARTESIAN_POINT('Ctrl Pts',(-32.5853222939409,69.3501285260828,
62.5738479625974));
#220276=CARTESIAN_POINT('Ctrl Pts',(-32.6504338848009,67.0593648594363,
63.9906830308551));
#220277=CARTESIAN_POINT('Ctrl Pts',(-32.7481012710909,64.5230776800325,
67.1360227552467));
#220278=CARTESIAN_POINT('Ctrl Pts',(-32.8457686573809,63.1744626819709,
70.9447840322971));
#220279=CARTESIAN_POINT('Ctrl Pts',(-32.9434360436709,63.1663071209847,
74.9852609507785));
#220280=CARTESIAN_POINT('Ctrl Pts',(-33.0411034299609,64.4995580412843,
78.7994383430527));
#220281=CARTESIAN_POINT('Ctrl Pts',(-33.1387708162509,67.0230794732875,
81.9549646900448));
#220282=CARTESIAN_POINT('Ctrl Pts',(-33.2364382025409,70.4508206617514,
84.0941463918273));
#220283=CARTESIAN_POINT('Ctrl Pts',(-33.3341055888209,74.3942314659886,
84.9744978657157));
#220284=CARTESIAN_POINT('Ctrl Pts',(-33.4317729751109,78.4063088519184,
84.4962273102157));
#220285=CARTESIAN_POINT('Ctrl Pts',(-33.5294403614009,82.0322659755195,
82.7135488322343));
#220286=CARTESIAN_POINT('Ctrl Pts',(-33.6271077476909,84.8610844810572,
79.828536961178));
#220287=CARTESIAN_POINT('Ctrl Pts',(-33.7247751339809,86.5721052093522,
76.1682206227876));
#220288=CARTESIAN_POINT('Ctrl Pts',(-33.8224425202709,86.9713763527652,
72.1475129506798));
#220289=CARTESIAN_POINT('Ctrl Pts',(-33.9201099065609,86.0136387515289,
68.2221790390765));
#220290=CARTESIAN_POINT('Ctrl Pts',(-34.0177772928509,83.8074562217176,
64.8371729422474));
#220291=CARTESIAN_POINT('Ctrl Pts',(-34.1154446791409,80.602909363651,62.3762001539254));
#220292=CARTESIAN_POINT('Ctrl Pts',(-34.2131120654309,76.7632478138661,
61.1182228832598));
#220293=CARTESIAN_POINT('Ctrl Pts',(-34.3107794517209,72.723714283464,61.2058384479297));
#220294=CARTESIAN_POINT('Ctrl Pts',(-34.4084468380109,68.9422078613546,
62.6291152340613));
#220295=CARTESIAN_POINT('Ctrl Pts',(-34.5061142243009,65.8473791163074,
65.226718488844));
#220296=CARTESIAN_POINT('Ctrl Pts',(-34.6037816105909,63.7900406488467,
68.7041983321679));
#220297=CARTESIAN_POINT('Ctrl Pts',(-34.7014489968809,63.0034009229566,
72.66736695993));
#220298=CARTESIAN_POINT('Ctrl Pts',(-34.7991163831709,63.5766290496323,
76.666981584516));
#220299=CARTESIAN_POINT('Ctrl Pts',(-34.8967837694509,65.4447470716599,
80.2496681025062));
#220300=CARTESIAN_POINT('Ctrl Pts',(-34.9944511557409,68.3959955039791,
83.0093130653877));
#220301=CARTESIAN_POINT('Ctrl Pts',(-35.0921185420309,72.0958372130047,
84.6330984448554));
#220302=CARTESIAN_POINT('Ctrl Pts',(-35.1897859283209,76.1248786883367,
84.9369609474145));
#220303=CARTESIAN_POINT('Ctrl Pts',(-35.2874533146109,80.0264101621715,
83.8864564071508));
#220304=CARTESIAN_POINT('Ctrl Pts',(-35.3851207009009,83.3581756923815,
81.6006641851604));
#220305=CARTESIAN_POINT('Ctrl Pts',(-35.4827880871909,85.7425048402343,
78.3386889944021));
#220306=CARTESIAN_POINT('Ctrl Pts',(-35.5804554734809,86.909123294031,74.4702902282876));
#220307=CARTESIAN_POINT('Ctrl Pts',(-35.6781228597709,86.7257896642541,
70.4339680891861));
#220308=CARTESIAN_POINT('Ctrl Pts',(-35.7757902460609,85.2132856330985,
66.6872576405197));
#220309=CARTESIAN_POINT('Ctrl Pts',(-35.8734576323509,82.5430602583853,
63.6548651727437));
#220310=CARTESIAN_POINT('Ctrl Pts',(-35.9711250186409,79.017795460459,61.6805258566955));
#220311=CARTESIAN_POINT('Ctrl Pts',(-36.0687924049309,75.0370956805214,
60.9880398334549));
#220312=CARTESIAN_POINT('Ctrl Pts',(-36.1664597912209,71.0521909402342,
61.6559034731574));
#220313=CARTESIAN_POINT('Ctrl Pts',(-36.2641271775109,67.5147879122209,
63.6084114623352));
#220314=CARTESIAN_POINT('Ctrl Pts',(-36.3617945638009,64.8258669600518,
66.6242383378935));
#220315=CARTESIAN_POINT('Ctrl Pts',(-36.4594619500909,63.2902292308876,
70.3615267125221));
#220316=CARTESIAN_POINT('Ctrl Pts',(-36.5571293363809,63.0819460901088,
74.3966383297692));
#220317=CARTESIAN_POINT('Ctrl Pts',(-36.6547967226709,64.2246273579156,
78.2721753442413));
#220318=CARTESIAN_POINT('Ctrl Pts',(-36.7524641089609,66.5887450312666,
81.5488284013896));
#220319=CARTESIAN_POINT('Ctrl Pts',(-36.8501314952509,69.9063158589901,
83.8551743063605));
#220320=CARTESIAN_POINT('Ctrl Pts',(-36.9477988815409,73.8012784349875,
84.9297784948445));
#220321=CARTESIAN_POINT('Ctrl Pts',(-37.0454662678409,77.8321214309277,
84.6508298034519));
#220322=CARTESIAN_POINT('Ctrl Pts',(-37.1431336541309,81.5419308686238,
83.0499483068092));
#220323=CARTESIAN_POINT('Ctrl Pts',(-37.2408010404209,84.510183351323,80.3086010414542));
#220324=CARTESIAN_POINT('Ctrl Pts',(-37.3384684267109,86.4004142607001,
76.7375319102928));
#220325=CARTESIAN_POINT('Ctrl Pts',(-37.4361358130009,86.9983575175985,
72.7415374793883));
#220326=CARTESIAN_POINT('Ctrl Pts',(-37.5338031992909,86.2362335948903,
68.7735814871058));
#220327=CARTESIAN_POINT('Ctrl Pts',(-37.6314705855809,84.2004326282222,
65.2834493901101));
#220328=CARTESIAN_POINT('Ctrl Pts',(-37.7291379718709,81.1217217102652,
62.6667631817018));
#220329=CARTESIAN_POINT('Ctrl Pts',(-37.8268053581609,77.3490864135083,
61.220135879683));
#220330=CARTESIAN_POINT('Ctrl Pts',(-37.9244727444509,73.3101717276327,
61.1075491215587));
#220331=CARTESIAN_POINT('Ctrl Pts',(-38.0221401307409,69.4628065837551,
62.3417651174235));
#220332=CARTESIAN_POINT('Ctrl Pts',(-38.1198075170309,66.2431069632321,
64.7828799942742));
#220333=CARTESIAN_POINT('Ctrl Pts',(-38.2174749033309,64.0160400101624,
68.1541825310843));
#220334=CARTESIAN_POINT('Ctrl Pts',(-38.3151422896209,63.0340541352225,
72.0735205728459));
#220335=CARTESIAN_POINT('Ctrl Pts',(-38.4128096759109,63.4084600571474,
76.0966198012584));
#220336=CARTESIAN_POINT('Ctrl Pts',(-38.5104770622009,65.0968237194401,
79.7674437395072));
#220337=CARTESIAN_POINT('Ctrl Pts',(-38.6081444484909,67.907737261243,82.669889249567));
#220338=CARTESIAN_POINT('Ctrl Pts',(-38.7058118347809,71.5226619404589,
84.4749471992292));
#220339=CARTESIAN_POINT('Ctrl Pts',(-38.7709234256409,74.195214694201,84.8103299141412));
#220340=CARTESIAN_POINT('Ctrl Pts',(-38.8034792210709,75.5216161759791,
84.7515103303026));
#220341=CARTESIAN_POINT('Ctrl Pts',(-32.7768946087909,70.4191672475379,
61.6764479484404));
#220342=CARTESIAN_POINT('Ctrl Pts',(-32.8094504042209,69.1435298570313,
62.1930014767527));
#220343=CARTESIAN_POINT('Ctrl Pts',(-32.8745619950809,66.7689999088247,
63.6616459075254));
#220344=CARTESIAN_POINT('Ctrl Pts',(-32.9722293813709,64.1399683974443,
66.9220011687802));
#220345=CARTESIAN_POINT('Ctrl Pts',(-33.0698967676509,62.7420386379846,
70.8700372973402));
#220346=CARTESIAN_POINT('Ctrl Pts',(-33.1675641539409,62.7335848528663,
75.0582622057643));
#220347=CARTESIAN_POINT('Ctrl Pts',(-33.2652315402309,64.1155887168238,
79.0119125004583));
#220348=CARTESIAN_POINT('Ctrl Pts',(-33.3628989265209,66.7313876761263,
82.2828268782175));
#220349=CARTESIAN_POINT('Ctrl Pts',(-33.4605663128109,70.2844709667367,
84.500231968704));
#220350=CARTESIAN_POINT('Ctrl Pts',(-33.5582336991009,74.3720803474283,
85.4127752267091));
#220351=CARTESIAN_POINT('Ctrl Pts',(-33.6559010853909,78.5308672385013,
84.9170157671447));
#220352=CARTESIAN_POINT('Ctrl Pts',(-33.7535684716809,82.2894146199872,
83.0691501424084));
#220353=CARTESIAN_POINT('Ctrl Pts',(-33.8512358579709,85.2216744411351,
80.0786421347599));
#220354=CARTESIAN_POINT('Ctrl Pts',(-33.9489032442609,86.9952620095349,
76.2844791261685));
#220355=CARTESIAN_POINT('Ctrl Pts',(-34.0465706305509,87.4091332880509,
72.1167463655193));
#220356=CARTESIAN_POINT('Ctrl Pts',(-34.1442380168409,86.4163741266587,
68.0478748946176));
#220357=CARTESIAN_POINT('Ctrl Pts',(-34.2419054031309,84.1295181910076,
64.5390893883722));
#220358=CARTESIAN_POINT('Ctrl Pts',(-34.3395727894109,80.8077907707222,
61.9881262869919));
#220359=CARTESIAN_POINT('Ctrl Pts',(-34.4372401757009,76.8277244401432,
60.684148601805));
#220360=CARTESIAN_POINT('Ctrl Pts',(-34.5349075619909,72.6404774166431,
60.7749680020176));
#220361=CARTESIAN_POINT('Ctrl Pts',(-34.6325749482809,68.7206927704309,
62.2502897047617));
#220362=CARTESIAN_POINT('Ctrl Pts',(-34.7302423345709,65.5126955218893,
64.9428794344855));
#220363=CARTESIAN_POINT('Ctrl Pts',(-34.8279097208609,63.3801264246424,
68.5475201717518));
#220364=CARTESIAN_POINT('Ctrl Pts',(-34.9255771071509,62.5647216691142,
72.6556098596656));
#220365=CARTESIAN_POINT('Ctrl Pts',(-35.0232444934409,63.1589110103241,
76.8014782640017));
#220366=CARTESIAN_POINT('Ctrl Pts',(-35.1209118797309,65.0953404441711,
80.5151727650388));
#220367=CARTESIAN_POINT('Ctrl Pts',(-35.2185792660209,68.1545070833008,
83.3757295768015));
#220368=CARTESIAN_POINT('Ctrl Pts',(-35.3162466523109,71.9896407854853,
85.0588918641796));
#220369=CARTESIAN_POINT('Ctrl Pts',(-35.4139140386009,76.1660120912788,
85.3738656971174));
#220370=CARTESIAN_POINT('Ctrl Pts',(-35.5115814248909,80.2102107414312,
84.2849473910145));
#220371=CARTESIAN_POINT('Ctrl Pts',(-35.6092488111809,83.6638088349665,
81.9155706781228));
#220372=CARTESIAN_POINT('Ctrl Pts',(-35.7069161974709,86.1353256703195,
78.5343149451388));
#220373=CARTESIAN_POINT('Ctrl Pts',(-35.8045835837609,87.3446038237173,
74.5244605653653));
#220374=CARTESIAN_POINT('Ctrl Pts',(-35.9022509700509,87.1545662389771,
70.3405423640075));
#220375=CARTESIAN_POINT('Ctrl Pts',(-35.9999183563409,85.5867545214038,
66.4568260744839));
#220376=CARTESIAN_POINT('Ctrl Pts',(-36.0975857426309,82.818887101022,63.3135482085524));
#220377=CARTESIAN_POINT('Ctrl Pts',(-36.1952531289209,79.1647140582467,
61.2670132900358));
#220378=CARTESIAN_POINT('Ctrl Pts',(-36.2929205152109,75.0384521570716,
60.5492051525981));
#220379=CARTESIAN_POINT('Ctrl Pts',(-36.3905879015009,70.9078315329049,
61.2414905405987));
#220380=CARTESIAN_POINT('Ctrl Pts',(-36.4882552877909,67.2410764017834,
63.2653958268243));
#220381=CARTESIAN_POINT('Ctrl Pts',(-36.5859226740809,64.4538297633518,
66.3915023470505));
#220382=CARTESIAN_POINT('Ctrl Pts',(-36.6835900603709,62.8620384185835,
70.2654520258604));
#220383=CARTESIAN_POINT('Ctrl Pts',(-36.7812574466609,62.6461389948745,
74.4481154402485));
#220384=CARTESIAN_POINT('Ctrl Pts',(-36.8789248329509,63.8306046519742,
78.4653690924802));
#220385=CARTESIAN_POINT('Ctrl Pts',(-36.9765922192409,66.2811709404978,
81.8618394169132));
#220386=CARTESIAN_POINT('Ctrl Pts',(-37.0742596055309,69.7200552743181,
84.2525213986484));
#220387=CARTESIAN_POINT('Ctrl Pts',(-37.1719269918209,73.7574448219614,
85.3664206040375));
#220388=CARTESIAN_POINT('Ctrl Pts',(-37.2695943781109,77.935683524501,85.0772716047947));
#220389=CARTESIAN_POINT('Ctrl Pts',(-37.3672617644009,81.7811494449743,
83.4178507257861));
#220390=CARTESIAN_POINT('Ctrl Pts',(-37.4649291506909,84.8579419210346,
80.5762607028601));
#220391=CARTESIAN_POINT('Ctrl Pts',(-37.5625965369809,86.8172928434819,
76.8746084012713));
#220392=CARTESIAN_POINT('Ctrl Pts',(-37.6602639232709,87.4371010722797,
72.7324925701221));
#220393=CARTESIAN_POINT('Ctrl Pts',(-37.7579313095609,86.6471085885194,
68.6194404582812));
#220394=CARTESIAN_POINT('Ctrl Pts',(-37.8555986958509,84.5368645531706,
65.0016848127869));
#220395=CARTESIAN_POINT('Ctrl Pts',(-37.9532660821509,81.3455745117745,
62.2893143236978));
#220396=CARTESIAN_POINT('Ctrl Pts',(-38.0509334684409,77.4349853810736,
60.7897882475));
#220397=CARTESIAN_POINT('Ctrl Pts',(-38.1486008547309,73.2483798313682,
60.6730845330001));
#220398=CARTESIAN_POINT('Ctrl Pts',(-38.2462682410209,69.2603282096219,
61.9524320656215));
#220399=CARTESIAN_POINT('Ctrl Pts',(-38.3439356273109,65.9228939362941,
64.4828111119111));
#220400=CARTESIAN_POINT('Ctrl Pts',(-38.4416030136009,63.6143898973541,
67.9773919605015));
#220401=CARTESIAN_POINT('Ctrl Pts',(-38.5392703998909,62.5964957764151,
72.040048310785));
#220402=CARTESIAN_POINT('Ctrl Pts',(-38.6369377861809,62.9845925876825,
76.2102600797003));
#220403=CARTESIAN_POINT('Ctrl Pts',(-38.7346051724709,64.7346945898851,
80.0153149192111));
#220404=CARTESIAN_POINT('Ctrl Pts',(-38.8322725587709,67.648394717053,83.0238940611853));
#220405=CARTESIAN_POINT('Ctrl Pts',(-38.9299399450609,71.39550623112,84.8949575070187));
#220406=CARTESIAN_POINT('Ctrl Pts',(-38.9950515359209,74.1657861357241,
85.2426041509183));
#220407=CARTESIAN_POINT('Ctrl Pts',(-39.0276073313509,75.5406900979627,
85.1816337132427));
#220408=CARTESIAN_POINT('Ctrl Pts',(-33.0010227190609,70.2575692325718,
61.2773790062616));
#220409=CARTESIAN_POINT('Ctrl Pts',(-33.0335785144909,68.9369311879788,
61.8121549909076));
#220410=CARTESIAN_POINT('Ctrl Pts',(-33.0986901053509,66.4786349582126,
63.3326087841967));
#220411=CARTESIAN_POINT('Ctrl Pts',(-33.1963574916409,63.7568591148654,
66.7079795823175));
#220412=CARTESIAN_POINT('Ctrl Pts',(-33.2940248779309,62.3096145940082,
70.7952905623853));
#220413=CARTESIAN_POINT('Ctrl Pts',(-33.3916922642209,62.3008625847488,
75.1312634607482));
#220414=CARTESIAN_POINT('Ctrl Pts',(-33.4893596505109,63.7316193923605,
79.224386657865));
#220415=CARTESIAN_POINT('Ctrl Pts',(-33.5870270368009,66.4396958789624,
82.610689066389));
#220416=CARTESIAN_POINT('Ctrl Pts',(-33.6846944230909,70.1181212717175,
84.9063175455788));
#220417=CARTESIAN_POINT('Ctrl Pts',(-33.7823618093809,74.3499292288595,
85.8510525877097));
#220418=CARTESIAN_POINT('Ctrl Pts',(-33.8800291956709,78.6554256250739,
85.3378042240803));
#220419=CARTESIAN_POINT('Ctrl Pts',(-33.9776965819609,82.5465632644516,
83.4247514525909));
#220420=CARTESIAN_POINT('Ctrl Pts',(-34.0753639682509,85.5822644011988,
80.32874730835));
#220421=CARTESIAN_POINT('Ctrl Pts',(-34.1730313545409,87.4184188097211,
76.4007376295671));
#220422=CARTESIAN_POINT('Ctrl Pts',(-34.2706987408209,87.8468902233397,
72.0859797803774));
#220423=CARTESIAN_POINT('Ctrl Pts',(-34.3683661271109,86.8191095017967,
67.8735707501784));
#220424=CARTESIAN_POINT('Ctrl Pts',(-34.4660335134009,84.4515801603142,
64.2410058345146));
#220425=CARTESIAN_POINT('Ctrl Pts',(-34.5637008996909,81.0126721778146,
61.6000524200778));
#220426=CARTESIAN_POINT('Ctrl Pts',(-34.6613682859809,76.8922010664508,
60.250074320352));
#220427=CARTESIAN_POINT('Ctrl Pts',(-34.7590356722709,72.5572405498546,
60.3440975560973));
#220428=CARTESIAN_POINT('Ctrl Pts',(-34.8567030585609,68.4991776795392,
61.8714641754451));
#220429=CARTESIAN_POINT('Ctrl Pts',(-34.9543704448509,65.1780119274846,
64.6590403800947));
#220430=CARTESIAN_POINT('Ctrl Pts',(-35.0520378311409,62.9702122004541,
68.390842011297));
#220431=CARTESIAN_POINT('Ctrl Pts',(-35.1497052174309,62.1260424152783,
72.6438527593594));
#220432=CARTESIAN_POINT('Ctrl Pts',(-35.2473726037209,62.7411929710006,
76.9359749434432));
#220433=CARTESIAN_POINT('Ctrl Pts',(-35.3450399900109,64.7459338166531,
80.780677427527));
#220434=CARTESIAN_POINT('Ctrl Pts',(-35.4427073763009,67.9130186625803,
83.7421460881763));
#220435=CARTESIAN_POINT('Ctrl Pts',(-35.5403747625909,71.8834443579084,
85.484685283491));
#220436=CARTESIAN_POINT('Ctrl Pts',(-35.6380421488809,76.2071454941548,
85.8107704468362));
#220437=CARTESIAN_POINT('Ctrl Pts',(-35.7357095351709,80.3940113206321,
84.6834383749048));
#220438=CARTESIAN_POINT('Ctrl Pts',(-35.8333769214609,83.9694419775097,
82.2304771711338));
#220439=CARTESIAN_POINT('Ctrl Pts',(-35.9310443077509,86.5281465003784,
78.729940895939));
#220440=CARTESIAN_POINT('Ctrl Pts',(-36.0287116940409,87.7800843533953,
74.5786309025152));
#220441=CARTESIAN_POINT('Ctrl Pts',(-36.1263790803309,87.5833428137125,
70.2471166389011));
#220442=CARTESIAN_POINT('Ctrl Pts',(-36.2240464666209,85.9602234097461,
66.2263945085208));
#220443=CARTESIAN_POINT('Ctrl Pts',(-36.3217138529109,83.0947139437118,
62.9722312444263));
#220444=CARTESIAN_POINT('Ctrl Pts',(-36.4193812392009,79.3116326561084,
60.8535007234067));
#220445=CARTESIAN_POINT('Ctrl Pts',(-36.5170486254909,75.0398086337074,
60.1103704717333));
#220446=CARTESIAN_POINT('Ctrl Pts',(-36.6147160117809,70.7634721256552,
60.8270776080123));
#220447=CARTESIAN_POINT('Ctrl Pts',(-36.7123833980709,66.967364891402,62.9223801912565));
#220448=CARTESIAN_POINT('Ctrl Pts',(-36.8100507843609,64.0817925667024,
66.1587663561376));
#220449=CARTESIAN_POINT('Ctrl Pts',(-36.9077181706509,62.433847606303,70.1693773391154));
#220450=CARTESIAN_POINT('Ctrl Pts',(-37.0053855569409,62.2103318996323,
74.4995925506424));
#220451=CARTESIAN_POINT('Ctrl Pts',(-37.1030529432309,63.4365819459936,
78.6585628406411));
#220452=CARTESIAN_POINT('Ctrl Pts',(-37.2007203295209,65.9735968496646,
82.1748504323778));
#220453=CARTESIAN_POINT('Ctrl Pts',(-37.2983877158209,69.5337946895659,
84.6498684909033));
#220454=CARTESIAN_POINT('Ctrl Pts',(-37.3960551021109,73.7136112088471,
85.8030627132265));
#220455=CARTESIAN_POINT('Ctrl Pts',(-37.4937224884009,78.0392456179921,
85.5037134061586));
#220456=CARTESIAN_POINT('Ctrl Pts',(-37.5913898746909,82.0203680212412,
83.7857531448031));
#220457=CARTESIAN_POINT('Ctrl Pts',(-37.6890572609809,85.2057004907068,
80.8439203643352));
#220458=CARTESIAN_POINT('Ctrl Pts',(-37.7867246472709,87.2341714262334,
77.0116848923229));
#220459=CARTESIAN_POINT('Ctrl Pts',(-37.8843920335609,87.8758446269618,
72.7234476609321));
#220460=CARTESIAN_POINT('Ctrl Pts',(-37.9820594198509,87.0579835821749,
68.4652994295259));
#220461=CARTESIAN_POINT('Ctrl Pts',(-38.0797268061409,84.873296478161,64.7199202355244));
#220462=CARTESIAN_POINT('Ctrl Pts',(-38.1773941924309,81.5694273133449,
61.9118654657189));
#220463=CARTESIAN_POINT('Ctrl Pts',(-38.2750615787209,77.520884348699,60.3594406153311));
#220464=CARTESIAN_POINT('Ctrl Pts',(-38.3727289650109,73.1865879351576,
60.238619944442));
#220465=CARTESIAN_POINT('Ctrl Pts',(-38.4703963513009,69.0578498355331,
61.5630990137956));
#220466=CARTESIAN_POINT('Ctrl Pts',(-38.5680637375909,65.602680909391,64.1827422295159));
#220467=CARTESIAN_POINT('Ctrl Pts',(-38.6657311238809,63.2127397845698,
67.8006013898867));
#220468=CARTESIAN_POINT('Ctrl Pts',(-38.7633985101709,62.1589374176099,
72.0065760486925));
#220469=CARTESIAN_POINT('Ctrl Pts',(-38.8610658964609,62.5607251182124,
76.3239003581206));
#220470=CARTESIAN_POINT('Ctrl Pts',(-38.9587332827509,64.3725654603181,
80.2631860989099));
#220471=CARTESIAN_POINT('Ctrl Pts',(-39.0564006690409,67.3890521728565,
83.3778988728009));
#220472=CARTESIAN_POINT('Ctrl Pts',(-39.1540680553309,71.2683505217792,
85.3149678148183));
#220473=CARTESIAN_POINT('Ctrl Pts',(-39.2191796461909,74.1363575772585,
85.6748783876892));
#220474=CARTESIAN_POINT('Ctrl Pts',(-39.2517354416209,75.5597640199593,
85.6117570961773));
#220475=CARTESIAN_POINT('Ctrl Pts',(-33.2251508293409,70.0959712176063,
60.8783100640841));
#220476=CARTESIAN_POINT('Ctrl Pts',(-33.2577066247709,68.7303325189268,
61.4313085050616));
#220477=CARTESIAN_POINT('Ctrl Pts',(-33.3228182156309,66.1882700076009,
63.0035716608669));
#220478=CARTESIAN_POINT('Ctrl Pts',(-33.4204856019209,63.3737498322777,
66.4939579958501));
#220479=CARTESIAN_POINT('Ctrl Pts',(-33.5181529882109,61.8771905500222,
70.7205438274275));
#220480=CARTESIAN_POINT('Ctrl Pts',(-33.6158203745009,61.8681403166308,
75.2042647157331));
#220481=CARTESIAN_POINT('Ctrl Pts',(-33.7134877607909,63.3476500679026,
79.4368608152641));
#220482=CARTESIAN_POINT('Ctrl Pts',(-33.8111551470709,66.1480040818002,
82.9385512545613));
#220483=CARTESIAN_POINT('Ctrl Pts',(-33.9088225333609,69.9517715767027,
85.3124031224554));
#220484=CARTESIAN_POINT('Ctrl Pts',(-34.0064899196509,74.3277781103001,
86.2893299487034));
#220485=CARTESIAN_POINT('Ctrl Pts',(-34.1041573059409,78.7799840116568,
85.7585926810094));
#220486=CARTESIAN_POINT('Ctrl Pts',(-34.2018246922309,82.8037119089286,
83.7803527627689));
#220487=CARTESIAN_POINT('Ctrl Pts',(-34.2994920785209,85.9428543612762,
80.5788524819328));
#220488=CARTESIAN_POINT('Ctrl Pts',(-34.3971594648109,87.8415756099131,
76.5169961329518));
#220489=CARTESIAN_POINT('Ctrl Pts',(-34.4948268511009,88.2846471586345,
72.0552131952207));
#220490=CARTESIAN_POINT('Ctrl Pts',(-34.5924942373909,87.2218448769265,
67.6992666057196));
#220491=CARTESIAN_POINT('Ctrl Pts',(-34.6901616236809,84.7736421296089,
63.9429222806305));
#220492=CARTESIAN_POINT('Ctrl Pts',(-34.7878290099709,81.2175535848858,
61.2119785531442));
#220493=CARTESIAN_POINT('Ctrl Pts',(-34.8854963962609,76.9566776927288,
59.8160000388975));
#220494=CARTESIAN_POINT('Ctrl Pts',(-34.9831637825509,72.4740036830308,
59.9132271101949));
#220495=CARTESIAN_POINT('Ctrl Pts',(-35.0808311688409,68.2776625886137,
61.4926386461447));
#220496=CARTESIAN_POINT('Ctrl Pts',(-35.1784985551309,64.8433283330666,
64.3752013257362));
#220497=CARTESIAN_POINT('Ctrl Pts',(-35.2761659414209,62.56029797625,68.2341638508804));
#220498=CARTESIAN_POINT('Ctrl Pts',(-35.3738333277109,61.6873631614363,
72.6320956590941));
#220499=CARTESIAN_POINT('Ctrl Pts',(-35.4715007140009,62.3234749316971,
77.0704716229308));
#220500=CARTESIAN_POINT('Ctrl Pts',(-35.5691681002909,64.3965271891681,
81.0461820900504));
#220501=CARTESIAN_POINT('Ctrl Pts',(-35.6668354865809,67.6715302419011,
84.1085625995897));
#220502=CARTESIAN_POINT('Ctrl Pts',(-35.7645028728709,71.7772479303871,
85.9104787028145));
#220503=CARTESIAN_POINT('Ctrl Pts',(-35.8621702591609,76.2482788970921,
86.247675196548));
#220504=CARTESIAN_POINT('Ctrl Pts',(-35.9598376454509,80.5778118998904,
85.081929358769));
#220505=CARTESIAN_POINT('Ctrl Pts',(-36.0575050317409,84.2750751200944,
82.5453836640971));
#220506=CARTESIAN_POINT('Ctrl Pts',(-36.1551724180309,86.9209673304724,
78.9255668466804));
#220507=CARTESIAN_POINT('Ctrl Pts',(-36.2528398043209,88.2155648830812,
74.6328012395938));
#220508=CARTESIAN_POINT('Ctrl Pts',(-36.3505071906109,88.0121193884434,
70.1536909137269));
#220509=CARTESIAN_POINT('Ctrl Pts',(-36.4481745769009,86.333692298055,65.995962942479));
#220510=CARTESIAN_POINT('Ctrl Pts',(-36.5458419631909,83.3705407863494,
62.6309142802354));
#220511=CARTESIAN_POINT('Ctrl Pts',(-36.6435093494809,79.4585512538933,
60.4399881567567));
#220512=CARTESIAN_POINT('Ctrl Pts',(-36.7411767357709,75.0411651102624,
59.6715357908677));
#220513=CARTESIAN_POINT('Ctrl Pts',(-36.8388441220609,70.6191127183272,
60.4126646754531));
#220514=CARTESIAN_POINT('Ctrl Pts',(-36.9365115083509,66.6936533809556,
62.5793645557409));
#220515=CARTESIAN_POINT('Ctrl Pts',(-37.0341788946409,63.7097553700125,
65.9260303652965));
#220516=CARTESIAN_POINT('Ctrl Pts',(-37.1318462809309,62.005656794,70.0733026524509));
#220517=CARTESIAN_POINT('Ctrl Pts',(-37.2295136672209,61.7745248044076,
74.5510696611246));
#220518=CARTESIAN_POINT('Ctrl Pts',(-37.3271810535109,63.0425592400513,
78.8517565888796));
#220519=CARTESIAN_POINT('Ctrl Pts',(-37.4248484398009,65.6660227588901,
82.4878614479098));
#220520=CARTESIAN_POINT('Ctrl Pts',(-37.5225158260909,69.3475341048888,
85.0472155832));
#220521=CARTESIAN_POINT('Ctrl Pts',(-37.6201832123809,73.6697775958153,
86.239704822428));
#220522=CARTESIAN_POINT('Ctrl Pts',(-37.7178505986709,78.142807711568,85.9301552074927));
#220523=CARTESIAN_POINT('Ctrl Pts',(-37.8155179849609,82.2595865975891,
84.1536555637811));
#220524=CARTESIAN_POINT('Ctrl Pts',(-37.9131853712509,85.5534590604176,
81.111580025743));
#220525=CARTESIAN_POINT('Ctrl Pts',(-38.0108527575409,87.6510500090054,
77.1487613832987));
#220526=CARTESIAN_POINT('Ctrl Pts',(-38.1085201438309,88.3145881816426,
72.7144027516668));
#220527=CARTESIAN_POINT('Ctrl Pts',(-38.2061875301209,87.4688585758041,
68.3111584007035));
#220528=CARTESIAN_POINT('Ctrl Pts',(-38.3038549164109,85.2097284031102,
64.4381556582015));
#220529=CARTESIAN_POINT('Ctrl Pts',(-38.4015223027009,81.793280114859,61.534416607706));
#220530=CARTESIAN_POINT('Ctrl Pts',(-38.4991896889909,77.6067833162661,
59.9290929831489));
#220531=CARTESIAN_POINT('Ctrl Pts',(-38.5968570752809,73.124796038894,59.8041553558838));
#220532=CARTESIAN_POINT('Ctrl Pts',(-38.6945244615809,68.8553714613998,
61.1737659619935));
#220533=CARTESIAN_POINT('Ctrl Pts',(-38.7921918478709,65.2824678824627,
63.8826733471558));
#220534=CARTESIAN_POINT('Ctrl Pts',(-38.8898592341609,62.8110896717617,
67.6238108193034));
#220535=CARTESIAN_POINT('Ctrl Pts',(-38.9875266204509,61.7213790587936,
71.9731037866268));
#220536=CARTESIAN_POINT('Ctrl Pts',(-39.0851940067409,62.1368576487401,
76.4375406365595));
#220537=CARTESIAN_POINT('Ctrl Pts',(-39.1828613930309,64.010436330763,80.5110572786137));
#220538=CARTESIAN_POINT('Ctrl Pts',(-39.2805287793209,67.1297096286665,
83.7319036844192));
#220539=CARTESIAN_POINT('Ctrl Pts',(-39.3781961656109,71.1411948124404,
85.7349781226078));
#220540=CARTESIAN_POINT('Ctrl Pts',(-39.4433077564709,74.1069290187816,
86.1071526244663));
#220541=CARTESIAN_POINT('Ctrl Pts',(-39.4758635519009,75.5788379419391,
86.0418804791266));
#220542=CARTESIAN_POINT('Ctrl Pts',(-37.9553013376164,87.0149197239272,
77.9529304850788));
#220543=CARTESIAN_POINT('Ctrl Pts',(-37.9473977182868,86.8780015006863,
78.2843261017427));
#220544=CARTESIAN_POINT('Ctrl Pts',(-37.9394869538629,86.7273493680408,
78.6101129500371));
#220545=CARTESIAN_POINT('Ctrl Pts',(-37.9144970719214,86.2123909976008,
79.6124821634823));
#220546=CARTESIAN_POINT('Ctrl Pts',(-37.8972347154438,85.8016507088589,
80.2630920822533));
#220547=CARTESIAN_POINT('Ctrl Pts',(-37.861062749303,84.8147782119131,81.5567570438918));
#220548=CARTESIAN_POINT('Ctrl Pts',(-37.8423268283133,84.2272138908917,
82.1865390631675));
#220549=CARTESIAN_POINT('Ctrl Pts',(-37.8109352049774,83.1683559811119,
83.1171154920924));
#220550=CARTESIAN_POINT('Ctrl Pts',(-37.7985801514998,82.7322228035195,
83.4538658241038));
#220551=CARTESIAN_POINT('Ctrl Pts',(-37.7691043490261,81.6361366088174,
84.1941557057341));
#220552=CARTESIAN_POINT('Ctrl Pts',(-37.752257135375,80.9589745053308,84.5684803366103));
#220553=CARTESIAN_POINT('Ctrl Pts',(-37.7176808869081,79.5333123286061,
85.19820586662));
#220554=CARTESIAN_POINT('Ctrl Pts',(-37.6999867825758,78.7866758654998,
85.4500052364488));
#220555=CARTESIAN_POINT('Ctrl Pts',(-37.6640158185303,77.2101795397193,
85.8267863844493));
#220556=CARTESIAN_POINT('Ctrl Pts',(-37.6457917771104,76.3816799860254,
85.9421693852411));
#220557=CARTESIAN_POINT('Ctrl Pts',(-37.6179096810754,75.1310310523308,
85.994921893685));
#220558=CARTESIAN_POINT('Ctrl Pts',(-37.6085662507976,74.7136034370356,
85.9924283920031));
#220559=CARTESIAN_POINT('Ctrl Pts',(-37.5800024872725,73.4378254535915,
85.9233392433153));
#220560=CARTESIAN_POINT('Ctrl Pts',(-37.5612098452054,72.5853703586956,
85.7916214301034));
#220561=CARTESIAN_POINT('Ctrl Pts',(-37.5247937388324,70.9944744540827,
85.3811504603076));
#220562=CARTESIAN_POINT('Ctrl Pts',(-37.5072061451635,70.2559520398793,
85.1176307511489));
#220563=CARTESIAN_POINT('Ctrl Pts',(-37.4706993708442,68.7656494933135,
84.4287851334567));
#220564=CARTESIAN_POINT('Ctrl Pts',(-37.4519645638645,68.023333774558,83.9918197602286));
#220565=CARTESIAN_POINT('Ctrl Pts',(-37.4235242747022,66.9920845151175,
83.2381830196114));
#220566=CARTESIAN_POINT('Ctrl Pts',(-37.4141649327465,66.6666862632069,
82.9754108736812));
#220567=CARTESIAN_POINT('Ctrl Pts',(-37.3855787197163,65.7119637817133,
82.1252268095932));
#220568=CARTESIAN_POINT('Ctrl Pts',(-37.3667763651694,65.1278034430708,
81.4906548248999));
#220569=CARTESIAN_POINT('Ctrl Pts',(-37.3288886089769,64.0999456460148,
80.1240580683699));
#220570=CARTESIAN_POINT('Ctrl Pts',(-37.3097662096208,63.6570533065481,
79.3966479349764));
#220571=CARTESIAN_POINT('Ctrl Pts',(-37.272377703877,62.9253191437379,77.877807166774));
#220572=CARTESIAN_POINT('Ctrl Pts',(-37.254105190141,62.6358835506584,77.0910921468174));
#220573=CARTESIAN_POINT('Ctrl Pts',(-37.2261945528014,62.3185864199717,
75.8793905009494));
#220574=CARTESIAN_POINT('Ctrl Pts',(-37.2168704007062,62.2325462548658,
75.4719058965277));
#220575=CARTESIAN_POINT('Ctrl Pts',(-37.1883348797388,62.0290488504922,
74.211526283995));
#220576=CARTESIAN_POINT('Ctrl Pts',(-37.1695527699318,61.976573836333,73.3505341020265));
#220577=CARTESIAN_POINT('Ctrl Pts',(-37.1324546123145,62.0406925031923,
71.6786460362011));
#220578=CARTESIAN_POINT('Ctrl Pts',(-37.1141663102993,62.1479090448059,
70.8713107952548));
#220579=CARTESIAN_POINT('Ctrl Pts',(-37.0776055317186,62.516745874674,69.2651664320858));
#220580=CARTESIAN_POINT('Ctrl Pts',(-37.0593609631848,62.7817337808106,
68.4709556012001));
#220581=CARTESIAN_POINT('Ctrl Pts',(-37.0287563265744,63.3398217425991,
67.215660861289));
#220582=CARTESIAN_POINT('Ctrl Pts',(-37.0166706476576,63.5889203893348,
66.7377147055205));
#220583=CARTESIAN_POINT('Ctrl Pts',(-36.9874851404225,64.265238862123,65.615967360191));
#220584=CARTESIAN_POINT('Ctrl Pts',(-36.9706554575621,64.7215535366351,
64.9921015471903));
#220585=CARTESIAN_POINT('Ctrl Pts',(-36.9368299488605,65.7273512419191,
63.8463945870026));
#220586=CARTESIAN_POINT('Ctrl Pts',(-36.9198965793821,66.2724671296937,
63.3246570379016));
#220587=CARTESIAN_POINT('Ctrl Pts',(-36.8938644179974,67.1856908905406,
62.591225377354));
#220588=CARTESIAN_POINT('Ctrl Pts',(-36.8846757297518,67.5241519284592,
62.3452743724052));
#220589=CARTESIAN_POINT('Ctrl Pts',(-36.8533476324862,68.7122918766856,
61.5665594371299));
#220590=CARTESIAN_POINT('Ctrl Pts',(-36.8309230429486,69.6114607858468,
61.1158732118304));
#220591=CARTESIAN_POINT('Ctrl Pts',(-36.789449487936,71.3612978449459,60.478934483044));
#220592=CARTESIAN_POINT('Ctrl Pts',(-36.7707178993297,72.1963470791442,
60.2657349591826));
#220593=CARTESIAN_POINT('Ctrl Pts',(-36.7386712593778,73.6205739630213,
60.0492377450129));
#220594=CARTESIAN_POINT('Ctrl Pts',(-36.7256353126083,74.2000425611145,
60.0005305295167));
#220595=CARTESIAN_POINT('Ctrl Pts',(-36.6954200029145,75.5551736723792,
59.9776797136377));
#220596=CARTESIAN_POINT('Ctrl Pts',(-36.6785226409056,76.3291455552397,
60.0338452720972));
#220597=CARTESIAN_POINT('Ctrl Pts',(-36.6444393144889,77.8457582702571,
60.2813083747787));
#220598=CARTESIAN_POINT('Ctrl Pts',(-36.627304088817,78.5857589156217,60.4699725631839));
#220599=CARTESIAN_POINT('Ctrl Pts',(-36.5912629985634,80.1156502750462,
61.006890255804));
#220600=CARTESIAN_POINT('Ctrl Pts',(-36.5725265788013,80.8961498629526,
61.3710752105735));
#220601=CARTESIAN_POINT('Ctrl Pts',(-36.5440917128894,81.9941544883828,
62.02274903122));
#220602=CARTESIAN_POINT('Ctrl Pts',(-36.5347393239334,82.342829524566,62.2530948295483));
#220603=CARTESIAN_POINT('Ctrl Pts',(-36.5061627867831,83.3740467851531,
63.0081240833622));
#220604=CARTESIAN_POINT('Ctrl Pts',(-36.4873647837522,84.016106273638,63.5840945893444));
#220605=CARTESIAN_POINT('Ctrl Pts',(-36.4508287270845,85.1283164207911,
64.8011777565554));
#220606=CARTESIAN_POINT('Ctrl Pts',(-36.4331132215764,85.6060584898116,
65.4302567802297));
#220607=CARTESIAN_POINT('Ctrl Pts',(-36.3984301762445,86.4326940815265,
66.7528247587721));
#220608=CARTESIAN_POINT('Ctrl Pts',(-36.3815971455766,86.7824975342673,
67.4420206214496));
#220609=CARTESIAN_POINT('Ctrl Pts',(-36.3484649019024,87.3367234482972,
68.8267002318701));
#220610=CARTESIAN_POINT('Ctrl Pts',(-36.3322686753667,87.5483011039315,
69.5163260239332));
#220611=CARTESIAN_POINT('Ctrl Pts',(-36.3002569422523,87.8552943718372,
70.9245458454455));
#220612=CARTESIAN_POINT('Ctrl Pts',(-36.2845007615987,87.9500046304174,
71.6407444007544));
#220613=CARTESIAN_POINT('Ctrl Pts',(-36.2513677547274,88.0220816726077,
73.1315272035965));
#220614=CARTESIAN_POINT('Ctrl Pts',(-36.2340081542728,87.9906885105661,
73.9037468834361));
#220615=CARTESIAN_POINT('Ctrl Pts',(-36.1994040444401,87.7891197532016,
75.4506851129428));
#220616=CARTESIAN_POINT('Ctrl Pts',(-36.1821713308326,87.6162554705602,
76.2218644197147));
#220617=CARTESIAN_POINT('Ctrl Pts',(-36.1568663165708,87.2678008992854,
77.3042636933753));
#220618=CARTESIAN_POINT('Ctrl Pts',(-36.149081613326,87.1478054025579,77.6312952059185));
#220619=CARTESIAN_POINT('Ctrl Pts',(-36.1412950695185,87.0149197055719,
77.9529305295058));
#220620=CARTESIAN_POINT('',(-32.7070373297029,66.4977334966964,64.749780674319));
#220621=CARTESIAN_POINT('Ctrl Pts',(-26.5424658037409,86.773203990145,73.1405558201253));
#220622=CARTESIAN_POINT('Ctrl Pts',(-26.5750215991709,86.7903065205387,
71.812960950527));
#220623=CARTESIAN_POINT('Ctrl Pts',(-26.6401331900309,86.3710927791314,
69.1522693813868));
#220624=CARTESIAN_POINT('Ctrl Pts',(-26.7378005763209,84.4533116811586,
65.595862444819));
#220625=CARTESIAN_POINT('Ctrl Pts',(-26.8354679626109,81.4639547431525,
62.8775596699702));
#220626=CARTESIAN_POINT('Ctrl Pts',(-26.9331353489009,77.7418800381493,
61.3054018749864));
#220627=CARTESIAN_POINT('Ctrl Pts',(-27.0308027351909,73.7090009717682,
61.0576244908064));
#220628=CARTESIAN_POINT('Ctrl Pts',(-27.1284701214809,69.8224624038905,
62.1623076602057));
#220629=CARTESIAN_POINT('Ctrl Pts',(-27.2261375077709,66.5228207415521,
64.4942323820705));
#220630=CARTESIAN_POINT('Ctrl Pts',(-27.3238048940609,64.1841050462514,
67.789064150928));
#220631=CARTESIAN_POINT('Ctrl Pts',(-27.4214722803509,63.0714191403804,
71.6733192596676));
#220632=CARTESIAN_POINT('Ctrl Pts',(-27.5191396666409,63.3108909197464,
75.7067000853347));
#220633=CARTESIAN_POINT('Ctrl Pts',(-27.6168070529309,64.8753751931555,
79.4320049844844));
#220634=CARTESIAN_POINT('Ctrl Pts',(-27.7144744392209,67.5875307112038,
82.4269540784776));
#220635=CARTESIAN_POINT('Ctrl Pts',(-27.8121418255109,71.139922585341,84.3520565700369));
#220636=CARTESIAN_POINT('Ctrl Pts',(-27.9098092118009,75.129871399649,84.9890935309176));
#220637=CARTESIAN_POINT('Ctrl Pts',(-28.0074765980909,79.1050987132879,
84.2658539888279));
#220638=CARTESIAN_POINT('Ctrl Pts',(-28.1051439843809,82.6149948329797,
82.2643203620044));
#220639=CARTESIAN_POINT('Ctrl Pts',(-28.2028113706709,85.2616974255471,
79.211375387585));
#220640=CARTESIAN_POINT('Ctrl Pts',(-28.3004787569609,86.745190982611,75.4530839544341));
#220641=CARTESIAN_POINT('Ctrl Pts',(-28.3981461432509,86.8973149125801,
71.4154651090891));
#220642=CARTESIAN_POINT('Ctrl Pts',(-28.4958135295409,85.7008252915377,
67.5562009023972));
#220643=CARTESIAN_POINT('Ctrl Pts',(-28.5934809158309,83.2913495386348,
64.3127560937844));
#220644=CARTESIAN_POINT('Ctrl Pts',(-28.6911483021209,79.9420124450654,
62.0527895754545));
#220645=CARTESIAN_POINT('Ctrl Pts',(-28.7888156884109,76.0324762644166,
61.0324786020043));
#220646=CARTESIAN_POINT('Ctrl Pts',(-28.8864830747009,72.005904307922,61.367479959455));
#220647=CARTESIAN_POINT('Ctrl Pts',(-28.9841504609909,68.3187264124431,
63.0198197542422));
#220648=CARTESIAN_POINT('Ctrl Pts',(-29.0818178472809,65.3889005887908,
65.8021979228998));
#220649=CARTESIAN_POINT('Ctrl Pts',(-29.1794852335709,63.5485356226125,
69.399219527172));
#220650=CARTESIAN_POINT('Ctrl Pts',(-29.2771526198609,63.00624506665,73.403146172761));
#220651=CARTESIAN_POINT('Ctrl Pts',(-29.3748200061509,63.823499966919,77.3601149694953));
#220652=CARTESIAN_POINT('Ctrl Pts',(-29.4724873924409,65.9076608462574,
80.8215859081835));
#220653=CARTESIAN_POINT('Ctrl Pts',(-29.5701547787309,69.0224788010218,
83.3951858652539));
#220654=CARTESIAN_POINT('Ctrl Pts',(-29.6678221650209,72.8148753648847,
84.789185841132));
#220655=CARTESIAN_POINT('Ctrl Pts',(-29.7654895513109,76.8549655230795,
84.8455697396331));
#220656=CARTESIAN_POINT('Ctrl Pts',(-29.8631569376009,80.6847870904639,
83.5579461951268));
#220657=CARTESIAN_POINT('Ctrl Pts',(-29.9608243238909,83.8702127616981,
81.0722730622719));
#220658=CARTESIAN_POINT('Ctrl Pts',(-30.0584917101809,86.0501603718022,
77.6703124441068));
#220659=CARTESIAN_POINT('Ctrl Pts',(-30.1561590964709,86.9775231652655,
73.7376917047466));
#220660=CARTESIAN_POINT('Ctrl Pts',(-30.2538264827609,86.5471804455886,
69.720190892803));
#220661=CARTESIAN_POINT('Ctrl Pts',(-30.3514938690509,84.8079134737197,
66.0732115905698));
#220662=CARTESIAN_POINT('Ctrl Pts',(-30.4491612553409,81.956875895195,63.2101551195606));
#220663=CARTESIAN_POINT('Ctrl Pts',(-30.5468286416309,78.3172454977062,
61.4555616623674));
#220664=CARTESIAN_POINT('Ctrl Pts',(-30.6444960279209,74.3015905717297,
61.0083221897942));
#220665=CARTESIAN_POINT('Ctrl Pts',(-30.7421634142109,70.365103460175,61.9191332848712));
#220666=CARTESIAN_POINT('Ctrl Pts',(-30.8398308005009,66.9540024821432,
64.0847504597222));
#220667=CARTESIAN_POINT('Ctrl Pts',(-30.9374981867909,64.4549511021745,
67.2596913773823));
#220668=CARTESIAN_POINT('Ctrl Pts',(-31.0351655730809,63.1512279071195,
71.0840623663198));
#220669=CARTESIAN_POINT('Ctrl Pts',(-31.1328329593709,63.1906157186087,
75.1243539684998));
#220670=CARTESIAN_POINT('Ctrl Pts',(-31.2305003456609,64.5686497530634,
78.9225811642114));
#220671=CARTESIAN_POINT('Ctrl Pts',(-31.3281677319509,67.1291237247518,
82.0481980106354));
#220672=CARTESIAN_POINT('Ctrl Pts',(-31.4258351182409,70.5817965229168,
84.1469019390543));
#220673=CARTESIAN_POINT('Ctrl Pts',(-31.5235025045309,74.5352923323311,
84.980795526557));
#220674=CARTESIAN_POINT('Ctrl Pts',(-31.6211698908209,78.5414648223814,
84.4553532267351));
#220675=CARTESIAN_POINT('Ctrl Pts',(-31.7188372771109,82.1461965263699,
82.630136261015));
#220676=CARTESIAN_POINT('Ctrl Pts',(-31.8165046634009,84.9408750761412,
79.712041088333));
#220677=CARTESIAN_POINT('Ctrl Pts',(-31.9141720496909,86.6087112297139,
76.031846775141));
#220678=CARTESIAN_POINT('Ctrl Pts',(-32.0118394359809,86.9606483455424,
72.0067197036773));
#220679=CARTESIAN_POINT('Ctrl Pts',(-32.1095068222709,85.9567927749161,
68.0929259582382));
#220680=CARTESIAN_POINT('Ctrl Pts',(-32.2071742085609,83.7109360542007,
64.7341113461544));
#220681=CARTESIAN_POINT('Ctrl Pts',(-32.3048415948509,80.4776558675686,
62.3110128795057));
#220682=CARTESIAN_POINT('Ctrl Pts',(-32.4025089811409,76.6234595071886,
61.0982979039962));
#220683=CARTESIAN_POINT('Ctrl Pts',(-32.5001763674309,72.5852350114378,
61.233439177867));
#220684=CARTESIAN_POINT('Ctrl Pts',(-32.5978437537209,68.8207415117928,
62.7010949855073));
#220685=CARTESIAN_POINT('Ctrl Pts',(-32.6955111400109,65.7566696348843,
65.3349852966985));
#220686=CARTESIAN_POINT('Ctrl Pts',(-32.7606227308709,64.4125318335594,
67.6691475357373));
#220687=CARTESIAN_POINT('Ctrl Pts',(-32.7931785263009,63.9531251169506,
68.9148385500207));
#220688=CARTESIAN_POINT('Ctrl Pts',(-26.7665939140209,87.2037143630092,
73.1461018017395));
#220689=CARTESIAN_POINT('Ctrl Pts',(-26.7991497094509,87.2214422810865,
71.7699608131094));
#220690=CARTESIAN_POINT('Ctrl Pts',(-26.8642613003109,86.7868991642302,
69.0119758206587));
#220691=CARTESIAN_POINT('Ctrl Pts',(-26.9619286865909,84.7989906263339,
65.3255218656522));
#220692=CARTESIAN_POINT('Ctrl Pts',(-27.0595960728809,81.7003219690098,
62.5078190003946));
#220693=CARTESIAN_POINT('Ctrl Pts',(-27.1572634591709,77.8421422775993,
60.8781721617227));
#220694=CARTESIAN_POINT('Ctrl Pts',(-27.2549308454609,73.6617930516903,
60.6213343098834));
#220695=CARTESIAN_POINT('Ctrl Pts',(-27.3525982317509,69.6331355526051,
61.766412393317));
#220696=CARTESIAN_POINT('Ctrl Pts',(-27.4502656180409,66.212835999391,64.1836085317264));
#220697=CARTESIAN_POINT('Ctrl Pts',(-27.5479330043309,63.7886005622341,
67.5989223082414));
#220698=CARTESIAN_POINT('Ctrl Pts',(-27.6456003906209,62.6352271065125,
71.6252128490112));
#220699=CARTESIAN_POINT('Ctrl Pts',(-27.7432677769109,62.8834556427626,
75.8060821820242));
#220700=CARTESIAN_POINT('Ctrl Pts',(-27.8409351632009,64.5051483624386,
79.6676101859859));
#220701=CARTESIAN_POINT('Ctrl Pts',(-27.9386025494909,67.3164791843653,
82.7720754874778));
#220702=CARTESIAN_POINT('Ctrl Pts',(-28.0362699357809,70.9987712582735,
84.767573140128));
#220703=CARTESIAN_POINT('Ctrl Pts',(-28.1339373220709,75.1346204029575,
85.4279046111303));
#220704=CARTESIAN_POINT('Ctrl Pts',(-28.2316047083609,79.2552097263266,
84.678218391901));
#220705=CARTESIAN_POINT('Ctrl Pts',(-28.3292720946509,82.8934521049011,
82.6034947491146));
#220706=CARTESIAN_POINT('Ctrl Pts',(-28.4269394809409,85.6369365863143,
79.4389128336909));
#220707=CARTESIAN_POINT('Ctrl Pts',(-28.5246068672309,87.1746770047232,
75.5431920781981));
#220708=CARTESIAN_POINT('Ctrl Pts',(-28.6222742535209,87.3323636455694,
71.3579297539834));
#220709=CARTESIAN_POINT('Ctrl Pts',(-28.7199416398109,86.0921220269066,
67.3575439567694));
#220710=CARTESIAN_POINT('Ctrl Pts',(-28.8176090261009,83.5945390513956,
63.9954962058266));
#220711=CARTESIAN_POINT('Ctrl Pts',(-28.9152764123909,80.1227268557061,
61.6528895642724));
#220712=CARTESIAN_POINT('Ctrl Pts',(-29.0129437986809,76.0702307908808,
60.5952689121648));
#220713=CARTESIAN_POINT('Ctrl Pts',(-29.1106111849709,71.8964193067431,
60.9425202535142));
#220714=CARTESIAN_POINT('Ctrl Pts',(-29.2082785712609,68.0744124953734,
62.6552811046037));
#220715=CARTESIAN_POINT('Ctrl Pts',(-29.3059459575509,65.0374518247561,
65.5394024065494));
#220716=CARTESIAN_POINT('Ctrl Pts',(-29.4036133438509,63.1297902918518,
69.2679561845011));
#220717=CARTESIAN_POINT('Ctrl Pts',(-29.5012807301409,62.5676698145191,
73.4182942873752));
#220718=CARTESIAN_POINT('Ctrl Pts',(-29.5989481164309,63.4148092485251,
77.5199574352399));
#220719=CARTESIAN_POINT('Ctrl Pts',(-29.6966155027209,65.5751815719184,
81.1080038707725));
#220720=CARTESIAN_POINT('Ctrl Pts',(-29.7942828890109,68.8038989749744,
83.7757125749618));
#220721=CARTESIAN_POINT('Ctrl Pts',(-29.8919502753009,72.7349719824068,
85.2206869032595));
#220722=CARTESIAN_POINT('Ctrl Pts',(-29.9896176615909,76.9227959878881,
85.2791325899756));
#220723=CARTESIAN_POINT('Ctrl Pts',(-30.0872850478809,80.8926625177431,
83.9444245566036));
#220724=CARTESIAN_POINT('Ctrl Pts',(-30.1849524341709,84.1945695473749,
81.3678578939925));
#220725=CARTESIAN_POINT('Ctrl Pts',(-30.2826198204609,86.4542312318516,
77.8414978909713));
#220726=CARTESIAN_POINT('Ctrl Pts',(-30.3802872067509,87.4155048708503,
73.7650731351128));
#220727=CARTESIAN_POINT('Ctrl Pts',(-30.4779545930409,86.9694258227422,
69.6006644997807));
#220728=CARTESIAN_POINT('Ctrl Pts',(-30.5756219793309,85.1665591312736,
65.820326222327));
#220729=CARTESIAN_POINT('Ctrl Pts',(-30.6732893656209,82.2112677530227,
62.8525764571268));
#220730=CARTESIAN_POINT('Ctrl Pts',(-30.7709567519109,78.4385471074775,
61.0338228372305));
#220731=CARTESIAN_POINT('Ctrl Pts',(-30.8686241382009,74.2760518565624,
60.5702291732061));
#220732=CARTESIAN_POINT('Ctrl Pts',(-30.9662915244909,70.1956193470026,
61.5143458683933));
#220733=CARTESIAN_POINT('Ctrl Pts',(-31.0639589107809,66.6597847488641,
63.7591530970452));
#220734=CARTESIAN_POINT('Ctrl Pts',(-31.1616262970709,64.0693506371989,
67.0501919774508));
#220735=CARTESIAN_POINT('Ctrl Pts',(-31.2592936833609,62.7179542378677,
71.0144086177314));
#220736=CARTESIAN_POINT('Ctrl Pts',(-31.3569610696509,62.7587823422011,
75.2024414334005));
#220737=CARTESIAN_POINT('Ctrl Pts',(-31.4546284559409,64.1872069030099,
79.1395582812057));
#220738=CARTESIAN_POINT('Ctrl Pts',(-31.5522958422309,66.8413096443314,
82.3794694586463));
#220739=CARTESIAN_POINT('Ctrl Pts',(-31.6499632285209,70.4202362180114,
84.5549166263379));
#220740=CARTESIAN_POINT('Ctrl Pts',(-31.7476306148109,74.5182993819421,
85.4193031739153));
#220741=CARTESIAN_POINT('Ctrl Pts',(-31.8452980011009,78.670965452998,84.8746470423662));
#220742=CARTESIAN_POINT('Ctrl Pts',(-31.9429653873909,82.4075112656457,
82.9826874263801));
#220743=CARTESIAN_POINT('Ctrl Pts',(-32.0406327736809,85.304382736349,79.9578863610725));
#220744=CARTESIAN_POINT('Ctrl Pts',(-32.1383001599709,87.0332066010756,
76.1431185004146));
#220745=CARTESIAN_POINT('Ctrl Pts',(-32.2359675462609,87.3980129901441,
71.970804736377));
#220746=CARTESIAN_POINT('Ctrl Pts',(-32.3336349325509,86.357449465044,67.9138954205205));
#220747=CARTESIAN_POINT('Ctrl Pts',(-32.4313023188409,84.0294685736218,
64.4322591422073));
#220748=CARTESIAN_POINT('Ctrl Pts',(-32.5289697051309,80.6779571340673,
61.9205553116033));
#220749=CARTESIAN_POINT('Ctrl Pts',(-32.6266370914209,76.6828244989406,
60.6634950264663));
#220750=CARTESIAN_POINT('Ctrl Pts',(-32.7243044777109,72.4969343775197,
60.8035780069627));
#220751=CARTESIAN_POINT('Ctrl Pts',(-32.8219718640009,68.5947847647611,
62.3249015374696));
#220752=CARTESIAN_POINT('Ctrl Pts',(-32.9196392502909,65.4186690697612,
65.0551052312264));
#220753=CARTESIAN_POINT('Ctrl Pts',(-32.9847508411509,64.025380224545,67.4746207060263));
#220754=CARTESIAN_POINT('Ctrl Pts',(-33.0173066365809,63.5491743972569,
68.7658628636919));
#220755=CARTESIAN_POINT('Ctrl Pts',(-26.9907220242909,87.6342247358637,
73.1516477833508));
#220756=CARTESIAN_POINT('Ctrl Pts',(-27.0232778197209,87.6525780416251,
71.7269606756879));
#220757=CARTESIAN_POINT('Ctrl Pts',(-27.0883894105809,87.2027055493278,
68.8716822599311));
#220758=CARTESIAN_POINT('Ctrl Pts',(-27.1860567968709,85.1446695715054,
65.0551812864947));
#220759=CARTESIAN_POINT('Ctrl Pts',(-27.2837241831609,81.9366891948709,
62.1380783308097));
#220760=CARTESIAN_POINT('Ctrl Pts',(-27.3813915694509,77.9424045170492,
60.4509424484589));
#220761=CARTESIAN_POINT('Ctrl Pts',(-27.4790589557409,73.6145851316153,
60.1850441289509));
#220762=CARTESIAN_POINT('Ctrl Pts',(-27.5767263420309,69.4438087013183,
61.3705171264289));
#220763=CARTESIAN_POINT('Ctrl Pts',(-27.6743937283209,65.9028512572195,
63.8729846813812));
#220764=CARTESIAN_POINT('Ctrl Pts',(-27.7720611146109,63.3930960782151,
67.4087804655588));
#220765=CARTESIAN_POINT('Ctrl Pts',(-27.8697285009009,62.1990350726515,
71.5771064383641));
#220766=CARTESIAN_POINT('Ctrl Pts',(-27.9673958871909,62.4560203657777,
75.9054642787187));
#220767=CARTESIAN_POINT('Ctrl Pts',(-28.0650632734809,64.1349215317246,
79.9032153874961));
#220768=CARTESIAN_POINT('Ctrl Pts',(-28.1627306597709,67.0454276575313,
83.1171968964906));
#220769=CARTESIAN_POINT('Ctrl Pts',(-28.2603980460609,70.8576199312134,
85.1830897102328));
#220770=CARTESIAN_POINT('Ctrl Pts',(-28.3580654323509,75.139369406275,85.8667156913576));
#220771=CARTESIAN_POINT('Ctrl Pts',(-28.4557328186409,79.4053207393797,
85.0905827949681));
#220772=CARTESIAN_POINT('Ctrl Pts',(-28.5534002049309,83.1719093768379,
82.9426691362138));
#220773=CARTESIAN_POINT('Ctrl Pts',(-28.6510675912209,86.012175747098,79.666450279783));
#220774=CARTESIAN_POINT('Ctrl Pts',(-28.7487349775109,87.6041630268346,
75.6333002019379));
#220775=CARTESIAN_POINT('Ctrl Pts',(-28.8464023638009,87.7674123785483,
71.3003943988506));
#220776=CARTESIAN_POINT('Ctrl Pts',(-28.9440697500909,86.4834187622644,
67.1588870111186));
#220777=CARTESIAN_POINT('Ctrl Pts',(-29.0417371363809,83.8977285641353,
63.6782363178493));
#220778=CARTESIAN_POINT('Ctrl Pts',(-29.1394045226709,80.3034412663224,
61.2529895530694));
#220779=CARTESIAN_POINT('Ctrl Pts',(-29.2370719089609,76.1079853173108,
60.1580592223219));
#220780=CARTESIAN_POINT('Ctrl Pts',(-29.3347392952509,71.7869343055323,
60.5175605475774));
#220781=CARTESIAN_POINT('Ctrl Pts',(-29.4324066815409,67.8300985782672,
62.2907424549827));
#220782=CARTESIAN_POINT('Ctrl Pts',(-29.5300740678309,64.6860030606972,
65.2766068902312));
#220783=CARTESIAN_POINT('Ctrl Pts',(-29.6277414541209,62.7110449610938,
69.1366928418758));
#220784=CARTESIAN_POINT('Ctrl Pts',(-29.7254088404109,62.1290945623912,
73.433442402035));
#220785=CARTESIAN_POINT('Ctrl Pts',(-29.8230762267009,63.0061185301486,
77.6797999010284));
#220786=CARTESIAN_POINT('Ctrl Pts',(-29.9207436129909,65.2427022976115,
81.3944218333965));
#220787=CARTESIAN_POINT('Ctrl Pts',(-30.0184109992809,68.5853191489713,
84.1562392846882));
#220788=CARTESIAN_POINT('Ctrl Pts',(-30.1160783855709,72.6550685999751,
85.6521879654061));
#220789=CARTESIAN_POINT('Ctrl Pts',(-30.2137457718609,76.9906264527469,
85.7126954403172));
#220790=CARTESIAN_POINT('Ctrl Pts',(-30.3114131581509,81.1005379450693,
84.3309029180554));
#220791=CARTESIAN_POINT('Ctrl Pts',(-30.4090805444409,84.5189263330808,
81.6634427256689));
#220792=CARTESIAN_POINT('Ctrl Pts',(-30.5067479307309,86.8583020919226,
78.0126833377833));
#220793=CARTESIAN_POINT('Ctrl Pts',(-30.6044153170209,87.8534865764371,
73.7924545654215));
#220794=CARTESIAN_POINT('Ctrl Pts',(-30.7020827033109,87.3916711998821,
69.4811381067028));
#220795=CARTESIAN_POINT('Ctrl Pts',(-30.7997500896009,85.5252047887965,
65.5674408540281));
#220796=CARTESIAN_POINT('Ctrl Pts',(-30.8974174758909,82.4656596108035,
62.4949977946519));
#220797=CARTESIAN_POINT('Ctrl Pts',(-30.9950848621809,78.5598487171896,
60.61208401208));
#220798=CARTESIAN_POINT('Ctrl Pts',(-31.0927522484709,74.2505131413366,
60.1321361566155));
#220799=CARTESIAN_POINT('Ctrl Pts',(-31.1904196347609,70.026135233775,61.1095584519391));
#220800=CARTESIAN_POINT('Ctrl Pts',(-31.2880870210509,66.3655670155455,
63.4335557344115));
#220801=CARTESIAN_POINT('Ctrl Pts',(-31.3857544073409,63.6837501722009,
66.8406925775739));
#220802=CARTESIAN_POINT('Ctrl Pts',(-31.4834217936309,62.2846805686123,
70.9447548692043));
#220803=CARTESIAN_POINT('Ctrl Pts',(-31.5810891799209,62.3269489658028,
75.2805288983569));
#220804=CARTESIAN_POINT('Ctrl Pts',(-31.6787565662109,63.8057640529833,
79.3565353982501));
#220805=CARTESIAN_POINT('Ctrl Pts',(-31.7764239525009,66.5534955639515,
82.7107409066956));
#220806=CARTESIAN_POINT('Ctrl Pts',(-31.8740913387909,70.2586759131592,
84.9629313136325));
#220807=CARTESIAN_POINT('Ctrl Pts',(-31.9717587250809,74.5013064316051,
85.8578108212735));
#220808=CARTESIAN_POINT('Ctrl Pts',(-32.0694261113709,78.8004660836611,
85.2939408579818));
#220809=CARTESIAN_POINT('Ctrl Pts',(-32.1670934976609,82.668826004946,83.335238591712));
#220810=CARTESIAN_POINT('Ctrl Pts',(-32.2647608839509,85.6678903965729,
80.203731633773));
#220811=CARTESIAN_POINT('Ctrl Pts',(-32.3624282702409,87.4577019724425,
76.2543902256493));
#220812=CARTESIAN_POINT('Ctrl Pts',(-32.4600956565309,87.8353776347299,
71.9348897690367));
#220813=CARTESIAN_POINT('Ctrl Pts',(-32.5577630428209,86.7581061551578,
67.7348648827743));
#220814=CARTESIAN_POINT('Ctrl Pts',(-32.6554304291109,84.3480010930265,
64.1304069382318));
#220815=CARTESIAN_POINT('Ctrl Pts',(-32.7530978154009,80.8782584005449,
61.5300977436922));
#220816=CARTESIAN_POINT('Ctrl Pts',(-32.8507652016909,76.7421894906778,
60.2286921489303));
#220817=CARTESIAN_POINT('Ctrl Pts',(-32.9484325879809,72.4086337435891,
60.373716836065));
#220818=CARTESIAN_POINT('Ctrl Pts',(-33.0460999742709,68.3688280177291,
61.9487080894351));
#220819=CARTESIAN_POINT('Ctrl Pts',(-33.1437673605609,65.0806685046385,
64.7752251657534));
#220820=CARTESIAN_POINT('Ctrl Pts',(-33.2088789514209,63.6382286155421,
67.2800938763135));
#220821=CARTESIAN_POINT('Ctrl Pts',(-33.2414347468509,63.1452236775756,
68.616887177359));
#220822=CARTESIAN_POINT('Ctrl Pts',(-27.2148501345709,88.0647351087276,
73.1571937649659));
#220823=CARTESIAN_POINT('Ctrl Pts',(-27.2474059300009,88.0837138021636,
71.6839605382665));
#220824=CARTESIAN_POINT('Ctrl Pts',(-27.3125175208609,87.6185119344257,
68.7313886992027));
#220825=CARTESIAN_POINT('Ctrl Pts',(-27.4101849071509,85.4903485166769,
64.7848407073372));
#220826=CARTESIAN_POINT('Ctrl Pts',(-27.5078522934409,82.1730564207291,
61.7683376612345));
#220827=CARTESIAN_POINT('Ctrl Pts',(-27.6055196797309,78.0426667564991,
60.0237127351951));
#220828=CARTESIAN_POINT('Ctrl Pts',(-27.7031870660209,73.5673772115374,
59.7487539480279));
#220829=CARTESIAN_POINT('Ctrl Pts',(-27.8008544523109,69.2544818500329,
60.9746218595402));
#220830=CARTESIAN_POINT('Ctrl Pts',(-27.8985218386009,65.5928665150491,
63.5623608310333));
#220831=CARTESIAN_POINT('Ctrl Pts',(-27.9961892248909,62.9975915941978,
67.2186386228722));
#220832=CARTESIAN_POINT('Ctrl Pts',(-28.0938566111809,61.7628430387832,
71.5290000277085));
#220833=CARTESIAN_POINT('Ctrl Pts',(-28.1915239974709,62.0285850887952,
76.0048463754076));
#220834=CARTESIAN_POINT('Ctrl Pts',(-28.2891913837609,63.7646947010089,
80.1388205889948));
#220835=CARTESIAN_POINT('Ctrl Pts',(-28.3868587700509,66.774376130688,83.4623183054996));
#220836=CARTESIAN_POINT('Ctrl Pts',(-28.4845261563409,70.7164686041459,
85.5986062803239));
#220837=CARTESIAN_POINT('Ctrl Pts',(-28.5821935426309,75.1441184095806,
86.3055267715799));
#220838=CARTESIAN_POINT('Ctrl Pts',(-28.6798609289209,79.5554317524179,
85.5029471980399));
#220839=CARTESIAN_POINT('Ctrl Pts',(-28.7775283152109,83.4503666487593,
83.281843523324));
#220840=CARTESIAN_POINT('Ctrl Pts',(-28.8751957015009,86.3874149078648,
79.8939877258898));
#220841=CARTESIAN_POINT('Ctrl Pts',(-28.9728630877909,88.0336490489472,
75.7234083257009));
#220842=CARTESIAN_POINT('Ctrl Pts',(-29.0705304740809,88.2024611115288,
71.2428590437401));
#220843=CARTESIAN_POINT('Ctrl Pts',(-29.1681978603709,86.874715497634,66.960230065489));
#220844=CARTESIAN_POINT('Ctrl Pts',(-29.2658652466609,84.200918076899,63.3609764298819));
#220845=CARTESIAN_POINT('Ctrl Pts',(-29.3635326329509,80.4841556769628,
60.8530895418872));
#220846=CARTESIAN_POINT('Ctrl Pts',(-29.4612000192409,76.1457398437741,
59.720849532482));
#220847=CARTESIAN_POINT('Ctrl Pts',(-29.5588674055309,71.6774493043503,
60.0926008416417));
#220848=CARTESIAN_POINT('Ctrl Pts',(-29.6565347918209,67.5857846611909,
61.9262038053416));
#220849=CARTESIAN_POINT('Ctrl Pts',(-29.7542021781109,64.3345542966621,
65.0138113738816));
#220850=CARTESIAN_POINT('Ctrl Pts',(-29.8518695644009,62.2922996303327,
69.0054294992058));
#220851=CARTESIAN_POINT('Ctrl Pts',(-29.9495369506909,61.6905193102603,
73.4485905166492));
#220852=CARTESIAN_POINT('Ctrl Pts',(-30.0472043369809,62.5974278117552,
77.8396423667743));
#220853=CARTESIAN_POINT('Ctrl Pts',(-30.1448717232709,64.9102230232763,
81.6808397959763));
#220854=CARTESIAN_POINT('Ctrl Pts',(-30.2425391095609,68.3667393229248,
84.5367659943965));
#220855=CARTESIAN_POINT('Ctrl Pts',(-30.3402064958509,72.5751652174933,
86.0836890275428));
#220856=CARTESIAN_POINT('Ctrl Pts',(-30.4378738821409,77.0584569175565,
86.1462582906601));
#220857=CARTESIAN_POINT('Ctrl Pts',(-30.5355412684309,81.3084133723522,
84.7173812795337));
#220858=CARTESIAN_POINT('Ctrl Pts',(-30.6332086547209,84.8432831187579,
81.9590275573887));
#220859=CARTESIAN_POINT('Ctrl Pts',(-30.7308760410109,87.2623729519723,
78.183868784647));
#220860=CARTESIAN_POINT('Ctrl Pts',(-30.8285434273009,88.2914682820311,
73.8198359957915));
#220861=CARTESIAN_POINT('Ctrl Pts',(-30.9262108135909,87.8139165770324,
69.361611713678));
#220862=CARTESIAN_POINT('Ctrl Pts',(-31.0238781998809,85.8838504463503,
65.3145554857853));
#220863=CARTESIAN_POINT('Ctrl Pts',(-31.1215455861709,82.7200514686303,
62.1374191322177));
#220864=CARTESIAN_POINT('Ctrl Pts',(-31.2192129724609,78.6811503269562,
60.190345186952));
#220865=CARTESIAN_POINT('Ctrl Pts',(-31.3168803587509,74.2249744261684,
59.694043140027));
#220866=CARTESIAN_POINT('Ctrl Pts',(-31.4145477450409,69.8566511206013,
60.7047710354618));
#220867=CARTESIAN_POINT('Ctrl Pts',(-31.5122151313309,66.0713492822661,
63.1079583717355));
#220868=CARTESIAN_POINT('Ctrl Pts',(-31.6098825176209,63.2981497072342,
66.6311931776472));
#220869=CARTESIAN_POINT('Ctrl Pts',(-31.7075499039109,61.8514068993598,
70.8751011206178));
#220870=CARTESIAN_POINT('Ctrl Pts',(-31.8052172902009,61.8951155893856,
75.3586163632547));
#220871=CARTESIAN_POINT('Ctrl Pts',(-31.9028846764909,63.424321202929,79.5735125152463));
#220872=CARTESIAN_POINT('Ctrl Pts',(-32.0005520627809,66.2656814835311,
83.0420123547065));
#220873=CARTESIAN_POINT('Ctrl Pts',(-32.0982194490709,70.0971156082545,
85.3709460009164));
#220874=CARTESIAN_POINT('Ctrl Pts',(-32.1958868353609,74.4843134812133,
86.2963184686414));
#220875=CARTESIAN_POINT('Ctrl Pts',(-32.2935542216509,78.9299667142801,
85.7132346736073));
#220876=CARTESIAN_POINT('Ctrl Pts',(-32.3912216079409,82.9301407442222,
83.6877897570762));
#220877=CARTESIAN_POINT('Ctrl Pts',(-32.4888889942309,86.0313980567812,
80.4495769065115));
#220878=CARTESIAN_POINT('Ctrl Pts',(-32.5865563805209,87.8821973438042,
76.3656619509229));
#220879=CARTESIAN_POINT('Ctrl Pts',(-32.6842237668109,88.2727422793224,
71.8989748017326));
#220880=CARTESIAN_POINT('Ctrl Pts',(-32.7818911531009,87.1587628452857,
67.5558343450567));
#220881=CARTESIAN_POINT('Ctrl Pts',(-32.8795585393909,84.6665336124505,
63.8285547342752));
#220882=CARTESIAN_POINT('Ctrl Pts',(-32.9772259256809,81.0785596670429,
61.1396401757895));
#220883=CARTESIAN_POINT('Ctrl Pts',(-33.0748933119709,76.8015544824298,
59.7938892714004));
#220884=CARTESIAN_POINT('Ctrl Pts',(-33.1725606982609,72.3203331096696,
59.9438556651612));
#220885=CARTESIAN_POINT('Ctrl Pts',(-33.2702280845509,68.1428712706964,
61.572514641397));
#220886=CARTESIAN_POINT('Ctrl Pts',(-33.3678954708409,64.7426679395154,
64.4953451002813));
#220887=CARTESIAN_POINT('Ctrl Pts',(-33.4330070617009,63.2510770065369,
67.0855670466063));
#220888=CARTESIAN_POINT('Ctrl Pts',(-33.4655628571309,62.7412729578912,
68.4679114910339));
#220889=CARTESIAN_POINT('',(-26.6970235948769,85.8892179113949,68.3402936518988));
#220890=CARTESIAN_POINT('Ctrl Pts',(-22.3657263431209,71.0427934340047,
84.0781567697158));
#220891=CARTESIAN_POINT('Ctrl Pts',(-22.4113638359009,72.7957341079248,
84.7036938863735));
#220892=CARTESIAN_POINT('Ctrl Pts',(-22.5026388214709,76.6021092212285,
85.1071590883939));
#220893=CARTESIAN_POINT('Ctrl Pts',(-22.6395512998309,81.9594314524499,
83.0382494769743));
#220894=CARTESIAN_POINT('Ctrl Pts',(-22.7764637781809,85.7803921824825,
78.7512421293735));
#220895=CARTESIAN_POINT('Ctrl Pts',(-22.9133762565409,87.2221381590131,
73.1924757376221));
#220896=CARTESIAN_POINT('Ctrl Pts',(-23.0502887348909,85.9663418720247,
67.5887670194206));
#220897=CARTESIAN_POINT('Ctrl Pts',(-23.1872012132509,82.2901999352476,
63.1769076868418));
#220898=CARTESIAN_POINT('Ctrl Pts',(-23.3241136916009,77.0050551559994,
60.9306245140911));
#220899=CARTESIAN_POINT('Ctrl Pts',(-23.4610261699609,71.2773803974512,
61.3456896355517));
#220900=CARTESIAN_POINT('Ctrl Pts',(-23.5979386483109,66.3713151444493,
64.3304948862029));
#220901=CARTESIAN_POINT('Ctrl Pts',(-23.7348511266709,63.3696644032273,
69.226271763487));
#220902=CARTESIAN_POINT('Ctrl Pts',(-23.8717636050209,62.9349146157014,
74.9524861359762));
#220903=CARTESIAN_POINT('Ctrl Pts',(-24.0086760833809,65.16301828311,80.2453202044371));
#220904=CARTESIAN_POINT('Ctrl Pts',(-24.1455885617309,69.5622164668703,
83.9366063979647));
#220905=CARTESIAN_POINT('Ctrl Pts',(-24.2825010400909,75.1615736379323,
85.211650591567));
#220906=CARTESIAN_POINT('Ctrl Pts',(-24.4194135184409,80.7252703137354,
83.7890411146378));
#220907=CARTESIAN_POINT('Ctrl Pts',(-24.5563259967909,85.0253575466822,
79.9827583856074));
#220908=CARTESIAN_POINT('Ctrl Pts',(-24.6932384751509,87.1127743256804,
74.6328771144894));
#220909=CARTESIAN_POINT('Ctrl Pts',(-24.8301509535009,86.5268123507618,
68.9201556099781));
#220910=CARTESIAN_POINT('Ctrl Pts',(-24.9670634318609,83.3967977574361,
64.1054337000071));
#220911=CARTESIAN_POINT('Ctrl Pts',(-25.1039759102109,78.4135478836825,
61.251356069971));
#220912=CARTESIAN_POINT('Ctrl Pts',(-25.2408883885709,72.6769027803898,
60.9878387312059));
#220913=CARTESIAN_POINT('Ctrl Pts',(-25.3778008669209,67.4529823927194,
63.37304190929));
#220914=CARTESIAN_POINT('Ctrl Pts',(-25.5147133452809,63.8947445237484,
67.8805336366522));
#220915=CARTESIAN_POINT('Ctrl Pts',(-25.6516258236309,62.787518582008,73.5154772357479));
#220916=CARTESIAN_POINT('Ctrl Pts',(-25.7885383019909,64.3756773943421,
79.034198897657));
#220917=CARTESIAN_POINT('Ctrl Pts',(-25.9254507803409,68.3087030144427,
83.2186765115834));
#220918=CARTESIAN_POINT('Ctrl Pts',(-26.0623632587009,73.7185460237825,
85.1453630258059));
#220919=CARTESIAN_POINT('Ctrl Pts',(-26.1992757370509,79.4112201475916,
84.3890317273548));
#220920=CARTESIAN_POINT('Ctrl Pts',(-26.3361882154009,84.1302876496623,
81.116583535284));
#220921=CARTESIAN_POINT('Ctrl Pts',(-26.4731006937609,86.8342994995147,
76.0503726420501));
#220922=CARTESIAN_POINT('Ctrl Pts',(-26.6100131721109,86.9261467426327,
70.3081733636108));
#220923=CARTESIAN_POINT('Ctrl Pts',(-26.7012881576809,85.2332010925808,
66.8752138971438));
#220924=CARTESIAN_POINT('Ctrl Pts',(-26.7469256504709,84.0408674757396,
65.446074912737));
#220925=CARTESIAN_POINT('Ctrl Pts',(-22.5898544533909,70.8980903883704,
84.4836576545961));
#220926=CARTESIAN_POINT('Ctrl Pts',(-22.6354919461809,72.7151307877147,
85.1320687669442));
#220927=CARTESIAN_POINT('Ctrl Pts',(-22.7267669317509,76.660693497755,85.5502874680715));
#220928=CARTESIAN_POINT('Ctrl Pts',(-22.8636794101009,82.2139167592551,
83.405724105221));
#220929=CARTESIAN_POINT('Ctrl Pts',(-23.0005918884609,86.1745984378018,
78.9619538973823));
#220930=CARTESIAN_POINT('Ctrl Pts',(-23.1375043668109,87.6690646932333,
73.1999202731972));
#220931=CARTESIAN_POINT('Ctrl Pts',(-23.2744168451709,86.3673477436804,
67.3913009179511));
#220932=CARTESIAN_POINT('Ctrl Pts',(-23.4113293235209,82.5567804425581,
62.8181132666061));
#220933=CARTESIAN_POINT('Ctrl Pts',(-23.5482418018809,77.078373943613,60.4896903290828));
#220934=CARTESIAN_POINT('Ctrl Pts',(-23.6851542802309,71.1412554857959,
60.9199331235346));
#220935=CARTESIAN_POINT('Ctrl Pts',(-23.8220667585909,66.0557903019732,
64.0138836520906));
#220936=CARTESIAN_POINT('Ctrl Pts',(-23.9589792369409,62.9443782943297,
69.088684245488));
#220937=CARTESIAN_POINT('Ctrl Pts',(-24.0958917153009,62.493731025262,75.0242889153554));
#220938=CARTESIAN_POINT('Ctrl Pts',(-24.2328041936509,64.8033096880395,
80.5106658775062));
#220939=CARTESIAN_POINT('Ctrl Pts',(-24.3697166720109,69.3633732107457,
84.3369312149315));
#220940=CARTESIAN_POINT('Ctrl Pts',(-24.5066291503609,75.1674818959678,
85.6585999086832));
#220941=CARTESIAN_POINT('Ctrl Pts',(-24.6435416287209,80.9346260897404,
84.1839699166284));
#220942=CARTESIAN_POINT('Ctrl Pts',(-24.7804541070709,85.3919544746771,
80.2385029690767));
#220943=CARTESIAN_POINT('Ctrl Pts',(-24.9173665854309,87.5557017561136,
74.6929927610359));
#220944=CARTESIAN_POINT('Ctrl Pts',(-25.0542790637809,86.9483129284454,
68.7713743524177));
#220945=CARTESIAN_POINT('Ctrl Pts',(-25.1911915421409,83.7038431918362,
63.7805926607207));
#220946=CARTESIAN_POINT('Ctrl Pts',(-25.3281040204909,78.5383709797127,
60.8221500654867));
#220947=CARTESIAN_POINT('Ctrl Pts',(-25.4650164988409,72.591954158844,60.5489966966418));
#220948=CARTESIAN_POINT('Ctrl Pts',(-25.6019289772009,67.177010841838,63.021419522869));
#220949=CARTESIAN_POINT('Ctrl Pts',(-25.7388414555509,63.4886590027825,
67.6937365557131));
#220950=CARTESIAN_POINT('Ctrl Pts',(-25.8757539339109,62.3409451655286,
73.5347329567422));
#220951=CARTESIAN_POINT('Ctrl Pts',(-26.0126664122609,63.9871781302336,
79.2552575367331));
#220952=CARTESIAN_POINT('Ctrl Pts',(-26.1495788906209,68.0640225720935,
83.5927488094103));
#220953=CARTESIAN_POINT('Ctrl Pts',(-26.2864913689709,73.671687137312,85.5898884076403));
#220954=CARTESIAN_POINT('Ctrl Pts',(-26.4234038473309,79.5725250933031,
84.8059003668432));
#220955=CARTESIAN_POINT('Ctrl Pts',(-26.5603163256809,84.4641545854305,
81.4137886666481));
#220956=CARTESIAN_POINT('Ctrl Pts',(-26.6972288040409,87.26704394991,76.1623218021049));
#220957=CARTESIAN_POINT('Ctrl Pts',(-26.8341412823909,87.3622497682239,
70.2101477067447));
#220958=CARTESIAN_POINT('Ctrl Pts',(-26.9254162679609,85.6073982288574,
66.6516553215257));
#220959=CARTESIAN_POINT('Ctrl Pts',(-26.9710537607409,84.3714645868736,
65.1702570576971));
#220960=CARTESIAN_POINT('Ctrl Pts',(-22.8139825636709,70.7533873427582,
84.8891585394854));
#220961=CARTESIAN_POINT('Ctrl Pts',(-22.8596200564509,72.6345274675306,
85.5604436475148));
#220962=CARTESIAN_POINT('Ctrl Pts',(-22.9508950420209,76.7192777743104,
85.9934158477393));
#220963=CARTESIAN_POINT('Ctrl Pts',(-23.0878075203809,82.4684020660794,
83.7731987334476));
#220964=CARTESIAN_POINT('Ctrl Pts',(-23.2247199987309,86.5688046931341,
79.1726656653597));
#220965=CARTESIAN_POINT('Ctrl Pts',(-23.3616324770909,88.1159912274573,
73.207364808737));
#220966=CARTESIAN_POINT('Ctrl Pts',(-23.4985449554409,86.7683536153187,
67.1938348164451));
#220967=CARTESIAN_POINT('Ctrl Pts',(-23.6354574338009,82.8233609498366,
62.4593188463356));
#220968=CARTESIAN_POINT('Ctrl Pts',(-23.7723699121509,77.1516927311802,
60.0487561440661));
#220969=CARTESIAN_POINT('Ctrl Pts',(-23.9092823905109,71.0051305740928,
60.4941766115334));
#220970=CARTESIAN_POINT('Ctrl Pts',(-24.0461948688609,65.7402654594603,
63.697272418015));
#220971=CARTESIAN_POINT('Ctrl Pts',(-24.1831073472209,62.5190921854207,
68.9510967275429));
#220972=CARTESIAN_POINT('Ctrl Pts',(-24.3200198255709,62.0525474348232,
75.0960916947856));
#220973=CARTESIAN_POINT('Ctrl Pts',(-24.4569323039309,64.4436010930036,
80.776011550622));
#220974=CARTESIAN_POINT('Ctrl Pts',(-24.5938447822809,69.164529954672,84.7372560319302));
#220975=CARTESIAN_POINT('Ctrl Pts',(-24.7307572606409,75.1733901540581,
86.1055492258112));
#220976=CARTESIAN_POINT('Ctrl Pts',(-24.8676697389909,81.1439818658025,
84.5788987185907));
#220977=CARTESIAN_POINT('Ctrl Pts',(-25.0045822173509,85.7585514027134,
80.4942475524982));
#220978=CARTESIAN_POINT('Ctrl Pts',(-25.1414946957009,87.9986291865511,
74.7531084075193));
#220979=CARTESIAN_POINT('Ctrl Pts',(-25.2784071740609,87.3698135061078,
68.6225930947988));
#220980=CARTESIAN_POINT('Ctrl Pts',(-25.4153196524109,84.0108886261921,
63.4557516213944));
#220981=CARTESIAN_POINT('Ctrl Pts',(-25.5522321307709,78.6631940756854,
60.3929440609894));
#220982=CARTESIAN_POINT('Ctrl Pts',(-25.6891446091209,72.5070055372434,
60.1101546620874));
#220983=CARTESIAN_POINT('Ctrl Pts',(-25.8260570874809,66.9010392909102,
62.6697971364818));
#220984=CARTESIAN_POINT('Ctrl Pts',(-25.9629695658309,63.0825734817967,
67.5069394748224));
#220985=CARTESIAN_POINT('Ctrl Pts',(-26.0998820441809,61.8943717490509,
73.5539886777849));
#220986=CARTESIAN_POINT('Ctrl Pts',(-26.2367945225409,63.5986788661504,
79.4763161758423));
#220987=CARTESIAN_POINT('Ctrl Pts',(-26.3737070008909,67.8193421297727,
83.9668211072706));
#220988=CARTESIAN_POINT('Ctrl Pts',(-26.5106194792509,73.6248282508795,
86.0344137894687));
#220989=CARTESIAN_POINT('Ctrl Pts',(-26.6475319576009,79.7338300390394,
85.2227690063213));
#220990=CARTESIAN_POINT('Ctrl Pts',(-26.7844444359609,84.7980215212156,
81.7109937979974));
#220991=CARTESIAN_POINT('Ctrl Pts',(-26.9213569143109,87.6997884003007,
76.2742709621448));
#220992=CARTESIAN_POINT('Ctrl Pts',(-27.0582693926709,87.7983527938067,
70.1121220498729));
#220993=CARTESIAN_POINT('Ctrl Pts',(-27.1495443782409,85.9815953651354,
66.4280967459094));
#220994=CARTESIAN_POINT('Ctrl Pts',(-27.1951818710209,84.7020616980161,
64.8944392026497));
#220995=CARTESIAN_POINT('Ctrl Pts',(-23.0381106739509,70.608684297128,85.2946594243566));
#220996=CARTESIAN_POINT('Ctrl Pts',(-23.0837481667309,72.5539241473244,
85.9888185280762));
#220997=CARTESIAN_POINT('Ctrl Pts',(-23.1750231523009,76.7778620508368,
86.4365442274169));
#220998=CARTESIAN_POINT('Ctrl Pts',(-23.3119356306609,82.7228873728753,
84.1406733616905));
#220999=CARTESIAN_POINT('Ctrl Pts',(-23.4488481090109,86.9630109484534,
79.3833774333685));
#221000=CARTESIAN_POINT('Ctrl Pts',(-23.5857605873609,88.5629177616779,
73.2148093443111));
#221001=CARTESIAN_POINT('Ctrl Pts',(-23.7226730657209,87.169359486974,66.9963687149764));
#221002=CARTESIAN_POINT('Ctrl Pts',(-23.8595855440709,83.0899414571462,
62.1005244260996));
#221003=CARTESIAN_POINT('Ctrl Pts',(-23.9964980224309,77.225011518789,59.6078219590666));
#221004=CARTESIAN_POINT('Ctrl Pts',(-24.1334105007809,70.8690056624368,
60.0684200995182));
#221005=CARTESIAN_POINT('Ctrl Pts',(-24.2703229791409,65.4247406169838,
63.3806611839035));
#221006=CARTESIAN_POINT('Ctrl Pts',(-24.4072354574909,62.0938060765228,
68.8135092095446));
#221007=CARTESIAN_POINT('Ctrl Pts',(-24.5441479358509,61.6113638443835,
75.1678944741657));
#221008=CARTESIAN_POINT('Ctrl Pts',(-24.6810604142009,64.0838924979292,
81.0413572237003));
#221009=CARTESIAN_POINT('Ctrl Pts',(-24.8179728925609,68.9656866985482,
85.1375808488973));
#221010=CARTESIAN_POINT('Ctrl Pts',(-24.9548853709109,75.1792984120937,
86.5524985429274));
#221011=CARTESIAN_POINT('Ctrl Pts',(-25.0917978492709,81.3533376418032,
84.9738275205784));
#221012=CARTESIAN_POINT('Ctrl Pts',(-25.2287103276209,86.1251483307086,
80.7499921359666));
#221013=CARTESIAN_POINT('Ctrl Pts',(-25.3656228059809,88.4415566169843,
74.8132240540658));
#221014=CARTESIAN_POINT('Ctrl Pts',(-25.5025352843309,87.7913140837909,
68.4738118372372));
#221015=CARTESIAN_POINT('Ctrl Pts',(-25.6394477626909,84.3179340605874,
63.1309105821169));
#221016=CARTESIAN_POINT('Ctrl Pts',(-25.7763602410409,78.7880171717146,
59.9637380565047));
#221017=CARTESIAN_POINT('Ctrl Pts',(-25.9132727194009,72.4220569156967,
59.6713126275229));
#221018=CARTESIAN_POINT('Ctrl Pts',(-26.0501851977509,66.6250677400192,
62.3181747500578));
#221019=CARTESIAN_POINT('Ctrl Pts',(-26.1870976761109,62.6764879608306,
67.320142393884));
#221020=CARTESIAN_POINT('Ctrl Pts',(-26.3240101544609,61.4477983325716,
73.5732443987792));
#221021=CARTESIAN_POINT('Ctrl Pts',(-26.4609226328209,63.2101796020395,
79.6973748149271));
#221022=CARTESIAN_POINT('Ctrl Pts',(-26.5978351111709,67.5746616874234,
84.3408934050975));
#221023=CARTESIAN_POINT('Ctrl Pts',(-26.7347475895209,73.5779693644099,
86.4789391713035));
#221024=CARTESIAN_POINT('Ctrl Pts',(-26.8716600678809,79.8951349847512,
85.6396376458088));
#221025=CARTESIAN_POINT('Ctrl Pts',(-27.0085725462309,85.1318884569838,
82.0081989293615));
#221026=CARTESIAN_POINT('Ctrl Pts',(-27.1454850245909,88.1325328506964,
76.3862201221988));
#221027=CARTESIAN_POINT('Ctrl Pts',(-27.2823975029409,88.2344558193887,
70.0140963930029));
#221028=CARTESIAN_POINT('Ctrl Pts',(-27.3736724885109,86.3557925014101,
66.2045381702959));
#221029=CARTESIAN_POINT('Ctrl Pts',(-27.4193099813009,85.032658809151,64.6186213476101));
#221030=CARTESIAN_POINT('',(-22.5674166601918,77.7863349909178,84.4952548267707));
#221031=CARTESIAN_POINT('Ctrl Pts',(-22.5675364832709,77.7863942292111,
84.4954770366417));
#221032=CARTESIAN_POINT('Ctrl Pts',(-22.5675364832709,77.2378487361899,
84.6563729599099));
#221033=CARTESIAN_POINT('Ctrl Pts',(-22.5675364832727,76.6778394979494,
84.7774848925877));
#221034=CARTESIAN_POINT('Ctrl Pts',(-22.5675364832727,75.5395172400914,
84.936908357079));
#221035=CARTESIAN_POINT('Ctrl Pts',(-22.5675364832709,74.9641682946092,
84.9749462493134));
#221036=CARTESIAN_POINT('Ctrl Pts',(-22.5675364832709,74.3890417160681,
84.9719151100471));
#221037=CARTESIAN_POINT('Ctrl Pts',(-22.5674166601918,77.7862809883271,
84.4950313516973));
#221038=CARTESIAN_POINT('Ctrl Pts',(-22.5674566012175,77.7893705430951,
84.4942847630104));
#221039=CARTESIAN_POINT('Ctrl Pts',(-22.5674965422431,77.7924597972905,
84.4935369402494));
#221040=CARTESIAN_POINT('Ctrl Pts',(-22.5675364832687,77.7955487498965,
84.4927878836051));
#221041=CARTESIAN_POINT('Origin',(-21.6548258024609,75.,72.9888893865801));
#221042=CARTESIAN_POINT('Ctrl Pts',(-25.6386080251009,88.0647351087276,
73.1571937649659));
#221043=CARTESIAN_POINT('Ctrl Pts',(-25.6711638205309,88.0837138021636,
71.6839605382665));
#221044=CARTESIAN_POINT('Ctrl Pts',(-25.7362754113909,87.6185119344257,
68.7313886992027));
#221045=CARTESIAN_POINT('Ctrl Pts',(-25.8339427976809,85.4903485166769,
64.7848407073372));
#221046=CARTESIAN_POINT('Ctrl Pts',(-25.9316101839709,82.1730564207291,
61.7683376612345));
#221047=CARTESIAN_POINT('Ctrl Pts',(-26.0292775702609,78.0426667564991,
60.0237127351951));
#221048=CARTESIAN_POINT('Ctrl Pts',(-26.1269449565509,73.5673772115374,
59.7487539480279));
#221049=CARTESIAN_POINT('Ctrl Pts',(-26.2246123428409,69.2544818500329,
60.9746218595402));
#221050=CARTESIAN_POINT('Ctrl Pts',(-26.3222797291309,65.5928665150491,
63.5623608310333));
#221051=CARTESIAN_POINT('Ctrl Pts',(-26.4199471154209,62.9975915941978,
67.2186386228722));
#221052=CARTESIAN_POINT('Ctrl Pts',(-26.5176145017109,61.7628430387832,
71.5290000277085));
#221053=CARTESIAN_POINT('Ctrl Pts',(-26.6152818880009,62.0285850887952,
76.0048463754076));
#221054=CARTESIAN_POINT('Ctrl Pts',(-26.7129492742909,63.7646947010089,
80.1388205889948));
#221055=CARTESIAN_POINT('Ctrl Pts',(-26.8106166605809,66.774376130688,83.4623183054996));
#221056=CARTESIAN_POINT('Ctrl Pts',(-26.9082840468709,70.7164686041459,
85.5986062803239));
#221057=CARTESIAN_POINT('Ctrl Pts',(-27.0059514331609,75.1441184095806,
86.3055267715799));
#221058=CARTESIAN_POINT('Ctrl Pts',(-27.1036188194509,79.5554317524179,
85.5029471980399));
#221059=CARTESIAN_POINT('Ctrl Pts',(-27.2012862057409,83.4503666487593,
83.281843523324));
#221060=CARTESIAN_POINT('Ctrl Pts',(-27.2989535920309,86.3874149078648,
79.8939877258898));
#221061=CARTESIAN_POINT('Ctrl Pts',(-27.3966209783209,88.0336490489472,
75.7234083257009));
#221062=CARTESIAN_POINT('Ctrl Pts',(-27.4942883646109,88.2024611115288,
71.2428590437401));
#221063=CARTESIAN_POINT('Ctrl Pts',(-27.5919557509009,86.874715497634,66.960230065489));
#221064=CARTESIAN_POINT('Ctrl Pts',(-27.6896231371909,84.200918076899,63.3609764298819));
#221065=CARTESIAN_POINT('Ctrl Pts',(-27.7872905234809,80.4841556769628,
60.8530895418872));
#221066=CARTESIAN_POINT('Ctrl Pts',(-27.8849579097709,76.1457398437741,
59.720849532482));
#221067=CARTESIAN_POINT('Ctrl Pts',(-27.9826252960609,71.6774493043503,
60.0926008416417));
#221068=CARTESIAN_POINT('Ctrl Pts',(-28.0802926823509,67.5857846611909,
61.9262038053416));
#221069=CARTESIAN_POINT('Ctrl Pts',(-28.1779600686409,64.3345542966621,
65.0138113738816));
#221070=CARTESIAN_POINT('Ctrl Pts',(-28.2756274549309,62.2922996303327,
69.0054294992058));
#221071=CARTESIAN_POINT('Ctrl Pts',(-28.3732948412209,61.6905193102603,
73.4485905166492));
#221072=CARTESIAN_POINT('Ctrl Pts',(-28.4709622275109,62.5974278117552,
77.8396423667743));
#221073=CARTESIAN_POINT('Ctrl Pts',(-28.5686296138009,64.9102230232763,
81.6808397959763));
#221074=CARTESIAN_POINT('Ctrl Pts',(-28.6662970000909,68.3667393229248,
84.5367659943965));
#221075=CARTESIAN_POINT('Ctrl Pts',(-28.7639643863809,72.5751652174933,
86.0836890275428));
#221076=CARTESIAN_POINT('Ctrl Pts',(-28.8616317726709,77.0584569175565,
86.1462582906601));
#221077=CARTESIAN_POINT('Ctrl Pts',(-28.9592991589609,81.3084133723522,
84.7173812795337));
#221078=CARTESIAN_POINT('Ctrl Pts',(-29.0569665452509,84.8432831187579,
81.9590275573887));
#221079=CARTESIAN_POINT('Ctrl Pts',(-29.1546339315409,87.2623729519723,
78.183868784647));
#221080=CARTESIAN_POINT('Ctrl Pts',(-29.2523013178309,88.2914682820311,
73.8198359957915));
#221081=CARTESIAN_POINT('Ctrl Pts',(-29.3499687041209,87.8139165770324,
69.361611713678));
#221082=CARTESIAN_POINT('Ctrl Pts',(-29.4476360904109,85.8838504463503,
65.3145554857853));
#221083=CARTESIAN_POINT('Ctrl Pts',(-29.5453034767009,82.7200514686303,
62.1374191322177));
#221084=CARTESIAN_POINT('Ctrl Pts',(-29.6429708629909,78.6811503269562,
60.190345186952));
#221085=CARTESIAN_POINT('Ctrl Pts',(-29.7406382492809,74.2249744261684,
59.694043140027));
#221086=CARTESIAN_POINT('Ctrl Pts',(-29.8383056355709,69.8566511206013,
60.7047710354618));
#221087=CARTESIAN_POINT('Ctrl Pts',(-29.9359730218609,66.0713492822661,
63.1079583717355));
#221088=CARTESIAN_POINT('Ctrl Pts',(-30.0336404081509,63.2981497072342,
66.6311931776472));
#221089=CARTESIAN_POINT('Ctrl Pts',(-30.1313077944409,61.8514068993598,
70.8751011206178));
#221090=CARTESIAN_POINT('Ctrl Pts',(-30.2289751807309,61.8951155893856,
75.3586163632547));
#221091=CARTESIAN_POINT('Ctrl Pts',(-30.3266425670209,63.424321202929,79.5735125152463));
#221092=CARTESIAN_POINT('Ctrl Pts',(-30.4243099533109,66.2656814835311,
83.0420123547065));
#221093=CARTESIAN_POINT('Ctrl Pts',(-30.5219773396009,70.0971156082545,
85.3709460009164));
#221094=CARTESIAN_POINT('Ctrl Pts',(-30.6196447258909,74.4843134812133,
86.2963184686414));
#221095=CARTESIAN_POINT('Ctrl Pts',(-30.7173121121809,78.9299667142801,
85.7132346736073));
#221096=CARTESIAN_POINT('Ctrl Pts',(-30.8149794984709,82.9301407442222,
83.6877897570762));
#221097=CARTESIAN_POINT('Ctrl Pts',(-30.9126468847609,86.0313980567812,
80.4495769065115));
#221098=CARTESIAN_POINT('Ctrl Pts',(-31.0103142710509,87.8821973438046,
76.3656619509219));
#221099=CARTESIAN_POINT('Ctrl Pts',(-31.1079816573409,88.2727422793224,
71.8989748017326));
#221100=CARTESIAN_POINT('Ctrl Pts',(-31.2056490436309,87.1587628452857,
67.5558343450567));
#221101=CARTESIAN_POINT('Ctrl Pts',(-31.3033164299209,84.6665336124505,
63.8285547342752));
#221102=CARTESIAN_POINT('Ctrl Pts',(-31.4009838162109,81.0785596670429,
61.1396401757895));
#221103=CARTESIAN_POINT('Ctrl Pts',(-31.4986512025009,76.8015544824298,
59.7938892714004));
#221104=CARTESIAN_POINT('Ctrl Pts',(-31.5963185887909,72.3203331096696,
59.9438556651612));
#221105=CARTESIAN_POINT('Ctrl Pts',(-31.6939859750809,68.1428712706964,
61.572514641397));
#221106=CARTESIAN_POINT('Ctrl Pts',(-31.7916533613709,64.7426679395154,
64.4953451002813));
#221107=CARTESIAN_POINT('Ctrl Pts',(-31.8567649522309,63.2510770065369,
67.0855670466063));
#221108=CARTESIAN_POINT('Ctrl Pts',(-31.8893207476609,62.7412729578912,
68.4679114910339));
#221109=CARTESIAN_POINT('Ctrl Pts',(-25.8627361353809,87.6342247358637,
73.1516477833508));
#221110=CARTESIAN_POINT('Ctrl Pts',(-25.8952919308109,87.6525780416251,
71.7269606756879));
#221111=CARTESIAN_POINT('Ctrl Pts',(-25.9604035216709,87.2027055493278,
68.8716822599311));
#221112=CARTESIAN_POINT('Ctrl Pts',(-26.0580709079509,85.1446695715054,
65.0551812864947));
#221113=CARTESIAN_POINT('Ctrl Pts',(-26.1557382942409,81.9366891948709,
62.1380783308097));
#221114=CARTESIAN_POINT('Ctrl Pts',(-26.2534056805309,77.9424045170492,
60.4509424484589));
#221115=CARTESIAN_POINT('Ctrl Pts',(-26.3510730668209,73.6145851316153,
60.1850441289509));
#221116=CARTESIAN_POINT('Ctrl Pts',(-26.4487404531109,69.4438087013183,
61.3705171264289));
#221117=CARTESIAN_POINT('Ctrl Pts',(-26.5464078394009,65.9028512572195,
63.8729846813812));
#221118=CARTESIAN_POINT('Ctrl Pts',(-26.6440752256909,63.3930960782151,
67.4087804655588));
#221119=CARTESIAN_POINT('Ctrl Pts',(-26.7417426119809,62.1990350726515,
71.5771064383641));
#221120=CARTESIAN_POINT('Ctrl Pts',(-26.8394099982709,62.4560203657777,
75.9054642787187));
#221121=CARTESIAN_POINT('Ctrl Pts',(-26.9370773845609,64.1349215317246,
79.9032153874961));
#221122=CARTESIAN_POINT('Ctrl Pts',(-27.0347447708509,67.0454276575313,
83.1171968964906));
#221123=CARTESIAN_POINT('Ctrl Pts',(-27.1324121571409,70.8576199312134,
85.1830897102328));
#221124=CARTESIAN_POINT('Ctrl Pts',(-27.2300795434309,75.139369406275,85.8667156913576));
#221125=CARTESIAN_POINT('Ctrl Pts',(-27.3277469297209,79.4053207393797,
85.0905827949681));
#221126=CARTESIAN_POINT('Ctrl Pts',(-27.4254143160109,83.1719093768379,
82.9426691362138));
#221127=CARTESIAN_POINT('Ctrl Pts',(-27.5230817023009,86.0121757470976,
79.666450279784));
#221128=CARTESIAN_POINT('Ctrl Pts',(-27.6207490885909,87.6041630268346,
75.6333002019379));
#221129=CARTESIAN_POINT('Ctrl Pts',(-27.7184164748809,87.7674123785483,
71.3003943988506));
#221130=CARTESIAN_POINT('Ctrl Pts',(-27.8160838611709,86.4834187622644,
67.1588870111186));
#221131=CARTESIAN_POINT('Ctrl Pts',(-27.9137512474609,83.8977285641353,
63.6782363178493));
#221132=CARTESIAN_POINT('Ctrl Pts',(-28.0114186337509,80.3034412663224,
61.2529895530694));
#221133=CARTESIAN_POINT('Ctrl Pts',(-28.1090860200409,76.1079853173108,
60.1580592223219));
#221134=CARTESIAN_POINT('Ctrl Pts',(-28.2067534063309,71.7869343055323,
60.5175605475774));
#221135=CARTESIAN_POINT('Ctrl Pts',(-28.3044207926209,67.8300985782672,
62.2907424549827));
#221136=CARTESIAN_POINT('Ctrl Pts',(-28.4020881789109,64.6860030606972,
65.2766068902312));
#221137=CARTESIAN_POINT('Ctrl Pts',(-28.4997555652109,62.7110449610938,
69.1366928418758));
#221138=CARTESIAN_POINT('Ctrl Pts',(-28.5974229515009,62.1290945623912,
73.433442402035));
#221139=CARTESIAN_POINT('Ctrl Pts',(-28.6950903377909,63.0061185301486,
77.6797999010284));
#221140=CARTESIAN_POINT('Ctrl Pts',(-28.7927577240809,65.2427022976115,
81.3944218333965));
#221141=CARTESIAN_POINT('Ctrl Pts',(-28.8904251103709,68.5853191489713,
84.1562392846882));
#221142=CARTESIAN_POINT('Ctrl Pts',(-28.9880924966609,72.6550685999751,
85.6521879654061));
#221143=CARTESIAN_POINT('Ctrl Pts',(-29.0857598829509,76.9906264527469,
85.7126954403172));
#221144=CARTESIAN_POINT('Ctrl Pts',(-29.1834272692409,81.1005379450693,
84.3309029180554));
#221145=CARTESIAN_POINT('Ctrl Pts',(-29.2810946555309,84.5189263330808,
81.6634427256689));
#221146=CARTESIAN_POINT('Ctrl Pts',(-29.3787620418209,86.8583020919226,
78.0126833377833));
#221147=CARTESIAN_POINT('Ctrl Pts',(-29.4764294281109,87.8534865764371,
73.7924545654215));
#221148=CARTESIAN_POINT('Ctrl Pts',(-29.5740968144009,87.3916711998821,
69.4811381067028));
#221149=CARTESIAN_POINT('Ctrl Pts',(-29.6717642006909,85.5252047887965,
65.5674408540281));
#221150=CARTESIAN_POINT('Ctrl Pts',(-29.7694315869809,82.4656596108035,
62.4949977946519));
#221151=CARTESIAN_POINT('Ctrl Pts',(-29.8670989732709,78.5598487171896,
60.61208401208));
#221152=CARTESIAN_POINT('Ctrl Pts',(-29.9647663595609,74.2505131413366,
60.1321361566155));
#221153=CARTESIAN_POINT('Ctrl Pts',(-30.0624337458509,70.026135233775,61.1095584519391));
#221154=CARTESIAN_POINT('Ctrl Pts',(-30.1601011321409,66.3655670155455,
63.4335557344115));
#221155=CARTESIAN_POINT('Ctrl Pts',(-30.2577685184309,63.6837501722009,
66.8406925775739));
#221156=CARTESIAN_POINT('Ctrl Pts',(-30.3554359047209,62.2846805686123,
70.9447548692043));
#221157=CARTESIAN_POINT('Ctrl Pts',(-30.4531032910109,62.3269489658028,
75.2805288983569));
#221158=CARTESIAN_POINT('Ctrl Pts',(-30.5507706773009,63.8057640529833,
79.3565353982501));
#221159=CARTESIAN_POINT('Ctrl Pts',(-30.6484380635909,66.5534955639515,
82.7107409066956));
#221160=CARTESIAN_POINT('Ctrl Pts',(-30.7461054498809,70.2586759131591,
84.9629313136325));
#221161=CARTESIAN_POINT('Ctrl Pts',(-30.8437728361709,74.5013064316051,
85.8578108212735));
#221162=CARTESIAN_POINT('Ctrl Pts',(-30.9414402224609,78.8004660836611,
85.2939408579818));
#221163=CARTESIAN_POINT('Ctrl Pts',(-31.0391076087509,82.668826004946,83.335238591712));
#221164=CARTESIAN_POINT('Ctrl Pts',(-31.1367749950409,85.6678903965733,
80.2037316337721));
#221165=CARTESIAN_POINT('Ctrl Pts',(-31.2344423813309,87.4577019724425,
76.2543902256493));
#221166=CARTESIAN_POINT('Ctrl Pts',(-31.3321097676209,87.8353776347299,
71.9348897690367));
#221167=CARTESIAN_POINT('Ctrl Pts',(-31.4297771539109,86.7581061551578,
67.7348648827743));
#221168=CARTESIAN_POINT('Ctrl Pts',(-31.5274445402009,84.3480010930265,
64.1304069382318));
#221169=CARTESIAN_POINT('Ctrl Pts',(-31.6251119264909,80.8782584005449,
61.5300977436922));
#221170=CARTESIAN_POINT('Ctrl Pts',(-31.7227793127809,76.7421894906778,
60.2286921489303));
#221171=CARTESIAN_POINT('Ctrl Pts',(-31.8204466990709,72.4086337435891,
60.373716836065));
#221172=CARTESIAN_POINT('Ctrl Pts',(-31.9181140853609,68.3688280177291,
61.9487080894351));
#221173=CARTESIAN_POINT('Ctrl Pts',(-32.0157814716509,65.0806685046385,
64.7752251657534));
#221174=CARTESIAN_POINT('Ctrl Pts',(-32.0808930625109,63.6382286155421,
67.2800938763135));
#221175=CARTESIAN_POINT('Ctrl Pts',(-32.1134488579409,63.1452236775756,
68.616887177359));
#221176=CARTESIAN_POINT('Ctrl Pts',(-26.0868642456509,87.2037143630092,
73.1461018017395));
#221177=CARTESIAN_POINT('Ctrl Pts',(-26.1194200410809,87.2214422810865,
71.7699608131094));
#221178=CARTESIAN_POINT('Ctrl Pts',(-26.1845316319409,86.7868991642302,
69.0119758206587));
#221179=CARTESIAN_POINT('Ctrl Pts',(-26.2821990182309,84.7989906263339,
65.3255218656522));
#221180=CARTESIAN_POINT('Ctrl Pts',(-26.3798664045209,81.7003219690098,
62.5078190003946));
#221181=CARTESIAN_POINT('Ctrl Pts',(-26.4775337908109,77.8421422775993,
60.8781721617227));
#221182=CARTESIAN_POINT('Ctrl Pts',(-26.5752011771009,73.6617930516903,
60.6213343098834));
#221183=CARTESIAN_POINT('Ctrl Pts',(-26.6728685633909,69.6331355526051,
61.766412393317));
#221184=CARTESIAN_POINT('Ctrl Pts',(-26.7705359496809,66.212835999391,64.1836085317264));
#221185=CARTESIAN_POINT('Ctrl Pts',(-26.8682033359709,63.7886005622341,
67.5989223082414));
#221186=CARTESIAN_POINT('Ctrl Pts',(-26.9658707222609,62.6352271065125,
71.6252128490112));
#221187=CARTESIAN_POINT('Ctrl Pts',(-27.0635381085509,62.8834556427626,
75.8060821820242));
#221188=CARTESIAN_POINT('Ctrl Pts',(-27.1612054948409,64.5051483624386,
79.6676101859859));
#221189=CARTESIAN_POINT('Ctrl Pts',(-27.2588728811309,67.3164791843653,
82.7720754874778));
#221190=CARTESIAN_POINT('Ctrl Pts',(-27.3565402674209,70.9987712582735,
84.767573140128));
#221191=CARTESIAN_POINT('Ctrl Pts',(-27.4542076537109,75.1346204029575,
85.4279046111303));
#221192=CARTESIAN_POINT('Ctrl Pts',(-27.5518750400009,79.2552097263266,
84.678218391901));
#221193=CARTESIAN_POINT('Ctrl Pts',(-27.6495424262909,82.8934521049011,
82.6034947491146));
#221194=CARTESIAN_POINT('Ctrl Pts',(-27.7472098125809,85.6369365863143,
79.4389128336909));
#221195=CARTESIAN_POINT('Ctrl Pts',(-27.8448771988709,87.1746770047232,
75.5431920781981));
#221196=CARTESIAN_POINT('Ctrl Pts',(-27.9425445851609,87.3323636455694,
71.3579297539834));
#221197=CARTESIAN_POINT('Ctrl Pts',(-28.0402119714509,86.0921220269066,
67.3575439567694));
#221198=CARTESIAN_POINT('Ctrl Pts',(-28.1378793577409,83.5945390513956,
63.9954962058266));
#221199=CARTESIAN_POINT('Ctrl Pts',(-28.2355467440309,80.1227268557061,
61.6528895642724));
#221200=CARTESIAN_POINT('Ctrl Pts',(-28.3332141303209,76.0702307908808,
60.5952689121648));
#221201=CARTESIAN_POINT('Ctrl Pts',(-28.4308815166109,71.8964193067431,
60.9425202535142));
#221202=CARTESIAN_POINT('Ctrl Pts',(-28.5285489029009,68.0744124953734,
62.6552811046037));
#221203=CARTESIAN_POINT('Ctrl Pts',(-28.6262162891909,65.0374518247561,
65.5394024065494));
#221204=CARTESIAN_POINT('Ctrl Pts',(-28.7238836754809,63.1297902918518,
69.2679561845011));
#221205=CARTESIAN_POINT('Ctrl Pts',(-28.8215510617709,62.5676698145191,
73.4182942873752));
#221206=CARTESIAN_POINT('Ctrl Pts',(-28.9192184480609,63.4148092485251,
77.5199574352399));
#221207=CARTESIAN_POINT('Ctrl Pts',(-29.0168858343509,65.5751815719184,
81.1080038707725));
#221208=CARTESIAN_POINT('Ctrl Pts',(-29.1145532206409,68.8038989749744,
83.7757125749618));
#221209=CARTESIAN_POINT('Ctrl Pts',(-29.2122206069309,72.7349719824068,
85.2206869032595));
#221210=CARTESIAN_POINT('Ctrl Pts',(-29.3098879932209,76.9227959878881,
85.2791325899756));
#221211=CARTESIAN_POINT('Ctrl Pts',(-29.4075553795109,80.8926625177431,
83.9444245566036));
#221212=CARTESIAN_POINT('Ctrl Pts',(-29.5052227658009,84.1945695473749,
81.3678578939925));
#221213=CARTESIAN_POINT('Ctrl Pts',(-29.6028901520909,86.4542312318516,
77.8414978909713));
#221214=CARTESIAN_POINT('Ctrl Pts',(-29.7005575383809,87.4155048708503,
73.7650731351128));
#221215=CARTESIAN_POINT('Ctrl Pts',(-29.7982249246709,86.9694258227422,
69.6006644997807));
#221216=CARTESIAN_POINT('Ctrl Pts',(-29.8958923109609,85.1665591312736,
65.820326222327));
#221217=CARTESIAN_POINT('Ctrl Pts',(-29.9935596972509,82.2112677530227,
62.8525764571268));
#221218=CARTESIAN_POINT('Ctrl Pts',(-30.0912270835409,78.4385471074775,
61.0338228372305));
#221219=CARTESIAN_POINT('Ctrl Pts',(-30.1888944698309,74.2760518565624,
60.5702291732061));
#221220=CARTESIAN_POINT('Ctrl Pts',(-30.2865618561209,70.1956193470026,
61.5143458683933));
#221221=CARTESIAN_POINT('Ctrl Pts',(-30.3842292424109,66.6597847488641,
63.7591530970452));
#221222=CARTESIAN_POINT('Ctrl Pts',(-30.4818966287009,64.0693506371989,
67.0501919774508));
#221223=CARTESIAN_POINT('Ctrl Pts',(-30.5795640149909,62.7179542378677,
71.0144086177314));
#221224=CARTESIAN_POINT('Ctrl Pts',(-30.6772314012809,62.7587823422011,
75.2024414334005));
#221225=CARTESIAN_POINT('Ctrl Pts',(-30.7748987875709,64.1872069030099,
79.1395582812057));
#221226=CARTESIAN_POINT('Ctrl Pts',(-30.8725661738609,66.8413096443314,
82.3794694586463));
#221227=CARTESIAN_POINT('Ctrl Pts',(-30.9702335601509,70.4202362180114,
84.5549166263379));
#221228=CARTESIAN_POINT('Ctrl Pts',(-31.0679009464409,74.5182993819421,
85.4193031739153));
#221229=CARTESIAN_POINT('Ctrl Pts',(-31.1655683327309,78.670965452998,84.8746470423662));
#221230=CARTESIAN_POINT('Ctrl Pts',(-31.2632357190209,82.4075112656457,
82.9826874263801));
#221231=CARTESIAN_POINT('Ctrl Pts',(-31.3609031053109,85.304382736349,79.9578863610725));
#221232=CARTESIAN_POINT('Ctrl Pts',(-31.4585704916009,87.0332066010756,
76.1431185004146));
#221233=CARTESIAN_POINT('Ctrl Pts',(-31.5562378778909,87.3980129901441,
71.970804736377));
#221234=CARTESIAN_POINT('Ctrl Pts',(-31.6539052641809,86.357449465044,67.9138954205205));
#221235=CARTESIAN_POINT('Ctrl Pts',(-31.7515726504709,84.0294685736218,
64.4322591422073));
#221236=CARTESIAN_POINT('Ctrl Pts',(-31.8492400367609,80.6779571340673,
61.9205553116033));
#221237=CARTESIAN_POINT('Ctrl Pts',(-31.9469074230509,76.6828244989406,
60.6634950264663));
#221238=CARTESIAN_POINT('Ctrl Pts',(-32.0445748093409,72.4969343775197,
60.8035780069627));
#221239=CARTESIAN_POINT('Ctrl Pts',(-32.1422421956309,68.5947847647611,
62.3249015374696));
#221240=CARTESIAN_POINT('Ctrl Pts',(-32.2399095819209,65.4186690697612,
65.0551052312264));
#221241=CARTESIAN_POINT('Ctrl Pts',(-32.3050211727809,64.025380224545,67.4746207060263));
#221242=CARTESIAN_POINT('Ctrl Pts',(-32.3375769682109,63.5491743972569,
68.7658628636919));
#221243=CARTESIAN_POINT('Ctrl Pts',(-26.3109923559309,86.773203990145,73.1405558201253));
#221244=CARTESIAN_POINT('Ctrl Pts',(-26.3435481513609,86.7903065205387,
71.812960950527));
#221245=CARTESIAN_POINT('Ctrl Pts',(-26.4086597422209,86.3710927791314,
69.1522693813868));
#221246=CARTESIAN_POINT('Ctrl Pts',(-26.5063271285109,84.4533116811586,
65.595862444819));
#221247=CARTESIAN_POINT('Ctrl Pts',(-26.6039945148009,81.4639547431525,
62.8775596699702));
#221248=CARTESIAN_POINT('Ctrl Pts',(-26.7016619010909,77.7418800381493,
61.3054018749864));
#221249=CARTESIAN_POINT('Ctrl Pts',(-26.7993292873809,73.7090009717682,
61.0576244908064));
#221250=CARTESIAN_POINT('Ctrl Pts',(-26.8969966736709,69.8224624038905,
62.1623076602057));
#221251=CARTESIAN_POINT('Ctrl Pts',(-26.9946640599609,66.5228207415521,
64.4942323820705));
#221252=CARTESIAN_POINT('Ctrl Pts',(-27.0923314462509,64.1841050462514,
67.789064150928));
#221253=CARTESIAN_POINT('Ctrl Pts',(-27.1899988325409,63.0714191403804,
71.6733192596676));
#221254=CARTESIAN_POINT('Ctrl Pts',(-27.2876662188309,63.3108909197464,
75.7067000853347));
#221255=CARTESIAN_POINT('Ctrl Pts',(-27.3853336051209,64.8753751931555,
79.4320049844844));
#221256=CARTESIAN_POINT('Ctrl Pts',(-27.4830009914109,67.5875307112038,
82.4269540784776));
#221257=CARTESIAN_POINT('Ctrl Pts',(-27.5806683777009,71.139922585341,84.3520565700369));
#221258=CARTESIAN_POINT('Ctrl Pts',(-27.6783357639909,75.129871399649,84.9890935309176));
#221259=CARTESIAN_POINT('Ctrl Pts',(-27.7760031502809,79.1050987132879,
84.2658539888279));
#221260=CARTESIAN_POINT('Ctrl Pts',(-27.8736705365709,82.6149948329797,
82.2643203620044));
#221261=CARTESIAN_POINT('Ctrl Pts',(-27.9713379228609,85.2616974255471,
79.211375387585));
#221262=CARTESIAN_POINT('Ctrl Pts',(-28.0690053091509,86.745190982611,75.4530839544341));
#221263=CARTESIAN_POINT('Ctrl Pts',(-28.1666726954409,86.8973149125801,
71.4154651090891));
#221264=CARTESIAN_POINT('Ctrl Pts',(-28.2643400817309,85.7008252915377,
67.5562009023972));
#221265=CARTESIAN_POINT('Ctrl Pts',(-28.3620074680209,83.2913495386348,
64.3127560937844));
#221266=CARTESIAN_POINT('Ctrl Pts',(-28.4596748543109,79.9420124450654,
62.0527895754545));
#221267=CARTESIAN_POINT('Ctrl Pts',(-28.5573422406009,76.0324762644166,
61.0324786020043));
#221268=CARTESIAN_POINT('Ctrl Pts',(-28.6550096268909,72.005904307922,61.367479959455));
#221269=CARTESIAN_POINT('Ctrl Pts',(-28.7526770131809,68.3187264124431,
63.0198197542422));
#221270=CARTESIAN_POINT('Ctrl Pts',(-28.8503443994709,65.3889005887908,
65.8021979228998));
#221271=CARTESIAN_POINT('Ctrl Pts',(-28.9480117857609,63.5485356226125,
69.399219527172));
#221272=CARTESIAN_POINT('Ctrl Pts',(-29.0456791720509,63.00624506665,73.403146172761));
#221273=CARTESIAN_POINT('Ctrl Pts',(-29.1433465583409,63.823499966919,77.3601149694953));
#221274=CARTESIAN_POINT('Ctrl Pts',(-29.2410139446309,65.9076608462574,
80.8215859081835));
#221275=CARTESIAN_POINT('Ctrl Pts',(-29.3386813309209,69.0224788010218,
83.3951858652539));
#221276=CARTESIAN_POINT('Ctrl Pts',(-29.4363487172109,72.8148753648847,
84.789185841132));
#221277=CARTESIAN_POINT('Ctrl Pts',(-29.5340161035009,76.8549655230795,
84.8455697396331));
#221278=CARTESIAN_POINT('Ctrl Pts',(-29.6316834897909,80.6847870904639,
83.5579461951268));
#221279=CARTESIAN_POINT('Ctrl Pts',(-29.7293508760809,83.8702127616981,
81.0722730622719));
#221280=CARTESIAN_POINT('Ctrl Pts',(-29.8270182623709,86.0501603718022,
77.6703124441068));
#221281=CARTESIAN_POINT('Ctrl Pts',(-29.9246856486609,86.9775231652655,
73.7376917047466));
#221282=CARTESIAN_POINT('Ctrl Pts',(-30.0223530349509,86.5471804455886,
69.720190892803));
#221283=CARTESIAN_POINT('Ctrl Pts',(-30.1200204212409,84.8079134737197,
66.0732115905698));
#221284=CARTESIAN_POINT('Ctrl Pts',(-30.2176878075309,81.956875895195,63.2101551195606));
#221285=CARTESIAN_POINT('Ctrl Pts',(-30.3153551938209,78.3172454977062,
61.4555616623674));
#221286=CARTESIAN_POINT('Ctrl Pts',(-30.4130225801109,74.3015905717297,
61.0083221897942));
#221287=CARTESIAN_POINT('Ctrl Pts',(-30.5106899664009,70.365103460175,61.9191332848712));
#221288=CARTESIAN_POINT('Ctrl Pts',(-30.6083573526909,66.9540024821432,
64.0847504597222));
#221289=CARTESIAN_POINT('Ctrl Pts',(-30.7060247389809,64.4549511021745,
67.2596913773823));
#221290=CARTESIAN_POINT('Ctrl Pts',(-30.8036921252709,63.1512279071195,
71.0840623663198));
#221291=CARTESIAN_POINT('Ctrl Pts',(-30.9013595115609,63.1906157186087,
75.1243539684998));
#221292=CARTESIAN_POINT('Ctrl Pts',(-30.9990268978509,64.5686497530634,
78.9225811642114));
#221293=CARTESIAN_POINT('Ctrl Pts',(-31.0966942841409,67.1291237247518,
82.0481980106354));
#221294=CARTESIAN_POINT('Ctrl Pts',(-31.1943616704309,70.5817965229168,
84.1469019390543));
#221295=CARTESIAN_POINT('Ctrl Pts',(-31.2920290567209,74.5352923323311,
84.980795526557));
#221296=CARTESIAN_POINT('Ctrl Pts',(-31.3896964430109,78.5414648223814,
84.4553532267351));
#221297=CARTESIAN_POINT('Ctrl Pts',(-31.4873638293009,82.1461965263699,
82.630136261015));
#221298=CARTESIAN_POINT('Ctrl Pts',(-31.5850312155909,84.9408750761412,
79.712041088333));
#221299=CARTESIAN_POINT('Ctrl Pts',(-31.6826986018809,86.6087112297139,
76.031846775141));
#221300=CARTESIAN_POINT('Ctrl Pts',(-31.7803659881709,86.9606483455424,
72.0067197036773));
#221301=CARTESIAN_POINT('Ctrl Pts',(-31.8780333744609,85.9567927749164,
68.0929259582372));
#221302=CARTESIAN_POINT('Ctrl Pts',(-31.9757007607509,83.7109360542007,
64.7341113461544));
#221303=CARTESIAN_POINT('Ctrl Pts',(-32.0733681470409,80.4776558675686,
62.3110128795057));
#221304=CARTESIAN_POINT('Ctrl Pts',(-32.1710355333309,76.6234595071886,
61.0982979039962));
#221305=CARTESIAN_POINT('Ctrl Pts',(-32.2687029196209,72.5852350114378,
61.233439177867));
#221306=CARTESIAN_POINT('Ctrl Pts',(-32.3663703059109,68.8207415117928,
62.7010949855073));
#221307=CARTESIAN_POINT('Ctrl Pts',(-32.4640376922009,65.7566696348843,
65.3349852966985));
#221308=CARTESIAN_POINT('Ctrl Pts',(-32.5291492830609,64.4125318335594,
67.6691475357373));
#221309=CARTESIAN_POINT('Ctrl Pts',(-32.5617050784909,63.9531251169506,
68.9148385500207));
#221310=CARTESIAN_POINT('',(-25.7929823067402,86.9560662404983,67.8848523453355));
#221311=CARTESIAN_POINT('Ctrl Pts',(-21.8528274563309,86.0743198651036,
79.922508163981));
#221312=CARTESIAN_POINT('Ctrl Pts',(-21.8943126079409,87.0706315571954,
78.331207182819));
#221313=CARTESIAN_POINT('Ctrl Pts',(-21.9772829111709,88.365914761124,74.7135063587071));
#221314=CARTESIAN_POINT('Ctrl Pts',(-22.1017383660109,87.8638206689949,
68.9705612798485));
#221315=CARTESIAN_POINT('Ctrl Pts',(-22.2261938208509,85.007906359249,63.9630709697879));
#221316=CARTESIAN_POINT('Ctrl Pts',(-22.3506492756909,80.3208945091187,
60.6069640495696));
#221317=CARTESIAN_POINT('Ctrl Pts',(-22.4751047305309,74.660314401302,59.516380349804));
#221318=CARTESIAN_POINT('Ctrl Pts',(-22.5995601853709,69.0618889064457,
60.8908421950948));
#221319=CARTESIAN_POINT('Ctrl Pts',(-22.7240156402109,64.5499522186845,
64.4788713483501));
#221320=CARTESIAN_POINT('Ctrl Pts',(-22.8484710950509,61.950049264097,69.6239686585277));
#221321=CARTESIAN_POINT('Ctrl Pts',(-22.9729265498909,61.737881126671,75.3847418289771));
#221322=CARTESIAN_POINT('Ctrl Pts',(-23.0973820047309,63.9522680392151,
80.7071485391446));
#221323=CARTESIAN_POINT('Ctrl Pts',(-23.2218374595709,68.1880460907971,
84.6173540230353));
#221324=CARTESIAN_POINT('Ctrl Pts',(-23.3462929144109,73.6701997203885,
86.3999123553094));
#221325=CARTESIAN_POINT('Ctrl Pts',(-23.4707483692509,79.3956654174182,
85.7286708365147));
#221326=CARTESIAN_POINT('Ctrl Pts',(-23.5952038240909,84.3168611364881,
82.726445774969));
#221327=CARTESIAN_POINT('Ctrl Pts',(-23.7196592789309,87.5333612087902,
77.9425509276693));
#221328=CARTESIAN_POINT('Ctrl Pts',(-23.8441147337709,88.4566462187817,
72.2522901765632));
#221329=CARTESIAN_POINT('Ctrl Pts',(-23.9685701886109,86.9177837423074,
66.6968041578818));
#221330=CARTESIAN_POINT('Ctrl Pts',(-24.0930256434509,83.1983377230885,
62.292573926019));
#221331=CARTESIAN_POINT('Ctrl Pts',(-24.2174810982909,77.9788510332431,
59.8454365534837));
#221332=CARTESIAN_POINT('Ctrl Pts',(-24.3419365531309,72.2143273064089,
59.8031420245331));
#221333=CARTESIAN_POINT('Ctrl Pts',(-24.4663920079709,66.959494991902,62.1734289212542));
#221334=CARTESIAN_POINT('Ctrl Pts',(-24.5908474628109,63.175824874085,66.522608506883));
#221335=CARTESIAN_POINT('Ctrl Pts',(-24.7153029176509,61.5556108309429,
72.0549162569263));
#221336=CARTESIAN_POINT('Ctrl Pts',(-24.8397583724909,62.3953016319811,
77.7581120451256));
#221337=CARTESIAN_POINT('Ctrl Pts',(-24.9642138273309,65.5412599143316,
82.5886884279321));
#221338=CARTESIAN_POINT('Ctrl Pts',(-25.0886692821709,70.417873503959,85.6628006211224));
#221339=CARTESIAN_POINT('Ctrl Pts',(-25.2131247370109,76.1328727949813,
86.4179803938818));
#221340=CARTESIAN_POINT('Ctrl Pts',(-25.3375801918409,81.6405947968609,
84.7160584470278));
#221341=CARTESIAN_POINT('Ctrl Pts',(-25.4620356466809,85.9332827488514,
80.8684145069104));
#221342=CARTESIAN_POINT('Ctrl Pts',(-25.5864911015209,88.2255644558482,
75.5791186817848));
#221343=CARTESIAN_POINT('Ctrl Pts',(-25.7109465563609,88.0978142907784,
69.8156825060805));
#221344=CARTESIAN_POINT('Ctrl Pts',(-25.7939168595909,86.4153968231172,
66.3609771213052));
#221345=CARTESIAN_POINT('Ctrl Pts',(-25.8354020112009,85.2513468075614,
64.8879315138231));
#221346=CARTESIAN_POINT('Ctrl Pts',(-22.0769555666009,85.7093978414631,
79.694030909732));
#221347=CARTESIAN_POINT('Ctrl Pts',(-22.1184407182209,86.672878977512,78.1551666272841));
#221348=CARTESIAN_POINT('Ctrl Pts',(-22.2014110214409,87.9254798881987,
74.6566766189857));
#221349=CARTESIAN_POINT('Ctrl Pts',(-22.3258664762809,87.4399308475407,
69.1029736033339));
#221350=CARTESIAN_POINT('Ctrl Pts',(-22.4503219311209,84.6781248931543,
64.2604905821707));
#221351=CARTESIAN_POINT('Ctrl Pts',(-22.5747773859609,80.1455598957456,
61.014974410985));
#221352=CARTESIAN_POINT('Ctrl Pts',(-22.6992328408009,74.6715077529058,
59.9603277272688));
#221353=CARTESIAN_POINT('Ctrl Pts',(-22.8236882956409,69.2575620984069,
61.2894981773207));
#221354=CARTESIAN_POINT('Ctrl Pts',(-22.9481437504809,64.8943031702593,
64.7592942584412));
#221355=CARTESIAN_POINT('Ctrl Pts',(-23.0725992053209,62.3800724609222,
69.7348498409865));
#221356=CARTESIAN_POINT('Ctrl Pts',(-23.1970546601609,62.1748957078033,
75.3057934752902));
#221357=CARTESIAN_POINT('Ctrl Pts',(-23.3215101150009,64.3163139357595,
80.4528157418881));
#221358=CARTESIAN_POINT('Ctrl Pts',(-23.4459655698409,68.4125142329405,
84.2341717690691));
#221359=CARTESIAN_POINT('Ctrl Pts',(-23.5704210246809,73.7140194235437,
85.9579910725118));
#221360=CARTESIAN_POINT('Ctrl Pts',(-23.6948764795209,79.2508190395935,
85.3088683670014));
#221361=CARTESIAN_POINT('Ctrl Pts',(-23.8193319343609,84.0098510571879,
82.4055729063877));
#221362=CARTESIAN_POINT('Ctrl Pts',(-23.9437873892009,87.1203607183689,
77.7793174093934));
#221363=CARTESIAN_POINT('Ctrl Pts',(-24.0682428440409,88.0132215543806,
72.2765626625984));
#221364=CARTESIAN_POINT('Ctrl Pts',(-24.1926982988809,86.5250678181105,
66.9041415386484));
#221365=CARTESIAN_POINT('Ctrl Pts',(-24.3171537537209,82.9281853318851,
62.6450399131802));
#221366=CARTESIAN_POINT('Ctrl Pts',(-24.4416092085609,77.8806916554658,
60.2785408401571));
#221367=CARTESIAN_POINT('Ctrl Pts',(-24.5660646634009,72.3061210534633,
60.2376400044814));
#221368=CARTESIAN_POINT('Ctrl Pts',(-24.6905201182409,67.2244464647128,
62.5298209857595));
#221369=CARTESIAN_POINT('Ctrl Pts',(-24.8149755730809,63.565456198401,66.7356859990377));
#221370=CARTESIAN_POINT('Ctrl Pts',(-24.9394310279209,61.9986315998985,
72.0856926268274));
#221371=CARTESIAN_POINT('Ctrl Pts',(-25.0638864827609,62.8106528311494,
77.6009561741625));
#221372=CARTESIAN_POINT('Ctrl Pts',(-25.1883419376009,65.8529452020323,
82.2723549523412));
#221373=CARTESIAN_POINT('Ctrl Pts',(-25.3127973924409,70.5688641646879,
85.2451687131141));
#221374=CARTESIAN_POINT('Ctrl Pts',(-25.4372528472809,76.0955422647207,
85.9754637313838));
#221375=CARTESIAN_POINT('Ctrl Pts',(-25.5617083021209,81.4217732962185,
84.3296236756516));
#221376=CARTESIAN_POINT('Ctrl Pts',(-25.6861637569609,85.5730081934492,
80.6087676584069));
#221377=CARTESIAN_POINT('Ctrl Pts',(-25.8106192118009,87.7897544193025,
75.4937652038599));
#221378=CARTESIAN_POINT('Ctrl Pts',(-25.9350746666409,87.6662138896252,
69.9202463159047));
#221379=CARTESIAN_POINT('Ctrl Pts',(-26.0180449698709,86.0392355996607,
66.5793807059785));
#221380=CARTESIAN_POINT('Ctrl Pts',(-26.0595301214809,84.9135434690527,
65.1548750350943));
#221381=CARTESIAN_POINT('Ctrl Pts',(-22.3010836768809,85.3444758178016,
79.4655536555077));
#221382=CARTESIAN_POINT('Ctrl Pts',(-22.3425688284909,86.2751263978158,
77.9791260717799));
#221383=CARTESIAN_POINT('Ctrl Pts',(-22.4255391317209,87.4850450152697,
74.5998468792995));
#221384=CARTESIAN_POINT('Ctrl Pts',(-22.5499945865609,87.0160410260944,
69.235385926855));
#221385=CARTESIAN_POINT('Ctrl Pts',(-22.6744500414009,84.3483434270861,
64.5579101945861));
#221386=CARTESIAN_POINT('Ctrl Pts',(-22.7989054962409,79.9702252824092,
61.4229847724263));
#221387=CARTESIAN_POINT('Ctrl Pts',(-22.9233609510809,74.6827011045569,
60.4042751047315));
#221388=CARTESIAN_POINT('Ctrl Pts',(-23.0478164059209,69.4532352904164,
61.6881541595265));
#221389=CARTESIAN_POINT('Ctrl Pts',(-23.1722718607609,65.238654121862,65.0397171684909));
#221390=CARTESIAN_POINT('Ctrl Pts',(-23.2967273156009,62.8100956577584,
69.8457310233925));
#221391=CARTESIAN_POINT('Ctrl Pts',(-23.4211827704409,62.6119102889162,
75.2268451215454));
#221392=CARTESIAN_POINT('Ctrl Pts',(-23.5456382252809,64.6803598322671,
80.1984829445947));
#221393=CARTESIAN_POINT('Ctrl Pts',(-23.6700936801209,68.6369823750294,
83.8509895150804));
#221394=CARTESIAN_POINT('Ctrl Pts',(-23.7945491349609,73.7578391266432,
85.516069789702));
#221395=CARTESIAN_POINT('Ctrl Pts',(-23.9190045898009,79.1059726617113,
84.8890658975066));
#221396=CARTESIAN_POINT('Ctrl Pts',(-24.0434600446409,83.7028409778482,
82.0847000378495));
#221397=CARTESIAN_POINT('Ctrl Pts',(-24.1679154994809,86.7073602279152,
77.6160838911697));
#221398=CARTESIAN_POINT('Ctrl Pts',(-24.2923709543209,87.5697968899769,
72.3008351486921));
#221399=CARTESIAN_POINT('Ctrl Pts',(-24.4168264091609,86.1323518939429,
67.1114789194617));
#221400=CARTESIAN_POINT('Ctrl Pts',(-24.5412818640009,82.6580329407277,
62.997505900382));
#221401=CARTESIAN_POINT('Ctrl Pts',(-24.6657373188409,77.7825322777459,
60.7116451268434));
#221402=CARTESIAN_POINT('Ctrl Pts',(-24.7901927736809,72.3979148005717,
60.6721379844194));
#221403=CARTESIAN_POINT('Ctrl Pts',(-24.9146482285209,67.4893979375692,
62.8862130502327));
#221404=CARTESIAN_POINT('Ctrl Pts',(-25.0391036833609,63.955087522728,66.9487634911397));
#221405=CARTESIAN_POINT('Ctrl Pts',(-25.1635591382009,62.4416523688531,
72.1164689966783));
#221406=CARTESIAN_POINT('Ctrl Pts',(-25.2880145930409,63.2260040303007,
77.4438003031568));
#221407=CARTESIAN_POINT('Ctrl Pts',(-25.4124700478809,66.1646304897018,
81.9560214767266));
#221408=CARTESIAN_POINT('Ctrl Pts',(-25.5369255027209,70.7198548253873,
84.8275368050829));
#221409=CARTESIAN_POINT('Ctrl Pts',(-25.6613809575609,76.0582117344314,
85.5329470688848));
#221410=CARTESIAN_POINT('Ctrl Pts',(-25.7858364124009,81.2029517955551,
83.9431889042895));
#221411=CARTESIAN_POINT('Ctrl Pts',(-25.9102918672409,85.2127336380402,
80.34912080992));
#221412=CARTESIAN_POINT('Ctrl Pts',(-26.0347473220809,87.3539443827526,
75.4084117259452));
#221413=CARTESIAN_POINT('Ctrl Pts',(-26.1592027769209,87.2346134884619,
70.024810125727));
#221414=CARTESIAN_POINT('Ctrl Pts',(-26.2421730801409,85.6630743761998,
66.7977842906575));
#221415=CARTESIAN_POINT('Ctrl Pts',(-26.2836582317609,84.5757401305432,
65.4218185563542));
#221416=CARTESIAN_POINT('Ctrl Pts',(-22.5252117871509,84.9795537941519,
79.2370764012549));
#221417=CARTESIAN_POINT('Ctrl Pts',(-22.5666969387709,85.8773738181418,
77.8030855162483));
#221418=CARTESIAN_POINT('Ctrl Pts',(-22.6496672419909,87.0446101423444,
74.5430171395781));
#221419=CARTESIAN_POINT('Ctrl Pts',(-22.7741226968309,86.5921512046365,
69.3677982503388));
#221420=CARTESIAN_POINT('Ctrl Pts',(-22.8985781516709,84.0185619609905,
64.8553298069685));
#221421=CARTESIAN_POINT('Ctrl Pts',(-23.0230336065109,79.7948906690355,
61.8309951338414));
#221422=CARTESIAN_POINT('Ctrl Pts',(-23.1474890613509,74.6938944561598,
60.8482224821959));
#221423=CARTESIAN_POINT('Ctrl Pts',(-23.2719445161909,69.6489084823822,
62.0868101417543));
#221424=CARTESIAN_POINT('Ctrl Pts',(-23.3963999710309,65.5830050734272,
65.3201400785792));
#221425=CARTESIAN_POINT('Ctrl Pts',(-23.5208554258709,63.2401188545836,
69.9566122058514));
#221426=CARTESIAN_POINT('Ctrl Pts',(-23.6453108807209,63.0489248700484,
75.1478967678585));
#221427=CARTESIAN_POINT('Ctrl Pts',(-23.7697663355609,65.0444057288086,
79.9441501473479));
#221428=CARTESIAN_POINT('Ctrl Pts',(-23.8942217904009,68.8614505171728,
83.4678072611142));
#221429=CARTESIAN_POINT('Ctrl Pts',(-24.0186772452409,73.8016588297993,
85.0741485069047));
#221430=CARTESIAN_POINT('Ctrl Pts',(-24.1431327000809,78.9611262838869,
84.4692634279924));
#221431=CARTESIAN_POINT('Ctrl Pts',(-24.2675881549209,83.3958308985575,
81.7638271692711));
#221432=CARTESIAN_POINT('Ctrl Pts',(-24.3920436097609,86.2943597374942,
77.4528503728929));
#221433=CARTESIAN_POINT('Ctrl Pts',(-24.5164990646009,87.1263722255761,
72.3251076347264));
#221434=CARTESIAN_POINT('Ctrl Pts',(-24.6409545194409,85.7396359697469,
67.3188163002233));
#221435=CARTESIAN_POINT('Ctrl Pts',(-24.7654099742709,82.3878805495234,
63.3499718875428));
#221436=CARTESIAN_POINT('Ctrl Pts',(-24.8898654291109,77.6843728999677,
61.1447494135163));
#221437=CARTESIAN_POINT('Ctrl Pts',(-25.0143208839509,72.489708547626,61.1066359643677));
#221438=CARTESIAN_POINT('Ctrl Pts',(-25.1387763387909,67.7543494103795,
63.2426051147388));
#221439=CARTESIAN_POINT('Ctrl Pts',(-25.2632317936309,64.344718847044,67.1618409832945));
#221440=CARTESIAN_POINT('Ctrl Pts',(-25.3876872484709,62.8846731378082,
72.1472453665802));
#221441=CARTESIAN_POINT('Ctrl Pts',(-25.5121427033109,63.6413552294693,
77.2866444321928));
#221442=CARTESIAN_POINT('Ctrl Pts',(-25.6365981581509,66.4763157774064,
81.6396880011265));
#221443=CARTESIAN_POINT('Ctrl Pts',(-25.7610536129909,70.8708454861167,
84.4099048970748));
#221444=CARTESIAN_POINT('Ctrl Pts',(-25.8855090678309,76.0208812041709,
85.0904304063868));
#221445=CARTESIAN_POINT('Ctrl Pts',(-26.0099645226709,80.9841302949145,
83.5567541329141));
#221446=CARTESIAN_POINT('Ctrl Pts',(-26.1344199775109,84.8524590826292,
80.0894739614117));
#221447=CARTESIAN_POINT('Ctrl Pts',(-26.2588754323509,86.9181343462161,
75.3230582480241));
#221448=CARTESIAN_POINT('Ctrl Pts',(-26.3833308871909,86.8030130873046,
70.1293739355507));
#221449=CARTESIAN_POINT('Ctrl Pts',(-26.4663011904209,85.2869131527418,
67.0161878753345));
#221450=CARTESIAN_POINT('Ctrl Pts',(-26.5077863420309,84.2379367920383,
65.6887620776161));
#221451=CARTESIAN_POINT('',(-22.5675364832709,86.9994393436682,73.0560055650937));
#221452=CARTESIAN_POINT('Ctrl Pts',(-22.5675364832709,86.9990620203006,
73.0559939530084));
#221453=CARTESIAN_POINT('Ctrl Pts',(-22.5675364832709,86.969760595878,73.6283224514649));
#221454=CARTESIAN_POINT('Ctrl Pts',(-22.5675364832698,86.8995247109982,
74.1992222599948));
#221455=CARTESIAN_POINT('Ctrl Pts',(-22.5675364832698,86.6763715914487,
75.321931358547));
#221456=CARTESIAN_POINT('Ctrl Pts',(-22.5675364832709,86.5248895569673,
75.8722213989229));
#221457=CARTESIAN_POINT('Ctrl Pts',(-22.5675364832709,86.3349224103826,
76.4088722773807));
#221458=CARTESIAN_POINT('Ctrl Pts',(-22.5673477912806,86.9996280326377,
73.0560066204832));
#221459=CARTESIAN_POINT('Ctrl Pts',(-22.5674106883502,86.999721811328,73.0504855961939));
#221460=CARTESIAN_POINT('Ctrl Pts',(-22.5674735854198,86.9998117796859,
73.0449644637686));
#221461=CARTESIAN_POINT('Ctrl Pts',(-22.5675364824894,86.9998979375059,
73.039443228467));
#221462=CARTESIAN_POINT('Origin',(-21.7675364832709,75.,72.9888893865801));
#221463=CARTESIAN_POINT('',(-23.0675424572509,84.7043582237312,76.9983072327893));
#221464=CARTESIAN_POINT('',(-23.0675424572509,65.2956417762688,68.9794715403709));
#221465=CARTESIAN_POINT('Origin',(-23.0675424572509,75.,72.9888893865801));
#221466=CARTESIAN_POINT('',(-38.5675364832709,84.7043582237312,76.9983072327893));
#221467=CARTESIAN_POINT('',(-21.7675364832709,84.7043582237312,76.9983072327893));
#221468=CARTESIAN_POINT('Origin',(-38.5675364832709,75.,72.9888893865801));
#221469=CARTESIAN_POINT('Origin',(-23.0675424572509,75.,72.9888893865801));
#221470=CARTESIAN_POINT('Origin',(-22.8175393993109,75.,72.9888893865801));
#221471=CARTESIAN_POINT('',(-22.5675364832709,64.8335236965284,68.7885444915902));
#221472=CARTESIAN_POINT('',(-22.8175393993109,65.0645826708248,68.8840079888883));
#221473=CARTESIAN_POINT('Origin',(-22.5675364832709,75.,72.9888893865801));
#221474=CARTESIAN_POINT('Origin',(-22.5675364832709,75.,72.9888893865801));
#221475=CARTESIAN_POINT('Origin',(-38.5675364832709,75.,72.9888893865801));
#221476=CARTESIAN_POINT('Origin',(-48.5675364832709,66.6819786653733,69.5522455184007));
#221477=CARTESIAN_POINT('',(-48.5675364832709,73.8447192590797,72.5115777382218));
#221478=CARTESIAN_POINT('Origin',(-48.5675364832709,66.6819786653733,69.5522455184007));
#221479=CARTESIAN_POINT('Origin',(-47.7675364832709,66.6819786653733,69.5522455184007));
#221480=CARTESIAN_POINT('',(-64.0675410045048,73.8447192590797,72.5115777382218));
#221481=CARTESIAN_POINT('',(-47.7675364832709,73.8447192590797,72.5115777382218));
#221482=CARTESIAN_POINT('Origin',(-64.0675410045048,66.6819786653733,69.5522455184007));
#221483=CARTESIAN_POINT('Origin',(-64.3175392245649,66.6819786653733,69.5522455184007));
#221484=CARTESIAN_POINT('',(-64.5675367041793,74.3068269192978,72.70250048211));
#221485=CARTESIAN_POINT('',(-64.3175392245649,74.075773247593,72.6070391756116));
#221486=CARTESIAN_POINT('Origin',(-64.5675367039552,66.6819786653733,69.5522455184007));
#221487=CARTESIAN_POINT('Origin',(-64.5675364832709,66.6819786653733,69.5522455184007));
#221488=CARTESIAN_POINT('Ctrl Pts',(-64.5675364832709,57.6609583680643,
70.6705889999386));
#221489=CARTESIAN_POINT('Ctrl Pts',(-64.5675364832709,57.6884511920649,
71.1096763190363));
#221490=CARTESIAN_POINT('Ctrl Pts',(-64.5675364832708,57.7483094871617,
71.5466701563318));
#221491=CARTESIAN_POINT('Ctrl Pts',(-64.5675364832708,57.9303798077129,
72.41066731052));
#221492=CARTESIAN_POINT('Ctrl Pts',(-64.5675364832709,58.0530241033855,
72.8375946044308));
#221493=CARTESIAN_POINT('Ctrl Pts',(-64.5675364832709,58.2054611415104,
73.2535681280901));
#221494=CARTESIAN_POINT('Origin',(-45.8894114130409,66.6819786653733,69.5522455184007));
#221495=CARTESIAN_POINT('',(-63.5674079539854,63.4392572871834,59.8285649416409));
#221496=CARTESIAN_POINT('Ctrl Pts',(-63.567539947994,63.4350769493012,59.8300991896842));
#221497=CARTESIAN_POINT('Ctrl Pts',(-63.5674959499171,63.4364702751625,
59.8295874742253));
#221498=CARTESIAN_POINT('Ctrl Pts',(-63.5674519518401,63.4378637211896,
59.8290760582624));
#221499=CARTESIAN_POINT('Ctrl Pts',(-63.5674079537632,63.4392572872537,
59.8285649418516));
#221500=CARTESIAN_POINT('',(-62.9075072593131,76.1552860519195,73.46618818022));
#221501=CARTESIAN_POINT('Ctrl Pts',(-63.5674123768639,63.4393239295404,
59.8286818576752));
#221502=CARTESIAN_POINT('Ctrl Pts',(-63.5537244696136,63.8950358571431,
59.6767091353507));
#221503=CARTESIAN_POINT('Ctrl Pts',(-63.5400136073417,64.3608717030263,
59.5569597714857));
#221504=CARTESIAN_POINT('Ctrl Pts',(-63.5129296748257,65.3050981973121,
59.3838289856031));
#221505=CARTESIAN_POINT('Ctrl Pts',(-63.4995889539748,65.7823014895405,
59.330549021255));
#221506=CARTESIAN_POINT('Ctrl Pts',(-63.4597780386861,67.2123915236249,
59.2718310830067));
#221507=CARTESIAN_POINT('Ctrl Pts',(-63.4325802602361,68.1641190178407,
59.3654163782555));
#221508=CARTESIAN_POINT('Ctrl Pts',(-63.3869424607676,69.7331885825598,
59.744516418622));
#221509=CARTESIAN_POINT('Ctrl Pts',(-63.3686283032081,70.3605758197365,
59.9621800299818));
#221510=CARTESIAN_POINT('Ctrl Pts',(-63.3128692356676,72.1773044290275,
60.7971770385974));
#221511=CARTESIAN_POINT('Ctrl Pts',(-63.2745815754463,73.2711609789934,
61.587793568521));
#221512=CARTESIAN_POINT('Ctrl Pts',(-63.2002097006855,75.093653850845,63.5444294238347));
#221513=CARTESIAN_POINT('Ctrl Pts',(-63.1618824850836,75.8047677283667,
64.6917037744082));
#221514=CARTESIAN_POINT('Ctrl Pts',(-63.1061663303517,76.5088612625986,
66.563278327776));
#221515=CARTESIAN_POINT('Ctrl Pts',(-63.0878060649445,76.6814853170575,
67.2046067609666));
#221516=CARTESIAN_POINT('Ctrl Pts',(-63.0553782680594,76.8696372913774,
68.3273127282598));
#221517=CARTESIAN_POINT('Ctrl Pts',(-63.0417928519769,76.9155090722919,
68.8014397964858));
#221518=CARTESIAN_POINT('Ctrl Pts',(-63.0081560309446,76.9474973885907,
69.9923893239148));
#221519=CARTESIAN_POINT('Ctrl Pts',(-62.9884692522367,76.8917445355874,
70.7077860596408));
#221520=CARTESIAN_POINT('Ctrl Pts',(-62.9483777816462,76.6320462074141,
72.1157259528595));
#221521=CARTESIAN_POINT('Ctrl Pts',(-62.9277656193976,76.4287171030932,
72.8043756242868));
#221522=CARTESIAN_POINT('Ctrl Pts',(-62.9075072593131,76.1552860519195,
73.46618818022));
#221523=CARTESIAN_POINT('Ctrl Pts',(-62.9075072593131,76.1552860519195,
73.46618818022));
#221524=CARTESIAN_POINT('Ctrl Pts',(-62.9075071281503,76.1552842815894,
73.4661924651273));
#221525=CARTESIAN_POINT('Ctrl Pts',(-62.9075069969875,76.1552825112564,
73.4661967500333));
#221526=CARTESIAN_POINT('Ctrl Pts',(-62.9075068658247,76.1552807409205,
73.4662010349381));
#221527=CARTESIAN_POINT('Ctrl Pts',(-64.7235137149846,58.9641128133577,
74.2288240611484));
#221528=CARTESIAN_POINT('Ctrl Pts',(-64.6818903153503,58.2898823562254,
73.1161259264028));
#221529=CARTESIAN_POINT('Ctrl Pts',(-64.5986435160818,57.4306928818431,
70.5953071644979));
#221530=CARTESIAN_POINT('Ctrl Pts',(-64.4737733171789,57.8453681147118,
66.6213799744606));
#221531=CARTESIAN_POINT('Ctrl Pts',(-64.3489031182761,59.8875902288061,
63.1873940424807));
#221532=CARTESIAN_POINT('Ctrl Pts',(-64.2240329193733,63.1811176368601,
60.9255881378499));
#221533=CARTESIAN_POINT('Ctrl Pts',(-64.0991627204705,67.1194100886389,
60.2525763176752));
#221534=CARTESIAN_POINT('Ctrl Pts',(-63.9742925215677,70.9771383669053,
61.2922934738364));
#221535=CARTESIAN_POINT('Ctrl Pts',(-63.8494223226649,74.0438220518638,
63.8532574547353));
#221536=CARTESIAN_POINT('Ctrl Pts',(-63.7245521237622,75.7546654243016,
67.4638112038693));
#221537=CARTESIAN_POINT('Ctrl Pts',(-63.5996819248594,75.7945804349819,
71.4589945804267));
#221538=CARTESIAN_POINT('Ctrl Pts',(-63.4748117259569,74.1562158093098,
75.103009768157));
#221539=CARTESIAN_POINT('Ctrl Pts',(-63.3499415270539,71.1413113950972,
77.7247325999806));
#221540=CARTESIAN_POINT('Ctrl Pts',(-63.2250713281509,67.305125597119,78.8413215436999));
#221541=CARTESIAN_POINT('Ctrl Pts',(-63.1002011292489,63.3541752639937,
78.2471160211359));
#221542=CARTESIAN_POINT('Ctrl Pts',(-62.9753309303459,60.0161061500815,
76.0516149086199));
#221543=CARTESIAN_POINT('Ctrl Pts',(-62.8504607314429,57.9057165985323,
72.6589303077136));
#221544=CARTESIAN_POINT('Ctrl Pts',(-62.7672139321749,57.5763043356606,
70.0161625645473));
#221545=CARTESIAN_POINT('Ctrl Pts',(-62.7255905325409,57.6961945356714,
68.7206664478601));
#221546=CARTESIAN_POINT('Ctrl Pts',(-64.4993856047086,58.5958913594194,
74.4519448802346));
#221547=CARTESIAN_POINT('Ctrl Pts',(-64.4577622050742,57.8894931859754,
73.2861596184455));
#221548=CARTESIAN_POINT('Ctrl Pts',(-64.3745154058057,56.9893115508722,
70.6450719159537));
#221549=CARTESIAN_POINT('Ctrl Pts',(-64.2496452069029,57.4237710505392,
66.4815475917032));
#221550=CARTESIAN_POINT('Ctrl Pts',(-64.1247750080001,59.5634281305272,
62.8837252680371));
#221551=CARTESIAN_POINT('Ctrl Pts',(-63.9999048090973,63.0140906163541,
60.5140079958519));
#221552=CARTESIAN_POINT('Ctrl Pts',(-63.8750346101945,67.1402800594054,
59.8088866008654));
#221553=CARTESIAN_POINT('Ctrl Pts',(-63.7501644112917,71.1820615905698,
60.8982089419637));
#221554=CARTESIAN_POINT('Ctrl Pts',(-63.6252942123889,74.395057578295,63.58135720264));
#221555=CARTESIAN_POINT('Ctrl Pts',(-63.5004240134859,76.1875257478145,
67.3641714414642));
#221556=CARTESIAN_POINT('Ctrl Pts',(-63.3755538145829,76.2293451143814,
71.5499660906056));
#221557=CARTESIAN_POINT('Ctrl Pts',(-63.2506836156809,74.5128136721155,
75.3678382222558));
#221558=CARTESIAN_POINT('Ctrl Pts',(-63.1258134167779,71.3540673580585,
78.1146441549625));
#221559=CARTESIAN_POINT('Ctrl Pts',(-63.0009432178749,67.3348561047015,
79.2845058572659));
#221560=CARTESIAN_POINT('Ctrl Pts',(-62.8760730189729,63.1954048693821,
78.6619506295289));
#221561=CARTESIAN_POINT('Ctrl Pts',(-62.7512028200699,59.6980755809505,
76.3617015689027));
#221562=CARTESIAN_POINT('Ctrl Pts',(-62.6263326211669,57.4869987767368,
72.8071510739182));
#221563=CARTESIAN_POINT('Ctrl Pts',(-62.5430858218989,57.1418701662744,
70.0382961714914));
#221564=CARTESIAN_POINT('Ctrl Pts',(-62.5014624222649,57.2674803599551,
68.6809915869218));
#221565=CARTESIAN_POINT('Ctrl Pts',(-64.2752574944325,58.2276699054746,
74.6750656993105));
#221566=CARTESIAN_POINT('Ctrl Pts',(-64.2336340947982,57.4891040157201,
73.4561933104751));
#221567=CARTESIAN_POINT('Ctrl Pts',(-64.1503872955297,56.5479302198967,
70.6948366673945));
#221568=CARTESIAN_POINT('Ctrl Pts',(-64.0255170966268,57.0021739863718,
66.341715208933));
#221569=CARTESIAN_POINT('Ctrl Pts',(-63.900646897724,59.2392660322718,62.5800564935892));
#221570=CARTESIAN_POINT('Ctrl Pts',(-63.7757766988212,62.8470635958519,
60.1024278538446));
#221571=CARTESIAN_POINT('Ctrl Pts',(-63.6509064999184,67.161150030173,59.3651968840528));
#221572=CARTESIAN_POINT('Ctrl Pts',(-63.5260363010159,71.3869848142425,
60.5041244100999));
#221573=CARTESIAN_POINT('Ctrl Pts',(-63.4011661021129,74.7462931047338,
63.3094569505521));
#221574=CARTESIAN_POINT('Ctrl Pts',(-63.2762959032099,76.6203860713289,
67.2645316790695));
#221575=CARTESIAN_POINT('Ctrl Pts',(-63.1514257043069,76.6641097937791,
71.6409376007935));
#221576=CARTESIAN_POINT('Ctrl Pts',(-63.0265555054049,74.8694115349166,
75.6326666763602));
#221577=CARTESIAN_POINT('Ctrl Pts',(-62.9016853065019,71.5668233210142,
78.5045557099475));
#221578=CARTESIAN_POINT('Ctrl Pts',(-62.7768151075989,67.3645866122776,
79.7276901708313));
#221579=CARTESIAN_POINT('Ctrl Pts',(-62.6519449086969,63.0366344747639,
79.0767852379246));
#221580=CARTESIAN_POINT('Ctrl Pts',(-62.5270747097939,59.3800450118199,
76.6717882291846));
#221581=CARTESIAN_POINT('Ctrl Pts',(-62.4022045108909,57.0682809549513,
72.9553718401247));
#221582=CARTESIAN_POINT('Ctrl Pts',(-62.3189577116229,56.707435996897,70.0604297784402));
#221583=CARTESIAN_POINT('Ctrl Pts',(-62.2773343119879,56.8387661842384,
68.6413167259844));
#221584=CARTESIAN_POINT('Ctrl Pts',(-64.0511293841564,57.8594484515271,
74.8981865183928));
#221585=CARTESIAN_POINT('Ctrl Pts',(-64.0095059845222,57.088714845479,73.6262270025225));
#221586=CARTESIAN_POINT('Ctrl Pts',(-63.9262591852536,56.1065488889258,
70.7446014188502));
#221587=CARTESIAN_POINT('Ctrl Pts',(-63.8013889863508,56.5805769221993,
66.2018828261753));
#221588=CARTESIAN_POINT('Ctrl Pts',(-63.676518787448,58.9151039339933,62.2763877191448));
#221589=CARTESIAN_POINT('Ctrl Pts',(-63.5516485885449,62.680036575337,59.6908477118419));
#221590=CARTESIAN_POINT('Ctrl Pts',(-63.4267783896419,67.182020000941,58.9215071672393));
#221591=CARTESIAN_POINT('Ctrl Pts',(-63.3019081907399,71.5919080379106,
60.1100398782212));
#221592=CARTESIAN_POINT('Ctrl Pts',(-63.1770379918369,75.0975286311649,
63.0375566984567));
#221593=CARTESIAN_POINT('Ctrl Pts',(-63.0521677929339,77.0532463948415,
67.1648919166655));
#221594=CARTESIAN_POINT('Ctrl Pts',(-62.9272975940309,77.0988744731788,
71.7319091109725));
#221595=CARTESIAN_POINT('Ctrl Pts',(-62.8024273951289,75.2260093977218,
75.8974951304588));
#221596=CARTESIAN_POINT('Ctrl Pts',(-62.6775571962259,71.7795792839757,
78.8944672649294));
#221597=CARTESIAN_POINT('Ctrl Pts',(-62.5526869973229,67.3943171198596,
80.170874484396));
#221598=CARTESIAN_POINT('Ctrl Pts',(-62.4278167984199,62.8778640801542,
79.491619846313));
#221599=CARTESIAN_POINT('Ctrl Pts',(-62.3029465995179,59.0620144426885,
76.9818748894683));
#221600=CARTESIAN_POINT('Ctrl Pts',(-62.1780764006149,56.6495631331558,
73.1035926063292));
#221601=CARTESIAN_POINT('Ctrl Pts',(-62.0948296013469,56.2730018275201,
70.0825633853882));
#221602=CARTESIAN_POINT('Ctrl Pts',(-62.0532062017119,56.410052008522,68.6016418650461));
#221603=CARTESIAN_POINT('Origin',(-113.778845940191,66.6819786653733,69.5522455184007));
#221604=CARTESIAN_POINT('',(-47.1840596451118,61.3985627647214,74.6727879441187));
#221605=CARTESIAN_POINT('Ctrl Pts',(-47.1840596451125,61.3985627647224,
74.6727879441184));
#221606=CARTESIAN_POINT('Ctrl Pts',(-47.1330608433754,61.0554912975567,
73.6555434581613));
#221607=CARTESIAN_POINT('Ctrl Pts',(-47.0897582262311,60.8615439161923,
72.5407972914318));
#221608=CARTESIAN_POINT('Ctrl Pts',(-47.0209270037,60.8476294176321,70.0468757692862));
#221609=CARTESIAN_POINT('Ctrl Pts',(-47.002286125824,61.1325740255311,68.6660964641816));
#221610=CARTESIAN_POINT('Ctrl Pts',(-47.002286125824,62.1277464170818,66.2573903246842));
#221611=CARTESIAN_POINT('Ctrl Pts',(-47.021100980925,62.9050951362454,65.0734714286778));
#221612=CARTESIAN_POINT('Ctrl Pts',(-47.0902140976192,64.6780140493426,
63.3201249465718));
#221613=CARTESIAN_POINT('Ctrl Pts',(-47.1333057957547,65.5971180331206,
62.671905978486));
#221614=CARTESIAN_POINT('Ctrl Pts',(-47.1840596451125,66.5535285669908,
62.1957559421795));
#221615=CARTESIAN_POINT('Origin',(-113.778845940191,64.1044957642388,75.7907615193708));
#221616=CARTESIAN_POINT('Origin',(-113.778845940191,66.6819786653733,69.5522455184007));
#221617=CARTESIAN_POINT('Origin',(-51.8559251551109,68.8530468966737,77.752655878079));
#221618=CARTESIAN_POINT('',(-47.1840596451109,61.3985627647217,74.6727879441188));
#221619=CARTESIAN_POINT('Origin',(-51.5615184913109,70.415046688923,71.0945865171214));
#221620=CARTESIAN_POINT('',(0.,0.,0.));
#221621=CARTESIAN_POINT('',(0.,0.,0.));
#221622=CARTESIAN_POINT('',(0.,0.,0.));
#221623=CARTESIAN_POINT('',(0.,0.,0.));
#221624=CARTESIAN_POINT('',(0.,0.,0.));
#221625=CARTESIAN_POINT('',(0.,0.,0.));
#221626=CARTESIAN_POINT('',(0.,0.,0.));
#221627=CARTESIAN_POINT('',(0.,0.,0.));
#221628=CARTESIAN_POINT('',(0.,0.,0.));
#221629=CARTESIAN_POINT('',(0.,0.,0.));
#221630=CARTESIAN_POINT('',(0.,0.,0.));
#221631=CARTESIAN_POINT('',(0.,0.,0.));
#221632=CARTESIAN_POINT('',(0.,0.,0.));
#221633=UNCERTAINTY_MEASURE_WITH_UNIT(LENGTH_MEASURE(0.01),#221663,
'DISTANCE_ACCURACY_VALUE',
'Maximum model space distance between geometric entities at asserted c
onnectivities');
#221634=UNCERTAINTY_MEASURE_WITH_UNIT(LENGTH_MEASURE(0.01),#221663,
'DISTANCE_ACCURACY_VALUE',
'Maximum model space distance between geometric entities at asserted c
onnectivities');
#221635=UNCERTAINTY_MEASURE_WITH_UNIT(LENGTH_MEASURE(0.01),#221663,
'DISTANCE_ACCURACY_VALUE',
'Maximum model space distance between geometric entities at asserted c
onnectivities');
#221636=UNCERTAINTY_MEASURE_WITH_UNIT(LENGTH_MEASURE(0.01),#221663,
'DISTANCE_ACCURACY_VALUE',
'Maximum model space distance between geometric entities at asserted c
onnectivities');
#221637=UNCERTAINTY_MEASURE_WITH_UNIT(LENGTH_MEASURE(0.01),#221663,
'DISTANCE_ACCURACY_VALUE',
'Maximum model space distance between geometric entities at asserted c
onnectivities');
#221638=UNCERTAINTY_MEASURE_WITH_UNIT(LENGTH_MEASURE(0.01),#221663,
'DISTANCE_ACCURACY_VALUE',
'Maximum model space distance between geometric entities at asserted c
onnectivities');
#221639=UNCERTAINTY_MEASURE_WITH_UNIT(LENGTH_MEASURE(0.01),#221663,
'DISTANCE_ACCURACY_VALUE',
'Maximum model space distance between geometric entities at asserted c
onnectivities');
#221640=UNCERTAINTY_MEASURE_WITH_UNIT(LENGTH_MEASURE(0.01),#221663,
'DISTANCE_ACCURACY_VALUE',
'Maximum model space distance between geometric entities at asserted c
onnectivities');
#221641=UNCERTAINTY_MEASURE_WITH_UNIT(LENGTH_MEASURE(0.01),#221663,
'DISTANCE_ACCURACY_VALUE',
'Maximum model space distance between geometric entities at asserted c
onnectivities');
#221642=UNCERTAINTY_MEASURE_WITH_UNIT(LENGTH_MEASURE(0.01),#221663,
'DISTANCE_ACCURACY_VALUE',
'Maximum model space distance between geometric entities at asserted c
onnectivities');
#221643=UNCERTAINTY_MEASURE_WITH_UNIT(LENGTH_MEASURE(0.01),#221663,
'DISTANCE_ACCURACY_VALUE',
'Maximum model space distance between geometric entities at asserted c
onnectivities');
#221644=UNCERTAINTY_MEASURE_WITH_UNIT(LENGTH_MEASURE(0.01),#221663,
'DISTANCE_ACCURACY_VALUE',
'Maximum model space distance between geometric entities at asserted c
onnectivities');
#221645=UNCERTAINTY_MEASURE_WITH_UNIT(LENGTH_MEASURE(0.01),#221663,
'DISTANCE_ACCURACY_VALUE',
'Maximum model space distance between geometric entities at asserted c
onnectivities');
#221646=UNCERTAINTY_MEASURE_WITH_UNIT(LENGTH_MEASURE(0.01),#221663,
'DISTANCE_ACCURACY_VALUE',
'Maximum model space distance between geometric entities at asserted c
onnectivities');
#221647=UNCERTAINTY_MEASURE_WITH_UNIT(LENGTH_MEASURE(0.01),#221663,
'DISTANCE_ACCURACY_VALUE',
'Maximum model space distance between geometric entities at asserted c
onnectivities');
#221648=(
GEOMETRIC_REPRESENTATION_CONTEXT(3)
GLOBAL_UNCERTAINTY_ASSIGNED_CONTEXT((#221633))
GLOBAL_UNIT_ASSIGNED_CONTEXT((#221663,#221665,#221666))
REPRESENTATION_CONTEXT('','3D')
);
#221649=(
GEOMETRIC_REPRESENTATION_CONTEXT(3)
GLOBAL_UNCERTAINTY_ASSIGNED_CONTEXT((#221634))
GLOBAL_UNIT_ASSIGNED_CONTEXT((#221663,#221665,#221666))
REPRESENTATION_CONTEXT('','3D')
);
#221650=(
GEOMETRIC_REPRESENTATION_CONTEXT(3)
GLOBAL_UNCERTAINTY_ASSIGNED_CONTEXT((#221635))
GLOBAL_UNIT_ASSIGNED_CONTEXT((#221663,#221665,#221666))
REPRESENTATION_CONTEXT('','3D')
);
#221651=(
GEOMETRIC_REPRESENTATION_CONTEXT(3)
GLOBAL_UNCERTAINTY_ASSIGNED_CONTEXT((#221636))
GLOBAL_UNIT_ASSIGNED_CONTEXT((#221663,#221665,#221666))
REPRESENTATION_CONTEXT('','3D')
);
#221652=(
GEOMETRIC_REPRESENTATION_CONTEXT(3)
GLOBAL_UNCERTAINTY_ASSIGNED_CONTEXT((#221637))
GLOBAL_UNIT_ASSIGNED_CONTEXT((#221663,#221665,#221666))
REPRESENTATION_CONTEXT('','3D')
);
#221653=(
GEOMETRIC_REPRESENTATION_CONTEXT(3)
GLOBAL_UNCERTAINTY_ASSIGNED_CONTEXT((#221638))
GLOBAL_UNIT_ASSIGNED_CONTEXT((#221663,#221665,#221666))
REPRESENTATION_CONTEXT('','3D')
);
#221654=(
GEOMETRIC_REPRESENTATION_CONTEXT(3)
GLOBAL_UNCERTAINTY_ASSIGNED_CONTEXT((#221639))
GLOBAL_UNIT_ASSIGNED_CONTEXT((#221663,#221665,#221666))
REPRESENTATION_CONTEXT('','3D')
);
#221655=(
GEOMETRIC_REPRESENTATION_CONTEXT(3)
GLOBAL_UNCERTAINTY_ASSIGNED_CONTEXT((#221640))
GLOBAL_UNIT_ASSIGNED_CONTEXT((#221663,#221665,#221666))
REPRESENTATION_CONTEXT('','3D')
);
#221656=(
GEOMETRIC_REPRESENTATION_CONTEXT(3)
GLOBAL_UNCERTAINTY_ASSIGNED_CONTEXT((#221641))
GLOBAL_UNIT_ASSIGNED_CONTEXT((#221663,#221665,#221666))
REPRESENTATION_CONTEXT('','3D')
);
#221657=(
GEOMETRIC_REPRESENTATION_CONTEXT(3)
GLOBAL_UNCERTAINTY_ASSIGNED_CONTEXT((#221642))
GLOBAL_UNIT_ASSIGNED_CONTEXT((#221663,#221665,#221666))
REPRESENTATION_CONTEXT('','3D')
);
#221658=(
GEOMETRIC_REPRESENTATION_CONTEXT(3)
GLOBAL_UNCERTAINTY_ASSIGNED_CONTEXT((#221643))
GLOBAL_UNIT_ASSIGNED_CONTEXT((#221663,#221665,#221666))
REPRESENTATION_CONTEXT('','3D')
);
#221659=(
GEOMETRIC_REPRESENTATION_CONTEXT(3)
GLOBAL_UNCERTAINTY_ASSIGNED_CONTEXT((#221644))
GLOBAL_UNIT_ASSIGNED_CONTEXT((#221663,#221665,#221666))
REPRESENTATION_CONTEXT('','3D')
);
#221660=(
GEOMETRIC_REPRESENTATION_CONTEXT(3)
GLOBAL_UNCERTAINTY_ASSIGNED_CONTEXT((#221645))
GLOBAL_UNIT_ASSIGNED_CONTEXT((#221663,#221665,#221666))
REPRESENTATION_CONTEXT('','3D')
);
#221661=(
GEOMETRIC_REPRESENTATION_CONTEXT(3)
GLOBAL_UNCERTAINTY_ASSIGNED_CONTEXT((#221646))
GLOBAL_UNIT_ASSIGNED_CONTEXT((#221663,#221665,#221666))
REPRESENTATION_CONTEXT('','3D')
);
#221662=(
GEOMETRIC_REPRESENTATION_CONTEXT(3)
GLOBAL_UNCERTAINTY_ASSIGNED_CONTEXT((#221647))
GLOBAL_UNIT_ASSIGNED_CONTEXT((#221663,#221665,#221666))
REPRESENTATION_CONTEXT('','3D')
);
#221663=(
LENGTH_UNIT()
NAMED_UNIT(*)
SI_UNIT(.MILLI.,.METRE.)
);
#221664=(
LENGTH_UNIT()
NAMED_UNIT(*)
SI_UNIT($,.METRE.)
);
#221665=(
NAMED_UNIT(*)
PLANE_ANGLE_UNIT()
SI_UNIT($,.RADIAN.)
);
#221666=(
NAMED_UNIT(*)
SI_UNIT($,.STERADIAN.)
SOLID_ANGLE_UNIT()
);
#221667=SHAPE_DEFINITION_REPRESENTATION(#221681,#221708);
#221668=SHAPE_DEFINITION_REPRESENTATION(#221682,#221709);
#221669=SHAPE_DEFINITION_REPRESENTATION(#221683,#221710);
#221670=SHAPE_DEFINITION_REPRESENTATION(#221684,#221711);
#221671=SHAPE_DEFINITION_REPRESENTATION(#221685,#221712);
#221672=SHAPE_DEFINITION_REPRESENTATION(#221686,#221713);
#221673=SHAPE_DEFINITION_REPRESENTATION(#221687,#221714);
#221674=SHAPE_DEFINITION_REPRESENTATION(#221688,#221715);
#221675=SHAPE_DEFINITION_REPRESENTATION(#221689,#221716);
#221676=SHAPE_DEFINITION_REPRESENTATION(#221690,#221717);
#221677=SHAPE_DEFINITION_REPRESENTATION(#221691,#221718);
#221678=SHAPE_DEFINITION_REPRESENTATION(#221692,#221719);
#221679=SHAPE_DEFINITION_REPRESENTATION(#221693,#221720);
#221680=SHAPE_DEFINITION_REPRESENTATION(#221694,#221721);
#221681=PRODUCT_DEFINITION_SHAPE('',$,#221723);
#221682=PRODUCT_DEFINITION_SHAPE('',$,#221724);
#221683=PRODUCT_DEFINITION_SHAPE('',$,#221725);
#221684=PRODUCT_DEFINITION_SHAPE('',$,#221726);
#221685=PRODUCT_DEFINITION_SHAPE('',$,#221727);
#221686=PRODUCT_DEFINITION_SHAPE('',$,#221728);
#221687=PRODUCT_DEFINITION_SHAPE('',$,#221729);
#221688=PRODUCT_DEFINITION_SHAPE('',$,#221730);
#221689=PRODUCT_DEFINITION_SHAPE('',$,#221731);
#221690=PRODUCT_DEFINITION_SHAPE('',$,#221732);
#221691=PRODUCT_DEFINITION_SHAPE('',$,#221733);
#221692=PRODUCT_DEFINITION_SHAPE('',$,#221734);
#221693=PRODUCT_DEFINITION_SHAPE('',$,#221735);
#221694=PRODUCT_DEFINITION_SHAPE('',$,#221736);
#221695=PRODUCT_DEFINITION_SHAPE($,$,#50);
#221696=PRODUCT_DEFINITION_SHAPE($,$,#51);
#221697=PRODUCT_DEFINITION_SHAPE($,$,#52);
#221698=PRODUCT_DEFINITION_SHAPE($,$,#53);
#221699=PRODUCT_DEFINITION_SHAPE($,$,#54);
#221700=PRODUCT_DEFINITION_SHAPE($,$,#55);
#221701=PRODUCT_DEFINITION_SHAPE($,$,#56);
#221702=PRODUCT_DEFINITION_SHAPE($,$,#57);
#221703=PRODUCT_DEFINITION_SHAPE($,$,#58);
#221704=PRODUCT_DEFINITION_SHAPE($,$,#59);
#221705=PRODUCT_DEFINITION_SHAPE($,$,#60);
#221706=PRODUCT_DEFINITION_SHAPE($,$,#61);
#221707=PRODUCT_DEFINITION_SHAPE($,$,#62);
#221708=SHAPE_REPRESENTATION('',(#79482,#86151,#86152,#86153,#86154,#86155,
#86156,#86157,#86158,#86159,#86160,#86161,#86162,#86163),#221648);
#221709=SHAPE_REPRESENTATION('',(#79483),#221649);
#221710=SHAPE_REPRESENTATION('',(#80379),#221650);
#221711=SHAPE_REPRESENTATION('',(#80522),#221651);
#221712=SHAPE_REPRESENTATION('',(#80620),#221652);
#221713=SHAPE_REPRESENTATION('',(#80667),#221653);
#221714=SHAPE_REPRESENTATION('',(#80719),#221654);
#221715=SHAPE_REPRESENTATION('',(#80766),#221655);
#221716=SHAPE_REPRESENTATION('',(#80796),#221656);
#221717=SHAPE_REPRESENTATION('',(#80848),#221657);
#221718=SHAPE_REPRESENTATION('',(#80951),#221658);
#221719=SHAPE_REPRESENTATION('',(#80981),#221659);
#221720=SHAPE_REPRESENTATION('',(#85967),#221660);
#221721=SHAPE_REPRESENTATION('',(#86059),#221661);
#221722=PRODUCT_DEFINITION_CONTEXT('part definition',#221766,'design');
#221723=PRODUCT_DEFINITION('X11134','MAS-607',#221737,#221722);
#221724=PRODUCT_DEFINITION('2026-10-05-23-02-19-012','Valve Body',#221738,
#221722);
#221725=PRODUCT_DEFINITION('2026-10-05-23-02-27-655','Control Handle',#221739,
#221722);
#221726=PRODUCT_DEFINITION('2026-10-05-23-02-30-143',
'Shower Hose Connector',#221740,#221722);
#221727=PRODUCT_DEFINITION('2026-10-05-23-02-32-151','Gasket (1)',#221741,
#221722);
#221728=PRODUCT_DEFINITION('2026-10-05-23-02-34-900','Coupling Nut',#221742,
#221722);
#221729=PRODUCT_DEFINITION('2026-10-05-23-02-36-870','Gasket',#221743,#221722);
#221730=PRODUCT_DEFINITION('2026-10-05-23-02-39-335',
'Wall Flange Rosette',#221744,#221722);
#221731=PRODUCT_DEFINITION('2026-10-05-23-02-40-799','Coupling Nut (1)',
#221745,#221722);
#221732=PRODUCT_DEFINITION('2026-10-05-23-02-42-253','Diverter',#221746,
#221722);
#221733=PRODUCT_DEFINITION('2026-10-05-23-02-44-166',
'Wall Flange Rosette (1)',#221747,#221722);
#221734=PRODUCT_DEFINITION('2026-10-05-23-02-46-115','Aerator',#221748,
#221722);
#221735=PRODUCT_DEFINITION('2026-10-05-23-02-49-354',
'Eccentric Connector (1)',#221749,#221722);
#221736=PRODUCT_DEFINITION('2026-10-05-23-03-42-219',
'Eccentric Connector',#221750,#221722);
#221737=PRODUCT_DEFINITION_FORMATION('',$,#221768);
#221738=PRODUCT_DEFINITION_FORMATION('',$,#221769);
#221739=PRODUCT_DEFINITION_FORMATION('',$,#221770);
#221740=PRODUCT_DEFINITION_FORMATION('',$,#221771);
#221741=PRODUCT_DEFINITION_FORMATION('',$,#221772);
#221742=PRODUCT_DEFINITION_FORMATION('',$,#221773);
#221743=PRODUCT_DEFINITION_FORMATION('',$,#221774);
#221744=PRODUCT_DEFINITION_FORMATION('',$,#221775);
#221745=PRODUCT_DEFINITION_FORMATION('',$,#221776);
#221746=PRODUCT_DEFINITION_FORMATION('',$,#221777);
#221747=PRODUCT_DEFINITION_FORMATION('',$,#221778);
#221748=PRODUCT_DEFINITION_FORMATION('',$,#221779);
#221749=PRODUCT_DEFINITION_FORMATION('',$,#221780);
#221750=PRODUCT_DEFINITION_FORMATION('',$,#221781);
#221751=PRODUCT_RELATED_PRODUCT_CATEGORY('MAS-607','MAS-607',(#221768));
#221752=PRODUCT_RELATED_PRODUCT_CATEGORY('Valve Body','Valve Body',(#221769));
#221753=PRODUCT_RELATED_PRODUCT_CATEGORY('Control Handle',
'Control Handle',(#221770));
#221754=PRODUCT_RELATED_PRODUCT_CATEGORY('Shower Hose Connector',
'Shower Hose Connector',(#221771));
#221755=PRODUCT_RELATED_PRODUCT_CATEGORY('Gasket (1)','Gasket (1)',(#221772));
#221756=PRODUCT_RELATED_PRODUCT_CATEGORY('Coupling Nut','Coupling Nut',
(#221773));
#221757=PRODUCT_RELATED_PRODUCT_CATEGORY('Gasket','Gasket',(#221774));
#221758=PRODUCT_RELATED_PRODUCT_CATEGORY('Wall Flange Rosette',
'Wall Flange Rosette',(#221775));
#221759=PRODUCT_RELATED_PRODUCT_CATEGORY('Coupling Nut (1)',
'Coupling Nut (1)',(#221776));
#221760=PRODUCT_RELATED_PRODUCT_CATEGORY('Diverter','Diverter',(#221777));
#221761=PRODUCT_RELATED_PRODUCT_CATEGORY('Wall Flange Rosette (1)',
'Wall Flange Rosette (1)',(#221778));
#221762=PRODUCT_RELATED_PRODUCT_CATEGORY('Aerator','Aerator',(#221779));
#221763=PRODUCT_RELATED_PRODUCT_CATEGORY('Eccentric Connector (1)',
'Eccentric Connector (1)',(#221780));
#221764=PRODUCT_RELATED_PRODUCT_CATEGORY('Eccentric Connector',
'Eccentric Connector',(#221781));
#221765=APPLICATION_PROTOCOL_DEFINITION('international standard',
'automotive_design',2009,#221766);
#221766=APPLICATION_CONTEXT(
'Core Data for Automotive Mechanical Design Process');
#221767=PRODUCT_CONTEXT('part definition',#221766,'mechanical');
#221768=PRODUCT('X11134','MAS-607','STEP AP214',(#221767));
#221769=PRODUCT('2026-10-05-23-02-19-012','Valve Body',$,(#221767));
#221770=PRODUCT('2026-10-05-23-02-27-655','Control Handle',$,(#221767));
#221771=PRODUCT('2026-10-05-23-02-30-143','Shower Hose Connector',$,(#221767));
#221772=PRODUCT('2026-10-05-23-02-32-151','Gasket (1)',$,(#221767));
#221773=PRODUCT('2026-10-05-23-02-34-900','Coupling Nut',$,(#221767));
#221774=PRODUCT('2026-10-05-23-02-36-870','Gasket',$,(#221767));
#221775=PRODUCT('2026-10-05-23-02-39-335','Wall Flange Rosette',$,(#221767));
#221776=PRODUCT('2026-10-05-23-02-40-799','Coupling Nut (1)',$,(#221767));
#221777=PRODUCT('2026-10-05-23-02-42-253','Diverter',$,(#221767));
#221778=PRODUCT('2026-10-05-23-02-44-166','Wall Flange Rosette (1)',$,(#221767));
#221779=PRODUCT('2026-10-05-23-02-46-115','Aerator',$,(#221767));
#221780=PRODUCT('2026-10-05-23-02-49-354','Eccentric Connector (1)',$,(#221767));
#221781=PRODUCT('2026-10-05-23-03-42-219','Eccentric Connector',$,(#221767));
#221782=PRESENTATION_STYLE_ASSIGNMENT((#221784));
#221783=PRESENTATION_STYLE_ASSIGNMENT((#221785));
#221784=SURFACE_STYLE_USAGE(.BOTH.,#221786);
#221785=SURFACE_STYLE_USAGE(.BOTH.,#221787);
#221786=SURFACE_SIDE_STYLE('',(#221788));
#221787=SURFACE_SIDE_STYLE('',(#221789));
#221788=SURFACE_STYLE_FILL_AREA(#221790);
#221789=SURFACE_STYLE_FILL_AREA(#221791);
#221790=FILL_AREA_STYLE('Steel - Satin',(#221792));
#221791=FILL_AREA_STYLE('Opaque(202,209,238)',(#221793));
#221792=FILL_AREA_STYLE_COLOUR('Steel - Satin',#221794);
#221793=FILL_AREA_STYLE_COLOUR('Opaque(202,209,238)',#221795);
#221794=COLOUR_RGB('Steel - Satin', 0.66274510, 0.83137255, 0.94901961);
#221795=COLOUR_RGB('Opaque(202,209,238)', 0.09019608, 0.27058824, 0.51372549);
ENDSEC;
END-ISO-10303-21;
